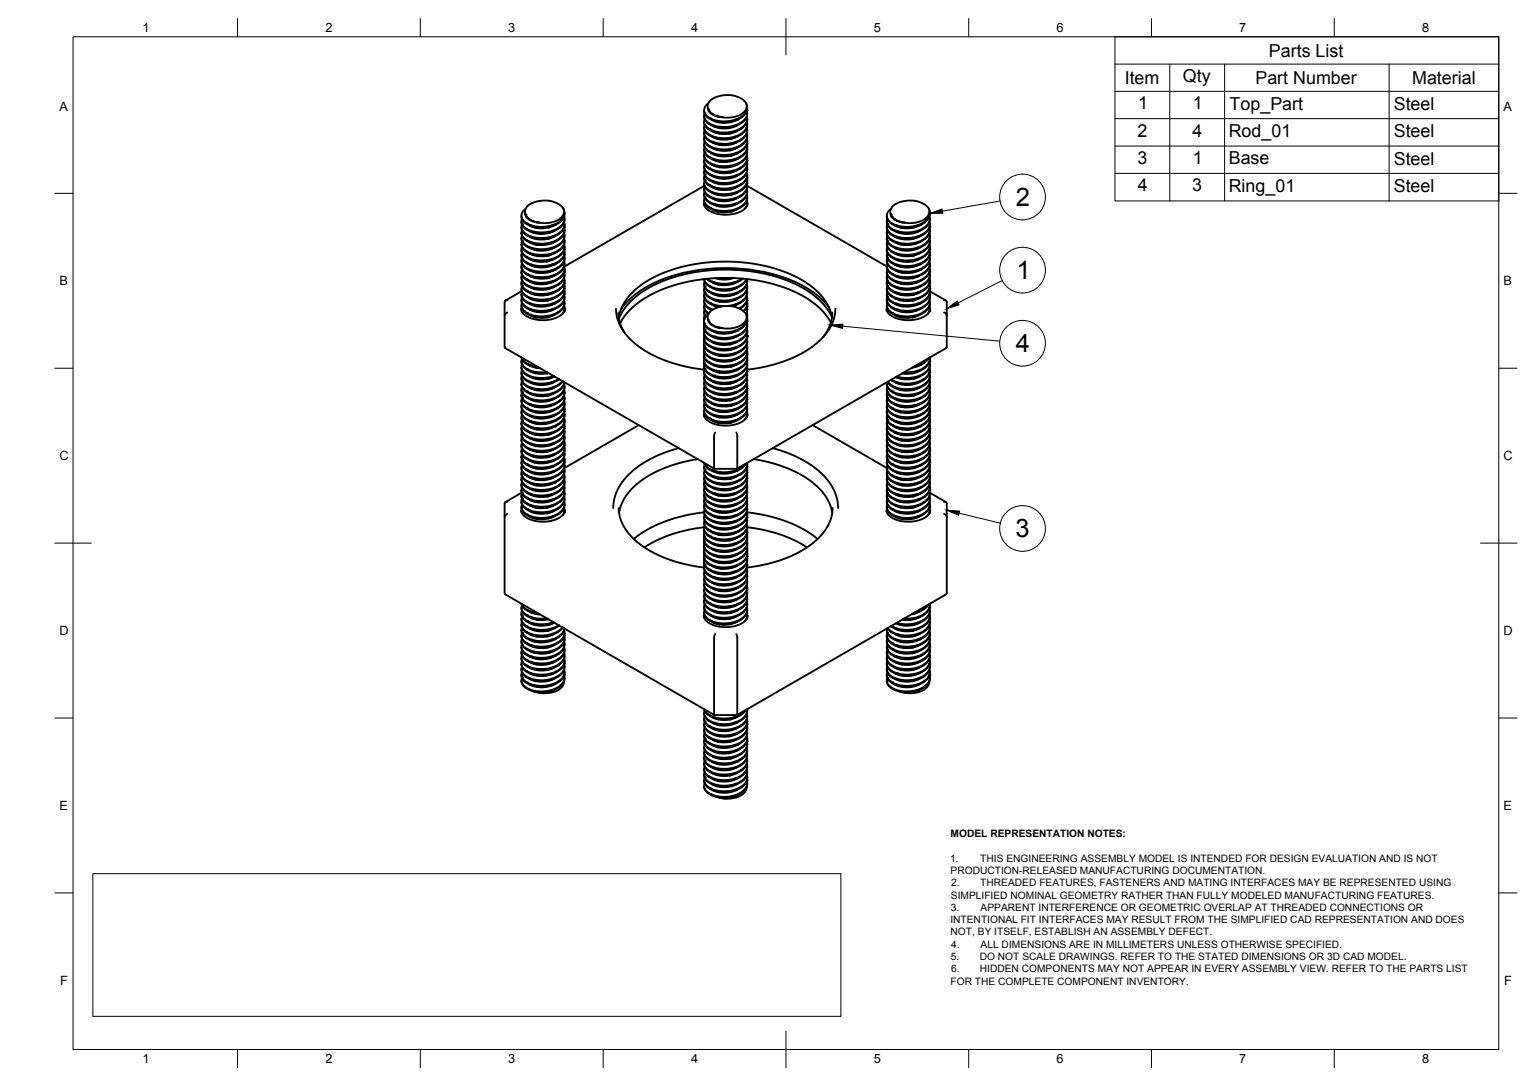
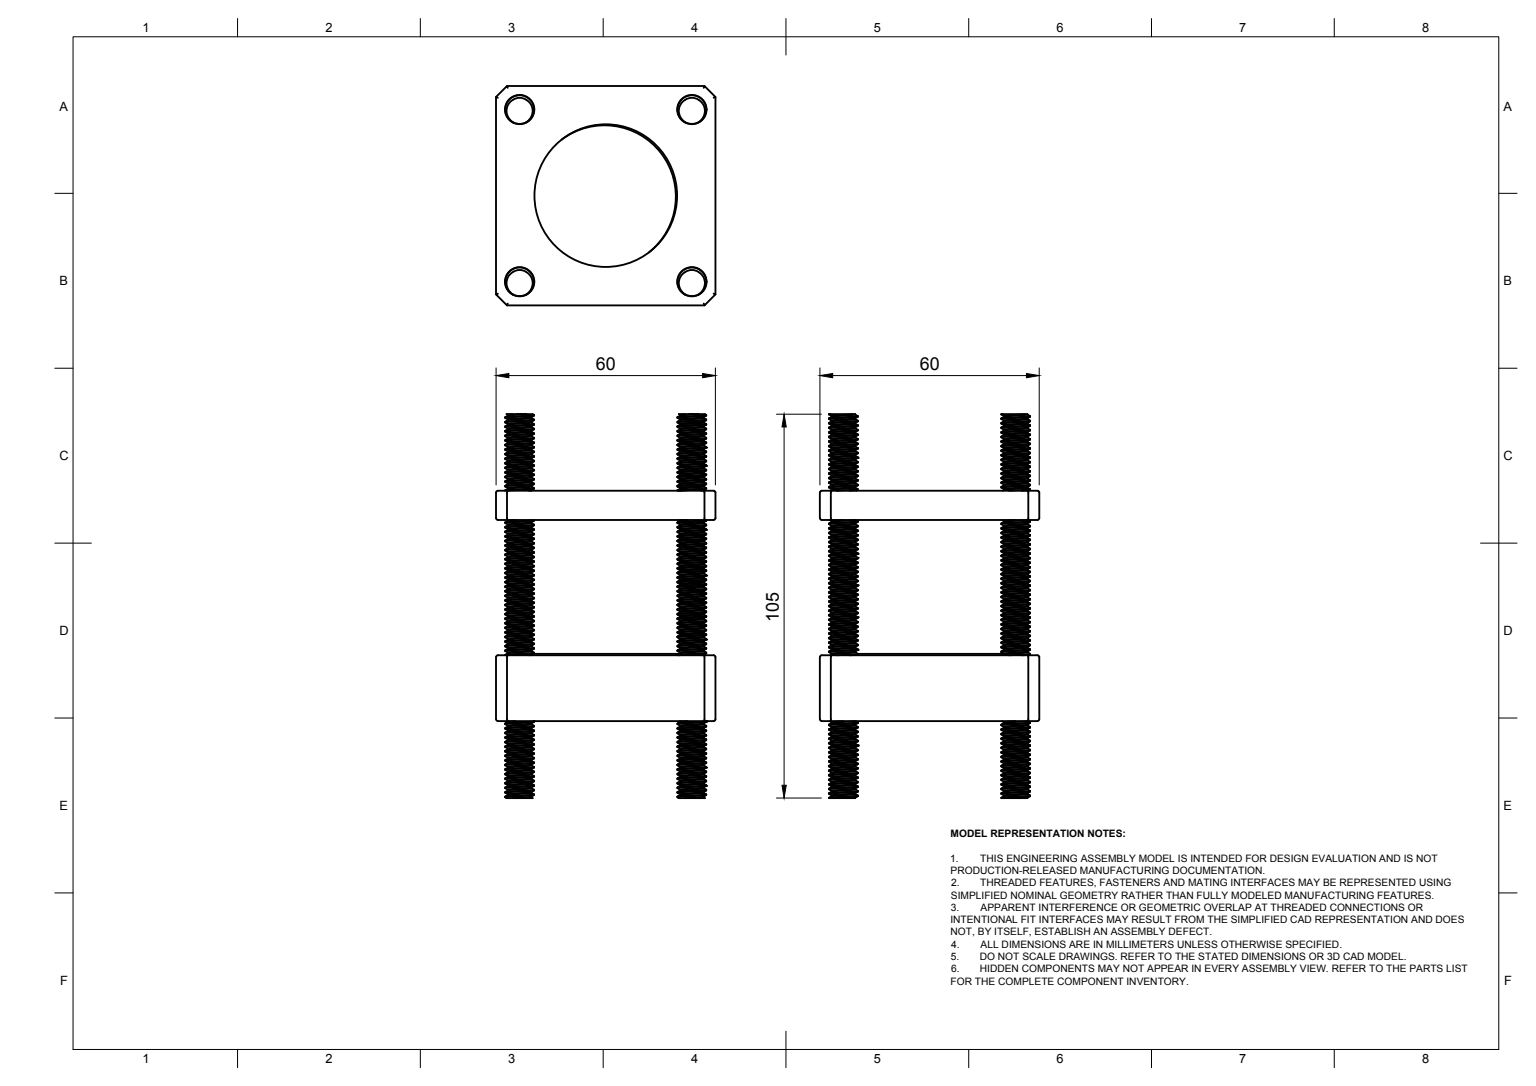
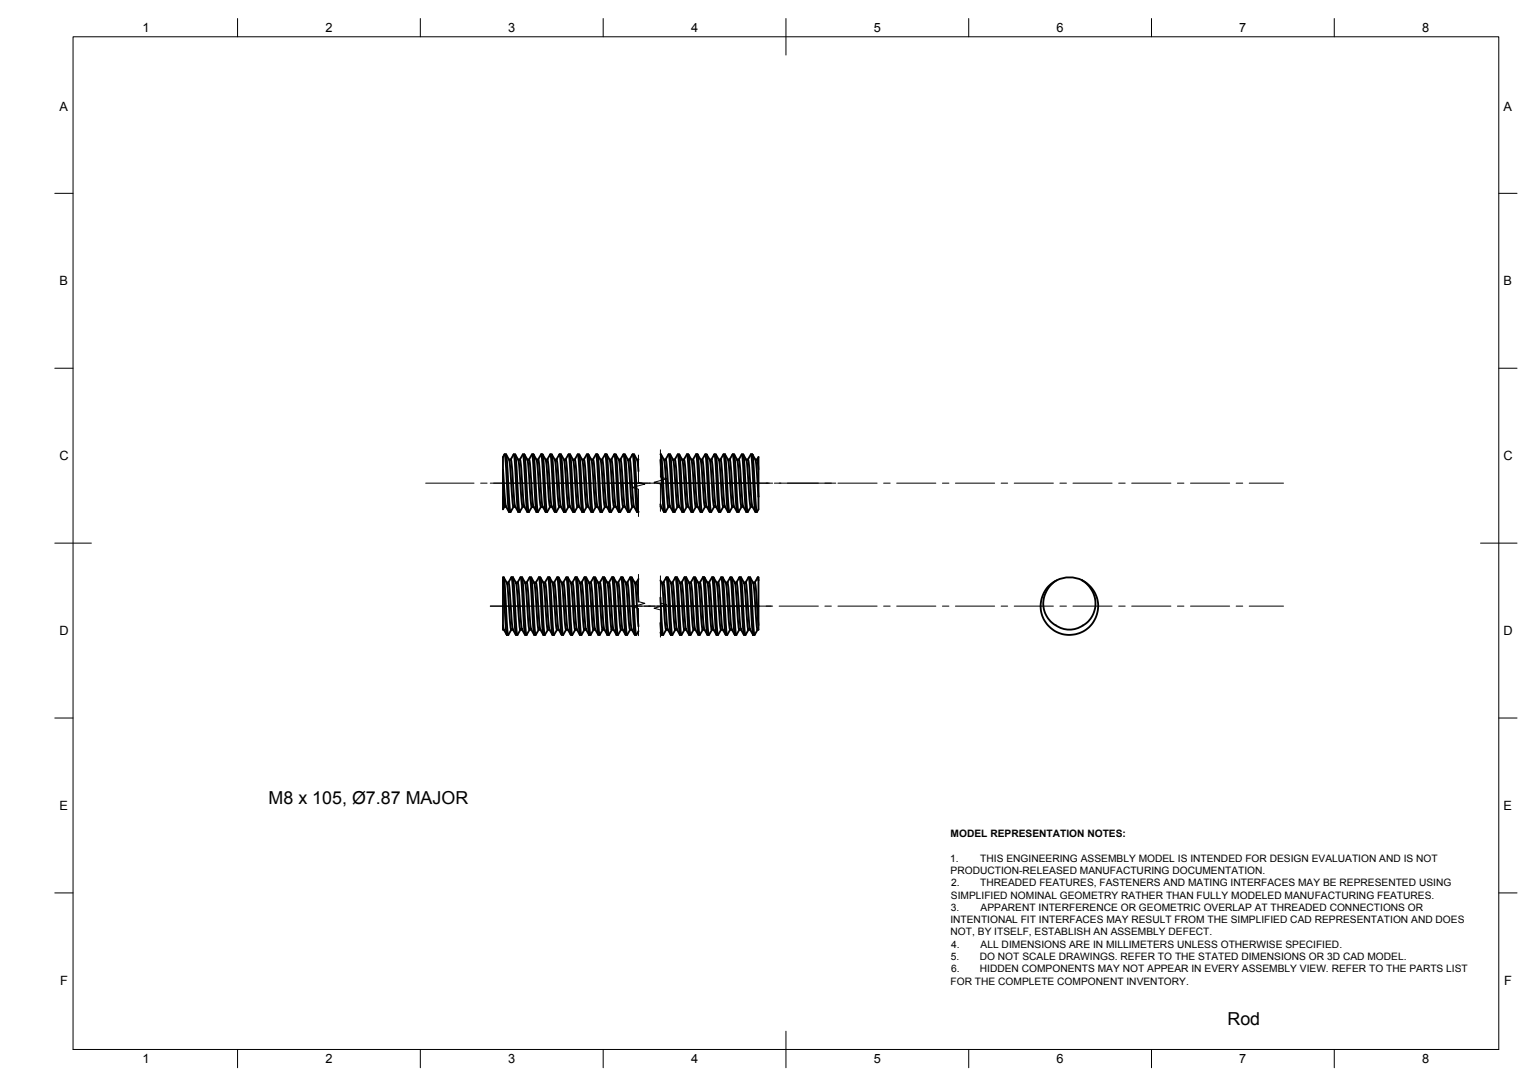
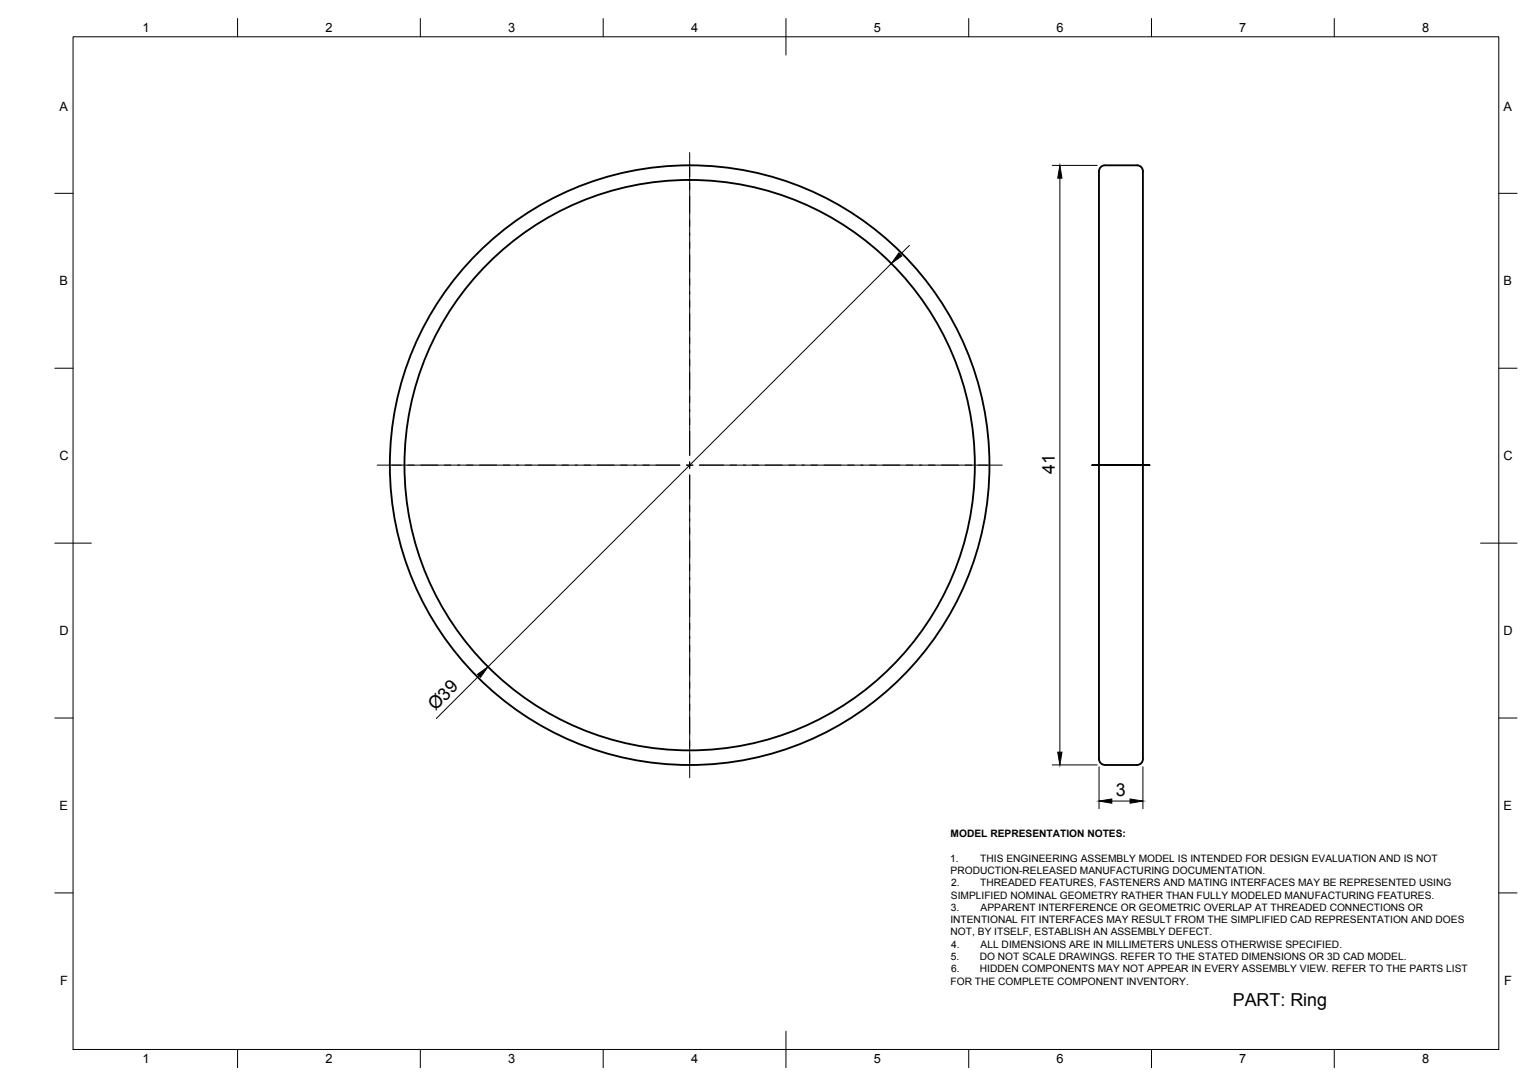
ISO-10303-21;
HEADER;
/* Generated by software containing ST-Developer
 * from STEP Tools, Inc. (www.steptools.com) 
 */

FILE_DESCRIPTION(
/* description */ (''),
/* implementation_level */ '2;1');

FILE_NAME(
/* name */ 'BR-170',
/* time_stamp */ '2026-10-05T14:32:37-07:00',
/* author */ (''),
/* organization */ (''),
/* preprocessor_version */ 'ST-DEVELOPER v20.2',
/* originating_system */ 'Autodesk Translation Framework v15.15.0.0',
/* authorisation */ '');

FILE_SCHEMA (('AUTOMOTIVE_DESIGN { 1 0 10303 214 3 1 1 }'));
ENDSEC;

DATA;
#10=MECHANICAL_DESIGN_GEOMETRIC_PRESENTATION_REPRESENTATION('',(#494,#495,
#496,#497),#74103);
#11=ITEM_DEFINED_TRANSFORMATION($,$,#4623,#4938);
#12=ITEM_DEFINED_TRANSFORMATION($,$,#4845,#4939);
#13=ITEM_DEFINED_TRANSFORMATION($,$,#4729,#4940);
#14=ITEM_DEFINED_TRANSFORMATION($,$,#4824,#4941);
#15=ITEM_DEFINED_TRANSFORMATION($,$,#4824,#4942);
#16=ITEM_DEFINED_TRANSFORMATION($,$,#4824,#4943);
#17=ITEM_DEFINED_TRANSFORMATION($,$,#4845,#4944);
#18=ITEM_DEFINED_TRANSFORMATION($,$,#4845,#4945);
#19=ITEM_DEFINED_TRANSFORMATION($,$,#4845,#4946);
#20=(
REPRESENTATION_RELATIONSHIP($,$,#74128,#74127)
REPRESENTATION_RELATIONSHIP_WITH_TRANSFORMATION(#11)
SHAPE_REPRESENTATION_RELATIONSHIP()
);
#21=(
REPRESENTATION_RELATIONSHIP($,$,#74131,#74127)
REPRESENTATION_RELATIONSHIP_WITH_TRANSFORMATION(#12)
SHAPE_REPRESENTATION_RELATIONSHIP()
);
#22=(
REPRESENTATION_RELATIONSHIP($,$,#74129,#74127)
REPRESENTATION_RELATIONSHIP_WITH_TRANSFORMATION(#13)
SHAPE_REPRESENTATION_RELATIONSHIP()
);
#23=(
REPRESENTATION_RELATIONSHIP($,$,#74130,#74127)
REPRESENTATION_RELATIONSHIP_WITH_TRANSFORMATION(#14)
SHAPE_REPRESENTATION_RELATIONSHIP()
);
#24=(
REPRESENTATION_RELATIONSHIP($,$,#74130,#74127)
REPRESENTATION_RELATIONSHIP_WITH_TRANSFORMATION(#15)
SHAPE_REPRESENTATION_RELATIONSHIP()
);
#25=(
REPRESENTATION_RELATIONSHIP($,$,#74130,#74127)
REPRESENTATION_RELATIONSHIP_WITH_TRANSFORMATION(#16)
SHAPE_REPRESENTATION_RELATIONSHIP()
);
#26=(
REPRESENTATION_RELATIONSHIP($,$,#74131,#74127)
REPRESENTATION_RELATIONSHIP_WITH_TRANSFORMATION(#17)
SHAPE_REPRESENTATION_RELATIONSHIP()
);
#27=(
REPRESENTATION_RELATIONSHIP($,$,#74131,#74127)
REPRESENTATION_RELATIONSHIP_WITH_TRANSFORMATION(#18)
SHAPE_REPRESENTATION_RELATIONSHIP()
);
#28=(
REPRESENTATION_RELATIONSHIP($,$,#74131,#74127)
REPRESENTATION_RELATIONSHIP_WITH_TRANSFORMATION(#19)
SHAPE_REPRESENTATION_RELATIONSHIP()
);
#29=CONTEXT_DEPENDENT_SHAPE_REPRESENTATION(#20,#74118);
#30=CONTEXT_DEPENDENT_SHAPE_REPRESENTATION(#21,#74119);
#31=CONTEXT_DEPENDENT_SHAPE_REPRESENTATION(#22,#74120);
#32=CONTEXT_DEPENDENT_SHAPE_REPRESENTATION(#23,#74121);
#33=CONTEXT_DEPENDENT_SHAPE_REPRESENTATION(#24,#74122);
#34=CONTEXT_DEPENDENT_SHAPE_REPRESENTATION(#25,#74123);
#35=CONTEXT_DEPENDENT_SHAPE_REPRESENTATION(#26,#74124);
#36=CONTEXT_DEPENDENT_SHAPE_REPRESENTATION(#27,#74125);
#37=CONTEXT_DEPENDENT_SHAPE_REPRESENTATION(#28,#74126);
#38=NEXT_ASSEMBLY_USAGE_OCCURRENCE('Top_Part:1','Top_Part:1',
'Top_Part:1',#74133,#74134,'Top_Part:1');
#39=NEXT_ASSEMBLY_USAGE_OCCURRENCE('Rod_01:1','Rod_01:1','Rod_01:1',#74133,
#74137,'Rod_01:1');
#40=NEXT_ASSEMBLY_USAGE_OCCURRENCE('Base:1','Base:1','Base:1',#74133,#74135,
'Base:1');
#41=NEXT_ASSEMBLY_USAGE_OCCURRENCE('Ring_01:1','Ring_01:1','Ring_01:1',
#74133,#74136,'Ring_01:1');
#42=NEXT_ASSEMBLY_USAGE_OCCURRENCE('Ring_01:2','Ring_01:2','Ring_01:2',
#74133,#74136,'Ring_01:2');
#43=NEXT_ASSEMBLY_USAGE_OCCURRENCE('Ring_01:3','Ring_01:3','Ring_01:3',
#74133,#74136,'Ring_01:3');
#44=NEXT_ASSEMBLY_USAGE_OCCURRENCE('Rod_01:2','Rod_01:2','Rod_01:2',#74133,
#74137,'Rod_01:2');
#45=NEXT_ASSEMBLY_USAGE_OCCURRENCE('Rod_01:3','Rod_01:3','Rod_01:3',#74133,
#74137,'Rod_01:3');
#46=NEXT_ASSEMBLY_USAGE_OCCURRENCE('Rod_01:4','Rod_01:4','Rod_01:4',#74133,
#74137,'Rod_01:4');
#47=B_SPLINE_SURFACE_WITH_KNOTS('',3,3,((#69430,#69431,#69432,#69433,#69434,
#69435,#69436,#69437,#69438,#69439,#69440,#69441,#69442,#69443,#69444,#69445,
#69446,#69447,#69448,#69449,#69450,#69451,#69452,#69453,#69454,#69455,#69456,
#69457,#69458,#69459,#69460,#69461,#69462,#69463,#69464,#69465,#69466,#69467,
#69468,#69469,#69470,#69471,#69472,#69473,#69474,#69475,#69476,#69477,#69478,
#69479,#69480,#69481,#69482,#69483,#69484,#69485,#69486,#69487,#69488,#69489,
#69490,#69491,#69492,#69493,#69494,#69495,#69496,#69497,#69498,#69499,#69500,
#69501,#69502,#69503,#69504,#69505,#69506,#69507,#69508,#69509,#69510,#69511,
#69512,#69513,#69514,#69515,#69516,#69517,#69518,#69519,#69520,#69521,#69522,
#69523,#69524,#69525,#69526,#69527,#69528,#69529,#69530,#69531,#69532,#69533,
#69534,#69535,#69536,#69537,#69538,#69539,#69540,#69541,#69542,#69543,#69544,
#69545,#69546,#69547,#69548,#69549,#69550,#69551,#69552,#69553,#69554,#69555,
#69556,#69557,#69558,#69559,#69560,#69561,#69562,#69563,#69564,#69565,#69566,
#69567,#69568,#69569,#69570,#69571,#69572,#69573,#69574,#69575,#69576,#69577,
#69578,#69579,#69580,#69581,#69582,#69583,#69584,#69585,#69586,#69587,#69588,
#69589,#69590,#69591,#69592,#69593,#69594,#69595,#69596,#69597,#69598,#69599,
#69600,#69601,#69602,#69603,#69604,#69605,#69606,#69607,#69608,#69609,#69610,
#69611,#69612,#69613,#69614,#69615,#69616,#69617,#69618,#69619,#69620,#69621,
#69622,#69623,#69624,#69625,#69626,#69627,#69628,#69629,#69630,#69631,#69632,
#69633,#69634,#69635,#69636,#69637,#69638,#69639,#69640,#69641,#69642,#69643,
#69644,#69645,#69646,#69647,#69648,#69649,#69650,#69651,#69652,#69653,#69654,
#69655,#69656,#69657,#69658,#69659,#69660,#69661,#69662,#69663,#69664,#69665,
#69666,#69667,#69668,#69669,#69670,#69671,#69672,#69673,#69674,#69675,#69676,
#69677,#69678,#69679,#69680,#69681,#69682,#69683,#69684,#69685,#69686,#69687,
#69688,#69689,#69690,#69691,#69692,#69693,#69694,#69695,#69696,#69697,#69698,
#69699,#69700,#69701,#69702,#69703,#69704,#69705,#69706,#69707,#69708,#69709,
#69710,#69711,#69712,#69713,#69714,#69715,#69716,#69717,#69718,#69719,#69720,
#69721,#69722,#69723,#69724,#69725,#69726,#69727,#69728,#69729,#69730,#69731,
#69732,#69733,#69734,#69735,#69736,#69737,#69738,#69739,#69740,#69741,#69742,
#69743,#69744,#69745,#69746,#69747,#69748,#69749,#69750,#69751,#69752,#69753,
#69754,#69755,#69756,#69757,#69758,#69759,#69760,#69761,#69762,#69763,#69764,
#69765,#69766,#69767,#69768,#69769,#69770,#69771,#69772,#69773,#69774,#69775,
#69776,#69777,#69778,#69779,#69780,#69781,#69782,#69783,#69784,#69785,#69786,
#69787,#69788,#69789,#69790,#69791,#69792,#69793,#69794,#69795,#69796,#69797,
#69798,#69799,#69800,#69801,#69802,#69803,#69804,#69805,#69806,#69807,#69808,
#69809,#69810,#69811,#69812,#69813,#69814,#69815,#69816,#69817,#69818,#69819,
#69820,#69821,#69822,#69823,#69824,#69825,#69826,#69827,#69828,#69829,#69830,
#69831,#69832,#69833,#69834,#69835,#69836,#69837,#69838,#69839,#69840,#69841,
#69842,#69843,#69844,#69845,#69846,#69847,#69848,#69849,#69850,#69851,#69852,
#69853,#69854,#69855,#69856,#69857,#69858,#69859,#69860,#69861,#69862,#69863,
#69864,#69865,#69866,#69867,#69868,#69869,#69870,#69871,#69872,#69873,#69874,
#69875,#69876,#69877,#69878,#69879,#69880,#69881,#69882,#69883,#69884,#69885,
#69886,#69887,#69888,#69889,#69890,#69891,#69892,#69893,#69894,#69895,#69896,
#69897,#69898,#69899,#69900,#69901,#69902,#69903,#69904,#69905,#69906,#69907,
#69908,#69909,#69910,#69911,#69912,#69913,#69914,#69915,#69916,#69917,#69918,
#69919,#69920,#69921,#69922,#69923,#69924,#69925,#69926,#69927,#69928,#69929,
#69930,#69931,#69932,#69933,#69934,#69935,#69936,#69937,#69938,#69939,#69940,
#69941,#69942,#69943,#69944,#69945,#69946,#69947,#69948,#69949,#69950,#69951,
#69952,#69953,#69954,#69955,#69956,#69957,#69958,#69959,#69960,#69961,#69962),
(#69963,#69964,#69965,#69966,#69967,#69968,#69969,#69970,#69971,#69972,
#69973,#69974,#69975,#69976,#69977,#69978,#69979,#69980,#69981,#69982,#69983,
#69984,#69985,#69986,#69987,#69988,#69989,#69990,#69991,#69992,#69993,#69994,
#69995,#69996,#69997,#69998,#69999,#70000,#70001,#70002,#70003,#70004,#70005,
#70006,#70007,#70008,#70009,#70010,#70011,#70012,#70013,#70014,#70015,#70016,
#70017,#70018,#70019,#70020,#70021,#70022,#70023,#70024,#70025,#70026,#70027,
#70028,#70029,#70030,#70031,#70032,#70033,#70034,#70035,#70036,#70037,#70038,
#70039,#70040,#70041,#70042,#70043,#70044,#70045,#70046,#70047,#70048,#70049,
#70050,#70051,#70052,#70053,#70054,#70055,#70056,#70057,#70058,#70059,#70060,
#70061,#70062,#70063,#70064,#70065,#70066,#70067,#70068,#70069,#70070,#70071,
#70072,#70073,#70074,#70075,#70076,#70077,#70078,#70079,#70080,#70081,#70082,
#70083,#70084,#70085,#70086,#70087,#70088,#70089,#70090,#70091,#70092,#70093,
#70094,#70095,#70096,#70097,#70098,#70099,#70100,#70101,#70102,#70103,#70104,
#70105,#70106,#70107,#70108,#70109,#70110,#70111,#70112,#70113,#70114,#70115,
#70116,#70117,#70118,#70119,#70120,#70121,#70122,#70123,#70124,#70125,#70126,
#70127,#70128,#70129,#70130,#70131,#70132,#70133,#70134,#70135,#70136,#70137,
#70138,#70139,#70140,#70141,#70142,#70143,#70144,#70145,#70146,#70147,#70148,
#70149,#70150,#70151,#70152,#70153,#70154,#70155,#70156,#70157,#70158,#70159,
#70160,#70161,#70162,#70163,#70164,#70165,#70166,#70167,#70168,#70169,#70170,
#70171,#70172,#70173,#70174,#70175,#70176,#70177,#70178,#70179,#70180,#70181,
#70182,#70183,#70184,#70185,#70186,#70187,#70188,#70189,#70190,#70191,#70192,
#70193,#70194,#70195,#70196,#70197,#70198,#70199,#70200,#70201,#70202,#70203,
#70204,#70205,#70206,#70207,#70208,#70209,#70210,#70211,#70212,#70213,#70214,
#70215,#70216,#70217,#70218,#70219,#70220,#70221,#70222,#70223,#70224,#70225,
#70226,#70227,#70228,#70229,#70230,#70231,#70232,#70233,#70234,#70235,#70236,
#70237,#70238,#70239,#70240,#70241,#70242,#70243,#70244,#70245,#70246,#70247,
#70248,#70249,#70250,#70251,#70252,#70253,#70254,#70255,#70256,#70257,#70258,
#70259,#70260,#70261,#70262,#70263,#70264,#70265,#70266,#70267,#70268,#70269,
#70270,#70271,#70272,#70273,#70274,#70275,#70276,#70277,#70278,#70279,#70280,
#70281,#70282,#70283,#70284,#70285,#70286,#70287,#70288,#70289,#70290,#70291,
#70292,#70293,#70294,#70295,#70296,#70297,#70298,#70299,#70300,#70301,#70302,
#70303,#70304,#70305,#70306,#70307,#70308,#70309,#70310,#70311,#70312,#70313,
#70314,#70315,#70316,#70317,#70318,#70319,#70320,#70321,#70322,#70323,#70324,
#70325,#70326,#70327,#70328,#70329,#70330,#70331,#70332,#70333,#70334,#70335,
#70336,#70337,#70338,#70339,#70340,#70341,#70342,#70343,#70344,#70345,#70346,
#70347,#70348,#70349,#70350,#70351,#70352,#70353,#70354,#70355,#70356,#70357,
#70358,#70359,#70360,#70361,#70362,#70363,#70364,#70365,#70366,#70367,#70368,
#70369,#70370,#70371,#70372,#70373,#70374,#70375,#70376,#70377,#70378,#70379,
#70380,#70381,#70382,#70383,#70384,#70385,#70386,#70387,#70388,#70389,#70390,
#70391,#70392,#70393,#70394,#70395,#70396,#70397,#70398,#70399,#70400,#70401,
#70402,#70403,#70404,#70405,#70406,#70407,#70408,#70409,#70410,#70411,#70412,
#70413,#70414,#70415,#70416,#70417,#70418,#70419,#70420,#70421,#70422,#70423,
#70424,#70425,#70426,#70427,#70428,#70429,#70430,#70431,#70432,#70433,#70434,
#70435,#70436,#70437,#70438,#70439,#70440,#70441,#70442,#70443,#70444,#70445,
#70446,#70447,#70448,#70449,#70450,#70451,#70452,#70453,#70454,#70455,#70456,
#70457,#70458,#70459,#70460,#70461,#70462,#70463,#70464,#70465,#70466,#70467,
#70468,#70469,#70470,#70471,#70472,#70473,#70474,#70475,#70476,#70477,#70478,
#70479,#70480,#70481,#70482,#70483,#70484,#70485,#70486,#70487,#70488,#70489,
#70490,#70491,#70492,#70493,#70494,#70495),(#70496,#70497,#70498,#70499,
#70500,#70501,#70502,#70503,#70504,#70505,#70506,#70507,#70508,#70509,#70510,
#70511,#70512,#70513,#70514,#70515,#70516,#70517,#70518,#70519,#70520,#70521,
#70522,#70523,#70524,#70525,#70526,#70527,#70528,#70529,#70530,#70531,#70532,
#70533,#70534,#70535,#70536,#70537,#70538,#70539,#70540,#70541,#70542,#70543,
#70544,#70545,#70546,#70547,#70548,#70549,#70550,#70551,#70552,#70553,#70554,
#70555,#70556,#70557,#70558,#70559,#70560,#70561,#70562,#70563,#70564,#70565,
#70566,#70567,#70568,#70569,#70570,#70571,#70572,#70573,#70574,#70575,#70576,
#70577,#70578,#70579,#70580,#70581,#70582,#70583,#70584,#70585,#70586,#70587,
#70588,#70589,#70590,#70591,#70592,#70593,#70594,#70595,#70596,#70597,#70598,
#70599,#70600,#70601,#70602,#70603,#70604,#70605,#70606,#70607,#70608,#70609,
#70610,#70611,#70612,#70613,#70614,#70615,#70616,#70617,#70618,#70619,#70620,
#70621,#70622,#70623,#70624,#70625,#70626,#70627,#70628,#70629,#70630,#70631,
#70632,#70633,#70634,#70635,#70636,#70637,#70638,#70639,#70640,#70641,#70642,
#70643,#70644,#70645,#70646,#70647,#70648,#70649,#70650,#70651,#70652,#70653,
#70654,#70655,#70656,#70657,#70658,#70659,#70660,#70661,#70662,#70663,#70664,
#70665,#70666,#70667,#70668,#70669,#70670,#70671,#70672,#70673,#70674,#70675,
#70676,#70677,#70678,#70679,#70680,#70681,#70682,#70683,#70684,#70685,#70686,
#70687,#70688,#70689,#70690,#70691,#70692,#70693,#70694,#70695,#70696,#70697,
#70698,#70699,#70700,#70701,#70702,#70703,#70704,#70705,#70706,#70707,#70708,
#70709,#70710,#70711,#70712,#70713,#70714,#70715,#70716,#70717,#70718,#70719,
#70720,#70721,#70722,#70723,#70724,#70725,#70726,#70727,#70728,#70729,#70730,
#70731,#70732,#70733,#70734,#70735,#70736,#70737,#70738,#70739,#70740,#70741,
#70742,#70743,#70744,#70745,#70746,#70747,#70748,#70749,#70750,#70751,#70752,
#70753,#70754,#70755,#70756,#70757,#70758,#70759,#70760,#70761,#70762,#70763,
#70764,#70765,#70766,#70767,#70768,#70769,#70770,#70771,#70772,#70773,#70774,
#70775,#70776,#70777,#70778,#70779,#70780,#70781,#70782,#70783,#70784,#70785,
#70786,#70787,#70788,#70789,#70790,#70791,#70792,#70793,#70794,#70795,#70796,
#70797,#70798,#70799,#70800,#70801,#70802,#70803,#70804,#70805,#70806,#70807,
#70808,#70809,#70810,#70811,#70812,#70813,#70814,#70815,#70816,#70817,#70818,
#70819,#70820,#70821,#70822,#70823,#70824,#70825,#70826,#70827,#70828,#70829,
#70830,#70831,#70832,#70833,#70834,#70835,#70836,#70837,#70838,#70839,#70840,
#70841,#70842,#70843,#70844,#70845,#70846,#70847,#70848,#70849,#70850,#70851,
#70852,#70853,#70854,#70855,#70856,#70857,#70858,#70859,#70860,#70861,#70862,
#70863,#70864,#70865,#70866,#70867,#70868,#70869,#70870,#70871,#70872,#70873,
#70874,#70875,#70876,#70877,#70878,#70879,#70880,#70881,#70882,#70883,#70884,
#70885,#70886,#70887,#70888,#70889,#70890,#70891,#70892,#70893,#70894,#70895,
#70896,#70897,#70898,#70899,#70900,#70901,#70902,#70903,#70904,#70905,#70906,
#70907,#70908,#70909,#70910,#70911,#70912,#70913,#70914,#70915,#70916,#70917,
#70918,#70919,#70920,#70921,#70922,#70923,#70924,#70925,#70926,#70927,#70928,
#70929,#70930,#70931,#70932,#70933,#70934,#70935,#70936,#70937,#70938,#70939,
#70940,#70941,#70942,#70943,#70944,#70945,#70946,#70947,#70948,#70949,#70950,
#70951,#70952,#70953,#70954,#70955,#70956,#70957,#70958,#70959,#70960,#70961,
#70962,#70963,#70964,#70965,#70966,#70967,#70968,#70969,#70970,#70971,#70972,
#70973,#70974,#70975,#70976,#70977,#70978,#70979,#70980,#70981,#70982,#70983,
#70984,#70985,#70986,#70987,#70988,#70989,#70990,#70991,#70992,#70993,#70994,
#70995,#70996,#70997,#70998,#70999,#71000,#71001,#71002,#71003,#71004,#71005,
#71006,#71007,#71008,#71009,#71010,#71011,#71012,#71013,#71014,#71015,#71016,
#71017,#71018,#71019,#71020,#71021,#71022,#71023,#71024,#71025,#71026,#71027,
#71028),(#71029,#71030,#71031,#71032,#71033,#71034,#71035,#71036,#71037,
#71038,#71039,#71040,#71041,#71042,#71043,#71044,#71045,#71046,#71047,#71048,
#71049,#71050,#71051,#71052,#71053,#71054,#71055,#71056,#71057,#71058,#71059,
#71060,#71061,#71062,#71063,#71064,#71065,#71066,#71067,#71068,#71069,#71070,
#71071,#71072,#71073,#71074,#71075,#71076,#71077,#71078,#71079,#71080,#71081,
#71082,#71083,#71084,#71085,#71086,#71087,#71088,#71089,#71090,#71091,#71092,
#71093,#71094,#71095,#71096,#71097,#71098,#71099,#71100,#71101,#71102,#71103,
#71104,#71105,#71106,#71107,#71108,#71109,#71110,#71111,#71112,#71113,#71114,
#71115,#71116,#71117,#71118,#71119,#71120,#71121,#71122,#71123,#71124,#71125,
#71126,#71127,#71128,#71129,#71130,#71131,#71132,#71133,#71134,#71135,#71136,
#71137,#71138,#71139,#71140,#71141,#71142,#71143,#71144,#71145,#71146,#71147,
#71148,#71149,#71150,#71151,#71152,#71153,#71154,#71155,#71156,#71157,#71158,
#71159,#71160,#71161,#71162,#71163,#71164,#71165,#71166,#71167,#71168,#71169,
#71170,#71171,#71172,#71173,#71174,#71175,#71176,#71177,#71178,#71179,#71180,
#71181,#71182,#71183,#71184,#71185,#71186,#71187,#71188,#71189,#71190,#71191,
#71192,#71193,#71194,#71195,#71196,#71197,#71198,#71199,#71200,#71201,#71202,
#71203,#71204,#71205,#71206,#71207,#71208,#71209,#71210,#71211,#71212,#71213,
#71214,#71215,#71216,#71217,#71218,#71219,#71220,#71221,#71222,#71223,#71224,
#71225,#71226,#71227,#71228,#71229,#71230,#71231,#71232,#71233,#71234,#71235,
#71236,#71237,#71238,#71239,#71240,#71241,#71242,#71243,#71244,#71245,#71246,
#71247,#71248,#71249,#71250,#71251,#71252,#71253,#71254,#71255,#71256,#71257,
#71258,#71259,#71260,#71261,#71262,#71263,#71264,#71265,#71266,#71267,#71268,
#71269,#71270,#71271,#71272,#71273,#71274,#71275,#71276,#71277,#71278,#71279,
#71280,#71281,#71282,#71283,#71284,#71285,#71286,#71287,#71288,#71289,#71290,
#71291,#71292,#71293,#71294,#71295,#71296,#71297,#71298,#71299,#71300,#71301,
#71302,#71303,#71304,#71305,#71306,#71307,#71308,#71309,#71310,#71311,#71312,
#71313,#71314,#71315,#71316,#71317,#71318,#71319,#71320,#71321,#71322,#71323,
#71324,#71325,#71326,#71327,#71328,#71329,#71330,#71331,#71332,#71333,#71334,
#71335,#71336,#71337,#71338,#71339,#71340,#71341,#71342,#71343,#71344,#71345,
#71346,#71347,#71348,#71349,#71350,#71351,#71352,#71353,#71354,#71355,#71356,
#71357,#71358,#71359,#71360,#71361,#71362,#71363,#71364,#71365,#71366,#71367,
#71368,#71369,#71370,#71371,#71372,#71373,#71374,#71375,#71376,#71377,#71378,
#71379,#71380,#71381,#71382,#71383,#71384,#71385,#71386,#71387,#71388,#71389,
#71390,#71391,#71392,#71393,#71394,#71395,#71396,#71397,#71398,#71399,#71400,
#71401,#71402,#71403,#71404,#71405,#71406,#71407,#71408,#71409,#71410,#71411,
#71412,#71413,#71414,#71415,#71416,#71417,#71418,#71419,#71420,#71421,#71422,
#71423,#71424,#71425,#71426,#71427,#71428,#71429,#71430,#71431,#71432,#71433,
#71434,#71435,#71436,#71437,#71438,#71439,#71440,#71441,#71442,#71443,#71444,
#71445,#71446,#71447,#71448,#71449,#71450,#71451,#71452,#71453,#71454,#71455,
#71456,#71457,#71458,#71459,#71460,#71461,#71462,#71463,#71464,#71465,#71466,
#71467,#71468,#71469,#71470,#71471,#71472,#71473,#71474,#71475,#71476,#71477,
#71478,#71479,#71480,#71481,#71482,#71483,#71484,#71485,#71486,#71487,#71488,
#71489,#71490,#71491,#71492,#71493,#71494,#71495,#71496,#71497,#71498,#71499,
#71500,#71501,#71502,#71503,#71504,#71505,#71506,#71507,#71508,#71509,#71510,
#71511,#71512,#71513,#71514,#71515,#71516,#71517,#71518,#71519,#71520,#71521,
#71522,#71523,#71524,#71525,#71526,#71527,#71528,#71529,#71530,#71531,#71532,
#71533,#71534,#71535,#71536,#71537,#71538,#71539,#71540,#71541,#71542,#71543,
#71544,#71545,#71546,#71547,#71548,#71549,#71550,#71551,#71552,#71553,#71554,
#71555,#71556,#71557,#71558,#71559,#71560,#71561)),.UNSPECIFIED.,.F.,.F.,
 .F.,(4,4),(4,1,1,1,1,1,1,1,1,1,1,1,1,1,1,1,1,1,1,1,1,1,1,1,1,1,1,1,1,1,
1,1,1,1,1,1,1,1,1,1,1,1,1,1,1,1,1,1,1,1,1,1,1,1,1,1,1,1,1,1,1,1,1,1,1,1,
1,1,1,1,1,1,1,1,1,1,1,1,1,1,1,1,1,1,1,1,1,1,1,1,1,1,1,1,1,1,1,1,1,1,1,1,
1,1,1,1,1,1,1,1,1,1,1,1,1,1,1,1,1,1,1,1,1,1,1,1,1,1,1,1,1,1,1,1,1,1,1,1,
1,1,1,1,1,1,1,1,1,1,1,1,1,1,1,1,1,1,1,1,1,1,1,1,1,1,1,1,1,1,1,1,1,1,1,1,
1,1,1,1,1,1,1,1,1,1,1,1,1,1,1,1,1,1,1,1,1,1,1,1,1,1,1,1,1,1,1,1,1,1,1,1,
1,1,1,1,1,1,1,1,1,1,1,1,1,1,1,1,1,1,1,1,1,1,1,1,1,1,1,1,1,1,1,1,1,1,1,1,
1,1,1,1,1,1,1,1,1,1,1,1,1,1,1,1,1,1,1,1,1,1,1,1,1,1,1,1,1,1,1,1,1,1,1,1,
1,1,1,1,1,1,1,1,1,1,1,1,1,1,1,1,1,1,1,1,1,1,1,1,1,1,1,1,1,1,1,1,1,1,1,1,
1,1,1,1,1,1,1,1,1,1,1,1,1,1,1,1,1,1,1,1,1,1,1,1,1,1,1,1,1,1,1,1,1,1,1,1,
1,1,1,1,1,1,1,1,1,1,1,1,1,1,1,1,1,1,1,1,1,1,1,1,1,1,1,1,1,1,1,1,1,1,1,1,
1,1,1,1,1,1,1,1,1,1,1,1,1,1,1,1,1,1,1,1,1,1,1,1,1,1,1,1,1,1,1,1,1,1,1,1,
1,1,1,1,1,1,1,1,1,1,1,1,1,1,1,1,1,1,1,1,1,1,1,1,1,1,1,1,1,1,1,1,1,1,1,1,
1,1,1,1,1,1,1,1,1,1,1,1,1,1,1,1,1,1,1,1,1,1,1,1,1,1,1,1,1,1,1,1,1,1,1,1,
1,1,1,1,1,1,1,1,1,1,1,1,1,1,1,1,1,1,1,1,1,1,1,1,1,1,1,1,1,1,1,1,4),(-0.000646701964609084,
0.0823585128613958),(8.31473274985906,9.3144474053319,10.3141620608047,
11.3138767162776,12.3135913717504,13.3133060272232,14.3130206826961,15.3127353381689,
16.3124499936417,17.3121646491146,18.3118793045874,19.3115939600602,20.3113086155331,
21.3110232710059,22.3107379264787,23.3104525819516,24.3101672374244,25.3098818928972,
26.30959654837,27.3093112038429,28.3090258593157,29.3087405147885,30.3084551702614,
31.3081698257342,32.307884481207,33.3075991366799,34.3073137921527,35.3070284476255,
36.3067431030984,37.3064577585712,38.306172414044,39.3058870695169,40.3056017249897,
41.3053163804625,42.3050310359354,43.3047456914082,44.304460346881,45.3041750023539,
46.3038896578267,47.3036043132995,48.3033189687724,49.3030336242452,50.302748279718,
51.3024629351909,52.3021775906637,53.3018922461365,54.3016069016094,55.3013215570822,
56.301036212555,57.3007508680278,58.3004655235007,59.3001801789735,60.2998948344463,
61.2996094899192,62.299324145392,63.2990388008648,64.2987534563377,65.2984681118105,
66.2981827672834,67.2978974227562,68.297612078229,69.2973267337018,70.2970413891747,
71.2967560446475,72.2964707001203,73.2961853555932,74.295900011066,75.2956146665388,
76.2953293220117,77.2950439774845,78.2947586329573,79.2944732884302,80.294187943903,
81.2939025993758,82.2936172548487,83.2933319103215,84.2930465657943,85.2927612212672,
86.29247587674,87.2921905322128,88.2919051876857,89.2916198431585,90.2913344986313,
91.2910491541042,92.290763809577,93.2904784650498,94.2901931205227,95.2899077759955,
96.2896224314683,97.2893370869411,98.289051742414,99.2887663978868,100.28848105336,
101.288195708832,102.287910364305,103.287625019778,104.287339675251,105.287054330724,
106.286768986197,107.286483641669,108.286198297142,109.285912952615,110.285627608088,
111.285342263561,112.285056919034,113.284771574506,114.284486229979,115.284200885452,
116.283915540925,117.283630196398,118.283344851871,119.283059507343,120.282774162816,
121.282488818289,122.282203473762,123.281918129235,124.281632784708,125.28134744018,
126.281062095653,127.280776751126,128.280491406599,129.280206062072,130.279920717545,
131.279635373017,132.27935002849,133.279064683963,134.278779339436,135.278493994909,
136.278208650382,137.277923305854,138.277637961327,139.2773526168,140.277067272273,
141.276781927746,142.276496583219,143.276211238691,144.275925894164,145.275640549637,
146.27535520511,147.275069860583,148.274784516056,149.274499171528,150.274213827001,
151.273928482474,152.273643137947,153.27335779342,154.273072448893,155.272787104365,
156.272501759838,157.272216415311,158.271931070784,159.271645726257,160.27136038173,
161.271075037202,162.270789692675,163.270504348148,164.270219003621,165.269933659094,
166.269648314567,167.269362970039,168.269077625512,169.268792280985,170.268506936458,
171.268221591931,172.267936247404,173.267650902876,174.267365558349,175.267080213822,
176.266794869295,177.266509524768,178.266224180241,179.265938835713,180.265653491186,
181.265368146659,182.265082802132,183.264797457605,184.264512113078,185.26422676855,
186.263941424023,187.263656079496,188.263370734969,189.263085390442,190.262800045915,
191.262514701387,192.26222935686,193.261944012333,194.261658667806,195.261373323279,
196.261087978752,197.260802634224,198.260517289697,199.26023194517,200.259946600643,
201.259661256116,202.259375911589,203.259090567061,204.258805222534,205.258519878007,
206.25823453348,207.257949188953,208.257663844426,209.257378499898,210.257093155371,
211.256807810844,212.256522466317,213.25623712179,214.255951777263,215.255666432735,
216.255381088208,217.255095743681,218.254810399154,219.254525054627,220.2542397101,
221.253954365572,222.253669021045,223.253383676518,224.253098331991,225.252812987464,
226.252527642937,227.252242298409,228.251956953882,229.251671609355,230.251386264828,
231.251100920301,232.250815575774,233.250530231246,234.250244886719,235.249959542192,
236.249674197665,237.249388853138,238.249103508611,239.248818164083,240.248532819556,
241.248247475029,242.247962130502,243.247676785975,244.247391441448,245.24710609692,
246.246820752393,247.246535407866,248.246250063339,249.245964718812,250.245679374285,
251.245394029757,252.24510868523,253.244823340703,254.244537996176,255.244252651649,
256.243967307122,257.243681962594,258.243396618067,259.24311127354,260.242825929013,
261.242540584486,262.242255239959,263.241969895431,264.241684550904,265.241399206377,
266.24111386185,267.240828517323,268.240543172795,269.240257828268,270.239972483741,
271.239687139214,272.239401794687,273.23911645016,274.238831105632,275.238545761105,
276.238260416578,277.237975072051,278.237689727524,279.237404382997,280.237119038469,
281.236833693942,282.236548349415,283.236263004888,284.235977660361,285.235692315834,
286.235406971306,287.235121626779,288.234836282252,289.234550937725,290.234265593198,
291.233980248671,292.233694904143,293.233409559616,294.233124215089,295.232838870562,
296.232553526035,297.232268181508,298.23198283698,299.231697492453,300.231412147926,
301.231126803399,302.230841458872,303.230556114345,304.230270769817,305.22998542529,
306.229700080763,307.229414736236,308.229129391709,309.228844047182,310.228558702654,
311.228273358127,312.2279880136,313.227702669073,314.227417324546,315.227131980019,
316.226846635491,317.226561290964,318.226275946437,319.22599060191,320.225705257383,
321.225419912856,322.225134568328,323.224849223801,324.224563879274,325.224278534747,
326.22399319022,327.223707845693,328.223422501165,329.223137156638,330.222851812111,
331.222566467584,332.222281123057,333.22199577853,334.221710434002,335.221425089475,
336.221139744948,337.220854400421,338.220569055894,339.220283711367,340.219998366839,
341.219713022312,342.219427677785,343.219142333258,344.218856988731,345.218571644204,
346.218286299676,347.218000955149,348.217715610622,349.217430266095,350.217144921568,
351.216859577041,352.216574232513,353.216288887986,354.216003543459,355.215718198932,
356.215432854405,357.215147509878,358.21486216535,359.214576820823,360.214291476296,
361.214006131769,362.213720787242,363.213435442715,364.213150098187,365.21286475366,
366.212579409133,367.212294064606,368.212008720079,369.211723375552,370.211438031024,
371.211152686497,372.21086734197,373.210581997443,374.210296652916,375.210011308389,
376.209725963861,377.209440619334,378.209155274807,379.20886993028,380.208584585753,
381.208299241226,382.208013896698,383.207728552171,384.207443207644,385.207157863117,
386.20687251859,387.206587174063,388.206301829535,389.206016485008,390.205731140481,
391.205445795954,392.205160451427,393.2048751069,394.204589762372,395.204304417845,
396.204019073318,397.203733728791,398.203448384264,399.203163039737,400.202877695209,
401.202592350682,402.202307006155,403.202021661628,404.201736317101,405.201450972574,
406.201165628046,407.200880283519,408.200594938992,409.200309594465,410.200024249938,
411.199738905411,412.199453560883,413.199168216356,414.198882871829,415.198597527302,
416.198312182775,417.198026838248,418.19774149372,419.197456149193,420.197170804666,
421.196885460139,422.196600115612,423.196314771085,424.196029426557,425.19574408203,
426.195458737503,427.195173392976,428.194888048449,429.194602703922,430.194317359394,
431.194032014867,432.19374667034,433.193461325813,434.193175981286,435.192890636758,
436.192605292231,437.192319947704,438.192034603177,439.19174925865,440.191463914123,
441.191178569595,442.190893225068,443.190607880541,444.190322536014,445.190037191487,
446.18975184696,447.189466502432,448.189181157905,449.188895813378,450.188610468851,
451.188325124324,452.188039779797,453.187754435269,454.187469090742,455.187183746215,
456.186898401688,457.186613057161,458.186327712634,459.186042368106,460.185757023579,
461.185471679052,462.185186334525,463.184900989998,464.184615645471,465.184330300943,
466.184044956416,467.183759611889,468.183474267362,469.183188922835,470.182903578308,
471.18261823378,472.182332889253,473.182047544726,474.181762200199,475.181476855672,
476.181191511145,477.180906166617,478.18062082209,479.180335477563,480.180050133036,
481.179764788509,482.179479443982,483.179194099454,484.178908754927,485.1786234104,
486.178338065873,487.178052721346,488.177767376819,489.177482032291,490.177196687764,
491.176911343237,492.17662599871,493.176340654183,494.176055309656,495.175769965128,
496.175484620601,497.175199276074,498.174913931547,499.17462858702,500.174343242493,
501.174057897965,502.173772553438,503.173487208911,504.173201864384,505.172916519857,
506.17263117533,507.172345830802,508.172060486275,509.171775141748,510.171489797221,
511.171204452694,512.170919108167,513.170633763639,514.170348419112,515.170063074585,
516.169777730058,517.169492385531,518.169207041004,519.168921696476,520.168636351949,
521.168351007422,522.168065662895,523.167780318368,524.167494973841,525.167209629313,
526.166924284786,527.166638940259,528.166353595732,529.166068251205,530.165782906678,
531.16549756215,532.165212217623,533.164926873096,534.164641528569,535.164356184042,
536.164070839515,537.163785494987,538.164146852425),.UNSPECIFIED.);
#48=B_SPLINE_SURFACE_WITH_KNOTS('',3,3,((#71753,#71754,#71755,#71756,#71757,
#71758,#71759,#71760,#71761,#71762,#71763,#71764,#71765,#71766,#71767,#71768,
#71769,#71770,#71771,#71772,#71773,#71774,#71775,#71776,#71777,#71778,#71779,
#71780,#71781,#71782,#71783,#71784,#71785,#71786,#71787,#71788,#71789,#71790,
#71791,#71792,#71793,#71794,#71795,#71796,#71797,#71798,#71799,#71800,#71801,
#71802,#71803,#71804,#71805,#71806,#71807,#71808,#71809,#71810,#71811,#71812,
#71813,#71814,#71815,#71816,#71817,#71818,#71819,#71820,#71821,#71822,#71823,
#71824,#71825,#71826,#71827,#71828,#71829,#71830,#71831,#71832,#71833,#71834,
#71835,#71836,#71837,#71838,#71839,#71840,#71841,#71842,#71843,#71844,#71845,
#71846,#71847,#71848,#71849,#71850,#71851,#71852,#71853,#71854,#71855,#71856,
#71857,#71858,#71859,#71860,#71861,#71862,#71863,#71864,#71865,#71866,#71867,
#71868,#71869,#71870,#71871,#71872,#71873,#71874,#71875,#71876,#71877,#71878,
#71879,#71880,#71881,#71882,#71883,#71884,#71885,#71886,#71887,#71888,#71889,
#71890,#71891,#71892,#71893,#71894,#71895,#71896,#71897,#71898,#71899,#71900,
#71901,#71902,#71903,#71904,#71905,#71906,#71907,#71908,#71909,#71910,#71911,
#71912,#71913,#71914,#71915,#71916,#71917,#71918,#71919,#71920,#71921,#71922,
#71923,#71924,#71925,#71926,#71927,#71928,#71929,#71930,#71931,#71932,#71933,
#71934,#71935,#71936,#71937,#71938,#71939,#71940,#71941,#71942,#71943,#71944,
#71945,#71946,#71947,#71948,#71949,#71950,#71951,#71952,#71953,#71954,#71955,
#71956,#71957,#71958,#71959,#71960,#71961,#71962,#71963,#71964,#71965,#71966,
#71967,#71968,#71969,#71970,#71971,#71972,#71973,#71974,#71975,#71976,#71977,
#71978,#71979,#71980,#71981,#71982,#71983,#71984,#71985,#71986,#71987,#71988,
#71989,#71990,#71991,#71992,#71993,#71994,#71995,#71996,#71997,#71998,#71999,
#72000,#72001,#72002,#72003,#72004,#72005,#72006,#72007,#72008,#72009,#72010,
#72011,#72012,#72013,#72014,#72015,#72016,#72017,#72018,#72019,#72020,#72021,
#72022,#72023,#72024,#72025,#72026,#72027,#72028,#72029,#72030,#72031,#72032,
#72033,#72034,#72035,#72036,#72037,#72038,#72039,#72040,#72041,#72042,#72043,
#72044,#72045,#72046,#72047,#72048,#72049,#72050,#72051,#72052,#72053,#72054,
#72055,#72056,#72057,#72058,#72059,#72060,#72061,#72062,#72063,#72064,#72065,
#72066,#72067,#72068,#72069,#72070,#72071,#72072,#72073,#72074,#72075,#72076,
#72077,#72078,#72079,#72080,#72081,#72082,#72083,#72084,#72085,#72086,#72087,
#72088,#72089,#72090,#72091,#72092,#72093,#72094,#72095,#72096,#72097,#72098,
#72099,#72100,#72101,#72102,#72103,#72104,#72105,#72106,#72107,#72108,#72109,
#72110,#72111,#72112,#72113,#72114,#72115,#72116,#72117,#72118,#72119,#72120,
#72121,#72122,#72123,#72124,#72125,#72126,#72127,#72128,#72129,#72130,#72131,
#72132,#72133,#72134,#72135,#72136,#72137,#72138,#72139,#72140,#72141,#72142,
#72143,#72144,#72145,#72146,#72147,#72148,#72149,#72150,#72151,#72152,#72153,
#72154,#72155,#72156,#72157,#72158,#72159,#72160,#72161,#72162,#72163,#72164,
#72165,#72166,#72167,#72168,#72169,#72170,#72171,#72172,#72173,#72174,#72175,
#72176,#72177,#72178,#72179,#72180,#72181,#72182,#72183,#72184,#72185,#72186,
#72187,#72188,#72189,#72190,#72191,#72192,#72193,#72194,#72195,#72196,#72197,
#72198,#72199,#72200,#72201,#72202,#72203,#72204,#72205,#72206,#72207,#72208,
#72209,#72210,#72211,#72212,#72213,#72214,#72215,#72216,#72217,#72218,#72219,
#72220,#72221,#72222,#72223,#72224,#72225,#72226,#72227,#72228,#72229,#72230,
#72231,#72232,#72233,#72234,#72235,#72236,#72237,#72238,#72239,#72240,#72241,
#72242,#72243,#72244,#72245,#72246,#72247,#72248,#72249,#72250,#72251,#72252,
#72253,#72254,#72255,#72256,#72257,#72258,#72259,#72260,#72261,#72262,#72263,
#72264,#72265,#72266,#72267,#72268,#72269,#72270,#72271,#72272,#72273,#72274,
#72275,#72276,#72277,#72278,#72279,#72280,#72281,#72282,#72283,#72284,#72285),
(#72286,#72287,#72288,#72289,#72290,#72291,#72292,#72293,#72294,#72295,
#72296,#72297,#72298,#72299,#72300,#72301,#72302,#72303,#72304,#72305,#72306,
#72307,#72308,#72309,#72310,#72311,#72312,#72313,#72314,#72315,#72316,#72317,
#72318,#72319,#72320,#72321,#72322,#72323,#72324,#72325,#72326,#72327,#72328,
#72329,#72330,#72331,#72332,#72333,#72334,#72335,#72336,#72337,#72338,#72339,
#72340,#72341,#72342,#72343,#72344,#72345,#72346,#72347,#72348,#72349,#72350,
#72351,#72352,#72353,#72354,#72355,#72356,#72357,#72358,#72359,#72360,#72361,
#72362,#72363,#72364,#72365,#72366,#72367,#72368,#72369,#72370,#72371,#72372,
#72373,#72374,#72375,#72376,#72377,#72378,#72379,#72380,#72381,#72382,#72383,
#72384,#72385,#72386,#72387,#72388,#72389,#72390,#72391,#72392,#72393,#72394,
#72395,#72396,#72397,#72398,#72399,#72400,#72401,#72402,#72403,#72404,#72405,
#72406,#72407,#72408,#72409,#72410,#72411,#72412,#72413,#72414,#72415,#72416,
#72417,#72418,#72419,#72420,#72421,#72422,#72423,#72424,#72425,#72426,#72427,
#72428,#72429,#72430,#72431,#72432,#72433,#72434,#72435,#72436,#72437,#72438,
#72439,#72440,#72441,#72442,#72443,#72444,#72445,#72446,#72447,#72448,#72449,
#72450,#72451,#72452,#72453,#72454,#72455,#72456,#72457,#72458,#72459,#72460,
#72461,#72462,#72463,#72464,#72465,#72466,#72467,#72468,#72469,#72470,#72471,
#72472,#72473,#72474,#72475,#72476,#72477,#72478,#72479,#72480,#72481,#72482,
#72483,#72484,#72485,#72486,#72487,#72488,#72489,#72490,#72491,#72492,#72493,
#72494,#72495,#72496,#72497,#72498,#72499,#72500,#72501,#72502,#72503,#72504,
#72505,#72506,#72507,#72508,#72509,#72510,#72511,#72512,#72513,#72514,#72515,
#72516,#72517,#72518,#72519,#72520,#72521,#72522,#72523,#72524,#72525,#72526,
#72527,#72528,#72529,#72530,#72531,#72532,#72533,#72534,#72535,#72536,#72537,
#72538,#72539,#72540,#72541,#72542,#72543,#72544,#72545,#72546,#72547,#72548,
#72549,#72550,#72551,#72552,#72553,#72554,#72555,#72556,#72557,#72558,#72559,
#72560,#72561,#72562,#72563,#72564,#72565,#72566,#72567,#72568,#72569,#72570,
#72571,#72572,#72573,#72574,#72575,#72576,#72577,#72578,#72579,#72580,#72581,
#72582,#72583,#72584,#72585,#72586,#72587,#72588,#72589,#72590,#72591,#72592,
#72593,#72594,#72595,#72596,#72597,#72598,#72599,#72600,#72601,#72602,#72603,
#72604,#72605,#72606,#72607,#72608,#72609,#72610,#72611,#72612,#72613,#72614,
#72615,#72616,#72617,#72618,#72619,#72620,#72621,#72622,#72623,#72624,#72625,
#72626,#72627,#72628,#72629,#72630,#72631,#72632,#72633,#72634,#72635,#72636,
#72637,#72638,#72639,#72640,#72641,#72642,#72643,#72644,#72645,#72646,#72647,
#72648,#72649,#72650,#72651,#72652,#72653,#72654,#72655,#72656,#72657,#72658,
#72659,#72660,#72661,#72662,#72663,#72664,#72665,#72666,#72667,#72668,#72669,
#72670,#72671,#72672,#72673,#72674,#72675,#72676,#72677,#72678,#72679,#72680,
#72681,#72682,#72683,#72684,#72685,#72686,#72687,#72688,#72689,#72690,#72691,
#72692,#72693,#72694,#72695,#72696,#72697,#72698,#72699,#72700,#72701,#72702,
#72703,#72704,#72705,#72706,#72707,#72708,#72709,#72710,#72711,#72712,#72713,
#72714,#72715,#72716,#72717,#72718,#72719,#72720,#72721,#72722,#72723,#72724,
#72725,#72726,#72727,#72728,#72729,#72730,#72731,#72732,#72733,#72734,#72735,
#72736,#72737,#72738,#72739,#72740,#72741,#72742,#72743,#72744,#72745,#72746,
#72747,#72748,#72749,#72750,#72751,#72752,#72753,#72754,#72755,#72756,#72757,
#72758,#72759,#72760,#72761,#72762,#72763,#72764,#72765,#72766,#72767,#72768,
#72769,#72770,#72771,#72772,#72773,#72774,#72775,#72776,#72777,#72778,#72779,
#72780,#72781,#72782,#72783,#72784,#72785,#72786,#72787,#72788,#72789,#72790,
#72791,#72792,#72793,#72794,#72795,#72796,#72797,#72798,#72799,#72800,#72801,
#72802,#72803,#72804,#72805,#72806,#72807,#72808,#72809,#72810,#72811,#72812,
#72813,#72814,#72815,#72816,#72817,#72818),(#72819,#72820,#72821,#72822,
#72823,#72824,#72825,#72826,#72827,#72828,#72829,#72830,#72831,#72832,#72833,
#72834,#72835,#72836,#72837,#72838,#72839,#72840,#72841,#72842,#72843,#72844,
#72845,#72846,#72847,#72848,#72849,#72850,#72851,#72852,#72853,#72854,#72855,
#72856,#72857,#72858,#72859,#72860,#72861,#72862,#72863,#72864,#72865,#72866,
#72867,#72868,#72869,#72870,#72871,#72872,#72873,#72874,#72875,#72876,#72877,
#72878,#72879,#72880,#72881,#72882,#72883,#72884,#72885,#72886,#72887,#72888,
#72889,#72890,#72891,#72892,#72893,#72894,#72895,#72896,#72897,#72898,#72899,
#72900,#72901,#72902,#72903,#72904,#72905,#72906,#72907,#72908,#72909,#72910,
#72911,#72912,#72913,#72914,#72915,#72916,#72917,#72918,#72919,#72920,#72921,
#72922,#72923,#72924,#72925,#72926,#72927,#72928,#72929,#72930,#72931,#72932,
#72933,#72934,#72935,#72936,#72937,#72938,#72939,#72940,#72941,#72942,#72943,
#72944,#72945,#72946,#72947,#72948,#72949,#72950,#72951,#72952,#72953,#72954,
#72955,#72956,#72957,#72958,#72959,#72960,#72961,#72962,#72963,#72964,#72965,
#72966,#72967,#72968,#72969,#72970,#72971,#72972,#72973,#72974,#72975,#72976,
#72977,#72978,#72979,#72980,#72981,#72982,#72983,#72984,#72985,#72986,#72987,
#72988,#72989,#72990,#72991,#72992,#72993,#72994,#72995,#72996,#72997,#72998,
#72999,#73000,#73001,#73002,#73003,#73004,#73005,#73006,#73007,#73008,#73009,
#73010,#73011,#73012,#73013,#73014,#73015,#73016,#73017,#73018,#73019,#73020,
#73021,#73022,#73023,#73024,#73025,#73026,#73027,#73028,#73029,#73030,#73031,
#73032,#73033,#73034,#73035,#73036,#73037,#73038,#73039,#73040,#73041,#73042,
#73043,#73044,#73045,#73046,#73047,#73048,#73049,#73050,#73051,#73052,#73053,
#73054,#73055,#73056,#73057,#73058,#73059,#73060,#73061,#73062,#73063,#73064,
#73065,#73066,#73067,#73068,#73069,#73070,#73071,#73072,#73073,#73074,#73075,
#73076,#73077,#73078,#73079,#73080,#73081,#73082,#73083,#73084,#73085,#73086,
#73087,#73088,#73089,#73090,#73091,#73092,#73093,#73094,#73095,#73096,#73097,
#73098,#73099,#73100,#73101,#73102,#73103,#73104,#73105,#73106,#73107,#73108,
#73109,#73110,#73111,#73112,#73113,#73114,#73115,#73116,#73117,#73118,#73119,
#73120,#73121,#73122,#73123,#73124,#73125,#73126,#73127,#73128,#73129,#73130,
#73131,#73132,#73133,#73134,#73135,#73136,#73137,#73138,#73139,#73140,#73141,
#73142,#73143,#73144,#73145,#73146,#73147,#73148,#73149,#73150,#73151,#73152,
#73153,#73154,#73155,#73156,#73157,#73158,#73159,#73160,#73161,#73162,#73163,
#73164,#73165,#73166,#73167,#73168,#73169,#73170,#73171,#73172,#73173,#73174,
#73175,#73176,#73177,#73178,#73179,#73180,#73181,#73182,#73183,#73184,#73185,
#73186,#73187,#73188,#73189,#73190,#73191,#73192,#73193,#73194,#73195,#73196,
#73197,#73198,#73199,#73200,#73201,#73202,#73203,#73204,#73205,#73206,#73207,
#73208,#73209,#73210,#73211,#73212,#73213,#73214,#73215,#73216,#73217,#73218,
#73219,#73220,#73221,#73222,#73223,#73224,#73225,#73226,#73227,#73228,#73229,
#73230,#73231,#73232,#73233,#73234,#73235,#73236,#73237,#73238,#73239,#73240,
#73241,#73242,#73243,#73244,#73245,#73246,#73247,#73248,#73249,#73250,#73251,
#73252,#73253,#73254,#73255,#73256,#73257,#73258,#73259,#73260,#73261,#73262,
#73263,#73264,#73265,#73266,#73267,#73268,#73269,#73270,#73271,#73272,#73273,
#73274,#73275,#73276,#73277,#73278,#73279,#73280,#73281,#73282,#73283,#73284,
#73285,#73286,#73287,#73288,#73289,#73290,#73291,#73292,#73293,#73294,#73295,
#73296,#73297,#73298,#73299,#73300,#73301,#73302,#73303,#73304,#73305,#73306,
#73307,#73308,#73309,#73310,#73311,#73312,#73313,#73314,#73315,#73316,#73317,
#73318,#73319,#73320,#73321,#73322,#73323,#73324,#73325,#73326,#73327,#73328,
#73329,#73330,#73331,#73332,#73333,#73334,#73335,#73336,#73337,#73338,#73339,
#73340,#73341,#73342,#73343,#73344,#73345,#73346,#73347,#73348,#73349,#73350,
#73351),(#73352,#73353,#73354,#73355,#73356,#73357,#73358,#73359,#73360,
#73361,#73362,#73363,#73364,#73365,#73366,#73367,#73368,#73369,#73370,#73371,
#73372,#73373,#73374,#73375,#73376,#73377,#73378,#73379,#73380,#73381,#73382,
#73383,#73384,#73385,#73386,#73387,#73388,#73389,#73390,#73391,#73392,#73393,
#73394,#73395,#73396,#73397,#73398,#73399,#73400,#73401,#73402,#73403,#73404,
#73405,#73406,#73407,#73408,#73409,#73410,#73411,#73412,#73413,#73414,#73415,
#73416,#73417,#73418,#73419,#73420,#73421,#73422,#73423,#73424,#73425,#73426,
#73427,#73428,#73429,#73430,#73431,#73432,#73433,#73434,#73435,#73436,#73437,
#73438,#73439,#73440,#73441,#73442,#73443,#73444,#73445,#73446,#73447,#73448,
#73449,#73450,#73451,#73452,#73453,#73454,#73455,#73456,#73457,#73458,#73459,
#73460,#73461,#73462,#73463,#73464,#73465,#73466,#73467,#73468,#73469,#73470,
#73471,#73472,#73473,#73474,#73475,#73476,#73477,#73478,#73479,#73480,#73481,
#73482,#73483,#73484,#73485,#73486,#73487,#73488,#73489,#73490,#73491,#73492,
#73493,#73494,#73495,#73496,#73497,#73498,#73499,#73500,#73501,#73502,#73503,
#73504,#73505,#73506,#73507,#73508,#73509,#73510,#73511,#73512,#73513,#73514,
#73515,#73516,#73517,#73518,#73519,#73520,#73521,#73522,#73523,#73524,#73525,
#73526,#73527,#73528,#73529,#73530,#73531,#73532,#73533,#73534,#73535,#73536,
#73537,#73538,#73539,#73540,#73541,#73542,#73543,#73544,#73545,#73546,#73547,
#73548,#73549,#73550,#73551,#73552,#73553,#73554,#73555,#73556,#73557,#73558,
#73559,#73560,#73561,#73562,#73563,#73564,#73565,#73566,#73567,#73568,#73569,
#73570,#73571,#73572,#73573,#73574,#73575,#73576,#73577,#73578,#73579,#73580,
#73581,#73582,#73583,#73584,#73585,#73586,#73587,#73588,#73589,#73590,#73591,
#73592,#73593,#73594,#73595,#73596,#73597,#73598,#73599,#73600,#73601,#73602,
#73603,#73604,#73605,#73606,#73607,#73608,#73609,#73610,#73611,#73612,#73613,
#73614,#73615,#73616,#73617,#73618,#73619,#73620,#73621,#73622,#73623,#73624,
#73625,#73626,#73627,#73628,#73629,#73630,#73631,#73632,#73633,#73634,#73635,
#73636,#73637,#73638,#73639,#73640,#73641,#73642,#73643,#73644,#73645,#73646,
#73647,#73648,#73649,#73650,#73651,#73652,#73653,#73654,#73655,#73656,#73657,
#73658,#73659,#73660,#73661,#73662,#73663,#73664,#73665,#73666,#73667,#73668,
#73669,#73670,#73671,#73672,#73673,#73674,#73675,#73676,#73677,#73678,#73679,
#73680,#73681,#73682,#73683,#73684,#73685,#73686,#73687,#73688,#73689,#73690,
#73691,#73692,#73693,#73694,#73695,#73696,#73697,#73698,#73699,#73700,#73701,
#73702,#73703,#73704,#73705,#73706,#73707,#73708,#73709,#73710,#73711,#73712,
#73713,#73714,#73715,#73716,#73717,#73718,#73719,#73720,#73721,#73722,#73723,
#73724,#73725,#73726,#73727,#73728,#73729,#73730,#73731,#73732,#73733,#73734,
#73735,#73736,#73737,#73738,#73739,#73740,#73741,#73742,#73743,#73744,#73745,
#73746,#73747,#73748,#73749,#73750,#73751,#73752,#73753,#73754,#73755,#73756,
#73757,#73758,#73759,#73760,#73761,#73762,#73763,#73764,#73765,#73766,#73767,
#73768,#73769,#73770,#73771,#73772,#73773,#73774,#73775,#73776,#73777,#73778,
#73779,#73780,#73781,#73782,#73783,#73784,#73785,#73786,#73787,#73788,#73789,
#73790,#73791,#73792,#73793,#73794,#73795,#73796,#73797,#73798,#73799,#73800,
#73801,#73802,#73803,#73804,#73805,#73806,#73807,#73808,#73809,#73810,#73811,
#73812,#73813,#73814,#73815,#73816,#73817,#73818,#73819,#73820,#73821,#73822,
#73823,#73824,#73825,#73826,#73827,#73828,#73829,#73830,#73831,#73832,#73833,
#73834,#73835,#73836,#73837,#73838,#73839,#73840,#73841,#73842,#73843,#73844,
#73845,#73846,#73847,#73848,#73849,#73850,#73851,#73852,#73853,#73854,#73855,
#73856,#73857,#73858,#73859,#73860,#73861,#73862,#73863,#73864,#73865,#73866,
#73867,#73868,#73869,#73870,#73871,#73872,#73873,#73874,#73875,#73876,#73877,
#73878,#73879,#73880,#73881,#73882,#73883,#73884)),.UNSPECIFIED.,.F.,.F.,
 .F.,(4,4),(4,1,1,1,1,1,1,1,1,1,1,1,1,1,1,1,1,1,1,1,1,1,1,1,1,1,1,1,1,1,
1,1,1,1,1,1,1,1,1,1,1,1,1,1,1,1,1,1,1,1,1,1,1,1,1,1,1,1,1,1,1,1,1,1,1,1,
1,1,1,1,1,1,1,1,1,1,1,1,1,1,1,1,1,1,1,1,1,1,1,1,1,1,1,1,1,1,1,1,1,1,1,1,
1,1,1,1,1,1,1,1,1,1,1,1,1,1,1,1,1,1,1,1,1,1,1,1,1,1,1,1,1,1,1,1,1,1,1,1,
1,1,1,1,1,1,1,1,1,1,1,1,1,1,1,1,1,1,1,1,1,1,1,1,1,1,1,1,1,1,1,1,1,1,1,1,
1,1,1,1,1,1,1,1,1,1,1,1,1,1,1,1,1,1,1,1,1,1,1,1,1,1,1,1,1,1,1,1,1,1,1,1,
1,1,1,1,1,1,1,1,1,1,1,1,1,1,1,1,1,1,1,1,1,1,1,1,1,1,1,1,1,1,1,1,1,1,1,1,
1,1,1,1,1,1,1,1,1,1,1,1,1,1,1,1,1,1,1,1,1,1,1,1,1,1,1,1,1,1,1,1,1,1,1,1,
1,1,1,1,1,1,1,1,1,1,1,1,1,1,1,1,1,1,1,1,1,1,1,1,1,1,1,1,1,1,1,1,1,1,1,1,
1,1,1,1,1,1,1,1,1,1,1,1,1,1,1,1,1,1,1,1,1,1,1,1,1,1,1,1,1,1,1,1,1,1,1,1,
1,1,1,1,1,1,1,1,1,1,1,1,1,1,1,1,1,1,1,1,1,1,1,1,1,1,1,1,1,1,1,1,1,1,1,1,
1,1,1,1,1,1,1,1,1,1,1,1,1,1,1,1,1,1,1,1,1,1,1,1,1,1,1,1,1,1,1,1,1,1,1,1,
1,1,1,1,1,1,1,1,1,1,1,1,1,1,1,1,1,1,1,1,1,1,1,1,1,1,1,1,1,1,1,1,1,1,1,1,
1,1,1,1,1,1,1,1,1,1,1,1,1,1,1,1,1,1,1,1,1,1,1,1,1,1,1,1,1,1,1,1,1,1,1,1,
1,1,1,1,1,1,1,1,1,1,1,1,1,1,1,1,1,1,1,1,1,1,1,1,1,1,1,1,1,1,1,1,4),(-0.000330931146184842,
0.0826790177557676),(11.6145478157386,12.6149288832288,13.6146435387017,
14.6143581941745,15.6140728496473,16.6137875051202,17.613502160593,18.6132168160658,
19.6129314715387,20.6126461270115,21.6123607824843,22.6120754379572,23.61179009343,
24.6115047489028,25.6112194043757,26.6109340598485,27.6106487153213,28.6103633707942,
29.610078026267,30.6097926817398,31.6095073372127,32.6092219926855,33.6089366481583,
34.6086513036311,35.608365959104,36.6080806145768,37.6077952700496,38.6075099255225,
39.6072245809953,40.6069392364681,41.606653891941,42.6063685474138,43.6060832028866,
44.6057978583595,45.6055125138323,46.6052271693051,47.604941824778,48.6046564802508,
49.6043711357236,50.6040857911965,51.6038004466693,52.6035151021421,53.603229757615,
54.6029444130878,55.6026590685606,56.6023737240335,57.6020883795063,58.6018030349791,
59.6015176904519,60.6012323459248,61.6009470013976,62.6006616568704,63.6003763123433,
64.6000909678161,65.5998056232889,66.5995202787618,67.5992349342346,68.5989495897074,
69.5986642451803,70.5983789006531,71.5980935561259,72.5978082115988,73.5975228670716,
74.5972375225444,75.5969521780173,76.5966668334901,77.5963814889629,78.5960961444358,
79.5958107999086,80.5955254553814,81.5952401108542,82.5949547663271,83.5946694217999,
84.5943840772727,85.5940987327456,86.5938133882184,87.5935280436913,88.5932426991641,
89.5929573546369,90.5926720101097,91.5923866655826,92.5921013210554,93.5918159765282,
94.5915306320011,95.5912452874739,96.5909599429467,97.5906745984196,98.5903892538924,
99.5901039093652,100.589818564838,101.589533220311,102.589247875784,103.588962531257,
104.588677186729,105.588391842202,106.588106497675,107.587821153148,108.587535808621,
109.587250464094,110.586965119566,111.586679775039,112.586394430512,113.586109085985,
114.585823741458,115.585538396931,116.585253052403,117.584967707876,118.584682363349,
119.584397018822,120.584111674295,121.583826329768,122.58354098524,123.583255640713,
124.582970296186,125.582684951659,126.582399607132,127.582114262605,128.581828918077,
129.58154357355,130.581258229023,131.580972884496,132.580687539969,133.580402195442,
134.580116850914,135.579831506387,136.57954616186,137.579260817333,138.578975472806,
139.578690128279,140.578404783751,141.578119439224,142.577834094697,143.57754875017,
144.577263405643,145.576978061116,146.576692716588,147.576407372061,148.576122027534,
149.575836683007,150.57555133848,151.575265993952,152.574980649425,153.574695304898,
154.574409960371,155.574124615844,156.573839271317,157.573553926789,158.573268582262,
159.572983237735,160.572697893208,161.572412548681,162.572127204154,163.571841859626,
164.571556515099,165.571271170572,166.570985826045,167.570700481518,168.570415136991,
169.570129792463,170.569844447936,171.569559103409,172.569273758882,173.568988414355,
174.568703069828,175.5684177253,176.568132380773,177.567847036246,178.567561691719,
179.567276347192,180.566991002665,181.566705658137,182.56642031361,183.566134969083,
184.565849624556,185.565564280029,186.565278935502,187.564993590974,188.564708246447,
189.56442290192,190.564137557393,191.563852212866,192.563566868339,193.563281523811,
194.562996179284,195.562710834757,196.56242549023,197.562140145703,198.561854801176,
199.561569456648,200.561284112121,201.560998767594,202.560713423067,203.56042807854,
204.560142734013,205.559857389485,206.559572044958,207.559286700431,208.559001355904,
209.558716011377,210.55843066685,211.558145322322,212.557859977795,213.557574633268,
214.557289288741,215.557003944214,216.556718599687,217.556433255159,218.556147910632,
219.555862566105,220.555577221578,221.555291877051,222.555006532524,223.554721187996,
224.554435843469,225.554150498942,226.553865154415,227.553579809888,228.553294465361,
229.553009120833,230.552723776306,231.552438431779,232.552153087252,233.551867742725,
234.551582398198,235.55129705367,236.551011709143,237.550726364616,238.550441020089,
239.550155675562,240.549870331035,241.549584986507,242.54929964198,243.549014297453,
244.548728952926,245.548443608399,246.548158263872,247.547872919344,248.547587574817,
249.54730223029,250.547016885763,251.546731541236,252.546446196709,253.546160852181,
254.545875507654,255.545590163127,256.5453048186,257.545019474073,258.544734129546,
259.544448785018,260.544163440491,261.543878095964,262.543592751437,263.54330740691,
264.543022062382,265.542736717855,266.542451373328,267.542166028801,268.541880684274,
269.541595339747,270.541309995219,271.541024650692,272.540739306165,273.540453961638,
274.540168617111,275.539883272584,276.539597928056,277.539312583529,278.539027239002,
279.538741894475,280.538456549948,281.538171205421,282.537885860893,283.537600516366,
284.537315171839,285.537029827312,286.536744482785,287.536459138258,288.53617379373,
289.535888449203,290.535603104676,291.535317760149,292.535032415622,293.534747071095,
294.534461726567,295.53417638204,296.533891037513,297.533605692986,298.533320348459,
299.533035003932,300.532749659404,301.532464314877,302.53217897035,303.531893625823,
304.531608281296,305.531322936769,306.531037592241,307.530752247714,308.530466903187,
309.53018155866,310.529896214133,311.529610869606,312.529325525078,313.529040180551,
314.528754836024,315.528469491497,316.52818414697,317.527898802443,318.527613457915,
319.527328113388,320.527042768861,321.526757424334,322.526472079807,323.52618673528,
324.525901390752,325.525616046225,326.525330701698,327.525045357171,328.524760012644,
329.524474668117,330.524189323589,331.523903979062,332.523618634535,333.523333290008,
334.523047945481,335.522762600954,336.522477256426,337.522191911899,338.521906567372,
339.521621222845,340.521335878318,341.521050533791,342.520765189263,343.520479844736,
344.520194500209,345.519909155682,346.519623811155,347.519338466628,348.5190531221,
349.518767777573,350.518482433046,351.518197088519,352.517911743992,353.517626399465,
354.517341054937,355.51705571041,356.516770365883,357.516485021356,358.516199676829,
359.515914332302,360.515628987774,361.515343643247,362.51505829872,363.514772954193,
364.514487609666,365.514202265139,366.513916920611,367.513631576084,368.513346231557,
369.51306088703,370.512775542503,371.512490197976,372.512204853448,373.511919508921,
374.511634164394,375.511348819867,376.51106347534,377.510778130813,378.510492786285,
379.510207441758,380.509922097231,381.509636752704,382.509351408177,383.509066063649,
384.508780719122,385.508495374595,386.508210030068,387.507924685541,388.507639341014,
389.507353996486,390.507068651959,391.506783307432,392.506497962905,393.506212618378,
394.505927273851,395.505641929323,396.505356584796,397.505071240269,398.504785895742,
399.504500551215,400.504215206688,401.50392986216,402.503644517633,403.503359173106,
404.503073828579,405.502788484052,406.502503139525,407.502217794997,408.50193245047,
409.501647105943,410.501361761416,411.501076416889,412.500791072362,413.500505727834,
414.500220383307,415.49993503878,416.499649694253,417.499364349726,418.499079005199,
419.498793660671,420.498508316144,421.498222971617,422.49793762709,423.497652282563,
424.497366938036,425.497081593508,426.496796248981,427.496510904454,428.496225559927,
429.4959402154,430.495654870873,431.495369526345,432.495084181818,433.494798837291,
434.494513492764,435.494228148237,436.49394280371,437.493657459182,438.493372114655,
439.493086770128,440.492801425601,441.492516081074,442.492230736547,443.491945392019,
444.491660047492,445.491374702965,446.491089358438,447.490804013911,448.490518669384,
449.490233324856,450.489947980329,451.489662635802,452.489377291275,453.489091946748,
454.488806602221,455.488521257693,456.488235913166,457.487950568639,458.487665224112,
459.487379879585,460.487094535058,461.48680919053,462.486523846003,463.486238501476,
464.485953156949,465.485667812422,466.485382467895,467.485097123367,468.48481177884,
469.484526434313,470.484241089786,471.483955745259,472.483670400732,473.483385056204,
474.483099711677,475.48281436715,476.482529022623,477.482243678096,478.481958333569,
479.481672989041,480.481387644514,481.481102299987,482.48081695546,483.480531610933,
484.480246266406,485.479960921878,486.479675577351,487.479390232824,488.479104888297,
489.47881954377,490.478534199243,491.478248854715,492.477963510188,493.477678165661,
494.477392821134,495.477107476607,496.47682213208,497.476536787552,498.476251443025,
499.475966098498,500.475680753971,501.475395409444,502.475110064917,503.474824720389,
504.474539375862,505.474254031335,506.473968686808,507.473683342281,508.473397997753,
509.473112653226,510.472827308699,511.472541964172,512.472256619645,513.471971275118,
514.471685930591,515.471400586063,516.471115241536,517.470829897009,518.470544552482,
519.470259207955,520.469973863428,521.4696885189,522.469403174373,523.469117829846,
524.468832485319,525.468547140792,526.468261796265,527.467976451737,528.46769110721,
529.467405762683,530.467120418156,531.466835073629,532.466549729102,533.466264384574,
534.465979040047,535.46569369552,536.465408350993,537.465123006466,538.464837661939,
539.464552317411,540.464266972884,541.463981628357),.UNSPECIFIED.);
#49=B_SPLINE_CURVE_WITH_KNOTS('',3,(#6229,#6230,#6231,#6232,#6233,#6234,
#6235,#6236,#6237,#6238,#6239,#6240,#6241,#6242,#6243,#6244,#6245,#6246,
#6247,#6248,#6249,#6250,#6251,#6252,#6253,#6254,#6255,#6256,#6257,#6258,
#6259,#6260,#6261,#6262,#6263,#6264,#6265,#6266,#6267,#6268,#6269,#6270,
#6271,#6272,#6273,#6274,#6275,#6276,#6277,#6278,#6279,#6280,#6281,#6282,
#6283,#6284,#6285,#6286,#6287,#6288,#6289,#6290,#6291,#6292,#6293,#6294,
#6295,#6296,#6297,#6298,#6299,#6300,#6301,#6302,#6303,#6304,#6305,#6306,
#6307,#6308,#6309,#6310,#6311,#6312,#6313,#6314,#6315,#6316,#6317,#6318,
#6319,#6320,#6321,#6322,#6323,#6324,#6325,#6326,#6327,#6328,#6329,#6330,
#6331,#6332,#6333,#6334,#6335,#6336,#6337,#6338,#6339,#6340),
 .UNSPECIFIED.,.F.,.F.,(4,3,3,3,3,3,3,3,3,3,3,3,3,3,3,3,3,3,3,3,3,3,3,3,
3,3,3,3,3,3,3,3,3,3,3,3,3,4),(10.3762600297592,10.4685665931634,10.5607519230172,
10.6548925221748,10.7469246166194,10.8389288274898,10.9309307648174,11.0266672526824,
11.1187945753552,11.21098417842,11.3033079207642,11.3138767162776,11.4071165017747,
11.5002333969254,11.5932547895379,11.6862120629539,11.7791363956122,11.8720524013631,
11.9649846805265,12.0580178810066,12.1511041087062,12.2443458788881,12.3135913717504,
12.4065309273335,12.4993426448501,12.5920543448581,12.6846963965842,12.7773022111874,
12.8698967723451,12.9625050478778,13.0552122586236,13.1479708846286,13.2408858091675,
13.3133060272232,13.4063880812434,13.4993598882143,13.5922296797452,13.6621187583616),
 .UNSPECIFIED.);
#50=B_SPLINE_CURVE_WITH_KNOTS('',3,(#6343,#6344,#6345,#6346,#6347,#6348,
#6349,#6350,#6351,#6352,#6353,#6354,#6355,#6356,#6357,#6358,#6359,#6360,
#6361,#6362,#6363,#6364,#6365,#6366,#6367,#6368,#6369,#6370,#6371,#6372,
#6373,#6374,#6375,#6376,#6377,#6378,#6379,#6380,#6381,#6382,#6383,#6384,
#6385,#6386,#6387,#6388,#6389,#6390,#6391,#6392,#6393,#6394,#6395,#6396,
#6397,#6398,#6399,#6400,#6401,#6402,#6403,#6404,#6405,#6406,#6407,#6408,
#6409,#6410,#6411,#6412),.UNSPECIFIED.,.F.,.F.,(4,3,3,3,3,3,3,3,3,3,3,3,
3,3,3,3,3,3,3,3,3,3,3,4),(11.615214227756,11.7104959116212,11.8057232883005,
11.9009184235368,11.9961303776916,12.0913569841311,12.1866182838285,12.2819343459706,
12.3773918355249,12.4729276001673,12.5686320048391,12.6149288832288,12.7070190024734,
12.7989699433795,12.8908105692998,12.9825692112577,13.074284158239,13.1659812591482,
13.2576863409985,13.3494866953367,13.4413348419307,13.5333428212227,13.6146435387017,
13.6618816120544),.UNSPECIFIED.);
#51=B_SPLINE_CURVE_WITH_KNOTS('',3,(#6418,#6419,#6420,#6421,#6422,#6423,
#6424,#6425,#6426,#6427,#6428,#6429,#6430,#6431,#6432,#6433,#6434,#6435,
#6436,#6437,#6438,#6439,#6440,#6441,#6442,#6443,#6444,#6445,#6446,#6447,
#6448,#6449,#6450,#6451,#6452,#6453,#6454,#6455,#6456,#6457,#6458,#6459,
#6460,#6461,#6462,#6463,#6464,#6465,#6466,#6467,#6468,#6469,#6470,#6471,
#6472,#6473,#6474,#6475,#6476,#6477,#6478,#6479,#6480,#6481,#6482,#6483,
#6484,#6485,#6486,#6487,#6488,#6489,#6490,#6491,#6492,#6493,#6494,#6495,
#6496,#6497,#6498,#6499,#6500,#6501,#6502,#6503,#6504,#6505,#6506,#6507,
#6508,#6509,#6510,#6511,#6512,#6513,#6514,#6515,#6516,#6517,#6518,#6519,
#6520,#6521,#6522,#6523,#6524,#6525,#6526,#6527,#6528,#6529,#6530,#6531,
#6532,#6533,#6534,#6535,#6536,#6537,#6538,#6539,#6540,#6541,#6542,#6543,
#6544,#6545,#6546,#6547,#6548,#6549,#6550,#6551,#6552,#6553,#6554,#6555,
#6556,#6557,#6558,#6559,#6560,#6561,#6562,#6563,#6564,#6565,#6566,#6567,
#6568,#6569,#6570,#6571,#6572,#6573,#6574,#6575,#6576,#6577,#6578,#6579,
#6580,#6581,#6582,#6583,#6584,#6585,#6586,#6587,#6588,#6589,#6590,#6591,
#6592,#6593,#6594,#6595,#6596,#6597,#6598,#6599,#6600,#6601,#6602,#6603,
#6604,#6605,#6606,#6607,#6608,#6609,#6610,#6611,#6612,#6613,#6614,#6615,
#6616,#6617,#6618,#6619,#6620,#6621,#6622,#6623,#6624,#6625,#6626,#6627,
#6628,#6629,#6630,#6631,#6632,#6633,#6634,#6635,#6636,#6637,#6638,#6639,
#6640,#6641),.UNSPECIFIED.,.F.,.F.,(4,2,2,2,2,2,2,2,2,2,2,2,2,2,2,2,2,2,
2,2,2,2,2,2,2,2,2,2,2,2,2,2,2,2,2,2,2,2,2,2,2,2,2,2,2,2,2,2,2,2,2,2,2,2,
2,2,2,2,2,2,2,2,2,2,2,2,2,2,2,2,2,2,2,2,2,2,2,2,2,2,2,2,2,2,2,2,2,2,2,2,
2,2,2,2,2,2,2,2,2,2,2,2,2,2,2,2,2,2,2,2,2,4),(-1.37050854120238,-1.33686904903339,
-1.33072403175994,-1.3288424066245,-1.32782554961424,-1.32684093532529,
-1.32565745787055,-1.32438895674942,-1.32241511154026,-1.31870205271146,
-1.28627791863757,-1.19926958768006,-1.16918622785395,-1.16721306646538,
-1.16646094713311,-1.16592393006015,-1.16541214936304,-1.16468441681,-1.16317092933403,
-1.14800714537606,-1.11834817571685,-1.0136951735994,-1.00754311183712,
-1.00566095854807,-1.00464417289918,-1.00373609491063,-1.00258295445742,
-1.00056264173604,-0.998101189694289,-0.993082440173186,-0.979991937626143,
-0.94892155709358,-0.854519963144241,-0.853262234263941,-0.851558616924278,
-0.850783309512972,-0.846170558774688,-0.844061146189821,-0.843287995728194,
-0.842745323028977,-0.842235931456424,-0.841523897978037,-0.840089157684197,
-0.82851852733971,-0.802213413640655,-0.791146689138107,-0.697761319418871,
-0.69575606688349,-0.691947664512984,-0.690830319699865,-0.684432465447507,
-0.682521001318348,-0.681384501819927,-0.680393748831362,-0.679164802063678,
-0.676799969115957,-0.673816631864688,-0.667310530459367,-0.648755647389044,
-0.612459523118121,-0.526346307995641,-0.526230332752949,-0.521572468867822,
-0.520511571556346,-0.519817869748106,-0.519312876766996,-0.518682589921299,
-0.517630001664061,-0.513738110463563,-0.486702008753863,-0.461910725925344,
-0.454196416613347,-0.447518154764842,-0.44163307395454,-0.421390758091795,
-0.378559862049454,-0.376244316775148,-0.372542987023873,-0.370309069712533,
-0.361945413504594,-0.360041423042474,-0.358795075578016,-0.357846978087917,
-0.356902683870432,-0.355246391938894,-0.350322464057847,-0.342892733340551,
-0.32080454515825,-0.277021714141936,-0.20291752202762,-0.198618262379819,
-0.197488127251727,-0.196834009920347,-0.196273762780795,-0.195586586322357,
-0.194270153380627,-0.186184436428434,-0.171723167580107,-0.0703203637749224,
-0.0647305693058463,-0.0591438239231535,-0.0571526928326631,-0.0527632841355329,
-0.039330003794461,-0.0370918086250107,-0.0357589772463339,-0.0347398117165327,
-0.0337993895037417,-0.0327331461366012,-0.0312440460767627,-0.0287420106566131,
-0.000966338742490973),.UNSPECIFIED.);
#52=B_SPLINE_CURVE_WITH_KNOTS('',3,(#6642,#6643,#6644,#6645,#6646,#6647,
#6648,#6649,#6650,#6651,#6652,#6653,#6654,#6655,#6656,#6657,#6658,#6659,
#6660,#6661,#6662,#6663,#6664,#6665,#6666,#6667,#6668,#6669,#6670,#6671,
#6672,#6673,#6674,#6675,#6676,#6677,#6678,#6679,#6680,#6681,#6682,#6683,
#6684,#6685,#6686,#6687,#6688,#6689,#6690,#6691,#6692,#6693,#6694,#6695,
#6696,#6697,#6698,#6699,#6700,#6701,#6702,#6703,#6704,#6705,#6706,#6707,
#6708),.UNSPECIFIED.,.F.,.F.,(4,3,3,3,3,3,3,3,3,3,3,3,3,3,3,3,3,3,3,3,3,
3,4),(13.6621187583616,13.7549005319316,13.8476657797449,13.9404392779984,
14.0335846291728,14.1264999104908,14.2197602965935,14.3130206826961,14.4061140507736,
14.49908173365,14.5919513377176,14.6847535760267,14.7775209326273,14.8702782077547,
14.963050186716,15.0559216401269,15.1488450689533,15.2419240039525,15.3127353381689,
15.4164785260033,15.5199069032915,15.6227703545641,15.7079632677646),
 .UNSPECIFIED.);
#53=B_SPLINE_CURVE_WITH_KNOTS('',3,(#6710,#6711,#6712,#6713,#6714,#6715,
#6716,#6717,#6718,#6719,#6720,#6721,#6722,#6723,#6724,#6725,#6726,#6727,
#6728,#6729,#6730,#6731,#6732,#6733,#6734,#6735,#6736,#6737,#6738,#6739,
#6740,#6741,#6742,#6743,#6744,#6745,#6746,#6747,#6748,#6749,#6750,#6751,
#6752,#6753,#6754,#6755,#6756,#6757,#6758,#6759,#6760,#6761,#6762,#6763,
#6764,#6765,#6766,#6767,#6768,#6769,#6770,#6771,#6772,#6773,#6774,#6775,
#6776,#6777,#6778,#6779),.UNSPECIFIED.,.F.,.F.,(4,3,3,3,3,3,3,3,3,3,3,3,
3,3,3,3,3,3,3,3,3,3,3,4),(13.6618816120544,13.755040813502,13.8480880614116,
13.943871828007,14.0367832476407,14.1296722777591,14.2225635417726,14.3154816579344,
14.4085037791136,14.5015885715,14.5948115027264,14.6143581941745,14.7075979796716,
14.8007148748224,14.8937362674349,14.9866935408508,15.0796178735092,15.1725338792599,
15.2654661584234,15.3584993589035,15.4515855866031,15.544827356785,15.6140728496473,
15.70796326795),.UNSPECIFIED.);
#54=B_SPLINE_CURVE_WITH_KNOTS('',3,(#6780,#6781,#6782,#6783,#6784,#6785,
#6786,#6787,#6788,#6789,#6790,#6791,#6792,#6793,#6794,#6795,#6796,#6797,
#6798,#6799,#6800,#6801,#6802,#6803,#6804,#6805,#6806,#6807,#6808,#6809,
#6810,#6811,#6812,#6813,#6814,#6815,#6816,#6817,#6818,#6819,#6820,#6821,
#6822,#6823,#6824,#6825,#6826,#6827,#6828,#6829,#6830,#6831,#6832,#6833,
#6834,#6835,#6836,#6837,#6838,#6839,#6840,#6841,#6842,#6843,#6844,#6845,
#6846,#6847,#6848,#6849,#6850,#6851,#6852,#6853,#6854,#6855,#6856,#6857,
#6858,#6859,#6860,#6861,#6862,#6863,#6864,#6865,#6866,#6867,#6868,#6869,
#6870,#6871,#6872,#6873,#6874,#6875,#6876,#6877,#6878,#6879,#6880,#6881,
#6882,#6883,#6884,#6885,#6886,#6887,#6888,#6889,#6890,#6891,#6892,#6893,
#6894,#6895,#6896,#6897,#6898,#6899,#6900,#6901,#6902,#6903,#6904,#6905,
#6906,#6907,#6908,#6909,#6910,#6911,#6912,#6913,#6914,#6915,#6916,#6917,
#6918,#6919,#6920,#6921,#6922,#6923,#6924,#6925,#6926,#6927,#6928,#6929,
#6930,#6931,#6932,#6933,#6934,#6935,#6936,#6937,#6938,#6939,#6940,#6941,
#6942,#6943,#6944,#6945,#6946,#6947,#6948,#6949,#6950,#6951,#6952,#6953,
#6954,#6955,#6956,#6957,#6958,#6959,#6960,#6961,#6962,#6963,#6964,#6965,
#6966,#6967,#6968,#6969,#6970,#6971,#6972,#6973,#6974,#6975,#6976,#6977,
#6978,#6979,#6980,#6981,#6982,#6983,#6984,#6985),.UNSPECIFIED.,.F.,.F.,
(4,2,2,2,2,2,2,2,2,2,2,2,2,2,2,2,2,2,2,2,2,2,2,2,2,2,2,2,2,2,2,2,2,2,2,
2,2,2,2,2,2,2,2,2,2,2,2,2,2,2,2,2,2,2,2,2,2,2,2,2,2,2,2,2,2,2,2,2,2,2,2,
2,2,2,2,2,2,2,2,2,2,2,2,2,2,2,2,2,2,2,2,2,2,2,2,2,2,2,2,2,2,2,4),(-4.06088750423127,
-3.98270680377003,-3.94902050874879,-3.93409679396766,-3.93173231106793,
-3.93050319997425,-3.92950573566426,-3.92851018028234,-3.92670761804885,
-3.92112233105714,-3.91621589067004,-3.91231513591603,-3.90979295400919,
-3.90855754571573,-3.90581624275564,-3.89863734561648,-3.80758676832066,
-3.79004338162275,-3.77660679586409,-3.77003879478894,-3.76880560729759,
-3.76825770336036,-3.76771751123279,-3.76717913951976,-3.7664216875051,
-3.76485491606738,-3.74853125028312,-3.74465622348553,-3.71561920182063,
-3.69457362358076,-3.64797354334687,-3.62313993854728,-3.6103993048201,
-3.60811419000323,-3.60689397465597,-3.60588689544302,-3.60486742733792,
-3.60298036921095,-3.59681251006346,-3.49391762777491,-3.46308145032798,
-3.45285932932485,-3.4493084620027,-3.447677660958,-3.44638470406621,-3.44570413703487,
-3.44514324778417,-3.44449194039282,-3.44337540036809,-3.43921909765203,
-3.37821818726799,-3.33515428180871,-3.29388134256588,-3.28737714752424,
-3.2855357866189,-3.28441486424675,-3.28340407126987,-3.28211496037622,
-3.27948937864557,-3.26356391662639,-3.26223176063392,-3.26027790675209,
-3.25718179573601,-3.25516490570098,-3.20437135341289,-3.1551247179711,
-3.13378540525712,-3.12788843578953,-3.12552012774694,-3.12431033772132,
-3.12329856556556,-3.12268249932224,-3.12211950360246,-3.12139626465456,
-3.1202377181613,-3.11424596499402,-3.11201577424126,-3.11011324882386,
-3.05696943428382,-3.00971316395337,-2.97065748142882,-2.96651050500656,
-2.96339939236119,-2.96201884361775,-2.96099595663445,-2.96004672655908,
-2.95875164760135,-2.9561977915361,-2.93537339284446,-2.93245578340497,
-2.8814031397907,-2.82524128965409,-2.80468746681851,-2.80249864285803,
-2.80135655517014,-2.80063314076899,-2.79996306429501,-2.79941399138725,
-2.79884711383219,-2.79779503118521,-2.79433434734377,-2.73746932256422,
-2.69251420336544),.UNSPECIFIED.);
#55=B_SPLINE_CURVE_WITH_KNOTS('',3,(#6990,#6991,#6992,#6993,#6994,#6995,
#6996,#6997,#6998,#6999,#7000,#7001,#7002,#7003,#7004,#7005,#7006,#7007,
#7008,#7009,#7010,#7011,#7012,#7013,#7014,#7015,#7016,#7017,#7018,#7019,
#7020,#7021,#7022,#7023,#7024,#7025,#7026,#7027,#7028,#7029,#7030,#7031,
#7032,#7033,#7034,#7035,#7036,#7037,#7038,#7039,#7040,#7041,#7042,#7043,
#7044,#7045,#7046,#7047,#7048,#7049,#7050,#7051,#7052,#7053,#7054,#7055,
#7056,#7057,#7058,#7059,#7060,#7061,#7062,#7063,#7064,#7065,#7066,#7067,
#7068,#7069,#7070,#7071,#7072,#7073,#7074,#7075,#7076,#7077,#7078,#7079,
#7080,#7081,#7082,#7083,#7084,#7085,#7086,#7087,#7088,#7089,#7090,#7091,
#7092,#7093,#7094,#7095,#7096,#7097,#7098,#7099,#7100,#7101,#7102,#7103,
#7104,#7105,#7106,#7107,#7108,#7109,#7110,#7111,#7112,#7113,#7114,#7115,
#7116,#7117,#7118,#7119,#7120,#7121,#7122,#7123,#7124,#7125,#7126,#7127,
#7128,#7129,#7130,#7131,#7132,#7133,#7134,#7135,#7136,#7137,#7138,#7139,
#7140,#7141,#7142,#7143,#7144,#7145,#7146,#7147,#7148,#7149,#7150,#7151,
#7152,#7153,#7154,#7155,#7156,#7157,#7158,#7159,#7160,#7161,#7162,#7163,
#7164,#7165,#7166,#7167,#7168,#7169,#7170,#7171,#7172,#7173,#7174,#7175,
#7176,#7177,#7178,#7179,#7180,#7181,#7182,#7183,#7184,#7185,#7186,#7187,
#7188,#7189,#7190,#7191,#7192,#7193,#7194,#7195,#7196,#7197,#7198,#7199,
#7200,#7201,#7202,#7203,#7204,#7205,#7206,#7207,#7208,#7209,#7210,#7211,
#7212,#7213,#7214,#7215,#7216,#7217,#7218,#7219,#7220,#7221,#7222,#7223,
#7224,#7225,#7226,#7227,#7228,#7229,#7230,#7231,#7232,#7233,#7234,#7235,
#7236,#7237,#7238,#7239,#7240,#7241,#7242,#7243,#7244,#7245,#7246,#7247,
#7248,#7249,#7250,#7251,#7252,#7253,#7254,#7255,#7256,#7257,#7258,#7259,
#7260,#7261,#7262,#7263,#7264,#7265,#7266,#7267,#7268,#7269,#7270,#7271,
#7272,#7273,#7274,#7275,#7276,#7277,#7278,#7279,#7280,#7281,#7282,#7283,
#7284,#7285,#7286,#7287,#7288,#7289,#7290,#7291,#7292,#7293,#7294,#7295),
 .UNSPECIFIED.,.F.,.F.,(4,2,2,2,2,2,2,2,2,2,2,2,2,2,2,2,2,2,2,2,2,2,2,2,
2,2,2,2,2,2,2,2,2,2,2,2,2,2,2,2,2,2,2,2,2,2,2,2,2,2,2,2,2,2,2,2,2,2,2,2,
2,2,2,2,2,2,2,2,2,2,2,2,2,2,2,2,2,2,2,2,2,2,2,2,2,2,2,2,2,2,2,2,2,2,2,2,
2,2,2,2,2,2,2,2,2,2,2,2,2,2,2,2,2,2,2,2,2,2,2,2,2,2,2,2,2,2,2,2,2,2,2,2,
2,2,2,2,2,2,2,2,2,2,2,2,2,2,2,2,2,2,2,2,4),(-3.4011377333033,-3.36823275924315,
-3.32533821537189,-3.27265437450256,-3.26865604607521,-3.26712639407524,
-3.2660739058206,-3.265043853067,-3.26380381678253,-3.26071400730694,-3.23220829558781,
-3.15095176434001,-3.12670411423292,-3.11475843323702,-3.1095136941263,
-3.10734121394413,-3.10620484611436,-3.10548345364643,-3.10481468339031,
-3.10429026756391,-3.10372889855353,-3.10270445685079,-3.09947053752061,
-3.04465964380899,-2.99454811141961,-2.96197290683038,-2.94728522867798,
-2.94491569875493,-2.94367932266106,-2.94267361224274,-2.94166786225046,
-2.93984131905043,-2.93414075334494,-2.93199195630718,-2.93160372108128,
-2.92851576866371,-2.92529794307563,-2.92322211794468,-2.9214532133722,
-2.91788094095474,-2.91376041243119,-2.83684897212456,-2.78518882672316,
-2.78368387208337,-2.7828098117944,-2.78203145617703,-2.78146702604608,
-2.78094044604795,-2.78022822524511,-2.77884177618253,-2.76833995864156,
-2.76641873406103,-2.76596119188914,-2.76472792758538,-2.76410563134707,
-2.69643998339443,-2.66153335048973,-2.63677116201241,-2.62412549906813,
-2.62184887722492,-2.62063216696009,-2.619724946571,-2.61858923324097,-2.61668153574633,
-2.61031680908487,-2.60636053074062,-2.60453904677733,-2.60198303071082,
-2.60152037623093,-2.59792402391556,-2.59672914490128,-2.59521926603126,
-2.58879152634298,-2.49809378839896,-2.47777153010542,-2.46279548833425,
-2.46097426568099,-2.45997357685033,-2.45930908792335,-2.45868089262802,
-2.45813218770527,-2.45743330613678,-2.45635570409385,-2.45148937546274,
-2.36098632184745,-2.33635010651568,-2.3128519701406,-2.30092112236153,
-2.29868134046041,-2.29747248323213,-2.29647745532457,-2.29545743433319,
-2.29356051817955,-2.28728834135306,-2.18099183893918,-2.16118010117057,
-2.14190503157979,-2.13721228745901,-2.1360907578785,-2.13544529991579,
-2.13488394985283,-2.13418459046293,-2.1331055409029,-2.12822180998189,
-2.032103268204,-1.9795721898221,-1.97611649381286,-1.97478101856965,-1.97382020337401,
-1.97280157186733,-1.97145534867438,-1.9685365723614,-1.92259296791803,
-1.87159625811684,-1.83509096392933,-1.83051685145161,-1.82919163820721,
-1.82886588656804,-1.82786851269959,-1.82748621335548,-1.82671557103509,
-1.81485654514485,-1.81342044189802,-1.8126954739005,-1.81216559767254,
-1.81159218325346,-1.81080431591203,-1.80896805578428,-1.80646730613653,
-1.71769871049646,-1.65712461093832,-1.65320117553788,-1.65179181790613,
-1.65081095645836,-1.6498204432176,-1.648568924652,-1.64720618779517,-1.64500858022436,
-1.64070728726306,-1.59914549485817,-1.54797600162877,-1.50528006205352,
-1.50276683936719,-1.49171924381045,-1.49017615949073,-1.48943945626034,
-1.48887237287596,-1.48825567194553,-1.48726262420503,-1.48394832870727,
-1.46329367104304,-1.44475410509111,-1.37050854120238),.UNSPECIFIED.);
#56=B_SPLINE_CURVE_WITH_KNOTS('',3,(#7296,#7297,#7298,#7299,#7300,#7301,
#7302,#7303,#7304,#7305,#7306,#7307,#7308,#7309,#7310,#7311,#7312,#7313,
#7314,#7315,#7316,#7317,#7318,#7319,#7320,#7321,#7322,#7323,#7324,#7325,
#7326,#7327,#7328,#7329,#7330,#7331,#7332,#7333,#7334,#7335,#7336,#7337,
#7338,#7339,#7340,#7341,#7342,#7343,#7344,#7345,#7346,#7347,#7348,#7349,
#7350,#7351,#7352,#7353,#7354,#7355,#7356,#7357,#7358,#7359,#7360,#7361,
#7362,#7363,#7364,#7365,#7366,#7367,#7368,#7369,#7370,#7371,#7372,#7373,
#7374,#7375,#7376,#7377,#7378,#7379,#7380,#7381,#7382,#7383,#7384,#7385,
#7386,#7387,#7388,#7389,#7390,#7391,#7392,#7393,#7394,#7395,#7396,#7397,
#7398,#7399,#7400,#7401,#7402,#7403,#7404,#7405,#7406,#7407,#7408,#7409,
#7410,#7411,#7412,#7413,#7414,#7415,#7416,#7417,#7418,#7419,#7420,#7421,
#7422,#7423,#7424,#7425,#7426,#7427,#7428,#7429,#7430,#7431,#7432,#7433,
#7434,#7435,#7436,#7437,#7438,#7439,#7440,#7441,#7442,#7443,#7444,#7445,
#7446,#7447,#7448,#7449,#7450,#7451,#7452,#7453,#7454,#7455,#7456,#7457,
#7458,#7459,#7460,#7461,#7462,#7463,#7464,#7465,#7466,#7467,#7468,#7469,
#7470,#7471,#7472,#7473,#7474,#7475,#7476,#7477,#7478,#7479,#7480,#7481,
#7482,#7483,#7484,#7485,#7486,#7487,#7488,#7489,#7490,#7491,#7492,#7493,
#7494,#7495,#7496,#7497,#7498,#7499,#7500,#7501,#7502,#7503,#7504,#7505,
#7506,#7507,#7508,#7509,#7510,#7511,#7512,#7513,#7514,#7515,#7516,#7517,
#7518,#7519,#7520,#7521,#7522,#7523,#7524,#7525,#7526,#7527,#7528,#7529,
#7530,#7531,#7532,#7533,#7534,#7535,#7536,#7537,#7538,#7539,#7540,#7541,
#7542,#7543,#7544,#7545,#7546,#7547,#7548,#7549,#7550,#7551,#7552,#7553,
#7554,#7555,#7556,#7557,#7558,#7559,#7560,#7561,#7562,#7563),
 .UNSPECIFIED.,.F.,.F.,(4,2,2,2,2,2,2,2,2,2,2,2,2,2,2,2,2,2,2,2,2,2,2,2,
2,2,2,2,2,2,2,2,2,2,2,2,2,2,2,2,2,2,2,2,2,2,2,2,2,2,2,2,2,2,2,2,2,2,2,2,
2,2,2,2,2,2,2,2,2,2,2,2,2,2,2,2,2,2,2,2,2,2,2,2,2,2,2,2,2,2,2,2,2,2,2,2,
2,2,2,2,2,2,2,2,2,2,2,2,2,2,2,2,2,2,2,2,2,2,2,2,2,2,2,2,2,2,2,2,2,2,2,2,
2,4),(-2.69251420336544,-2.68743982535714,-2.65670177515205,-2.64243281012259,
-2.64008073513957,-2.63884792231432,-2.63784229275467,-2.63683426427094,
-2.63499691828289,-2.62921290210747,-2.51143796312435,-2.48004853099937,
-2.47865904349976,-2.47783210181189,-2.47708786259477,-2.47652916151592,
-2.47599386585528,-2.47524827367568,-2.47331619898672,-2.44599466435854,
-2.35668072882398,-2.33189655382166,-2.31921224504848,-2.31693399151984,
-2.31571706237886,-2.3148099609339,-2.31381865280317,-2.3120635098971,-2.30689736605355,
-2.22623717162586,-2.18360411974992,-2.16439293879996,-2.15594739736146,
-2.1546152455268,-2.15392442368147,-2.15336391139615,-2.15271262869491,
-2.15159371303526,-2.14740359044218,-2.07653151215772,-2.0314321842155,
-2.01934157870124,-2.01594347965038,-2.01286236046132,-1.99679998770164,
-1.99416828925841,-1.99287827098515,-1.99186772900896,-1.99074807308968,
-1.98891104724204,-1.98244468198175,-1.94156700420968,-1.89078621850982,
-1.83588688648386,-1.83251607524864,-1.83147484998298,-1.83091017756209,
-1.83040554070078,-1.82973706651059,-1.8285100164995,-1.82224745656665,
-1.80971373122685,-1.78612899253336,-1.67856948429592,-1.67242843821675,
-1.67054751116332,-1.66953091806029,-1.66852640434665,-1.66733340638653,
-1.6651348378526,-1.66240542810702,-1.60674448273095,-1.52135221251814,
-1.51027509585722,-1.50873099538414,-1.50799415273625,-1.50742714350185,
-1.50681077345624,-1.50581859792568,-1.50251024972305,-1.48191202369889,
-1.46051674485748,-1.35552683343781,-1.34934410262455,-1.34745832000521,
-1.34644082583539,-1.34544611770702,-1.34425915877244,-1.3420869824649,
-1.33939755051221,-1.28717929727067,-1.191452680538,-1.18653362244472,-1.18545204534978,
-1.18475205439321,-1.18419087652432,-1.18354637425512,-1.18242834828442,
-1.1777755789512,-1.15443954878669,-1.10891751165469,-1.07967579614171,
-1.02894701027745,-1.02551165061383,-1.02417976765711,-1.02322008538327,
-1.02220131377168,-1.02087964575332,-1.01806464060844,-1.01436656814974,
-1.00568249936415,-0.985107469143868,-0.935354203012806,-0.875932703915884,
-0.864292370535118,-0.862864123902574,-0.862141248974212,-0.861612002916771,
-0.861038348984915,-0.860248572322031,-0.85840077336365,-0.810428042730951,
-0.740767073980838,-0.705665428428054,-0.70247901695341,-0.701189372013492,
-0.700240680139341,-0.699280419850705,-0.697957571269769,-0.695136013903449,
-0.691427643732457,-0.682711188630784,-0.664998255990807,-0.662324499038495),
 .UNSPECIFIED.);
#57=B_SPLINE_CURVE_WITH_KNOTS('',3,(#7569,#7570,#7571,#7572,#7573,#7574,
#7575,#7576,#7577,#7578,#7579,#7580,#7581,#7582,#7583,#7584,#7585,#7586,
#7587,#7588,#7589,#7590,#7591,#7592,#7593,#7594,#7595,#7596,#7597,#7598,
#7599,#7600,#7601,#7602,#7603,#7604,#7605,#7606,#7607,#7608,#7609,#7610,
#7611,#7612,#7613,#7614,#7615,#7616,#7617,#7618,#7619,#7620,#7621,#7622,
#7623,#7624,#7625,#7626,#7627,#7628,#7629,#7630,#7631,#7632,#7633,#7634,
#7635,#7636,#7637,#7638,#7639,#7640,#7641,#7642,#7643,#7644,#7645,#7646,
#7647,#7648,#7649,#7650,#7651,#7652,#7653,#7654,#7655,#7656,#7657,#7658,
#7659,#7660,#7661,#7662,#7663,#7664,#7665,#7666,#7667,#7668,#7669,#7670,
#7671,#7672,#7673,#7674,#7675,#7676,#7677,#7678,#7679,#7680,#7681,#7682,
#7683,#7684,#7685,#7686,#7687,#7688,#7689,#7690,#7691,#7692,#7693,#7694,
#7695,#7696,#7697,#7698,#7699,#7700,#7701,#7702,#7703,#7704,#7705,#7706,
#7707,#7708,#7709,#7710,#7711,#7712,#7713,#7714,#7715,#7716,#7717,#7718,
#7719,#7720,#7721,#7722,#7723,#7724,#7725,#7726,#7727,#7728,#7729,#7730,
#7731,#7732,#7733,#7734,#7735,#7736,#7737,#7738,#7739,#7740,#7741,#7742,
#7743,#7744,#7745,#7746,#7747,#7748,#7749,#7750,#7751,#7752,#7753,#7754,
#7755,#7756,#7757,#7758,#7759,#7760,#7761,#7762,#7763,#7764,#7765,#7766,
#7767,#7768,#7769,#7770,#7771,#7772,#7773,#7774,#7775,#7776,#7777,#7778,
#7779,#7780,#7781,#7782),.UNSPECIFIED.,.F.,.F.,(4,2,2,2,2,2,2,2,2,2,2,2,
2,2,2,2,2,2,2,2,2,2,2,2,2,2,2,2,2,2,2,2,2,2,2,2,2,2,2,2,2,2,2,2,2,2,2,2,
2,2,2,2,2,2,2,2,2,2,2,2,2,2,2,2,2,2,2,2,2,2,2,2,2,2,2,2,2,2,2,2,2,2,2,2,
2,2,2,2,2,2,2,2,2,2,2,2,2,2,2,2,2,2,2,2,2,2,4),(-1.3701619549454,-1.34115135310392,
-1.31831143699482,-1.30718929834551,-1.30564344268663,-1.30490626846844,
-1.30435218608931,-1.30375216196324,-1.3031277417398,-1.30222323139391,
-1.30064309239597,-1.24528350026959,-1.15177538253259,-1.14613845984611,
-1.1443203021435,-1.14331636224977,-1.14231064046418,-1.14107155873233,
-1.13868849943003,-1.12366248269812,-1.08974344022715,-0.987868290400893,
-0.986822996530763,-0.983186710591633,-0.982113951081348,-0.981542821111783,
-0.98099365147284,-0.980329445335926,-0.979614060402389,-0.978492035852106,
-0.976357342255281,-0.971236116919608,-0.955627814543821,-0.934846726973935,
-0.852954257674139,-0.825111183074129,-0.822039555561863,-0.820802474280758,
-0.819773155029944,-0.818719659790828,-0.81718534091166,-0.813156739775617,
-0.758839966014531,-0.747758346212163,-0.665010199820993,-0.660321635888516,
-0.659258604637777,-0.65856430707468,-0.658015962476613,-0.657384888306055,
-0.656716066726844,-0.65570497956919,-0.653857248037782,-0.649645546401276,
-0.636737810240214,-0.612905633827277,-0.506307326496183,-0.499990038807665,
-0.498088066322018,-0.496953741209485,-0.496046491865546,-0.494828274735134,
-0.492544085647648,-0.479740753278492,-0.454951691761461,-0.426336711451099,
-0.417587091025077,-0.410178173361807,-0.403755795062053,-0.382479796443228,
-0.350300316886761,-0.337965584207506,-0.336513557558312,-0.335784655597205,
-0.335253856673224,-0.334692898554503,-0.333933312413152,-0.333085051521418,
-0.331643159827392,-0.32863425489269,-0.320470219075656,-0.29463715519072,
-0.204446540705489,-0.198191257648153,-0.196622558825525,-0.195413048405089,
-0.194131911134594,-0.178294807567187,-0.175674360440021,-0.174386559422068,
-0.173376236049085,-0.172255261325581,-0.170412504796756,-0.163890267301671,
-0.12241414700715,-0.0246162518267315,-0.0211795458601249,-0.0194053746103256,
-0.0142397686502214,-0.0131389262299117,-0.0124329152529533,-0.011900026942397,
-0.0113735739312462,-0.0107535690494248,-0.00985983528173989,-0.00681011635358851,
-0.000961031473661812),.UNSPECIFIED.);
#58=B_SPLINE_CURVE_WITH_KNOTS('',3,(#7783,#7784,#7785,#7786,#7787,#7788,
#7789,#7790,#7791,#7792,#7793,#7794,#7795,#7796,#7797,#7798,#7799,#7800,
#7801,#7802,#7803,#7804,#7805,#7806,#7807,#7808,#7809,#7810,#7811,#7812,
#7813,#7814,#7815,#7816,#7817,#7818,#7819,#7820,#7821,#7822,#7823,#7824,
#7825,#7826,#7827,#7828,#7829,#7830,#7831,#7832,#7833,#7834,#7835,#7836,
#7837,#7838,#7839,#7840,#7841,#7842,#7843,#7844,#7845,#7846,#7847,#7848,
#7849,#7850,#7851,#7852,#7853,#7854,#7855,#7856,#7857,#7858,#7859,#7860,
#7861,#7862,#7863,#7864,#7865,#7866,#7867,#7868,#7869,#7870,#7871,#7872,
#7873,#7874,#7875,#7876,#7877,#7878),.UNSPECIFIED.,.F.,.F.,(4,2,2,2,2,2,
2,2,2,2,2,2,2,2,2,2,2,2,2,2,2,2,2,2,2,2,2,2,2,2,2,2,2,2,2,2,2,2,2,2,2,2,
2,2,2,2,2,4),(-4.06232412567137,-3.96648542039376,-3.91745202059908,-3.91421284775563,
-3.9128083751604,-3.91178041528948,-3.91083535965951,-3.90955947355159,
-3.9064506929146,-3.8747357219951,-3.78887590179063,-3.7756751336445,-3.76010141945642,
-3.75519218831468,-3.75312329102701,-3.75202650859378,-3.75109128955129,
-3.7504930279537,-3.74993642574647,-3.74919383136785,-3.74756103250365,
-3.73466055024734,-3.70723196379845,-3.68300067981111,-3.63224595767332,
-3.59793957823797,-3.5921300575717,-3.59036326721542,-3.58925927663615,
-3.58824463406113,-3.58694545772515,-3.58419647026443,-3.56559655365699,
-3.56409065731819,-3.55754880898839,-3.46820308152277,-3.44286360191163,
-3.43422314357478,-3.43108660190526,-3.42959997565459,-3.42873342317246,
-3.42796037449361,-3.42739701062215,-3.42686930655741,-3.42615245717212,
-3.42474780319502,-3.41376750612561,-3.4011377333033),.UNSPECIFIED.);
#59=B_SPLINE_CURVE_WITH_KNOTS('',3,(#7880,#7881,#7882,#7883,#7884,#7885,
#7886,#7887,#7888,#7889,#7890,#7891,#7892,#7893,#7894,#7895,#7896,#7897,
#7898,#7899,#7900,#7901,#7902,#7903,#7904,#7905,#7906,#7907,#7908,#7909,
#7910,#7911,#7912,#7913,#7914,#7915,#7916,#7917,#7918,#7919,#7920,#7921,
#7922,#7923,#7924,#7925,#7926,#7927,#7928,#7929,#7930,#7931,#7932,#7933,
#7934,#7935,#7936,#7937,#7938,#7939,#7940,#7941,#7942,#7943,#7944,#7945,
#7946,#7947,#7948,#7949,#7950,#7951,#7952,#7953,#7954,#7955,#7956,#7957,
#7958,#7959,#7960,#7961,#7962,#7963,#7964,#7965,#7966,#7967,#7968,#7969,
#7970,#7971,#7972,#7973,#7974,#7975,#7976,#7977),.UNSPECIFIED.,.F.,.F.,
(4,2,2,2,2,2,2,2,2,2,2,2,2,2,2,2,2,2,2,2,2,2,2,2,2,2,2,2,2,2,2,2,2,2,2,
2,2,2,2,2,2,2,2,2,2,2,2,2,4),(-0.662324499038495,-0.626175222042389,-0.552344439691317,
-0.54131308533216,-0.539906618530502,-0.539189281204045,-0.538661429449004,
-0.538086599985878,-0.537290470234446,-0.535406146089974,-0.500679915735166,
-0.491155572976965,-0.483490151623553,-0.477046575968648,-0.471502134149543,
-0.425114532282901,-0.411311074824101,-0.382554733539475,-0.379498385594101,
-0.378243028774384,-0.377302877209851,-0.376347958398889,-0.375341429865526,
-0.372969289010916,-0.358026215372137,-0.32436524713951,-0.308620889977391,
-0.222511483520392,-0.22214655906175,-0.22131142190472,-0.217568310114071,
-0.216483410522155,-0.215909810754102,-0.215405633767391,-0.214749497017367,
-0.213579298370337,-0.208222875361436,-0.126052566752693,-0.108774115850613,
-0.102898337167071,-0.0599323184146636,-0.0566002057968977,-0.0552854519641184,
-0.0543301611443897,-0.0533086148152846,-0.0523063404258367,-0.0509863049470586,
-0.0488902604045168,-0.000961571770198283),.UNSPECIFIED.);
#60=B_SPLINE_CURVE_WITH_KNOTS('',3,(#7978,#7979,#7980,#7981,#7982,#7983,
#7984,#7985,#7986,#7987,#7988,#7989,#7990,#7991,#7992,#7993,#7994,#7995,
#7996,#7997,#7998,#7999,#8000,#8001,#8002,#8003,#8004,#8005,#8006,#8007,
#8008,#8009,#8010,#8011,#8012,#8013,#8014,#8015,#8016,#8017,#8018,#8019,
#8020,#8021,#8022,#8023,#8024,#8025,#8026,#8027,#8028,#8029,#8030,#8031,
#8032,#8033,#8034,#8035,#8036,#8037,#8038,#8039,#8040,#8041,#8042,#8043,
#8044,#8045,#8046,#8047,#8048,#8049,#8050,#8051,#8052,#8053,#8054,#8055,
#8056,#8057,#8058,#8059,#8060,#8061,#8062,#8063,#8064,#8065,#8066,#8067,
#8068,#8069,#8070,#8071,#8072,#8073,#8074,#8075,#8076,#8077,#8078,#8079,
#8080,#8081,#8082,#8083,#8084,#8085,#8086,#8087,#8088,#8089,#8090,#8091,
#8092,#8093,#8094,#8095,#8096,#8097,#8098,#8099,#8100,#8101,#8102,#8103,
#8104,#8105,#8106,#8107,#8108,#8109,#8110,#8111,#8112,#8113,#8114,#8115,
#8116,#8117,#8118,#8119,#8120,#8121,#8122,#8123,#8124,#8125,#8126,#8127,
#8128,#8129,#8130,#8131,#8132,#8133,#8134,#8135,#8136,#8137,#8138,#8139,
#8140,#8141,#8142,#8143,#8144,#8145,#8146,#8147,#8148,#8149,#8150,#8151,
#8152,#8153,#8154,#8155),.UNSPECIFIED.,.F.,.F.,(4,2,2,2,2,2,2,2,2,2,2,2,
2,2,2,2,2,2,2,2,2,2,2,2,2,2,2,2,2,2,2,2,2,2,2,2,2,2,2,2,2,2,2,2,2,2,2,2,
2,2,2,2,2,2,2,2,2,2,2,2,2,2,2,2,2,2,2,2,2,2,2,2,2,2,2,2,2,2,2,2,2,2,2,2,
2,2,2,2,4),(-4.06054529852164,-3.98499342916419,-3.96351933523899,-3.95458984271673,
-3.95323878401419,-3.95254398434728,-3.95203688610906,-3.95148678706787,
-3.95051806646734,-3.94770210468645,-3.90001299330774,-3.84766270383631,
-3.82771146819536,-3.79595055807878,-3.79302160190387,-3.79195328463526,
-3.7910119860081,-3.78999227252994,-3.78866075176049,-3.78584856748139,
-3.76480733076895,-3.76223716102674,-3.74640747779537,-3.7210404799264,
-3.70226630622101,-3.66438359736754,-3.64155118912963,-3.63182187502163,
-3.63044238804677,-3.62974169932912,-3.62923388473046,-3.62868651327399,
-3.6277313640613,-3.62501262598604,-3.62256216102106,-3.53672861148087,
-3.50251456318248,-3.48236223092972,-3.47180603464155,-3.46965169258818,
-3.46866804518156,-3.46769606043423,-3.4667298715607,-3.4653734753377,-3.46257824363259,
-3.43347623187295,-3.38507497476963,-3.34963539046534,-3.32727707081713,
-3.31681389342674,-3.30882084993112,-3.30750761579816,-3.30682078487585,
-3.30626048572905,-3.30560598286827,-3.30447325828035,-3.30014349969786,
-3.22589303350608,-3.17725600621282,-3.15877126067808,-3.15228340077766,
-3.1493063812167,-3.14694759491979,-3.1457191457725,-3.14480787156796,-3.14383417408783,
-3.14245006371774,-3.13868966235461,-3.05957683303757,-3.01421957331284,
-2.99019544265606,-2.98554901355322,-2.98443154252778,-2.98378719074342,
-2.98322603903951,-2.98252594638656,-2.98144396557571,-2.97651924030072,
-2.88158371114211,-2.8286678032174,-2.82597007868055,-2.82379545857293,
-2.8226063431288,-2.82169971238678,-2.82056255518472,-2.8186472056681,-2.81221278259547,
-2.70676879774558,-2.6920647855843),.UNSPECIFIED.);
#61=B_SPLINE_CURVE_WITH_KNOTS('',3,(#8160,#8161,#8162,#8163,#8164,#8165,
#8166,#8167,#8168,#8169,#8170,#8171,#8172,#8173,#8174,#8175,#8176,#8177,
#8178,#8179,#8180,#8181,#8182,#8183,#8184,#8185,#8186,#8187,#8188,#8189,
#8190,#8191,#8192,#8193,#8194,#8195,#8196,#8197,#8198,#8199,#8200,#8201,
#8202,#8203,#8204,#8205,#8206,#8207,#8208,#8209,#8210,#8211,#8212,#8213,
#8214,#8215,#8216,#8217,#8218,#8219,#8220,#8221,#8222,#8223,#8224,#8225,
#8226,#8227,#8228,#8229,#8230,#8231,#8232,#8233,#8234,#8235,#8236,#8237,
#8238,#8239,#8240,#8241,#8242,#8243,#8244,#8245,#8246,#8247,#8248,#8249,
#8250,#8251,#8252,#8253,#8254,#8255,#8256,#8257,#8258,#8259,#8260,#8261,
#8262,#8263,#8264,#8265,#8266,#8267,#8268,#8269,#8270,#8271,#8272,#8273,
#8274,#8275,#8276,#8277,#8278,#8279,#8280,#8281,#8282,#8283,#8284,#8285,
#8286,#8287,#8288,#8289,#8290,#8291,#8292,#8293,#8294,#8295,#8296,#8297,
#8298,#8299,#8300,#8301,#8302,#8303,#8304,#8305,#8306,#8307,#8308,#8309,
#8310,#8311,#8312,#8313,#8314,#8315,#8316,#8317,#8318,#8319,#8320,#8321,
#8322,#8323,#8324,#8325,#8326,#8327,#8328,#8329,#8330,#8331,#8332,#8333,
#8334,#8335,#8336,#8337,#8338,#8339,#8340,#8341,#8342,#8343,#8344,#8345,
#8346,#8347,#8348,#8349,#8350,#8351,#8352,#8353,#8354,#8355,#8356,#8357,
#8358,#8359,#8360,#8361,#8362,#8363,#8364,#8365,#8366,#8367,#8368,#8369,
#8370,#8371,#8372,#8373,#8374,#8375,#8376,#8377,#8378,#8379,#8380,#8381,
#8382,#8383,#8384,#8385,#8386,#8387,#8388,#8389,#8390,#8391,#8392,#8393,
#8394,#8395,#8396,#8397,#8398,#8399,#8400,#8401,#8402,#8403,#8404,#8405,
#8406,#8407,#8408,#8409,#8410,#8411,#8412,#8413,#8414,#8415,#8416,#8417,
#8418,#8419,#8420,#8421,#8422,#8423,#8424,#8425,#8426,#8427,#8428,#8429,
#8430,#8431,#8432,#8433,#8434,#8435,#8436,#8437,#8438,#8439,#8440,#8441,
#8442,#8443,#8444,#8445,#8446,#8447),.UNSPECIFIED.,.F.,.F.,(4,2,2,2,2,2,
2,2,2,2,2,2,2,2,2,2,2,2,2,2,2,2,2,2,2,2,2,2,2,2,2,2,2,2,2,2,2,2,2,2,2,2,
2,2,2,2,2,2,2,2,2,2,2,2,2,2,2,2,2,2,2,2,2,2,2,2,2,2,2,2,2,2,2,2,2,2,2,2,
2,2,2,2,2,2,2,2,2,2,2,2,2,2,2,2,2,2,2,2,2,2,2,2,2,2,2,2,2,2,2,2,2,2,2,2,
2,2,2,2,2,2,2,2,2,2,2,2,2,2,2,2,2,2,2,2,2,2,2,2,2,2,2,2,2,4),(-3.4011014600555,
-3.39940690323357,-3.36821987190727,-3.30906870334161,-3.29935110609441,
-3.28807316327819,-3.27184011470122,-3.24994950733,-3.24528032609246,-3.24416062170285,
-3.2435155487649,-3.24295411679195,-3.24225412307298,-3.2411731245627,-3.23626566689753,
-3.14036220638563,-3.10216066430334,-3.09150590138587,-3.08719901143788,
-3.08499918454455,-3.08363544201015,-3.08238367081698,-3.08139290121133,
-3.08041224923559,-3.07900398090188,-3.07508859236555,-3.0112223607403,
-2.97240527940232,-2.96314717273488,-2.92404966028106,-2.92164154053198,
-2.92076268779955,-2.92017109449524,-2.91959758810996,-2.91890661572345,
-2.91718392001004,-2.90149083721128,-2.81497729793915,-2.76886105966987,
-2.7643054894577,-2.76201315710154,-2.76061070199914,-2.75932974800709,
-2.75833544147687,-2.7573656446848,-2.75599680856933,-2.75233520602908,
-2.69646612233531,-2.66685302246514,-2.60001381245473,-2.59826906781251,
-2.59749748183649,-2.59692686035156,-2.59639279454439,-2.59565192534417,
-2.59415280855494,-2.5803285603877,-2.57958608687794,-2.57754255472367,
-2.57639270456604,-2.4890183126688,-2.44548986278611,-2.44107462095199,
-2.43883439737757,-2.43745376762172,-2.43618981222795,-2.43519760947577,
-2.43422212780552,-2.43254708841092,-2.42793862720706,-2.35769359271476,
-2.33170256884607,-2.30388935359502,-2.29084594135386,-2.28117132325032,
-2.27598888088953,-2.2748308049314,-2.27417732336373,-2.27367319426155,
-2.27309750749487,-2.27200227891033,-2.26816606493582,-2.26746175827766,
-2.16447935097377,-2.13136885459105,-2.11654750944929,-2.11417242570336,
-2.11293486850434,-2.11202542158643,-2.11104418129392,-2.1093397513608,
-2.10453191919316,-2.03132658348778,-1.95700579608364,-1.95274821953981,
-1.95162232699873,-1.95096927304073,-1.95040867107091,-1.94971953446012,
-1.94839604318288,-1.94016937207797,-1.92269442738877,-1.8978763978881,
-1.821232657027,-1.81401550114089,-1.8123170311346,-1.81111419628571,-1.8094506028626,
-1.80738480834939,-1.80604608859597,-1.80401203016697,-1.80185476084991,
-1.79308955402763,-1.7911532017242,-1.78989709401582,-1.78888977685416,
-1.78774889838939,-1.78581815796213,-1.77837235200505,-1.68702556580016,
-1.64335131533585,-1.64298019569692,-1.64206622556867,-1.63038694086426,
-1.62881908297876,-1.62807735792684,-1.62752258343268,-1.62701725393456,
-1.62616202898285,-1.62517961730373,-1.62340473675258,-1.60908957788495,
-1.59123682585296,-1.47526132780508,-1.46924213718703,-1.46737582758715,
-1.46636209971794,-1.46535724172279,-1.46413474859306,-1.46183059637055,
-1.44861454618318,-1.42730382860027,-1.38255916814419,-1.3701619549454),
 .UNSPECIFIED.);
#62=B_SPLINE_CURVE_WITH_KNOTS('',3,(#8448,#8449,#8450,#8451,#8452,#8453,
#8454,#8455,#8456,#8457,#8458,#8459,#8460,#8461,#8462,#8463,#8464,#8465,
#8466,#8467,#8468,#8469,#8470,#8471,#8472,#8473,#8474,#8475,#8476,#8477,
#8478,#8479,#8480,#8481,#8482,#8483,#8484,#8485,#8486,#8487,#8488,#8489,
#8490,#8491,#8492,#8493,#8494,#8495,#8496,#8497,#8498,#8499,#8500,#8501,
#8502,#8503,#8504,#8505,#8506,#8507,#8508,#8509,#8510,#8511,#8512,#8513,
#8514,#8515,#8516,#8517,#8518,#8519,#8520,#8521,#8522,#8523,#8524,#8525,
#8526,#8527,#8528,#8529,#8530,#8531,#8532,#8533,#8534,#8535,#8536,#8537,
#8538,#8539,#8540,#8541,#8542,#8543,#8544,#8545,#8546,#8547,#8548,#8549,
#8550,#8551,#8552,#8553,#8554,#8555,#8556,#8557,#8558,#8559,#8560,#8561,
#8562,#8563,#8564,#8565,#8566,#8567,#8568,#8569,#8570,#8571,#8572,#8573,
#8574,#8575,#8576,#8577,#8578,#8579,#8580,#8581,#8582,#8583,#8584,#8585,
#8586,#8587,#8588,#8589,#8590,#8591,#8592,#8593,#8594,#8595,#8596,#8597,
#8598,#8599,#8600,#8601,#8602,#8603,#8604,#8605,#8606,#8607,#8608,#8609,
#8610,#8611,#8612,#8613,#8614,#8615,#8616,#8617,#8618,#8619,#8620,#8621,
#8622,#8623,#8624,#8625,#8626,#8627,#8628,#8629,#8630,#8631,#8632,#8633,
#8634,#8635,#8636,#8637,#8638,#8639,#8640,#8641,#8642,#8643,#8644,#8645,
#8646,#8647,#8648,#8649,#8650,#8651,#8652,#8653,#8654,#8655,#8656,#8657,
#8658,#8659,#8660,#8661,#8662,#8663,#8664,#8665,#8666,#8667,#8668,#8669,
#8670,#8671,#8672,#8673,#8674,#8675,#8676,#8677,#8678,#8679,#8680,#8681,
#8682,#8683,#8684,#8685,#8686,#8687,#8688,#8689,#8690,#8691,#8692,#8693,
#8694,#8695,#8696,#8697,#8698,#8699,#8700,#8701,#8702,#8703,#8704,#8705,
#8706,#8707),.UNSPECIFIED.,.F.,.F.,(4,2,2,2,2,2,2,2,2,2,2,2,2,2,2,2,2,2,
2,2,2,2,2,2,2,2,2,2,2,2,2,2,2,2,2,2,2,2,2,2,2,2,2,2,2,2,2,2,2,2,2,2,2,2,
2,2,2,2,2,2,2,2,2,2,2,2,2,2,2,2,2,2,2,2,2,2,2,2,2,2,2,2,2,2,2,2,2,2,2,2,
2,2,2,2,2,2,2,2,2,2,2,2,2,2,2,2,2,2,2,2,2,2,2,2,2,2,2,2,2,2,2,2,2,2,2,2,
2,2,2,4),(-2.6920647855843,-2.66439261547396,-2.66193825728155,-2.66105299386178,
-2.66046018819521,-2.6598879651661,-2.65920135247204,-2.65756862797743,
-2.64406122980707,-2.64053004716835,-2.56143407129139,-2.5056417960861,
-2.50291085483323,-2.50071109499098,-2.49951789594537,-2.49851337085416,
-2.49749689004228,-2.49561653548507,-2.48948027174901,-2.38667307843778,
-2.34027846590777,-2.33855360027067,-2.33778574179126,-2.33721584912747,
-2.33668093742887,-2.33593656977653,-2.33401120484566,-2.30710349538859,
-2.21743524360764,-2.19279905329067,-2.17989162835144,-2.17760238305398,
-2.17638310291426,-2.17537843865337,-2.17436282065688,-2.17248698357659,
-2.1663889042745,-2.05648998007698,-2.03056475998383,-2.01699332659318,
-2.01535823770699,-2.01467111254571,-2.0140986696264,-2.01350586053559,
-2.01262100101754,-2.01017032332889,-1.96809556660331,-1.86200096319919,
-1.85585457622815,-1.85397288165234,-1.85295606383677,-1.85195144726959,
-1.85073399928539,-1.84845343997416,-1.83572390997298,-1.81091914864285,
-1.7213192650137,-1.69425360604937,-1.69232564832215,-1.69158082104481,
-1.69104576288015,-1.69047589252731,-1.68970836279523,-1.68810122419827,
-1.68592167227656,-1.66553866046491,-1.65233079280088,-1.5648096915393,
-1.53482899583954,-1.53201243250427,-1.53065067214364,-1.52968292349312,
-1.52876931186694,-1.52749990888916,-1.5250215757515,-1.50875902994798,
-1.46976995418952,-1.39929752851573,-1.37126321419471,-1.3693200759058,
-1.36857276604585,-1.36803705525047,-1.36752459514755,-1.36679288908419,
-1.36529022067289,-1.35180677557876,-1.32683745905079,-1.25789085770878,
-1.21232048863365,-1.20895036993735,-1.20762926120843,-1.2066723500484,
-1.20565187119117,-1.20429300032847,-1.20139080977996,-1.17621503570113,
-1.15530484615385,-1.09474525280727,-1.04952295291457,-1.04668888547896,
-1.04571731400844,-1.04516658429636,-1.04465953398093,-1.04396574864625,
-1.04264688189498,-1.03444003665025,-1.01706883906462,-0.951643867993534,
-0.889959209039997,-0.886170537817232,-0.884781846522835,-0.883806746443549,
-0.882895608308876,-0.881644348070232,-0.879268059234405,-0.864062309113781,
-0.82939499609107,-0.78215980211301,-0.727249928427786,-0.723878179017082,
-0.722836679154761,-0.722271860405961,-0.721767149491578,-0.721098633495444,
-0.720390907539149,-0.717514463815689,-0.71305909372594,-0.69915158303225,
-0.680503822703977,-0.661689072177721),.UNSPECIFIED.);
#63=B_SPLINE_CURVE_WITH_KNOTS('',3,(#8713,#8714,#8715,#8716,#8717,#8718,
#8719,#8720,#8721,#8722,#8723,#8724,#8725,#8726,#8727,#8728,#8729,#8730,
#8731,#8732,#8733,#8734,#8735,#8736,#8737,#8738,#8739,#8740,#8741,#8742,
#8743,#8744,#8745,#8746,#8747,#8748,#8749,#8750,#8751,#8752,#8753,#8754,
#8755,#8756,#8757,#8758,#8759,#8760,#8761,#8762,#8763,#8764,#8765,#8766,
#8767,#8768,#8769,#8770,#8771,#8772,#8773,#8774,#8775,#8776,#8777,#8778,
#8779,#8780,#8781,#8782,#8783,#8784,#8785,#8786,#8787,#8788,#8789,#8790,
#8791,#8792,#8793,#8794,#8795,#8796,#8797,#8798,#8799,#8800,#8801,#8802,
#8803,#8804,#8805,#8806,#8807,#8808,#8809,#8810,#8811,#8812,#8813,#8814,
#8815,#8816,#8817,#8818,#8819,#8820,#8821,#8822,#8823,#8824,#8825,#8826,
#8827,#8828,#8829,#8830,#8831,#8832,#8833,#8834,#8835,#8836,#8837,#8838,
#8839,#8840,#8841,#8842,#8843,#8844,#8845,#8846,#8847,#8848,#8849,#8850,
#8851,#8852,#8853,#8854,#8855,#8856,#8857,#8858,#8859,#8860,#8861,#8862,
#8863,#8864,#8865,#8866,#8867,#8868,#8869,#8870,#8871,#8872,#8873,#8874,
#8875,#8876,#8877,#8878,#8879,#8880,#8881,#8882,#8883,#8884,#8885,#8886,
#8887,#8888,#8889,#8890,#8891,#8892,#8893,#8894,#8895,#8896),
 .UNSPECIFIED.,.F.,.F.,(4,2,2,2,2,2,2,2,2,2,2,2,2,2,2,2,2,2,2,2,2,2,2,2,
2,2,2,2,2,2,2,2,2,2,2,2,2,2,2,2,2,2,2,2,2,2,2,2,2,2,2,2,2,2,2,2,2,2,2,2,
2,2,2,2,2,2,2,2,2,2,2,2,2,2,2,2,2,2,2,2,2,2,2,2,2,2,2,2,2,2,2,4),(-1.37035830239853,
-1.31313469101143,-1.28727965526401,-1.28426708703911,-1.28291822818799,
-1.28191644837135,-1.28086040695646,-1.27977354847701,-1.2782345349457,
-1.2756126501719,-1.2288193851385,-1.14860878768378,-1.14293376372204,-1.14074797571466,
-1.14047560813828,-1.13957734603937,-1.13793978753991,-1.13721267716872,
-1.12337513007256,-1.12187579809469,-1.1211349326605,-1.12060091996006,
-1.12003040419328,-1.11925904343146,-1.11751515380254,-1.05374170161686,
-0.993413216191368,-0.964378189601015,-0.961584130435153,-0.9602278372092,
-0.95926151143448,-0.958266871905048,-0.956977065171376,-0.95556234090598,
-0.953240486527951,-0.948604637073653,-0.936840576964002,-0.911121856136205,
-0.861652194387613,-0.811880750102781,-0.800279953603009,-0.798852923724145,
-0.798130299688123,-0.797601061850922,-0.797027252856783,-0.796236957908265,
-0.79438656020786,-0.744558170991191,-0.703913481258456,-0.6424904784718,
-0.638706943199471,-0.637318984531292,-0.636344039736707,-0.635351752003725,
-0.634084742226636,-0.632701647372255,-0.63045544182614,-0.62602391725306,
-0.614951456988997,-0.574360562937398,-0.481440911052703,-0.476567587938416,
-0.475489403267113,-0.474790329948266,-0.474229030039711,-0.473583432638654,
-0.472461149625609,-0.467758159441654,-0.426623297611181,-0.385670316276792,
-0.361297649963714,-0.318768890711419,-0.315443933775958,-0.31413025679984,
-0.313175136936421,-0.31217363314459,-0.310846434625592,-0.309380139520474,
-0.306934604089779,-0.301960731676674,-0.210513498715984,-0.16914182131995,
-0.166176332788331,-0.154126780661544,-0.152524337792522,-0.151787175084658,
-0.151219934211912,-0.150603296624108,-0.149610752665144,-0.146301732861082,
-0.125702996532957,-0.000961965831634676),.UNSPECIFIED.);
#64=B_SPLINE_CURVE_WITH_KNOTS('',3,(#8897,#8898,#8899,#8900,#8901,#8902,
#8903,#8904,#8905,#8906,#8907,#8908,#8909,#8910,#8911,#8912,#8913,#8914,
#8915,#8916,#8917,#8918,#8919,#8920,#8921,#8922,#8923,#8924,#8925,#8926,
#8927,#8928,#8929,#8930,#8931,#8932,#8933,#8934,#8935,#8936,#8937,#8938,
#8939,#8940,#8941,#8942,#8943,#8944,#8945,#8946,#8947,#8948,#8949,#8950,
#8951,#8952,#8953,#8954,#8955,#8956,#8957,#8958,#8959,#8960,#8961,#8962,
#8963,#8964,#8965,#8966,#8967,#8968,#8969,#8970,#8971,#8972,#8973,#8974,
#8975,#8976,#8977,#8978,#8979,#8980,#8981,#8982,#8983,#8984,#8985,#8986,
#8987,#8988,#8989,#8990,#8991,#8992,#8993,#8994,#8995,#8996,#8997,#8998,
#8999,#9000,#9001,#9002,#9003,#9004,#9005,#9006,#9007,#9008,#9009,#9010,
#9011,#9012,#9013,#9014,#9015,#9016),.UNSPECIFIED.,.F.,.F.,(4,2,2,2,2,2,
2,2,2,2,2,2,2,2,2,2,2,2,2,2,2,2,2,2,2,2,2,2,2,2,2,2,2,2,2,2,2,2,2,2,2,2,
2,2,2,2,2,2,2,2,2,2,2,2,2,2,2,2,2,4),(-4.06269744394932,-4.05769728268495,
-4.05419629673872,-4.05294702562819,-4.05196861910404,-4.0509894985384,
-4.05001337596529,-4.04833553111765,-4.04370937424276,-4.03757889468122,
-3.92938250846978,-3.914999855999,-3.89455864540268,-3.89126521792167,-3.89027431643437,
-3.88965799366881,-3.88909054528441,-3.8883524303158,-3.88674523345941,
-3.87457357768122,-3.87138149839504,-3.87039493851564,-3.86953012344522,
-3.79046894215544,-3.74926025335208,-3.73808046044618,-3.7336163870156,
-3.73135782098288,-3.72996937850653,-3.72869875596071,-3.72770560947298,
-3.72673173606717,-3.72534850187567,-3.72159730980179,-3.66086285289679,
-3.63147909661404,-3.62248639548299,-3.59378428428253,-3.57693136772514,
-3.56874615748008,-3.56742409996392,-3.56673514001948,-3.56617438810977,
-3.5655208236653,-3.56439324801888,-3.56012080636243,-3.5573491571516,-3.55584622145444,
-3.55456601528934,-3.46797793993311,-3.43119932851864,-3.41668157031755,
-3.41126043071538,-3.4086541645731,-3.40712139099913,-3.4057464346528,-3.40473662551545,
-3.40379344411166,-3.40252675287791,-3.4011014600555),.UNSPECIFIED.);
#65=B_SPLINE_CURVE_WITH_KNOTS('',3,(#9018,#9019,#9020,#9021,#9022,#9023,
#9024,#9025,#9026,#9027,#9028,#9029,#9030,#9031,#9032,#9033,#9034,#9035,
#9036,#9037,#9038,#9039,#9040,#9041,#9042,#9043,#9044,#9045,#9046,#9047,
#9048,#9049,#9050,#9051,#9052,#9053,#9054,#9055,#9056,#9057,#9058,#9059,
#9060,#9061,#9062,#9063,#9064,#9065,#9066,#9067,#9068,#9069,#9070,#9071,
#9072,#9073,#9074,#9075,#9076,#9077,#9078,#9079,#9080,#9081,#9082,#9083,
#9084,#9085,#9086,#9087,#9088,#9089,#9090,#9091,#9092,#9093,#9094,#9095,
#9096,#9097,#9098,#9099,#9100,#9101,#9102,#9103,#9104,#9105,#9106,#9107,
#9108,#9109,#9110,#9111,#9112,#9113,#9114,#9115,#9116,#9117,#9118,#9119,
#9120,#9121,#9122,#9123,#9124,#9125,#9126,#9127,#9128,#9129),
 .UNSPECIFIED.,.F.,.F.,(4,2,2,2,2,2,2,2,2,2,2,2,2,2,2,2,2,2,2,2,2,2,2,2,
2,2,2,2,2,2,2,2,2,2,2,2,2,2,2,2,2,2,2,2,2,2,2,2,2,2,2,2,2,2,2,4),(-0.661689072177721,
-0.635438189052493,-0.590996444194058,-0.58493164743744,-0.583468913200705,
-0.58224814615159,-0.580453319943521,-0.578372682005945,-0.576005193915886,
-0.57003350679353,-0.563972131075917,-0.562100578561216,-0.561085735082499,
-0.560080862959325,-0.558859928007559,-0.557564122547763,-0.552016600234222,
-0.519309604037286,-0.469724083183996,-0.410843999933654,-0.40985829866635,
-0.408088015642741,-0.401494588357825,-0.400296671927898,-0.39956884099718,
-0.399003123434441,-0.398382236902337,-0.397741810305707,-0.396798698479298,
-0.388532639403567,-0.370531405029497,-0.343430014275277,-0.318524206658404,
-0.245129471291207,-0.240599080285158,-0.238935990916333,-0.237962947212669,
-0.23705110872491,-0.235794798424088,-0.234449996398847,-0.232295025769849,
-0.215562697395506,-0.177460993323038,-0.164103860879277,-0.150549097395737,
-0.0822736035438614,-0.0781767092023072,-0.0770669934721367,-0.0764177237101079,
-0.0759129736330026,-0.0752443049929717,-0.0745363801645729,-0.0734321417212298,
-0.0713440483731208,-0.0663737342799348,-0.000961608844988501),
 .UNSPECIFIED.);
#66=B_SPLINE_CURVE_WITH_KNOTS('',3,(#9130,#9131,#9132,#9133,#9134,#9135,
#9136,#9137,#9138,#9139,#9140,#9141,#9142,#9143,#9144,#9145,#9146,#9147,
#9148,#9149,#9150,#9151,#9152,#9153,#9154,#9155,#9156,#9157,#9158,#9159,
#9160,#9161,#9162,#9163,#9164,#9165,#9166,#9167,#9168,#9169,#9170,#9171,
#9172,#9173,#9174,#9175,#9176,#9177,#9178,#9179,#9180,#9181,#9182,#9183,
#9184,#9185,#9186,#9187,#9188,#9189,#9190,#9191,#9192,#9193,#9194,#9195,
#9196,#9197,#9198,#9199,#9200,#9201,#9202,#9203,#9204,#9205,#9206,#9207,
#9208,#9209,#9210,#9211,#9212,#9213,#9214,#9215,#9216,#9217,#9218,#9219,
#9220,#9221,#9222,#9223,#9224,#9225,#9226,#9227,#9228,#9229,#9230,#9231,
#9232,#9233,#9234,#9235,#9236,#9237,#9238,#9239,#9240,#9241,#9242,#9243,
#9244,#9245,#9246,#9247,#9248,#9249,#9250,#9251,#9252,#9253,#9254,#9255,
#9256,#9257,#9258,#9259,#9260,#9261,#9262,#9263,#9264,#9265,#9266,#9267,
#9268,#9269,#9270,#9271,#9272,#9273,#9274,#9275,#9276,#9277,#9278,#9279,
#9280,#9281,#9282,#9283,#9284,#9285,#9286,#9287,#9288,#9289,#9290,#9291,
#9292,#9293,#9294,#9295,#9296,#9297,#9298,#9299,#9300,#9301,#9302,#9303,
#9304,#9305,#9306,#9307,#9308,#9309,#9310,#9311,#9312,#9313,#9314,#9315),
 .UNSPECIFIED.,.F.,.F.,(4,2,2,2,2,2,2,2,2,2,2,2,2,2,2,2,2,2,2,2,2,2,2,2,
2,2,2,2,2,2,2,2,2,2,2,2,2,2,2,2,2,2,2,2,2,2,2,2,2,2,2,2,2,2,2,2,2,2,2,2,
2,2,2,2,2,2,2,2,2,2,2,2,2,2,2,2,2,2,2,2,2,2,2,2,2,2,2,2,2,2,2,2,4),(-4.06100209435087,
-3.99455560708784,-3.9799802658478,-3.97790988131639,-3.97660085526456,
-3.97537049774392,-3.97446220133678,-3.97347818791015,-3.97175853731164,
-3.96684176792589,-3.8898848744918,-3.87632607302362,-3.86335695204296,
-3.82964209247129,-3.81598622941117,-3.81491794097997,-3.81422522916569,
-3.81356751272227,-3.81306352537448,-3.81249163710651,-3.81141437192997,
-3.80773615102716,-3.74489621682546,-3.72512656377337,-3.70572059584182,
-3.67134460217803,-3.66137806910723,-3.65518898642008,-3.65384984143269,
-3.65259772176189,-3.6516867355372,-3.65071253387599,-3.64904230119304,
-3.64446232015115,-3.57072446860636,-3.52360757989629,-3.49393137331868,
-3.49187666891556,-3.49124009192201,-3.49062194848218,-3.49005570650699,
-3.48932309362008,-3.48774316428525,-3.47625840010405,-3.42646231826365,
-3.37883915944638,-3.34767087233704,-3.3382353631171,-3.33230296159233,
-3.33098072401437,-3.3297408039214,-3.3288313216303,-3.32785167709853,-3.3264458286726,
-3.32254334017667,-3.26199759757763,-3.22016726552227,-3.17084226879795,
-3.16898847479866,-3.16818886319945,-3.1676135052689,-3.16708660809439,
-3.16637263726346,-3.16497889110281,-3.15427841300663,-3.1117435476327,
-3.04871541558155,-3.035863543586,-3.01149295543485,-3.00852050467562,-3.0071495207056,
-3.00612731388847,-3.00517410550499,-3.00386643315513,-3.00057430202474,
-2.95990623994496,-2.90573108384631,-2.84868236481933,-2.84633542609704,
-2.84545874198934,-2.84486782798132,-2.84429435542709,-2.84360270342334,
-2.84187453489065,-2.82596590609577,-2.82516723917376,-2.82398244416466,
-2.82283234395509,-2.81810332315078,-2.80653581748999,-2.74224851330479,
-2.71809003659731,-2.6925136763791),.UNSPECIFIED.);
#67=B_SPLINE_CURVE_WITH_KNOTS('',3,(#9320,#9321,#9322,#9323,#9324,#9325,
#9326,#9327,#9328,#9329,#9330,#9331,#9332,#9333,#9334,#9335,#9336,#9337,
#9338,#9339,#9340,#9341,#9342,#9343,#9344,#9345,#9346,#9347,#9348,#9349,
#9350,#9351,#9352,#9353,#9354,#9355,#9356,#9357,#9358,#9359,#9360,#9361,
#9362,#9363,#9364,#9365,#9366,#9367,#9368,#9369,#9370,#9371,#9372,#9373,
#9374,#9375,#9376,#9377,#9378,#9379,#9380,#9381,#9382,#9383,#9384,#9385,
#9386,#9387,#9388,#9389,#9390,#9391,#9392,#9393,#9394,#9395,#9396,#9397,
#9398,#9399,#9400,#9401,#9402,#9403,#9404,#9405,#9406,#9407,#9408,#9409,
#9410,#9411,#9412,#9413,#9414,#9415,#9416,#9417,#9418,#9419,#9420,#9421,
#9422,#9423,#9424,#9425,#9426,#9427,#9428,#9429,#9430,#9431,#9432,#9433,
#9434,#9435,#9436,#9437,#9438,#9439,#9440,#9441,#9442,#9443,#9444,#9445,
#9446,#9447,#9448,#9449,#9450,#9451,#9452,#9453,#9454,#9455,#9456,#9457,
#9458,#9459,#9460,#9461,#9462,#9463,#9464,#9465,#9466,#9467,#9468,#9469,
#9470,#9471,#9472,#9473,#9474,#9475,#9476,#9477,#9478,#9479,#9480,#9481,
#9482,#9483,#9484,#9485,#9486,#9487,#9488,#9489,#9490,#9491,#9492,#9493,
#9494,#9495,#9496,#9497,#9498,#9499,#9500,#9501,#9502,#9503,#9504,#9505,
#9506,#9507,#9508,#9509,#9510,#9511,#9512,#9513,#9514,#9515,#9516,#9517,
#9518,#9519,#9520,#9521,#9522,#9523,#9524,#9525,#9526,#9527,#9528,#9529,
#9530,#9531,#9532,#9533,#9534,#9535,#9536,#9537,#9538,#9539,#9540,#9541,
#9542,#9543,#9544,#9545,#9546,#9547,#9548,#9549,#9550,#9551,#9552,#9553,
#9554,#9555,#9556,#9557,#9558,#9559,#9560,#9561,#9562,#9563,#9564,#9565,
#9566,#9567,#9568,#9569,#9570,#9571,#9572,#9573,#9574,#9575,#9576,#9577,
#9578,#9579,#9580,#9581,#9582,#9583,#9584,#9585,#9586,#9587,#9588,#9589,
#9590,#9591,#9592,#9593,#9594,#9595,#9596,#9597,#9598,#9599,#9600,#9601,
#9602,#9603,#9604,#9605,#9606,#9607,#9608,#9609,#9610,#9611,#9612,#9613,
#9614,#9615,#9616,#9617,#9618,#9619),.UNSPECIFIED.,.F.,.F.,(4,2,2,2,2,2,
2,2,2,2,2,2,2,2,2,2,2,2,2,2,2,2,2,2,2,2,2,2,2,2,2,2,2,2,2,2,2,2,2,2,2,2,
2,2,2,2,2,2,2,2,2,2,2,2,2,2,2,2,2,2,2,2,2,2,2,2,2,2,2,2,2,2,2,2,2,2,2,2,
2,2,2,2,2,2,2,2,2,2,2,2,2,2,2,2,2,2,2,2,2,2,2,2,2,2,2,2,2,2,2,2,2,2,2,2,
2,2,2,2,2,2,2,2,2,2,2,2,2,2,2,2,2,2,2,2,2,2,2,2,2,2,2,2,2,2,2,2,2,2,2,4),
(-3.39999468752269,-3.39888508074895,-3.38864706455002,-3.38509663653904,
-3.38268746164111,-3.38181149302039,-3.38128715723683,-3.38071938172533,
-3.37997472378146,-3.3783895199414,-3.36620885509757,-3.36431102179285,
-3.36350557505008,-3.36066389792965,-3.35826263009743,-3.28322487147196,
-3.27240876426585,-3.25782147723038,-3.23721101923308,-3.22399249708449,
-3.22168999736582,-3.22046862673111,-3.21946481876955,-3.21845225744448,
-3.21658840847785,-3.21057959252479,-3.09478492549836,-3.07038515236454,
-3.06397606651343,-3.06145808168865,-3.06019301332519,-3.05917426282592,
-3.05854171868414,-3.05798110276021,-3.05728378940053,-3.05620999191957,
-3.05138190052675,-3.04960353058936,-2.95023621548289,-2.92055330625379,
-2.91441984394696,-2.90100967030443,-2.89869793968004,-2.89747449778693,
-2.89647044774759,-2.89545887927529,-2.89360042141055,-2.88763692976508,
-2.77233105442108,-2.73876116446253,-2.73735042193173,-2.73651509781933,
-2.73578906201379,-2.73522736804566,-2.73469843432204,-2.73397595410638,
-2.73254839467543,-2.72090997493493,-2.68617234992351,-2.6422701669739,
-2.58203916238946,-2.57692658816435,-2.57524317301434,-2.57415807470247,
-2.57313731475397,-2.57179671244384,-2.56953289705597,-2.56112848814692,
-2.55874935774861,-2.55747416869619,-2.55643606692916,-2.55434453136443,
-2.5524633351361,-2.55123620156271,-2.54953914460951,-2.54330753556182,
-2.53550203470692,-2.51802674103955,-2.44612949765603,-2.4383487614759,
-2.41763880761357,-2.41543956523201,-2.41429325959219,-2.41356785869525,
-2.41293267031608,-2.41238213272442,-2.41182567081232,-2.41082439908466,
-2.40776673548098,-2.35821704159072,-2.33281474312137,-2.30729793574649,
-2.27115952245672,-2.2555488883302,-2.25314360446534,-2.25190019672765,
-2.25089456907919,-2.24989370347248,-2.24808939695326,-2.24255523589577,
-2.12307154915067,-2.10104919731347,-2.09198834659389,-2.09063259873344,
-2.08993690514599,-2.08937614274246,-2.08881277172444,-2.08777782748419,
-2.0844578196934,-2.03185402404902,-1.96193156576471,-1.93351498386433,
-1.93042826785742,-1.92918895701729,-1.92815930181385,-1.92710701207653,
-1.92557727089689,-1.92157658895362,-1.8687140264278,-1.77366811607669,
-1.76873953027171,-1.76765722655489,-1.76695702573442,-1.76639585391538,
-1.76575155236312,-1.76463435124635,-1.75999152737085,-1.73561832620679,
-1.68788408213307,-1.61284999384229,-1.60813010439633,-1.60643876948035,
-1.60546029039319,-1.60447009905361,-1.60321326545907,-1.60184409976123,
-1.59963082210951,-1.59528713057083,-1.55299102686655,-1.45000802481392,
-1.44929931922799,-1.44546650164039,-1.4443717360424,-1.44379618910936,
-1.44329212511127,-1.44263864881901,-1.44148035732081,-1.43629338899788,
-1.38259972603757,-1.37035830239853),.UNSPECIFIED.);
#68=B_SPLINE_CURVE_WITH_KNOTS('',3,(#9620,#9621,#9622,#9623,#9624,#9625,
#9626,#9627,#9628,#9629,#9630,#9631,#9632,#9633,#9634,#9635,#9636,#9637,
#9638,#9639,#9640,#9641,#9642,#9643,#9644,#9645,#9646,#9647,#9648,#9649,
#9650,#9651,#9652,#9653,#9654,#9655,#9656,#9657,#9658,#9659,#9660,#9661,
#9662,#9663,#9664,#9665,#9666,#9667,#9668,#9669,#9670,#9671,#9672,#9673,
#9674,#9675,#9676,#9677,#9678,#9679,#9680,#9681,#9682,#9683,#9684,#9685,
#9686,#9687,#9688,#9689,#9690,#9691,#9692,#9693,#9694,#9695,#9696,#9697,
#9698,#9699,#9700,#9701,#9702,#9703,#9704,#9705,#9706,#9707,#9708,#9709,
#9710,#9711,#9712,#9713,#9714,#9715,#9716,#9717,#9718,#9719,#9720,#9721,
#9722,#9723,#9724,#9725,#9726,#9727,#9728,#9729,#9730,#9731,#9732,#9733,
#9734,#9735,#9736,#9737,#9738,#9739,#9740,#9741,#9742,#9743,#9744,#9745,
#9746,#9747,#9748,#9749,#9750,#9751,#9752,#9753,#9754,#9755,#9756,#9757,
#9758,#9759,#9760,#9761,#9762,#9763,#9764,#9765,#9766,#9767,#9768,#9769,
#9770,#9771,#9772,#9773,#9774,#9775,#9776,#9777,#9778,#9779,#9780,#9781,
#9782,#9783,#9784,#9785,#9786,#9787,#9788,#9789,#9790,#9791,#9792,#9793,
#9794,#9795,#9796,#9797,#9798,#9799,#9800,#9801,#9802,#9803,#9804,#9805,
#9806,#9807,#9808,#9809,#9810,#9811,#9812,#9813,#9814,#9815,#9816,#9817,
#9818,#9819,#9820,#9821,#9822,#9823,#9824,#9825,#9826,#9827,#9828,#9829,
#9830,#9831,#9832,#9833,#9834,#9835,#9836,#9837,#9838,#9839,#9840,#9841,
#9842,#9843,#9844,#9845,#9846,#9847,#9848,#9849,#9850,#9851,#9852,#9853,
#9854,#9855,#9856,#9857,#9858,#9859,#9860,#9861,#9862,#9863,#9864,#9865,
#9866,#9867,#9868,#9869,#9870,#9871,#9872,#9873,#9874,#9875,#9876,#9877,
#9878,#9879,#9880,#9881,#9882,#9883,#9884,#9885,#9886,#9887,#9888,#9889,
#9890,#9891,#9892,#9893,#9894,#9895,#9896,#9897),.UNSPECIFIED.,.F.,.F.,
(4,2,2,2,2,2,2,2,2,2,2,2,2,2,2,2,2,2,2,2,2,2,2,2,2,2,2,2,2,2,2,2,2,2,2,
2,2,2,2,2,2,2,2,2,2,2,2,2,2,2,2,2,2,2,2,2,2,2,2,2,2,2,2,2,2,2,2,2,2,2,2,
2,2,2,2,2,2,2,2,2,2,2,2,2,2,2,2,2,2,2,2,2,2,2,2,2,2,2,2,2,2,2,2,2,2,2,2,
2,2,2,2,2,2,2,2,2,2,2,2,2,2,2,2,2,2,2,2,2,2,2,2,2,2,2,2,2,2,2,4),(-2.6925136763791,
-2.691349806873,-2.68640116471688,-2.6847420978949,-2.68365459336578,-2.68263420918073,
-2.68129791328207,-2.67835241356829,-2.65458726286017,-2.57907715134864,
-2.52685699631286,-2.52369001010775,-2.52271639452321,-2.5220997531916,
-2.52153294171388,-2.52079693011943,-2.51919931032582,-2.50726036352065,
-2.50504097216832,-2.5045954377761,-2.50143518369202,-2.49992602349204,
-2.49005744146085,-2.40221200913805,-2.36925639200468,-2.36361340174826,
-2.36186981615955,-2.36076313081419,-2.3597493959125,-2.35845602235567,
-2.35573665319751,-2.33780810447716,-2.23833461440736,-2.20212271255252,
-2.20022827525242,-2.19943044815193,-2.19885534515629,-2.19832793751886,
-2.19761220027943,-2.19621182765393,-2.18534109143103,-2.09464422253666,
-2.06218172455028,-2.04193918166971,-2.03938353835468,-2.03810881243561,
-2.03719455235325,-2.03622905099406,-2.03487522894154,-2.03130487181021,
-1.97577546092888,-1.88285738028345,-1.87796215404449,-1.87688239824507,
-1.87618293235685,-1.8756217371776,-1.8749767271081,-1.87385661720462,-1.86917864839645,
-1.84850855819866,-1.82401713854521,-1.72446273836435,-1.71775253061962,
-1.71580567719067,-1.71466137512114,-1.7136643584933,-1.71241861201454,
-1.71000381108026,-1.69446940103456,-1.65855407987267,-1.56117872848709,
-1.56005999373534,-1.55536844185267,-1.55398410911901,-1.55327244697552,
-1.5527460198217,-1.55216990393184,-1.55138317673594,-1.54954048025857,
-1.54700661574797,-1.45836767630944,-1.39757116530015,-1.39378758417087,
-1.39239971367785,-1.39142486356331,-1.3905136993963,-1.38926200027535,
-1.38681901008649,-1.37053883454821,-1.33180691023247,-1.25892054890241,
-1.2329218234999,-1.23101122226387,-1.23026929813183,-1.22973502606504,
-1.22916472525219,-1.22840998355347,-1.22673891589629,-1.22449778758587,
-1.20312610057062,-1.14465354267821,-1.07538637235953,-1.07102003655398,
-1.06938228554458,-1.06841426881729,-1.06750074604691,-1.06623200970819,
-1.06370643325601,-1.04487226252374,-1.01612719711402,-0.951140483009,-0.928195914060588,
-0.923765851911744,-0.92344539762017,-0.922559001780413,-0.92206110623185,
-0.921239750865158,-0.909445831829231,-0.908012143660318,-0.907287848318172,
-0.906758201819078,-0.906184771704657,-0.905616981718027,-0.904234372019432,
-0.894275702962061,-0.868548219656582,-0.824502336248255,-0.786177246901088,
-0.750861781069498,-0.747670596246262,-0.746380038215635,-0.7454310422672,
-0.744405458233358,-0.743016065842197,-0.739862866114819,-0.735647400735218,
-0.72529396470047,-0.688761199217399,-0.662310186026634),.UNSPECIFIED.);
#69=B_SPLINE_CURVE_WITH_KNOTS('',3,(#9903,#9904,#9905,#9906,#9907,#9908,
#9909,#9910,#9911,#9912,#9913,#9914,#9915,#9916,#9917,#9918,#9919,#9920,
#9921,#9922,#9923,#9924,#9925,#9926,#9927,#9928,#9929,#9930,#9931,#9932,
#9933,#9934,#9935,#9936,#9937,#9938,#9939,#9940,#9941,#9942,#9943,#9944,
#9945,#9946,#9947,#9948,#9949,#9950,#9951,#9952,#9953,#9954,#9955,#9956,
#9957,#9958,#9959,#9960,#9961,#9962,#9963,#9964,#9965,#9966,#9967,#9968,
#9969,#9970,#9971,#9972,#9973,#9974,#9975,#9976,#9977,#9978,#9979,#9980,
#9981,#9982,#9983,#9984,#9985,#9986,#9987,#9988,#9989,#9990,#9991,#9992,
#9993,#9994,#9995,#9996,#9997,#9998,#9999,#10000,#10001,#10002,#10003,#10004,
#10005,#10006,#10007,#10008,#10009,#10010,#10011,#10012,#10013,#10014,#10015,
#10016,#10017,#10018,#10019,#10020,#10021,#10022,#10023,#10024,#10025,#10026,
#10027,#10028,#10029,#10030,#10031,#10032,#10033,#10034,#10035,#10036,#10037,
#10038,#10039,#10040,#10041,#10042,#10043,#10044,#10045,#10046,#10047,#10048,
#10049,#10050,#10051,#10052,#10053,#10054,#10055,#10056,#10057,#10058,#10059,
#10060,#10061,#10062,#10063,#10064,#10065,#10066,#10067,#10068,#10069,#10070,
#10071,#10072,#10073,#10074,#10075,#10076,#10077,#10078,#10079,#10080,#10081,
#10082,#10083,#10084,#10085,#10086,#10087,#10088,#10089,#10090,#10091,#10092,
#10093,#10094,#10095,#10096,#10097,#10098,#10099,#10100,#10101,#10102,#10103,
#10104),.UNSPECIFIED.,.F.,.F.,(4,2,2,2,2,2,2,2,2,2,2,2,2,2,2,2,2,2,2,2,
2,2,2,2,2,2,2,2,2,2,2,2,2,2,2,2,2,2,2,2,2,2,2,2,2,2,2,2,2,2,2,2,2,2,2,2,
2,2,2,2,2,2,2,2,2,2,2,2,2,2,2,2,2,2,2,2,2,2,2,2,2,2,2,2,2,2,2,2,2,2,2,2,
2,2,2,2,2,2,2,2,4),(-1.3702925990382,-1.3646065123406,-1.27381134544931,
-1.26205774028186,-1.26048731237941,-1.25974516762392,-1.25917732763983,
-1.2585757189674,-1.25762589165693,-1.25650806933852,-1.25438432904009,
-1.20624500881719,-1.12921162168623,-1.12272149643121,-1.12122673262677,
-1.12003174308615,-1.11602423209939,-1.11530461207618,-1.11455244310793,
-1.11259160846636,-1.1105820478428,-1.10240224398722,-1.09984033023852,
-1.09854647352297,-1.09753532305077,-1.09641744438754,-1.09458889816991,
-1.08820716803191,-1.04822639192728,-0.94698832566313,-0.944720812359825,
-0.939614549818961,-0.937602984484482,-0.936844557767111,-0.93630582110514,
-0.935765248411139,-0.935040869744138,-0.933530231521145,-0.931550960094603,
-0.926928277091865,-0.912352090239843,-0.86819304746328,-0.783333380593811,
-0.777841309673415,-0.776041777992556,-0.775041428159509,-0.774044511468714,
-0.772802473239471,-0.770406213141967,-0.755060245452764,-0.719928202648477,
-0.680221302447579,-0.627071353120496,-0.615888049739316,-0.614339582183063,
-0.613601817153927,-0.613034613347241,-0.612430946893631,-0.611472420612584,
-0.608449013701643,-0.603696300615647,-0.588628875062841,-0.558037195675566,
-0.480775846255374,-0.477210432570438,-0.456630396520522,-0.453799586835005,
-0.452484579458253,-0.451467380005995,-0.450370380424853,-0.448635643767317,
-0.443107075048842,-0.411414326406116,-0.364605389980612,-0.343762929276641,
-0.315764345385161,-0.304771280431548,-0.292978694522289,-0.291545053713341,
-0.290820771269963,-0.290291128937723,-0.289756696103606,-0.289196703169409,
-0.287886894078347,-0.279897516335745,-0.269422982829613,-0.250014896693966,
-0.159080377076261,-0.152993827463823,-0.151575859332063,-0.150360477391903,
-0.149235963728482,-0.133323365037272,-0.130698876511579,-0.129410171985675,
-0.128399637948359,-0.12727894164361,-0.125437813426122,-0.118933080236084,
-0.0776491223565139,-0.000962580391007859),.UNSPECIFIED.);
#70=B_SPLINE_CURVE_WITH_KNOTS('',3,(#10105,#10106,#10107,#10108,#10109,
#10110,#10111,#10112,#10113,#10114,#10115,#10116,#10117,#10118,#10119,#10120,
#10121,#10122,#10123,#10124,#10125,#10126,#10127,#10128,#10129,#10130,#10131,
#10132,#10133,#10134,#10135,#10136,#10137,#10138,#10139,#10140,#10141,#10142,
#10143,#10144,#10145,#10146,#10147,#10148,#10149,#10150,#10151,#10152,#10153,
#10154,#10155,#10156,#10157,#10158,#10159,#10160,#10161,#10162,#10163,#10164,
#10165,#10166,#10167,#10168,#10169,#10170,#10171,#10172,#10173,#10174,#10175,
#10176,#10177,#10178,#10179,#10180,#10181,#10182,#10183,#10184,#10185,#10186,
#10187,#10188,#10189,#10190,#10191,#10192,#10193,#10194,#10195,#10196,#10197,
#10198,#10199,#10200,#10201,#10202,#10203,#10204,#10205,#10206,#10207,#10208),
 .UNSPECIFIED.,.F.,.F.,(4,2,2,2,2,2,2,2,2,2,2,2,2,2,2,2,2,2,2,2,2,2,2,2,
2,2,2,2,2,2,2,2,2,2,2,2,2,2,2,2,2,2,2,2,2,2,2,2,2,2,2,4),(-4.06022502783442,
-4.02941315715002,-4.02823287730869,-4.02749340286536,-4.02693407807125,
-4.02640041630651,-4.02587157338326,-4.02514859807187,-4.02371819358163,
-4.01197934923213,-4.00949075323713,-4.0064615868957,-4.00521260221354,
-3.99508509257341,-3.99114949833664,-3.90677322024206,-3.8821592639454,
-3.86927324002438,-3.86698720772121,-3.86576956874246,-3.86486342118252,
-3.86373134735246,-3.86183522300634,-3.85555453413604,-3.74871266922852,
-3.72825477858468,-3.71320185323394,-3.70601251083289,-3.70474081534874,
-3.70418537588386,-3.70364868783383,-3.70311530088758,-3.70237512240616,
-3.70047179238169,-3.67479848416132,-3.63234380886613,-3.62733850302291,
-3.6215698809821,-3.6148179562441,-3.60673143078635,-3.59666542673705,-3.56642698230218,
-3.54702559194131,-3.54449541904677,-3.54322663484052,-3.54231396997977,
-3.54134768856648,-3.53998875073913,-3.53718047533541,-3.50744583280931,
-3.41987959723944,-3.39999468752269),.UNSPECIFIED.);
#71=B_SPLINE_CURVE_WITH_KNOTS('',3,(#10210,#10211,#10212,#10213,#10214,
#10215,#10216,#10217,#10218,#10219,#10220,#10221,#10222,#10223,#10224,#10225,
#10226,#10227,#10228,#10229,#10230,#10231,#10232,#10233,#10234,#10235,#10236,
#10237,#10238,#10239,#10240,#10241,#10242,#10243,#10244,#10245,#10246,#10247,
#10248,#10249,#10250,#10251,#10252,#10253,#10254,#10255,#10256,#10257,#10258,
#10259,#10260,#10261,#10262,#10263,#10264,#10265,#10266,#10267,#10268,#10269,
#10270,#10271,#10272,#10273,#10274,#10275,#10276,#10277,#10278,#10279,#10280,
#10281,#10282,#10283,#10284,#10285,#10286,#10287,#10288,#10289,#10290,#10291,
#10292,#10293,#10294,#10295,#10296,#10297,#10298,#10299,#10300,#10301,#10302,
#10303,#10304,#10305),.UNSPECIFIED.,.F.,.F.,(4,2,2,2,2,2,2,2,2,2,2,2,2,
2,2,2,2,2,2,2,2,2,2,2,2,2,2,2,2,2,2,2,2,2,2,2,2,2,2,2,2,2,2,2,2,2,2,4),
(-0.662310186026634,-0.63675288603753,-0.588333427674046,-0.585495917556745,
-0.584523823481245,-0.583972982986467,-0.583465948922825,-0.582926218405347,
-0.582247573747971,-0.579734924363326,-0.554581793756154,-0.513735407137791,
-0.430827978459099,-0.42545535422149,-0.423671792629946,-0.422674708205422,
-0.421677361040954,-0.420429282494195,-0.418003824836794,-0.402185690190519,
-0.365209064224272,-0.341759075045079,-0.318182644017952,-0.272511262305969,
-0.271630528862389,-0.269488261566253,-0.268791595284995,-0.263087101133857,
-0.261947064187762,-0.261228984229397,-0.260666055906529,-0.260033283919376,
-0.259375842766903,-0.258391869657778,-0.248318115196362,-0.218297281671593,
-0.196686020435488,-0.164401118176624,-0.105937940264548,-0.102102229561359,
-0.100706312914663,-0.0997292351256157,-0.0988186995731407,-0.0975720540397754,
-0.0951534505095346,-0.0921177860775552,-0.0854576127161563,-0.000962002473629624),
 .UNSPECIFIED.);
#72=B_SPLINE_CURVE_WITH_KNOTS('',3,(#10306,#10307,#10308,#10309,#10310,
#10311,#10312,#10313,#10314,#10315,#10316,#10317,#10318,#10319,#10320,#10321,
#10322,#10323,#10324,#10325,#10326,#10327,#10328,#10329,#10330,#10331,#10332,
#10333,#10334,#10335,#10336,#10337,#10338,#10339,#10340,#10341,#10342,#10343,
#10344,#10345,#10346,#10347,#10348,#10349,#10350,#10351,#10352,#10353,#10354,
#10355,#10356,#10357,#10358,#10359,#10360,#10361,#10362,#10363,#10364,#10365,
#10366,#10367,#10368,#10369,#10370,#10371,#10372,#10373,#10374,#10375,#10376,
#10377,#10378,#10379,#10380,#10381,#10382,#10383,#10384,#10385,#10386,#10387,
#10388,#10389,#10390,#10391,#10392,#10393,#10394,#10395,#10396,#10397,#10398,
#10399,#10400,#10401,#10402,#10403,#10404,#10405,#10406,#10407,#10408,#10409,
#10410,#10411,#10412,#10413,#10414,#10415,#10416,#10417,#10418,#10419,#10420,
#10421,#10422,#10423,#10424,#10425,#10426,#10427,#10428,#10429,#10430,#10431,
#10432,#10433,#10434,#10435,#10436,#10437,#10438,#10439,#10440,#10441,#10442,
#10443,#10444,#10445,#10446,#10447,#10448,#10449,#10450,#10451,#10452,#10453,
#10454,#10455,#10456,#10457,#10458,#10459,#10460,#10461,#10462,#10463,#10464,
#10465,#10466,#10467,#10468,#10469,#10470,#10471,#10472,#10473,#10474,#10475,
#10476,#10477,#10478,#10479,#10480,#10481,#10482,#10483,#10484,#10485,#10486,
#10487,#10488,#10489,#10490,#10491,#10492,#10493,#10494,#10495,#10496,#10497,
#10498,#10499,#10500,#10501,#10502,#10503,#10504,#10505,#10506,#10507,#10508,
#10509,#10510,#10511,#10512,#10513),.UNSPECIFIED.,.F.,.F.,(4,2,2,2,2,2,
2,2,2,2,2,2,2,2,2,2,2,2,2,2,2,2,2,2,2,2,2,2,2,2,2,2,2,2,2,2,2,2,2,2,2,2,
2,2,2,2,2,2,2,2,2,2,2,2,2,2,2,2,2,2,2,2,2,2,2,2,2,2,2,2,2,2,2,2,2,2,2,2,
2,2,2,2,2,2,2,2,2,2,2,2,2,2,2,2,2,2,2,2,2,2,2,2,2,4),(-4.06056306224649,
-4.00985058969614,-4.00047566401566,-3.99927624979501,-3.99852851797568,
-3.99796591941104,-3.99739545221306,-3.99686196455536,-3.99612255299507,
-3.99462843663741,-3.98095180342464,-3.93541206834487,-3.92650036975616,
-3.91864565346336,-3.90263572260438,-3.85548687998933,-3.84042440568608,
-3.83801353337325,-3.83676872045931,-3.83577191818468,-3.83477364763648,
-3.83298324221768,-3.82755697749892,-3.74384889337152,-3.72134051564925,
-3.69445809408888,-3.68274511411716,-3.67882574084003,-3.67622341349027,
-3.67553726710497,-3.67499540862029,-3.67443926633666,-3.6738805548619,
-3.67286882114242,-3.66973286857439,-3.61554262387277,-3.56900443110658,
-3.5615389306865,-3.53162004954608,-3.51746577710315,-3.5151073368869,-3.51387348504589,
-3.51296468059732,-3.51198212267652,-3.5105658689147,-3.50659468729772,
-3.50525807506071,-3.42574751033429,-3.37579235840384,-3.36107607754459,
-3.35402005146516,-3.35275377957752,-3.35207139440789,-3.35156565972193,
-3.35100929345434,-3.35000930641327,-3.34696359670673,-3.29818937034096,
-3.22980483856678,-3.21024608269278,-3.19475618838003,-3.19226724864279,
-3.19100618385251,-3.19009389309821,-3.18912317551664,-3.18775003749894,
-3.18405936842057,-3.12813059961869,-3.08586260021177,-3.05379676072633,
-3.03848417538124,-3.03366158559336,-3.03060479226204,-3.02964209897921,
-3.02902795844688,-3.02846032211443,-3.02771892548804,-3.02615182056934,
-3.01448024757926,-2.99043663390157,-2.98859997049405,-2.92422629668604,
-2.90054553349135,-2.87289571018539,-2.86980768386537,-2.86841422289142,
-2.86738814031535,-2.86644045265128,-2.86515437796379,-2.86263875821785,
-2.8429386004191,-2.83537413996105,-2.81050277336572,-2.74989750382703,
-2.72666473447658,-2.71056167749424,-2.70866304294895,-2.70720333005324,
-2.70648887007284,-2.70597692831379,-2.70544057491816,-2.70469054667675,
-2.70272995443796,-2.69255696121762),.UNSPECIFIED.);
#73=B_SPLINE_CURVE_WITH_KNOTS('',3,(#10518,#10519,#10520,#10521,#10522,
#10523,#10524,#10525,#10526,#10527,#10528,#10529,#10530,#10531,#10532,#10533,
#10534,#10535,#10536,#10537,#10538,#10539,#10540,#10541,#10542,#10543,#10544,
#10545,#10546,#10547,#10548,#10549,#10550,#10551,#10552,#10553,#10554,#10555,
#10556,#10557,#10558,#10559,#10560,#10561,#10562,#10563,#10564,#10565,#10566,
#10567,#10568,#10569,#10570,#10571,#10572,#10573,#10574,#10575,#10576,#10577,
#10578,#10579,#10580,#10581,#10582,#10583,#10584,#10585,#10586,#10587,#10588,
#10589,#10590,#10591,#10592,#10593,#10594,#10595,#10596,#10597,#10598,#10599,
#10600,#10601,#10602,#10603,#10604,#10605,#10606,#10607,#10608,#10609,#10610,
#10611,#10612,#10613,#10614,#10615,#10616,#10617,#10618,#10619,#10620,#10621,
#10622,#10623,#10624,#10625,#10626,#10627,#10628,#10629,#10630,#10631,#10632,
#10633,#10634,#10635,#10636,#10637,#10638,#10639,#10640,#10641,#10642,#10643,
#10644,#10645,#10646,#10647,#10648,#10649,#10650,#10651,#10652,#10653,#10654,
#10655,#10656,#10657,#10658,#10659,#10660,#10661,#10662,#10663,#10664,#10665,
#10666,#10667,#10668,#10669,#10670,#10671,#10672,#10673,#10674,#10675,#10676,
#10677,#10678,#10679,#10680,#10681,#10682,#10683,#10684,#10685,#10686,#10687,
#10688,#10689,#10690,#10691,#10692,#10693,#10694,#10695,#10696,#10697,#10698,
#10699,#10700,#10701,#10702,#10703,#10704,#10705,#10706,#10707,#10708,#10709,
#10710,#10711,#10712,#10713,#10714,#10715,#10716,#10717,#10718,#10719,#10720,
#10721,#10722,#10723,#10724,#10725,#10726,#10727,#10728,#10729,#10730,#10731,
#10732,#10733,#10734,#10735,#10736,#10737,#10738,#10739,#10740,#10741,#10742,
#10743,#10744,#10745,#10746,#10747,#10748,#10749,#10750,#10751,#10752,#10753,
#10754,#10755,#10756,#10757,#10758,#10759,#10760,#10761,#10762,#10763,#10764,
#10765,#10766,#10767,#10768,#10769,#10770,#10771,#10772,#10773,#10774,#10775,
#10776,#10777,#10778,#10779,#10780,#10781,#10782,#10783,#10784,#10785),
 .UNSPECIFIED.,.F.,.F.,(4,2,2,2,2,2,2,2,2,2,2,2,2,2,2,2,2,2,2,2,2,2,2,2,
2,2,2,2,2,2,2,2,2,2,2,2,2,2,2,2,2,2,2,2,2,2,2,2,2,2,2,2,2,2,2,2,2,2,2,2,
2,2,2,2,2,2,2,2,2,2,2,2,2,2,2,2,2,2,2,2,2,2,2,2,2,2,2,2,2,2,2,2,2,2,2,2,
2,2,2,2,2,2,2,2,2,2,2,2,2,2,2,2,2,2,2,2,2,2,2,2,2,2,2,2,2,2,2,2,2,2,2,2,
2,4),(-3.40057646114791,-3.3780758375725,-3.36840278722896,-3.36439526785602,
-3.36139066010006,-3.36003268291409,-3.35900778506154,-3.35805801068777,
-3.35676422234127,-3.35355406154749,-3.31732904006563,-3.25931176082143,
-3.20442000492122,-3.19964546742521,-3.19851778925455,-3.19787109583537,
-3.19731006463557,-3.19661289279918,-3.19554052128646,-3.19073688093825,
-3.09832867860021,-3.05734155849525,-3.04620138352563,-3.04174970751654,
-3.0384784757685,-3.03707203272324,-3.03603828474931,-3.03509933095838,
-3.03384862317527,-3.03069334908051,-2.9997172075566,-2.9073834549355,-2.88585953030803,
-2.87691742550064,-2.87556570906745,-2.87487069761884,-2.87436349810518,
-2.87381334287839,-2.87284465653319,-2.87002961105812,-2.82258056836125,
-2.76553546368132,-2.74376287413353,-2.72046257855111,-2.71740968374126,
-2.71500027297125,-2.71376159515059,-2.71284869005617,-2.71187876017533,
-2.71023148262299,-2.70580415276338,-2.63426635093943,-2.59485501008328,
-2.55547466289783,-2.55306270362863,-2.5521834029862,-2.55159179444874,
-2.55101850171338,-2.55032804948362,-2.54860802356007,-2.53299904863972,
-2.53178136180014,-2.52719285099008,-2.51082670325984,-2.43744959529829,
-2.39948166775018,-2.39540070561707,-2.39234956544545,-2.39098399974005,
-2.38995768692751,-2.38900967660309,-2.38772299610491,-2.38520569491823,
-2.36547304665328,-2.35916863505314,-2.31965368483067,-2.29150191595262,
-2.23174377692246,-2.22989088471125,-2.22910016632392,-2.22852629161711,
-2.22799716987455,-2.22727496350389,-2.22584954038574,-2.2142939055225,
-2.12000667675021,-2.09061033387173,-2.07151651223088,-2.06899302358442,
-2.0677247414752,-2.06681130988596,-2.06584317093537,-2.06447990860073,
-2.06165713416645,-2.03140669551207,-1.99870026317578,-1.91238098137092,
-1.90773273885563,-1.90659111469871,-1.90587251143088,-1.9053094776008,
-1.90467691294312,-1.90361277126463,-1.89959162510923,-1.87091329328997,
-1.75279313579684,-1.74703576206788,-1.74520218219657,-1.74419513535759,
-1.74318978669074,-1.74195629503858,-1.73959979183382,-1.72521372622106,
-1.69391427539177,-1.64349039658081,-1.58747708851794,-1.58414250765324,
-1.58310566475482,-1.5825418493938,-1.58199208355738,-1.58138143495541,
-1.58019275912579,-1.57871983899557,-1.52439730404018,-1.50196938745237,
-1.4285183148996,-1.42382087528214,-1.42213282314433,-1.42115497894894,
-1.42024486927613,-1.41900056264828,-1.41659254089449,-1.40093136737134,
-1.3702925990382),.UNSPECIFIED.);
#74=B_SPLINE_CURVE_WITH_KNOTS('',3,(#10786,#10787,#10788,#10789,#10790,
#10791,#10792,#10793,#10794,#10795,#10796,#10797,#10798,#10799,#10800,#10801,
#10802,#10803,#10804,#10805,#10806,#10807,#10808,#10809,#10810,#10811,#10812,
#10813,#10814,#10815,#10816,#10817,#10818,#10819,#10820,#10821,#10822,#10823,
#10824,#10825,#10826,#10827,#10828,#10829,#10830,#10831,#10832,#10833,#10834,
#10835,#10836,#10837,#10838,#10839,#10840,#10841,#10842,#10843,#10844,#10845,
#10846,#10847,#10848,#10849,#10850,#10851,#10852,#10853,#10854,#10855,#10856,
#10857,#10858,#10859,#10860,#10861,#10862,#10863,#10864,#10865,#10866,#10867,
#10868,#10869,#10870,#10871,#10872,#10873,#10874,#10875,#10876,#10877,#10878,
#10879,#10880,#10881,#10882,#10883,#10884,#10885,#10886,#10887,#10888,#10889,
#10890,#10891,#10892,#10893,#10894,#10895,#10896,#10897,#10898,#10899,#10900,
#10901,#10902,#10903,#10904,#10905,#10906,#10907,#10908,#10909,#10910,#10911,
#10912,#10913,#10914,#10915,#10916,#10917,#10918,#10919,#10920,#10921,#10922,
#10923,#10924,#10925,#10926,#10927,#10928,#10929,#10930,#10931,#10932,#10933,
#10934,#10935,#10936,#10937,#10938,#10939,#10940,#10941,#10942,#10943,#10944,
#10945,#10946,#10947,#10948,#10949,#10950,#10951,#10952,#10953,#10954,#10955,
#10956,#10957,#10958,#10959,#10960,#10961,#10962,#10963,#10964,#10965,#10966,
#10967,#10968,#10969,#10970,#10971,#10972,#10973,#10974,#10975,#10976,#10977,
#10978,#10979,#10980,#10981,#10982,#10983,#10984,#10985,#10986,#10987,#10988,
#10989,#10990,#10991,#10992,#10993,#10994,#10995,#10996,#10997,#10998,#10999,
#11000,#11001,#11002,#11003,#11004,#11005,#11006,#11007,#11008,#11009,#11010,
#11011,#11012,#11013,#11014,#11015,#11016,#11017,#11018,#11019,#11020,#11021,
#11022,#11023,#11024,#11025,#11026,#11027,#11028,#11029,#11030,#11031,#11032,
#11033,#11034,#11035,#11036,#11037,#11038,#11039,#11040,#11041,#11042,#11043,
#11044,#11045,#11046,#11047,#11048,#11049,#11050,#11051,#11052,#11053,#11054,
#11055,#11056,#11057,#11058,#11059),.UNSPECIFIED.,.F.,.F.,(4,2,2,2,2,2,
2,2,2,2,2,2,2,2,2,2,2,2,2,2,2,2,2,2,2,2,2,2,2,2,2,2,2,2,2,2,2,2,2,2,2,2,
2,2,2,2,2,2,2,2,2,2,2,2,2,2,2,2,2,2,2,2,2,2,2,2,2,2,2,2,2,2,2,2,2,2,2,2,
2,2,2,2,2,2,2,2,2,2,2,2,2,2,2,2,2,2,2,2,2,2,2,2,2,2,2,2,2,2,2,2,2,2,2,2,
2,2,2,2,2,2,2,2,2,2,2,2,2,2,2,2,2,2,2,2,2,2,4),(-2.69255696121762,-2.67347825365679,
-2.58627168165284,-2.56149935779709,-2.54871425959265,-2.54641935350897,
-2.54519901389999,-2.54419449474869,-2.54317989025542,-2.54130844106319,
-2.53524468708342,-2.53382390960164,-2.53032962086112,-2.52891162285775,
-2.52695364768927,-2.52638753891779,-2.52430067698228,-2.52283416157334,
-2.52162851903848,-2.43863644977151,-2.38689160927336,-2.38459379329566,
-2.38373349105708,-2.38314223414127,-2.38256896794985,-2.38187818563985,
-2.38015544412112,-2.36443917379122,-2.36316922629901,-2.36036926766921,
-2.33089201040431,-2.30943930201984,-2.26127805319402,-2.23771083080318,
-2.22575006705512,-2.2235092113134,-2.22230036069438,-2.22130564404892,
-2.22028621102971,-2.21839117853824,-2.21213174163553,-2.10603927950583,
-2.06406759692736,-2.06161860087352,-2.06073403343725,-2.06014132686672,
-2.05956890896528,-2.05888173030109,-2.05724612486324,-2.04365574694947,
-2.04264276182633,-2.04175486668268,-2.03980651095245,-2.03163715773507,
-2.00666100196485,-1.9321063232717,-1.90397608063725,-1.90089649835486,
-1.89965811561594,-1.89862846601625,-1.89757540094881,-1.89604310966808,
-1.89202774447157,-1.83842965554268,-1.74401127242429,-1.73915707855529,
-1.7380804923654,-1.73738194892242,-1.73682073384261,-1.73617485361328,
-1.7350511371394,-1.73032903796948,-1.68862554964978,-1.58501101641814,
-1.57878582148155,-1.5768946391431,-1.57587586821121,-1.57489139084082,
-1.57378044474401,-1.57172400210714,-1.56920970632291,-1.50931814281801,
-1.42059534518491,-1.41590881346204,-1.41484591730983,-1.41415164371323,
-1.41364679943432,-1.41301741940066,-1.41196762672463,-1.40809999507898,
-1.31951541095213,-1.25872899378092,-1.25491189372383,-1.25351877264869,
-1.25254242039694,-1.2515506176788,-1.25028713834807,-1.24890899174348,
-1.24667458029896,-1.24227469835377,-1.19900755503168,-1.11838292016377,
-1.1147739056282,-1.10971912165377,-1.0936723088765,-1.09196223365962,-1.09126180524186,
-1.09073813577941,-1.0901592269365,-1.08934194338152,-1.08733263624776,
-1.07582970671104,-1.05011163146483,-0.94025281949781,-0.938009259376781,
-0.932295131056112,-0.930466905752835,-0.929460849025636,-0.928459893107989,
-0.927251225905809,-0.924981745348664,-0.922144062674089,-0.916062186601247,
-0.899111483269984,-0.850763426831215,-0.774075947140235,-0.77303897685378,
-0.76941738138719,-0.768346310796388,-0.767775522739613,-0.767220581802722,
-0.766539180666425,-0.765252084217158,-0.757842297137281,-0.742329307309087,
-0.692272519594694,-0.661978904396988),.UNSPECIFIED.);
#75=B_SPLINE_CURVE_WITH_KNOTS('',3,(#11065,#11066,#11067,#11068,#11069,
#11070,#11071,#11072,#11073,#11074,#11075,#11076,#11077,#11078,#11079,#11080,
#11081,#11082,#11083,#11084,#11085,#11086,#11087,#11088,#11089,#11090,#11091,
#11092,#11093,#11094,#11095,#11096,#11097,#11098,#11099,#11100,#11101,#11102,
#11103,#11104,#11105,#11106,#11107,#11108,#11109,#11110,#11111,#11112,#11113,
#11114,#11115,#11116,#11117,#11118,#11119,#11120,#11121,#11122,#11123,#11124,
#11125,#11126,#11127,#11128,#11129,#11130,#11131,#11132,#11133,#11134,#11135,
#11136,#11137,#11138,#11139,#11140,#11141,#11142,#11143,#11144,#11145,#11146,
#11147,#11148,#11149,#11150,#11151,#11152,#11153,#11154,#11155,#11156,#11157,
#11158,#11159,#11160,#11161,#11162,#11163,#11164,#11165,#11166,#11167,#11168,
#11169,#11170,#11171,#11172,#11173,#11174,#11175,#11176,#11177,#11178,#11179,
#11180,#11181,#11182,#11183,#11184,#11185,#11186,#11187,#11188,#11189,#11190,
#11191,#11192,#11193,#11194,#11195,#11196,#11197,#11198,#11199,#11200,#11201,
#11202,#11203,#11204,#11205,#11206,#11207,#11208,#11209,#11210,#11211,#11212,
#11213,#11214,#11215,#11216,#11217,#11218,#11219,#11220,#11221,#11222,#11223,
#11224,#11225,#11226,#11227,#11228,#11229,#11230,#11231,#11232,#11233,#11234,
#11235,#11236,#11237,#11238,#11239,#11240,#11241,#11242,#11243,#11244,#11245,
#11246,#11247,#11248,#11249,#11250,#11251,#11252,#11253,#11254,#11255,#11256,
#11257,#11258,#11259,#11260,#11261,#11262,#11263,#11264,#11265,#11266,#11267,
#11268,#11269,#11270,#11271,#11272,#11273,#11274,#11275,#11276,#11277,#11278),
 .UNSPECIFIED.,.F.,.F.,(4,2,2,2,2,2,2,2,2,2,2,2,2,2,2,2,2,2,2,2,2,2,2,2,
2,2,2,2,2,2,2,2,2,2,2,2,2,2,2,2,2,2,2,2,2,2,2,2,2,2,2,2,2,2,2,2,2,2,2,2,
2,2,2,2,2,2,2,2,2,2,2,2,2,2,2,2,2,2,2,2,2,2,2,2,2,2,2,2,2,2,2,2,2,2,2,2,
2,2,2,2,2,2,2,2,2,2,4),(-1.36955217660447,-1.35438198264554,-1.25171466928822,
-1.25033018241312,-1.24914578420268,-1.24301205659692,-1.23878392598788,
-1.23716839589181,-1.23620494527356,-1.23529005058641,-1.23403597046894,
-1.23155997848618,-1.22839810301241,-1.20364425443094,-1.16867765533724,
-1.08136737778924,-1.07656897407976,-1.07549716123163,-1.07480024117134,
-1.07423933653693,-1.07359270291284,-1.07246491629994,-1.06768689371836,
-1.01284384328921,-0.942114783682391,-0.938532701363764,-0.917968568710297,
-0.915138967765725,-0.913824413434402,-0.912807518047145,-0.911866303834704,
-0.910303617717483,-0.906056780776339,-0.899891974116983,-0.882628837322805,
-0.832110521666651,-0.757878793394048,-0.753557253638437,-0.752425300070153,
-0.751770959267558,-0.751210624089526,-0.750523531878927,-0.749209144944406,
-0.741190293935152,-0.738233644375573,-0.708836955097061,-0.637043657867222,
-0.619994283552344,-0.614485917866933,-0.61316077870147,-0.611957685387143,
-0.610340246165035,-0.608271667092593,-0.607313404898065,-0.606954649605142,
-0.604895585846466,-0.603068038590231,-0.595302423768686,-0.592609148376004,
-0.591278027862611,-0.590318600232067,-0.5892998263656,-0.588302580971732,
-0.58601675705447,-0.573027783792601,-0.548746586826365,-0.517863639930038,
-0.441029531642349,-0.438542062858685,-0.431056438844321,-0.429807528471815,
-0.429064682762545,-0.428496772427648,-0.427883186691457,-0.426903424071744,
-0.423705627302623,-0.375612653486214,-0.349181283099561,-0.317951095689469,
-0.299029579476036,-0.292124685105148,-0.290630298769369,-0.289435352112233,
-0.285481070328898,-0.284903076009555,-0.283105697494471,-0.281984092017214,
-0.279456172279823,-0.271022965258246,-0.269113986430642,-0.267866539798169,
-0.266860117346127,-0.265913977110473,-0.264790170791789,-0.261315824987277,
-0.227785563293494,-0.207412476083892,-0.112675597240101,-0.107768758366129,
-0.10668800903978,-0.105988198957318,-0.105426928374396,-0.104782055466478,
-0.103662735871478,-0.098995661539217,-0.077082042319963,-0.000962379967314271),
 .UNSPECIFIED.);
#76=B_SPLINE_CURVE_WITH_KNOTS('',3,(#11279,#11280,#11281,#11282,#11283,
#11284,#11285,#11286,#11287,#11288,#11289,#11290,#11291,#11292,#11293,#11294,
#11295,#11296,#11297,#11298,#11299,#11300,#11301,#11302,#11303,#11304,#11305,
#11306,#11307,#11308,#11309,#11310,#11311,#11312,#11313,#11314,#11315,#11316,
#11317,#11318,#11319,#11320,#11321,#11322,#11323,#11324,#11325,#11326,#11327,
#11328,#11329,#11330,#11331,#11332,#11333,#11334,#11335,#11336,#11337,#11338,
#11339,#11340,#11341,#11342,#11343,#11344,#11345,#11346,#11347,#11348,#11349,
#11350,#11351,#11352,#11353,#11354,#11355,#11356,#11357,#11358,#11359,#11360,
#11361,#11362,#11363,#11364,#11365,#11366,#11367,#11368,#11369,#11370),
 .UNSPECIFIED.,.F.,.F.,(4,2,2,2,2,2,2,2,2,2,2,2,2,2,2,2,2,2,2,2,2,2,2,2,
2,2,2,2,2,2,2,2,2,2,2,2,2,2,2,2,2,2,2,2,2,4),(-4.06187856554517,-4.01028312517064,
-4.00820489509965,-4.0068923922961,-4.0058928370161,-4.00487275991072,-4.00391515288097,
-4.00259138783777,-3.99920542054684,-3.9525570417565,-3.94657911598626,
-3.88751088390632,-3.84654652891285,-3.84480147835424,-3.84402993595295,
-3.84345941770221,-3.84292550177109,-3.84218492111564,-3.84068664078943,
-3.82688268891551,-3.74615381186573,-3.7159189363492,-3.69966566393637,
-3.68621704629759,-3.68390936706516,-3.68290969500177,-3.68188956907854,
-3.6809321172671,-3.6796088846704,-3.67622598294025,-3.62977230807033,-3.58097983958198,
-3.57477522245894,-3.56738464730999,-3.54128548606904,-3.52895553115468,
-3.5227682477937,-3.5215455595657,-3.52087802652391,-3.5203734036592,-3.51972328912141,
-3.5186097497611,-3.51447447247373,-3.44129701154587,-3.41074387972596,
-3.40057646114791),.UNSPECIFIED.);
#77=B_SPLINE_CURVE_WITH_KNOTS('',3,(#11372,#11373,#11374,#11375,#11376,
#11377,#11378,#11379,#11380,#11381,#11382,#11383,#11384,#11385,#11386,#11387,
#11388,#11389,#11390,#11391,#11392,#11393,#11394,#11395,#11396,#11397,#11398,
#11399,#11400,#11401,#11402,#11403,#11404,#11405,#11406,#11407,#11408,#11409,
#11410,#11411,#11412,#11413,#11414,#11415,#11416,#11417,#11418,#11419,#11420,
#11421,#11422,#11423,#11424,#11425,#11426,#11427,#11428,#11429,#11430,#11431,
#11432,#11433,#11434,#11435,#11436,#11437,#11438,#11439,#11440,#11441,#11442,
#11443,#11444,#11445,#11446,#11447,#11448,#11449,#11450,#11451,#11452,#11453,
#11454,#11455,#11456,#11457,#11458,#11459,#11460,#11461,#11462,#11463,#11464,
#11465,#11466,#11467,#11468,#11469,#11470,#11471,#11472,#11473,#11474,#11475,
#11476,#11477,#11478,#11479,#11480,#11481,#11482,#11483,#11484,#11485),
 .UNSPECIFIED.,.F.,.F.,(4,2,2,2,2,2,2,2,2,2,2,2,2,2,2,2,2,2,2,2,2,2,2,2,
2,2,2,2,2,2,2,2,2,2,2,2,2,2,2,2,2,2,2,2,2,2,2,2,2,2,2,2,2,2,2,2,4),(-0.661978904396988,
-0.627113612311915,-0.625151163231897,-0.62348303709909,-0.62290918167699,
-0.620856007709331,-0.618943009507162,-0.610528516700987,-0.608266312585233,
-0.606925688624173,-0.605904347407471,-0.604962839063766,-0.6034324881459,
-0.599407480486424,-0.593643195553803,-0.577872309154318,-0.542083767646264,
-0.451494885974086,-0.44661902210718,-0.44554068247425,-0.444841586676769,
-0.444280321015988,-0.443634820720731,-0.44251284879718,-0.437813133082642,
-0.396765190853775,-0.361946912313917,-0.34265857858922,-0.312600887769801,
-0.307916047922302,-0.306381113769936,-0.305185331643166,-0.301966963503426,
-0.300776472795027,-0.298770439246987,-0.2972617768537,-0.293642477561785,
-0.286617164155146,-0.284658728239131,-0.283500186979867,-0.282497224578451,
-0.281533106752897,-0.27958565297195,-0.271909090059396,-0.258705282415628,
-0.235142472812011,-0.185650843905423,-0.135759820580576,-0.124318912392373,
-0.12274003009909,-0.122007385789521,-0.121440896279995,-0.120822250592115,
-0.119820473506015,-0.116426053729279,-0.094944610367713,-0.000962465205791075),
 .UNSPECIFIED.);
#78=B_SPLINE_CURVE_WITH_KNOTS('',3,(#11486,#11487,#11488,#11489,#11490,
#11491,#11492,#11493,#11494,#11495,#11496,#11497,#11498,#11499,#11500,#11501,
#11502,#11503,#11504,#11505,#11506,#11507,#11508,#11509,#11510,#11511,#11512,
#11513,#11514,#11515,#11516,#11517,#11518,#11519,#11520,#11521,#11522,#11523,
#11524,#11525,#11526,#11527,#11528,#11529,#11530,#11531,#11532,#11533,#11534,
#11535,#11536,#11537,#11538,#11539,#11540,#11541,#11542,#11543,#11544,#11545,
#11546,#11547,#11548,#11549,#11550,#11551,#11552,#11553,#11554,#11555,#11556,
#11557,#11558,#11559,#11560,#11561,#11562,#11563,#11564,#11565,#11566,#11567,
#11568,#11569,#11570,#11571,#11572,#11573,#11574,#11575,#11576,#11577,#11578,
#11579,#11580,#11581,#11582,#11583,#11584,#11585,#11586,#11587,#11588,#11589,
#11590,#11591,#11592,#11593,#11594,#11595,#11596,#11597,#11598,#11599,#11600,
#11601,#11602,#11603,#11604,#11605,#11606,#11607,#11608,#11609,#11610,#11611,
#11612,#11613,#11614,#11615,#11616,#11617,#11618,#11619,#11620,#11621,#11622,
#11623,#11624,#11625,#11626,#11627,#11628,#11629,#11630,#11631,#11632,#11633,
#11634,#11635,#11636,#11637,#11638,#11639,#11640,#11641,#11642,#11643,#11644,
#11645,#11646,#11647,#11648,#11649,#11650,#11651,#11652,#11653,#11654,#11655,
#11656,#11657,#11658,#11659,#11660,#11661,#11662,#11663,#11664,#11665,#11666,
#11667,#11668,#11669,#11670,#11671,#11672,#11673,#11674,#11675,#11676,#11677,
#11678,#11679,#11680,#11681,#11682,#11683,#11684,#11685,#11686,#11687,#11688,
#11689,#11690,#11691,#11692,#11693),.UNSPECIFIED.,.F.,.F.,(4,2,2,2,2,2,
2,2,2,2,2,2,2,2,2,2,2,2,2,2,2,2,2,2,2,2,2,2,2,2,2,2,2,2,2,2,2,2,2,2,2,2,
2,2,2,2,2,2,2,2,2,2,2,2,2,2,2,2,2,2,2,2,2,2,2,2,2,2,2,2,2,2,2,2,2,2,2,2,
2,2,2,2,2,2,2,2,2,2,2,2,2,2,2,2,2,2,2,2,2,2,2,2,2,4),(-4.06320052515722,
-4.02854659369987,-4.02599157095642,-4.02447993867694,-4.02340400408273,
-4.02246226240333,-4.02144475844287,-4.02012926886495,-4.01729707730144,
-3.99669577433376,-3.99312836322317,-3.98530089655057,-3.97963874261392,
-3.88624641242043,-3.8704720939628,-3.86288476576896,-3.86158897077024,
-3.8609055477264,-3.86035029452704,-3.85969415400662,-3.85855553514836,
-3.8541705904117,-3.85152464773105,-3.84994677000181,-3.84859115908881,
-3.75448400553711,-3.73323402184924,-3.71332681142404,-3.70286602615713,
-3.70071681448195,-3.69973324466078,-3.69876000633362,-3.69779226512787,
-3.69643140569658,-3.6936195848049,-3.66387448893644,-3.61235814755693,
-3.60669416211047,-3.60022607679449,-3.59270528889197,-3.54058024380383,
-3.53874399284793,-3.53795603208496,-3.53738251282187,-3.53685251236143,
-3.53612733400141,-3.53469069499509,-3.52282235557942,-3.4500196497108,
-3.41731444533606,-3.39305972575065,-3.38451997204443,-3.38086718866179,
-3.37891645798891,-3.37724671847994,-3.37617286166545,-3.37515480795055,
-3.37383603810287,-3.37098673137131,-3.34995425528351,-3.34772134843608,
-3.26007371048579,-3.24805499743998,-3.22583736628036,-3.21672609650072,
-3.21536768741551,-3.21467111370844,-3.21410988571839,-3.21346220395574,
-3.2123599241163,-3.20833776362933,-3.14026803353591,-3.09383598516356,
-3.06930428855282,-3.06114459270299,-3.05761346013487,-3.05490057619976,
-3.05359939075846,-3.05263339336126,-3.05167625924942,-3.05035532632213,
-3.04698823597713,-3.00171040552554,-2.95208950291395,-2.89643105074264,
-2.89301061865856,-2.89200587526018,-2.89138646188723,-2.89082000728871,
-2.89008841060147,-2.88851563696069,-2.87723505703119,-2.87498944770347,
-2.87402207025079,-2.79055858921925,-2.73577857512061,-2.73331283961937,
-2.7318380947509,-2.7305058327933,-2.72950310380974,-2.72854969004676,-2.72724288730549,
-2.72395893684818,-2.69352985927485),.UNSPECIFIED.);
#79=B_SPLINE_CURVE_WITH_KNOTS('',3,(#11698,#11699,#11700,#11701,#11702,
#11703,#11704,#11705,#11706,#11707,#11708,#11709,#11710,#11711,#11712,#11713,
#11714,#11715,#11716,#11717,#11718,#11719,#11720,#11721,#11722,#11723,#11724,
#11725,#11726,#11727,#11728,#11729,#11730,#11731,#11732,#11733,#11734,#11735,
#11736,#11737,#11738,#11739,#11740,#11741,#11742,#11743,#11744,#11745,#11746,
#11747,#11748,#11749,#11750,#11751,#11752,#11753,#11754,#11755,#11756,#11757,
#11758,#11759,#11760,#11761,#11762,#11763,#11764,#11765,#11766,#11767,#11768,
#11769,#11770,#11771,#11772,#11773,#11774,#11775,#11776,#11777,#11778,#11779,
#11780,#11781,#11782,#11783,#11784,#11785,#11786,#11787,#11788,#11789,#11790,
#11791,#11792,#11793,#11794,#11795,#11796,#11797,#11798,#11799,#11800,#11801,
#11802,#11803,#11804,#11805,#11806,#11807,#11808,#11809,#11810,#11811,#11812,
#11813,#11814,#11815,#11816,#11817,#11818,#11819,#11820,#11821,#11822,#11823,
#11824,#11825,#11826,#11827,#11828,#11829,#11830,#11831,#11832,#11833,#11834,
#11835,#11836,#11837,#11838,#11839,#11840,#11841,#11842,#11843,#11844,#11845,
#11846,#11847,#11848,#11849,#11850,#11851,#11852,#11853,#11854,#11855,#11856,
#11857,#11858,#11859,#11860,#11861,#11862,#11863,#11864,#11865,#11866,#11867,
#11868,#11869,#11870,#11871,#11872,#11873,#11874,#11875,#11876,#11877,#11878,
#11879,#11880,#11881,#11882,#11883,#11884,#11885,#11886,#11887,#11888,#11889,
#11890,#11891,#11892,#11893,#11894,#11895,#11896,#11897,#11898,#11899,#11900,
#11901,#11902,#11903,#11904,#11905,#11906,#11907,#11908,#11909,#11910,#11911,
#11912,#11913,#11914,#11915,#11916,#11917,#11918,#11919,#11920,#11921,#11922,
#11923,#11924,#11925,#11926,#11927,#11928,#11929,#11930,#11931,#11932,#11933,
#11934,#11935,#11936,#11937,#11938,#11939,#11940,#11941,#11942,#11943,#11944,
#11945,#11946,#11947,#11948,#11949,#11950,#11951,#11952,#11953,#11954,#11955,
#11956,#11957,#11958,#11959,#11960,#11961,#11962,#11963,#11964,#11965,#11966,
#11967,#11968,#11969,#11970,#11971,#11972,#11973,#11974,#11975,#11976,#11977,
#11978,#11979,#11980,#11981,#11982,#11983,#11984,#11985,#11986,#11987,#11988,
#11989,#11990,#11991,#11992,#11993,#11994,#11995,#11996,#11997,#11998,#11999),
 .UNSPECIFIED.,.F.,.F.,(4,2,2,2,2,2,2,2,2,2,2,2,2,2,2,2,2,2,2,2,2,2,2,2,
2,2,2,2,2,2,2,2,2,2,2,2,2,2,2,2,2,2,2,2,2,2,2,2,2,2,2,2,2,2,2,2,2,2,2,2,
2,2,2,2,2,2,2,2,2,2,2,2,2,2,2,2,2,2,2,2,2,2,2,2,2,2,2,2,2,2,2,2,2,2,2,2,
2,2,2,2,2,2,2,2,2,2,2,2,2,2,2,2,2,2,2,2,2,2,2,2,2,2,2,2,2,2,2,2,2,2,2,2,
2,2,2,2,2,2,2,2,2,2,2,2,2,2,2,2,2,2,4),(-3.39969022993959,-3.3786984878877,
-3.35948849290766,-3.34588685838186,-3.34066440146017,-3.33741257346593,
-3.33667800306114,-3.33599027095376,-3.33542991438605,-3.33486178715339,
-3.33380349977984,-3.33029044840005,-3.27407115351213,-3.23037848365561,
-3.19417663529458,-3.1785634569545,-3.17617159355712,-3.17491717091749,
-3.17400575597167,-3.17303227208262,-3.1716490720901,-3.16789482769006,
-3.1111685143221,-3.04883083834845,-3.01879730840282,-3.01469228204835,
-3.01361069668949,-3.01297432080491,-3.01241208527157,-3.01170007109684,
-3.01057962584175,-3.00803289862645,-2.95743123880408,-2.89036843290398,
-2.88079374861989,-2.85644449364307,-2.85354392084936,-2.85218550142441,
-2.85116523679675,-2.85020843480577,-2.84888733181381,-2.84551645678593,
-2.79985844443754,-2.72383796005469,-2.70139477583681,-2.69224033718215,
-2.69088518689225,-2.69018377698549,-2.68967584873648,-2.68912875353269,
-2.68833957542714,-2.68612486896696,-2.65176470822932,-2.57959614065157,
-2.55146179005225,-2.53912698298267,-2.53183584758135,-2.5299242234798,
-2.5287790683472,-2.52777253658323,-2.52652335916783,-2.52460876611352,
-2.51610554048112,-2.42034506873497,-2.39568997735949,-2.37218284936963,
-2.36981326432523,-2.36809663853903,-2.36730595152729,-2.36673211313041,
-2.36620303475001,-2.36548090202363,-2.36405566770089,-2.35250576326666,
-2.34899396760495,-2.25827081396586,-2.22885301940535,-2.20975161615233,
-2.20722801904973,-2.20595975867361,-2.20504637292322,-2.20407831055815,
-2.2027152019381,-2.19989289495155,-2.19231065962865,-2.19049665751667,
-2.18843335879618,-2.1879774800841,-2.18595995267805,-2.1842444171534,-2.18005147146979,
-2.17600593781256,-2.13071837941265,-2.0491810894737,-2.04555416463119,
-2.04452818154351,-2.04390419560876,-2.04333935203872,-2.042617587916,-2.04109496590049,
-2.0309832034178,-2.0038184010449,-1.91302938216084,-1.90676618036601,-1.90509849742528,
-1.90388230575305,-1.90277294404895,-1.88685573810697,-1.88423103243504,
-1.88294229078672,-1.88193175961283,-1.8808110993466,-1.87897010541056,
-1.87246659847572,-1.83119558278224,-1.7468639512005,-1.74290785871373,
-1.74173322294893,-1.73871648379443,-1.72360881608827,-1.72207368100775,
-1.72132394702616,-1.72078759294804,-1.72027546718284,-1.71954576601438,
-1.71802253485886,-1.70231312007715,-1.68480950659857,-1.56814511771077,
-1.56227450805133,-1.56042673025002,-1.55941684969971,-1.55841184490607,
-1.55720811082083,-1.55496048900531,-1.55215631988702,-1.53205293842959,
-1.4953197925989,-1.42967105561337,-1.41926180505218,-1.41767793565167,
-1.4168456357559,-1.40051394412944,-1.39894702510061,-1.39818954967374,
-1.3976511820023,-1.39714015844877,-1.3964168464538,-1.39492552270816,-1.3809138042181,
-1.36955217660447),.UNSPECIFIED.);
#80=B_SPLINE_CURVE_WITH_KNOTS('',3,(#12000,#12001,#12002,#12003,#12004,
#12005,#12006,#12007,#12008,#12009,#12010,#12011,#12012,#12013,#12014,#12015,
#12016,#12017,#12018,#12019,#12020,#12021,#12022,#12023,#12024,#12025,#12026,
#12027,#12028,#12029,#12030,#12031,#12032,#12033,#12034,#12035,#12036,#12037,
#12038,#12039,#12040,#12041,#12042,#12043,#12044,#12045,#12046,#12047,#12048,
#12049,#12050,#12051,#12052,#12053,#12054,#12055,#12056,#12057,#12058,#12059,
#12060,#12061,#12062,#12063,#12064,#12065,#12066,#12067,#12068,#12069,#12070,
#12071,#12072,#12073,#12074,#12075,#12076,#12077,#12078,#12079,#12080,#12081,
#12082,#12083,#12084,#12085,#12086,#12087,#12088,#12089,#12090,#12091,#12092,
#12093,#12094,#12095,#12096,#12097,#12098,#12099,#12100,#12101,#12102,#12103,
#12104,#12105,#12106,#12107,#12108,#12109,#12110,#12111,#12112,#12113,#12114,
#12115,#12116,#12117,#12118,#12119,#12120,#12121,#12122,#12123,#12124,#12125,
#12126,#12127,#12128,#12129,#12130,#12131,#12132,#12133,#12134,#12135,#12136,
#12137,#12138,#12139,#12140,#12141,#12142,#12143,#12144,#12145,#12146,#12147,
#12148,#12149,#12150,#12151,#12152,#12153,#12154,#12155,#12156,#12157,#12158,
#12159,#12160,#12161,#12162,#12163,#12164,#12165,#12166,#12167,#12168,#12169,
#12170,#12171,#12172,#12173,#12174,#12175,#12176,#12177,#12178,#12179,#12180,
#12181,#12182,#12183,#12184,#12185,#12186,#12187,#12188,#12189,#12190,#12191,
#12192,#12193,#12194,#12195,#12196,#12197,#12198,#12199,#12200,#12201,#12202,
#12203,#12204,#12205,#12206,#12207,#12208,#12209,#12210,#12211,#12212,#12213,
#12214,#12215,#12216,#12217,#12218,#12219,#12220,#12221,#12222,#12223,#12224,
#12225,#12226,#12227,#12228,#12229,#12230,#12231,#12232,#12233,#12234,#12235,
#12236,#12237,#12238,#12239,#12240,#12241,#12242,#12243,#12244,#12245,#12246,
#12247,#12248,#12249,#12250,#12251,#12252,#12253,#12254,#12255,#12256,#12257),
 .UNSPECIFIED.,.F.,.F.,(4,2,2,2,2,2,2,2,2,2,2,2,2,2,2,2,2,2,2,2,2,2,2,2,
2,2,2,2,2,2,2,2,2,2,2,2,2,2,2,2,2,2,2,2,2,2,2,2,2,2,2,2,2,2,2,2,2,2,2,2,
2,2,2,2,2,2,2,2,2,2,2,2,2,2,2,2,2,2,2,2,2,2,2,2,2,2,2,2,2,2,2,2,2,2,2,2,
2,2,2,2,2,2,2,2,2,2,2,2,2,2,2,2,2,2,2,2,2,2,2,2,2,2,2,2,2,2,2,2,4),(-2.69352985927485,
-2.68389408092132,-2.60895562576247,-2.57442617333315,-2.57001717621488,
-2.56891863774995,-2.56827823318252,-2.56771617440436,-2.56700928507732,
-2.56590617795353,-2.56117999440359,-2.46394710576004,-2.41681557895182,
-2.41220764718302,-2.40989587106581,-2.40848521826122,-2.40719934367583,
-2.40620397129558,-2.40523627289003,-2.4038755451556,-2.40106422809616,
-2.37133936304647,-2.3603291951398,-2.3343502247734,-2.31454743131305,-2.27191343437527,
-2.25012374099055,-2.246699990916,-2.24569497922519,-2.24507555973505,-2.24450920989543,
-2.24377789824917,-2.24256862938517,-2.23804864061365,-2.14719133378575,
-2.08851797323181,-2.08553160793023,-2.08417263674111,-2.0831519485819,
-2.0821947427239,-2.08087307150257,-2.07750068975277,-2.03181498087369,
-1.98056479987243,-1.92702006997968,-1.92363794576221,-1.92259502376976,
-1.92202982800443,-1.92152501194605,-1.92085668661933,-1.91963091765707,
-1.91339528336818,-1.90093649743885,-1.87739211464657,-1.76965303694037,
-1.76349706667714,-1.7616140385948,-1.76059684980213,-1.7595920855993,-1.75837477271154,
-1.75609539301282,-1.74339496883304,-1.71859441017217,-1.62915304762118,
-1.60187371291614,-1.59994212688075,-1.59919663265854,-1.59866134308105,
-1.59810283215021,-1.59735829862927,-1.59653133042307,-1.59514148102259,
-1.56367441790498,-1.44590148758449,-1.44010022486342,-1.43826091523625,
-1.43725261591757,-1.43624723253123,-1.43501548018086,-1.43266774869513,
-1.41849163181968,-1.3882140135813,-1.33839842020177,-1.28083526847851,
-1.27723866545663,-1.27617050602013,-1.27560032105911,-1.27505170089691,
-1.27438590571161,-1.2736687765961,-1.2725425666678,-1.27039683871987,-1.25054747273822,
-1.23743471056791,-1.16003570544902,-1.14806361545362,-1.11924620331764,
-1.11618834952474,-1.11493276805087,-1.11399259596314,-1.11295992814161,
-1.11153072021232,-1.10815124861225,-1.10355545695711,-1.05663818122653,
-0.965110746092647,-0.954966681861803,-0.953442507424782,-0.952720396319068,
-0.952168323258122,-0.951560783861697,-0.950586321666152,-0.949432248676162,
-0.947213137913438,-0.941815696279655,-0.925302507687756,-0.901010654267849,
-0.835269718565094,-0.819460834165034,-0.81687248291935,-0.795845331885353,
-0.792996734735651,-0.79167830333446,-0.790660514890877,-0.789564917209215,
-0.787836700103267,-0.782363986452277,-0.690580316824922,-0.662566381801328),
 .UNSPECIFIED.);
#81=B_SPLINE_CURVE_WITH_KNOTS('',3,(#12263,#12264,#12265,#12266,#12267,
#12268,#12269,#12270,#12271,#12272,#12273,#12274,#12275,#12276,#12277,#12278,
#12279,#12280,#12281,#12282,#12283,#12284,#12285,#12286,#12287,#12288,#12289,
#12290,#12291,#12292,#12293,#12294,#12295,#12296,#12297,#12298,#12299,#12300,
#12301,#12302,#12303,#12304,#12305,#12306,#12307,#12308,#12309,#12310,#12311,
#12312,#12313,#12314,#12315,#12316,#12317,#12318,#12319,#12320,#12321,#12322,
#12323,#12324,#12325,#12326,#12327,#12328,#12329,#12330,#12331,#12332,#12333,
#12334,#12335,#12336,#12337,#12338,#12339,#12340,#12341,#12342,#12343,#12344,
#12345,#12346,#12347,#12348,#12349,#12350,#12351,#12352,#12353,#12354,#12355,
#12356,#12357,#12358,#12359,#12360,#12361,#12362,#12363,#12364,#12365,#12366,
#12367,#12368,#12369,#12370,#12371,#12372,#12373,#12374,#12375,#12376,#12377,
#12378,#12379,#12380,#12381,#12382,#12383,#12384,#12385,#12386,#12387,#12388,
#12389,#12390,#12391,#12392,#12393,#12394,#12395,#12396,#12397,#12398,#12399,
#12400,#12401,#12402,#12403,#12404,#12405,#12406,#12407,#12408,#12409,#12410,
#12411,#12412,#12413,#12414,#12415,#12416,#12417,#12418,#12419,#12420,#12421,
#12422,#12423,#12424,#12425,#12426,#12427,#12428,#12429,#12430,#12431,#12432,
#12433,#12434,#12435,#12436,#12437,#12438,#12439,#12440,#12441,#12442,#12443,
#12444,#12445,#12446,#12447,#12448,#12449,#12450,#12451,#12452,#12453,#12454,
#12455,#12456,#12457,#12458,#12459,#12460,#12461,#12462,#12463,#12464,#12465,
#12466,#12467,#12468,#12469,#12470,#12471,#12472),.UNSPECIFIED.,.F.,.F.,
(4,2,2,2,2,2,2,2,2,2,2,2,2,2,2,2,2,2,2,2,2,2,2,2,2,2,2,2,2,2,2,2,2,2,2,
2,2,2,2,2,2,2,2,2,2,2,2,2,2,2,2,2,2,2,2,2,2,2,2,2,2,2,2,2,2,2,2,2,2,2,2,
2,2,2,2,2,2,2,2,2,2,2,2,2,2,2,2,2,2,2,2,2,2,2,2,2,2,2,2,2,2,2,2,2,4),(-1.3700182626362,
-1.36592562693376,-1.32703128660657,-1.25909429378232,-1.21787961320516,
-1.21546755798024,-1.21464948497662,-1.21409426026938,-1.21358817863959,
-1.2129032860087,-1.21162585450702,-1.20478274722828,-1.19054162214828,
-1.16723812606352,-1.10697677551043,-1.08480759494741,-1.07677163629666,
-1.07532377515967,-1.07410481494186,-1.07233361323219,-1.07025749908928,
-1.06713614545577,-1.06401195172129,-1.05616817902585,-1.05412729849195,
-1.05294968001654,-1.05204570821936,-1.05087779711243,-1.04886631659573,
-1.04039844011434,-1.01159811942756,-0.949868610417787,-0.90669708736391,
-0.906325899185845,-0.905417407009432,-0.893732973258678,-0.892165068910575,
-0.891423391432866,-0.890855583658289,-0.890241302265071,-0.889258754608297,
-0.88611724013485,-0.843727933985025,-0.79642093626542,-0.735959297627083,
-0.732167039801404,-0.730777755800238,-0.729802464698541,-0.72889132704975,
-0.727640345236682,-0.725249884435287,-0.709843293116012,-0.69029644310253,
-0.636374030976765,-0.592576630663127,-0.585624928757988,-0.584158212509357,
-0.582852244954422,-0.570808925093855,-0.56920707694905,-0.568470162594901,
-0.567903102066476,-0.567286649447224,-0.566294379877547,-0.563058952118846,
-0.533504230194774,-0.484529409184136,-0.413772855735669,-0.409410560106277,
-0.407773411133712,-0.406805491487863,-0.405891890800374,-0.40462277712555,
-0.403260255069271,-0.396705220210389,-0.385968489064426,-0.347295834274742,
-0.318840352571299,-0.277563615076129,-0.269436645821019,-0.265370862260202,
-0.264340778134366,-0.262008173980406,-0.259906803819862,-0.24787069071717,
-0.246269174766381,-0.24553234569493,-0.244965321982282,-0.244348879722596,
-0.243356564352854,-0.24219154956837,-0.228381061006591,-0.193047608999555,
-0.179385784785977,-0.165160845705691,-0.0914217283366651,-0.0897382975120328,
-0.0861859627833301,-0.0848347804093064,-0.0838698861247194,-0.0829551577119613,
-0.0816781069745883,-0.0803045910796622,-0.0780811396084523,-0.000961462500411059),
 .UNSPECIFIED.);
#82=B_SPLINE_CURVE_WITH_KNOTS('',3,(#12473,#12474,#12475,#12476,#12477,
#12478,#12479,#12480,#12481,#12482,#12483,#12484,#12485,#12486,#12487,#12488,
#12489,#12490,#12491,#12492,#12493,#12494,#12495,#12496,#12497,#12498,#12499,
#12500,#12501,#12502,#12503,#12504,#12505,#12506,#12507,#12508,#12509,#12510,
#12511,#12512,#12513,#12514,#12515,#12516,#12517,#12518,#12519,#12520,#12521,
#12522,#12523,#12524,#12525,#12526,#12527,#12528,#12529,#12530,#12531,#12532,
#12533,#12534,#12535,#12536,#12537,#12538,#12539,#12540,#12541,#12542,#12543,
#12544,#12545,#12546,#12547,#12548,#12549,#12550,#12551,#12552,#12553,#12554,
#12555,#12556,#12557,#12558,#12559,#12560,#12561,#12562,#12563,#12564),
 .UNSPECIFIED.,.F.,.F.,(4,2,2,2,2,2,2,2,2,2,2,2,2,2,2,2,2,2,2,2,2,2,2,2,
2,2,2,2,2,2,2,2,2,2,2,2,2,2,2,2,2,2,2,2,2,4),(-4.06035618685406,-3.99361167849707,
-3.98439999022834,-3.98322214866527,-3.98248341448087,-3.98179268930348,
-3.98123216837419,-3.98058076863918,-3.97946144696294,-3.97526766961926,
-3.90378714042804,-3.89074774847312,-3.8781122663538,-3.84219985006292,
-3.82546256057995,-3.82330259771421,-3.82195579736669,-3.82069809982943,
-3.81978625098544,-3.81881413273403,-3.81715495200595,-3.81264863723276,
-3.74278858558718,-3.71703578795096,-3.68974695454361,-3.66956640223594,
-3.66384816204599,-3.66036248865856,-3.65961238107755,-3.65891347862774,
-3.65835241515155,-3.65770720013465,-3.6566143936515,-3.65267846424478,
-3.58488437228641,-3.53713831131176,-3.50614519376003,-3.50030166824999,
-3.49898555618717,-3.49775003070747,-3.49684099707044,-3.49585916066768,
-3.49444560403126,-3.49049260806214,-3.42563801691695,-3.39969022993959),
 .UNSPECIFIED.);
#83=B_SPLINE_CURVE_WITH_KNOTS('',3,(#12566,#12567,#12568,#12569,#12570,
#12571,#12572,#12573,#12574,#12575,#12576,#12577,#12578,#12579,#12580,#12581,
#12582,#12583,#12584,#12585,#12586,#12587,#12588,#12589,#12590,#12591,#12592,
#12593,#12594,#12595,#12596,#12597,#12598,#12599,#12600,#12601,#12602,#12603,
#12604,#12605,#12606,#12607,#12608,#12609,#12610,#12611,#12612,#12613,#12614,
#12615,#12616,#12617,#12618,#12619,#12620,#12621,#12622,#12623,#12624,#12625,
#12626,#12627,#12628,#12629,#12630,#12631,#12632,#12633,#12634,#12635,#12636,
#12637,#12638,#12639,#12640,#12641,#12642,#12643,#12644,#12645,#12646,#12647,
#12648,#12649,#12650,#12651,#12652,#12653,#12654,#12655),.UNSPECIFIED.,
 .F.,.F.,(4,2,2,2,2,2,2,2,2,2,2,2,2,2,2,2,2,2,2,2,2,2,2,2,2,2,2,2,2,2,2,
2,2,2,2,2,2,2,2,2,2,2,2,2,4),(-0.662566381801328,-0.642307042402579,-0.631927247965306,
-0.630545453535587,-0.629834389016777,-0.629308056282692,-0.628743230621758,
-0.627963160501452,-0.627086856245606,-0.625576482979552,-0.622372085393098,
-0.613477033548835,-0.593317933234046,-0.47687922138088,-0.470865665074005,
-0.469000027277596,-0.467986425240083,-0.466981540872009,-0.465758797128514,
-0.463453519228134,-0.450214186112101,-0.429788140307287,-0.376603389375201,
-0.352555446920475,-0.310102493005206,-0.307662135184486,-0.306840102703051,
-0.306283784139431,-0.305730622929776,-0.305039438187828,-0.303775956894423,
-0.302135288918424,-0.298549825141854,-0.288178350049604,-0.257620541822341,
-0.154107817669735,-0.147874941188741,-0.145983065491394,-0.144964276040553,
-0.143969534392672,-0.142759728502392,-0.140514393987957,-0.128469004090863,
-0.104709114538698,-0.000962379493694885),.UNSPECIFIED.);
#84=B_SPLINE_CURVE_WITH_KNOTS('',3,(#12656,#12657,#12658,#12659,#12660,
#12661,#12662,#12663,#12664,#12665,#12666,#12667,#12668,#12669,#12670,#12671,
#12672,#12673,#12674,#12675,#12676,#12677,#12678,#12679,#12680,#12681,#12682,
#12683,#12684,#12685,#12686,#12687,#12688,#12689,#12690,#12691,#12692,#12693,
#12694,#12695,#12696,#12697,#12698,#12699,#12700,#12701,#12702,#12703,#12704,
#12705,#12706,#12707,#12708,#12709,#12710,#12711,#12712,#12713,#12714,#12715,
#12716,#12717,#12718,#12719,#12720,#12721,#12722,#12723,#12724,#12725,#12726,
#12727,#12728,#12729,#12730,#12731,#12732,#12733,#12734,#12735,#12736,#12737,
#12738,#12739,#12740,#12741,#12742,#12743,#12744,#12745,#12746,#12747,#12748,
#12749,#12750,#12751,#12752,#12753,#12754,#12755,#12756,#12757,#12758,#12759,
#12760,#12761,#12762,#12763,#12764,#12765,#12766,#12767,#12768,#12769,#12770,
#12771,#12772,#12773,#12774,#12775,#12776,#12777,#12778,#12779,#12780,#12781,
#12782,#12783,#12784,#12785,#12786,#12787,#12788,#12789,#12790,#12791,#12792,
#12793,#12794,#12795,#12796,#12797,#12798,#12799,#12800,#12801,#12802,#12803,
#12804,#12805,#12806,#12807,#12808,#12809,#12810,#12811,#12812,#12813,#12814,
#12815,#12816,#12817,#12818,#12819,#12820,#12821,#12822,#12823,#12824,#12825,
#12826,#12827,#12828,#12829,#12830,#12831,#12832,#12833,#12834,#12835,#12836,
#12837,#12838,#12839,#12840,#12841,#12842,#12843,#12844,#12845,#12846,#12847,
#12848,#12849,#12850,#12851,#12852,#12853,#12854,#12855,#12856,#12857,#12858,
#12859,#12860,#12861,#12862,#12863,#12864,#12865,#12866,#12867,#12868,#12869,
#12870,#12871),.UNSPECIFIED.,.F.,.F.,(4,2,2,2,2,2,2,2,2,2,2,2,2,2,2,2,2,
2,2,2,2,2,2,2,2,2,2,2,2,2,2,2,2,2,2,2,2,2,2,2,2,2,2,2,2,2,2,2,2,2,2,2,2,
2,2,2,2,2,2,2,2,2,2,2,2,2,2,2,2,2,2,2,2,2,2,2,2,2,2,2,2,2,2,2,2,2,2,2,2,
2,2,2,2,2,2,2,2,2,2,2,2,2,2,2,2,2,2,4),(-4.06047319610046,-4.04534584298061,
-4.04416539400911,-4.04342571802198,-4.04286616394116,-4.04233217020568,
-4.04180297221772,-4.04107932890953,-4.03964705149221,-4.02786985803002,
-4.0262296518368,-4.02273295415447,-3.93530219498073,-3.90496108430936,
-3.88551862057472,-3.88298665323852,-3.88171726745532,-3.88080428751781,
-3.87983778136405,-3.87847870528836,-3.87567072018144,-3.84597591307066,
-3.75834525501736,-3.74511926195674,-3.72942328193803,-3.72446010513923,
-3.7223747566678,-3.72127184208784,-3.72033338154978,-3.71973421294788,
-3.71917838645758,-3.71843917992707,-3.71720182332762,-3.70991742469021,
-3.65693198605897,-3.65171157372666,-3.64580315825785,-3.63901498916356,
-3.63106046243552,-3.62145481653966,-3.56675865525092,-3.56134919016542,
-3.5596294281448,-3.55853631809543,-3.55751883756009,-3.55619796928395,
-3.55333293238161,-3.53181712534797,-3.51438522036448,-3.51335591294048,
-3.43487651601576,-3.42175414833139,-3.40648152019466,-3.40167102851742,
-3.39963319065503,-3.39854848198509,-3.39784895002736,-3.39722245491491,
-3.39667359783532,-3.39610292231898,-3.39503112368044,-3.3913990297126,
-3.39034561572905,-3.30815746727068,-3.29739957779183,-3.28438570763044,
-3.25393966719276,-3.23973628797277,-3.23738856875607,-3.23615732533456,
-3.23515261322027,-3.2341452008143,-3.23230811804009,-3.22651846056045,
-3.10872130567222,-3.08564326288441,-3.07945647921663,-3.07700285920929,
-3.07576136466618,-3.07499607997045,-3.07431450390968,-3.07376151595188,
-3.07321463287533,-3.07226141163202,-3.06955450193642,-3.02624149133466,
-3.00985954781861,-2.96046465672555,-2.91803799525615,-2.91486242600556,
-2.91346939124196,-2.91244353904541,-2.91149600520922,-2.91021004927341,
-2.90769439567261,-2.88798357653557,-2.88168747283358,-2.80433381257472,
-2.75603059941067,-2.75390269102062,-2.75278338950051,-2.7520692484402,
-2.75140592379423,-2.75085691570476,-2.75028550288771,-2.74921062600865,
-2.7455534977854,-2.6924050095202),.UNSPECIFIED.);
#85=B_SPLINE_CURVE_WITH_KNOTS('',3,(#12876,#12877,#12878,#12879,#12880,
#12881,#12882,#12883,#12884,#12885,#12886,#12887,#12888,#12889,#12890,#12891,
#12892,#12893,#12894,#12895,#12896,#12897,#12898,#12899,#12900,#12901,#12902,
#12903,#12904,#12905,#12906,#12907,#12908,#12909,#12910,#12911,#12912,#12913,
#12914,#12915,#12916,#12917,#12918,#12919,#12920,#12921,#12922,#12923,#12924,
#12925,#12926,#12927,#12928,#12929,#12930,#12931,#12932,#12933,#12934,#12935,
#12936,#12937,#12938,#12939,#12940,#12941,#12942,#12943,#12944,#12945,#12946,
#12947,#12948,#12949,#12950,#12951,#12952,#12953,#12954,#12955,#12956,#12957,
#12958,#12959,#12960,#12961,#12962,#12963,#12964,#12965,#12966,#12967,#12968,
#12969,#12970,#12971,#12972,#12973,#12974,#12975,#12976,#12977,#12978,#12979,
#12980,#12981,#12982,#12983,#12984,#12985,#12986,#12987,#12988,#12989,#12990,
#12991,#12992,#12993,#12994,#12995,#12996,#12997,#12998,#12999,#13000,#13001,
#13002,#13003,#13004,#13005,#13006,#13007,#13008,#13009,#13010,#13011,#13012,
#13013,#13014,#13015,#13016,#13017,#13018,#13019,#13020,#13021,#13022,#13023,
#13024,#13025,#13026,#13027,#13028,#13029,#13030,#13031,#13032,#13033,#13034,
#13035,#13036,#13037,#13038,#13039,#13040,#13041,#13042,#13043,#13044,#13045,
#13046,#13047,#13048,#13049,#13050,#13051,#13052,#13053,#13054,#13055,#13056,
#13057,#13058,#13059,#13060,#13061,#13062,#13063,#13064,#13065,#13066,#13067,
#13068,#13069,#13070,#13071,#13072,#13073,#13074,#13075,#13076,#13077,#13078,
#13079,#13080,#13081,#13082,#13083,#13084,#13085,#13086,#13087,#13088,#13089,
#13090,#13091,#13092,#13093,#13094,#13095,#13096,#13097,#13098,#13099,#13100,
#13101,#13102,#13103,#13104,#13105,#13106,#13107,#13108,#13109,#13110,#13111,
#13112,#13113,#13114,#13115,#13116,#13117,#13118,#13119,#13120,#13121,#13122,
#13123,#13124,#13125,#13126,#13127,#13128,#13129,#13130,#13131,#13132,#13133,
#13134,#13135,#13136,#13137,#13138,#13139,#13140,#13141,#13142,#13143,#13144,
#13145,#13146,#13147,#13148,#13149,#13150,#13151,#13152,#13153,#13154,#13155,
#13156,#13157,#13158,#13159,#13160,#13161,#13162,#13163,#13164,#13165,#13166,
#13167),.UNSPECIFIED.,.F.,.F.,(4,2,2,2,2,2,2,2,2,2,2,2,2,2,2,2,2,2,2,2,
2,2,2,2,2,2,2,2,2,2,2,2,2,2,2,2,2,2,2,2,2,2,2,2,2,2,2,2,2,2,2,2,2,2,2,2,
2,2,2,2,2,2,2,2,2,2,2,2,2,2,2,2,2,2,2,2,2,2,2,2,2,2,2,2,2,2,2,2,2,2,2,2,
2,2,2,2,2,2,2,2,2,2,2,2,2,2,2,2,2,2,2,2,2,2,2,2,2,2,2,2,2,2,2,2,2,2,2,2,
2,2,2,2,2,2,2,2,2,2,2,2,2,2,2,2,2,4),(-3.39963798704962,-3.3801463624031,
-3.33503323920271,-3.31747483966743,-3.31498860782002,-3.31372820042422,
-3.31281609888343,-3.31184531483645,-3.3101923769096,-3.30572577982014,
-3.23578479200766,-3.19718455641332,-3.16541403173404,-3.15412338052256,
-3.15270150731027,-3.15212963486832,-3.15155394251863,-3.15102749152131,
-3.15031520774104,-3.14892793874885,-3.13839446348343,-3.1365083456454,
-3.1355832342568,-3.13412120005603,-3.11027876147053,-3.04140611119487,
-3.00000319293854,-2.99348740885993,-2.99164549279878,-2.9905248184623,
-2.98951462919597,-2.98822681126885,-2.98560567867272,-2.9773442356549,
-2.97586363935894,-2.97448427771589,-2.97213428695755,-2.97007180630593,
-2.96835338791431,-2.96715148591709,-2.9654647030675,-2.95822543174843,
-2.93329148827552,-2.88200765458009,-2.83254193996605,-2.83027173378525,
-2.82941336621256,-2.82882263855469,-2.82824911811561,-2.82755714495274,
-2.82582678866122,-2.80983706645041,-2.8028903314239,-2.72639022844628,
-2.68792343573436,-2.67171269761921,-2.66927301641488,-2.66802226850856,
-2.66711149323465,-2.66613677203362,-2.66474860313483,-2.6609612565459,
-2.60026563696323,-2.51140709835283,-2.50893300242785,-2.50712520641222,
-2.50634488924346,-2.50577010993714,-2.5052424755221,-2.50452567253001,
-2.50312096632339,-2.49213091847282,-2.49109047059713,-2.40545604696581,
-2.35100639651447,-2.34697619345248,-2.34544191327064,-2.3443886510429,
-2.34335972021447,-2.34212329769835,-2.33905431486547,-2.31127975027033,
-2.2217148279477,-2.18601475110079,-2.18412392317036,-2.1833267571815,-2.18275181345288,
-2.18222432256387,-2.18150814089206,-2.18010591665074,-2.16918354718316,
-2.1658631395019,-2.16545353103077,-2.16263341147185,-2.1608514978219,-2.15902128399188,
-2.12316188851408,-2.07229719421697,-2.03118377265546,-2.02482385120089,
-2.02291701539089,-2.02178167954957,-2.02087468505537,-2.01965817915969,
-2.01738162394926,-2.00472874048174,-1.97995857104196,-1.89085274533575,
-1.86319994536807,-1.86126286456821,-1.86051658610009,-1.85998118146519,
-1.85941161750617,-1.85864563128774,-1.85693088564842,-1.81478627941541,
-1.7621476763672,-1.70487425613477,-1.70108226061158,-1.69969310680157,
-1.69871791772339,-1.69780688383685,-1.69655605759408,-1.69433108046041,
-1.69146228328892,-1.67054178538779,-1.64795565705583,-1.56603769255167,
-1.54017868939998,-1.53827039839572,-1.53752885577601,-1.53699468089012,
-1.53642431052022,-1.53565368344678,-1.53406491830582,-1.52042369118033,
-1.49436519595056,-1.4161911279273,-1.38099170084747,-1.37780306017645,
-1.37651298043796,-1.37556413751083,-1.37453852831644,-1.37314876494592,
-1.37006446976188,-1.3700182626362),.UNSPECIFIED.);
#86=B_SPLINE_CURVE_WITH_KNOTS('',3,(#13168,#13169,#13170,#13171,#13172,
#13173,#13174,#13175,#13176,#13177,#13178,#13179,#13180,#13181,#13182,#13183,
#13184,#13185,#13186,#13187,#13188,#13189,#13190,#13191,#13192,#13193,#13194,
#13195,#13196,#13197,#13198,#13199,#13200,#13201,#13202,#13203,#13204,#13205,
#13206,#13207,#13208,#13209,#13210,#13211,#13212,#13213,#13214,#13215,#13216,
#13217,#13218,#13219,#13220,#13221,#13222,#13223,#13224,#13225,#13226,#13227,
#13228,#13229,#13230,#13231,#13232,#13233,#13234,#13235,#13236,#13237,#13238,
#13239,#13240,#13241,#13242,#13243,#13244,#13245,#13246,#13247,#13248,#13249,
#13250,#13251,#13252,#13253,#13254,#13255,#13256,#13257,#13258,#13259,#13260,
#13261,#13262,#13263,#13264,#13265,#13266,#13267,#13268,#13269,#13270,#13271,
#13272,#13273,#13274,#13275,#13276,#13277,#13278,#13279,#13280,#13281,#13282,
#13283,#13284,#13285,#13286,#13287,#13288,#13289,#13290,#13291,#13292,#13293,
#13294,#13295,#13296,#13297,#13298,#13299,#13300,#13301,#13302,#13303,#13304,
#13305,#13306,#13307,#13308,#13309,#13310,#13311,#13312,#13313,#13314,#13315,
#13316,#13317,#13318,#13319,#13320,#13321,#13322,#13323,#13324,#13325,#13326,
#13327,#13328,#13329,#13330,#13331,#13332,#13333,#13334,#13335,#13336,#13337,
#13338,#13339,#13340,#13341,#13342,#13343,#13344,#13345,#13346,#13347,#13348,
#13349,#13350,#13351,#13352,#13353,#13354,#13355,#13356,#13357,#13358,#13359,
#13360,#13361,#13362,#13363,#13364,#13365,#13366,#13367,#13368,#13369,#13370,
#13371,#13372,#13373,#13374,#13375,#13376,#13377,#13378,#13379,#13380,#13381,
#13382,#13383,#13384,#13385,#13386,#13387,#13388,#13389,#13390,#13391,#13392,
#13393,#13394,#13395,#13396,#13397,#13398,#13399,#13400,#13401,#13402,#13403,
#13404,#13405,#13406,#13407,#13408,#13409,#13410,#13411,#13412,#13413,#13414,
#13415,#13416,#13417,#13418,#13419,#13420,#13421,#13422,#13423,#13424,#13425,
#13426,#13427,#13428,#13429,#13430,#13431,#13432,#13433,#13434,#13435),
 .UNSPECIFIED.,.F.,.F.,(4,2,2,2,2,2,2,2,2,2,2,2,2,2,2,2,2,2,2,2,2,2,2,2,
2,2,2,2,2,2,2,2,2,2,2,2,2,2,2,2,2,2,2,2,2,2,2,2,2,2,2,2,2,2,2,2,2,2,2,2,
2,2,2,2,2,2,2,2,2,2,2,2,2,2,2,2,2,2,2,2,2,2,2,2,2,2,2,2,2,2,2,2,2,2,2,2,
2,2,2,2,2,2,2,2,2,2,2,2,2,2,2,2,2,2,2,2,2,2,2,2,2,2,2,2,2,2,2,2,2,2,2,2,
2,4),(-2.6924050095202,-2.68642891308495,-2.64342279511557,-2.60911170960607,
-2.59398314520964,-2.5915962610922,-2.5903564984864,-2.5893508801732,-2.5883475873379,
-2.5865321228209,-2.58091462116684,-2.48819071299198,-2.43336099519159,
-2.43109790870853,-2.42992737528862,-2.42919171106608,-2.42851294842858,
-2.42796299827926,-2.42731748260204,-2.42622333824083,-2.42227452987842,
-2.35808439070906,-2.33325900814762,-2.30428544406198,-2.27504080974453,
-2.2697836267792,-2.26808174249944,-2.26699221143255,-2.2659725753604,-2.26464106510559,
-2.26182857348486,-2.24077454455778,-2.23828694620631,-2.22172473220441,
-2.13832501443953,-2.11664611819253,-2.10766753253107,-2.10631461940788,
-2.10561942724472,-2.10505858878972,-2.10441054397551,-2.10330574668048,
-2.09925544159485,-2.03172869249018,-1.95195643851913,-1.94685995131592,
-1.94511457370892,-1.94412527893165,-1.94321788528285,-1.94199738915162,
-1.9397021457465,-1.92666792358696,-1.90254407047974,-1.81458824953252,
-1.80700198628684,-1.79811745036071,-1.79762434913496,-1.79680812683313,
-1.78500867117236,-1.78357487636116,-1.7828505835689,-1.78232096597438,
-1.78174759439861,-1.78095937424306,-1.77912044841993,-1.73401008824978,
-1.63026584462984,-1.62402675192692,-1.62213417783524,-1.62111526929572,
-1.6201868888682,-1.61904718632739,-1.61782195897111,-1.61595046703596,
-1.61250012800757,-1.58381013371298,-1.54061546022415,-1.46562662399494,
-1.46511055584924,-1.46113603254543,-1.46003913909064,-1.45939295372624,
-1.45883196278505,-1.45813432692258,-1.45676958414006,-1.44746566983231,
-1.42445685182236,-1.30655372447723,-1.30077308952915,-1.29893680009627,
-1.29792935119908,-1.29694439517905,-1.29574603455664,-1.29445773953861,
-1.29243651969806,-1.28859980192737,-1.25434760256718,-1.15940771580721,
-1.1555336512672,-1.1545735800796,-1.13892822369334,-1.13720757342173,-1.13651714760256,
-1.1359439873102,-1.13535263347187,-1.13447392429836,-1.13206489299596,
-1.09284674087391,-0.983821308633121,-0.977721682838613,-0.975846038465802,
-0.974830673799416,-0.973846436504311,-0.972662332388304,-0.971392381494991,
-0.969414633580607,-0.965690836890829,-0.933100508755005,-0.844865441353235,
-0.834999250179034,-0.833101662099482,-0.831773057111843,-0.815851704052827,
-0.814123258818844,-0.813431583065616,-0.812858125965805,-0.812267264778896,
-0.81139072582339,-0.808996437677532,-0.770749363486924,-0.758866562162959,
-0.74889831689786,-0.687082703388265,-0.662225552500327),.UNSPECIFIED.);
#87=B_SPLINE_CURVE_WITH_KNOTS('',3,(#13441,#13442,#13443,#13444,#13445,
#13446,#13447,#13448,#13449,#13450,#13451,#13452,#13453,#13454,#13455,#13456,
#13457,#13458,#13459,#13460,#13461,#13462,#13463,#13464,#13465,#13466,#13467,
#13468,#13469,#13470,#13471,#13472,#13473,#13474,#13475,#13476,#13477,#13478,
#13479,#13480,#13481,#13482,#13483,#13484,#13485,#13486,#13487,#13488,#13489,
#13490,#13491,#13492,#13493,#13494,#13495,#13496,#13497,#13498,#13499,#13500,
#13501,#13502,#13503,#13504,#13505,#13506,#13507,#13508,#13509,#13510,#13511,
#13512,#13513,#13514,#13515,#13516,#13517,#13518,#13519,#13520,#13521,#13522,
#13523,#13524,#13525,#13526,#13527,#13528,#13529,#13530,#13531,#13532,#13533,
#13534,#13535,#13536,#13537,#13538,#13539,#13540,#13541,#13542,#13543,#13544,
#13545,#13546,#13547,#13548,#13549,#13550,#13551,#13552,#13553,#13554,#13555,
#13556,#13557,#13558,#13559,#13560,#13561,#13562,#13563,#13564,#13565,#13566,
#13567,#13568,#13569,#13570,#13571,#13572,#13573,#13574,#13575,#13576,#13577,
#13578,#13579,#13580,#13581,#13582,#13583,#13584,#13585,#13586,#13587,#13588,
#13589,#13590,#13591,#13592,#13593,#13594,#13595,#13596,#13597,#13598,#13599,
#13600,#13601,#13602,#13603,#13604,#13605,#13606,#13607,#13608,#13609,#13610,
#13611,#13612,#13613,#13614,#13615,#13616,#13617,#13618,#13619,#13620,#13621,
#13622,#13623,#13624,#13625,#13626,#13627,#13628,#13629,#13630,#13631,#13632,
#13633,#13634,#13635,#13636,#13637,#13638,#13639,#13640,#13641,#13642,#13643,
#13644,#13645,#13646,#13647,#13648,#13649,#13650,#13651,#13652,#13653,#13654,
#13655,#13656,#13657,#13658,#13659,#13660,#13661,#13662,#13663,#13664,#13665,
#13666,#13667,#13668,#13669,#13670),.UNSPECIFIED.,.F.,.F.,(4,2,2,2,2,2,
2,2,2,2,2,2,2,2,2,2,2,2,2,2,2,2,2,2,2,2,2,2,2,2,2,2,2,2,2,2,2,2,2,2,2,2,
2,2,2,2,2,2,2,2,2,2,2,2,2,2,2,2,2,2,2,2,2,2,2,2,2,2,2,2,2,2,2,2,2,2,2,2,
2,2,2,2,2,2,2,2,2,2,2,2,2,2,2,2,2,2,2,2,2,2,2,2,2,2,2,2,2,2,2,2,2,2,2,2,
4),(-1.36933580029482,-1.36685434590888,-1.36489436748477,-1.35480597029584,
-1.35328431549134,-1.3525627033398,-1.35199784247543,-1.35137369114127,
-1.35036769919804,-1.34691195881337,-1.32465236042517,-1.25872574888066,
-1.19709907076041,-1.19331180451753,-1.19192329337445,-1.19094821534783,
-1.19003701479565,-1.18878553999599,-1.18634394507964,-1.17007358821919,
-1.13138876938743,-1.06590527017317,-1.05302557088158,-1.0506948760313,
-1.04925113861638,-1.04715896223443,-1.04631814496416,-1.04591121633372,
-1.0451413396503,-1.04440053621934,-1.04311229353906,-1.03188745467814,
-1.03031738950424,-1.02958648241428,-1.02902031422942,-1.02840095652667,
-1.02741593142817,-1.02416366506071,-1.01893919292446,-1.00541698416013,
-0.974196927855472,-0.932524209166809,-0.874216467908195,-0.870382552085268,
-0.868986838394231,-0.868009763794535,-0.867099121419448,-0.865852160241502,
-0.863432359506044,-0.849122318907712,-0.830666780537513,-0.79029497564326,
-0.748728636782336,-0.71809664715751,-0.716809030995085,-0.715305151953588,
-0.712529953720571,-0.708262431568275,-0.707135605047334,-0.70648236059627,
-0.705921812086907,-0.705383324993881,-0.704287162729645,-0.699881061533425,
-0.692083071464235,-0.67272299237665,-0.633143989027252,-0.552940401187442,
-0.547830955348225,-0.546083555098341,-0.545093722574369,-0.544186206801683,
-0.542966098823524,-0.540673383588316,-0.527947292407187,-0.495752375365148,
-0.487868121601157,-0.481545700416331,-0.43852589759176,-0.402500153446669,
-0.386264157382296,-0.384699329270653,-0.383942292282003,-0.383403977149381,
-0.382892781691509,-0.382344655882414,-0.381638936574097,-0.378789560123842,
-0.37438776330426,-0.360698708546912,-0.337609289557772,-0.317116640240227,
-0.285708452326109,-0.228315541179422,-0.22451663837901,-0.223126351679466,
-0.222150802348841,-0.221239777422601,-0.21998949920154,-0.21755356641792,
-0.202477368397074,-0.153312818696664,-0.136544937420956,-0.128280902080467,
-0.119063008784389,-0.0749051582841398,-0.0631519213070257,-0.0615814607740693,
-0.0608392917967397,-0.0602714293384798,-0.0596574167597624,-0.059026908384464,
-0.0581076872292814,-0.056491098985421,-0.000961071678187754),
 .UNSPECIFIED.);
#88=B_SPLINE_CURVE_WITH_KNOTS('',3,(#13671,#13672,#13673,#13674,#13675,
#13676,#13677,#13678,#13679,#13680,#13681,#13682,#13683,#13684,#13685,#13686,
#13687,#13688,#13689,#13690,#13691,#13692,#13693,#13694,#13695,#13696,#13697,
#13698,#13699,#13700,#13701,#13702,#13703,#13704,#13705,#13706,#13707,#13708,
#13709,#13710,#13711,#13712,#13713,#13714,#13715,#13716,#13717,#13718,#13719,
#13720,#13721,#13722,#13723,#13724,#13725,#13726,#13727,#13728,#13729,#13730,
#13731,#13732,#13733,#13734,#13735,#13736,#13737,#13738,#13739,#13740,#13741,
#13742,#13743,#13744,#13745,#13746,#13747,#13748,#13749,#13750,#13751,#13752,
#13753,#13754,#13755,#13756,#13757,#13758,#13759,#13760),.UNSPECIFIED.,
 .F.,.F.,(4,2,2,2,2,2,2,2,2,2,2,2,2,2,2,2,2,2,2,2,2,2,2,2,2,2,2,2,2,2,2,
2,2,2,2,2,2,2,2,2,2,2,2,2,4),(-4.06081080818158,-3.97254646944807,-3.96598950378341,
-3.96298913079805,-3.96059351635776,-3.95935201078245,-3.9583463749307,
-3.95734422127451,-3.95553403847313,-3.94995623461136,-3.85805141253993,
-3.83816751636306,-3.81202015485741,-3.79979020396287,-3.79875902822199,
-3.79808190059324,-3.79754275723518,-3.79703610009293,-3.7964848361183,
-3.79550986711415,-3.79265100789042,-3.74366436221132,-3.71970253130055,
-3.69647514053989,-3.65675031186624,-3.64021162345936,-3.63776051829344,
-3.6365073688447,-3.63559624731789,-3.63462248064216,-3.63323788429951,
-3.62947380489197,-3.57261200094989,-3.54162896394138,-3.50239471556971,
-3.47853849129411,-3.47599500762396,-3.47531398579534,-3.47477369631238,
-3.4742665248669,-3.47371730766684,-3.47275256641134,-3.46996415707241,
-3.42646651277619,-3.39963798704962),.UNSPECIFIED.);
#89=B_SPLINE_CURVE_WITH_KNOTS('',3,(#13762,#13763,#13764,#13765,#13766,
#13767,#13768,#13769,#13770,#13771,#13772,#13773,#13774,#13775,#13776,#13777,
#13778,#13779,#13780,#13781,#13782,#13783,#13784,#13785,#13786,#13787,#13788,
#13789,#13790,#13791,#13792,#13793,#13794,#13795,#13796,#13797,#13798,#13799,
#13800,#13801,#13802,#13803,#13804,#13805,#13806,#13807,#13808,#13809,#13810,
#13811,#13812,#13813,#13814,#13815,#13816,#13817,#13818,#13819,#13820,#13821,
#13822,#13823,#13824,#13825,#13826,#13827,#13828,#13829,#13830,#13831,#13832,
#13833,#13834,#13835,#13836,#13837,#13838,#13839,#13840,#13841,#13842,#13843,
#13844,#13845,#13846,#13847,#13848,#13849,#13850,#13851,#13852,#13853,#13854,
#13855,#13856,#13857,#13858,#13859,#13860,#13861,#13862,#13863,#13864,#13865,
#13866,#13867,#13868,#13869,#13870,#13871),.UNSPECIFIED.,.F.,.F.,(4,2,2,
2,2,2,2,2,2,2,2,2,2,2,2,2,2,2,2,2,2,2,2,2,2,2,2,2,2,2,2,2,2,2,2,2,2,2,2,
2,2,2,2,2,2,2,2,2,2,2,2,2,2,2,4),(-0.662225552500327,-0.656915475901761,
-0.654094279685166,-0.652731584139461,-0.651763761058461,-0.650769380826292,
-0.649484912821886,-0.648077451830496,-0.645772576183879,-0.607416192165025,
-0.509195274519436,-0.508993483768699,-0.507062659781684,-0.506699670647006,
-0.505795926386445,-0.505322534985358,-0.504525025115455,-0.492702146991682,
-0.49126760132188,-0.490543137750809,-0.490013495181177,-0.489440197184266,
-0.488652252520684,-0.486814750144522,-0.442009704914305,-0.418914184542673,
-0.390121669982303,-0.334541928051994,-0.331059469460802,-0.329719800275287,
-0.328758040194021,-0.327760691969241,-0.32645741569573,-0.325023968814133,
-0.322657030438605,-0.276333688584542,-0.173374216379223,-0.172657714031728,
-0.168830077812296,-0.16773580740683,-0.167160321233803,-0.1666561992001,
-0.16600249409107,-0.164843360661631,-0.159645732572176,-0.105976682679097,
-0.0344455005358403,-0.0131096786969769,-0.0083810641565655,-0.00668827843886096,
-0.00570931015307833,-0.00472820051572089,-0.0037516187691957,-0.00214249435605951,
-0.000961424493519781),.UNSPECIFIED.);
#90=B_SPLINE_CURVE_WITH_KNOTS('',3,(#13872,#13873,#13874,#13875,#13876,
#13877,#13878,#13879,#13880,#13881,#13882,#13883,#13884,#13885,#13886,#13887,
#13888,#13889,#13890,#13891,#13892,#13893,#13894,#13895,#13896,#13897,#13898,
#13899,#13900,#13901,#13902,#13903,#13904,#13905,#13906,#13907,#13908,#13909,
#13910,#13911,#13912,#13913,#13914,#13915,#13916,#13917,#13918,#13919,#13920,
#13921,#13922,#13923,#13924,#13925,#13926,#13927,#13928,#13929,#13930,#13931,
#13932,#13933,#13934,#13935,#13936,#13937,#13938,#13939,#13940,#13941,#13942,
#13943,#13944,#13945,#13946,#13947,#13948,#13949,#13950,#13951,#13952,#13953,
#13954,#13955,#13956,#13957,#13958,#13959,#13960,#13961,#13962,#13963,#13964,
#13965,#13966,#13967,#13968,#13969,#13970,#13971,#13972,#13973,#13974,#13975,
#13976,#13977,#13978,#13979,#13980,#13981,#13982,#13983,#13984,#13985,#13986,
#13987,#13988,#13989,#13990,#13991,#13992,#13993,#13994,#13995,#13996,#13997,
#13998,#13999,#14000,#14001,#14002,#14003,#14004,#14005,#14006,#14007,#14008,
#14009,#14010,#14011,#14012,#14013,#14014,#14015,#14016,#14017,#14018,#14019,
#14020,#14021,#14022,#14023,#14024,#14025,#14026,#14027,#14028,#14029,#14030,
#14031,#14032,#14033,#14034,#14035,#14036,#14037,#14038,#14039,#14040,#14041,
#14042,#14043),.UNSPECIFIED.,.F.,.F.,(4,2,2,2,2,2,2,2,2,2,2,2,2,2,2,2,2,
2,2,2,2,2,2,2,2,2,2,2,2,2,2,2,2,2,2,2,2,2,2,2,2,2,2,2,2,2,2,2,2,2,2,2,2,
2,2,2,2,2,2,2,2,2,2,2,2,2,2,2,2,2,2,2,2,2,2,2,2,2,2,2,2,2,2,2,2,4),(-4.06144638480364,
-4.05919065566942,-4.05240797511435,-3.95307084923477,-3.91100322525023,
-3.90626966855807,-3.90514515424867,-3.9044991495446,-3.9039380295739,-3.90323986657943,
-3.90216435092963,-3.89732232099656,-3.80722477802761,-3.76990221440686,
-3.75486044676713,-3.74636537497466,-3.74490620736317,-3.74358422074853,
-3.74258382916825,-3.74162763243638,-3.74030911630387,-3.73695406553281,
-3.69242830353027,-3.64226878304747,-3.5884916767847,-3.58332682229674,
-3.58217014215797,-3.58151704059188,-3.58101300797117,-3.58043721918569,
-3.57934116056596,-3.57549624057306,-3.57480496710874,-3.47182663685071,
-3.4295773122845,-3.42298330110116,-3.42162708554947,-3.42037954516056,
-3.41939014538462,-3.4184075240817,-3.41699122507982,-3.41301988914435,
-3.34837077914238,-3.30192778344226,-3.26121341061206,-3.25946289062047,
-3.25869043566116,-3.25811983883966,-3.25758629563526,-3.25684690632901,
-3.25535314513071,-3.24169502201747,-3.24097321767489,-3.23642293525557,
-3.22647997778993,-3.14395608015912,-3.1061319003723,-3.09996078234044,
-3.0986312201838,-3.09740300637273,-3.0964158872732,-3.09528045882963,-3.09345145010086,
-3.08743065874654,-2.97142865816801,-2.94710271775015,-2.93747541316192,
-2.9360991743505,-2.93539907398724,-2.93483779561794,-2.93427646322084,
-2.93325228912262,-2.93002026140098,-2.87469654985874,-2.82404422793751,
-2.8022728656313,-2.78620986520908,-2.77728541406992,-2.77580607264692,
-2.7744695323233,-2.77346665202304,-2.77251440473491,-2.77121127070329,
-2.76794725507986,-2.76576455985351,-2.6922410793174),.UNSPECIFIED.);
#91=B_SPLINE_CURVE_WITH_KNOTS('',3,(#14048,#14049,#14050,#14051,#14052,
#14053,#14054,#14055,#14056,#14057,#14058,#14059,#14060,#14061,#14062,#14063,
#14064,#14065,#14066,#14067,#14068,#14069,#14070,#14071,#14072,#14073,#14074,
#14075,#14076,#14077,#14078,#14079,#14080,#14081,#14082,#14083,#14084,#14085,
#14086,#14087,#14088,#14089,#14090,#14091,#14092,#14093,#14094,#14095,#14096,
#14097,#14098,#14099,#14100,#14101,#14102,#14103,#14104,#14105,#14106,#14107,
#14108,#14109,#14110,#14111,#14112,#14113,#14114,#14115,#14116,#14117,#14118,
#14119,#14120,#14121,#14122,#14123,#14124,#14125,#14126,#14127,#14128,#14129,
#14130,#14131,#14132,#14133,#14134,#14135,#14136,#14137,#14138,#14139,#14140,
#14141,#14142,#14143,#14144,#14145,#14146,#14147,#14148,#14149,#14150,#14151,
#14152,#14153,#14154,#14155,#14156,#14157,#14158,#14159,#14160,#14161,#14162,
#14163,#14164,#14165,#14166,#14167,#14168,#14169,#14170,#14171,#14172,#14173,
#14174,#14175,#14176,#14177,#14178,#14179,#14180,#14181,#14182,#14183,#14184,
#14185,#14186,#14187,#14188,#14189,#14190,#14191,#14192,#14193,#14194,#14195,
#14196,#14197,#14198,#14199,#14200,#14201,#14202,#14203,#14204,#14205,#14206,
#14207,#14208,#14209,#14210,#14211,#14212,#14213,#14214,#14215,#14216,#14217,
#14218,#14219,#14220,#14221,#14222,#14223,#14224,#14225,#14226,#14227,#14228,
#14229,#14230,#14231,#14232,#14233,#14234,#14235,#14236,#14237,#14238,#14239,
#14240,#14241,#14242,#14243,#14244,#14245,#14246,#14247,#14248,#14249,#14250,
#14251,#14252,#14253,#14254,#14255,#14256,#14257,#14258,#14259,#14260,#14261,
#14262,#14263,#14264,#14265,#14266,#14267,#14268,#14269,#14270,#14271,#14272,
#14273,#14274,#14275,#14276,#14277,#14278,#14279,#14280,#14281,#14282,#14283,
#14284,#14285,#14286,#14287,#14288,#14289,#14290,#14291,#14292,#14293,#14294,
#14295,#14296,#14297,#14298,#14299,#14300,#14301,#14302,#14303,#14304,#14305,
#14306,#14307,#14308,#14309,#14310,#14311,#14312,#14313,#14314,#14315,#14316,
#14317,#14318,#14319),.UNSPECIFIED.,.F.,.F.,(4,2,2,2,2,2,2,2,2,2,2,2,2,
2,2,2,2,2,2,2,2,2,2,2,2,2,2,2,2,2,2,2,2,2,2,2,2,2,2,2,2,2,2,2,2,2,2,2,2,
2,2,2,2,2,2,2,2,2,2,2,2,2,2,2,2,2,2,2,2,2,2,2,2,2,2,2,2,2,2,2,2,2,2,2,2,
2,2,2,2,2,2,2,2,2,2,2,2,2,2,2,2,2,2,2,2,2,2,2,2,2,2,2,2,2,2,2,2,2,2,2,2,
2,2,2,2,2,2,2,2,2,2,2,2,2,2,4),(-3.3998905608284,-3.36728512983728,-3.3165216220863,
-3.29570632376686,-3.29237695365769,-3.29138239889647,-3.29076545694202,
-3.29019859875152,-3.28946284154685,-3.28786700497707,-3.27598056772875,
-3.23198105457235,-3.18076690676289,-3.15238114038521,-3.13998197611609,
-3.13516108703912,-3.13277135392944,-3.13132835682328,-3.13006799864135,
-3.12906467308018,-3.12811325689239,-3.12681322208736,-3.12356706488969,
-3.0855108628911,-3.02936706775133,-2.9744847644014,-2.96970572635586,-2.96857766105995,
-2.96793086156635,-2.96736980881946,-2.96667270043273,-2.96560059202097,
-2.96080073717221,-2.87355072079388,-2.81239917000519,-2.80987572896211,
-2.80781582597809,-2.80665261889776,-2.80571970314026,-2.80470291168966,
-2.80282144819128,-2.79667725886823,-2.68911732543282,-2.66174267098193,
-2.64710249109855,-2.64559839026613,-2.64487240022135,-2.64436081871292,
-2.64382311078167,-2.64306850486718,-2.6410803078615,-2.60987299144671,
-2.5665066275203,-2.52174437638913,-2.49143691183562,-2.48787073890102,
-2.48595376388476,-2.48430629344025,-2.48323828799571,-2.48221827430095,
-2.48088630108514,-2.47807294162079,-2.45701599986302,-2.45471210149877,
-2.445019818415,-2.36282815790668,-2.3413564855565,-2.33174645977177,-2.32378480571599,
-2.32247247876214,-2.321785647723,-2.32127927532706,-2.32072487587035,-2.3197354266716,
-2.31677039913419,-2.31462818929304,-2.22872147501193,-2.18192664339179,
-2.16430705711538,-2.16182893207435,-2.16056979431106,-2.15965746997792,
-2.15868537829655,-2.15730807998916,-2.15359343388215,-2.15215529351109,
-2.07939411929984,-2.03049674697944,-2.02021791334108,-2.01765418671469,
-2.00133669964159,-1.99976965660553,-1.9990119964218,-1.99847344097666,
-1.99796219088357,-1.99723848147826,-1.99574604504187,-1.98170403922362,
-1.95507862560463,-1.84740260657027,-1.84595560832858,-1.84000167342805,
-1.83814327200301,-1.83713108216853,-1.83612600059368,-1.8349007012432,
-1.8325836561893,-1.81909510120922,-1.80058279614118,-1.7592247357299,-1.70323561741335,
-1.69832449905212,-1.69408189729303,-1.67817944339364,-1.67645107467533,
-1.67575926478383,-1.67518563150524,-1.67459451913173,-1.67373535088149,
-1.67144523440998,-1.62052436010717,-1.53977960825839,-1.5186843633618,
-1.51611832414237,-1.51481920601549,-1.51386804504227,-1.51284405677621,
-1.51146373831998,-1.50836035977558,-1.49011983684336,-1.4606238808476,
-1.37642590569432,-1.37376626747478,-1.37226986844979,-1.3702919615779,
-1.36933580029482),.UNSPECIFIED.);
#92=B_SPLINE_CURVE_WITH_KNOTS('',3,(#14320,#14321,#14322,#14323,#14324,
#14325,#14326,#14327,#14328,#14329,#14330,#14331,#14332,#14333,#14334,#14335,
#14336,#14337,#14338,#14339,#14340,#14341,#14342,#14343,#14344,#14345,#14346,
#14347,#14348,#14349,#14350,#14351,#14352,#14353,#14354,#14355,#14356,#14357,
#14358,#14359,#14360,#14361,#14362,#14363,#14364,#14365,#14366,#14367,#14368,
#14369,#14370,#14371,#14372,#14373,#14374,#14375,#14376,#14377,#14378,#14379,
#14380,#14381,#14382,#14383,#14384,#14385,#14386,#14387,#14388,#14389,#14390,
#14391,#14392,#14393,#14394,#14395,#14396,#14397,#14398,#14399,#14400,#14401,
#14402,#14403,#14404,#14405,#14406,#14407,#14408,#14409,#14410,#14411,#14412,
#14413,#14414,#14415,#14416,#14417,#14418,#14419,#14420,#14421,#14422,#14423,
#14424,#14425,#14426,#14427,#14428,#14429,#14430,#14431,#14432,#14433,#14434,
#14435,#14436,#14437,#14438,#14439,#14440,#14441,#14442,#14443,#14444,#14445,
#14446,#14447,#14448,#14449,#14450,#14451,#14452,#14453,#14454,#14455,#14456,
#14457,#14458,#14459,#14460,#14461,#14462,#14463,#14464,#14465,#14466,#14467,
#14468,#14469,#14470,#14471,#14472,#14473,#14474,#14475,#14476,#14477,#14478,
#14479,#14480,#14481,#14482,#14483,#14484,#14485,#14486,#14487,#14488,#14489,
#14490,#14491,#14492,#14493,#14494,#14495,#14496,#14497,#14498,#14499,#14500,
#14501,#14502,#14503,#14504,#14505,#14506,#14507,#14508,#14509,#14510,#14511,
#14512,#14513,#14514,#14515,#14516,#14517,#14518,#14519,#14520,#14521,#14522,
#14523,#14524,#14525,#14526,#14527,#14528,#14529,#14530,#14531,#14532,#14533,
#14534,#14535,#14536,#14537,#14538,#14539,#14540,#14541,#14542,#14543,#14544,
#14545,#14546,#14547,#14548,#14549,#14550,#14551,#14552,#14553,#14554,#14555,
#14556,#14557,#14558,#14559,#14560,#14561,#14562,#14563,#14564,#14565,#14566,
#14567,#14568,#14569,#14570,#14571,#14572,#14573,#14574,#14575,#14576,#14577,
#14578,#14579,#14580,#14581,#14582,#14583,#14584,#14585,#14586,#14587,#14588,
#14589,#14590,#14591,#14592,#14593,#14594,#14595,#14596,#14597,#14598,#14599,
#14600,#14601,#14602,#14603,#14604,#14605,#14606,#14607,#14608,#14609,#14610,
#14611),.UNSPECIFIED.,.F.,.F.,(4,2,2,2,2,2,2,2,2,2,2,2,2,2,2,2,2,2,2,2,
2,2,2,2,2,2,2,2,2,2,2,2,2,2,2,2,2,2,2,2,2,2,2,2,2,2,2,2,2,2,2,2,2,2,2,2,
2,2,2,2,2,2,2,2,2,2,2,2,2,2,2,2,2,2,2,2,2,2,2,2,2,2,2,2,2,2,2,2,2,2,2,2,
2,2,2,2,2,2,2,2,2,2,2,2,2,2,2,2,2,2,2,2,2,2,2,2,2,2,2,2,2,2,2,2,2,2,2,2,
2,2,2,2,2,2,2,2,2,2,2,2,2,2,2,2,2,4),(-2.6922410793174,-2.68713462272044,
-2.64823997998648,-2.62408582515161,-2.61450042249326,-2.61312557337638,
-2.61242574270667,-2.61186446364603,-2.61121958928161,-2.61012871639063,
-2.60621286827792,-2.60561728037059,-2.50244536075739,-2.46034444360088,
-2.45376363155032,-2.45240811610361,-2.45116107621633,-2.45017190993429,
-2.44918897635062,-2.44777179075376,-2.44379548677097,-2.44214989183045,
-2.35711071102754,-2.331909315746,-2.29283407919076,-2.29042678077883,-2.28954818758804,
-2.28895675687757,-2.28838339815196,-2.28769259177839,-2.28597024774855,
-2.270277566579,-2.22975440958395,-2.17871775924245,-2.15058635241785,-2.13196261563494,
-2.12945305774455,-2.12818757464308,-2.12727448816167,-2.12630516097562,
-2.12493767291909,-2.12128365515612,-2.06285430825287,-2.03077692330812,
-1.98320272125178,-1.9827691275745,-1.98211228742657,-1.98099312574363,
-1.96881277315717,-1.96722633012536,-1.96648094994786,-1.96591256137913,
-1.96529993928841,-1.96432476689283,-1.96116788120736,-1.90901210828921,
-1.84748766450742,-1.83134000860834,-1.80960283654488,-1.80672794264587,
-1.80540461505629,-1.80438611967032,-1.80329278402458,-1.8015744786572,
-1.79618406098519,-1.76574598111205,-1.72086324532706,-1.68873903751014,
-1.64735824939117,-1.64475232609375,-1.64381391807694,-1.64326982933107,
-1.64271553751978,-1.64199820900581,-1.6412086522539,-1.63990912343395,
-1.6372977843104,-1.60941290023342,-1.49017200065016,-1.48462612211848,
-1.48281988023028,-1.48181838956609,-1.48081242586797,-1.47956903877008,
-1.47716516419016,-1.4616084856093,-1.42567471149632,-1.33270251610063,
-1.32253259850076,-1.3210074890702,-1.32028528398105,-1.31972042577709,
-1.31910934427433,-1.31811887402089,-1.31694145154479,-1.31466018507528,
-1.23135337311723,-1.19359734994182,-1.1637887241948,-1.16097645325252,
-1.15961582414204,-1.15864845161507,-1.15773484750122,-1.15646490249426,
-1.15393294366652,-1.13454213039803,-1.10434983166698,-1.00349420131543,
-1.00105446347532,-0.998426007332181,-0.997484208043545,-0.996939417015215,
-0.996385338786349,-0.995668860798337,-0.994881252118572,-0.993586459037281,
-0.990988183862428,-0.98430248978452,-0.958260620862715,-0.872080674700547,
-0.865052497408185,-0.85978181409044,-0.855181814541239,-0.853109715711091,
-0.849293231856371,-0.845532490556877,-0.838770700936585,-0.836817912953404,
-0.835672171381988,-0.834675141219425,-0.833430981514482,-0.831024353935636,
-0.815408676963877,-0.779259016791593,-0.768382155130384,-0.686574073417267,
-0.676406981929468,-0.674881783655769,-0.674159475809447,-0.673594510143407,
-0.672983285351853,-0.671993516232607,-0.670816451190077,-0.668536307392394,
-0.662936658298539,-0.661877334975925),.UNSPECIFIED.);
#93=B_SPLINE_CURVE_WITH_KNOTS('',3,(#14617,#14618,#14619,#14620,#14621,
#14622,#14623,#14624,#14625,#14626,#14627,#14628,#14629,#14630,#14631,#14632,
#14633,#14634,#14635,#14636,#14637,#14638,#14639,#14640,#14641,#14642,#14643,
#14644,#14645,#14646,#14647,#14648,#14649,#14650,#14651,#14652,#14653,#14654,
#14655,#14656,#14657,#14658,#14659,#14660,#14661,#14662,#14663,#14664,#14665,
#14666,#14667,#14668,#14669,#14670,#14671,#14672,#14673,#14674,#14675,#14676,
#14677,#14678,#14679,#14680,#14681,#14682,#14683,#14684,#14685,#14686,#14687,
#14688,#14689,#14690,#14691,#14692,#14693,#14694,#14695,#14696,#14697,#14698,
#14699,#14700,#14701,#14702,#14703,#14704,#14705,#14706,#14707,#14708,#14709,
#14710,#14711,#14712,#14713,#14714,#14715,#14716,#14717,#14718,#14719,#14720,
#14721,#14722,#14723,#14724,#14725,#14726,#14727,#14728,#14729,#14730,#14731,
#14732,#14733,#14734,#14735,#14736,#14737,#14738,#14739,#14740,#14741,#14742,
#14743,#14744,#14745,#14746,#14747,#14748,#14749,#14750,#14751,#14752,#14753,
#14754,#14755,#14756,#14757,#14758,#14759,#14760,#14761,#14762,#14763,#14764,
#14765,#14766,#14767,#14768,#14769,#14770,#14771,#14772,#14773,#14774,#14775,
#14776,#14777,#14778,#14779,#14780,#14781,#14782,#14783,#14784,#14785,#14786,
#14787,#14788,#14789,#14790,#14791,#14792,#14793,#14794,#14795,#14796,#14797,
#14798,#14799,#14800,#14801,#14802,#14803,#14804,#14805,#14806,#14807,#14808,
#14809,#14810,#14811,#14812,#14813,#14814,#14815,#14816,#14817,#14818,#14819,
#14820,#14821,#14822,#14823,#14824,#14825,#14826,#14827,#14828,#14829,#14830,
#14831,#14832,#14833,#14834,#14835,#14836,#14837,#14838,#14839,#14840,#14841,
#14842,#14843,#14844,#14845,#14846,#14847,#14848,#14849,#14850,#14851,#14852),
 .UNSPECIFIED.,.F.,.F.,(4,2,2,2,2,2,2,2,2,2,2,2,2,2,2,2,2,2,2,2,2,2,2,2,
2,2,2,2,2,2,2,2,2,2,2,2,2,2,2,2,2,2,2,2,2,2,2,2,2,2,2,2,2,2,2,2,2,2,2,2,
2,2,2,2,2,2,2,2,2,2,2,2,2,2,2,2,2,2,2,2,2,2,2,2,2,2,2,2,2,2,2,2,2,2,2,2,
2,2,2,2,2,2,2,2,2,2,2,2,2,2,2,2,2,2,2,2,2,4),(-1.3706021342809,-1.33968790873535,
-1.33401856145952,-1.33219611259199,-1.33119124182556,-1.33020562887945,
-1.32900320820066,-1.32770815951129,-1.32567126229208,-1.32179411806332,
-1.28694575622446,-1.18969573353665,-1.18724711149206,-1.17210366014068,
-1.17056744965157,-1.16981741516319,-1.16928094905498,-1.16876880551868,
-1.16803922229462,-1.16651679777185,-1.15086122351035,-1.13346846105473,
-1.01711551700477,-1.01084781452235,-1.00895174280275,-1.00793206835958,
-1.00702199189956,-1.00587166081457,-1.00386491049888,-1.00142321564038,
-0.996459223325355,-0.983561038025477,-0.953233618460723,-0.860087611558867,
-0.848637054403729,-0.847057996362212,-0.846325398928482,-0.845759001205586,
-0.84514051388519,-0.844139117633422,-0.84074713483859,-0.819288600678181,
-0.804879385123748,-0.79419062765631,-0.706327556382138,-0.704355576413767,
-0.702290172124463,-0.688799318849554,-0.68655653396867,-0.685221665917053,
-0.684201348806267,-0.683134805995026,-0.68149517466419,-0.679587812504406,
-0.676045958981582,-0.667851210282897,-0.643240497144552,-0.555880283953574,
-0.544980834416855,-0.543055155749907,-0.541784414057877,-0.525796932951882,
-0.524066125889073,-0.523373908728048,-0.522800161807121,-0.522209173753513,
-0.521332755836952,-0.518940682511649,-0.480883771885869,-0.470737638773909,
-0.462440339963734,-0.455371834935408,-0.449211566916693,-0.443764109072833,
-0.391834080392399,-0.385723458468287,-0.384350631729943,-0.383139853290937,
-0.381890920660856,-0.380734584892317,-0.378726169769955,-0.378274759633109,
-0.376211384241394,-0.374396806030457,-0.36681284380364,-0.363990923932303,
-0.362627781209224,-0.361659596428653,-0.360686126573825,-0.359412315683539,
-0.356838541751506,-0.353525769315386,-0.346035527004777,-0.323716324096793,
-0.304845271156971,-0.2244268547986,-0.217235472111384,-0.216807594226912,
-0.214523303241535,-0.20262634171097,-0.201029914946419,-0.200293970633825,
-0.199727004845841,-0.199109983184496,-0.198115379408065,-0.194786555305278,
-0.17398250401675,-0.0770206757634432,-0.0714024034177756,-0.0435884196513709,
-0.0405174833187884,-0.0392804771056761,-0.0382511397177548,-0.0373052319327293,
-0.0362747903774904,-0.0348785279011245,-0.0326008214399287,-0.000960744511183088),
 .UNSPECIFIED.);
#94=B_SPLINE_CURVE_WITH_KNOTS('',3,(#14853,#14854,#14855,#14856,#14857,
#14858,#14859,#14860,#14861,#14862,#14863,#14864,#14865,#14866,#14867,#14868,
#14869,#14870,#14871,#14872,#14873,#14874,#14875,#14876,#14877,#14878,#14879,
#14880,#14881,#14882,#14883,#14884,#14885,#14886,#14887,#14888,#14889,#14890,
#14891,#14892,#14893,#14894,#14895,#14896,#14897,#14898,#14899,#14900,#14901,
#14902,#14903,#14904,#14905,#14906,#14907,#14908,#14909,#14910,#14911,#14912,
#14913,#14914,#14915,#14916,#14917,#14918,#14919,#14920,#14921,#14922,#14923,
#14924,#14925,#14926,#14927,#14928,#14929,#14930,#14931,#14932,#14933,#14934,
#14935,#14936,#14937,#14938,#14939,#14940,#14941,#14942,#14943,#14944,#14945,
#14946,#14947,#14948,#14949,#14950,#14951,#14952,#14953,#14954),
 .UNSPECIFIED.,.F.,.F.,(4,2,2,2,2,2,2,2,2,2,2,2,2,2,2,2,2,2,2,2,2,2,2,2,
2,2,2,2,2,2,2,2,2,2,2,2,2,2,2,2,2,2,2,2,2,2,2,2,2,2,4),(-4.06089064309864,
-3.96335235672118,-3.94175675000815,-3.93835198066777,-3.93734921724052,
-3.93673043128563,-3.93616413894775,-3.93543219329238,-3.93385652356892,
-3.92249076690551,-3.91961350040436,-3.91861505179853,-3.91748448977263,
-3.91660111691796,-3.87731498072753,-3.82630983363265,-3.81059068443923,
-3.78986722396061,-3.78279530828148,-3.77806295378722,-3.77643045528318,
-3.77548755109764,-3.7744768041985,-3.77318713787788,-3.77055829171436,
-3.7545630006739,-3.74990497964328,-3.74591858543458,-3.70217391470195,
-3.67084846939447,-3.61859619825551,-3.61540924804387,-3.61443062183609,
-3.61381722569045,-3.61324911756206,-3.61250549498024,-3.61086773933177,
-3.60682639938017,-3.51400656001251,-3.47646817282647,-3.46331420601142,
-3.45827684851337,-3.45580848090533,-3.45378609440468,-3.45263089382435,
-3.45172366915353,-3.45070819523185,-3.44883324870267,-3.44274305947501,
-3.43878172892971,-3.3998905608284),.UNSPECIFIED.);
#95=B_SPLINE_CURVE_WITH_KNOTS('',3,(#14956,#14957,#14958,#14959,#14960,
#14961,#14962,#14963,#14964,#14965,#14966,#14967,#14968,#14969,#14970,#14971,
#14972,#14973,#14974,#14975,#14976,#14977,#14978,#14979,#14980,#14981,#14982,
#14983,#14984,#14985,#14986,#14987,#14988,#14989,#14990,#14991,#14992,#14993,
#14994,#14995,#14996,#14997,#14998,#14999,#15000,#15001,#15002,#15003,#15004,
#15005,#15006,#15007,#15008,#15009,#15010,#15011,#15012,#15013,#15014,#15015,
#15016,#15017,#15018,#15019,#15020,#15021,#15022,#15023,#15024,#15025,#15026,
#15027,#15028,#15029,#15030,#15031,#15032,#15033,#15034,#15035,#15036,#15037,
#15038,#15039,#15040,#15041,#15042,#15043,#15044,#15045,#15046,#15047,#15048,
#15049,#15050,#15051,#15052,#15053,#15054,#15055,#15056,#15057,#15058,#15059,
#15060,#15061),.UNSPECIFIED.,.F.,.F.,(4,2,2,2,2,2,2,2,2,2,2,2,2,2,2,2,2,
2,2,2,2,2,2,2,2,2,2,2,2,2,2,2,2,2,2,2,2,2,2,2,2,2,2,2,2,2,2,2,2,2,2,2,4),
(-0.661877334975925,-0.643648093147668,-0.598629952563144,-0.593209413012196,
-0.519753098729238,-0.515191858152316,-0.513524045209656,-0.512550046423522,
-0.511638474291198,-0.510384341549493,-0.507930040296465,-0.491011222933779,
-0.449850944372571,-0.440733349264975,-0.433186533921284,-0.426761311763646,
-0.421189247754163,-0.416290444791287,-0.371545985948876,-0.370380562012174,
-0.369457716532448,-0.353765601871672,-0.352043229174806,-0.351352398356726,
-0.350779015061414,-0.350252870931183,-0.34944154868183,-0.347455288281762,
-0.344672343238775,-0.33733227221629,-0.312022014438792,-0.224118836026523,
-0.194673419639501,-0.191869549367345,-0.190510912482517,-0.189544015592249,
-0.188630095191333,-0.187358491820614,-0.184818789933339,-0.165163829781162,
-0.134271791019828,-0.0559302248217822,-0.0522241009295653,-0.0465244163130091,
-0.0307401376884319,-0.0290151397822052,-0.0283238822308065,-0.0277503922061148,
-0.0272242268041416,-0.0266439166341936,-0.0258493377915546,-0.0245377297322901,
-0.00096062754245072),.UNSPECIFIED.);
#96=B_SPLINE_CURVE_WITH_KNOTS('',3,(#15062,#15063,#15064,#15065,#15066,
#15067,#15068,#15069,#15070,#15071,#15072,#15073,#15074,#15075,#15076,#15077,
#15078,#15079,#15080,#15081,#15082,#15083,#15084,#15085,#15086,#15087,#15088,
#15089,#15090,#15091,#15092,#15093,#15094,#15095,#15096,#15097,#15098,#15099,
#15100,#15101,#15102,#15103,#15104,#15105,#15106,#15107,#15108,#15109,#15110,
#15111,#15112,#15113,#15114,#15115,#15116,#15117,#15118,#15119,#15120,#15121,
#15122,#15123,#15124,#15125,#15126,#15127,#15128,#15129,#15130,#15131,#15132,
#15133,#15134,#15135,#15136,#15137,#15138,#15139,#15140,#15141,#15142,#15143,
#15144,#15145,#15146,#15147,#15148,#15149,#15150,#15151,#15152,#15153,#15154,
#15155,#15156,#15157,#15158,#15159,#15160,#15161,#15162,#15163,#15164,#15165,
#15166,#15167,#15168,#15169,#15170,#15171,#15172,#15173,#15174,#15175,#15176,
#15177,#15178,#15179,#15180,#15181,#15182,#15183,#15184,#15185,#15186,#15187,
#15188,#15189,#15190,#15191,#15192,#15193,#15194,#15195,#15196,#15197,#15198,
#15199,#15200,#15201,#15202,#15203),.UNSPECIFIED.,.F.,.F.,(4,3,3,3,3,3,
3,3,3,3,3,3,3,3,3,3,3,3,3,3,3,3,3,3,3,3,3,3,3,3,3,3,3,3,3,3,3,3,3,3,3,3,
3,3,3,3,3,4),(103.672557568728,103.764546167889,103.856418305638,103.948199630661,
104.039931731389,104.131640502381,104.223351810979,104.315152260498,104.406995790917,
104.49899760578,104.588677186729,104.681750131005,104.774696970642,104.867545341827,
104.960325846482,105.053071168639,105.14580613374,105.238555552081,105.331404192816,
105.424304633428,105.517360529512,105.588391842202,105.681464786478,105.774411626115,
105.867259997299,105.960040501955,106.052785824111,106.145520789212,106.238270207553,
106.331118848288,106.4240192889,106.517075184984,106.588106497675,106.681179441951,
106.774126281588,106.866974652772,106.959755157428,107.052500479584,107.145235444685,
107.237984863027,107.330833503762,107.423733944374,107.516789840458,107.587821153148,
107.680878189667,107.773824604379,107.866666658252,107.909967710001),
 .UNSPECIFIED.);
#97=B_SPLINE_CURVE_WITH_KNOTS('',3,(#15208,#15209,#15210,#15211,#15212,
#15213,#15214,#15215,#15216,#15217,#15218,#15219,#15220,#15221,#15222,#15223,
#15224,#15225,#15226,#15227,#15228,#15229,#15230,#15231,#15232,#15233,#15234,
#15235,#15236,#15237,#15238,#15239,#15240,#15241,#15242,#15243,#15244,#15245,
#15246,#15247,#15248,#15249,#15250,#15251,#15252,#15253,#15254,#15255,#15256,
#15257,#15258,#15259,#15260,#15261,#15262,#15263,#15264,#15265,#15266,#15267,
#15268,#15269,#15270,#15271,#15272,#15273,#15274,#15275,#15276,#15277,#15278,
#15279,#15280,#15281,#15282,#15283,#15284,#15285,#15286,#15287,#15288,#15289,
#15290,#15291,#15292,#15293,#15294,#15295,#15296,#15297,#15298,#15299,#15300,
#15301,#15302,#15303,#15304,#15305,#15306,#15307,#15308,#15309,#15310,#15311,
#15312,#15313,#15314,#15315,#15316,#15317,#15318,#15319,#15320,#15321,#15322,
#15323,#15324,#15325,#15326,#15327,#15328,#15329,#15330,#15331,#15332,#15333,
#15334,#15335,#15336,#15337,#15338,#15339,#15340,#15341,#15342,#15343,#15344,
#15345,#15346,#15347,#15348,#15349,#15350,#15351,#15352,#15353,#15354,#15355,
#15356,#15357,#15358,#15359,#15360,#15361,#15362,#15363,#15364,#15365,#15366,
#15367,#15368,#15369,#15370,#15371,#15372,#15373,#15374,#15375,#15376,#15377,
#15378,#15379,#15380,#15381,#15382,#15383,#15384,#15385,#15386,#15387,#15388,
#15389,#15390,#15391,#15392,#15393,#15394,#15395,#15396,#15397,#15398,#15399,
#15400,#15401,#15402,#15403,#15404,#15405,#15406,#15407,#15408,#15409,#15410,
#15411,#15412,#15413,#15414,#15415,#15416,#15417,#15418,#15419,#15420,#15421,
#15422,#15423,#15424,#15425,#15426,#15427,#15428,#15429,#15430,#15431,#15432,
#15433,#15434,#15435,#15436,#15437,#15438,#15439,#15440,#15441,#15442,#15443,
#15444,#15445,#15446,#15447,#15448,#15449,#15450,#15451,#15452,#15453,#15454,
#15455,#15456,#15457,#15458,#15459,#15460,#15461,#15462,#15463,#15464,#15465,
#15466,#15467,#15468,#15469,#15470,#15471,#15472,#15473,#15474,#15475,#15476,
#15477,#15478,#15479,#15480,#15481,#15482,#15483,#15484,#15485,#15486,#15487,
#15488,#15489,#15490,#15491,#15492,#15493),.UNSPECIFIED.,.F.,.F.,(4,2,2,
2,2,2,2,2,2,2,2,2,2,2,2,2,2,2,2,2,2,2,2,2,2,2,2,2,2,2,2,2,2,2,2,2,2,2,2,
2,2,2,2,2,2,2,2,2,2,2,2,2,2,2,2,2,2,2,2,2,2,2,2,2,2,2,2,2,2,2,2,2,2,2,2,
2,2,2,2,2,2,2,2,2,2,2,2,2,2,2,2,2,2,2,2,2,2,2,2,2,2,2,2,2,2,2,2,2,2,2,2,
2,2,2,2,2,2,2,2,2,2,2,2,2,2,2,2,2,2,2,2,2,2,2,2,2,2,2,2,2,2,2,4),(-3.40187331252921,
-3.36412124741289,-3.30968310554371,-3.28608354083431,-3.27410832604247,
-3.27186664126087,-3.27065758594873,-3.2696628274175,-3.26864346275063,
-3.26674888429633,-3.26049364152775,-3.15332102102897,-3.1257659449776,
-3.11580735230516,-3.11232706015273,-3.11072202079272,-3.10980744504818,
-3.10917884723728,-3.1085758553691,-3.10802293458334,-3.10729205971141,
-3.10572208952273,-3.09449893029603,-3.09219247862971,-3.08920596146183,
-3.08809569036755,-3.07839057879091,-2.98858825442644,-2.96381425827186,
-2.95100065462571,-2.94871591170645,-2.94749755404456,-2.94649287895053,
-2.94547659206097,-2.94359760397715,-2.93747391092113,-2.82773537074217,
-2.78880149043531,-2.78733927968874,-2.78648263518727,-2.78571664844179,
-2.78515451385923,-2.78462497140541,-2.78390128039199,-2.78209775218967,
-2.76173234952193,-2.75726073354586,-2.69909324078275,-2.66508296371755,
-2.64039610954141,-2.62783194945586,-2.62555925016183,-2.62434330631159,
-2.62343608172097,-2.62229961111581,-2.62038884459864,-2.61399876941403,
-2.610051734052,-2.60824352892161,-2.60733015666557,-2.60621263482647,-2.6041198166312,
-2.60224541782368,-2.60101789112454,-2.59932561643077,-2.59308879565364,
-2.50205677295237,-2.48155234346152,-2.46650122405959,-2.46467469179825,
-2.46367188647583,-2.46300648749872,-2.46237763301092,-2.46182905485978,
-2.46113103489759,-2.46005629618995,-2.45522619501713,-2.36265078853053,
-2.3402540630495,-2.31659704727469,-2.30459564179387,-2.30235197212246,
-2.30114222195348,-2.30014708758433,-2.29912750990517,-2.29723304092275,
-2.29098231587382,-2.18671154325818,-2.15674679769867,-2.14641390693721,
-2.14097511127026,-2.13979909461423,-2.13914157569107,-2.13863723003993,
-2.13806439216471,-2.1369837437247,-2.13328004243408,-2.13238636149393,
-2.12981840417762,-2.12824965721844,-2.12691426838688,-2.03243562210988,
-2.01027382174837,-1.98259601532943,-1.9795283221164,-1.97829166807945,
-1.97726224509052,-1.97620817401335,-1.97467215817602,-1.9706342356214,
-1.91585480950935,-1.85558843051331,-1.84039005226584,-1.83240927518667,
-1.81860824190332,-1.81710973959543,-1.816368997954,-1.81583494124016,-1.81526424800612,
-1.81449242717506,-1.81274657021488,-1.7717242492526,-1.66353824274835,
-1.6574001086916,-1.65551917891161,-1.65450238888879,-1.65353048984947,
-1.65235227216252,-1.65109083620079,-1.64913385871923,-1.64546457146241,
-1.61367682834028,-1.56791778459778,-1.4984820109138,-1.49448297144557,
-1.49338328522574,-1.49273631606901,-1.49217519101371,-1.49147808848675,
-1.49011658876561,-1.48091265233273,-1.45831578482449,-1.3706021342809),
 .UNSPECIFIED.);
#98=B_SPLINE_CURVE_WITH_KNOTS('',3,(#15495,#15496,#15497,#15498,#15499,
#15500,#15501,#15502,#15503,#15504,#15505,#15506,#15507,#15508,#15509,#15510,
#15511,#15512,#15513,#15514,#15515,#15516,#15517,#15518,#15519,#15520,#15521,
#15522,#15523,#15524,#15525,#15526,#15527,#15528,#15529,#15530,#15531,#15532,
#15533,#15534,#15535,#15536,#15537,#15538,#15539,#15540,#15541,#15542,#15543,
#15544,#15545,#15546,#15547,#15548,#15549,#15550,#15551,#15552,#15553,#15554,
#15555,#15556,#15557,#15558,#15559,#15560,#15561,#15562,#15563,#15564),
 .UNSPECIFIED.,.F.,.F.,(4,3,3,3,3,3,3,3,3,3,3,3,3,3,3,3,3,3,3,3,3,3,3,4),
(107.909967710001,108.002728714755,108.095466118645,108.188204737573,108.280969381588,
108.373839389017,108.466771599224,108.559846662765,108.587535808621,108.680608752897,
108.773555592534,108.866403963719,108.959184468374,109.051929790531,109.144664755632,
109.237414173973,109.330262814708,109.42316325532,109.516219151404,109.587250464094,
109.693194910979,109.798742509158,109.903582591639,109.955742875448),
 .UNSPECIFIED.);
#99=B_SPLINE_CURVE_WITH_KNOTS('',3,(#15565,#15566,#15567,#15568,#15569,
#15570,#15571,#15572,#15573,#15574,#15575,#15576,#15577,#15578,#15579,#15580,
#15581,#15582,#15583,#15584,#15585,#15586,#15587,#15588,#15589,#15590,#15591,
#15592,#15593,#15594,#15595,#15596,#15597,#15598,#15599,#15600,#15601,#15602,
#15603,#15604,#15605,#15606,#15607,#15608,#15609,#15610,#15611,#15612,#15613,
#15614,#15615,#15616,#15617,#15618,#15619,#15620,#15621,#15622,#15623,#15624,
#15625,#15626,#15627,#15628,#15629,#15630,#15631,#15632,#15633,#15634,#15635,
#15636,#15637,#15638,#15639,#15640,#15641,#15642,#15643,#15644,#15645,#15646,
#15647,#15648,#15649,#15650,#15651,#15652,#15653,#15654,#15655,#15656,#15657,
#15658,#15659,#15660,#15661,#15662,#15663,#15664,#15665,#15666,#15667,#15668,
#15669,#15670,#15671,#15672,#15673,#15674,#15675,#15676,#15677,#15678,#15679,
#15680,#15681,#15682,#15683,#15684,#15685,#15686,#15687,#15688,#15689,#15690,
#15691,#15692,#15693,#15694,#15695,#15696,#15697,#15698,#15699,#15700,#15701,
#15702,#15703,#15704,#15705,#15706,#15707,#15708,#15709,#15710,#15711,#15712,
#15713,#15714,#15715,#15716,#15717,#15718,#15719,#15720,#15721,#15722,#15723,
#15724,#15725,#15726,#15727,#15728,#15729,#15730,#15731,#15732,#15733,#15734,
#15735,#15736,#15737,#15738,#15739,#15740,#15741,#15742,#15743,#15744,#15745,
#15746,#15747,#15748,#15749,#15750,#15751,#15752,#15753,#15754,#15755,#15756,
#15757,#15758,#15759,#15760,#15761,#15762,#15763,#15764,#15765,#15766,#15767,
#15768,#15769,#15770,#15771,#15772,#15773,#15774,#15775,#15776,#15777,#15778,
#15779,#15780,#15781,#15782,#15783,#15784,#15785,#15786,#15787,#15788,#15789,
#15790,#15791,#15792,#15793,#15794),.UNSPECIFIED.,.F.,.F.,(4,2,2,2,2,2,
2,2,2,2,2,2,2,2,2,2,2,2,2,2,2,2,2,2,2,2,2,2,2,2,2,2,2,2,2,2,2,2,2,2,2,2,
2,2,2,2,2,2,2,2,2,2,2,2,2,2,2,2,2,2,2,2,2,2,2,2,2,2,2,2,2,2,2,2,2,2,2,2,
2,2,2,2,2,2,2,2,2,2,2,2,2,2,2,2,2,2,2,2,2,2,2,2,2,2,2,2,2,2,2,2,2,2,2,2,
4),(-4.06398272956981,-4.02654081354827,-4.02446721588437,-4.02315633577637,
-4.02215694944922,-4.0211965879973,-4.02024817632782,-4.01896165171567,
-4.01644672542685,-3.99681327641816,-3.99055248907445,-3.98295092746506,
-3.97726740099106,-3.89472643356396,-3.86560891437986,-3.86293525861883,
-3.86099843345383,-3.86019292754274,-3.85961598417565,-3.85908953963678,
-3.85837891222914,-3.85699968832063,-3.84670078631966,-3.75261826487865,
-3.7278174683751,-3.71096634124997,-3.70490944193815,-3.70072162314768,
-3.69916617934145,-3.69822406961208,-3.69720511181753,-3.69588259377633,
-3.69301503694688,-3.68507315740922,-3.68273549462731,-3.68149055527552,
-3.68044338737323,-3.67978478709712,-3.6757927034971,-3.67459643863632,
-3.67310037544265,-3.66849699075183,-3.6611111438708,-3.60923402252179,
-3.60341269043478,-3.57432184551967,-3.54879406223136,-3.53887235319483,
-3.53748554181394,-3.53678297630624,-3.53627455231809,-3.53572725505765,
-3.53477405051823,-3.53207146328394,-3.52971850461946,-3.44456140600255,
-3.40691101698071,-3.38849483783438,-3.38202346311345,-3.37905135526909,
-3.37669424445445,-3.37546602027281,-3.37447386328896,-3.37333523506362,
-3.37141643028461,-3.36496208804944,-3.36104167655824,-3.35926349675722,
-3.35711468686016,-3.35503022912267,-3.35015563032939,-3.34515601621909,
-3.26083015931368,-3.24957928187052,-3.21629008336503,-3.21445309556672,
-3.21366482647362,-3.21309108577417,-3.21256088286679,-3.21183543072234,
-3.21039825905946,-3.19852592481607,-3.13956530349988,-3.09330829475832,
-3.0685063857932,-3.06010413968315,-3.05649486624137,-3.05373321458639,
-3.05242208983903,-3.05145815311605,-3.05050426580544,-3.04919648771829,
-3.04590838953056,-3.00566473059495,-2.96728200593774,-2.92047610553774,
-2.90090444746831,-2.89238870437015,-2.89105279108915,-2.89036078957903,
-2.88979970071162,-2.88923318120779,-2.8881845453131,-2.88475769855497,
-2.82866084758995,-2.73688129554516,-2.7332534662231,-2.73131225924506,
-2.72964797470032,-2.72857582118082,-2.72755680439306,-2.72623343293228,
-2.72336095381366,-2.70172361874953,-2.69388977725967),.UNSPECIFIED.);
#100=B_SPLINE_CURVE_WITH_KNOTS('',3,(#15800,#15801,#15802,#15803,#15804,
#15805,#15806,#15807,#15808,#15809,#15810,#15811,#15812,#15813,#15814,#15815,
#15816,#15817,#15818,#15819,#15820,#15821,#15822,#15823,#15824,#15825,#15826,
#15827,#15828,#15829,#15830,#15831,#15832,#15833,#15834,#15835,#15836,#15837,
#15838,#15839,#15840,#15841,#15842,#15843,#15844,#15845,#15846,#15847,#15848,
#15849,#15850,#15851,#15852,#15853,#15854,#15855,#15856,#15857,#15858,#15859,
#15860,#15861,#15862,#15863,#15864,#15865,#15866,#15867,#15868,#15869,#15870,
#15871,#15872,#15873,#15874,#15875,#15876,#15877,#15878,#15879,#15880,#15881,
#15882,#15883,#15884,#15885,#15886,#15887,#15888,#15889,#15890,#15891,#15892,
#15893,#15894,#15895,#15896,#15897,#15898,#15899,#15900,#15901,#15902,#15903,
#15904,#15905,#15906,#15907,#15908,#15909,#15910,#15911,#15912,#15913,#15914,
#15915,#15916,#15917,#15918,#15919,#15920,#15921,#15922,#15923,#15924,#15925,
#15926,#15927,#15928,#15929,#15930,#15931,#15932,#15933,#15934,#15935,#15936,
#15937,#15938,#15939,#15940,#15941,#15942,#15943,#15944,#15945,#15946,#15947,
#15948,#15949,#15950,#15951,#15952,#15953,#15954,#15955,#15956,#15957,#15958,
#15959,#15960,#15961,#15962,#15963,#15964,#15965,#15966,#15967,#15968,#15969,
#15970,#15971,#15972,#15973,#15974,#15975,#15976,#15977,#15978,#15979,#15980,
#15981,#15982,#15983,#15984,#15985,#15986,#15987,#15988,#15989,#15990,#15991,
#15992,#15993,#15994,#15995,#15996,#15997,#15998,#15999,#16000,#16001,#16002,
#16003,#16004,#16005,#16006,#16007,#16008,#16009,#16010,#16011,#16012,#16013,
#16014,#16015,#16016,#16017,#16018,#16019,#16020,#16021,#16022,#16023,#16024,
#16025),.UNSPECIFIED.,.F.,.F.,(4,2,2,2,2,2,2,2,2,2,2,2,2,2,2,2,2,2,2,2,
2,2,2,2,2,2,2,2,2,2,2,2,2,2,2,2,2,2,2,2,2,2,2,2,2,2,2,2,2,2,2,2,2,2,2,2,
2,2,2,2,2,2,2,2,2,2,2,2,2,2,2,2,2,2,2,2,2,2,2,2,2,2,2,2,2,2,2,2,2,2,2,2,
2,2,2,2,2,2,2,2,2,2,2,2,2,2,2,2,2,2,2,2,4),(-1.37047652883368,-1.32015777460888,
-1.31866669325793,-1.31713841650632,-1.31469840959735,-1.31341532264545,
-1.30992192873267,-1.30886572146225,-1.30829787964147,-1.30774832096595,
-1.30707857700824,-1.30635572846671,-1.30521599870066,-1.30303483706847,
-1.28262796328326,-1.26941444163345,-1.18240240930743,-1.15193855433878,
-1.14911052091622,-1.14774587239272,-1.14677727201455,-1.1458638296299,
-1.14459620530877,-1.14207645991256,-1.12311889143595,-1.0940855982088,
-0.991401973109268,-0.990372138340198,-0.986748198684808,-0.98567666999011,
-0.98510568741204,-0.984556342112059,-0.983888687264163,-0.983171268684019,
-0.982044564542278,-0.979897811491443,-0.974737869163734,-0.959430256075991,
-0.946215905879761,-0.859252288528087,-0.828716109103562,-0.825886092919283,
-0.824520857644493,-0.8235520078953,-0.822638465682966,-0.821370917252886,
-0.818852097037579,-0.799935527825703,-0.771015318814669,-0.758535945108684,
-0.747263999051615,-0.668316289869753,-0.667256980918422,-0.663622509221959,
-0.662549773116947,-0.661978548022892,-0.661429132480898,-0.660764599594385,
-0.660048822273431,-0.658926026716913,-0.656789537254835,-0.651662985562846,
-0.636072203056154,-0.614635644907025,-0.50957791636679,-0.503424390670518,
-0.501541571629006,-0.50052437820154,-0.499519535850313,-0.498302022789894,
-0.496021957196585,-0.483310172221965,-0.458504351789894,-0.430070672743369,
-0.421427016637148,-0.414111829165556,-0.407776380358645,-0.390596515324826,
-0.361798197447345,-0.341726506647209,-0.339929551797598,-0.339207013956112,
-0.338677782721056,-0.338115520135312,-0.337349416180117,-0.336491757610056,
-0.335027054029267,-0.331953504174857,-0.32355009940443,-0.301903294756425,
-0.186219288193886,-0.180223076974626,-0.178359645701891,-0.177346535773835,
-0.176341692319634,-0.175118351602603,-0.172810012876453,-0.159503064781469,
-0.144312393986993,-0.113889603883803,-0.0311711628329554,-0.0277257105112761,
-0.0255750214978552,-0.0239273561288705,-0.0176862322117764,-0.0165103725667851,
-0.0157813568243212,-0.0152362952012227,-0.0147109123534575,-0.0141006338598269,
-0.0132307052039227,-0.011735848888498,-0.000960909134095826),
 .UNSPECIFIED.);
#101=B_SPLINE_CURVE_WITH_KNOTS('',3,(#16026,#16027,#16028,#16029,#16030,
#16031,#16032,#16033,#16034,#16035,#16036,#16037,#16038,#16039,#16040,#16041,
#16042,#16043,#16044,#16045,#16046,#16047,#16048,#16049,#16050,#16051,#16052,
#16053,#16054,#16055,#16056,#16057,#16058,#16059,#16060,#16061,#16062,#16063,
#16064,#16065,#16066,#16067,#16068,#16069,#16070,#16071,#16072,#16073,#16074,
#16075,#16076,#16077,#16078,#16079,#16080,#16081,#16082,#16083,#16084,#16085,
#16086,#16087,#16088,#16089,#16090,#16091,#16092,#16093,#16094,#16095,#16096,
#16097,#16098,#16099,#16100,#16101,#16102,#16103,#16104,#16105,#16106,#16107,
#16108,#16109,#16110,#16111,#16112,#16113,#16114,#16115,#16116,#16117,#16118,
#16119,#16120,#16121,#16122,#16123,#16124,#16125,#16126,#16127,#16128,#16129,
#16130,#16131,#16132,#16133,#16134,#16135),.UNSPECIFIED.,.F.,.F.,(4,2,2,
2,2,2,2,2,2,2,2,2,2,2,2,2,2,2,2,2,2,2,2,2,2,2,2,2,2,2,2,2,2,2,2,2,2,2,2,
2,2,2,2,2,2,2,2,2,2,2,2,2,2,2,4),(-4.06305007721485,-3.97924169820498,-3.9244464609644,
-3.9190345797772,-3.91731422313055,-3.9162207785557,-3.91520301699057,-3.91388182695187,
-3.91101626260136,-3.90308596809809,-3.90123825875958,-3.8991811117024,
-3.89863748447152,-3.8978367324572,-3.89576500712487,-3.89418233327144,
-3.89297875150491,-3.89166879807271,-3.88550812741958,-3.79491451298384,
-3.76868497009556,-3.76086909432057,-3.75795521282537,-3.75654704327038,
-3.7557126879182,-3.75496272130919,-3.75440362541422,-3.75387023445072,
-3.75313115750644,-3.75163834424098,-3.73800291105518,-3.70971297963672,
-3.68536572454858,-3.6325979423156,-3.60908025085917,-3.59714155810716,
-3.59490212374948,-3.59369368950823,-3.59269913265779,-3.59167970264798,
-3.58978420336728,-3.58351933365664,-3.4764260459048,-3.45722877594643,
-3.44155274378925,-3.43644594432405,-3.43431586889472,-3.43319567853982,
-3.43224424692824,-3.43164226031687,-3.43108906362718,-3.43035608281952,
-3.42877459387615,-3.41725489965834,-3.40187331252921),.UNSPECIFIED.);
#102=B_SPLINE_CURVE_WITH_KNOTS('',3,(#16136,#16137,#16138,#16139,#16140,
#16141,#16142,#16143,#16144,#16145,#16146,#16147,#16148,#16149,#16150,#16151,
#16152,#16153,#16154,#16155,#16156,#16157,#16158,#16159,#16160,#16161,#16162,
#16163,#16164,#16165,#16166,#16167,#16168,#16169,#16170,#16171,#16172,#16173,
#16174,#16175,#16176,#16177,#16178,#16179,#16180,#16181,#16182,#16183,#16184,
#16185,#16186,#16187,#16188,#16189,#16190,#16191,#16192,#16193,#16194,#16195,
#16196,#16197,#16198,#16199,#16200,#16201,#16202,#16203,#16204,#16205,#16206,
#16207,#16208,#16209,#16210,#16211,#16212,#16213,#16214,#16215,#16216,#16217,
#16218,#16219,#16220,#16221,#16222,#16223,#16224,#16225,#16226,#16227,#16228,
#16229,#16230,#16231,#16232,#16233,#16234,#16235,#16236,#16237,#16238,#16239,
#16240,#16241,#16242,#16243,#16244,#16245,#16246,#16247,#16248,#16249,#16250,
#16251,#16252,#16253,#16254,#16255,#16256,#16257,#16258,#16259,#16260,#16261,
#16262,#16263,#16264,#16265,#16266,#16267,#16268,#16269,#16270,#16271,#16272,
#16273,#16274,#16275,#16276,#16277,#16278,#16279,#16280,#16281,#16282,#16283,
#16284,#16285,#16286,#16287,#16288,#16289,#16290,#16291,#16292,#16293,#16294,
#16295,#16296,#16297,#16298,#16299,#16300,#16301,#16302,#16303,#16304,#16305,
#16306,#16307,#16308,#16309,#16310,#16311,#16312,#16313,#16314,#16315,#16316,
#16317,#16318,#16319,#16320,#16321,#16322,#16323,#16324,#16325,#16326,#16327,
#16328,#16329,#16330,#16331,#16332,#16333,#16334,#16335,#16336,#16337,#16338,
#16339,#16340,#16341,#16342,#16343,#16344,#16345,#16346,#16347,#16348,#16349,
#16350,#16351,#16352,#16353,#16354,#16355,#16356,#16357,#16358,#16359,#16360,
#16361,#16362,#16363,#16364,#16365,#16366,#16367,#16368,#16369,#16370,#16371,
#16372,#16373,#16374,#16375,#16376,#16377,#16378,#16379,#16380,#16381,#16382,
#16383,#16384,#16385,#16386,#16387,#16388,#16389,#16390,#16391,#16392,#16393,
#16394,#16395,#16396,#16397,#16398,#16399,#16400,#16401,#16402,#16403,#16404,
#16405,#16406,#16407,#16408,#16409,#16410,#16411,#16412,#16413,#16414,#16415,
#16416,#16417,#16418,#16419,#16420,#16421,#16422,#16423,#16424,#16425),
 .UNSPECIFIED.,.F.,.F.,(4,2,2,2,2,2,2,2,2,2,2,2,2,2,2,2,2,2,2,2,2,2,2,2,
2,2,2,2,2,2,2,2,2,2,2,2,2,2,2,2,2,2,2,2,2,2,2,2,2,2,2,2,2,2,2,2,2,2,2,2,
2,2,2,2,2,2,2,2,2,2,2,2,2,2,2,2,2,2,2,2,2,2,2,2,2,2,2,2,2,2,2,2,2,2,2,2,
2,2,2,2,2,2,2,2,2,2,2,2,2,2,2,2,2,2,2,2,2,2,2,2,2,2,2,2,2,2,2,2,2,2,2,2,
2,2,2,2,2,2,2,2,2,2,2,2,4),(-2.69388977725967,-2.6851136547513,-2.61508267689467,
-2.57346186320606,-2.56874085581754,-2.56761681423595,-2.56697064634882,
-2.5664091192115,-2.56571010875245,-2.56463265998276,-2.55977238602004,
-2.46532306061889,-2.41568959032365,-2.41096053871554,-2.40860405341503,
-2.40717463869383,-2.40587521721452,-2.4048776062012,-2.4039141931778,-2.40256993632514,
-2.39982602501282,-2.39212326781216,-2.3903017890458,-2.38823990838823,
-2.38787532026275,-2.38692370568897,-2.38485288537864,-2.38323576033008,
-2.3820313730094,-2.3807166856708,-2.3751448680323,-2.35820669967274,-2.32027375313843,
-2.28706216750734,-2.24654485926836,-2.24479322940269,-2.24402024177927,
-2.24344923450465,-2.24291529478182,-2.24217533675948,-2.24068036653065,
-2.22700823551189,-2.22590929780619,-2.22031929864552,-2.12518392886676,
-2.09085500383044,-2.08504169249523,-2.08327375147513,-2.0821690422674,
-2.08115373943468,-2.07985371792872,-2.07710294276368,-2.05849088157125,
-2.05698223736249,-2.05042651663368,-2.03207056949148,-1.98163952081821,
-1.92564681838314,-1.92221191363842,-1.92116248378489,-1.92059590049224,
-1.92003498584034,-1.91934354497545,-1.91800977156754,-1.90954056255925,
-1.89021498696306,-1.84481093873609,-1.81454832599172,-1.79436341789003,
-1.76429220620313,-1.76147239776307,-1.76010948432152,-1.75914110446856,
-1.75822704975483,-1.75695727380209,-1.75442853761386,-1.73519315324488,
-1.70542779608413,-1.61955303866336,-1.61750300535891,-1.61730236241659,
-1.61457685229036,-1.61418079831197,-1.61206074665341,-1.60003086215566,
-1.59842886360977,-1.59769167048632,-1.59713759557758,-1.59653690345812,
-1.59591182193447,-1.59500613068263,-1.59342352533907,-1.53777337459545,
-1.44446072373319,-1.43882355023647,-1.43700460201491,-1.43600005926753,
-1.43499362553581,-1.43375350669716,-1.43136795542398,-1.41631078014225,
-1.38228818157669,-1.30454420496675,-1.2773032585065,-1.2753717200684,-1.27462607521874,
-1.27409062056098,-1.27353195134802,-1.2727867131723,-1.27195915095113,
-1.27056808868535,-1.23902434373396,-1.12128239433162,-1.11547286980214,
-1.11363210807778,-1.11262327901102,-1.11171811271651,-1.11052958564131,
-1.10838423209916,-1.09808135107253,-1.07861922967001,-1.01936677984926,
-0.963502042356076,-0.953313039447118,-0.951786579945251,-0.95106391431444,
-0.950515700316939,-0.949909496111643,-0.948941007298574,-0.947795579378007,
-0.945599540308642,-0.940278503737567,-0.929807066247697,-0.906269457025552,
-0.798485071534662,-0.792332489804904,-0.790449756938305,-0.789432565622241,
-0.788427697491999,-0.787210113173972,-0.784929795867358,-0.772213717519427,
-0.747406024807181,-0.69539673935075,-0.662451535145792),.UNSPECIFIED.);
#103=B_SPLINE_CURVE_WITH_KNOTS('',3,(#16430,#16431,#16432,#16433,#16434,
#16435,#16436,#16437,#16438,#16439,#16440,#16441,#16442,#16443,#16444,#16445,
#16446,#16447,#16448,#16449,#16450,#16451,#16452,#16453,#16454,#16455,#16456,
#16457,#16458,#16459,#16460,#16461,#16462,#16463,#16464,#16465,#16466,#16467,
#16468,#16469,#16470,#16471,#16472,#16473,#16474,#16475,#16476,#16477,#16478,
#16479,#16480,#16481,#16482,#16483,#16484,#16485,#16486,#16487,#16488,#16489,
#16490,#16491,#16492,#16493,#16494,#16495,#16496,#16497,#16498,#16499,#16500,
#16501,#16502,#16503,#16504,#16505,#16506,#16507,#16508,#16509,#16510,#16511,
#16512,#16513,#16514,#16515,#16516,#16517,#16518,#16519,#16520,#16521,#16522,
#16523,#16524,#16525,#16526,#16527,#16528,#16529,#16530,#16531,#16532,#16533,
#16534,#16535,#16536,#16537,#16538,#16539,#16540,#16541,#16542,#16543,#16544,
#16545,#16546,#16547,#16548,#16549,#16550,#16551,#16552,#16553,#16554,#16555,
#16556,#16557,#16558,#16559,#16560,#16561,#16562,#16563,#16564,#16565,#16566,
#16567,#16568,#16569,#16570,#16571,#16572,#16573,#16574,#16575,#16576,#16577,
#16578,#16579,#16580,#16581,#16582,#16583,#16584,#16585,#16586,#16587,#16588,
#16589,#16590,#16591,#16592,#16593,#16594,#16595,#16596,#16597,#16598,#16599,
#16600,#16601,#16602,#16603,#16604,#16605,#16606,#16607,#16608,#16609,#16610,
#16611,#16612,#16613,#16614,#16615,#16616,#16617,#16618,#16619,#16620,#16621,
#16622,#16623,#16624,#16625,#16626,#16627,#16628,#16629,#16630,#16631,#16632,
#16633,#16634,#16635,#16636,#16637,#16638,#16639,#16640,#16641,#16642,#16643,
#16644,#16645,#16646,#16647,#16648,#16649,#16650,#16651,#16652,#16653,#16654,
#16655,#16656,#16657,#16658,#16659,#16660,#16661,#16662,#16663,#16664,#16665,
#16666,#16667,#16668,#16669,#16670,#16671,#16672,#16673,#16674,#16675,#16676,
#16677,#16678,#16679,#16680,#16681,#16682,#16683,#16684,#16685,#16686,#16687,
#16688,#16689,#16690,#16691,#16692,#16693,#16694,#16695,#16696,#16697,#16698,
#16699,#16700,#16701,#16702,#16703,#16704,#16705,#16706,#16707,#16708,#16709,
#16710,#16711,#16712,#16713,#16714,#16715,#16716,#16717,#16718,#16719,#16720,
#16721,#16722,#16723),.UNSPECIFIED.,.F.,.F.,(4,2,2,2,2,2,2,2,2,2,2,2,2,
2,2,2,2,2,2,2,2,2,2,2,2,2,2,2,2,2,2,2,2,2,2,2,2,2,2,2,2,2,2,2,2,2,2,2,2,
2,2,2,2,2,2,2,2,2,2,2,2,2,2,2,2,2,2,2,2,2,2,2,2,2,2,2,2,2,2,2,2,2,2,2,2,
2,2,2,2,2,2,2,2,2,2,2,2,2,2,2,2,2,2,2,2,2,2,2,2,2,2,2,2,2,2,2,2,2,2,2,2,
2,2,2,2,2,2,2,2,2,2,2,2,2,2,2,2,2,2,2,2,2,2,2,2,2,4),(-3.40092133460055,
-3.37208765681694,-3.31259585721469,-3.30287183130673,-3.29158746134574,
-3.27527702434948,-3.25717197177797,-3.24888597237038,-3.24756043838951,
-3.24687104916474,-3.24631065909886,-3.24574362833148,-3.24469060006688,
-3.24122141334538,-3.18492861723304,-3.13471292523924,-3.10367567637488,
-3.09425915413262,-3.09033129069727,-3.08827509555633,-3.0869720042922,
-3.08576406007583,-3.08477821218417,-3.08377702567792,-3.08197218007508,
-3.0764366481723,-2.95691450953366,-2.94778867218672,-2.93384219629616,
-2.92575638141298,-2.92443895184821,-2.92375114518264,-2.92319068109186,
-2.92262240457085,-2.92156372400094,-2.91804841430752,-2.86060572053334,
-2.8107650970263,-2.77153003703433,-2.76736954974624,-2.76522490347797,
-2.76388445465652,-2.76264834371954,-2.76165979248964,-2.76067170750641,
-2.75923613124485,-2.75513646594884,-2.69248720588548,-2.60767496413981,
-2.60244469714682,-2.6012832540454,-2.60062903860656,-2.60012490403089,
-2.59954981358211,-2.59845751905003,-2.59464788579388,-2.5939069826619,
-2.49102007879781,-2.44866434201676,-2.44431637222793,-2.44210133799806,
-2.44073133572249,-2.43947506033328,-2.4384839714167,-2.43750558492391,
-2.4358154068616,-2.43110474638592,-2.35765706617824,-2.3317830747326,-2.30270885500215,
-2.28703564616352,-2.27953421961183,-2.27824284099499,-2.2775605428162,
-2.27700558081775,-2.27643540003602,-2.27536728549531,-2.27177116387227,
-2.27064391621703,-2.26817708014668,-2.26662127526971,-2.2652965151977,
-2.23423738136989,-2.17262510943809,-2.1358806488201,-2.12010503638469,
-2.11769231035247,-2.11644687972784,-2.1155364849899,-2.11455884679202,
-2.11316092862699,-2.10931221871045,-2.10778326254082,-2.03148842072216,
-1.96051602255745,-1.95624819748195,-1.95512130961897,-1.95446803346771,
-1.95390746014414,-1.9532186341145,-1.95189657368913,-1.94370358202902,
-1.92667926578758,-1.90207254210137,-1.82788091212383,-1.79813946047098,
-1.79532832375655,-1.79396783153678,-1.79300036966583,-1.79208652947597,
-1.79081601510622,-1.78828204470306,-1.76883578310293,-1.73850093792796,
-1.64532967358157,-1.63388389161355,-1.63230479047895,-1.63157209534144,
-1.6310186656775,-1.63050976754623,-1.62963997049116,-1.62863680051688,
-1.62680932053924,-1.61174540830877,-1.59121009070122,-1.50019332639202,
-1.49399410575801,-1.49262009457137,-1.49141530177704,-1.48988426238721,
-1.48780582812421,-1.487143904756,-1.48612181119718,-1.48477891199037,-1.48394343719247,
-1.48288896541455,-1.47796765379112,-1.47271119125132,-1.47094319661123,
-1.46994915323991,-1.46904227540172,-1.46782966682866,-1.46557240374456,
-1.45330935913335,-1.42909842763686,-1.3874405607434,-1.37047652883368),
 .UNSPECIFIED.);
#104=B_SPLINE_CURVE_WITH_KNOTS('',3,(#16725,#16726,#16727,#16728,#16729,
#16730,#16731,#16732,#16733,#16734,#16735,#16736,#16737,#16738,#16739,#16740,
#16741,#16742,#16743,#16744,#16745,#16746,#16747,#16748,#16749,#16750,#16751,
#16752,#16753,#16754,#16755,#16756,#16757,#16758,#16759,#16760,#16761,#16762,
#16763,#16764,#16765,#16766,#16767,#16768,#16769,#16770,#16771,#16772,#16773,
#16774,#16775,#16776,#16777,#16778,#16779,#16780,#16781,#16782,#16783,#16784,
#16785,#16786,#16787,#16788,#16789,#16790,#16791,#16792,#16793,#16794,#16795,
#16796,#16797,#16798,#16799,#16800,#16801,#16802,#16803,#16804,#16805,#16806,
#16807,#16808,#16809,#16810,#16811,#16812,#16813,#16814,#16815,#16816,#16817,
#16818,#16819,#16820,#16821,#16822,#16823,#16824,#16825,#16826),
 .UNSPECIFIED.,.F.,.F.,(4,2,2,2,2,2,2,2,2,2,2,2,2,2,2,2,2,2,2,2,2,2,2,2,
2,2,2,2,2,2,2,2,2,2,2,2,2,2,2,2,2,2,2,2,2,2,2,2,2,2,4),(-0.662451535145792,
-0.645810712341655,-0.644992134691527,-0.643181364863394,-0.642810009039171,
-0.641843904234085,-0.630229765060319,-0.628802146326098,-0.628079329335985,
-0.627550000758681,-0.626987636164697,-0.626220616775371,-0.625362573165249,
-0.623896974244966,-0.620820950420398,-0.612408530545876,-0.591397558806022,
-0.475122203490112,-0.469095202339053,-0.467227927771129,-0.466213998841606,
-0.465209145512529,-0.46398695277449,-0.461684246652782,-0.448499038718396,
-0.426312219124871,-0.374675550308374,-0.351107634455943,-0.308106662573644,
-0.305833170026884,-0.305035194368541,-0.304485632399452,-0.303937410649659,
-0.303235080666701,-0.301924337612005,-0.30020772363746,-0.296395477252509,
-0.285118325946625,-0.265002978359321,-0.174999601100703,-0.167332949980977,
-0.165301147192011,-0.147579253528041,-0.144868849869099,-0.143563104117543,
-0.142550501601466,-0.14143893040224,-0.139638392106187,-0.133522190226728,
-0.0962401497852022,-0.000962418729335946),.UNSPECIFIED.);
#105=B_SPLINE_CURVE_WITH_KNOTS('',3,(#16827,#16828,#16829,#16830,#16831,
#16832,#16833,#16834,#16835,#16836,#16837,#16838,#16839,#16840,#16841,#16842,
#16843,#16844,#16845,#16846,#16847,#16848,#16849,#16850,#16851,#16852,#16853,
#16854,#16855,#16856,#16857,#16858,#16859,#16860,#16861,#16862,#16863,#16864,
#16865,#16866,#16867,#16868,#16869,#16870,#16871,#16872,#16873,#16874,#16875,
#16876,#16877,#16878,#16879,#16880,#16881,#16882,#16883,#16884,#16885,#16886,
#16887,#16888,#16889,#16890,#16891,#16892,#16893,#16894,#16895,#16896,#16897,
#16898,#16899,#16900,#16901,#16902,#16903,#16904,#16905,#16906,#16907,#16908,
#16909,#16910,#16911,#16912,#16913,#16914,#16915,#16916,#16917,#16918,#16919,
#16920,#16921,#16922,#16923,#16924,#16925,#16926,#16927,#16928,#16929,#16930,
#16931,#16932,#16933,#16934,#16935,#16936,#16937,#16938,#16939,#16940,#16941,
#16942,#16943,#16944,#16945,#16946,#16947,#16948,#16949,#16950,#16951,#16952,
#16953,#16954,#16955,#16956,#16957,#16958,#16959,#16960,#16961,#16962,#16963,
#16964,#16965,#16966,#16967,#16968,#16969,#16970,#16971,#16972,#16973,#16974,
#16975,#16976,#16977,#16978,#16979,#16980,#16981,#16982,#16983,#16984,#16985,
#16986,#16987,#16988,#16989,#16990,#16991,#16992,#16993,#16994,#16995,#16996,
#16997,#16998,#16999,#17000,#17001,#17002,#17003,#17004,#17005,#17006,#17007,
#17008,#17009,#17010,#17011,#17012,#17013,#17014,#17015,#17016,#17017,#17018,
#17019,#17020,#17021,#17022,#17023,#17024,#17025,#17026,#17027,#17028,#17029,
#17030,#17031,#17032,#17033,#17034,#17035,#17036,#17037,#17038,#17039,#17040,
#17041,#17042,#17043,#17044,#17045,#17046,#17047,#17048,#17049,#17050,#17051,
#17052,#17053,#17054,#17055,#17056,#17057,#17058,#17059,#17060,#17061,#17062,
#17063,#17064,#17065,#17066),.UNSPECIFIED.,.F.,.F.,(4,2,2,2,2,2,2,2,2,2,
2,2,2,2,2,2,2,2,2,2,2,2,2,2,2,2,2,2,2,2,2,2,2,2,2,2,2,2,2,2,2,2,2,2,2,2,
2,2,2,2,2,2,2,2,2,2,2,2,2,2,2,2,2,2,2,2,2,2,2,2,2,2,2,2,2,2,2,2,2,2,2,2,
2,2,2,2,2,2,2,2,2,2,2,2,2,2,2,2,2,2,2,2,2,2,2,2,2,2,2,2,2,2,2,2,2,2,2,2,
2,4),(-4.05916345069716,-4.04238701742415,-4.0412065698486,-4.04046692611738,
-4.03990742164276,-4.03937351232827,-4.03884440649689,-4.03812094878392,
-4.03668921855855,-4.02492401590026,-4.02166665959467,-4.01813823905508,
-3.9311910304044,-3.90169236769069,-3.88256796975933,-3.88004547504971,
-3.87877812076469,-3.87786552687871,-3.87689843295007,-3.87553689947498,
-3.87271854108454,-3.84257004358246,-3.75536061535205,-3.73490766426559,
-3.72432949815798,-3.72069292615289,-3.71903545146009,-3.71772750156719,
-3.71704540014503,-3.71648838763052,-3.71584320447735,-3.71474935093017,
-3.71079893284687,-3.70739428217192,-3.70626206387556,-3.7045076413685,
-3.65362265165293,-3.6484681959611,-3.64263023559689,-3.63591998347896,
-3.62805570770431,-3.61856255594855,-3.60648396660814,-3.56522070048555,
-3.55871926063678,-3.55687939890934,-3.55575954493738,-3.55474981667737,
-3.55346220331885,-3.55084015757565,-3.53494715461474,-3.53379878434067,
-3.5325852347665,-3.53117874568734,-3.52542289888392,-3.48073866948945,
-3.43153015691186,-3.41025156527975,-3.40111765815316,-3.39785158352882,
-3.39632032357312,-3.39509350441574,-3.39442924084434,-3.39388048678388,
-3.39330996719067,-3.39223860286589,-3.38860919490417,-3.38755019788473,
-3.30514201999507,-3.29444807927639,-3.28153437390937,-3.24232442513772,
-3.23816708976306,-3.23504939593596,-3.23366720607616,-3.23264360723344,
-3.23169407521747,-3.2303991361461,-3.22784720277224,-3.20710276626331,
-3.20384980220311,-3.12578467054706,-3.10057067855046,-3.08208610857851,
-3.07657532391301,-3.0743225768046,-3.07315613877911,-3.07242234778116,
-3.07174471321827,-3.07119520108778,-3.07063293801307,-3.06960254686128,
-3.06631667699852,-3.00983817987694,-2.96129739873415,-2.9199064471678,
-2.91339311804808,-2.91155203701303,-2.91043190081032,-2.90942221607034,
-2.90813506801497,-2.90551539111582,-2.88966969124545,-2.88842054088033,
-2.88721063871179,-2.88571490739149,-2.88030591338413,-2.86004764387467,
-2.7865337635708,-2.77343855903824,-2.75370065406698,-2.75156289485082,
-2.75043998084599,-2.74972443465644,-2.74906021157489,-2.74851140739545,
-2.74794109974639,-2.7468709075016,-2.74325209895275,-2.69174590048981),
 .UNSPECIFIED.);
#106=B_SPLINE_CURVE_WITH_KNOTS('',3,(#17072,#17073,#17074,#17075,#17076,
#17077,#17078,#17079,#17080,#17081,#17082,#17083,#17084,#17085,#17086,#17087,
#17088,#17089,#17090,#17091,#17092,#17093,#17094,#17095,#17096,#17097,#17098,
#17099,#17100,#17101,#17102,#17103,#17104,#17105,#17106,#17107,#17108,#17109,
#17110,#17111,#17112,#17113,#17114,#17115,#17116,#17117,#17118,#17119,#17120,
#17121,#17122,#17123,#17124,#17125,#17126,#17127,#17128,#17129,#17130,#17131,
#17132,#17133,#17134,#17135,#17136,#17137,#17138,#17139,#17140,#17141,#17142,
#17143,#17144,#17145,#17146,#17147,#17148,#17149,#17150,#17151,#17152,#17153,
#17154,#17155,#17156,#17157,#17158,#17159,#17160,#17161,#17162,#17163,#17164,
#17165,#17166,#17167,#17168,#17169,#17170,#17171,#17172,#17173,#17174,#17175,
#17176,#17177,#17178,#17179,#17180,#17181,#17182,#17183,#17184,#17185,#17186,
#17187,#17188,#17189,#17190,#17191,#17192,#17193,#17194,#17195,#17196,#17197,
#17198,#17199,#17200,#17201,#17202,#17203,#17204,#17205,#17206,#17207,#17208,
#17209,#17210,#17211,#17212,#17213,#17214,#17215,#17216,#17217,#17218,#17219,
#17220,#17221,#17222,#17223,#17224,#17225,#17226,#17227,#17228,#17229,#17230,
#17231,#17232,#17233,#17234,#17235,#17236,#17237,#17238,#17239),
 .UNSPECIFIED.,.F.,.F.,(4,2,2,2,2,2,2,2,2,2,2,2,2,2,2,2,2,2,2,2,2,2,2,2,
2,2,2,2,2,2,2,2,2,2,2,2,2,2,2,2,2,2,2,2,2,2,2,2,2,2,2,2,2,2,2,2,2,2,2,2,
2,2,2,2,2,2,2,2,2,2,2,2,2,2,2,2,2,2,2,2,2,2,2,4),(-1.37002790224387,-1.29458298591376,
-1.28832508550233,-1.2864304459289,-1.28541121093775,-1.28442747248207,
-1.28324781545256,-1.28198537890397,-1.28002551568158,-1.27634808511337,
-1.24443219341799,-1.17754373071881,-1.12805991616991,-1.12519837762381,
-1.12422299783737,-1.123671630036,-1.12316495861639,-1.12247314039283,-1.12113598052038,
-1.11256179051614,-1.09266919370706,-1.0374060098776,-0.969107684862878,
-0.964884191471012,-0.963269402451135,-0.962306094948808,-0.961310768302774,
-0.960013783520247,-0.95858897723759,-0.956242509914642,-0.95153904273292,
-0.902399762192698,-0.807554643742085,-0.802637298308287,-0.801555880602724,
-0.800855951415351,-0.800294795385586,-0.799650287599147,-0.798532176764302,
-0.793878024485553,-0.770703558316142,-0.717435588570115,-0.686797711688131,
-0.644875675102968,-0.641561826201076,-0.640250351806751,-0.639296066098815,
-0.638294730544241,-0.636966622950325,-0.635498860213016,-0.633049327612804,
-0.628063681706848,-0.615089653853534,-0.584469575245545,-0.490284224177784,
-0.48019066509845,-0.478668854023999,-0.477947241727922,-0.477382413841213,
-0.476758334024105,-0.475731953869423,-0.472101190199959,-0.39060262223377,
-0.36530153366235,-0.321837415997487,-0.318498418093149,-0.317182581462893,
-0.316227074300268,-0.315226251145087,-0.313901775479984,-0.312439146319131,
-0.310002126542875,-0.305051208421974,-0.249972416504298,-0.16121522939384,
-0.156532897892942,-0.155470365242569,-0.154776212944072,-0.154271385927652,
-0.153641949625458,-0.152591867695583,-0.148721055014533,-0.0601448328895587,
-0.000961830990748762),.UNSPECIFIED.);
#107=B_SPLINE_CURVE_WITH_KNOTS('',3,(#17240,#17241,#17242,#17243,#17244,
#17245,#17246,#17247,#17248,#17249,#17250,#17251,#17252,#17253,#17254,#17255,
#17256,#17257,#17258,#17259,#17260,#17261,#17262,#17263,#17264,#17265,#17266,
#17267,#17268,#17269,#17270,#17271,#17272,#17273,#17274,#17275,#17276,#17277,
#17278,#17279,#17280,#17281,#17282,#17283,#17284,#17285,#17286,#17287,#17288,
#17289,#17290,#17291,#17292,#17293,#17294,#17295,#17296,#17297,#17298,#17299,
#17300,#17301,#17302,#17303,#17304,#17305,#17306,#17307,#17308,#17309,#17310,
#17311,#17312,#17313,#17314,#17315,#17316,#17317,#17318,#17319,#17320,#17321,
#17322,#17323,#17324,#17325,#17326,#17327,#17328,#17329,#17330,#17331,#17332,
#17333,#17334,#17335,#17336,#17337,#17338,#17339,#17340,#17341,#17342,#17343,
#17344,#17345,#17346,#17347),.UNSPECIFIED.,.F.,.F.,(4,2,2,2,2,2,2,2,2,2,
2,2,2,2,2,2,2,2,2,2,2,2,2,2,2,2,2,2,2,2,2,2,2,2,2,2,2,2,2,2,2,2,2,2,2,2,
2,2,2,2,2,2,2,4),(-4.06190468854636,-4.05761219415629,-4.05608881464177,
-4.05500854406393,-4.05406745855219,-4.05308867736803,-4.05178374552866,
-4.04968755611875,-4.04315095466864,-3.92840391957809,-3.90419065775357,
-3.89459214996301,-3.89321725719404,-3.89251757875117,-3.892009953747,-3.89146225608665,
-3.89050521829901,-3.88777302654306,-3.8453969310288,-3.78760225529129,
-3.74109176150481,-3.73651688209514,-3.73421771582856,-3.73281262704672,
-3.73152999954154,-3.73053584087752,-3.72956741803743,-3.72820254100494,
-3.72456322827935,-3.66534941440886,-3.6349238978713,-3.61149141065625,
-3.57322864657244,-3.57083416967513,-3.56995760052672,-3.56936673100346,
-3.56879327548793,-3.5681016143232,-3.56637326683988,-3.5504562188279,-3.54491878933992,
-3.52870610568813,-3.50950837695847,-3.46487134489713,-3.41829829944362,
-3.4137201847873,-3.41141981631327,-3.41001422015431,-3.40873113336743,
-3.40773691935731,-3.40676859542921,-3.40540410820989,-3.40257565754072,
-3.40092133460055),.UNSPECIFIED.);
#108=B_SPLINE_CURVE_WITH_KNOTS('',3,(#17348,#17349,#17350,#17351,#17352,
#17353,#17354,#17355,#17356,#17357,#17358,#17359,#17360,#17361,#17362,#17363,
#17364,#17365,#17366,#17367,#17368,#17369,#17370,#17371,#17372,#17373,#17374,
#17375,#17376,#17377,#17378,#17379,#17380,#17381,#17382,#17383,#17384,#17385,
#17386,#17387,#17388,#17389,#17390,#17391,#17392,#17393,#17394,#17395,#17396,
#17397,#17398,#17399,#17400,#17401,#17402,#17403,#17404,#17405,#17406,#17407,
#17408,#17409,#17410,#17411,#17412,#17413,#17414,#17415,#17416,#17417,#17418,
#17419,#17420,#17421,#17422,#17423,#17424,#17425,#17426,#17427,#17428,#17429,
#17430,#17431,#17432,#17433,#17434,#17435,#17436,#17437,#17438,#17439,#17440,
#17441,#17442,#17443,#17444,#17445,#17446,#17447,#17448,#17449,#17450,#17451,
#17452,#17453,#17454,#17455,#17456,#17457,#17458,#17459,#17460,#17461,#17462,
#17463,#17464,#17465,#17466,#17467,#17468,#17469,#17470,#17471,#17472,#17473,
#17474,#17475,#17476,#17477,#17478,#17479,#17480,#17481,#17482,#17483,#17484,
#17485,#17486,#17487,#17488,#17489,#17490,#17491,#17492,#17493,#17494,#17495,
#17496,#17497,#17498,#17499,#17500,#17501,#17502,#17503,#17504,#17505,#17506,
#17507,#17508,#17509,#17510,#17511,#17512,#17513,#17514,#17515,#17516,#17517,
#17518,#17519,#17520,#17521,#17522,#17523,#17524,#17525,#17526,#17527,#17528,
#17529,#17530,#17531,#17532,#17533,#17534,#17535,#17536,#17537,#17538,#17539,
#17540,#17541,#17542,#17543,#17544,#17545,#17546,#17547,#17548,#17549,#17550,
#17551,#17552,#17553,#17554,#17555,#17556,#17557,#17558,#17559,#17560,#17561,
#17562,#17563,#17564,#17565,#17566,#17567,#17568,#17569,#17570,#17571,#17572,
#17573,#17574,#17575,#17576,#17577,#17578,#17579,#17580,#17581,#17582,#17583,
#17584,#17585,#17586,#17587,#17588,#17589,#17590,#17591,#17592,#17593,#17594,
#17595,#17596,#17597,#17598,#17599,#17600,#17601,#17602,#17603,#17604,#17605,
#17606,#17607,#17608,#17609),.UNSPECIFIED.,.F.,.F.,(4,2,2,2,2,2,2,2,2,2,
2,2,2,2,2,2,2,2,2,2,2,2,2,2,2,2,2,2,2,2,2,2,2,2,2,2,2,2,2,2,2,2,2,2,2,2,
2,2,2,2,2,2,2,2,2,2,2,2,2,2,2,2,2,2,2,2,2,2,2,2,2,2,2,2,2,2,2,2,2,2,2,2,
2,2,2,2,2,2,2,2,2,2,2,2,2,2,2,2,2,2,2,2,2,2,2,2,2,2,2,2,2,2,2,2,2,2,2,2,
2,2,2,2,2,2,2,2,2,2,2,2,4),(-2.69174590048981,-2.68518422100538,-2.64003823633685,
-2.60659309213456,-2.59169192256623,-2.58931503417848,-2.58807770775278,
-2.58707267938913,-2.58606882256754,-2.58424911351925,-2.57859487991175,
-2.57414315645939,-2.57259213429865,-2.57085753983321,-2.56936317190141,
-2.56729950316768,-2.56617916488438,-2.56300960283324,-2.55676670780608,
-2.46584600275137,-2.44568437236955,-2.43038560345629,-2.42854262904682,
-2.42753364084114,-2.42686589087765,-2.42625938040751,-2.42575546550729,
-2.42517968100698,-2.42408247907887,-2.42022300962866,-2.35746791911276,
-2.33192924551851,-2.30190752123575,-2.28205772270088,-2.26881662806319,
-2.26651231815674,-2.26529023771498,-2.26428597610859,-2.26327306724939,
-2.2614088962616,-2.25540154310491,-2.13960846954174,-2.11515924678835,
-2.10550346585773,-2.10412673045116,-2.10342671501855,-2.1028656719539,
-2.10222149556217,-2.10113278542222,-2.09723415042546,-2.03121125257412,
-1.94981376148369,-1.94470382150031,-1.94295686441705,-1.94196743686215,
-1.94106038615009,-1.93984104290258,-1.93755021816621,-1.9245975184417,
-1.90010143480742,-1.81074963803791,-1.78343885676484,-1.78150762229552,
-1.78076242818885,-1.78022740943251,-1.77965787522611,-1.7788912910346,
-1.77717256811746,-1.73327966500754,-1.62812175692323,-1.62192907899042,
-1.62004235066097,-1.61902480023222,-1.61811763844147,-1.61698630835668,
-1.61577111044837,-1.61392312457034,-1.58992061227593,-1.56817641336249,
-1.51750027515747,-1.46219421320072,-1.45897098851102,-1.45794828032615,
-1.45738743478175,-1.45682643179475,-1.45612636192972,-1.45474918525135,
-1.44507755445118,-1.42056623661874,-1.30489392770242,-1.29889587327511,
-1.29703291311642,-1.29602029151251,-1.29503615893875,-1.29384711139481,
-1.29257162773646,-1.29058045929385,-1.2499399174154,-1.14391045076237,
-1.13646078816555,-1.13521411609317,-1.13447205707712,-1.13390442655053,
-1.13329081492958,-1.1323103301683,-1.12910432393532,-1.0808283994584,-1.02077805548855,
-0.978429817451106,-0.975109792652688,-0.973797522204595,-0.97284322924698,
-0.971842478659921,-0.970518016291771,-0.96905340597356,-0.966611113498652,
-0.913842469785866,-0.818160693128627,-0.813241130670578,-0.812159624357048,
-0.811459713751008,-0.810898623380081,-0.810254246866453,-0.809136500887032,
-0.804485742183531,-0.781021794947152,-0.765140823279486,-0.753974165049035,
-0.744311195506223,-0.685210091495683,-0.66212538598945),.UNSPECIFIED.);
#109=B_SPLINE_CURVE_WITH_KNOTS('',3,(#17614,#17615,#17616,#17617,#17618,
#17619,#17620,#17621,#17622,#17623,#17624,#17625,#17626,#17627,#17628,#17629,
#17630,#17631,#17632,#17633,#17634,#17635,#17636,#17637,#17638,#17639,#17640,
#17641,#17642,#17643,#17644,#17645,#17646,#17647,#17648,#17649,#17650,#17651,
#17652,#17653,#17654,#17655,#17656,#17657,#17658,#17659,#17660,#17661,#17662,
#17663,#17664,#17665,#17666,#17667,#17668,#17669,#17670,#17671,#17672,#17673,
#17674,#17675,#17676,#17677,#17678,#17679,#17680,#17681,#17682,#17683,#17684,
#17685,#17686,#17687,#17688,#17689,#17690,#17691,#17692,#17693,#17694,#17695,
#17696,#17697,#17698,#17699,#17700,#17701,#17702,#17703,#17704,#17705,#17706,
#17707,#17708,#17709,#17710,#17711,#17712,#17713,#17714,#17715,#17716,#17717,
#17718,#17719,#17720,#17721,#17722,#17723,#17724,#17725,#17726,#17727,#17728,
#17729,#17730,#17731,#17732,#17733,#17734,#17735,#17736,#17737,#17738,#17739,
#17740,#17741,#17742,#17743,#17744,#17745,#17746,#17747,#17748,#17749,#17750,
#17751,#17752,#17753,#17754,#17755,#17756,#17757,#17758,#17759,#17760,#17761,
#17762,#17763,#17764,#17765,#17766,#17767,#17768,#17769,#17770,#17771,#17772,
#17773,#17774,#17775,#17776,#17777,#17778,#17779,#17780,#17781,#17782,#17783,
#17784,#17785,#17786,#17787,#17788,#17789,#17790,#17791,#17792,#17793,#17794,
#17795,#17796,#17797,#17798,#17799,#17800,#17801,#17802,#17803,#17804,#17805,
#17806,#17807,#17808,#17809,#17810,#17811,#17812,#17813,#17814,#17815,#17816,
#17817,#17818,#17819,#17820,#17821,#17822,#17823,#17824,#17825,#17826,#17827,
#17828,#17829,#17830,#17831,#17832,#17833,#17834,#17835,#17836,#17837,#17838,
#17839,#17840,#17841,#17842,#17843,#17844,#17845,#17846,#17847,#17848,#17849,
#17850,#17851,#17852,#17853,#17854,#17855,#17856,#17857,#17858,#17859,#17860,
#17861,#17862,#17863,#17864,#17865,#17866,#17867,#17868,#17869,#17870,#17871,
#17872,#17873,#17874,#17875,#17876,#17877,#17878,#17879,#17880,#17881,#17882,
#17883,#17884,#17885,#17886,#17887,#17888,#17889,#17890,#17891,#17892,#17893,
#17894,#17895,#17896,#17897,#17898,#17899,#17900,#17901,#17902,#17903,#17904,
#17905,#17906,#17907),.UNSPECIFIED.,.F.,.F.,(4,2,2,2,2,2,2,2,2,2,2,2,2,
2,2,2,2,2,2,2,2,2,2,2,2,2,2,2,2,2,2,2,2,2,2,2,2,2,2,2,2,2,2,2,2,2,2,2,2,
2,2,2,2,2,2,2,2,2,2,2,2,2,2,2,2,2,2,2,2,2,2,2,2,2,2,2,2,2,2,2,2,2,2,2,2,
2,2,2,2,2,2,2,2,2,2,2,2,2,2,2,2,2,2,2,2,2,2,2,2,2,2,2,2,2,2,2,2,2,2,2,2,
2,2,2,2,2,2,2,2,2,2,2,2,2,2,2,2,2,2,2,2,2,2,2,2,2,4),(-3.39964611755361,
-3.39764880888014,-3.39028359886401,-3.38749424433923,-3.38550393410291,
-3.38469269291067,-3.38416690616382,-3.38359400042095,-3.38290404404684,
-3.38118540884625,-3.36559581815718,-3.36436761100055,-3.28070406807476,
-3.24304656119502,-3.22703271126754,-3.22461221137527,-3.22336563749605,
-3.22236898473675,-3.22122623484675,-3.21928478740514,-3.21261766559457,
-3.20881186389429,-3.20714389248125,-3.20505499277876,-3.20449832602741,
-3.20241085374811,-3.20095249922505,-3.1997471079553,-3.1984230487437,-3.1922863270394,
-3.10163115893095,-3.07529061139275,-3.06757581273616,-3.06468977181308,
-3.06329156039486,-3.06246134374105,-3.0617143696158,-3.06115588937341,
-3.06062177726627,-3.05987976564568,-3.05796726431532,-3.03180746501154,
-3.01888433749514,-2.95560870912241,-2.92423949613558,-2.90440753338004,
-2.9018638478,-2.90059180591221,-2.89967818185691,-2.89871216321321,-2.89735567976228,
-2.89455921559808,-2.86537843065831,-2.82456358735152,-2.76628710912738,
-2.74377472923209,-2.74146478104603,-2.74027675049345,-2.73953382822886,
-2.73885060380401,-2.73830037251212,-2.7377417052022,-2.73672975184566,
-2.73359093184269,-2.68277282211097,-2.61870836531877,-2.59392326861083,
-2.5812015010272,-2.57892208010584,-2.57770520857356,-2.57670105134096,
-2.57568468361527,-2.57380378207173,-2.5676596352238,-2.45877194550658,
-2.4191061799309,-2.41763814338397,-2.41677924292446,-2.41601039439534,
-2.41544842557432,-2.41491941479278,-2.41419714142552,-2.41277092951605,
-2.40118202915324,-2.35737506413223,-2.32944818877692,-2.29845856239273,
-2.25953607015129,-2.25642151629098,-2.25503938725787,-2.25401530686515,
-2.25306495253363,-2.25176831283154,-2.24921129294349,-2.22835565554174,
-2.22529473950393,-2.14729337158211,-2.12201290518429,-2.10337701005734,
-2.09502276808912,-2.0936943728541,-2.09300435900876,-2.09244390443422,
-2.09187718836772,-2.09082582177403,-2.08737088277271,-2.03160578560812,
-1.93986722104493,-1.93435358872919,-1.93255166984769,-1.93155110640454,
-1.93055470128873,-1.9293143747895,-1.92692480416711,-1.91172902694223,
-1.87715650469911,-1.78508051585075,-1.78446470697245,-1.77239739388375,
-1.77079491512526,-1.77005798632339,-1.7694910321886,-1.76887481618364,
-1.76788318212385,-1.76457926095916,-1.74402529726688,-1.72000062346364,
-1.61745201802918,-1.6113913106676,-1.60952027060051,-1.60850577276141,
-1.60752139961626,-1.60633420674337,-1.60506146114842,-1.6030771863552,
-1.59933660911843,-1.56650360112663,-1.47701329868817,-1.44984351680212,
-1.4479143038609,-1.44716938464344,-1.44663439303519,-1.44606472260467,
-1.44529767900208,-1.44357678235006,-1.39885146808684,-1.37002790224387),
 .UNSPECIFIED.);
#110=B_SPLINE_CURVE_WITH_KNOTS('',3,(#17909,#17910,#17911,#17912,#17913,
#17914,#17915,#17916,#17917,#17918,#17919,#17920,#17921,#17922,#17923,#17924,
#17925,#17926,#17927,#17928,#17929,#17930,#17931,#17932,#17933,#17934,#17935,
#17936,#17937,#17938,#17939,#17940,#17941,#17942,#17943,#17944,#17945,#17946,
#17947,#17948,#17949,#17950,#17951,#17952,#17953,#17954,#17955,#17956,#17957,
#17958,#17959,#17960,#17961,#17962,#17963,#17964,#17965,#17966,#17967,#17968,
#17969,#17970,#17971,#17972,#17973,#17974,#17975,#17976,#17977,#17978,#17979,
#17980,#17981,#17982,#17983,#17984,#17985,#17986,#17987,#17988,#17989,#17990,
#17991,#17992,#17993,#17994,#17995,#17996,#17997,#17998,#17999,#18000,#18001,
#18002,#18003,#18004,#18005,#18006,#18007,#18008,#18009,#18010,#18011,#18012),
 .UNSPECIFIED.,.F.,.F.,(4,2,2,2,2,2,2,2,2,2,2,2,2,2,2,2,2,2,2,2,2,2,2,2,
2,2,2,2,2,2,2,2,2,2,2,2,2,2,2,2,2,2,2,2,2,2,2,2,2,2,2,4),(-0.66212538598945,
-0.655149255888499,-0.652080313642583,-0.650811460957387,-0.649868153424591,
-0.648859619637481,-0.647488713627128,-0.645961473694271,-0.635908521032501,
-0.617069796067174,-0.593499644285835,-0.505001047530479,-0.504025019200631,
-0.503623336120885,-0.502843125226789,-0.490998101015034,-0.489562816761166,
-0.488838174162473,-0.488308493585097,-0.487735247959456,-0.486947537252467,
-0.48511130522012,-0.440577912753107,-0.417866669091863,-0.388735385598929,
-0.332843740543996,-0.329358827539456,-0.328018773799749,-0.32705692603359,
-0.326059655065999,-0.324756717039751,-0.323323765517538,-0.32095798966878,
-0.274723435099736,-0.171670772576037,-0.170995440758908,-0.167137915343662,
-0.16604039123246,-0.165464260407457,-0.164960166302212,-0.164307311623509,
-0.163151992707949,-0.158007635387551,-0.104186532232884,-0.0435463687287092,
-0.0107744231480432,-0.00654643351052616,-0.00493057774174045,-0.00396677176403925,
-0.00299633523756008,-0.00201057957694441,-0.000961474156681484),
 .UNSPECIFIED.);
#111=B_SPLINE_CURVE_WITH_KNOTS('',3,(#18013,#18014,#18015,#18016,#18017,
#18018,#18019,#18020,#18021,#18022,#18023,#18024,#18025,#18026,#18027,#18028,
#18029,#18030,#18031,#18032,#18033,#18034,#18035,#18036,#18037,#18038,#18039,
#18040,#18041,#18042,#18043,#18044,#18045,#18046,#18047,#18048,#18049,#18050,
#18051,#18052,#18053,#18054,#18055,#18056,#18057,#18058,#18059,#18060,#18061,
#18062,#18063,#18064,#18065,#18066,#18067,#18068,#18069,#18070,#18071,#18072,
#18073,#18074,#18075,#18076,#18077,#18078,#18079,#18080,#18081,#18082,#18083,
#18084,#18085,#18086,#18087,#18088,#18089,#18090,#18091,#18092,#18093,#18094,
#18095,#18096,#18097,#18098,#18099,#18100,#18101,#18102,#18103,#18104,#18105,
#18106,#18107,#18108,#18109,#18110,#18111,#18112,#18113,#18114,#18115,#18116,
#18117,#18118,#18119,#18120,#18121,#18122,#18123,#18124,#18125,#18126,#18127,
#18128,#18129,#18130,#18131,#18132,#18133,#18134,#18135,#18136,#18137,#18138,
#18139,#18140,#18141,#18142,#18143,#18144,#18145,#18146,#18147,#18148,#18149,
#18150,#18151,#18152,#18153,#18154,#18155,#18156,#18157,#18158,#18159,#18160,
#18161,#18162,#18163,#18164,#18165,#18166,#18167,#18168,#18169,#18170,#18171,
#18172,#18173,#18174,#18175,#18176,#18177,#18178,#18179,#18180,#18181,#18182,
#18183,#18184,#18185,#18186,#18187,#18188,#18189,#18190,#18191,#18192,#18193,
#18194,#18195,#18196,#18197,#18198,#18199,#18200,#18201,#18202,#18203,#18204,
#18205,#18206,#18207,#18208,#18209,#18210,#18211,#18212,#18213,#18214,#18215,
#18216,#18217,#18218,#18219,#18220,#18221,#18222,#18223,#18224,#18225,#18226,
#18227,#18228,#18229,#18230,#18231,#18232,#18233,#18234,#18235,#18236,#18237,
#18238,#18239,#18240,#18241,#18242,#18243,#18244,#18245,#18246,#18247,#18248,
#18249,#18250,#18251,#18252,#18253,#18254,#18255,#18256,#18257,#18258,#18259,
#18260,#18261,#18262,#18263,#18264,#18265,#18266,#18267,#18268,#18269,#18270,
#18271,#18272,#18273,#18274,#18275,#18276,#18277,#18278,#18279,#18280,#18281,
#18282,#18283,#18284,#18285,#18286,#18287,#18288,#18289,#18290,#18291,#18292,
#18293,#18294,#18295,#18296,#18297,#18298,#18299,#18300,#18301,#18302,#18303,
#18304,#18305,#18306,#18307,#18308,#18309,#18310,#18311,#18312,#18313,#18314,
#18315,#18316,#18317,#18318,#18319,#18320),.UNSPECIFIED.,.F.,.F.,(4,2,2,
2,2,2,2,2,2,2,2,2,2,2,2,2,2,2,2,2,2,2,2,2,2,2,2,2,2,2,2,2,2,2,2,2,2,2,2,
2,2,2,2,2,2,2,2,2,2,2,2,2,2,2,2,2,2,2,2,2,2,2,2,2,2,2,2,2,2,2,2,2,2,2,2,
2,2,2,2,2,2,2,2,2,2,2,2,2,2,2,2,2,2,2,2,2,2,2,2,2,2,2,2,2,2,2,2,2,2,2,2,
2,2,2,2,2,2,2,2,2,2,2,2,2,2,2,2,2,2,2,2,2,2,2,2,2,2,2,2,2,2,2,2,2,2,2,2,
2,2,2,2,2,2,4),(-4.06013899922515,-4.0586875745572,-4.05295619445666,-3.99595432886195,
-3.90743304213108,-3.90366172672679,-3.9026234205714,-3.90199788786373,
-3.90143561105364,-3.90071047995764,-3.89920370627736,-3.88936904934743,
-3.88684592202701,-3.81217450881903,-3.74707911988152,-3.74334802637265,
-3.7422113591884,-3.74112176452309,-3.74111999729241,-3.74111822680033,
-3.7411164531622,-3.74111467572886,-3.7411128952234,-3.74111111147165,-3.74110932534831,
-3.74110753614702,-3.7411057433825,-3.74110394773589,-3.74110214858439,
-3.74110034609982,-3.7410985400745,-3.74109673033107,-3.74109491721153,
-3.74109310051361,-3.74109128002891,-3.74108945631834,-3.74108762903612,
-3.74108579803414,-3.74108396384155,-3.74108212583386,-3.74108028448055,
-3.74107843874733,-3.7410765893995,-3.74107473673564,-3.74107288051646,
-3.74107102081256,-3.74106915737625,-3.74106729018932,-3.74106541859219,
-3.74106354290762,-3.74106166315262,-3.74105977868544,-3.74105789078802,
-3.74105599908219,-3.74105410274061,-3.74105220305217,-3.74105029914567,
-3.74104751496156,-3.74104470505104,-3.7410418684829,-3.74103900455023,
-3.74103611326526,-3.74103319465499,-3.74103024734447,-3.74102727051948,
-3.74102426449811,-3.74102122826827,-3.74101816106587,-3.7410150623111,
-3.74101193147574,-3.74100876844032,-3.74100557245444,-3.74100234234137,
-3.74099907762704,-3.74099577750281,-3.74099244148926,-3.7409890683824,
-3.74098565787669,-3.74098220890591,-3.74097872100004,-3.74097519287914,
-3.74097162372978,-3.74096801278414,-3.74096435879223,-3.74096066129493,
-3.74095691891617,-3.74095313081701,-3.74094929622517,-3.74094332869619,
-3.74093704221519,-3.74093041375631,-3.7409234120281,-3.7399139229473,-3.73854382662273,
-3.73553411410434,-3.70768162913358,-3.62007844788081,-3.60552854608082,
-3.58442644552575,-3.58106949416065,-3.58007204741027,-3.57945453703141,
-3.57888801313887,-3.57815385954381,-3.57656605164298,-3.5648825007658,
-3.56232404342509,-3.56027754174261,-3.4619521364563,-3.42279275873346,
-3.4199305806262,-3.41861253167617,-3.41761323426829,-3.4166563244859,-3.41513103219056,
-3.41126264148037,-3.34847176150003,-3.26355811940794,-3.25831745488997,
-3.25715554793509,-3.25650136437895,-3.25599739509,-3.25542264390492,-3.25433144278923,
-3.25052967342322,-3.24977986530622,-3.14697028190909,-3.11377686894825,
-3.09893687628056,-3.09656165651435,-3.09534132874385,-3.09435504983365,
-3.09321443905326,-3.09136357056326,-3.08515666266749,-2.98167556854355,
-2.93982136656069,-2.9350954318702,-2.93397165273407,-2.93332588423217,
-2.9327648558476,-2.93206666100736,-2.93099082796192,-2.92614329445909,
-2.82980065311447,-2.79195551304572,-2.77588988085229,-2.77346676628664,
-2.77223640868239,-2.77124893766084,-2.77025857221109,-2.76857508300121,
-2.76367198214429,-2.69189203107631),.UNSPECIFIED.);
#112=B_SPLINE_CURVE_WITH_KNOTS('',3,(#18326,#18327,#18328,#18329,#18330,
#18331,#18332,#18333,#18334,#18335,#18336,#18337,#18338,#18339,#18340,#18341,
#18342,#18343,#18344,#18345,#18346,#18347,#18348,#18349,#18350,#18351,#18352,
#18353,#18354,#18355,#18356,#18357,#18358,#18359,#18360,#18361,#18362,#18363,
#18364,#18365,#18366,#18367,#18368,#18369,#18370,#18371,#18372,#18373,#18374,
#18375,#18376,#18377,#18378,#18379,#18380,#18381,#18382,#18383,#18384,#18385,
#18386,#18387,#18388,#18389,#18390,#18391,#18392,#18393,#18394,#18395,#18396,
#18397,#18398,#18399,#18400,#18401,#18402,#18403,#18404,#18405,#18406,#18407,
#18408,#18409,#18410,#18411,#18412,#18413,#18414,#18415,#18416,#18417,#18418,
#18419,#18420,#18421,#18422,#18423,#18424,#18425,#18426,#18427,#18428,#18429,
#18430,#18431,#18432,#18433,#18434,#18435,#18436,#18437,#18438,#18439,#18440,
#18441,#18442,#18443,#18444,#18445,#18446,#18447,#18448,#18449,#18450,#18451,
#18452,#18453,#18454,#18455,#18456,#18457,#18458,#18459,#18460,#18461,#18462,
#18463,#18464,#18465,#18466,#18467,#18468,#18469,#18470,#18471,#18472,#18473,
#18474,#18475,#18476,#18477,#18478,#18479,#18480,#18481,#18482,#18483,#18484,
#18485,#18486,#18487,#18488,#18489,#18490,#18491,#18492,#18493,#18494,#18495,
#18496,#18497,#18498,#18499,#18500,#18501,#18502,#18503,#18504,#18505,#18506,
#18507,#18508,#18509,#18510,#18511,#18512,#18513,#18514,#18515,#18516,#18517,
#18518,#18519,#18520,#18521,#18522,#18523,#18524,#18525,#18526,#18527),
 .UNSPECIFIED.,.F.,.F.,(4,2,2,2,2,2,2,2,2,2,2,2,2,2,2,2,2,2,2,2,2,2,2,2,
2,2,2,2,2,2,2,2,2,2,2,2,2,2,2,2,2,2,2,2,2,2,2,2,2,2,2,2,2,2,2,2,2,2,2,2,
2,2,2,2,2,2,2,2,2,2,2,2,2,2,2,2,2,2,2,2,2,2,2,2,2,2,2,2,2,2,2,2,2,2,2,2,
2,2,2,2,4),(-1.37062515302182,-1.36641565482268,-1.27609363253147,-1.26562488983865,
-1.26423972759399,-1.26352783689801,-1.26300133782122,-1.26247372834128,
-1.26171841145412,-1.26087668762849,-1.25945086169902,-1.22444716232454,
-1.13858179229422,-1.10688293184699,-1.10377375487603,-1.10249756865072,
-1.10155223976081,-1.10052393330455,-1.09911889985823,-1.09587804837423,
-1.04675590837091,-0.946551994728326,-0.941859909657036,-0.940796500239114,
-0.940102038450828,-0.939575187889014,-0.93895137279626,-0.937907271255098,
-0.936650218564192,-0.934155066534423,-0.927827521204583,-0.899425032528053,
-0.808650900285716,-0.802532597614302,-0.801173537062347,-0.799964094549804,
-0.798665305579509,-0.782832549823992,-0.780211716714131,-0.778923583851746,
-0.777912934643645,-0.776791531014876,-0.774947915245976,-0.768421086683194,
-0.726905038828855,-0.68406974733959,-0.624696442346727,-0.622925876576024,
-0.618703690967211,-0.617581295242227,-0.616929046836719,-0.616424022140671,
-0.615771846088075,-0.614600359435976,-0.613154372708063,-0.610134125503863,
-0.601928887601961,-0.580910874897554,-0.464140372440386,-0.458268274441317,
-0.456420165562351,-0.455410135141127,-0.454405001029571,-0.453176438344879,
-0.450843551000649,-0.43700154314809,-0.408941259757973,-0.364818871370853,
-0.344159311728564,-0.314840045020435,-0.31358851248783,-0.310477109160586,
-0.308256695420992,-0.296314855252144,-0.294717055376978,-0.29398097973713,
-0.293414127242867,-0.292889086160957,-0.29199968528913,-0.289517197510724,
-0.285822258016314,-0.275015586313579,-0.255279241027809,-0.171671402440776,
-0.159356029159895,-0.157289607043008,-0.15350026880912,-0.152476312074276,
-0.150374446373386,-0.14988330362345,-0.146282643557815,-0.142688989105406,
-0.135623691065618,-0.133661519840756,-0.132502387149721,-0.131597772448471,
-0.130411008793144,-0.128271970319934,-0.118055918508685,-0.0988087748871246,
-0.000962583817212411),.UNSPECIFIED.);
#113=B_SPLINE_CURVE_WITH_KNOTS('',3,(#18528,#18529,#18530,#18531,#18532,
#18533,#18534,#18535,#18536,#18537,#18538,#18539,#18540,#18541,#18542,#18543,
#18544,#18545,#18546,#18547,#18548,#18549,#18550,#18551,#18552,#18553,#18554,
#18555,#18556,#18557,#18558,#18559,#18560,#18561,#18562,#18563,#18564,#18565,
#18566,#18567,#18568,#18569,#18570,#18571,#18572,#18573,#18574,#18575,#18576,
#18577,#18578,#18579,#18580,#18581,#18582,#18583,#18584,#18585,#18586,#18587,
#18588,#18589,#18590,#18591,#18592,#18593,#18594,#18595,#18596,#18597,#18598,
#18599,#18600,#18601,#18602,#18603,#18604,#18605,#18606,#18607,#18608,#18609,
#18610,#18611,#18612,#18613,#18614,#18615,#18616,#18617,#18618,#18619,#18620,
#18621,#18622,#18623,#18624,#18625,#18626,#18627,#18628,#18629,#18630,#18631,
#18632,#18633),.UNSPECIFIED.,.F.,.F.,(4,2,2,2,2,2,2,2,2,2,2,2,2,2,2,2,2,
2,2,2,2,2,2,2,2,2,2,2,2,2,2,2,2,2,2,2,2,2,2,2,2,2,2,2,2,2,2,2,2,2,2,2,4),
(-4.06029665726298,-4.0330737903042,-4.03176370135331,-4.03096997183204,
-4.03039022437582,-4.02986449540016,-4.02929144962724,-4.02860060027115,
-4.02687594833907,-4.01106606720309,-4.00984336132231,-4.00852759203014,
-4.00163337731891,-3.99781065304034,-3.91009007232647,-3.88535200576533,
-3.87253178240235,-3.87024812020121,-3.86903061361906,-3.86802678392069,
-3.86701147475226,-3.86513465134125,-3.8590208814528,-3.74931545505425,
-3.72766723372853,-3.71721139895684,-3.71193257618668,-3.7097500843038,
-3.70811682592704,-3.70736822882574,-3.70683438297157,-3.7063054457511,
-3.70558295904313,-3.70415538162247,-3.69251660275401,-3.68146748042713,
-3.63725605826443,-3.63216025395095,-3.62630630478957,-3.61947666376359,
-3.61132656722799,-3.60122956298365,-3.56541335487771,-3.54988863808648,
-3.54748673218128,-3.54624405741294,-3.54523851754718,-3.54423732196841,
-3.54243126367529,-3.53688341933244,-3.44549490931712,-3.41522988039278,
-3.39964611755361),.UNSPECIFIED.);
#114=B_SPLINE_CURVE_WITH_KNOTS('',3,(#18634,#18635,#18636,#18637,#18638,
#18639,#18640,#18641,#18642,#18643,#18644,#18645,#18646,#18647,#18648,#18649,
#18650,#18651,#18652,#18653,#18654,#18655,#18656,#18657,#18658,#18659,#18660,
#18661,#18662,#18663,#18664,#18665,#18666,#18667,#18668,#18669,#18670,#18671,
#18672,#18673,#18674,#18675,#18676,#18677,#18678,#18679,#18680,#18681,#18682,
#18683,#18684,#18685,#18686,#18687,#18688,#18689,#18690,#18691,#18692,#18693,
#18694,#18695,#18696,#18697,#18698,#18699,#18700,#18701,#18702,#18703,#18704,
#18705,#18706,#18707,#18708,#18709,#18710,#18711,#18712,#18713,#18714,#18715,
#18716,#18717,#18718,#18719,#18720,#18721,#18722,#18723,#18724,#18725,#18726,
#18727,#18728,#18729,#18730,#18731,#18732,#18733,#18734,#18735,#18736,#18737,
#18738,#18739,#18740,#18741,#18742,#18743,#18744,#18745,#18746,#18747,#18748,
#18749,#18750,#18751,#18752,#18753,#18754,#18755,#18756,#18757,#18758,#18759,
#18760,#18761,#18762,#18763,#18764,#18765,#18766,#18767,#18768,#18769,#18770,
#18771,#18772,#18773,#18774,#18775,#18776,#18777,#18778,#18779,#18780,#18781,
#18782,#18783,#18784,#18785,#18786,#18787,#18788,#18789,#18790,#18791,#18792,
#18793,#18794,#18795,#18796,#18797,#18798,#18799,#18800,#18801,#18802,#18803,
#18804,#18805,#18806,#18807,#18808,#18809,#18810,#18811,#18812,#18813,#18814,
#18815,#18816,#18817,#18818,#18819,#18820,#18821,#18822,#18823,#18824,#18825,
#18826,#18827,#18828,#18829,#18830,#18831,#18832,#18833,#18834,#18835,#18836,
#18837,#18838,#18839,#18840,#18841,#18842,#18843,#18844,#18845,#18846,#18847,
#18848,#18849,#18850,#18851,#18852,#18853,#18854,#18855,#18856,#18857,#18858,
#18859,#18860,#18861,#18862,#18863,#18864,#18865,#18866,#18867,#18868,#18869,
#18870,#18871,#18872,#18873,#18874,#18875,#18876,#18877,#18878,#18879,#18880,
#18881,#18882,#18883,#18884,#18885,#18886,#18887,#18888,#18889,#18890,#18891,
#18892,#18893,#18894,#18895,#18896,#18897,#18898,#18899,#18900,#18901,#18902,
#18903,#18904,#18905,#18906,#18907,#18908,#18909,#18910,#18911,#18912,#18913,
#18914,#18915,#18916,#18917,#18918,#18919,#18920,#18921,#18922,#18923,#18924,
#18925),.UNSPECIFIED.,.F.,.F.,(4,2,2,2,2,2,2,2,2,2,2,2,2,2,2,2,2,2,2,2,
2,2,2,2,2,2,2,2,2,2,2,2,2,2,2,2,2,2,2,2,2,2,2,2,2,2,2,2,2,2,2,2,2,2,2,2,
2,2,2,2,2,2,2,2,2,2,2,2,2,2,2,2,2,2,2,2,2,2,2,2,2,2,2,2,2,2,2,2,2,2,2,2,
2,2,2,2,2,2,2,2,2,2,2,2,2,2,2,2,2,2,2,2,2,2,2,2,2,2,2,2,2,2,2,2,2,2,2,2,
2,2,2,2,2,2,2,2,2,2,2,2,2,2,2,2,2,4),(-2.69189203107631,-2.68428954741764,
-2.63577028753381,-2.62012960018365,-2.61238426504089,-2.61108192787796,
-2.61039739510307,-2.6098914560354,-2.60933626224789,-2.60851802068271,
-2.60610395742506,-2.564929278542,-2.55019284037311,-2.49941060665319,-2.4674509839559,
-2.45291320005841,-2.4505502910439,-2.44933256056893,-2.44834619326602,
-2.44734936719158,-2.44563610965843,-2.44051929215305,-2.35731338105497,
-2.33387149942606,-2.30254696645546,-2.29394201988924,-2.28918833002886,
-2.28806237545317,-2.28741611932471,-2.28685513184095,-2.28615758357564,
-2.28508384177392,-2.28026230880883,-2.18738861074219,-2.13083518514162,
-2.12785887366782,-2.12650217679043,-2.12548225021629,-2.12452506714646,
-2.12320233496673,-2.11982140322233,-2.07345579051452,-2.06198652144675,
-2.03063095140453,-1.97859342104963,-1.96698553589971,-1.96555859045138,
-1.96483610477134,-1.96430701420904,-1.96373341107364,-1.96294347934999,
-1.96109429151167,-1.91191506401489,-1.83699430017802,-1.80815237797425,
-1.80509441513226,-1.80383898566697,-1.80289900119436,-1.80186661256809,
-1.80043792556712,-1.79706030830855,-1.7924673930074,-1.74559642138161,
-1.64808388347933,-1.64797257560582,-1.64330978443652,-1.64224875224037,
-1.64155514277817,-1.64103102677971,-1.64048243994302,-1.63951645074417,
-1.6383746596351,-1.63618784648208,-1.61568724978367,-1.60246140939823,
-1.51467727485812,-1.48511456120563,-1.48230817638317,-1.48094901167397,
-1.47998205258638,-1.47906832841281,-1.47779740410006,-1.47526053726908,
-1.45569619747916,-1.42504224288354,-1.33340698606674,-1.3320666941687,
-1.32090461532728,-1.31935709805975,-1.31861956395952,-1.31805243699706,
-1.31744875566235,-1.31649056345389,-1.31536015107664,-1.31320336592572,
-1.29317967364103,-1.26115104658759,-1.20041699230803,-1.1831287740944,
-1.17777754742295,-1.17539535899219,-1.17483817482101,-1.16119885319424,
-1.15894813934127,-1.15761091405091,-1.15659017354175,-1.15550263120088,
-1.1538103739092,-1.14863280827768,-1.12009233516503,-1.07716178845513,
-1.0015082165501,-0.997263024023724,-0.996138404731537,-0.995485673245957,
-0.994936220794554,-0.994265637615803,-0.993541869054831,-0.992399879013481,
-0.990212659799501,-0.984919984839318,-0.974430455778944,-0.94830974808123,
-0.843058150211126,-0.836976675519868,-0.835102846831557,-0.834087635337282,
-0.833082943865943,-0.831863013735416,-0.829570716675205,-0.816600450796806,
-0.792142239192224,-0.777669894878879,-0.766654656886504,-0.682022446493819,
-0.67998888177348,-0.676202864791703,-0.673710969432534,-0.672789109668688,
-0.672248301687609,-0.671706309084773,-0.670986762361964,-0.669498760182229,
-0.667556852017813,-0.663051728732441,-0.661909204026248),.UNSPECIFIED.);
#115=B_SPLINE_CURVE_WITH_KNOTS('',3,(#18930,#18931,#18932,#18933,#18934,
#18935,#18936,#18937,#18938,#18939,#18940,#18941,#18942,#18943,#18944,#18945,
#18946,#18947,#18948,#18949,#18950,#18951,#18952,#18953,#18954,#18955,#18956,
#18957,#18958,#18959,#18960,#18961,#18962,#18963,#18964,#18965,#18966,#18967,
#18968,#18969,#18970,#18971,#18972,#18973,#18974,#18975,#18976,#18977,#18978,
#18979,#18980,#18981,#18982,#18983,#18984,#18985,#18986,#18987,#18988,#18989,
#18990,#18991,#18992,#18993,#18994,#18995,#18996,#18997,#18998,#18999,#19000,
#19001,#19002,#19003,#19004,#19005,#19006,#19007,#19008,#19009,#19010,#19011,
#19012,#19013,#19014,#19015,#19016,#19017,#19018,#19019,#19020,#19021,#19022,
#19023,#19024,#19025,#19026,#19027,#19028,#19029,#19030,#19031,#19032,#19033,
#19034,#19035,#19036,#19037,#19038,#19039,#19040,#19041,#19042,#19043,#19044,
#19045,#19046,#19047,#19048,#19049,#19050,#19051,#19052,#19053,#19054,#19055,
#19056,#19057,#19058,#19059,#19060,#19061,#19062,#19063,#19064,#19065,#19066,
#19067,#19068,#19069,#19070,#19071,#19072,#19073,#19074,#19075,#19076,#19077,
#19078,#19079,#19080,#19081,#19082,#19083,#19084,#19085,#19086,#19087,#19088,
#19089,#19090,#19091,#19092,#19093,#19094,#19095,#19096,#19097,#19098,#19099,
#19100,#19101,#19102,#19103,#19104,#19105,#19106,#19107,#19108,#19109,#19110,
#19111,#19112,#19113,#19114,#19115,#19116,#19117,#19118,#19119,#19120,#19121,
#19122,#19123,#19124,#19125,#19126,#19127,#19128,#19129,#19130,#19131,#19132,
#19133,#19134,#19135,#19136,#19137,#19138,#19139,#19140,#19141,#19142,#19143,
#19144,#19145,#19146,#19147,#19148,#19149,#19150,#19151,#19152,#19153,#19154,
#19155,#19156,#19157,#19158,#19159,#19160,#19161,#19162,#19163,#19164,#19165,
#19166,#19167,#19168,#19169,#19170,#19171,#19172,#19173,#19174,#19175,#19176,
#19177,#19178,#19179,#19180,#19181,#19182,#19183,#19184,#19185,#19186,#19187,
#19188,#19189,#19190,#19191,#19192,#19193,#19194,#19195,#19196,#19197,#19198,
#19199,#19200,#19201,#19202,#19203,#19204,#19205,#19206,#19207,#19208,#19209,
#19210,#19211,#19212,#19213,#19214,#19215,#19216,#19217,#19218,#19219,#19220,
#19221,#19222,#19223,#19224,#19225,#19226,#19227,#19228,#19229,#19230,#19231,
#19232,#19233,#19234,#19235,#19236,#19237,#19238,#19239,#19240,#19241,#19242,
#19243,#19244,#19245,#19246,#19247,#19248,#19249,#19250,#19251,#19252,#19253,
#19254,#19255,#19256,#19257,#19258,#19259,#19260,#19261,#19262,#19263,#19264,
#19265,#19266,#19267,#19268,#19269),.UNSPECIFIED.,.F.,.F.,(4,2,2,2,2,2,
2,2,2,2,2,2,2,2,2,2,2,2,2,2,2,2,2,2,2,2,2,2,2,2,2,2,2,2,2,2,2,2,2,2,2,2,
2,2,2,2,2,2,2,2,2,2,2,2,2,2,2,2,2,2,2,2,2,2,2,2,2,2,2,2,2,2,2,2,2,2,2,2,
2,2,2,2,2,2,2,2,2,2,2,2,2,2,2,2,2,2,2,2,2,2,2,2,2,2,2,2,2,2,2,2,2,2,2,2,
2,2,2,2,2,2,2,2,2,2,2,2,2,2,2,2,2,2,2,2,2,2,2,2,2,2,2,2,2,2,2,2,2,2,2,2,
2,2,2,2,2,2,2,2,2,2,2,2,2,2,2,2,2,2,2,4),(-3.4001166352834,-3.39564261836977,
-3.37616524052795,-3.36941798495544,-3.36485558168374,-3.3632482619308,
-3.36230636766994,-3.36129397703547,-3.35998890427821,-3.35728133684505,
-3.33961572743597,-3.33518013814448,-3.31906953623153,-3.24018730414167,
-3.22759461540252,-3.20720523332922,-3.20252512153085,-3.20140498778015,
-3.2007600499941,-3.20019896994023,-3.19949971659798,-3.19842041850966,
-3.19352924184026,-3.10060309886798,-3.06918752383647,-3.05210539664945,
-3.04598842633795,-3.04176762323625,-3.04020882849883,-3.03926768004243,
-3.0382503793547,-3.03693302321202,-3.03408848868579,-3.01314356240239,
-3.01028412262459,-2.92224963350563,-2.90323327544859,-2.88257465692825,
-2.87926081585319,-2.87826808666874,-2.87765162627742,-2.87708475354703,
-2.87634835100729,-2.87474866373784,-2.86275543003986,-2.78145337213415,
-2.74808258044113,-2.72361434716246,-2.72047353004736,-2.71800753224254,
-2.71675729891402,-2.71584290321642,-2.71487786799725,-2.71325460944369,
-2.70897871509158,-2.63976086734888,-2.60475770566463,-2.57659600239261,
-2.56484949276183,-2.55691103753076,-2.55560017821475,-2.55491385154032,
-2.55440773804194,-2.55385350876891,-2.55303866911201,-2.55064852714377,
-2.50952779864725,-2.47577205766266,-2.43138002370964,-2.40155082020723,
-2.39801897501125,-2.396115577788,-2.39447877729578,-2.39341301322893,-2.39239261644031,
-2.39105652283003,-2.388809206635,-2.3752284595319,-2.37482097768049,-2.37105931791733,
-2.36986421081892,-2.3683635813474,-2.36191857079865,-2.33260941447581,
-2.31329725759443,-2.27791843377717,-2.24938214713646,-2.23444088820955,
-2.23293162307917,-2.23220478034812,-2.23169321709032,-2.23115610611128,
-2.23040323354746,-2.22842467048224,-2.19790230589511,-2.16823799983893,
-2.11866638260439,-2.07991458848427,-2.07578462549641,-2.07268303192678,
-2.07130320632852,-2.07027946409882,-2.06932844546283,-2.06802938822681,
-2.06546306160851,-2.04434849015913,-2.04280191404333,-2.03145870303487,
-1.98649813292062,-1.91513391353612,-1.91095137650226,-1.90983316408563,
-1.90918201246127,-1.90862145705115,-1.90793037727574,-1.90659705049921,
-1.89812291193671,-1.87875205747178,-1.83287173781374,-1.7859622288385,
-1.77835402456422,-1.77209394423961,-1.77063563252481,-1.76943343616851,
-1.76774319362738,-1.76567945694773,-1.76394298951131,-1.76355309734664,
-1.7626563397301,-1.76035941487434,-1.75150420858391,-1.74951747451604,
-1.74824588494161,-1.7472372968675,-1.74610676149564,-1.74422150470573,
-1.73726668053863,-1.69079917427546,-1.60332742698091,-1.6029479463537,
-1.60067882859647,-1.59985317398128,-1.5887261823831,-1.58718007304828,
-1.58644282478939,-1.58587574275852,-1.5852719599226,-1.5843134936857,-1.58318249126872,
-1.58102415313264,-1.53260425992577,-1.45501474975192,-1.44886593969182,
-1.44755085003209,-1.44634616004722,-1.44482420145199,-1.44274506882589,
-1.44209996053122,-1.44096799817853,-1.44013234428156,-1.43846164559023,
-1.4346519845408,-1.42798591948393,-1.42604390303145,-1.42490061909869,
-1.4239033794519,-1.42265591411376,-1.42023318024337,-1.40418746964708,
-1.37062515302182),.UNSPECIFIED.);
#116=B_SPLINE_CURVE_WITH_KNOTS('',3,(#19271,#19272,#19273,#19274,#19275,
#19276,#19277,#19278,#19279,#19280,#19281,#19282,#19283,#19284,#19285,#19286,
#19287,#19288,#19289,#19290,#19291,#19292,#19293,#19294,#19295,#19296,#19297,
#19298,#19299,#19300,#19301,#19302,#19303,#19304,#19305,#19306,#19307,#19308,
#19309,#19310,#19311,#19312,#19313,#19314,#19315,#19316,#19317,#19318,#19319,
#19320,#19321,#19322,#19323,#19324,#19325,#19326,#19327,#19328,#19329,#19330,
#19331,#19332,#19333,#19334,#19335,#19336,#19337,#19338,#19339,#19340,#19341,
#19342,#19343,#19344,#19345,#19346,#19347,#19348,#19349,#19350,#19351,#19352,
#19353,#19354,#19355,#19356,#19357,#19358,#19359,#19360,#19361,#19362,#19363,
#19364,#19365,#19366,#19367,#19368,#19369,#19370,#19371,#19372,#19373,#19374,
#19375,#19376,#19377,#19378,#19379,#19380,#19381,#19382,#19383,#19384,#19385,
#19386,#19387,#19388,#19389,#19390,#19391,#19392,#19393,#19394,#19395,#19396,
#19397,#19398,#19399,#19400,#19401,#19402),.UNSPECIFIED.,.F.,.F.,(4,2,2,
2,2,2,2,2,2,2,2,2,2,2,2,2,2,2,2,2,2,2,2,2,2,2,2,2,2,2,2,2,2,2,2,2,2,2,2,
2,2,2,2,2,2,2,2,2,2,2,2,2,2,2,2,2,2,2,2,2,2,2,2,2,2,4),(-0.661909204026248,
-0.64894264803278,-0.615825256544206,-0.5443609960742,-0.516002197635334,
-0.512916278428946,-0.511676844897361,-0.510646912975357,-0.509594162221055,
-0.508063426432141,-0.504058319056844,-0.451014403122912,-0.441219446831309,
-0.433199637354459,-0.426413430898802,-0.420550549096795,-0.415409209026523,
-0.368269023539108,-0.366492418389508,-0.36602307444709,-0.364593807208228,
-0.363806897593697,-0.3519689895989,-0.350533823138102,-0.34980916580575,
-0.34927943892428,-0.348744958111922,-0.347997179095996,-0.346367121026489,
-0.344191805489356,-0.338937959916859,-0.328394755129598,-0.308502790868293,
-0.2190657860621,-0.212593682883621,-0.21109924407627,-0.209904353644704,
-0.205963735391409,-0.205409206202199,-0.203284985320601,-0.201550802131789,
-0.197675256604626,-0.191141340166538,-0.189214338808994,-0.18807444314546,
-0.187167957324008,-0.185957437854189,-0.183709052622849,-0.171608261792693,
-0.147728591862738,-0.052618070603708,-0.0489589398069684,-0.0444524664038431,
-0.0436386920629048,-0.0417526484775384,-0.0413534608729569,-0.0400173683724421,
-0.0288495962310037,-0.0273017853572611,-0.0265641664968555,-0.0259969993937612,
-0.025471908524072,-0.0248660680095603,-0.0240071157144323,-0.0225391935736945,
-0.000960648637719504),.UNSPECIFIED.);
#117=B_SPLINE_CURVE_WITH_KNOTS('',3,(#19403,#19404,#19405,#19406,#19407,
#19408,#19409,#19410,#19411,#19412,#19413,#19414,#19415,#19416,#19417,#19418,
#19419,#19420,#19421,#19422,#19423,#19424,#19425,#19426,#19427,#19428,#19429,
#19430,#19431,#19432,#19433,#19434,#19435,#19436,#19437,#19438,#19439,#19440,
#19441,#19442,#19443,#19444,#19445,#19446,#19447,#19448,#19449,#19450,#19451,
#19452,#19453,#19454,#19455,#19456,#19457,#19458,#19459,#19460,#19461,#19462,
#19463,#19464,#19465,#19466,#19467,#19468,#19469,#19470,#19471,#19472,#19473,
#19474,#19475,#19476,#19477,#19478,#19479,#19480,#19481,#19482,#19483,#19484,
#19485,#19486,#19487,#19488,#19489,#19490,#19491,#19492,#19493,#19494,#19495,
#19496,#19497,#19498,#19499,#19500,#19501,#19502,#19503,#19504,#19505,#19506,
#19507,#19508,#19509,#19510,#19511,#19512,#19513,#19514,#19515,#19516,#19517,
#19518,#19519,#19520,#19521,#19522,#19523,#19524,#19525,#19526,#19527,#19528,
#19529,#19530,#19531,#19532,#19533,#19534,#19535,#19536,#19537,#19538,#19539,
#19540,#19541,#19542,#19543,#19544,#19545,#19546,#19547,#19548,#19549,#19550,
#19551,#19552,#19553,#19554,#19555,#19556,#19557,#19558,#19559,#19560,#19561,
#19562,#19563,#19564,#19565,#19566,#19567,#19568,#19569,#19570,#19571,#19572,
#19573,#19574,#19575,#19576,#19577,#19578,#19579,#19580,#19581,#19582,#19583,
#19584,#19585,#19586,#19587,#19588,#19589,#19590,#19591,#19592,#19593,#19594,
#19595,#19596,#19597,#19598,#19599,#19600,#19601,#19602,#19603,#19604,#19605,
#19606,#19607,#19608,#19609,#19610,#19611,#19612,#19613,#19614,#19615,#19616,
#19617,#19618,#19619,#19620,#19621,#19622,#19623,#19624,#19625,#19626,#19627,
#19628,#19629,#19630,#19631,#19632,#19633,#19634,#19635,#19636,#19637,#19638,
#19639,#19640,#19641,#19642,#19643,#19644,#19645,#19646,#19647,#19648),
 .UNSPECIFIED.,.F.,.F.,(4,2,2,2,2,2,2,2,2,2,2,2,2,2,2,2,2,2,2,2,2,2,2,2,
2,2,2,2,2,2,2,2,2,2,2,2,2,2,2,2,2,2,2,2,2,2,2,2,2,2,2,2,2,2,2,2,2,2,2,2,
2,2,2,2,2,2,2,2,2,2,2,2,2,2,2,2,2,2,2,2,2,2,2,2,2,2,2,2,2,2,2,2,2,2,2,2,
2,2,2,2,2,2,2,2,2,2,2,2,2,2,2,2,2,2,2,2,2,2,2,2,2,2,4),(-4.06067477183731,
-3.97551640619293,-3.9342284616751,-3.92772495826773,-3.92588498946432,
-3.92476517266495,-3.92375554426393,-3.92246814951183,-3.91984686563877,
-3.90396583415625,-3.90295869860179,-3.90173117253988,-3.9002119804425,
-3.89432030234605,-3.81658839468245,-3.79159166232957,-3.77368860319943,
-3.7682250166568,-3.76598654563151,-3.76432118432354,-3.76356574784999,
-3.76303343468061,-3.76250682440761,-3.76179313429406,-3.76039961735992,
-3.74968903149156,-3.71625838004261,-3.69518018081669,-3.65201766648963,
-3.62047670404653,-3.60604092805952,-3.60368353731701,-3.60245037507324,
-3.60144569757689,-3.60029045863565,-3.59834286996244,-3.59140702241851,
-3.58774543555818,-3.58406071244966,-3.58305700211639,-3.57976601426175,
-3.57857133878931,-3.57704299950396,-3.57063533556551,-3.49353204733034,
-3.4686513064837,-3.45331140846403,-3.45076992011312,-3.44549699742683,
-3.44331638907036,-3.44217719964726,-3.44121278003219,-3.44060813199362,
-3.44004195136439,-3.43930817802696,-3.4377209417783,-3.42603375358544,
-3.42513867933139,-3.42458461240024,-3.4237335467686,-3.4233510596538,-3.42250904713076,
-3.42040822392064,-3.41894690111654,-3.37564523076464,-3.33228234050492,
-3.30279574465384,-3.28367426668513,-3.28115146415914,-3.27988389619273,
-3.27897112507605,-3.27800382166548,-3.2766419577825,-3.27382280010805,
-3.26624431667473,-3.26443066446623,-3.26236874195894,-3.26192149977942,
-3.26002087266932,-3.25718406517421,-3.25453080176283,-3.24819757365304,
-3.15838578792251,-3.13280354848664,-3.12441487666233,-3.12134610741856,
-3.11988342403432,-3.11870176475175,-3.1180820179147,-3.1175329884998,-3.11688018000654,
-3.11575395648471,-3.11148714487279,-3.10871771107924,-3.10720408449865,
-3.10598422312306,-3.08739565940028,-2.99793681821398,-2.97315817473116,
-2.96044088479583,-2.95816211305024,-2.956945569,-2.95594167196336,-2.95492555898799,
-2.95304510364951,-2.94690220825838,-2.83798881269394,-2.82054046335701,
-2.79987321065769,-2.79767658182068,-2.79653124418734,-2.79556254638864,
-2.79495682144533,-2.79439079408035,-2.79365880230651,-2.79208153670383,
-2.78065897366069,-2.77954596476192,-2.777999644062,-2.77492103113334,-2.75066375205298,
-2.7183576420267,-2.6926898927874),.UNSPECIFIED.);
#118=B_SPLINE_CURVE_WITH_KNOTS('',3,(#19654,#19655,#19656,#19657,#19658,
#19659,#19660,#19661,#19662,#19663,#19664,#19665,#19666,#19667,#19668,#19669,
#19670,#19671,#19672,#19673,#19674,#19675,#19676,#19677,#19678,#19679,#19680,
#19681,#19682,#19683,#19684,#19685,#19686,#19687,#19688,#19689,#19690,#19691,
#19692,#19693,#19694,#19695,#19696,#19697,#19698,#19699,#19700,#19701,#19702,
#19703,#19704,#19705,#19706,#19707,#19708,#19709,#19710,#19711,#19712,#19713,
#19714,#19715,#19716,#19717,#19718,#19719,#19720,#19721,#19722,#19723,#19724,
#19725,#19726,#19727,#19728,#19729,#19730,#19731,#19732,#19733,#19734,#19735,
#19736,#19737,#19738,#19739,#19740,#19741,#19742,#19743,#19744,#19745,#19746,
#19747,#19748,#19749,#19750,#19751,#19752,#19753,#19754,#19755,#19756,#19757,
#19758,#19759,#19760,#19761,#19762,#19763,#19764,#19765,#19766,#19767,#19768,
#19769,#19770,#19771,#19772,#19773,#19774,#19775,#19776,#19777,#19778,#19779,
#19780,#19781,#19782,#19783,#19784,#19785,#19786,#19787,#19788,#19789,#19790,
#19791,#19792,#19793,#19794,#19795,#19796,#19797,#19798,#19799,#19800,#19801,
#19802,#19803,#19804,#19805,#19806,#19807,#19808,#19809,#19810,#19811,#19812,
#19813,#19814,#19815,#19816,#19817,#19818,#19819,#19820,#19821,#19822,#19823,
#19824,#19825,#19826,#19827,#19828,#19829,#19830,#19831,#19832,#19833,#19834,
#19835,#19836,#19837,#19838,#19839,#19840,#19841,#19842,#19843,#19844,#19845,
#19846,#19847,#19848,#19849),.UNSPECIFIED.,.F.,.F.,(4,2,2,2,2,2,2,2,2,2,
2,2,2,2,2,2,2,2,2,2,2,2,2,2,2,2,2,2,2,2,2,2,2,2,2,2,2,2,2,2,2,2,2,2,2,2,
2,2,2,2,2,2,2,2,2,2,2,2,2,2,2,2,2,2,2,2,2,2,2,2,2,2,2,2,2,2,2,2,2,2,2,2,
2,2,2,2,2,2,2,2,2,2,2,2,2,2,2,4),(-1.36960102657385,-1.34982761332196,-1.24890809839695,
-1.24272075299376,-1.24083457604496,-1.23981708968323,-1.23882252599685,
-1.2376358992272,-1.23547225687161,-1.23279091301979,-1.18122375085026,
-1.08474811374041,-1.07991196085698,-1.0788371021054,-1.07813924133682,
-1.07757827990661,-1.07693236305532,-1.0758077688474,-1.07107060341839,
-1.02886732836974,-0.946595968867606,-0.940605099092659,-0.939049465645938,
-0.937816098240649,-0.936810060770758,-0.92096351145887,-0.918342767296007,
-0.91705498295753,-0.916044747584459,-0.914946559303704,-0.913164350388299,
-0.907173809342364,-0.89762015760281,-0.865676629489227,-0.826471418902932,
-0.760631984890354,-0.756821620927213,-0.75572952277531,-0.755154617222093,
-0.75465069049022,-0.753996807615432,-0.752836133365388,-0.747612150863471,
-0.689411339787425,-0.633110379915867,-0.620751973431156,-0.617906243109689,
-0.616480196360992,-0.615273714997185,-0.613866172069521,-0.61176986249144,
-0.611258779020742,-0.608228095142774,-0.605285835283282,-0.601712844553965,
-0.599768078656407,-0.596092818235156,-0.594722176292371,-0.593752172237995,
-0.592839706060771,-0.591867511500152,-0.589828663436281,-0.580990681173594,
-0.565079977637646,-0.526060554051278,-0.438872147529599,-0.434072173214614,
-0.433000184184496,-0.432303181670121,-0.431742232340601,-0.431095571433228,
-0.429967797566877,-0.425190683234534,-0.370339811654537,-0.346775348786968,
-0.317096885436763,-0.301345038953997,-0.295090898114237,-0.291384491907739,
-0.275222402886052,-0.272585379971146,-0.271294188797298,-0.270283386382439,
-0.269340702951088,-0.268243023454457,-0.265030388520121,-0.233332259594882,
-0.21335180609637,-0.115854043978622,-0.111506568750345,-0.110078756724497,
-0.109358220791414,-0.108794973226389,-0.108163552433763,-0.107104517788285,
-0.103138472583711,-0.0751682503225802,-0.000962417701089617),
 .UNSPECIFIED.);
#119=B_SPLINE_CURVE_WITH_KNOTS('',3,(#19850,#19851,#19852,#19853,#19854,
#19855,#19856,#19857,#19858,#19859,#19860,#19861,#19862,#19863,#19864,#19865,
#19866,#19867,#19868,#19869,#19870,#19871,#19872,#19873,#19874,#19875,#19876,
#19877,#19878,#19879,#19880,#19881,#19882,#19883,#19884,#19885,#19886,#19887,
#19888,#19889,#19890,#19891,#19892,#19893,#19894,#19895,#19896,#19897,#19898,
#19899,#19900,#19901,#19902,#19903,#19904,#19905,#19906,#19907,#19908,#19909,
#19910,#19911,#19912,#19913,#19914,#19915,#19916,#19917,#19918,#19919,#19920,
#19921,#19922,#19923,#19924,#19925,#19926,#19927,#19928,#19929,#19930,#19931,
#19932,#19933,#19934,#19935,#19936,#19937,#19938,#19939,#19940,#19941,#19942,
#19943),.UNSPECIFIED.,.F.,.F.,(4,2,2,2,2,2,2,2,2,2,2,2,2,2,2,2,2,2,2,2,
2,2,2,2,2,2,2,2,2,2,2,2,2,2,2,2,2,2,2,2,2,2,2,2,2,2,4),(-4.06128526371725,
-4.01403618995952,-4.01152595456631,-4.01003311647368,-4.00896502788193,
-4.00802392688564,-4.00700442585582,-4.00567317438803,-4.00286152966641,
-3.98182348253844,-3.97954915416361,-3.96368781931084,-3.95863231897075,
-3.95274423953934,-3.87253627244141,-3.85144434700357,-3.84808841602249,
-3.84709110228388,-3.84647363530591,-3.84590712421589,-3.84517295092564,
-3.84358495971133,-3.83189569354908,-3.83099593072355,-3.75034058225151,
-3.73224143377886,-3.70305082147155,-3.68908120855673,-3.68675054332559,
-3.68574863716805,-3.68472746022651,-3.68377252179041,-3.68245826359875,
-3.67912746588137,-3.63618255982295,-3.58765059069244,-3.58169623636757,
-3.52890990782499,-3.52526005340221,-3.52423192291307,-3.52360755959704,
-3.52304300081289,-3.52232243367425,-3.52080540484074,-3.51081153605494,
-3.43568210163337,-3.4001166352834),.UNSPECIFIED.);
#120=B_SPLINE_CURVE_WITH_KNOTS('',3,(#19944,#19945,#19946,#19947,#19948,
#19949,#19950,#19951,#19952,#19953,#19954,#19955,#19956,#19957,#19958,#19959,
#19960,#19961,#19962,#19963,#19964,#19965,#19966,#19967,#19968,#19969,#19970,
#19971,#19972,#19973,#19974,#19975,#19976,#19977,#19978,#19979,#19980,#19981,
#19982,#19983,#19984,#19985,#19986,#19987,#19988,#19989,#19990,#19991,#19992,
#19993,#19994,#19995,#19996,#19997,#19998,#19999,#20000,#20001,#20002,#20003,
#20004,#20005,#20006,#20007,#20008,#20009,#20010,#20011,#20012,#20013,#20014,
#20015,#20016,#20017,#20018,#20019,#20020,#20021,#20022,#20023,#20024,#20025,
#20026,#20027,#20028,#20029,#20030,#20031,#20032,#20033,#20034,#20035,#20036,
#20037,#20038,#20039,#20040,#20041,#20042,#20043,#20044,#20045,#20046,#20047,
#20048,#20049,#20050,#20051,#20052,#20053,#20054,#20055,#20056,#20057,#20058,
#20059,#20060,#20061,#20062,#20063,#20064,#20065,#20066,#20067,#20068,#20069,
#20070,#20071,#20072,#20073,#20074,#20075,#20076,#20077,#20078,#20079,#20080,
#20081,#20082,#20083,#20084,#20085,#20086,#20087,#20088,#20089,#20090,#20091,
#20092,#20093,#20094,#20095,#20096,#20097,#20098,#20099,#20100,#20101,#20102,
#20103,#20104,#20105,#20106,#20107,#20108,#20109,#20110,#20111,#20112,#20113,
#20114,#20115,#20116,#20117,#20118,#20119,#20120,#20121,#20122,#20123,#20124,
#20125,#20126,#20127,#20128,#20129,#20130,#20131,#20132,#20133,#20134,#20135,
#20136,#20137,#20138,#20139,#20140,#20141,#20142,#20143,#20144,#20145,#20146,
#20147,#20148,#20149,#20150,#20151,#20152,#20153,#20154,#20155,#20156,#20157,
#20158,#20159,#20160,#20161,#20162,#20163,#20164,#20165,#20166,#20167,#20168,
#20169,#20170,#20171,#20172,#20173,#20174,#20175,#20176,#20177,#20178,#20179,
#20180,#20181,#20182,#20183,#20184,#20185,#20186,#20187,#20188,#20189,#20190,
#20191,#20192,#20193,#20194,#20195,#20196,#20197,#20198,#20199,#20200,#20201,
#20202,#20203,#20204,#20205,#20206,#20207,#20208,#20209,#20210,#20211,#20212,
#20213,#20214,#20215),.UNSPECIFIED.,.F.,.F.,(4,2,2,2,2,2,2,2,2,2,2,2,2,
2,2,2,2,2,2,2,2,2,2,2,2,2,2,2,2,2,2,2,2,2,2,2,2,2,2,2,2,2,2,2,2,2,2,2,2,
2,2,2,2,2,2,2,2,2,2,2,2,2,2,2,2,2,2,2,2,2,2,2,2,2,2,2,2,2,2,2,2,2,2,2,2,
2,2,2,2,2,2,2,2,2,2,2,2,2,2,2,2,2,2,2,2,2,2,2,2,2,2,2,2,2,2,2,2,2,2,2,2,
2,2,2,2,2,2,2,2,2,2,2,2,2,2,4),(-2.6926898927874,-2.67309610584487,-2.65079332468313,
-2.6376223350769,-2.63532116467435,-2.63409967375698,-2.63309533864024,
-2.632081881767,-2.63021533282697,-2.6241895089379,-2.50797674714693,-2.4903136656093,
-2.47608552821513,-2.4743172710447,-2.47333762249951,-2.47268205537713,
-2.47207555368219,-2.4715271305527,-2.47082739347038,-2.46974645239456,
-2.46483403008942,-2.36982806351589,-2.3520224639032,-2.32724270077514,
-2.31445625380223,-2.31217338982096,-2.31095567275187,-2.30995133689594,
-2.30893523174088,-2.30705610907138,-2.30092818926197,-2.19266536184236,
-2.15174924909108,-2.15000257646364,-2.14923082951768,-2.14866036331882,
-2.14812664817978,-2.14738657584853,-2.14589004330382,-2.13213786646308,
-2.13030845937606,-2.03150354455633,-2.01578039377114,-2.01323778502252,
-1.99220920365282,-1.9893978529876,-1.98806664174814,-1.98704712776963,
-1.98595762336159,-1.98425556599443,-1.97899618841049,-1.94972598638336,
-1.90580790895638,-1.83203006109701,-1.82778063464633,-1.82665580497947,
-1.82600314062181,-1.82544273263893,-1.82475365742679,-1.82342974653971,
-1.81518440728078,-1.79747160871322,-1.77256181535091,-1.70505671542748,
-1.66994256903903,-1.66675631053237,-1.665466817991,-1.66451827091473,-1.66351352612049,
-1.66216680657377,-1.66067109200021,-1.65815396504563,-1.59784210417049,
-1.50966089918513,-1.50862858552766,-1.50475311233365,-1.50366667055202,
-1.50302290574208,-1.50246162346838,-1.5017605388016,-1.50037923993155,
-1.49059743568069,-1.46602356718208,-1.35040889565067,-1.34445907007786,
-1.34260159083249,-1.34158982239805,-1.34058510790954,-1.33938500790588,
-1.33715211052937,-1.33437093403008,-1.28554542521502,-1.19180671739098,
-1.19006458328631,-1.1888837108712,-1.1820399564423,-1.18079197504582,-1.18004941480431,
-1.1794815650415,-1.17886788367999,-1.17788763418365,-1.17468537838819,
-1.12650129169932,-1.03420952760566,-1.03353359906517,-1.03070056822006,
-1.02193126400388,-1.01999500356996,-1.01873916102006,-1.01773219189751,
-1.01661487386807,-1.01475541697356,-1.01252870448309,-1.00814894137876,
-0.997248604953662,-0.957641827754534,-0.863436897465518,-0.858642230018257,
-0.857570621662452,-0.856873719572898,-0.856312751700649,-0.855665957665397,
-0.854537673064802,-0.849754446542577,-0.794918901056801,-0.727925121726972,
-0.700390097395911,-0.697633517928579,-0.696286600793523,-0.695322911328846,
-0.694352622595137,-0.693069516366336,-0.690446835669292,-0.687057802964749,
-0.679334366621671,-0.662311037573458),.UNSPECIFIED.);
#121=B_SPLINE_CURVE_WITH_KNOTS('',3,(#20220,#20221,#20222,#20223,#20224,
#20225,#20226,#20227,#20228,#20229,#20230,#20231,#20232,#20233,#20234,#20235,
#20236,#20237,#20238,#20239,#20240,#20241,#20242,#20243,#20244,#20245,#20246,
#20247,#20248,#20249,#20250,#20251,#20252,#20253,#20254,#20255,#20256,#20257,
#20258,#20259,#20260,#20261,#20262,#20263,#20264,#20265,#20266,#20267,#20268,
#20269,#20270,#20271,#20272,#20273,#20274,#20275,#20276,#20277,#20278,#20279,
#20280,#20281,#20282,#20283,#20284,#20285,#20286,#20287,#20288,#20289,#20290,
#20291,#20292,#20293,#20294,#20295,#20296,#20297,#20298,#20299,#20300,#20301,
#20302,#20303,#20304,#20305,#20306,#20307,#20308,#20309,#20310,#20311,#20312,
#20313,#20314,#20315,#20316,#20317,#20318,#20319,#20320,#20321,#20322,#20323,
#20324,#20325,#20326,#20327,#20328,#20329,#20330,#20331,#20332,#20333,#20334,
#20335,#20336,#20337,#20338,#20339,#20340,#20341,#20342,#20343,#20344,#20345,
#20346,#20347,#20348,#20349,#20350,#20351,#20352,#20353,#20354,#20355,#20356,
#20357,#20358,#20359,#20360,#20361,#20362,#20363,#20364,#20365,#20366,#20367,
#20368,#20369,#20370,#20371,#20372,#20373,#20374,#20375,#20376,#20377,#20378,
#20379,#20380,#20381,#20382,#20383,#20384,#20385,#20386,#20387,#20388,#20389,
#20390,#20391,#20392,#20393,#20394,#20395,#20396,#20397,#20398,#20399,#20400,
#20401,#20402,#20403,#20404,#20405,#20406,#20407,#20408,#20409,#20410,#20411,
#20412,#20413,#20414,#20415,#20416,#20417,#20418,#20419,#20420,#20421,#20422,
#20423,#20424,#20425,#20426,#20427,#20428,#20429,#20430,#20431,#20432,#20433,
#20434,#20435,#20436,#20437,#20438,#20439,#20440,#20441,#20442,#20443,#20444,
#20445,#20446,#20447,#20448,#20449,#20450,#20451,#20452,#20453,#20454,#20455,
#20456,#20457,#20458,#20459,#20460,#20461,#20462,#20463,#20464,#20465,#20466,
#20467,#20468,#20469,#20470,#20471,#20472,#20473,#20474,#20475,#20476,#20477,
#20478,#20479,#20480,#20481,#20482,#20483,#20484,#20485,#20486,#20487,#20488,
#20489,#20490,#20491,#20492,#20493,#20494,#20495,#20496,#20497,#20498,#20499,
#20500,#20501,#20502,#20503),.UNSPECIFIED.,.F.,.F.,(4,2,2,2,2,2,2,2,2,2,
2,2,2,2,2,2,2,2,2,2,2,2,2,2,2,2,2,2,2,2,2,2,2,2,2,2,2,2,2,2,2,2,2,2,2,2,
2,2,2,2,2,2,2,2,2,2,2,2,2,2,2,2,2,2,2,2,2,2,2,2,2,2,2,2,2,2,2,2,2,2,2,2,
2,2,2,2,2,2,2,2,2,2,2,2,2,2,2,2,2,2,2,2,2,2,2,2,2,2,2,2,2,2,2,2,2,2,2,2,
2,2,2,2,2,2,2,2,2,2,2,2,2,2,2,2,2,2,2,2,2,2,2,4),(-3.39850283521087,-3.37886812956445,
-3.35863417788478,-3.34815667885647,-3.3428698297973,-3.3395876243599,-3.33885124461285,
-3.33816229195313,-3.33760213256738,-3.3370352286123,-3.33598213307277,
-3.33251025005807,-3.27716760410847,-3.22895465939362,-3.19561684758958,
-3.18075950080207,-3.17839837805032,-3.1771508565237,-3.17624071684908,
-3.17526504871281,-3.17387280024893,-3.17005745442605,-3.11028981764791,
-3.04921563593415,-3.02668723895948,-3.01751398340293,-3.01615870372652,
-3.01545749525619,-3.01494982493158,-3.01440311675706,-3.01345038785351,
-3.01074596600773,-2.96837921632043,-2.91277159198561,-2.8743181558504,
-2.8581111532748,-2.85572669639301,-2.85445870946526,-2.85354576295307,
-2.85257839079847,-2.85121662197714,-2.84839828479699,-2.84081673236981,
-2.83900228001641,-2.8369399274836,-2.83649857993593,-2.83454470737958,
-2.83176097806481,-2.82864398242382,-2.76037986710993,-2.72113089851205,
-2.69774691342335,-2.69538517933984,-2.69364243940109,-2.69286518531221,
-2.69229398386132,-2.69176206386797,-2.69102820915135,-2.68916360644994,
-2.66571984327507,-2.59663181379918,-2.54019963759614,-2.53622532688605,
-2.53324123818374,-2.53187052946614,-2.53084866246442,-2.52989586798446,
-2.52858891470685,-2.52599041901296,-2.50388608054255,-2.49189420206403,
-2.40209123729086,-2.38080309629431,-2.37192935284491,-2.37058498347194,
-2.36988602781303,-2.36932513602276,-2.36876374324739,-2.36773823531028,
-2.36449315455294,-2.32356634328817,-2.30068727261435,-2.25214754331056,
-2.21396008915135,-2.21058521867599,-2.20915720567671,-2.20812512394539,
-2.20718529483922,-2.20592988903343,-2.2028710916244,-2.17397654566229,
-2.10376167784597,-2.05161848634036,-2.04846670436279,-2.04749241938952,
-2.04688018907063,-2.04631204496277,-2.04556682040451,-2.04398010615256,
-2.03177749085631,-2.03070064005706,-2.00584359882914,-1.91841591852406,
-1.89063640474908,-1.88756777891063,-1.88633158265758,-1.88530287138216,
-1.88424986712639,-1.88271602355577,-1.87868731257916,-1.82427536413008,
-1.73814774423759,-1.72657719722811,-1.72515173125588,-1.72442968233519,
-1.72390076138609,-1.72332719049738,-1.72253704007209,-1.7206861526361,
-1.66815061273637,-1.59809180037001,-1.56782790453629,-1.56500562514299,
-1.56364274645502,-1.56267494712003,-1.56176189117269,-1.56051969634375,
-1.55809103037091,-1.55500826702422,-1.53130386529167,-1.50867529136043,
-1.41839328011026,-1.41712017264588,-1.41530234542897,-1.40366426115492,
-1.4022363065904,-1.40151358132533,-1.40098444574681,-1.40041092582284,
-1.39962133865539,-1.39777399412751,-1.36960102657385),.UNSPECIFIED.);
#122=B_SPLINE_CURVE_WITH_KNOTS('',3,(#20505,#20506,#20507,#20508,#20509,
#20510,#20511,#20512,#20513,#20514,#20515,#20516,#20517,#20518,#20519,#20520,
#20521,#20522,#20523,#20524,#20525,#20526,#20527,#20528,#20529,#20530,#20531,
#20532,#20533,#20534,#20535,#20536,#20537,#20538,#20539,#20540,#20541,#20542,
#20543,#20544,#20545,#20546,#20547,#20548,#20549,#20550,#20551,#20552,#20553,
#20554,#20555,#20556,#20557,#20558,#20559,#20560,#20561,#20562,#20563,#20564,
#20565,#20566,#20567,#20568,#20569,#20570,#20571,#20572,#20573,#20574,#20575,
#20576,#20577,#20578,#20579,#20580,#20581,#20582,#20583,#20584,#20585,#20586,
#20587,#20588,#20589,#20590,#20591,#20592,#20593,#20594,#20595,#20596,#20597,
#20598,#20599,#20600,#20601,#20602,#20603,#20604,#20605,#20606,#20607,#20608,
#20609,#20610,#20611,#20612,#20613,#20614,#20615,#20616,#20617,#20618,#20619,
#20620),.UNSPECIFIED.,.F.,.F.,(4,2,2,2,2,2,2,2,2,2,2,2,2,2,2,2,2,2,2,2,
2,2,2,2,2,2,2,2,2,2,2,2,2,2,2,2,2,2,2,2,2,2,2,2,2,2,2,2,2,2,2,2,2,2,2,2,
2,4),(-0.662311037573458,-0.65615864758013,-0.621327529538634,-0.546607691738824,
-0.536271025882487,-0.534891182292375,-0.53418071286439,-0.533654619493689,
-0.533078302530182,-0.532274100277144,-0.530342446873173,-0.527677247150757,
-0.498714599855855,-0.473433228537379,-0.467231993997839,-0.461833297893715,
-0.414695956770623,-0.403065358324979,-0.396789851754358,-0.377110831010752,
-0.374595601363168,-0.373309493263339,-0.372361668917608,-0.371401948437605,
-0.370403468112348,-0.36810717373799,-0.354906680588511,-0.333674848406216,
-0.312504400846729,-0.217671366150407,-0.21275570861585,-0.211674206174472,
-0.210974135129431,-0.210412807011706,-0.209768036166981,-0.208649307564375,
-0.203990371876987,-0.181168749103709,-0.0987139729391346,-0.0929458877557674,
-0.0867890769430741,-0.0761086949448165,-0.0716907483743516,-0.0704319797769508,
-0.069289570689577,-0.0672269001869602,-0.0645928228927022,-0.0622057754009242,
-0.0552355304567586,-0.0516840728705253,-0.0503329443696014,-0.0493679951394072,
-0.0483967711885841,-0.0474118047662053,-0.0461420102717969,-0.0441651812178458,
-0.0418034854322739,-0.000960728331950941),.UNSPECIFIED.);
#123=B_SPLINE_CURVE_WITH_KNOTS('',3,(#20621,#20622,#20623,#20624,#20625,
#20626,#20627,#20628,#20629,#20630,#20631,#20632,#20633,#20634,#20635,#20636,
#20637,#20638,#20639,#20640,#20641,#20642,#20643,#20644,#20645,#20646,#20647,
#20648,#20649,#20650,#20651,#20652,#20653,#20654,#20655,#20656,#20657,#20658,
#20659,#20660,#20661,#20662,#20663,#20664,#20665,#20666,#20667,#20668,#20669,
#20670,#20671,#20672,#20673,#20674,#20675,#20676,#20677,#20678,#20679,#20680,
#20681,#20682,#20683,#20684,#20685,#20686,#20687,#20688,#20689,#20690,#20691,
#20692,#20693,#20694,#20695,#20696,#20697,#20698,#20699,#20700,#20701,#20702,
#20703,#20704,#20705,#20706,#20707,#20708,#20709,#20710,#20711,#20712,#20713,
#20714,#20715,#20716,#20717,#20718,#20719,#20720,#20721,#20722,#20723,#20724,
#20725,#20726,#20727,#20728,#20729,#20730,#20731,#20732,#20733,#20734,#20735,
#20736,#20737,#20738,#20739,#20740,#20741,#20742,#20743,#20744,#20745,#20746,
#20747,#20748,#20749,#20750,#20751,#20752,#20753,#20754,#20755,#20756,#20757,
#20758,#20759,#20760,#20761,#20762,#20763,#20764,#20765,#20766,#20767,#20768,
#20769,#20770,#20771,#20772,#20773,#20774,#20775,#20776,#20777,#20778,#20779,
#20780,#20781,#20782,#20783,#20784,#20785,#20786,#20787,#20788,#20789,#20790,
#20791,#20792,#20793,#20794,#20795,#20796,#20797,#20798,#20799,#20800,#20801,
#20802,#20803,#20804,#20805,#20806,#20807,#20808,#20809,#20810,#20811,#20812,
#20813,#20814,#20815,#20816,#20817,#20818,#20819,#20820,#20821,#20822,#20823,
#20824,#20825,#20826,#20827,#20828,#20829,#20830,#20831,#20832),
 .UNSPECIFIED.,.F.,.F.,(4,2,2,2,2,2,2,2,2,2,2,2,2,2,2,2,2,2,2,2,2,2,2,2,
2,2,2,2,2,2,2,2,2,2,2,2,2,2,2,2,2,2,2,2,2,2,2,2,2,2,2,2,2,2,2,2,2,2,2,2,
2,2,2,2,2,2,2,2,2,2,2,2,2,2,2,2,2,2,2,2,2,2,2,2,2,2,2,2,2,2,2,2,2,2,2,2,
2,2,2,2,2,2,2,2,2,4),(-4.06063332408298,-3.98236991709419,-3.95320453615512,
-3.95052955335759,-3.94859227911098,-3.94778707522546,-3.94721052505372,
-3.94668456591702,-3.94597477485033,-3.94459770260344,-3.93433364574729,
-3.84157460790404,-3.82739425556801,-3.80261686092121,-3.78982620747972,
-3.78754935282277,-3.78655292974462,-3.78559181464287,-3.78464181428129,
-3.78334716467498,-3.7801320560732,-3.74366656763003,-3.70375877370762,
-3.67040461009186,-3.64521482460296,-3.63271241003713,-3.62646192791595,
-3.62523558672442,-3.62456727221709,-3.6240626119361,-3.62341321174684,
-3.62230269576563,-3.6181969932488,-3.61785402268241,-3.61743362918342,
-3.52933667216842,-3.49468886115026,-3.4764059325892,-3.46997087970417,
-3.467011779248,-3.4646678291807,-3.46344063939049,-3.46244924477717,-3.46131146910951,
-3.45939393506891,-3.45294245443382,-3.44902628257763,-3.44725068513935,
-3.44510421343851,-3.4430214198239,-3.44121546447319,-3.43999371677761,
-3.43576387757898,-3.38331862852359,-3.3478774847442,-3.31901016227127,
-3.30881699017053,-3.30343285852135,-3.30226097034257,-3.30160456531029,
-3.30110050550384,-3.30052738456975,-3.29944441106512,-3.2957169802745,
-3.29486140579635,-3.21946970695645,-3.17112487026757,-3.1533080760608,
-3.14699593738473,-3.14407893408819,-3.14175845196327,-3.14053847068118,
-3.13954367627796,-3.13854584456083,-3.13675808601833,-3.13135286050662,
-3.126606525182,-3.12502934150732,-3.12400333337963,-3.12353258683031,-3.12233498535378,
-3.1202435137834,-3.11634149039697,-3.11276022528805,-3.01163211448398,
-2.98972837020966,-2.98069498812585,-2.97933988969156,-2.9786441827773,
-2.97808323518364,-2.97751952974331,-2.97648355902078,-2.97315703750576,
-2.91749739474139,-2.86347692809833,-2.82467482328823,-2.82140468273544,
-2.81885849671408,-2.81759011837506,-2.81661497617751,-2.81564436746798,
-2.81399355244866,-2.80954311589934,-2.73750778148851,-2.73165942825708,
-2.69197257292336),.UNSPECIFIED.);
#124=B_SPLINE_CURVE_WITH_KNOTS('',3,(#20838,#20839,#20840,#20841,#20842,
#20843,#20844,#20845,#20846,#20847,#20848,#20849,#20850,#20851,#20852,#20853,
#20854,#20855,#20856,#20857,#20858,#20859,#20860,#20861,#20862,#20863,#20864,
#20865,#20866,#20867,#20868,#20869,#20870,#20871,#20872,#20873,#20874,#20875,
#20876,#20877,#20878,#20879,#20880,#20881,#20882,#20883,#20884,#20885,#20886,
#20887,#20888,#20889,#20890,#20891,#20892,#20893,#20894,#20895,#20896,#20897,
#20898,#20899,#20900,#20901,#20902,#20903,#20904,#20905,#20906,#20907,#20908,
#20909,#20910,#20911,#20912,#20913,#20914,#20915,#20916,#20917,#20918,#20919,
#20920,#20921,#20922,#20923,#20924,#20925,#20926,#20927,#20928,#20929,#20930,
#20931,#20932,#20933,#20934,#20935,#20936,#20937,#20938,#20939,#20940,#20941,
#20942,#20943,#20944,#20945,#20946,#20947,#20948,#20949,#20950,#20951,#20952,
#20953,#20954,#20955,#20956,#20957,#20958,#20959,#20960,#20961,#20962,#20963,
#20964,#20965,#20966,#20967,#20968,#20969,#20970,#20971,#20972,#20973,#20974,
#20975,#20976,#20977,#20978,#20979,#20980,#20981,#20982,#20983,#20984,#20985,
#20986,#20987,#20988,#20989,#20990,#20991,#20992,#20993,#20994,#20995,#20996,
#20997,#20998,#20999,#21000,#21001,#21002,#21003,#21004,#21005,#21006,#21007,
#21008,#21009,#21010,#21011,#21012,#21013,#21014,#21015,#21016,#21017,#21018,
#21019,#21020,#21021),.UNSPECIFIED.,.F.,.F.,(4,2,2,2,2,2,2,2,2,2,2,2,2,
2,2,2,2,2,2,2,2,2,2,2,2,2,2,2,2,2,2,2,2,2,2,2,2,2,2,2,2,2,2,2,2,2,2,2,2,
2,2,2,2,2,2,2,2,2,2,2,2,2,2,2,2,2,2,2,2,2,2,2,2,2,2,2,2,2,2,2,2,2,2,2,2,
2,2,2,2,2,2,4),(-1.3699358201607,-1.36179106215317,-1.33700599593838,-1.26250800794385,
-1.22119362735239,-1.21873461434529,-1.21781859495292,-1.21727897556568,
-1.2167684148196,-1.21604836910061,-1.21460325264151,-1.20387418969816,
-1.1745527156667,-1.11414316664539,-1.06168371488393,-1.05822984159744,
-1.05689488358093,-1.0559343769297,-1.05491601390065,-1.05357004652269,
-1.05072962867412,-1.02626798798076,-1.01711969656458,-0.951238458716924,
-0.905843311234644,-0.905155783260641,-0.896754164277783,-0.89533322147786,
-0.894614214596374,-0.894051207980658,-0.893419040152832,-0.89276244664608,
-0.890510383945906,-0.871438213757604,-0.852249316263751,-0.803495795394027,
-0.739442413547856,-0.735500614661386,-0.734088646566974,-0.733107179052976,
-0.732197914129689,-0.730961202072346,-0.729643479836477,-0.723781333455508,
-0.714489497572144,-0.6843874755459,-0.635848988356629,-0.576781444265308,
-0.573196265074093,-0.57212946056436,-0.571559566551961,-0.571004622957775,
-0.570321975310099,-0.569594523395977,-0.566443918806259,-0.537851381464733,
-0.490782728245281,-0.417331891131705,-0.412768252981907,-0.411100235969678,
-0.410126302354737,-0.409214909514243,-0.407961207719627,-0.406619963347496,
-0.400402331781344,-0.390376348937076,-0.35566722600915,-0.319610410938011,
-0.254029909536792,-0.250280406441938,-0.249194910144441,-0.248621253097742,
-0.24811717128004,-0.247461360125111,-0.24677140022959,-0.245709852847748,
-0.232056823450463,-0.19815637288566,-0.185123259500274,-0.171506873114694,
-0.119528406112877,-0.110777651274884,-0.107669823985291,-0.0916032390522574,
-0.0889709189572523,-0.0876806029094163,-0.0866698307376031,-0.0855499228265693,
-0.0843957491233048,-0.0826936213980666,-0.0796703625964687,-0.000961575125209731),
 .UNSPECIFIED.);
#125=B_SPLINE_CURVE_WITH_KNOTS('',3,(#21022,#21023,#21024,#21025,#21026,
#21027,#21028,#21029,#21030,#21031,#21032,#21033,#21034,#21035,#21036,#21037,
#21038,#21039,#21040,#21041,#21042,#21043,#21044,#21045,#21046,#21047,#21048,
#21049,#21050,#21051,#21052,#21053,#21054,#21055,#21056,#21057,#21058,#21059,
#21060,#21061,#21062,#21063,#21064,#21065,#21066,#21067,#21068,#21069,#21070,
#21071,#21072,#21073,#21074,#21075,#21076,#21077,#21078,#21079,#21080,#21081,
#21082,#21083,#21084,#21085,#21086,#21087,#21088,#21089,#21090,#21091,#21092,
#21093,#21094,#21095,#21096,#21097,#21098,#21099,#21100,#21101,#21102,#21103,
#21104,#21105,#21106,#21107,#21108,#21109,#21110,#21111,#21112,#21113,#21114,
#21115,#21116,#21117,#21118,#21119,#21120,#21121,#21122,#21123,#21124,#21125,
#21126,#21127,#21128,#21129,#21130,#21131),.UNSPECIFIED.,.F.,.F.,(4,2,2,
2,2,2,2,2,2,2,2,2,2,2,2,2,2,2,2,2,2,2,2,2,2,2,2,2,2,2,2,2,2,2,2,2,2,2,2,
2,2,2,2,2,2,2,2,2,2,2,2,2,2,2,4),(-4.05879903554358,-3.99554088987618,-3.98621912338381,
-3.98503812881777,-3.98429819559836,-3.98360668770163,-3.98304637835795,
-3.98239618382111,-3.98128120791761,-3.97712723929307,-3.90870012322013,
-3.89521413325899,-3.88194115673587,-3.84409423659441,-3.82737011219942,
-3.8252062298073,-3.82385799780418,-3.82259940454519,-3.82168779637406,
-3.82071676951049,-3.81906151916928,-3.81457777495714,-3.7416071005807,
-3.71739937374859,-3.6918251124252,-3.67155298878052,-3.66582267743168,
-3.66233178819508,-3.66158159881658,-3.66088271451388,-3.6603218979078,
-3.65967722540041,-3.65858593458801,-3.65466124682145,-3.58976116230847,
-3.5406275262575,-3.50903661801502,-3.50249712733391,-3.50113652069968,
-3.49986898133139,-3.49895612217392,-3.4979886247264,-3.49662632269505,
-3.49380572196624,-3.48622776825605,-3.48441706283362,-3.4823554363696,
-3.48188080183464,-3.48103750001944,-3.47700410389334,-3.47580949027072,
-3.4743142426484,-3.46972980628327,-3.42460957868219,-3.39850283521087),
 .UNSPECIFIED.);
#126=B_SPLINE_CURVE_WITH_KNOTS('',3,(#21132,#21133,#21134,#21135,#21136,
#21137,#21138,#21139,#21140,#21141,#21142,#21143,#21144,#21145,#21146,#21147,
#21148,#21149,#21150,#21151,#21152,#21153,#21154,#21155,#21156,#21157,#21158,
#21159,#21160,#21161,#21162,#21163,#21164,#21165,#21166,#21167,#21168,#21169,
#21170,#21171,#21172,#21173,#21174,#21175,#21176,#21177,#21178,#21179,#21180,
#21181,#21182,#21183,#21184,#21185,#21186,#21187,#21188,#21189,#21190,#21191,
#21192,#21193,#21194,#21195,#21196,#21197,#21198,#21199,#21200,#21201,#21202,
#21203,#21204,#21205,#21206,#21207,#21208,#21209,#21210,#21211,#21212,#21213,
#21214,#21215,#21216,#21217,#21218,#21219,#21220,#21221,#21222,#21223,#21224,
#21225,#21226,#21227,#21228,#21229,#21230,#21231,#21232,#21233,#21234,#21235,
#21236,#21237,#21238,#21239,#21240,#21241,#21242,#21243,#21244,#21245,#21246,
#21247,#21248,#21249,#21250,#21251,#21252,#21253,#21254,#21255,#21256,#21257,
#21258,#21259,#21260,#21261,#21262,#21263,#21264,#21265,#21266,#21267,#21268,
#21269,#21270,#21271,#21272,#21273,#21274,#21275,#21276,#21277,#21278,#21279,
#21280,#21281,#21282,#21283,#21284,#21285,#21286,#21287,#21288,#21289,#21290,
#21291,#21292,#21293,#21294,#21295,#21296,#21297,#21298,#21299,#21300,#21301,
#21302,#21303,#21304,#21305,#21306,#21307,#21308,#21309,#21310,#21311,#21312,
#21313,#21314,#21315,#21316,#21317,#21318,#21319,#21320,#21321,#21322,#21323,
#21324,#21325,#21326,#21327,#21328,#21329,#21330,#21331,#21332,#21333,#21334,
#21335,#21336,#21337,#21338,#21339,#21340,#21341,#21342,#21343,#21344,#21345,
#21346,#21347,#21348,#21349,#21350,#21351,#21352,#21353,#21354,#21355,#21356,
#21357,#21358,#21359,#21360,#21361,#21362,#21363,#21364,#21365,#21366,#21367,
#21368,#21369,#21370,#21371,#21372,#21373,#21374,#21375,#21376,#21377,#21378,
#21379,#21380,#21381,#21382,#21383,#21384,#21385,#21386,#21387,#21388,#21389,
#21390,#21391,#21392,#21393,#21394,#21395,#21396,#21397,#21398,#21399,#21400,
#21401,#21402,#21403,#21404,#21405,#21406,#21407,#21408,#21409,#21410,#21411,
#21412,#21413,#21414,#21415,#21416,#21417,#21418,#21419),.UNSPECIFIED.,
 .F.,.F.,(4,2,2,2,2,2,2,2,2,2,2,2,2,2,2,2,2,2,2,2,2,2,2,2,2,2,2,2,2,2,2,
2,2,2,2,2,2,2,2,2,2,2,2,2,2,2,2,2,2,2,2,2,2,2,2,2,2,2,2,2,2,2,2,2,2,2,2,
2,2,2,2,2,2,2,2,2,2,2,2,2,2,2,2,2,2,2,2,2,2,2,2,2,2,2,2,2,2,2,2,2,2,2,2,
2,2,2,2,2,2,2,2,2,2,2,2,2,2,2,2,2,2,2,2,2,2,2,2,2,2,2,2,2,2,2,2,2,2,2,2,
2,2,2,2,4),(-2.69197257292336,-2.68558870129701,-2.66197432596306,-2.65732281965966,
-2.65620475698648,-2.65556017445217,-2.65499888971945,-2.65429871859818,
-2.65321677820789,-2.6482947366379,-2.55263675802256,-2.49984122693837,
-2.49739779419988,-2.49593251052439,-2.49460753532955,-2.4936063254273,
-2.49265165286103,-2.49133892620616,-2.48801813592373,-2.44567859191875,
-2.39872534191373,-2.37499323447793,-2.3362198199124,-2.33381717772997,
-2.33293929681208,-2.33234804835674,-2.33177462881831,-2.33108347569428,
-2.32935883503651,-2.31358264844087,-2.31036822500928,-2.25628471440178,
-2.21082490355755,-2.18700079132994,-2.17492369987761,-2.1726764694906,
-2.1714661553163,-2.17047126273508,-2.16945255230329,-2.16756151098957,
-2.16133698384822,-2.05444444382153,-2.03064192808659,-2.02911065115783,
-2.02652218651379,-2.02593947813371,-2.01212372440356,-2.01062498993237,
-2.00988425790518,-2.0093502659947,-2.00877969844171,-2.00800814222508,
-2.00626328234132,-1.96524687361196,-1.85708769983655,-1.85095311777042,
-1.84907282605336,-1.84805628217632,-1.84705163282641,-1.8458337094549,
-1.84355097253,-1.83077785636157,-1.80597512459368,-1.71619481115066,-1.6893468850248,
-1.68742236962878,-1.68667810568068,-1.68614319260008,-1.68557322423781,
-1.6848051389134,-1.68312046652754,-1.68085309042961,-1.6590548811644,-1.63514327775534,
-1.55139690222005,-1.52956577859469,-1.52672439216678,-1.52538691167949,
-1.52436610645546,-1.52327862093308,-1.52158671018237,-1.51652232160609,
-1.45628053824052,-1.38467312540276,-1.38300216294716,-1.38212046344854,
-1.38100624156066,-1.38011864633581,-1.37977223855767,-1.37884347203643,
-1.37839978712563,-1.37762182981665,-1.36577082316945,-1.36433508942931,
-1.36361024735128,-1.36308043411033,-1.3625070581423,-1.36171919124365,
-1.35992603610337,-1.35747595786608,-1.26852972763752,-1.20788237429976,
-1.20409557524715,-1.20270717231946,-1.20173215053389,-1.20082098680541,
-1.19956953811251,-1.19718005917181,-1.18175771447576,-1.14627263588776,
-1.08547717658398,-1.04406229685018,-1.04155987831136,-1.04063639832981,
-1.04009526286447,-1.03958522583693,-1.03886899605185,-1.03753216136736,
-1.02793239847405,-1.00368360305475,-0.948181389592564,-0.885069889383899,
-0.881191899349148,-0.879789513393375,-0.87881063862359,-0.877900579757035,
-0.87665789336991,-0.874321858833368,-0.860604748253787,-0.83329142814411,
-0.775457946310528,-0.730581824977383,-0.719733106799663,-0.718333429689929,
-0.717617822010414,-0.717090399030972,-0.716515165503138,-0.715716956764076,
-0.713867675680136,-0.711320399142619,-0.70481222419764,-0.696070547323417,
-0.684622170995794,-0.66165633052871),.UNSPECIFIED.);
#127=B_SPLINE_CURVE_WITH_KNOTS('',3,(#21424,#21425,#21426,#21427,#21428,
#21429,#21430,#21431,#21432,#21433,#21434,#21435,#21436,#21437,#21438,#21439,
#21440,#21441,#21442,#21443,#21444,#21445,#21446,#21447,#21448,#21449,#21450,
#21451,#21452,#21453,#21454,#21455,#21456,#21457,#21458,#21459,#21460,#21461,
#21462,#21463,#21464,#21465,#21466,#21467,#21468,#21469,#21470,#21471,#21472,
#21473,#21474,#21475,#21476,#21477,#21478,#21479,#21480,#21481,#21482,#21483,
#21484,#21485,#21486,#21487,#21488,#21489,#21490,#21491,#21492,#21493,#21494,
#21495,#21496,#21497,#21498,#21499,#21500,#21501,#21502,#21503,#21504,#21505,
#21506,#21507,#21508,#21509,#21510,#21511,#21512,#21513,#21514,#21515,#21516,
#21517,#21518,#21519,#21520,#21521,#21522,#21523,#21524,#21525,#21526,#21527,
#21528,#21529,#21530,#21531,#21532,#21533,#21534,#21535,#21536,#21537,#21538,
#21539,#21540,#21541,#21542,#21543,#21544,#21545,#21546,#21547,#21548,#21549,
#21550,#21551,#21552,#21553,#21554,#21555,#21556,#21557,#21558,#21559,#21560,
#21561,#21562,#21563,#21564,#21565,#21566,#21567,#21568,#21569,#21570,#21571,
#21572,#21573,#21574,#21575,#21576,#21577,#21578,#21579,#21580,#21581,#21582,
#21583,#21584,#21585,#21586,#21587,#21588,#21589,#21590,#21591,#21592,#21593,
#21594,#21595,#21596,#21597,#21598,#21599,#21600,#21601,#21602,#21603,#21604,
#21605,#21606,#21607,#21608,#21609,#21610,#21611,#21612,#21613,#21614,#21615,
#21616,#21617,#21618,#21619,#21620,#21621,#21622,#21623,#21624,#21625,#21626,
#21627,#21628,#21629,#21630,#21631,#21632,#21633,#21634,#21635,#21636,#21637,
#21638,#21639,#21640,#21641,#21642,#21643,#21644,#21645,#21646,#21647,#21648,
#21649,#21650,#21651,#21652,#21653,#21654,#21655,#21656,#21657,#21658,#21659,
#21660,#21661,#21662,#21663,#21664,#21665,#21666,#21667,#21668,#21669,#21670,
#21671,#21672,#21673,#21674,#21675,#21676,#21677,#21678,#21679,#21680,#21681,
#21682,#21683,#21684,#21685,#21686,#21687,#21688,#21689,#21690,#21691,#21692,
#21693,#21694,#21695,#21696,#21697,#21698,#21699,#21700,#21701,#21702,#21703,
#21704,#21705,#21706,#21707,#21708,#21709,#21710,#21711,#21712,#21713,#21714,
#21715,#21716,#21717,#21718,#21719,#21720,#21721,#21722,#21723,#21724,#21725,
#21726,#21727,#21728,#21729,#21730,#21731,#21732,#21733,#21734,#21735),
 .UNSPECIFIED.,.F.,.F.,(4,2,2,2,2,2,2,2,2,2,2,2,2,2,2,2,2,2,2,2,2,2,2,2,
2,2,2,2,2,2,2,2,2,2,2,2,2,2,2,2,2,2,2,2,2,2,2,2,2,2,2,2,2,2,2,2,2,2,2,2,
2,2,2,2,2,2,2,2,2,2,2,2,2,2,2,2,2,2,2,2,2,2,2,2,2,2,2,2,2,2,2,2,2,2,2,2,
2,2,2,2,2,2,2,2,2,2,2,2,2,2,2,2,2,2,2,2,2,2,2,2,2,2,2,2,2,2,2,2,2,2,2,2,
2,2,2,2,2,2,2,2,2,2,2,2,2,2,2,2,2,2,2,2,2,2,2,4),(-3.39994190379461,-3.36686671547447,
-3.3353143830966,-3.32088860049697,-3.31851875602958,-3.31728242357063,
-3.31637324834893,-3.31539169536757,-3.31368516309039,-3.30886169714366,
-3.23465097473941,-3.18488367286284,-3.16591242973773,-3.16034992324727,
-3.15693752967021,-3.15593522920706,-3.1553119929754,-3.15474703411569,
-3.15402406301256,-3.15249496903317,-3.14223517336176,-3.11168002817093,
-3.04859834456225,-3.01783989468509,-2.99824871151382,-2.99570139463886,
-2.99442829638924,-2.99351421204596,-2.99254798202207,-2.99119165018948,
-2.98839694551298,-2.95932544966547,-2.94092748259092,-2.88926552585634,
-2.83712026523338,-2.83399167194498,-2.83301979899301,-2.83240351614683,
-2.8318365067624,-2.83109951512332,-2.8295545202872,-2.81845345414458,-2.81706355541898,
-2.81543496704861,-2.8123635238008,-2.80950952767162,-2.79962581751556,
-2.7208056509041,-2.68047808446914,-2.67625076409714,-2.6730904645732,-2.67169993695668,
-2.67067429421303,-2.66972579526836,-2.66843675721008,-2.6652535811524,
-2.63029675143227,-2.62598101683703,-2.55653590222699,-2.53454206936298,
-2.51432613623547,-2.51106838865576,-2.51008401004515,-2.50946487433436,
-2.50889877342128,-2.50816776951067,-2.50659679170939,-2.49534468176697,
-2.39767689545897,-2.35743677085424,-2.35105242774565,-2.34920988297564,
-2.34808896687107,-2.34707865085006,-2.34579079668514,-2.34317002487223,
-2.32732565526589,-2.32605362037779,-2.32484356954319,-2.32335734684001,
-2.31793892446429,-2.31107748677495,-2.2201415332063,-2.19777364778313,
-2.18862767193993,-2.187268558565,-2.1865720666893,-2.18601112699911,-2.18536402764059,
-2.18426332121985,-2.18025267640077,-2.17978475919677,-2.07644517793773,
-2.03106152580403,-2.027288211116,-2.02590209091859,-2.02492783924187,-2.02401673205298,
-2.02276433029175,-2.02031723875477,-2.00358819772434,-1.96317906022367,
-1.86996907063978,-1.86539299402114,-1.86421448054179,-1.86349249576684,
-1.86292765753868,-1.86230386418786,-1.86127861082753,-1.85765838314073,
-1.776143950284,-1.73096656151708,-1.72666906629073,-1.72462057014749,-1.72341556570895,
-1.72191617834342,-1.7198341138536,-1.71922605406235,-1.71777617153632,
-1.71717606508104,-1.71543648900971,-1.71155567855791,-1.70503258657368,
-1.70310681812096,-1.70196719615696,-1.7010606744472,-1.69984978381114,
-1.69764462865564,-1.68622134319837,-1.66388713706814,-1.6197904993009,
-1.56402705404717,-1.5613312353022,-1.55976279743349,-1.55900937887274,
-1.54310235539281,-1.54137404069008,-1.54068229855055,-1.54010873964246,
-1.5395177235168,-1.53864086524163,-1.53630061824498,-1.47992250780356,
-1.40229277090721,-1.39874793901543,-1.39668724913639,-1.3928877448191,
-1.38932053123187,-1.38787135919095,-1.38195088094742,-1.38009682707836,
-1.37908563541282,-1.37808067429462,-1.37685425645365,-1.37457771026683,
-1.3699358201607),.UNSPECIFIED.);
#128=B_SPLINE_CURVE_WITH_KNOTS('',3,(#21737,#21738,#21739,#21740,#21741,
#21742,#21743,#21744,#21745,#21746,#21747,#21748,#21749,#21750,#21751,#21752,
#21753,#21754,#21755,#21756,#21757,#21758,#21759,#21760,#21761,#21762,#21763,
#21764,#21765,#21766,#21767,#21768,#21769,#21770,#21771,#21772,#21773,#21774,
#21775,#21776,#21777,#21778,#21779,#21780,#21781,#21782,#21783,#21784,#21785,
#21786,#21787,#21788,#21789,#21790,#21791,#21792,#21793,#21794,#21795,#21796,
#21797,#21798,#21799,#21800,#21801,#21802,#21803,#21804,#21805,#21806,#21807,
#21808,#21809,#21810,#21811,#21812,#21813,#21814,#21815,#21816,#21817,#21818,
#21819,#21820,#21821,#21822,#21823,#21824,#21825,#21826,#21827,#21828,#21829,
#21830,#21831,#21832,#21833,#21834,#21835,#21836),.UNSPECIFIED.,.F.,.F.,
(4,2,2,2,2,2,2,2,2,2,2,2,2,2,2,2,2,2,2,2,2,2,2,2,2,2,2,2,2,2,2,2,2,2,2,
2,2,2,2,2,2,2,2,2,2,2,2,2,2,4),(-0.66165633052871,-0.635984384500012,-0.562974439167031,
-0.55846545761205,-0.556805679247827,-0.555833318267037,-0.554921310569708,
-0.553663501486698,-0.552316608348213,-0.54600727273951,-0.512179291842036,
-0.460240222757477,-0.399721702144545,-0.395981677764637,-0.394897181874368,
-0.394323694392617,-0.393819559522827,-0.393163399143196,-0.392472969700445,
-0.389819399905494,-0.385801683552211,-0.373690020797935,-0.343571448335568,
-0.31846175840726,-0.283613520019905,-0.267874805845795,-0.238065132715674,
-0.235252396569741,-0.233891513264224,-0.232923946812276,-0.232010148828416,
-0.230739917280611,-0.229375868741327,-0.227175090855721,-0.210421535739774,
-0.169549262745376,-0.155229153504232,-0.140886456995155,-0.0865925462122985,
-0.085810963723819,-0.0739648514776291,-0.0725293002386787,-0.0718045093759444,
-0.0712747139713807,-0.070701337578965,-0.0699134359344539,-0.0690395041762753,
-0.0675348758374232,-0.0643468711601317,-0.00096143554933532),
 .UNSPECIFIED.);
#129=B_SPLINE_CURVE_WITH_KNOTS('',3,(#21837,#21838,#21839,#21840,#21841,
#21842,#21843,#21844,#21845,#21846,#21847,#21848,#21849,#21850,#21851,#21852,
#21853,#21854,#21855,#21856,#21857,#21858,#21859,#21860,#21861,#21862,#21863,
#21864,#21865,#21866,#21867,#21868,#21869,#21870,#21871,#21872,#21873,#21874,
#21875,#21876,#21877,#21878,#21879,#21880,#21881,#21882,#21883,#21884,#21885,
#21886,#21887,#21888,#21889,#21890,#21891,#21892,#21893,#21894,#21895,#21896,
#21897,#21898,#21899,#21900,#21901,#21902,#21903,#21904,#21905,#21906,#21907,
#21908,#21909,#21910,#21911,#21912,#21913,#21914,#21915,#21916,#21917,#21918,
#21919,#21920,#21921,#21922,#21923,#21924,#21925,#21926,#21927,#21928,#21929,
#21930,#21931,#21932,#21933,#21934,#21935,#21936,#21937,#21938,#21939,#21940,
#21941,#21942,#21943,#21944,#21945,#21946,#21947,#21948,#21949,#21950,#21951,
#21952,#21953,#21954,#21955,#21956,#21957,#21958,#21959,#21960,#21961,#21962,
#21963,#21964,#21965,#21966,#21967,#21968,#21969,#21970,#21971,#21972,#21973,
#21974,#21975,#21976,#21977,#21978,#21979,#21980,#21981,#21982,#21983,#21984,
#21985,#21986,#21987,#21988,#21989,#21990,#21991,#21992,#21993,#21994,#21995,
#21996,#21997,#21998,#21999,#22000,#22001,#22002,#22003,#22004,#22005,#22006,
#22007,#22008,#22009,#22010,#22011,#22012,#22013,#22014,#22015,#22016,#22017,
#22018,#22019,#22020,#22021,#22022),.UNSPECIFIED.,.F.,.F.,(4,2,2,2,2,2,
2,2,2,2,2,2,2,2,2,2,2,2,2,2,2,2,2,2,2,2,2,2,2,2,2,2,2,2,2,2,2,2,2,2,2,2,
2,2,2,2,2,2,2,2,2,2,2,2,2,2,2,2,2,2,2,2,2,2,2,2,2,2,2,2,2,2,2,2,2,2,2,2,
2,2,2,2,2,2,2,2,2,2,2,2,2,2,4),(-4.06047580903049,-3.98883313326063,-3.97433174222971,
-3.97231615819279,-3.97103026322687,-3.96981660773599,-3.9689101138855,
-3.96791765123857,-3.96615558855538,-3.96093779637892,-3.87982606029779,
-3.86711580617506,-3.85513990465006,-3.82410279092963,-3.81045430326376,
-3.80939165982954,-3.80870133594423,-3.80804533399209,-3.80754143495988,
-3.80696833782391,-3.80588493988309,-3.80215190100195,-3.74191149701363,
-3.70677328960837,-3.66727014731604,-3.65078911791453,-3.64906328254663,
-3.64753294432398,-3.64648057880591,-3.64545111107353,-3.64421233997431,
-3.64112862306226,-3.61281424433995,-3.5955781109469,-3.56064874121213,
-3.5133444215052,-3.4879053506647,-3.48626766082138,-3.48567275931329,-3.48508275686296,
-3.48450875733961,-3.48381483723945,-3.48214040520487,-3.46729561720466,
-3.46590327425025,-3.46492562397453,-3.46331580987113,-3.425703124508,-3.37740946237235,
-3.34309732977652,-3.3331423515119,-3.32695868926105,-3.32562004072067,
-3.32436829888795,-3.32345741237483,-3.32248315168608,-3.32081240291859,
-3.31622857999019,-3.24619217601516,-3.19027105678354,-3.1728249390854,
-3.16461403063333,-3.16329556551346,-3.16260203825595,-3.16209519610309,
-3.16154471064184,-3.16057361738588,-3.15774124008521,-3.11245370346695,
-3.05411473487646,-3.03178403192391,-3.00612640876865,-3.00314283346351,
-3.00176982781755,-3.00074735164778,-2.99979478305143,-2.99848937510751,
-2.99521015756728,-2.95532292213387,-2.90218565081376,-2.86662338193906,
-2.84999521019353,-2.8418396676274,-2.84052324068034,-2.83996270506864,
-2.83939335217304,-2.83885807977053,-2.83811188456463,-2.83617445442692,
-2.80846934513124,-2.74391432612601,-2.69999660334342,-2.69216032599444),
 .UNSPECIFIED.);
#130=B_SPLINE_CURVE_WITH_KNOTS('',3,(#22028,#22029,#22030,#22031,#22032,
#22033,#22034,#22035,#22036,#22037,#22038,#22039,#22040,#22041,#22042,#22043,
#22044,#22045,#22046,#22047,#22048,#22049,#22050,#22051,#22052,#22053,#22054,
#22055,#22056,#22057,#22058,#22059,#22060,#22061,#22062,#22063,#22064,#22065,
#22066,#22067,#22068,#22069,#22070,#22071,#22072,#22073,#22074,#22075,#22076,
#22077,#22078,#22079,#22080,#22081,#22082,#22083,#22084,#22085,#22086,#22087,
#22088,#22089,#22090,#22091,#22092,#22093,#22094,#22095,#22096,#22097,#22098,
#22099,#22100,#22101,#22102,#22103,#22104,#22105,#22106,#22107,#22108,#22109,
#22110,#22111,#22112,#22113,#22114,#22115,#22116,#22117,#22118,#22119,#22120,
#22121,#22122,#22123,#22124,#22125,#22126,#22127,#22128,#22129,#22130,#22131,
#22132,#22133,#22134,#22135,#22136,#22137,#22138,#22139,#22140,#22141,#22142,
#22143,#22144,#22145,#22146,#22147,#22148,#22149,#22150,#22151,#22152,#22153,
#22154,#22155,#22156,#22157,#22158,#22159,#22160,#22161,#22162,#22163,#22164,
#22165,#22166,#22167,#22168,#22169,#22170,#22171,#22172,#22173,#22174,#22175,
#22176,#22177,#22178,#22179,#22180,#22181,#22182,#22183,#22184,#22185,#22186,
#22187,#22188,#22189,#22190,#22191,#22192,#22193,#22194,#22195,#22196,#22197,
#22198,#22199,#22200,#22201,#22202,#22203,#22204,#22205,#22206,#22207,#22208,
#22209,#22210,#22211,#22212,#22213,#22214,#22215,#22216,#22217,#22218,#22219,
#22220,#22221,#22222,#22223,#22224,#22225,#22226,#22227,#22228,#22229,#22230,
#22231,#22232,#22233,#22234,#22235,#22236,#22237,#22238,#22239,#22240,#22241,
#22242,#22243,#22244,#22245,#22246,#22247),.UNSPECIFIED.,.F.,.F.,(4,2,2,
2,2,2,2,2,2,2,2,2,2,2,2,2,2,2,2,2,2,2,2,2,2,2,2,2,2,2,2,2,2,2,2,2,2,2,2,
2,2,2,2,2,2,2,2,2,2,2,2,2,2,2,2,2,2,2,2,2,2,2,2,2,2,2,2,2,2,2,2,2,2,2,2,
2,2,2,2,2,2,2,2,2,2,2,2,2,2,2,2,2,2,2,2,2,2,2,2,2,2,2,2,2,2,2,2,2,2,4),
(-1.36933136652665,-1.35859732837197,-1.35679844377335,-1.3560756299863,
-1.35554637601637,-1.35497267364315,-1.35419864345503,-1.35242748297969,
-1.35001542973958,-1.29723606513501,-1.23799221414758,-1.2202622694919,
-1.19902079686839,-1.1961645522769,-1.19484476680884,-1.19382686061541,
-1.19273205156696,-1.19100700614308,-1.18567401504065,-1.15554947806589,
-1.08392996334039,-1.03702220569548,-1.03420218753497,-1.0332327701601,
-1.03268247099359,-1.0321753118985,-1.03163529287504,-1.03052243514212,
-1.02591438107519,-0.986920138840623,-0.941386962772281,-0.877672530167167,
-0.873749491490016,-0.872340260322915,-0.871359481999703,-0.870449906166499,
-0.869211323069769,-0.86683139099472,-0.852481402160477,-0.834722860015409,
-0.79528494363612,-0.754802711299645,-0.713568240721987,-0.711147339135666,
-0.710328017645314,-0.709772443060438,-0.709266430859045,-0.708729123885893,
-0.708058962826953,-0.705648388506033,-0.702093570402397,-0.691843265438953,
-0.651595348269289,-0.623878390672399,-0.59084091278337,-0.578798136419498,
-0.572594587476458,-0.571198852570911,-0.569993318363737,-0.568512451345134,
-0.566427324196033,-0.565844930417326,-0.5641022026392,-0.563076093071555,
-0.561496730412553,-0.556726341606073,-0.551340673535203,-0.54955529351537,
-0.548557801069253,-0.547560445768462,-0.546312955568382,-0.543890556503511,
-0.528720613115969,-0.49936180784944,-0.491941695176374,-0.445450396081606,
-0.401591305535271,-0.389481453388935,-0.387877094519413,-0.387139706156022,
-0.386572570986094,-0.385956335709198,-0.385322617974015,-0.384395670430321,
-0.376732035161832,-0.360961361345349,-0.338245353325395,-0.317451678039698,
-0.233796636418477,-0.228371867418463,-0.22658133227778,-0.22558284130101,
-0.224585720923131,-0.22334036572751,-0.220927982166584,-0.205857449705273,
-0.158454538121891,-0.142348808427161,-0.134443639150519,-0.125493795394888,
-0.0690603051038075,-0.0655771059460002,-0.0645222179554844,-0.0639547035293388,
-0.0633941699555315,-0.0628556305844188,-0.0621810628609401,-0.0611562183700187,
-0.0592733000428786,-0.000961179395231121),.UNSPECIFIED.);
#131=B_SPLINE_CURVE_WITH_KNOTS('',3,(#22248,#22249,#22250,#22251,#22252,
#22253,#22254,#22255,#22256,#22257,#22258,#22259,#22260,#22261,#22262,#22263,
#22264,#22265,#22266,#22267,#22268,#22269,#22270,#22271,#22272,#22273,#22274,
#22275,#22276,#22277,#22278,#22279,#22280,#22281,#22282,#22283,#22284,#22285,
#22286,#22287,#22288,#22289,#22290,#22291,#22292,#22293,#22294,#22295,#22296,
#22297,#22298,#22299,#22300,#22301,#22302,#22303,#22304,#22305,#22306,#22307,
#22308,#22309,#22310,#22311,#22312,#22313,#22314,#22315,#22316,#22317,#22318,
#22319,#22320,#22321,#22322,#22323,#22324,#22325,#22326,#22327,#22328,#22329,
#22330,#22331,#22332,#22333,#22334,#22335,#22336,#22337,#22338,#22339),
 .UNSPECIFIED.,.F.,.F.,(4,2,2,2,2,2,2,2,2,2,2,2,2,2,2,2,2,2,2,2,2,2,2,2,
2,2,2,2,2,2,2,2,2,2,2,2,2,2,2,2,2,2,2,2,2,4),(-4.06120382105492,-3.97640958314511,
-3.96975879707925,-3.96672639584915,-3.96430994746887,-3.96306390334572,
-3.9621535973804,-3.96117656644359,-3.9597803792858,-3.95594182519937,-3.89726557700427,
-3.86480146420021,-3.84329555144617,-3.81339687041797,-3.80343721157549,
-3.80245568316642,-3.80179931577592,-3.80116733848241,-3.80060440339047,
-3.79988535767731,-3.79846392784794,-3.79005022970795,-3.78938383091348,
-3.74400169621109,-3.72002255434853,-3.69601452988427,-3.65958898768583,
-3.64391669635236,-3.64149710214395,-3.64025038758376,-3.63925332739859,
-3.63825585745862,-3.63646977753036,-3.63107681825785,-3.54785806701969,
-3.5071706777738,-3.48213777894182,-3.47963593964031,-3.47895828503783,
-3.47841890659564,-3.4779120817863,-3.47736088245231,-3.47638665970961,
-3.47353389442328,-3.42479367187728,-3.39994190379461),.UNSPECIFIED.);
#132=B_SPLINE_CURVE_WITH_KNOTS('',3,(#22340,#22341,#22342,#22343,#22344,
#22345,#22346,#22347,#22348,#22349,#22350,#22351,#22352,#22353,#22354,#22355,
#22356,#22357,#22358,#22359,#22360,#22361,#22362,#22363,#22364,#22365,#22366,
#22367,#22368,#22369,#22370,#22371,#22372,#22373,#22374,#22375,#22376,#22377,
#22378,#22379,#22380,#22381,#22382,#22383,#22384,#22385,#22386,#22387,#22388,
#22389,#22390,#22391,#22392,#22393,#22394,#22395,#22396,#22397,#22398,#22399,
#22400,#22401,#22402,#22403,#22404,#22405,#22406,#22407,#22408,#22409,#22410,
#22411,#22412,#22413,#22414,#22415,#22416,#22417,#22418,#22419,#22420,#22421,
#22422,#22423,#22424,#22425,#22426,#22427,#22428,#22429,#22430,#22431,#22432,
#22433,#22434,#22435,#22436,#22437,#22438,#22439,#22440,#22441,#22442,#22443,
#22444,#22445,#22446,#22447,#22448,#22449,#22450,#22451,#22452,#22453,#22454,
#22455,#22456,#22457,#22458,#22459,#22460,#22461,#22462,#22463,#22464,#22465,
#22466,#22467,#22468,#22469,#22470,#22471,#22472,#22473,#22474,#22475,#22476,
#22477,#22478,#22479,#22480,#22481,#22482,#22483,#22484,#22485,#22486,#22487,
#22488,#22489,#22490,#22491,#22492,#22493,#22494,#22495,#22496,#22497,#22498,
#22499,#22500,#22501,#22502,#22503,#22504,#22505,#22506,#22507,#22508,#22509,
#22510,#22511,#22512,#22513,#22514,#22515,#22516,#22517,#22518,#22519,#22520,
#22521,#22522,#22523,#22524,#22525,#22526,#22527,#22528,#22529,#22530,#22531,
#22532,#22533,#22534,#22535,#22536,#22537,#22538,#22539,#22540,#22541,#22542,
#22543,#22544,#22545,#22546,#22547,#22548,#22549,#22550,#22551,#22552,#22553,
#22554,#22555,#22556,#22557,#22558,#22559,#22560,#22561,#22562,#22563,#22564,
#22565,#22566,#22567,#22568,#22569,#22570,#22571,#22572,#22573,#22574,#22575,
#22576,#22577,#22578,#22579,#22580,#22581,#22582,#22583,#22584,#22585,#22586,
#22587,#22588,#22589,#22590,#22591,#22592,#22593,#22594,#22595,#22596,#22597,
#22598,#22599,#22600,#22601,#22602,#22603,#22604,#22605,#22606,#22607,#22608,
#22609,#22610,#22611,#22612,#22613,#22614,#22615),.UNSPECIFIED.,.F.,.F.,
(4,2,2,2,2,2,2,2,2,2,2,2,2,2,2,2,2,2,2,2,2,2,2,2,2,2,2,2,2,2,2,2,2,2,2,
2,2,2,2,2,2,2,2,2,2,2,2,2,2,2,2,2,2,2,2,2,2,2,2,2,2,2,2,2,2,2,2,2,2,2,2,
2,2,2,2,2,2,2,2,2,2,2,2,2,2,2,2,2,2,2,2,2,2,2,2,2,2,2,2,2,2,2,2,2,2,2,2,
2,2,2,2,2,2,2,2,2,2,2,2,2,2,2,2,2,2,2,2,2,2,2,2,2,2,2,2,2,2,4),(-2.69216032599444,
-2.68256417590344,-2.68007713642079,-2.6788062022544,-2.67789264630646,
-2.67692602743868,-2.67556760439536,-2.67276359534767,-2.64327892100576,
-2.57086876165611,-2.52042625896441,-2.5181422908361,-2.51728383272484,
-2.51669308696804,-2.51611956159346,-2.51542759662574,-2.51369733528641,
-2.49771168508564,-2.41046215113946,-2.37493365698338,-2.35950229976759,
-2.35711082110835,-2.35585997463697,-2.35494919890404,-2.35397454470261,
-2.35258658412885,-2.34880049841245,-2.2880662356285,-2.19930509586882,
-2.19680480713766,-2.19496902789737,-2.19418144646227,-2.19360827039963,
-2.19307863629407,-2.1923540315637,-2.1909187478434,-2.17907073651276,-2.12977394733911,
-2.08031455149015,-2.04176552373685,-2.03764833910232,-2.03455448358542,
-2.03317608994889,-2.03215261015968,-2.03120126284038,-2.02964907861517,
-2.02550019593995,-1.97134839628577,-1.87763228495316,-1.87283790101063,
-1.87176629945954,-1.87106939154301,-1.87050841205929,-1.86986159689154,
-1.86873325614486,-1.86394951813639,-1.80911394186765,-1.74311979734322,
-1.71462403543459,-1.71153454203009,-1.71029458016937,-1.70926456707442,
-1.70821209800044,-1.70668243512435,-1.70277420196482,-1.65350355853836,
-1.56391901330394,-1.56218150430741,-1.55047099935864,-1.54904016339376,
-1.54831657964489,-1.54778710342285,-1.547213504572,-1.5464402249623,-1.54467402977646,
-1.5422700451172,-1.46078336800303,-1.41563364008452,-1.41121782448186,
-1.4096041767702,-1.40840915117971,-1.4045518372305,-1.40409700130604,-1.39063331823151,
-1.38839187943923,-1.38705736102138,-1.38603704690316,-1.38494836940782,
-1.38325107425292,-1.37814516105983,-1.31782573627011,-1.2524940840427,
-1.24879604868922,-1.24368515122984,-1.22766826844726,-1.22593662829394,
-1.22524427368686,-1.22467048991183,-1.22407954653552,-1.22322096294083,
-1.22095467146577,-1.17183282655734,-1.11892842194507,-1.09893475995475,
-1.06867398955178,-1.06585070310348,-1.06448723373829,-1.06351896770124,
-1.06260543310214,-1.06133703451081,-1.05888273429333,-1.04148420725421,
-0.998092735258393,-0.9462339516449,-0.922939634532858,-0.92100927969179,
-0.904769821228077,-0.903204833015748,-0.902447730867808,-0.901909374934994,
-0.901398145291054,-0.900674195685458,-0.899210215999472,-0.886232376356095,
-0.861009631202176,-0.816054798288133,-0.781907803041267,-0.745979175078631,
-0.742774989588326,-0.741482132788039,-0.740532510972375,-0.739507269624768,
-0.738120140040361,-0.735078190385059,-0.730994764849574,-0.721074799918885,
-0.68696880144044,-0.662395452864075),.UNSPECIFIED.);
#133=B_SPLINE_CURVE_WITH_KNOTS('',3,(#22620,#22621,#22622,#22623,#22624,
#22625,#22626,#22627,#22628,#22629,#22630,#22631,#22632,#22633,#22634,#22635,
#22636,#22637,#22638,#22639,#22640,#22641,#22642,#22643,#22644,#22645,#22646,
#22647,#22648,#22649,#22650,#22651,#22652,#22653,#22654,#22655,#22656,#22657,
#22658,#22659,#22660,#22661,#22662,#22663,#22664,#22665,#22666,#22667,#22668,
#22669,#22670,#22671,#22672,#22673,#22674,#22675,#22676,#22677,#22678,#22679,
#22680,#22681,#22682,#22683,#22684,#22685,#22686,#22687,#22688,#22689,#22690,
#22691,#22692,#22693,#22694,#22695,#22696,#22697,#22698,#22699,#22700,#22701,
#22702,#22703,#22704,#22705,#22706,#22707,#22708,#22709,#22710,#22711,#22712,
#22713,#22714,#22715,#22716,#22717,#22718,#22719,#22720,#22721,#22722,#22723,
#22724,#22725,#22726,#22727,#22728,#22729,#22730,#22731,#22732,#22733,#22734,
#22735,#22736,#22737,#22738,#22739,#22740,#22741,#22742,#22743,#22744,#22745,
#22746,#22747,#22748,#22749,#22750,#22751,#22752,#22753,#22754,#22755,#22756,
#22757,#22758,#22759,#22760,#22761,#22762,#22763,#22764,#22765,#22766,#22767,
#22768,#22769,#22770,#22771,#22772,#22773,#22774,#22775,#22776,#22777,#22778,
#22779,#22780,#22781,#22782,#22783,#22784,#22785,#22786,#22787,#22788,#22789,
#22790,#22791,#22792,#22793,#22794,#22795,#22796,#22797,#22798,#22799,#22800,
#22801,#22802,#22803,#22804,#22805,#22806,#22807,#22808,#22809,#22810,#22811,
#22812,#22813,#22814,#22815,#22816,#22817,#22818,#22819,#22820,#22821,#22822,
#22823,#22824,#22825,#22826,#22827,#22828,#22829,#22830,#22831,#22832,#22833,
#22834,#22835,#22836,#22837,#22838,#22839,#22840,#22841,#22842,#22843,#22844,
#22845,#22846,#22847,#22848,#22849,#22850,#22851,#22852,#22853,#22854,#22855,
#22856,#22857,#22858,#22859,#22860,#22861,#22862,#22863,#22864,#22865,#22866,
#22867,#22868,#22869,#22870,#22871,#22872,#22873,#22874,#22875,#22876,#22877,
#22878,#22879,#22880,#22881,#22882,#22883,#22884,#22885,#22886,#22887,#22888,
#22889,#22890,#22891,#22892,#22893,#22894,#22895,#22896,#22897,#22898,#22899,
#22900,#22901,#22902,#22903,#22904,#22905,#22906,#22907,#22908,#22909),
 .UNSPECIFIED.,.F.,.F.,(4,2,2,2,2,2,2,2,2,2,2,2,2,2,2,2,2,2,2,2,2,2,2,2,
2,2,2,2,2,2,2,2,2,2,2,2,2,2,2,2,2,2,2,2,2,2,2,2,2,2,2,2,2,2,2,2,2,2,2,2,
2,2,2,2,2,2,2,2,2,2,2,2,2,2,2,2,2,2,2,2,2,2,2,2,2,2,2,2,2,2,2,2,2,2,2,2,
2,2,2,2,2,2,2,2,2,2,2,2,2,2,2,2,2,2,2,2,2,2,2,2,2,2,2,2,2,2,2,2,2,2,2,2,
2,2,2,2,2,2,2,2,2,2,2,2,4),(-3.39977149278874,-3.38090444245079,-3.34558587810495,
-3.29698398445742,-3.29513477038172,-3.2943446600453,-3.29377086426373,
-3.29324155046521,-3.29251869404242,-3.29109082141869,-3.27946752807907,
-3.27851113591785,-3.27791993458937,-3.27535674479116,-3.21737635612005,
-3.17205070245837,-3.14839549078539,-3.14053273971339,-3.13709799326763,
-3.13444542537949,-3.13315666524144,-3.13218771724792,-3.1312260803416,
-3.12988740567935,-3.12641208834923,-3.07178887484913,-3.03252891959327,
-2.97764820410214,-2.97286607845193,-2.9717376936666,-2.97109078116529,
-2.97052967304816,-2.96983255046175,-2.96876052033718,-2.96396260594337,
-2.87655431671365,-2.8155400939395,-2.81301730177609,-2.81151909283647,
-2.81016892174822,-2.80916371719404,-2.80821499292269,-2.80692557156988,
-2.80374106149397,-2.76871256812483,-2.6861348869615,-2.67294394698349,
-2.6574246147251,-2.65001321130818,-2.64872593199498,-2.64804444686028,
-2.64748944441994,-2.6469185996763,-2.64584744123566,-2.64222572299929,
-2.64118773642224,-2.64087829827459,-2.54317278266234,-2.49647707131484,
-2.49189195377732,-2.48958879730833,-2.48818188948226,-2.48689864547418,
-2.48590469157775,-2.48493658992919,-2.48357365316847,-2.48075244045645,
-2.4505770359127,-2.43163922203203,-2.36658929029306,-2.32852548778813,
-2.32613335409478,-2.32525692182561,-2.3246659266834,-2.32409217472185,
-2.32339995470954,-2.32166915212564,-2.30568284989736,-2.30441447683426,
-2.30212845782966,-2.2921277586897,-2.24595588792538,-2.20148288131914,
-2.18055017202233,-2.16732336259214,-2.1650184638292,-2.16379570749562,
-2.16288786280276,-2.16189928442285,-2.16015836863715,-2.1550963624773,
-2.14994731037251,-2.14887023577338,-2.14748281520703,-2.14697493512781,
-2.14561049694145,-2.14352001371974,-2.14166729228366,-2.14044159183517,
-2.1386827353804,-2.1310226569701,-2.05564338000376,-2.03051649775536,-2.00495779899638,
-2.00305443343479,-2.00231367367199,-2.00177967169533,-2.0012091033308,
-2.00043756338333,-1.99869281358552,-1.95768226619634,-1.84993839895519,
-1.8434532454316,-1.8415317447069,-1.84039302913161,-1.83948632541065,-1.83827403833674,
-1.83601765734853,-1.82376595128609,-1.79957709990969,-1.75378016684408,
-1.69540852828863,-1.69364875373075,-1.69169087896402,-1.68122655765804,
-1.67984167366494,-1.67912989312402,-1.67860345939771,-1.6780274200856,
-1.67724096301429,-1.67539993296399,-1.67286869204425,-1.58422623865686,
-1.52342992023747,-1.51964633387812,-1.51825851644815,-1.51728372084873,
-1.51637262137671,-1.51512103251473,-1.51267833237566,-1.49731365652859,
-1.46183850426419,-1.38162107220087,-1.37876532622551,-1.36933136652665),
 .UNSPECIFIED.);
#134=B_SPLINE_CURVE_WITH_KNOTS('',3,(#22911,#22912,#22913,#22914,#22915,
#22916,#22917,#22918,#22919,#22920,#22921,#22922,#22923,#22924,#22925,#22926,
#22927,#22928,#22929,#22930,#22931,#22932,#22933,#22934,#22935,#22936,#22937,
#22938,#22939,#22940,#22941,#22942,#22943,#22944,#22945,#22946,#22947,#22948,
#22949,#22950,#22951,#22952,#22953,#22954,#22955,#22956,#22957,#22958,#22959,
#22960,#22961,#22962,#22963,#22964,#22965,#22966,#22967,#22968,#22969,#22970,
#22971,#22972,#22973,#22974,#22975,#22976,#22977,#22978,#22979,#22980,#22981,
#22982,#22983,#22984,#22985,#22986,#22987,#22988,#22989,#22990,#22991,#22992,
#22993,#22994,#22995,#22996,#22997,#22998,#22999,#23000,#23001,#23002,#23003,
#23004,#23005,#23006,#23007,#23008,#23009,#23010,#23011,#23012),
 .UNSPECIFIED.,.F.,.F.,(4,2,2,2,2,2,2,2,2,2,2,2,2,2,2,2,2,2,2,2,2,2,2,2,
2,2,2,2,2,2,2,2,2,2,2,2,2,2,2,2,2,2,2,2,2,2,2,2,2,2,4),(-0.662395452864075,
-0.636565501350124,-0.590829186366297,-0.589512179980496,-0.587975443379499,
-0.585595470404861,-0.583104391398326,-0.580517051134528,-0.579581367318058,
-0.579037786371118,-0.578528599275995,-0.577818467473817,-0.57705282609667,
-0.573316651020191,-0.547688846920168,-0.504753401896079,-0.425388452164051,
-0.42070173659393,-0.418843089666003,-0.417830834810713,-0.416825732222374,
-0.41560047040439,-0.414298672346237,-0.40867105374896,-0.39985425249306,
-0.390990068151443,-0.350308828085196,-0.319371310780197,-0.261149804359824,
-0.257753554155548,-0.256709046194757,-0.256143601808686,-0.25563892205914,
-0.254971287059037,-0.254264803884776,-0.25316399171694,-0.239472971966821,
-0.209699904381192,-0.19815665668234,-0.1857773545203,-0.102943180665461,
-0.0975759915845706,-0.0957931285325462,-0.0947961661521012,-0.0937987644111212,
-0.0925503530051014,-0.0912164737157821,-0.0890874625231243,-0.0849683350027143,
-0.0749314486993903,-0.000961829325271721),.UNSPECIFIED.);
#135=B_SPLINE_CURVE_WITH_KNOTS('',3,(#23013,#23014,#23015,#23016,#23017,
#23018,#23019,#23020,#23021,#23022,#23023,#23024,#23025,#23026,#23027,#23028,
#23029,#23030,#23031,#23032,#23033,#23034,#23035,#23036,#23037,#23038,#23039,
#23040,#23041,#23042,#23043,#23044,#23045,#23046,#23047,#23048,#23049,#23050,
#23051,#23052,#23053,#23054,#23055,#23056,#23057,#23058,#23059,#23060,#23061,
#23062,#23063,#23064,#23065,#23066,#23067,#23068,#23069,#23070,#23071,#23072,
#23073,#23074,#23075,#23076,#23077,#23078,#23079,#23080,#23081,#23082,#23083,
#23084,#23085,#23086,#23087,#23088,#23089,#23090,#23091,#23092,#23093,#23094,
#23095,#23096,#23097,#23098,#23099,#23100,#23101,#23102,#23103,#23104,#23105,
#23106,#23107,#23108,#23109,#23110,#23111,#23112,#23113,#23114,#23115,#23116,
#23117,#23118,#23119,#23120,#23121,#23122,#23123,#23124,#23125,#23126,#23127,
#23128,#23129,#23130,#23131,#23132,#23133,#23134,#23135,#23136,#23137,#23138,
#23139,#23140,#23141,#23142,#23143,#23144,#23145,#23146,#23147,#23148,#23149,
#23150,#23151,#23152,#23153,#23154,#23155,#23156,#23157,#23158,#23159,#23160,
#23161,#23162,#23163,#23164,#23165,#23166,#23167,#23168,#23169,#23170,#23171,
#23172,#23173,#23174,#23175,#23176,#23177,#23178,#23179,#23180,#23181,#23182,
#23183,#23184,#23185,#23186,#23187,#23188,#23189,#23190,#23191,#23192,#23193,
#23194,#23195,#23196,#23197,#23198,#23199,#23200,#23201,#23202,#23203,#23204,
#23205,#23206,#23207,#23208,#23209,#23210,#23211,#23212,#23213,#23214,#23215,
#23216,#23217,#23218),.UNSPECIFIED.,.F.,.F.,(4,2,2,2,2,2,2,2,2,2,2,2,2,
2,2,2,2,2,2,2,2,2,2,2,2,2,2,2,2,2,2,2,2,2,2,2,2,2,2,2,2,2,2,2,2,2,2,2,2,
2,2,2,2,2,2,2,2,2,2,2,2,2,2,2,2,2,2,2,2,2,2,2,2,2,2,2,2,2,2,2,2,2,2,2,2,
2,2,2,2,2,2,2,2,2,2,2,2,2,2,2,2,2,4),(-4.06006530123386,-3.99593991466936,
-3.99430387186957,-3.9933769546758,-3.99274336851389,-3.99212731294241,
-3.9915604833862,-3.99082368469873,-3.98922136288891,-3.9771514282463,-3.97510372004162,
-3.97461684272393,-3.97374861055896,-3.96784184438647,-3.95507851342347,
-3.92543386522881,-3.91690570768221,-3.90966437886953,-3.89489898230916,
-3.85256905838493,-3.83588564108468,-3.83381613980117,-3.83250748149031,
-3.83127738652211,-3.83036911203196,-3.82938495512678,-3.82796266426522,
-3.82395043408515,-3.82266924319363,-3.74316329855756,-3.72031522011211,
-3.69481234516365,-3.67906531570999,-3.67407311879412,-3.67093248230224,
-3.67020563918313,-3.66952348234982,-3.66896871779134,-3.66839881246668,
-3.66733142307643,-3.6637395159226,-3.60549518398974,-3.55950594500283,
-3.55189279906574,-3.51687800481418,-3.51100915382049,-3.50969145809721,
-3.50845483010772,-3.50754577578874,-3.50656467935198,-3.50485977975429,
-3.50004614720885,-3.42544685303681,-3.37701913855712,-3.35727362876052,
-3.34873949569421,-3.34740795648504,-3.34671162303826,-3.34615080630097,
-3.34558777111391,-3.34455452491803,-3.34124837980412,-3.28905379980431,
-3.22614436275744,-3.20153367704954,-3.18913095355246,-3.18682598251588,
-3.18559021312565,-3.18468124314283,-3.18369971007095,-3.18228699071446,
-3.178338898215,-3.11411446234708,-3.06060876373378,-3.03538624870023,-3.0259492755416,
-3.02458443852319,-3.02388107681627,-3.02337298006682,-3.02282691301624,
-3.02187801821909,-3.01920017826794,-2.97745115374412,-2.91086901244872,
-2.87166941637895,-2.86539241627176,-2.86355689715973,-2.86243762648458,
-2.86142708543733,-2.86013658978368,-2.85750224874746,-2.84138979380937,
-2.83808653633522,-2.81844691435209,-2.75778430521744,-2.70557692191206,
-2.70241421602068,-2.70144053860748,-2.7008239226418,-2.70025717708969,
-2.69952130947825,-2.6979242304867,-2.69214944809879),.UNSPECIFIED.);
#136=B_SPLINE_CURVE_WITH_KNOTS('',3,(#23224,#23225,#23226,#23227,#23228,
#23229,#23230,#23231,#23232,#23233,#23234,#23235,#23236,#23237,#23238,#23239,
#23240,#23241,#23242,#23243,#23244,#23245,#23246,#23247,#23248,#23249,#23250,
#23251,#23252,#23253,#23254,#23255,#23256,#23257,#23258,#23259,#23260,#23261,
#23262,#23263,#23264,#23265,#23266,#23267,#23268,#23269,#23270,#23271,#23272,
#23273,#23274,#23275,#23276,#23277,#23278,#23279,#23280,#23281,#23282,#23283,
#23284,#23285,#23286,#23287,#23288,#23289,#23290,#23291,#23292,#23293,#23294,
#23295,#23296,#23297,#23298,#23299,#23300,#23301,#23302,#23303,#23304,#23305,
#23306,#23307,#23308,#23309,#23310,#23311,#23312,#23313,#23314,#23315,#23316,
#23317,#23318,#23319,#23320,#23321,#23322,#23323,#23324,#23325,#23326,#23327,
#23328,#23329,#23330,#23331,#23332,#23333,#23334,#23335,#23336,#23337,#23338,
#23339,#23340,#23341,#23342,#23343,#23344,#23345,#23346,#23347,#23348,#23349,
#23350,#23351,#23352,#23353,#23354,#23355,#23356,#23357,#23358,#23359,#23360,
#23361,#23362,#23363,#23364,#23365,#23366,#23367,#23368,#23369,#23370,#23371,
#23372,#23373,#23374,#23375,#23376,#23377,#23378,#23379,#23380,#23381,#23382,
#23383,#23384,#23385,#23386,#23387,#23388,#23389,#23390,#23391,#23392,#23393,
#23394,#23395,#23396,#23397,#23398,#23399,#23400,#23401,#23402,#23403,#23404,
#23405,#23406,#23407,#23408,#23409,#23410,#23411,#23412,#23413,#23414,#23415,
#23416,#23417,#23418,#23419,#23420,#23421,#23422,#23423,#23424,#23425,#23426,
#23427,#23428,#23429,#23430,#23431,#23432,#23433,#23434,#23435,#23436,#23437),
 .UNSPECIFIED.,.F.,.F.,(4,2,2,2,2,2,2,2,2,2,2,2,2,2,2,2,2,2,2,2,2,2,2,2,
2,2,2,2,2,2,2,2,2,2,2,2,2,2,2,2,2,2,2,2,2,2,2,2,2,2,2,2,2,2,2,2,2,2,2,2,
2,2,2,2,2,2,2,2,2,2,2,2,2,2,2,2,2,2,2,2,2,2,2,2,2,2,2,2,2,2,2,2,2,2,2,2,
2,2,2,2,2,2,2,2,2,2,4),(-1.37024023670309,-1.36885167238846,-1.33918962176659,
-1.33638108529293,-1.33502146057737,-1.3340544383004,-1.33305966031228,
-1.33177427202646,-1.3303641635137,-1.3280530028917,-1.32344559768138,-1.27628892863603,
-1.17911015497803,-1.17434917215125,-1.17326514267846,-1.1725643668986,
-1.17200309625918,-1.17135908291938,-1.17024336810341,-1.16562014005557,
-1.12657943799402,-1.02060934691787,-1.0140511329824,-1.01212151688076,
-1.01098112950292,-1.00998834902539,-1.00876456961566,-1.00642464706627,
-1.00347844038503,-0.997080642333151,-0.977435942618436,-0.927270753068591,
-0.886221429308439,-0.873693875777526,-0.867040205987696,-0.852105177954858,
-0.850427825445548,-0.849733316503579,-0.849159091260957,-0.84856913663225,
-0.847696981178548,-0.84533302716629,-0.787568498767643,-0.711474735972392,
-0.708321437405196,-0.692358461587232,-0.689731838698381,-0.688442875037336,
-0.687432500458816,-0.686334866794259,-0.684559153910981,-0.682455766303399,
-0.678403807561126,-0.668585031234653,-0.635050126915235,-0.532622904138751,
-0.531763392050551,-0.528038059754367,-0.526955284617288,-0.526382182847298,
-0.525878091846954,-0.525221580052896,-0.524049310450672,-0.518660244991595,
-0.508455649384645,-0.479514883812686,-0.470545709694636,-0.463050638639729,
-0.456597765866444,-0.450942365951417,-0.399256529645745,-0.370093641699301,
-0.367296592158299,-0.365939646120318,-0.364973218567505,-0.36400101406144,
-0.363017270793776,-0.360863175342903,-0.350312791231922,-0.330173896685716,
-0.309272020054442,-0.215129716287474,-0.213784119410423,-0.212208998046509,
-0.209582714806551,-0.209190457159851,-0.205121174966834,-0.204014264593347,
-0.203365635890036,-0.20280470427498,-0.202109923132213,-0.200759446328427,
-0.191852023116426,-0.170477733469139,-0.0836889393789725,-0.0780371380388596,
-0.0704778394857391,-0.0674444858369929,-0.046585140615017,-0.0440273660684284,
-0.0427303186481333,-0.0417796549327277,-0.0408180730834325,-0.0398220982889161,
-0.0385198626423396,-0.0364660321025074,-0.000960727209027502),
 .UNSPECIFIED.);
#137=B_SPLINE_CURVE_WITH_KNOTS('',3,(#23438,#23439,#23440,#23441,#23442,
#23443,#23444,#23445,#23446,#23447,#23448,#23449,#23450,#23451,#23452,#23453,
#23454,#23455,#23456,#23457,#23458,#23459,#23460,#23461,#23462,#23463,#23464,
#23465,#23466,#23467,#23468,#23469,#23470,#23471,#23472,#23473,#23474,#23475,
#23476,#23477,#23478,#23479,#23480,#23481,#23482,#23483,#23484,#23485,#23486,
#23487,#23488,#23489,#23490,#23491,#23492,#23493,#23494,#23495,#23496,#23497,
#23498,#23499,#23500,#23501,#23502,#23503,#23504,#23505,#23506,#23507,#23508,
#23509,#23510,#23511,#23512,#23513,#23514,#23515,#23516,#23517,#23518,#23519,
#23520,#23521,#23522,#23523,#23524,#23525,#23526,#23527,#23528,#23529),
 .UNSPECIFIED.,.F.,.F.,(4,2,2,2,2,2,2,2,2,2,2,2,2,2,2,2,2,2,2,2,2,2,2,2,
2,2,2,2,2,2,2,2,2,2,2,2,2,2,2,2,2,2,2,2,2,4),(-4.06085215427619,-3.96661118569572,
-3.94505040122191,-3.94164875373561,-3.94064622429485,-3.94002742739455,
-3.93946101715168,-3.93872877242596,-3.93715189450824,-3.92576039072985,
-3.92461321105174,-3.881110884479,-3.82992662093111,-3.81419971635615,-3.79323860015488,
-3.7823613668101,-3.78018703772864,-3.779201058095,-3.77823068752792,-3.77726700444125,
-3.77592080727929,-3.77316795992076,-3.74580419666669,-3.70680899915316,
-3.67860169565895,-3.6237167615223,-3.61893501839857,-3.61780662874518,
-3.61715969714152,-3.6165985625392,-3.61590139435704,-3.61482927084666,
-3.61003056804398,-3.51717975406838,-3.47935504024415,-3.46641744885073,
-3.46144162184887,-3.45899543550808,-3.45698860284708,-3.45583645997346,
-3.45492707099901,-3.45390846893587,-3.45201849694706,-3.44580458898125,
-3.4444266686727,-3.39977149278874),.UNSPECIFIED.);
#138=B_SPLINE_CURVE_WITH_KNOTS('',3,(#23530,#23531,#23532,#23533,#23534,
#23535,#23536,#23537,#23538,#23539,#23540,#23541,#23542,#23543,#23544,#23545,
#23546,#23547,#23548,#23549,#23550,#23551,#23552,#23553,#23554,#23555,#23556,
#23557,#23558,#23559,#23560,#23561,#23562,#23563,#23564,#23565,#23566,#23567,
#23568,#23569,#23570,#23571,#23572,#23573,#23574,#23575,#23576,#23577,#23578,
#23579,#23580,#23581,#23582,#23583,#23584,#23585,#23586,#23587,#23588,#23589,
#23590,#23591,#23592,#23593,#23594,#23595,#23596,#23597,#23598,#23599,#23600,
#23601,#23602,#23603,#23604,#23605,#23606,#23607,#23608,#23609,#23610,#23611,
#23612,#23613,#23614,#23615,#23616,#23617,#23618,#23619,#23620,#23621,#23622,
#23623,#23624,#23625,#23626,#23627,#23628,#23629,#23630,#23631,#23632,#23633,
#23634,#23635,#23636,#23637,#23638,#23639,#23640,#23641,#23642,#23643,#23644,
#23645,#23646,#23647,#23648,#23649,#23650,#23651,#23652,#23653,#23654,#23655,
#23656,#23657,#23658,#23659,#23660,#23661,#23662,#23663,#23664,#23665,#23666,
#23667,#23668,#23669,#23670,#23671,#23672,#23673,#23674,#23675,#23676,#23677,
#23678,#23679,#23680,#23681,#23682,#23683,#23684,#23685,#23686,#23687,#23688,
#23689,#23690,#23691,#23692,#23693,#23694,#23695,#23696,#23697,#23698,#23699,
#23700,#23701,#23702,#23703,#23704,#23705,#23706,#23707,#23708,#23709,#23710,
#23711,#23712,#23713,#23714,#23715,#23716,#23717,#23718,#23719,#23720,#23721,
#23722,#23723,#23724,#23725,#23726,#23727,#23728,#23729,#23730,#23731,#23732,
#23733,#23734,#23735,#23736,#23737,#23738,#23739,#23740,#23741,#23742,#23743,
#23744,#23745,#23746,#23747,#23748,#23749,#23750,#23751,#23752,#23753,#23754,
#23755,#23756,#23757,#23758,#23759,#23760,#23761,#23762,#23763,#23764,#23765,
#23766,#23767,#23768,#23769,#23770,#23771,#23772,#23773,#23774,#23775,#23776,
#23777,#23778,#23779,#23780,#23781,#23782,#23783,#23784,#23785,#23786,#23787,
#23788,#23789,#23790,#23791,#23792,#23793,#23794,#23795,#23796,#23797,#23798,
#23799,#23800,#23801,#23802,#23803,#23804,#23805,#23806,#23807,#23808,#23809,
#23810,#23811,#23812,#23813,#23814,#23815,#23816,#23817,#23818,#23819,#23820,
#23821,#23822,#23823),.UNSPECIFIED.,.F.,.F.,(4,2,2,2,2,2,2,2,2,2,2,2,2,
2,2,2,2,2,2,2,2,2,2,2,2,2,2,2,2,2,2,2,2,2,2,2,2,2,2,2,2,2,2,2,2,2,2,2,2,
2,2,2,2,2,2,2,2,2,2,2,2,2,2,2,2,2,2,2,2,2,2,2,2,2,2,2,2,2,2,2,2,2,2,2,2,
2,2,2,2,2,2,2,2,2,2,2,2,2,2,2,2,2,2,2,2,2,2,2,2,2,2,2,2,2,2,2,2,2,2,2,2,
2,2,2,2,2,2,2,2,2,2,2,2,2,2,2,2,2,2,2,2,2,2,2,2,2,4),(-2.69214944809879,
-2.68599658157334,-2.67164723329084,-2.65509714678797,-2.62302784577316,
-2.57819043594351,-2.55508852161463,-2.54343864667162,-2.54116300941676,
-2.53993686756713,-2.5389320190232,-2.5379208437841,-2.536066545589,-2.53014312996771,
-2.52835564554769,-2.52586301442259,-2.52446243206274,-2.52344138183711,
-2.52302472034248,-2.43489025317887,-2.38268558995137,-2.37952643746347,
-2.37855319968038,-2.37793656392635,-2.37736971714667,-2.37663360430841,
-2.37503554803698,-2.36308644350046,-2.36087945763509,-2.36049387330735,
-2.32702594666857,-2.30391962788928,-2.25052638850229,-2.23391651921538,
-2.22054467523627,-2.21823333148908,-2.21700936486661,-2.21600450708303,
-2.21499180532168,-2.21313034550096,-2.20715001965889,-2.10547356610973,
-2.08147726364995,-2.05996426419309,-2.05656741720115,-2.05556550413876,
-2.05494690653567,-2.0543805526434,-2.05364820869943,-2.0520704543158,-2.04065253546098,
-2.03952931049749,-2.03914938575955,-2.03631552362315,-2.0352630986408,
-2.03410163508923,-2.03130204021125,-2.00261033368606,-1.93396926714356,
-1.89894135520261,-1.89575631506156,-1.89446685351192,-1.89351816229621,
-1.89249242633389,-1.89110197661171,-1.88794272980815,-1.84713509200039,
-1.78939754286815,-1.74366517471266,-1.74246691729439,-1.74094611924842,
-1.73823781239039,-1.73391081223565,-1.7327781881313,-1.73212361544069,
-1.73156317725347,-1.73087607758004,-1.72956203351273,-1.72155551617218,
-1.71106989723019,-1.68755219755491,-1.57975761495329,-1.57361537612516,
-1.57173429009616,-1.57071765644577,-1.5697131311958,-1.56852014575054,
-1.56632053594682,-1.5635903138388,-1.50786062815447,-1.43010552010928,
-1.42871949470108,-1.42786781760932,-1.42684354708768,-1.41167903906937,
-1.41014209882668,-1.4093919523983,-1.40885551810102,-1.40834350163467,
-1.40761425417709,-1.40609313506553,-1.39049976505409,-1.3732305669527,
-1.25634517856986,-1.25038514061555,-1.24852638739162,-1.24751435322766,
-1.24650964645382,-1.24530990826964,-1.24308525745988,-1.24031256631594,
-1.17480270146845,-1.09798392690746,-1.09545748565058,-1.08800232770736,
-1.08675514599148,-1.08601284293542,-1.08544506075773,-1.08483132089616,
-1.08385070524348,-1.08064490803196,-1.03238043366701,-0.940483867016562,
-0.939790740022388,-0.938376955615533,-0.934889008839562,-0.93347217413441,
-0.927396635145153,-0.92552378011985,-0.924508907565407,-0.923504432870422,
-0.922309172581548,-0.92010157690178,-0.917357183811406,-0.911542850101569,
-0.895585524246291,-0.878811346126955,-0.775268882508638,-0.765126928909412,
-0.763603068084822,-0.762873291272256,-0.762309023457881,-0.761682957156301,
-0.76064752433179,-0.756925759970814,-0.668028289659514,-0.661829640843947),
 .UNSPECIFIED.);
#139=B_SPLINE_CURVE_WITH_KNOTS('',3,(#23828,#23829,#23830,#23831,#23832,
#23833,#23834,#23835,#23836,#23837,#23838,#23839,#23840,#23841,#23842,#23843,
#23844,#23845,#23846,#23847,#23848,#23849,#23850,#23851,#23852,#23853,#23854,
#23855,#23856,#23857,#23858,#23859,#23860,#23861,#23862,#23863,#23864,#23865,
#23866,#23867,#23868,#23869,#23870,#23871,#23872,#23873,#23874,#23875,#23876,
#23877,#23878,#23879,#23880,#23881,#23882,#23883,#23884,#23885,#23886,#23887,
#23888,#23889,#23890,#23891,#23892,#23893,#23894,#23895,#23896,#23897,#23898,
#23899,#23900,#23901,#23902,#23903,#23904,#23905,#23906,#23907,#23908,#23909,
#23910,#23911,#23912,#23913,#23914,#23915,#23916,#23917,#23918,#23919,#23920,
#23921,#23922,#23923,#23924,#23925,#23926,#23927,#23928,#23929,#23930,#23931,
#23932,#23933,#23934,#23935,#23936,#23937,#23938,#23939,#23940,#23941,#23942,
#23943,#23944,#23945,#23946,#23947,#23948,#23949,#23950,#23951,#23952,#23953,
#23954,#23955,#23956,#23957,#23958,#23959,#23960,#23961,#23962,#23963,#23964,
#23965,#23966,#23967,#23968,#23969,#23970,#23971,#23972,#23973,#23974,#23975,
#23976,#23977,#23978,#23979,#23980,#23981,#23982,#23983,#23984,#23985,#23986,
#23987,#23988,#23989,#23990,#23991,#23992,#23993,#23994,#23995,#23996,#23997,
#23998,#23999,#24000,#24001,#24002,#24003,#24004,#24005,#24006,#24007,#24008,
#24009,#24010,#24011,#24012,#24013,#24014,#24015,#24016,#24017,#24018,#24019,
#24020,#24021,#24022,#24023,#24024,#24025,#24026,#24027,#24028,#24029,#24030,
#24031,#24032,#24033,#24034,#24035,#24036,#24037,#24038,#24039,#24040,#24041,
#24042,#24043,#24044,#24045,#24046,#24047,#24048,#24049,#24050,#24051,#24052,
#24053,#24054,#24055,#24056,#24057,#24058,#24059,#24060,#24061,#24062,#24063,
#24064,#24065,#24066,#24067,#24068,#24069,#24070,#24071,#24072,#24073,#24074,
#24075,#24076,#24077,#24078,#24079,#24080,#24081,#24082,#24083,#24084,#24085,
#24086,#24087,#24088,#24089,#24090,#24091,#24092,#24093,#24094,#24095,#24096,
#24097,#24098,#24099,#24100,#24101,#24102,#24103),.UNSPECIFIED.,.F.,.F.,
(4,2,2,2,2,2,2,2,2,2,2,2,2,2,2,2,2,2,2,2,2,2,2,2,2,2,2,2,2,2,2,2,2,2,2,
2,2,2,2,2,2,2,2,2,2,2,2,2,2,2,2,2,2,2,2,2,2,2,2,2,2,2,2,2,2,2,2,2,2,2,2,
2,2,2,2,2,2,2,2,2,2,2,2,2,2,2,2,2,2,2,2,2,2,2,2,2,2,2,2,2,2,2,2,2,2,2,2,
2,2,2,2,2,2,2,2,2,2,2,2,2,2,2,2,2,2,2,2,2,2,2,2,2,2,2,2,2,2,4),(-3.40024812751307,
-3.37021916983221,-3.32505019996527,-3.29549526830059,-3.27634593457388,
-3.27382180366001,-3.27255376852381,-3.27164074029554,-3.27067323796775,
-3.26931121453177,-3.26649211847317,-3.25891046188894,-3.25709606806721,
-3.25503353230855,-3.25458896974936,-3.25267312412952,-3.24984890603887,
-3.24865288393459,-3.24708911667439,-3.23994482018547,-3.15121175955301,
-3.12608702916532,-3.1172488270471,-3.1140601592006,-3.11255553194174,-3.11168174036197,
-3.11090401195614,-3.11033974796076,-3.10981351113754,-3.10910193962852,
-3.10771729758783,-3.09724890235979,-3.03503339651356,-2.98935503809951,
-2.95761659599998,-2.9520834524647,-2.9503486946786,-2.94925202831025,-2.9482353774998,
-2.94692141582952,-2.9440941679695,-2.92357931905998,-2.91988743292052,
-2.84174555527698,-2.79252922098714,-2.79036968852979,-2.78923835395744,
-2.78851916476895,-2.7878519530383,-2.7873038773602,-2.78673510546515,-2.78567331828929,
-2.78212950731031,-2.78092411161475,-2.7784739014207,-2.77692093140824,
-2.77549266362795,-2.68198167080393,-2.64592939769034,-2.63034070536811,
-2.62793597241531,-2.62669255959398,-2.62568678346382,-2.62468565083225,
-2.62288053256954,-2.61734151151723,-2.52610469716422,-2.46866414594993,
-2.4669309876275,-2.46596527014986,-2.46531553269414,-2.46469783232534,
-2.46417692554638,-2.46347710868523,-2.46239584831783,-2.45747895060558,
-2.36318259380599,-2.34220468439246,-2.32268794950534,-2.30730096877307,
-2.30490399878233,-2.30366218180784,-2.30265648912325,-2.30165444058315,
-2.29984489728978,-2.29427231313607,-2.17518737874915,-2.15286470772111,
-2.14372993825883,-2.14237127619577,-2.1416748952449,-2.14111398449238,
-2.14046685084458,-2.13936592841587,-2.13535293397075,-2.13488836811322,
-2.03154911500209,-1.98560467267569,-1.98222998666102,-1.98090832922995,
-1.97995145026512,-1.97893140643873,-1.97757380041888,-1.97459247319502,
-1.9168325927431,-1.83074030828404,-1.82084482997164,-1.81933216524787,
-1.81860461207888,-1.81804064490914,-1.81741342729343,-1.81637276606867,
-1.81259753465822,-1.72383023213061,-1.66332207640873,-1.65938351405851,
-1.65797215662046,-1.6569909468046,-1.65600096995921,-1.65475202895635,
-1.65339223458445,-1.65120127405137,-1.64691717922249,-1.6056349906904,
-1.55463124828268,-1.51653942581854,-1.51528751052423,-1.51211488756194,
-1.51021841535422,-1.49802245798605,-1.49643573940522,-1.4956904168319,
-1.49512215526703,-1.49450975473211,-1.49353510962024,-1.49038140500459,
-1.4382436320602,-1.37024023670309),.UNSPECIFIED.);
#140=B_SPLINE_CURVE_WITH_KNOTS('',3,(#24105,#24106,#24107,#24108,#24109,
#24110,#24111,#24112,#24113,#24114,#24115,#24116,#24117,#24118,#24119,#24120,
#24121,#24122,#24123,#24124,#24125,#24126,#24127,#24128,#24129,#24130,#24131,
#24132,#24133,#24134,#24135,#24136,#24137,#24138,#24139,#24140,#24141,#24142,
#24143,#24144,#24145,#24146,#24147,#24148,#24149,#24150,#24151,#24152,#24153,
#24154,#24155,#24156,#24157,#24158,#24159,#24160,#24161,#24162,#24163,#24164,
#24165,#24166,#24167,#24168,#24169,#24170,#24171,#24172,#24173,#24174,#24175,
#24176,#24177,#24178,#24179,#24180,#24181,#24182,#24183,#24184,#24185,#24186,
#24187,#24188,#24189,#24190,#24191,#24192,#24193,#24194,#24195,#24196),
 .UNSPECIFIED.,.F.,.F.,(4,2,2,2,2,2,2,2,2,2,2,2,2,2,2,2,2,2,2,2,2,2,2,2,
2,2,2,2,2,2,2,2,2,2,2,2,2,2,2,2,2,2,2,2,2,4),(-0.661829640843947,-0.612715495677179,
-0.609522028636577,-0.604119517181893,-0.602332136058833,-0.601334391212832,
-0.600339656054466,-0.599119487924847,-0.596806779067315,-0.593896446576099,
-0.587603514970783,-0.569857605629294,-0.535118957266086,-0.468698656885868,
-0.442776896139604,-0.44086781458186,-0.440126211952284,-0.439592078982841,
-0.439021836344277,-0.438251521035448,-0.43651283520404,-0.380557851560157,
-0.352976448378946,-0.317068882730308,-0.305814394758379,-0.303764843847665,
-0.283059322801507,-0.280223842026451,-0.278908057692136,-0.277890852002289,
-0.276949508423118,-0.275874397196253,-0.272880906583698,-0.245790281652857,
-0.226149685341142,-0.122939428242058,-0.122348526875143,-0.118428655112071,
-0.117337330991179,-0.116692336686235,-0.116131046265131,-0.115431322461575,
-0.114057065785592,-0.104489937707715,-0.0741047509759709,-0.000962458815746768),
 .UNSPECIFIED.);
#141=B_SPLINE_CURVE_WITH_KNOTS('',3,(#24197,#24198,#24199,#24200,#24201,
#24202,#24203,#24204,#24205,#24206,#24207,#24208,#24209,#24210,#24211,#24212,
#24213,#24214,#24215,#24216,#24217,#24218,#24219,#24220,#24221,#24222,#24223,
#24224,#24225,#24226,#24227,#24228,#24229,#24230,#24231,#24232,#24233,#24234,
#24235,#24236,#24237,#24238,#24239,#24240,#24241,#24242,#24243,#24244,#24245,
#24246,#24247,#24248,#24249,#24250,#24251,#24252,#24253,#24254,#24255,#24256,
#24257,#24258,#24259,#24260,#24261,#24262,#24263,#24264,#24265,#24266,#24267,
#24268,#24269,#24270,#24271,#24272,#24273,#24274,#24275,#24276,#24277,#24278,
#24279,#24280,#24281,#24282,#24283,#24284,#24285,#24286,#24287,#24288,#24289,
#24290,#24291,#24292,#24293,#24294,#24295,#24296,#24297,#24298,#24299,#24300,
#24301,#24302,#24303,#24304,#24305,#24306,#24307,#24308,#24309,#24310,#24311,
#24312,#24313,#24314,#24315,#24316,#24317,#24318,#24319,#24320,#24321,#24322,
#24323,#24324,#24325,#24326,#24327,#24328,#24329,#24330,#24331,#24332,#24333,
#24334,#24335,#24336,#24337,#24338,#24339,#24340,#24341,#24342,#24343,#24344,
#24345,#24346,#24347,#24348,#24349,#24350,#24351,#24352,#24353,#24354,#24355,
#24356,#24357,#24358,#24359,#24360,#24361,#24362,#24363,#24364,#24365,#24366,
#24367,#24368,#24369,#24370,#24371,#24372,#24373,#24374,#24375,#24376,#24377,
#24378,#24379,#24380,#24381,#24382,#24383,#24384,#24385,#24386,#24387,#24388),
 .UNSPECIFIED.,.F.,.F.,(4,2,2,2,2,2,2,2,2,2,2,2,2,2,2,2,2,2,2,2,2,2,2,2,
2,2,2,2,2,2,2,2,2,2,2,2,2,2,2,2,2,2,2,2,2,2,2,2,2,2,2,2,2,2,2,2,2,2,2,2,
2,2,2,2,2,2,2,2,2,2,2,2,2,2,2,2,2,2,2,2,2,2,2,2,2,2,2,2,2,2,2,2,2,2,2,4),
(-4.06434128415624,-4.0235371652522,-4.02147772617206,-4.0201729447231,
-4.01917586288143,-4.0182144098793,-4.01726414507108,-4.01596962822361,
-4.01275735295853,-3.97648937458706,-3.97075261283844,-3.88496254663774,
-3.86338044728011,-3.85870753133827,-3.8575873851824,-3.85694213702144,
-3.85638060100868,-3.85568053937851,-3.85459955003203,-3.84982856687511,
-3.75265760584019,-3.72967907984624,-3.70953059977957,-3.69897396417434,
-3.69681873467038,-3.69583448739759,-3.6948617922275,-3.69389487008252,
-3.692537242744,-3.68973882301341,-3.66056268890683,-3.62783061094541,-3.53916688352163,
-3.53530040134573,-3.53425040860409,-3.53362080452173,-3.53311572485325,
-3.53242104173421,-3.53135736474281,-3.52666512443278,-3.52470534154804,
-3.52268180933885,-3.52177204832499,-3.44482679401666,-3.40988559860286,
-3.38736966622947,-3.3798251942801,-3.37649407866723,-3.37390737872275,
-3.37263117305147,-3.37165782117644,-3.37069000434681,-3.36932931693261,
-3.36651875320827,-3.33684487209056,-3.24939477818891,-3.23528733525964,
-3.21987123318882,-3.2125110214233,-3.21122568242145,-3.21054439387533,
-3.20998911961032,-3.2094176112918,-3.2083440938561,-3.20470484662442,-3.20370616047174,
-3.12780535613794,-3.06003893212251,-3.05485716287473,-3.05233629789206,
-3.05027706748941,-3.04911388927411,-3.04820856951106,-3.04719831149225,
-3.04535136529604,-3.03949502681541,-2.94860271366907,-2.89370248792994,
-2.88891342821127,-2.88778405825408,-2.88713669242884,-2.88657525872605,
-2.88587781754436,-2.88480545482924,-2.88000857223905,-2.79325492436669,
-2.75746353606728,-2.73286597244475,-2.72971425450522,-2.72724047666725,
-2.72598815011584,-2.72500628237635,-2.72402647278784,-2.7226221422139,
-2.71873495995085,-2.69413699669498),.UNSPECIFIED.);
#142=B_SPLINE_CURVE_WITH_KNOTS('',3,(#24394,#24395,#24396,#24397,#24398,
#24399,#24400,#24401,#24402,#24403,#24404,#24405,#24406,#24407,#24408,#24409,
#24410,#24411,#24412,#24413,#24414,#24415,#24416,#24417,#24418,#24419,#24420,
#24421,#24422,#24423,#24424,#24425,#24426,#24427,#24428,#24429,#24430,#24431,
#24432,#24433,#24434,#24435,#24436,#24437,#24438,#24439,#24440,#24441,#24442,
#24443,#24444,#24445,#24446,#24447,#24448,#24449,#24450,#24451,#24452,#24453,
#24454,#24455,#24456,#24457,#24458,#24459,#24460,#24461,#24462,#24463,#24464,
#24465,#24466,#24467,#24468,#24469,#24470,#24471,#24472,#24473,#24474,#24475,
#24476,#24477,#24478,#24479,#24480,#24481,#24482,#24483,#24484,#24485,#24486,
#24487,#24488,#24489,#24490,#24491,#24492,#24493,#24494,#24495,#24496,#24497,
#24498,#24499,#24500,#24501,#24502,#24503,#24504,#24505,#24506,#24507,#24508,
#24509,#24510,#24511,#24512,#24513,#24514,#24515,#24516,#24517,#24518,#24519,
#24520,#24521,#24522,#24523,#24524,#24525,#24526,#24527,#24528,#24529,#24530,
#24531,#24532,#24533,#24534,#24535,#24536,#24537,#24538,#24539,#24540,#24541,
#24542,#24543,#24544,#24545,#24546,#24547,#24548,#24549,#24550,#24551,#24552,
#24553,#24554,#24555,#24556,#24557,#24558,#24559,#24560,#24561,#24562,#24563,
#24564,#24565,#24566,#24567,#24568,#24569,#24570,#24571,#24572,#24573,#24574,
#24575,#24576,#24577,#24578,#24579,#24580,#24581,#24582,#24583,#24584,#24585,
#24586,#24587,#24588,#24589,#24590,#24591,#24592,#24593,#24594,#24595,#24596,
#24597,#24598,#24599,#24600,#24601,#24602,#24603,#24604,#24605,#24606,#24607,
#24608,#24609,#24610,#24611,#24612,#24613),.UNSPECIFIED.,.F.,.F.,(4,2,2,
2,2,2,2,2,2,2,2,2,2,2,2,2,2,2,2,2,2,2,2,2,2,2,2,2,2,2,2,2,2,2,2,2,2,2,2,
2,2,2,2,2,2,2,2,2,2,2,2,2,2,2,2,2,2,2,2,2,2,2,2,2,2,2,2,2,2,2,2,2,2,2,2,
2,2,2,2,2,2,2,2,2,2,2,2,2,2,2,2,2,2,2,2,2,2,2,2,2,2,2,2,2,2,2,2,2,2,4),
(-1.37029241472368,-1.34852183284429,-1.32293951683633,-1.32190342284898,
-1.32024765934368,-1.31568780184551,-1.31290518130904,-1.31194094441941,
-1.31139159029801,-1.31083876931964,-1.31013340499299,-1.30936095701649,
-1.30810273240195,-1.30560447221522,-1.21681269106214,-1.15605542670002,
-1.15226951861025,-1.15088107844413,-1.14990591692488,-1.1489945323053,
-1.14774264003818,-1.14529965598708,-1.12871102886337,-1.08886453232611,
-1.02576386691761,-0.991713875009911,-0.989560785485333,-0.988780806232009,
-0.988236141085219,-0.987681891714349,-0.987015362115503,-0.986251110731604,
-0.985012511128443,-0.982567395750004,-0.976411545159215,-0.953528875623381,
-0.835360269432715,-0.829606039922391,-0.827772662119502,-0.826765541908211,
-0.825760001368634,-0.824526100042465,-0.822168279555364,-0.807758621240536,
-0.776358983332107,-0.763557029442697,-0.752734994118637,-0.671336471262862,
-0.670352264020728,-0.666707046606074,-0.665633237725656,-0.665061881665321,
-0.664512611575234,-0.663901279564926,-0.663207842460111,-0.662138098892671,
-0.660139713329433,-0.655456388248882,-0.640646275202323,-0.627648913650835,
-0.512387104486719,-0.50642894179736,-0.504570223350185,-0.503558085194288,
-0.502553197247076,-0.50132834042526,-0.499012752832494,-0.4855490784644,
-0.469710938186427,-0.437836036271502,-0.4285707453202,-0.420841685803779,
-0.414214832438632,-0.408426633596053,-0.390147630057129,-0.373870415288781,
-0.345056568661516,-0.343102105789311,-0.342353047923185,-0.341816943064706,
-0.341278234841024,-0.340548126230012,-0.339006781639323,-0.336978302727952,
-0.332198752012145,-0.317035413522846,-0.303946243446485,-0.231170726504234,
-0.214521106857462,-0.185638263948231,-0.182579033906513,-0.181323329014338,
-0.180383230149897,-0.179350806895634,-0.177922239428873,-0.1745456798893,
-0.136176385911942,-0.037752960116968,-0.0342634325543829,-0.0338225101078654,
-0.0321021075804736,-0.0213809779737077,-0.0199861799137145,-0.019271842407949,
-0.0187447579747701,-0.0182119709174758,-0.0176494579022497,-0.0169022101124036,
-0.0157041435510641,-0.00096080709203007),.UNSPECIFIED.);
#143=B_SPLINE_CURVE_WITH_KNOTS('',3,(#24614,#24615,#24616,#24617,#24618,
#24619,#24620,#24621,#24622,#24623,#24624,#24625,#24626,#24627,#24628,#24629,
#24630,#24631,#24632,#24633,#24634,#24635,#24636,#24637,#24638,#24639,#24640,
#24641,#24642,#24643,#24644,#24645,#24646,#24647,#24648,#24649,#24650,#24651,
#24652,#24653,#24654,#24655,#24656,#24657,#24658,#24659,#24660,#24661,#24662,
#24663,#24664,#24665,#24666,#24667,#24668,#24669,#24670,#24671,#24672,#24673,
#24674,#24675,#24676,#24677,#24678,#24679,#24680,#24681,#24682,#24683,#24684,
#24685,#24686,#24687,#24688,#24689,#24690,#24691,#24692,#24693,#24694,#24695,
#24696,#24697,#24698,#24699,#24700,#24701,#24702,#24703,#24704,#24705),
 .UNSPECIFIED.,.F.,.F.,(4,2,2,2,2,2,2,2,2,2,2,2,2,2,2,2,2,2,2,2,2,2,2,2,
2,2,2,2,2,2,2,2,2,2,2,2,2,2,2,2,2,2,2,2,2,4),(-4.06134520834936,-3.96837948446271,
-3.9364107850448,-3.92187733576561,-3.91951624335496,-3.91828247988687,
-3.91727798879559,-3.91627270178459,-3.91444486983007,-3.90872447596486,
-3.79049585550717,-3.76979665848526,-3.76230356525439,-3.7594789094282,
-3.75810271474695,-3.75728164958469,-3.75654128918839,-3.75598402753498,
-3.75544818963429,-3.75469930248761,-3.75274412429328,-3.72382050698897,
-3.71026053601232,-3.68639899843738,-3.63442545529601,-3.61208571490417,
-3.59892025391591,-3.59661980038905,-3.59539866077819,-3.59439459939926,
-3.59338140594459,-3.59151530522612,-3.58549063863911,-3.4693180023132,
-3.44878262753612,-3.44002310160713,-3.43685535994991,-3.43535805703827,
-3.43448728028723,-3.43371128428702,-3.43314755786976,-3.43262086474612,
-3.43190732131699,-3.43051485449375,-3.4198407493259,-3.40024812751307),
 .UNSPECIFIED.);
#144=B_SPLINE_CURVE_WITH_KNOTS('',3,(#24706,#24707,#24708,#24709,#24710,
#24711,#24712,#24713,#24714,#24715,#24716,#24717,#24718,#24719,#24720,#24721,
#24722,#24723,#24724,#24725,#24726,#24727,#24728,#24729,#24730,#24731,#24732,
#24733,#24734,#24735,#24736,#24737,#24738,#24739,#24740,#24741,#24742,#24743,
#24744,#24745,#24746,#24747,#24748,#24749,#24750,#24751,#24752,#24753,#24754,
#24755,#24756,#24757,#24758,#24759,#24760,#24761,#24762,#24763,#24764,#24765,
#24766,#24767,#24768,#24769,#24770,#24771,#24772,#24773,#24774,#24775,#24776,
#24777,#24778,#24779,#24780,#24781,#24782,#24783,#24784,#24785,#24786,#24787,
#24788,#24789,#24790,#24791,#24792,#24793,#24794,#24795,#24796,#24797,#24798,
#24799,#24800,#24801,#24802,#24803,#24804,#24805,#24806,#24807,#24808,#24809,
#24810,#24811,#24812,#24813,#24814,#24815,#24816,#24817,#24818,#24819,#24820,
#24821,#24822,#24823,#24824,#24825,#24826,#24827,#24828,#24829,#24830,#24831,
#24832,#24833,#24834,#24835,#24836,#24837,#24838,#24839,#24840,#24841,#24842,
#24843,#24844,#24845,#24846,#24847,#24848,#24849,#24850,#24851,#24852,#24853,
#24854,#24855,#24856,#24857,#24858,#24859,#24860,#24861,#24862,#24863,#24864,
#24865,#24866,#24867,#24868,#24869,#24870,#24871,#24872,#24873,#24874,#24875,
#24876,#24877,#24878,#24879,#24880,#24881,#24882,#24883,#24884,#24885,#24886,
#24887,#24888,#24889,#24890,#24891,#24892,#24893,#24894,#24895,#24896,#24897,
#24898,#24899,#24900,#24901,#24902,#24903,#24904,#24905,#24906,#24907,#24908,
#24909,#24910,#24911,#24912,#24913,#24914,#24915,#24916,#24917,#24918,#24919,
#24920,#24921,#24922,#24923,#24924,#24925,#24926,#24927,#24928,#24929,#24930,
#24931,#24932,#24933,#24934,#24935,#24936,#24937,#24938,#24939,#24940,#24941,
#24942,#24943,#24944,#24945,#24946,#24947,#24948,#24949,#24950,#24951,#24952,
#24953,#24954,#24955,#24956,#24957,#24958,#24959,#24960,#24961,#24962,#24963),
 .UNSPECIFIED.,.F.,.F.,(4,2,2,2,2,2,2,2,2,2,2,2,2,2,2,2,2,2,2,2,2,2,2,2,
2,2,2,2,2,2,2,2,2,2,2,2,2,2,2,2,2,2,2,2,2,2,2,2,2,2,2,2,2,2,2,2,2,2,2,2,
2,2,2,2,2,2,2,2,2,2,2,2,2,2,2,2,2,2,2,2,2,2,2,2,2,2,2,2,2,2,2,2,2,2,2,2,
2,2,2,2,2,2,2,2,2,2,2,2,2,2,2,2,2,2,2,2,2,2,2,2,2,2,2,2,2,2,2,2,4),(-2.69413699669498,
-2.65797776204501,-2.56931048756278,-2.56543521196518,-2.5643842166337,
-2.56375429385175,-2.56324910870668,-2.56255451391301,-2.56149139705641,
-2.55680783167898,-2.46801353521712,-2.40813218440491,-2.40561640634868,
-2.4041207825857,-2.40277371487563,-2.40176817375987,-2.40081836411621,
-2.39952637163187,-2.39632998847909,-2.36084875337876,-2.33231101723818,
-2.31117440016871,-2.26557826022934,-2.25003376666667,-2.24260966383499,
-2.24132123523769,-2.24063926694692,-2.24008393596067,-2.23951281047455,
-2.23844129049829,-2.2348197614001,-2.17592014514316,-2.12654974716623,
-2.08424067310959,-2.08106316752288,-2.07966882575442,-2.07864183293595,
-2.07769311971313,-2.07640537097843,-2.07388564174684,-2.05412065468879,
-2.04780444377394,-2.03225337437467,-1.9834337411955,-1.93172019386119,
-1.91994713227829,-1.91851341140619,-1.91778884323659,-1.91725887431838,
-1.91668497125008,-1.91589575837881,-1.91405334140259,-1.86842143808323,
-1.76504935290494,-1.75883181450551,-1.75694085555721,-1.75592174891191,
-1.75492619560002,-1.75371468991757,-1.75146410969886,-1.73934326474796,
-1.71542218993718,-1.66983139631379,-1.59983232496637,-1.59583271754432,
-1.59473265491292,-1.59408541648728,-1.59353514947438,-1.59285742383072,
-1.59212330276364,-1.59095696848503,-1.58870581325269,-1.56718073530101,
-1.54317890354222,-1.50380677742589,-1.438992685355,-1.43503797408942,-1.43362346308503,
-1.43264085978811,-1.4317310357451,-1.4304943134161,-1.42812538488915,-1.41347923261291,
-1.38108711810398,-1.32996150914465,-1.2759824527835,-1.27258227925585,
-1.2715369193024,-1.27097109186211,-1.27042111694214,-1.26974708236269,
-1.26901862253513,-1.2678658018507,-1.26565047210073,-1.24470459842785,
-1.22298393026765,-1.11866745130031,-1.11241699140463,-1.11052222025656,
-1.10950239922201,-1.10850697640287,-1.10729680437512,-1.10505214411997,
-1.09304078830953,-1.06935809579366,-1.02396750534711,-0.964205306191557,
-0.950353234860537,-0.948852988011463,-0.948111730139071,-0.947577462289241,
-0.947018098770191,-0.946289924464967,-0.945467787321109,-0.944089852382067,
-0.941261804712596,-0.93376064929237,-0.902449198161415,-0.795457231966841,
-0.789166929538688,-0.787267626220621,-0.786133589670826,-0.785225835029717,
-0.784005988649509,-0.781715658909512,-0.7688016245874,-0.744143923004743,
-0.69298902551095,-0.66256616552324),.UNSPECIFIED.);
#145=B_SPLINE_CURVE_WITH_KNOTS('',3,(#24968,#24969,#24970,#24971,#24972,
#24973,#24974,#24975,#24976,#24977,#24978,#24979,#24980,#24981,#24982,#24983,
#24984,#24985,#24986,#24987,#24988,#24989,#24990,#24991,#24992,#24993,#24994,
#24995,#24996,#24997,#24998,#24999,#25000,#25001,#25002,#25003,#25004,#25005,
#25006,#25007,#25008,#25009,#25010,#25011,#25012,#25013,#25014,#25015,#25016,
#25017,#25018,#25019,#25020,#25021,#25022,#25023,#25024,#25025,#25026,#25027,
#25028,#25029,#25030,#25031,#25032,#25033,#25034,#25035,#25036,#25037,#25038,
#25039,#25040,#25041,#25042,#25043,#25044,#25045,#25046,#25047,#25048,#25049,
#25050,#25051,#25052,#25053,#25054,#25055,#25056,#25057,#25058,#25059,#25060,
#25061,#25062,#25063,#25064,#25065,#25066,#25067,#25068,#25069,#25070,#25071,
#25072,#25073,#25074,#25075,#25076,#25077,#25078,#25079,#25080,#25081,#25082,
#25083,#25084,#25085,#25086,#25087,#25088,#25089,#25090,#25091,#25092,#25093,
#25094,#25095,#25096,#25097,#25098,#25099,#25100,#25101,#25102,#25103,#25104,
#25105,#25106,#25107,#25108,#25109,#25110,#25111,#25112,#25113,#25114,#25115,
#25116,#25117,#25118,#25119,#25120,#25121,#25122,#25123,#25124,#25125,#25126,
#25127,#25128,#25129,#25130,#25131,#25132,#25133,#25134,#25135,#25136,#25137,
#25138,#25139,#25140,#25141,#25142,#25143,#25144,#25145,#25146,#25147,#25148,
#25149,#25150,#25151,#25152,#25153,#25154,#25155,#25156,#25157,#25158,#25159,
#25160,#25161,#25162,#25163,#25164,#25165,#25166,#25167,#25168,#25169,#25170,
#25171,#25172,#25173,#25174,#25175,#25176,#25177,#25178,#25179,#25180,#25181,
#25182,#25183,#25184,#25185,#25186,#25187,#25188,#25189,#25190,#25191,#25192,
#25193,#25194,#25195,#25196,#25197,#25198,#25199,#25200,#25201,#25202,#25203,
#25204,#25205,#25206,#25207,#25208,#25209,#25210,#25211,#25212,#25213,#25214,
#25215,#25216,#25217,#25218,#25219,#25220,#25221,#25222,#25223,#25224,#25225,
#25226,#25227,#25228,#25229,#25230,#25231,#25232,#25233,#25234,#25235),
 .UNSPECIFIED.,.F.,.F.,(4,2,2,2,2,2,2,2,2,2,2,2,2,2,2,2,2,2,2,2,2,2,2,2,
2,2,2,2,2,2,2,2,2,2,2,2,2,2,2,2,2,2,2,2,2,2,2,2,2,2,2,2,2,2,2,2,2,2,2,2,
2,2,2,2,2,2,2,2,2,2,2,2,2,2,2,2,2,2,2,2,2,2,2,2,2,2,2,2,2,2,2,2,2,2,2,2,
2,2,2,2,2,2,2,2,2,2,2,2,2,2,2,2,2,2,2,2,2,2,2,2,2,2,2,2,2,2,2,2,2,2,2,2,
2,4),(-3.40165445961574,-3.37651397343408,-3.31546800009253,-3.3055998640551,
-3.29396037018036,-3.26719634061028,-3.25311387375933,-3.25162047993218,
-3.25089653352018,-3.25038520291807,-3.24984664392857,-3.24908910657498,
-3.24752273708241,-3.23123774401991,-3.23022642079531,-3.22777500349404,
-3.13227826096747,-3.09785532997197,-3.09400584524469,-3.09197936447331,
-3.09068857816998,-3.08948930936203,-3.08850363838942,-3.08749657854455,
-3.08566417248586,-3.07991939968857,-2.96163122907052,-2.95278662553835,
-2.93700132916986,-2.92939720600353,-2.92810061813168,-2.92741701828514,
-2.92686174596242,-2.92620572969147,-2.92506768209998,-2.92068870539787,
-2.91803591657381,-2.91645773231244,-2.91509026791511,-2.82059313048553,
-2.77564341861965,-2.77114935357919,-2.7688796939199,-2.76748663922636,
-2.76621237580926,-2.7652188597922,-2.76424628694146,-2.76258668675173,
-2.7580812877869,-2.68495853290408,-2.63437171567505,-2.61050859690884,
-2.60585756064919,-2.60473925821006,-2.60409447560672,-2.60353297882944,
-2.60283249502999,-2.60174998251649,-2.5968239649577,-2.5011547536028,-2.45274112610681,
-2.44807013939555,-2.44573516061797,-2.44431484185283,-2.44302214861118,
-2.44202576751674,-2.44106056102874,-2.43970897634766,-2.43615578235766,
-2.43448157044393,-2.3576469212505,-2.33098899209477,-2.29861840213104,
-2.28331145355877,-2.28179484072996,-2.28106630172311,-2.28055423752006,
-2.28001724589956,-2.27926553826187,-2.27729565075319,-2.24748171454464,
-2.16024537730253,-2.13625534223526,-2.12319767711703,-2.1209005669633,
-2.11967934854468,-2.11877153337843,-2.11778189287501,-2.11603620855763,
-2.11094079922776,-2.03141703483579,-1.96353232804275,-1.95945518807607,
-1.95834730569696,-1.95769835664803,-1.95713730476804,-1.95644257414832,
-1.95509281509891,-1.94621081317906,-1.92494782026015,-1.87578506546496,
-1.82511041445525,-1.82150465774966,-1.80093991482197,-1.79810903878438,
-1.7967937601229,-1.7957762479802,-1.7946788091398,-1.79294316156894,-1.78740991264778,
-1.75568061070349,-1.70995083999306,-1.64042837910348,-1.6363908266861,
-1.63528697858705,-1.63463894565946,-1.63408883271241,-1.63341233050254,
-1.63267997428938,-1.63151771686193,-1.62927718663556,-1.60792121829486,
-1.58417470245642,-1.48202673335687,-1.47606685813653,-1.47420745542301,
-1.47319491108913,-1.47218959857971,-1.47096419336311,-1.46864747618132,
-1.45517478309306,-1.43885884009542,-1.41487041060513,-1.37029241472368),
 .UNSPECIFIED.);
#146=B_SPLINE_CURVE_WITH_KNOTS('',3,(#25237,#25238,#25239,#25240,#25241,
#25242,#25243,#25244,#25245,#25246,#25247,#25248,#25249,#25250,#25251,#25252,
#25253,#25254,#25255,#25256,#25257,#25258,#25259,#25260,#25261,#25262,#25263,
#25264,#25265,#25266,#25267,#25268,#25269,#25270,#25271,#25272,#25273,#25274,
#25275,#25276,#25277,#25278,#25279,#25280,#25281,#25282,#25283,#25284,#25285,
#25286,#25287,#25288,#25289,#25290,#25291,#25292,#25293,#25294,#25295,#25296,
#25297,#25298,#25299,#25300,#25301,#25302,#25303,#25304,#25305,#25306,#25307,
#25308,#25309,#25310,#25311,#25312,#25313,#25314,#25315,#25316,#25317,#25318,
#25319,#25320,#25321,#25322,#25323,#25324,#25325,#25326,#25327,#25328,#25329,
#25330),.UNSPECIFIED.,.F.,.F.,(4,2,2,2,2,2,2,2,2,2,2,2,2,2,2,2,2,2,2,2,
2,2,2,2,2,2,2,2,2,2,2,2,2,2,2,2,2,2,2,2,2,2,2,2,2,2,4),(-0.66256616552324,
-0.650642016057342,-0.627475925094102,-0.62561516282241,-0.624881560281531,
-0.624349371729995,-0.623788924323196,-0.623032695985302,-0.622189761079398,
-0.620761154543921,-0.61779040074806,-0.609768495821252,-0.589501938977944,
-0.471571106734159,-0.465783642166481,-0.463945924216361,-0.462937861064067,
-0.461932304695768,-0.460699741725335,-0.458348635350572,-0.444099907637023,
-0.413458500453692,-0.36897150926728,-0.347330245893649,-0.311466084634063,
-0.310602870351287,-0.303457661623643,-0.302227387371033,-0.301489951931337,
-0.300934018935329,-0.300333286097983,-0.299387675320691,-0.29646845572393,
-0.29192714869184,-0.277672888677262,-0.250982452063922,-0.148756806892039,
-0.142772884609283,-0.140910911626179,-0.139898067918963,-0.138893155076745,
-0.137669246928664,-0.135358390084581,-0.121999232846878,-0.119887552893688,
-0.0848123304289776,-0.000962485193680865),.UNSPECIFIED.);
#147=B_SPLINE_CURVE_WITH_KNOTS('',3,(#25331,#25332,#25333,#25334,#25335,
#25336,#25337,#25338,#25339,#25340,#25341,#25342,#25343,#25344,#25345,#25346,
#25347,#25348,#25349,#25350,#25351,#25352,#25353,#25354,#25355,#25356,#25357,
#25358,#25359,#25360,#25361,#25362,#25363,#25364,#25365,#25366,#25367,#25368,
#25369,#25370,#25371,#25372,#25373,#25374,#25375,#25376,#25377,#25378,#25379,
#25380,#25381,#25382,#25383,#25384,#25385,#25386,#25387,#25388,#25389,#25390,
#25391,#25392,#25393,#25394,#25395,#25396,#25397,#25398,#25399,#25400,#25401,
#25402,#25403,#25404,#25405,#25406,#25407,#25408,#25409,#25410,#25411,#25412,
#25413,#25414,#25415,#25416,#25417,#25418,#25419,#25420,#25421,#25422,#25423,
#25424,#25425,#25426,#25427,#25428,#25429,#25430,#25431,#25432,#25433,#25434,
#25435,#25436,#25437,#25438,#25439,#25440,#25441,#25442,#25443,#25444,#25445,
#25446,#25447,#25448,#25449,#25450,#25451,#25452,#25453,#25454,#25455,#25456,
#25457,#25458,#25459,#25460,#25461,#25462,#25463,#25464,#25465,#25466,#25467,
#25468,#25469,#25470,#25471,#25472,#25473,#25474,#25475,#25476,#25477,#25478,
#25479,#25480,#25481,#25482,#25483,#25484,#25485,#25486,#25487,#25488,#25489,
#25490,#25491,#25492,#25493,#25494,#25495,#25496,#25497,#25498,#25499,#25500,
#25501,#25502,#25503,#25504,#25505,#25506,#25507,#25508,#25509,#25510,#25511,
#25512,#25513,#25514,#25515,#25516,#25517,#25518,#25519,#25520,#25521,#25522,
#25523,#25524,#25525,#25526,#25527,#25528,#25529,#25530,#25531,#25532,#25533,
#25534,#25535,#25536,#25537,#25538,#25539,#25540,#25541,#25542,#25543,#25544,
#25545,#25546,#25547,#25548,#25549,#25550,#25551,#25552,#25553,#25554,#25555,
#25556),.UNSPECIFIED.,.F.,.F.,(4,2,2,2,2,2,2,2,2,2,2,2,2,2,2,2,2,2,2,2,
2,2,2,2,2,2,2,2,2,2,2,2,2,2,2,2,2,2,2,2,2,2,2,2,2,2,2,2,2,2,2,2,2,2,2,2,
2,2,2,2,2,2,2,2,2,2,2,2,2,2,2,2,2,2,2,2,2,2,2,2,2,2,2,2,2,2,2,2,2,2,2,2,
2,2,2,2,2,2,2,2,2,2,2,2,2,2,2,2,2,2,2,2,4),(-4.06163240503467,-4.04157573871171,
-4.04038201218937,-4.03963672300573,-4.0390750840685,-4.03854225091604,
-4.03801492403181,-4.03729886330514,-4.03589657414182,-4.02496218233544,
-4.02165983126325,-4.02093279376469,-4.01760821936916,-4.0140022612106,
-3.91647499154767,-3.89304517433229,-3.88114562152254,-3.87890888848764,
-3.87770131040074,-3.87679556589489,-3.87565467318111,-3.87372130724079,
-3.86712512399437,-3.8632839039215,-3.85934748122755,-3.85727724938406,
-3.85553286928691,-3.85431652569437,-3.85243683125332,-3.84515648624425,
-3.75504915554739,-3.73426065508786,-3.72343230095042,-3.71973263653401,
-3.71724397111261,-3.71635637203914,-3.71583160126477,-3.71526486181131,
-3.71452813641032,-3.71298339915092,-3.70187492498724,-3.69944465522738,
-3.65297477414986,-3.64811917839652,-3.64263042313296,-3.63634166400954,
-3.62901188123814,-3.59918788681215,-3.57227927282716,-3.5585504412355,
-3.55622343135512,-3.55499645190537,-3.5539918368805,-3.55298167272471,
-3.55113144962901,-3.5452382130096,-3.42856493187509,-3.40752233891435,
-3.39931294818784,-3.39629208498634,-3.39484607536417,-3.39367524510972,
-3.39302310729654,-3.39251844971999,-3.39195191389418,-3.39090135838375,
-3.38745295466888,-3.29862834838403,-3.28752756707905,-3.27293780923546,
-3.24825155902145,-3.23537512073953,-3.23308778798072,-3.23186909255781,
-3.23096200222637,-3.22982854702158,-3.22792962567114,-3.22163566559073,
-3.11531009309017,-3.09538121386358,-3.07959756646609,-3.07456765324311,
-3.07246130587609,-3.07135017461772,-3.07063941780253,-3.06997820865267,
-3.06942925963572,-3.06885594749971,-3.0677719646759,-3.06403533195082,
-3.06319326508204,-2.95986961545267,-2.91796811334442,-2.91140622988108,
-2.90955959352537,-2.90843781969178,-2.90742778519324,-2.90614173724338,
-2.90352964544845,-2.88103381242773,-2.86886802818526,-2.78493286844683,
-2.771758488508,-2.7516230394206,-2.74945952361181,-2.74832662820939,-2.74760674657255,
-2.74693941431449,-2.7463901610028,-2.74582137478078,-2.74475978602781,
-2.74121851702462,-2.69291085651066),.UNSPECIFIED.);
#148=B_SPLINE_CURVE_WITH_KNOTS('',3,(#25562,#25563,#25564,#25565,#25566,
#25567,#25568,#25569,#25570,#25571,#25572,#25573,#25574,#25575,#25576,#25577,
#25578,#25579,#25580,#25581,#25582,#25583,#25584,#25585,#25586,#25587,#25588,
#25589,#25590,#25591,#25592,#25593,#25594,#25595,#25596,#25597,#25598,#25599,
#25600,#25601,#25602,#25603,#25604,#25605,#25606,#25607,#25608,#25609,#25610,
#25611,#25612,#25613,#25614,#25615,#25616,#25617,#25618,#25619,#25620,#25621,
#25622,#25623,#25624,#25625,#25626,#25627,#25628,#25629,#25630,#25631,#25632,
#25633,#25634,#25635,#25636,#25637,#25638,#25639,#25640,#25641,#25642,#25643,
#25644,#25645,#25646,#25647,#25648,#25649,#25650,#25651,#25652,#25653,#25654,
#25655,#25656,#25657,#25658,#25659,#25660,#25661,#25662,#25663,#25664,#25665,
#25666,#25667,#25668,#25669,#25670,#25671,#25672,#25673,#25674,#25675,#25676,
#25677,#25678,#25679,#25680,#25681,#25682,#25683,#25684,#25685,#25686,#25687,
#25688,#25689,#25690,#25691,#25692,#25693,#25694,#25695,#25696,#25697,#25698,
#25699,#25700,#25701,#25702,#25703,#25704,#25705,#25706,#25707,#25708,#25709,
#25710,#25711,#25712,#25713,#25714,#25715,#25716,#25717,#25718,#25719,#25720,
#25721,#25722,#25723,#25724,#25725,#25726,#25727,#25728,#25729,#25730,#25731,
#25732,#25733,#25734,#25735,#25736,#25737,#25738,#25739,#25740,#25741,#25742,
#25743,#25744,#25745),.UNSPECIFIED.,.F.,.F.,(4,2,2,2,2,2,2,2,2,2,2,2,2,
2,2,2,2,2,2,2,2,2,2,2,2,2,2,2,2,2,2,2,2,2,2,2,2,2,2,2,2,2,2,2,2,2,2,2,2,
2,2,2,2,2,2,2,2,2,2,2,2,2,2,2,2,2,2,2,2,2,2,2,2,2,2,2,2,2,2,2,2,2,2,2,2,
2,2,2,2,2,2,4),(-1.36994082487413,-1.29603031198163,-1.29492405155685,-1.29097890040597,
-1.28956651607252,-1.28858499749473,-1.28759533239186,-1.2863455444552,
-1.28498602773553,-1.28279577186211,-1.23873322779561,-1.18847552089364,
-1.13212801695096,-1.12865639430014,-1.1276029913557,-1.12703583714301,
-1.12647537588788,-1.12578597295757,-1.12446063616401,-1.11618252681527,
-1.09815219310377,-1.06594107454888,-0.997095234521415,-0.984161026241984,
-0.983254624225425,-0.969794336805012,-0.967354308988684,-0.966076315947826,
-0.965087812338502,-0.963990292039223,-0.962843346257242,-0.961158379590627,
-0.946133958449461,-0.912221055408388,-0.834128051109883,-0.807182576143023,
-0.805256765335285,-0.804512362897235,-0.803977473044589,-0.80340764905284,
-0.802639959516383,-0.800915790566093,-0.754767053782881,-0.721703380028494,
-0.719073473633127,-0.688566799212006,-0.648197139496502,-0.644909582623209,
-0.643602521349625,-0.642649333299487,-0.64164720603178,-0.640314730180309,
-0.638840954602102,-0.636377016551929,-0.585924081096949,-0.504414296391204,
-0.501348766352125,-0.500210244449823,-0.483903780959305,-0.482337225289159,
-0.481579752799313,-0.48104130908245,-0.480530146495798,-0.479806531466997,
-0.478314176922611,-0.464265304664495,-0.437612850160603,-0.374178376701174,
-0.325373235946942,-0.321959878370101,-0.320631548344275,-0.319672724424056,
-0.318673671339005,-0.317360235912869,-0.315912921617537,-0.313512805330025,
-0.264500142443476,-0.17001048278854,-0.168371874730889,-0.16694049061098,
-0.164941408620806,-0.159977242239485,-0.158891862606302,-0.158190569316189,
-0.157629121469594,-0.156985167881734,-0.155870201828929,-0.151258814046137,
-0.112526851773713,-0.00998850380131196,-0.00354524911410741,-0.00096169998764838),
 .UNSPECIFIED.);
#149=B_SPLINE_CURVE_WITH_KNOTS('',3,(#25746,#25747,#25748,#25749,#25750,
#25751,#25752,#25753,#25754,#25755,#25756,#25757,#25758,#25759,#25760,#25761,
#25762,#25763,#25764,#25765,#25766,#25767,#25768,#25769,#25770,#25771,#25772,
#25773,#25774,#25775,#25776,#25777,#25778,#25779,#25780,#25781,#25782,#25783,
#25784,#25785,#25786,#25787,#25788,#25789,#25790,#25791,#25792,#25793,#25794,
#25795,#25796,#25797,#25798,#25799,#25800,#25801,#25802,#25803,#25804,#25805,
#25806,#25807,#25808,#25809,#25810,#25811,#25812,#25813,#25814,#25815,#25816,
#25817,#25818,#25819,#25820,#25821,#25822,#25823,#25824,#25825,#25826,#25827,
#25828,#25829,#25830,#25831,#25832,#25833,#25834,#25835,#25836,#25837,#25838,
#25839,#25840,#25841,#25842,#25843,#25844,#25845,#25846,#25847),
 .UNSPECIFIED.,.F.,.F.,(4,2,2,2,2,2,2,2,2,2,2,2,2,2,2,2,2,2,2,2,2,2,2,2,
2,2,2,2,2,2,2,2,2,2,2,2,2,2,2,2,2,2,2,2,2,2,2,2,2,2,4),(-4.06334679065876,
-4.0614676879816,-4.06023683188313,-4.0592641980323,-4.05827705711106,-4.05728978078462,
-4.05555580478751,-4.05054278406359,-4.02655588148113,-3.93101169180052,
-3.9028098550946,-3.89882546095418,-3.89776450235261,-3.89713252793102,
-3.89656917207661,-3.89584901909655,-3.89470271198501,-3.88891192429347,
-3.88757741407342,-3.88650615930939,-3.88473245356577,-3.79028214035835,
-3.74549045229745,-3.74100514892433,-3.73873880066728,-3.73734717590536,
-3.73607402101243,-3.73508072801975,-3.73410790828129,-3.73272815964916,
-3.72899836538777,-3.66801956698602,-3.57943188427975,-3.5755380354782,
-3.57448554566139,-3.5738554466752,-3.57329168545548,-3.57256820155787,
-3.57107737979007,-3.56680112404204,-3.46927446488557,-3.42239407658512,
-3.417798908159,-3.41549186252672,-3.41408320032954,-3.41279768493003,-3.41180262857148,
-3.41083425782256,-3.40947097156366,-3.40664913081027,-3.40165445961574),
 .UNSPECIFIED.);
#150=B_SPLINE_CURVE_WITH_KNOTS('',3,(#25848,#25849,#25850,#25851,#25852,
#25853,#25854,#25855,#25856,#25857,#25858,#25859,#25860,#25861,#25862,#25863,
#25864,#25865,#25866,#25867,#25868,#25869,#25870,#25871,#25872,#25873,#25874,
#25875,#25876,#25877,#25878,#25879,#25880,#25881,#25882,#25883,#25884,#25885,
#25886,#25887,#25888,#25889,#25890,#25891,#25892,#25893,#25894,#25895,#25896,
#25897,#25898,#25899,#25900,#25901,#25902,#25903,#25904,#25905,#25906,#25907,
#25908,#25909,#25910,#25911,#25912,#25913,#25914,#25915,#25916,#25917,#25918,
#25919,#25920,#25921,#25922,#25923,#25924,#25925,#25926,#25927,#25928,#25929,
#25930,#25931,#25932,#25933,#25934,#25935,#25936,#25937,#25938,#25939,#25940,
#25941,#25942,#25943,#25944,#25945,#25946,#25947,#25948,#25949,#25950,#25951,
#25952,#25953,#25954,#25955,#25956,#25957,#25958,#25959,#25960,#25961,#25962,
#25963,#25964,#25965,#25966,#25967,#25968,#25969,#25970,#25971,#25972,#25973,
#25974,#25975,#25976,#25977,#25978,#25979,#25980,#25981,#25982,#25983,#25984,
#25985,#25986,#25987,#25988,#25989,#25990,#25991,#25992,#25993,#25994,#25995,
#25996,#25997,#25998,#25999,#26000,#26001,#26002,#26003,#26004,#26005,#26006,
#26007,#26008,#26009,#26010,#26011,#26012,#26013,#26014,#26015,#26016,#26017,
#26018,#26019,#26020,#26021,#26022,#26023,#26024,#26025,#26026,#26027,#26028,
#26029,#26030,#26031,#26032,#26033,#26034,#26035,#26036,#26037,#26038,#26039,
#26040,#26041,#26042,#26043,#26044,#26045,#26046,#26047,#26048,#26049,#26050,
#26051,#26052,#26053,#26054,#26055,#26056,#26057,#26058,#26059,#26060,#26061,
#26062,#26063,#26064,#26065,#26066,#26067,#26068,#26069,#26070,#26071,#26072,
#26073,#26074,#26075,#26076,#26077,#26078,#26079,#26080,#26081,#26082,#26083,
#26084,#26085,#26086,#26087,#26088,#26089,#26090,#26091,#26092,#26093,#26094,
#26095,#26096,#26097,#26098,#26099,#26100,#26101,#26102,#26103,#26104,#26105,
#26106,#26107),.UNSPECIFIED.,.F.,.F.,(4,2,2,2,2,2,2,2,2,2,2,2,2,2,2,2,2,
2,2,2,2,2,2,2,2,2,2,2,2,2,2,2,2,2,2,2,2,2,2,2,2,2,2,2,2,2,2,2,2,2,2,2,2,
2,2,2,2,2,2,2,2,2,2,2,2,2,2,2,2,2,2,2,2,2,2,2,2,2,2,2,2,2,2,2,2,2,2,2,2,
2,2,2,2,2,2,2,2,2,2,2,2,2,2,2,2,2,2,2,2,2,2,2,2,2,2,2,2,2,2,2,2,2,2,2,2,
2,2,2,2,4),(-2.69291085651066,-2.68483550196456,-2.63175781315807,-2.59453214581927,
-2.58842111889877,-2.58662122692198,-2.58550985634893,-2.58449730481997,
-2.58319143929397,-2.58048011880597,-2.5627341192017,-2.56070138624403,
-2.5554977272015,-2.47750698729298,-2.42871120830902,-2.4265515182855,-2.42542005379274,
-2.42470075482836,-2.42403387557628,-2.42347995758067,-2.42290948848786,
-2.42183967505021,-2.41822796826577,-2.3584291822467,-2.33287252748695,
-2.30398635587902,-2.27929043290245,-2.26641354891322,-2.26412582489114,
-2.26290688320973,-2.26190225157808,-2.26088645654468,-2.25900968153982,
-2.25290365961186,-2.14298108650705,-2.1045499646331,-2.10215219233093,
-2.10127492902509,-2.10068374611877,-2.10011010983474,-2.09941837242733,
-2.09769057906015,-2.08181125684333,-2.08043691419415,-2.07839069856121,
-2.03210973013485,-1.94744299533067,-1.94224607278765,-1.9404864877677,
-1.93949420115805,-1.93858713024149,-1.93737161160444,-1.93510041509311,
-1.92256147488824,-1.89789957648225,-1.80996532116847,-1.8062218569041,
-1.79586973230887,-1.79507323407456,-1.79354893993996,-1.79281544358036,
-1.79154642977009,-1.78029833685377,-1.77872725313645,-1.77799612124083,
-1.77742988718088,-1.77681056963108,-1.77580567093845,-1.77238181189004,
-1.75059182328577,-1.72632260840022,-1.67037088712027,-1.62202120263258,
-1.61861268862138,-1.61716706029754,-1.61614241426979,-1.61519354646335,
-1.61417263921128,-1.61161591158002,-1.59135857889265,-1.5588587626773,
-1.46137199625791,-1.45696788098358,-1.45557285966385,-1.45485925454564,
-1.45429662086237,-1.45366071900825,-1.45258211618047,-1.44840291232943,
-1.41756323602812,-1.30205182218662,-1.29607304721407,-1.2942487356737,
-1.29313690631429,-1.29214303502324,-1.29117456508021,-1.28913758390785,
-1.28039658225398,-1.26477103761199,-1.24223401994546,-1.19147447850136,
-1.1362534129299,-1.1330601389816,-1.13204086129924,-1.1314804921133,-1.13092437392153,
-1.13022495392216,-1.12885214501725,-1.11932666108276,-1.09083100733912,
-1.00240288889988,-0.975035052016722,-0.972038341799565,-0.970670524523666,
-0.969661761801333,-0.96871831060029,-0.967675708467565,-0.964911838216675,
-0.93420291292175,-0.922831668509246,-0.838592420836438,-0.81150048814873,
-0.809572003159847,-0.808827057408071,-0.808291942922505,-0.807722040540725,
-0.806954514568413,-0.805231830163798,-0.759955563739871,-0.662267969628587),
 .UNSPECIFIED.);
#151=B_SPLINE_CURVE_WITH_KNOTS('',3,(#26112,#26113,#26114,#26115,#26116,
#26117,#26118,#26119,#26120,#26121,#26122,#26123,#26124,#26125,#26126,#26127,
#26128,#26129,#26130,#26131,#26132,#26133,#26134,#26135,#26136,#26137,#26138,
#26139,#26140,#26141,#26142,#26143,#26144,#26145,#26146,#26147,#26148,#26149,
#26150,#26151,#26152,#26153,#26154,#26155,#26156,#26157,#26158,#26159,#26160,
#26161,#26162,#26163,#26164,#26165,#26166,#26167,#26168,#26169,#26170,#26171,
#26172,#26173,#26174,#26175,#26176,#26177,#26178,#26179,#26180,#26181,#26182,
#26183,#26184,#26185,#26186,#26187,#26188,#26189,#26190,#26191,#26192,#26193,
#26194,#26195,#26196,#26197,#26198,#26199,#26200,#26201,#26202,#26203,#26204,
#26205,#26206,#26207,#26208,#26209,#26210,#26211,#26212,#26213,#26214,#26215,
#26216,#26217,#26218,#26219,#26220,#26221,#26222,#26223,#26224,#26225,#26226,
#26227,#26228,#26229,#26230,#26231,#26232,#26233,#26234,#26235,#26236,#26237,
#26238,#26239,#26240,#26241,#26242,#26243,#26244,#26245,#26246,#26247,#26248,
#26249,#26250,#26251,#26252,#26253,#26254,#26255,#26256,#26257,#26258,#26259,
#26260,#26261,#26262,#26263,#26264,#26265,#26266,#26267,#26268,#26269,#26270,
#26271,#26272,#26273,#26274,#26275,#26276,#26277,#26278,#26279,#26280,#26281,
#26282,#26283,#26284,#26285,#26286,#26287,#26288,#26289,#26290,#26291,#26292,
#26293,#26294,#26295,#26296,#26297,#26298,#26299,#26300,#26301,#26302,#26303,
#26304,#26305,#26306,#26307,#26308,#26309,#26310,#26311,#26312,#26313,#26314,
#26315,#26316,#26317,#26318,#26319,#26320,#26321,#26322,#26323,#26324,#26325,
#26326,#26327,#26328,#26329,#26330,#26331,#26332,#26333,#26334,#26335,#26336,
#26337,#26338,#26339,#26340,#26341,#26342,#26343,#26344,#26345,#26346,#26347,
#26348,#26349,#26350,#26351,#26352,#26353,#26354,#26355,#26356,#26357,#26358,
#26359,#26360,#26361,#26362,#26363,#26364,#26365,#26366,#26367,#26368,#26369,
#26370,#26371,#26372,#26373,#26374,#26375,#26376,#26377,#26378,#26379,#26380,
#26381,#26382,#26383,#26384,#26385,#26386,#26387,#26388,#26389,#26390,#26391,
#26392,#26393,#26394,#26395,#26396,#26397,#26398,#26399,#26400,#26401,#26402,
#26403,#26404,#26405,#26406,#26407,#26408,#26409,#26410,#26411),
 .UNSPECIFIED.,.F.,.F.,(4,2,2,2,2,2,2,2,2,2,2,2,2,2,2,2,2,2,2,2,2,2,2,2,
2,2,2,2,2,2,2,2,2,2,2,2,2,2,2,2,2,2,2,2,2,2,2,2,2,2,2,2,2,2,2,2,2,2,2,2,
2,2,2,2,2,2,2,2,2,2,2,2,2,2,2,2,2,2,2,2,2,2,2,2,2,2,2,2,2,2,2,2,2,2,2,2,
2,2,2,2,2,2,2,2,2,2,2,2,2,2,2,2,2,2,2,2,2,2,2,2,2,2,2,2,2,2,2,2,2,2,2,2,
2,2,2,2,2,2,2,2,2,2,2,2,2,2,2,2,2,4),(-3.39905562805101,-3.3986699384756,
-3.39720180526091,-3.39190640431446,-3.38971888762928,-3.38808097034261,
-3.38733247960283,-3.3867986607061,-3.38626974911432,-3.38554728983858,
-3.38411974379569,-3.37248028154884,-3.28933011170741,-3.27783349011705,
-3.24888080575984,-3.22995922470087,-3.22744230425333,-3.2261759310716,
-3.22526332232139,-3.22429554298103,-3.22293194666987,-3.22010574508331,
-3.18963746712672,-3.10268644497334,-3.07632509123859,-3.06978633775776,
-3.06723084153549,-3.06595196616715,-3.06517117168965,-3.06445971556827,
-3.06390666882451,-3.06336054141764,-3.06241065271926,-3.05972482703521,
-3.01720005158188,-2.98411126843357,-2.94025091241868,-2.91100757322446,
-2.90575142860157,-2.90405015562316,-2.90296108636246,-2.90194193229755,
-2.90061112298654,-2.8978003724413,-2.87676775237228,-2.87420551087048,
-2.8583565003042,-2.79843755596687,-2.74624998893677,-2.74414329951607,
-2.74303218260706,-2.74232154754129,-2.74169176920089,-2.74114234503394,
-2.74057827571828,-2.73953932909358,-2.73618511443869,-2.68283241446274,
-2.62323973103681,-2.5889514290326,-2.58314482637424,-2.58137887768191,
-2.58027540224033,-2.57926122580341,-2.57796263625027,-2.5752148524396,
-2.55662202539812,-2.55510995371541,-2.54833664258733,-2.4715202614367,
-2.46071833832439,-2.42215998939823,-2.42070194060178,-2.41984719434025,
-2.41908319135597,-2.41852160291228,-2.4179923249728,-2.41726865202679,
-2.4158365566108,-2.40407091510391,-2.37530191281133,-2.35692500368991,
-2.32727054756971,-2.29077996059181,-2.27139508429334,-2.26112417283738,
-2.25898218897382,-2.25779504572126,-2.25689071284536,-2.25588258531324,
-2.25404245997039,-2.24823003307144,-2.13068933116611,-2.10156316604489,
-2.09889049714317,-2.09695468628881,-2.09614988910252,-2.09557355722074,
-2.09504774530097,-2.0943380789986,-2.09296103325885,-2.08268953884468,
-2.08086863707242,-2.07784366970475,-2.07654119765468,-2.03125364127204,
-1.99906316433315,-1.97884394746461,-1.97161463890321,-1.93973307258011,
-1.93662013100313,-1.93534346946044,-1.93439818211379,-1.9333703030968,
-1.93196653990711,-1.92873164333418,-1.88020924667334,-1.7879215533845,
-1.78657229472881,-1.77542135151552,-1.77387436359239,-1.77313696918752,
-1.77256989857996,-1.77195380463532,-1.77096289000188,-1.76766602530795,
-1.74718532434993,-1.73396230204563,-1.64632871888124,-1.61659057824934,
-1.61353052414316,-1.61226317438258,-1.61132017450241,-1.61032300956624,
-1.60895754589759,-1.60743792718969,-1.60486296867588,-1.56146999677902,
-1.51111495076938,-1.45500715430153,-1.45157858195507,-1.45053031726415,
-1.44996419452574,-1.44940362642723,-1.44871245411735,-1.44737871334427,
-1.43889460717303,-1.41946963007192,-1.37324998273249,-1.36994082487413),
 .UNSPECIFIED.);
#152=B_SPLINE_CURVE_WITH_KNOTS('',3,(#26413,#26414,#26415,#26416,#26417,
#26418,#26419,#26420,#26421,#26422,#26423,#26424,#26425,#26426,#26427,#26428,
#26429,#26430,#26431,#26432,#26433,#26434,#26435,#26436,#26437,#26438,#26439,
#26440,#26441,#26442,#26443,#26444,#26445,#26446,#26447,#26448,#26449,#26450,
#26451,#26452,#26453,#26454,#26455,#26456,#26457,#26458,#26459,#26460,#26461,
#26462,#26463,#26464,#26465,#26466,#26467,#26468,#26469,#26470,#26471,#26472,
#26473,#26474,#26475,#26476,#26477,#26478,#26479,#26480,#26481,#26482,#26483,
#26484,#26485,#26486,#26487,#26488,#26489,#26490,#26491,#26492,#26493,#26494,
#26495,#26496,#26497,#26498,#26499,#26500,#26501,#26502,#26503,#26504,#26505,
#26506,#26507,#26508,#26509,#26510,#26511,#26512),.UNSPECIFIED.,.F.,.F.,
(4,2,2,2,2,2,2,2,2,2,2,2,2,2,2,2,2,2,2,2,2,2,2,2,2,2,2,2,2,2,2,2,2,2,2,
2,2,2,2,2,2,2,2,2,2,2,2,2,2,4),(-0.662267969628587,-0.656023241631284,-0.649906582883767,
-0.64806596154954,-0.646950363692581,-0.645954340698451,-0.644987197316384,
-0.642963829703752,-0.634398844025601,-0.542932602219484,-0.497333269948792,
-0.495144278173578,-0.494245840517306,-0.490575941454874,-0.486880676462917,
-0.485801182679687,-0.485228684430029,-0.484724483902254,-0.484066939921601,
-0.482890258037996,-0.477437933404764,-0.467069832420578,-0.436585264058004,
-0.414257558544152,-0.389882563565053,-0.329821797885483,-0.326147117059869,
-0.324654368488396,-0.323619287580412,-0.322666199478999,-0.321655778378131,
-0.319198646559563,-0.302198934422417,-0.260708699561111,-0.175336862317592,
-0.16466336406662,-0.163270153193844,-0.162556139838001,-0.16202905573395,
-0.161453333567352,-0.160652932858231,-0.158744386743169,-0.156119409559968,
-0.127971580737986,-0.0317350575781189,-0.0223250194030482,-0.00512195002278438,
-0.00248768498826383,-0.00122476864328915,-0.000961573598619955),
 .UNSPECIFIED.);
#153=B_SPLINE_CURVE_WITH_KNOTS('',3,(#26513,#26514,#26515,#26516,#26517,
#26518,#26519,#26520,#26521,#26522,#26523,#26524,#26525,#26526,#26527,#26528,
#26529,#26530,#26531,#26532,#26533,#26534,#26535,#26536,#26537,#26538,#26539,
#26540,#26541,#26542,#26543,#26544,#26545,#26546,#26547,#26548,#26549,#26550,
#26551,#26552,#26553,#26554,#26555,#26556,#26557,#26558,#26559,#26560,#26561,
#26562,#26563,#26564,#26565,#26566,#26567,#26568,#26569,#26570,#26571,#26572,
#26573,#26574,#26575,#26576,#26577,#26578,#26579,#26580,#26581,#26582,#26583,
#26584,#26585,#26586,#26587,#26588,#26589,#26590,#26591,#26592,#26593,#26594,
#26595,#26596,#26597,#26598,#26599,#26600,#26601,#26602,#26603,#26604,#26605,
#26606,#26607,#26608,#26609,#26610,#26611,#26612,#26613,#26614,#26615,#26616,
#26617,#26618,#26619,#26620,#26621,#26622,#26623,#26624,#26625,#26626,#26627,
#26628,#26629,#26630,#26631,#26632,#26633,#26634,#26635,#26636,#26637,#26638,
#26639,#26640,#26641,#26642,#26643,#26644,#26645,#26646,#26647,#26648,#26649,
#26650,#26651,#26652,#26653,#26654,#26655,#26656,#26657,#26658,#26659,#26660,
#26661,#26662,#26663,#26664,#26665,#26666,#26667,#26668,#26669,#26670,#26671,
#26672,#26673,#26674,#26675,#26676,#26677,#26678,#26679,#26680,#26681,#26682,
#26683,#26684,#26685,#26686,#26687,#26688,#26689,#26690,#26691,#26692,#26693,
#26694,#26695,#26696),.UNSPECIFIED.,.F.,.F.,(4,2,2,2,2,2,2,2,2,2,2,2,2,
2,2,2,2,2,2,2,2,2,2,2,2,2,2,2,2,2,2,2,2,2,2,2,2,2,2,2,2,2,2,2,2,2,2,2,2,
2,2,2,2,2,2,2,2,2,2,2,2,2,2,2,2,2,2,2,2,2,2,2,2,2,2,2,2,2,2,2,2,2,2,2,2,
2,2,2,2,2,2,4),(-4.06231940115315,-4.06180759515383,-4.06079267865506,-4.05939540104,
-4.05624487799662,-4.0532022843239,-3.9424777929911,-3.90396032272885,-3.90156122198485,
-3.90068376038417,-3.90009253062331,-3.89951891829682,-3.89882728977886,
-3.89710018829005,-3.88124564745109,-3.83630906365861,-3.78677498115249,
-3.76088784226537,-3.74304340076237,-3.74055807558855,-3.73954468988837,
-3.73853530026321,-3.73759188141429,-3.73613538678742,-3.73266658508861,
-3.67873597587883,-3.64085397514781,-3.63143354367246,-3.60038961646899,
-3.58754743551197,-3.57947671512071,-3.5781598278382,-3.57747209254732,
-3.57691157692918,-3.57634315327523,-3.57528392699597,-3.57176455340614,
-3.51497871156925,-3.46492125578514,-3.4207589708795,-3.4178533296904,-3.41679587937533,
-3.41575921816129,-3.41474546475796,-3.41335356104129,-3.41023291768028,
-3.37806717194243,-3.32556928343734,-3.31603859829061,-3.30572739075148,
-3.29307842166342,-3.27327501218121,-3.26458607681714,-3.25654649446471,
-3.255230961657,-3.25454352106071,-3.25398303182519,-3.25332865876994,-3.25219700649735,
-3.24788046080548,-3.17371029214313,-3.13003583735646,-3.10097359772646,
-3.09573641244768,-3.09447138566884,-3.09329064532566,-3.09233920123119,
-3.09132991006396,-3.08955980118985,-3.0840167303125,-2.9646942651452,-2.95556621861452,
-2.94045892842583,-2.93323472331399,-2.93195626433792,-2.93127657644906,
-2.9307215382597,-2.93014932162394,-2.9290717029883,-2.92539458002595,-2.92412346345475,
-2.82631763989466,-2.80257022693576,-2.77707481939084,-2.77224766956423,
-2.77101389900872,-2.77004036023397,-2.76905108190309,-2.76806482889069,
-2.7664019721073,-2.76164844464432,-2.69296972658525),.UNSPECIFIED.);
#154=B_SPLINE_CURVE_WITH_KNOTS('',3,(#26702,#26703,#26704,#26705,#26706,
#26707,#26708,#26709,#26710,#26711,#26712,#26713,#26714,#26715,#26716,#26717,
#26718,#26719,#26720,#26721,#26722,#26723,#26724,#26725,#26726,#26727,#26728,
#26729,#26730,#26731,#26732,#26733,#26734,#26735,#26736,#26737,#26738,#26739,
#26740,#26741,#26742,#26743,#26744,#26745,#26746,#26747,#26748,#26749,#26750,
#26751,#26752,#26753,#26754,#26755,#26756,#26757,#26758,#26759,#26760,#26761,
#26762,#26763,#26764,#26765,#26766,#26767,#26768,#26769,#26770,#26771,#26772,
#26773,#26774,#26775,#26776,#26777,#26778,#26779,#26780,#26781,#26782,#26783,
#26784,#26785,#26786,#26787,#26788,#26789,#26790,#26791,#26792,#26793,#26794,
#26795,#26796,#26797,#26798,#26799,#26800,#26801,#26802,#26803,#26804,#26805,
#26806,#26807,#26808,#26809,#26810,#26811,#26812,#26813,#26814,#26815,#26816,
#26817,#26818,#26819,#26820,#26821,#26822,#26823,#26824,#26825,#26826,#26827,
#26828,#26829,#26830,#26831,#26832,#26833,#26834,#26835,#26836,#26837,#26838,
#26839,#26840,#26841,#26842,#26843,#26844,#26845,#26846,#26847,#26848,#26849,
#26850,#26851,#26852,#26853,#26854,#26855,#26856,#26857,#26858,#26859,#26860,
#26861,#26862,#26863,#26864,#26865,#26866,#26867,#26868,#26869,#26870,#26871,
#26872,#26873,#26874,#26875,#26876,#26877,#26878,#26879,#26880,#26881,#26882,
#26883,#26884,#26885,#26886,#26887,#26888,#26889,#26890,#26891,#26892,#26893,
#26894,#26895,#26896,#26897,#26898,#26899,#26900,#26901,#26902,#26903,#26904,
#26905,#26906,#26907),.UNSPECIFIED.,.F.,.F.,(4,2,2,2,2,2,2,2,2,2,2,2,2,
2,2,2,2,2,2,2,2,2,2,2,2,2,2,2,2,2,2,2,2,2,2,2,2,2,2,2,2,2,2,2,2,2,2,2,2,
2,2,2,2,2,2,2,2,2,2,2,2,2,2,2,2,2,2,2,2,2,2,2,2,2,2,2,2,2,2,2,2,2,2,2,2,
2,2,2,2,2,2,2,2,2,2,2,2,2,2,2,2,2,4),(-1.37023206616483,-1.36812966361624,
-1.31495988064365,-1.28033116872487,-1.26872960285219,-1.26730259113486,
-1.26657998762061,-1.26605077026252,-1.26548848956129,-1.26472150735698,
-1.26386347679314,-1.26239780624463,-1.21544819021846,-1.1932339046631,
-1.11272357861048,-1.10757180926247,-1.10581847031458,-1.10482746207289,
-1.10392019817567,-1.10270240312946,-1.10042043505791,-1.0876645510105,
-1.06285764487118,-0.973142332264336,-0.954735945592908,-0.953459607769599,
-0.951956994763824,-0.949186331896358,-0.944914352439075,-0.943787044256786,
-0.943133664459087,-0.942584157805125,-0.941914368128,-0.940664557757263,
-0.939097805969844,-0.93572985566497,-0.92620885310859,-0.899459465785207,
-0.790737433724329,-0.784595174758264,-0.782713971899396,-0.781697251055323,
-0.780692624614882,-0.779475013023821,-0.777193699614575,-0.76444906438141,
-0.739643230788104,-0.689662903122298,-0.625647408021433,-0.621708484638798,
-0.620615248209474,-0.61996986684673,-0.619412573859502,-0.618729544632254,
-0.617416517373076,-0.615752896765813,-0.612099286665519,-0.601457722911825,
-0.568140987320813,-0.498018646632726,-0.485493248689937,-0.482050548550778,
-0.47887318870941,-0.462939220777084,-0.460313579950492,-0.459024613167074,
-0.458014013093852,-0.456893387024039,-0.455052701898673,-0.44855281448265,
-0.407322099037772,-0.365246197278059,-0.344693621299669,-0.313483607794391,
-0.29972154074754,-0.29822460434893,-0.297484392501702,-0.296950603967475,
-0.296413443383186,-0.295677169972216,-0.294102935764683,-0.292021725646933,
-0.287073339626908,-0.271407256029271,-0.256206865639362,-0.166479195264413,
-0.16011771861926,-0.158437408867385,-0.157235944336469,-0.155485998957491,
-0.153424555031228,-0.149574665412683,-0.145998697765913,-0.144549876647307,
-0.138643839787367,-0.136791574428554,-0.135780742574086,-0.134775747228059,
-0.13354871754341,-0.13122286451297,-0.117534835788489,-0.0912986355765214,
-0.00096255119342937),.UNSPECIFIED.);
#155=B_SPLINE_CURVE_WITH_KNOTS('',3,(#26908,#26909,#26910,#26911,#26912,
#26913,#26914,#26915,#26916,#26917,#26918,#26919,#26920,#26921,#26922,#26923,
#26924,#26925,#26926,#26927,#26928,#26929,#26930,#26931,#26932,#26933,#26934,
#26935,#26936,#26937,#26938,#26939,#26940,#26941,#26942,#26943,#26944,#26945,
#26946,#26947,#26948,#26949,#26950,#26951,#26952,#26953,#26954,#26955,#26956,
#26957,#26958,#26959,#26960,#26961,#26962,#26963,#26964,#26965,#26966,#26967,
#26968,#26969,#26970,#26971,#26972,#26973,#26974,#26975,#26976,#26977,#26978,
#26979,#26980,#26981,#26982,#26983,#26984,#26985,#26986,#26987,#26988,#26989,
#26990,#26991,#26992,#26993,#26994,#26995,#26996,#26997,#26998,#26999,#27000,
#27001,#27002,#27003,#27004,#27005,#27006,#27007,#27008,#27009,#27010,#27011,
#27012,#27013,#27014,#27015,#27016,#27017,#27018,#27019,#27020,#27021,#27022,
#27023,#27024,#27025,#27026,#27027,#27028,#27029),.UNSPECIFIED.,.F.,.F.,
(4,2,2,2,2,2,2,2,2,2,2,2,2,2,2,2,2,2,2,2,2,2,2,2,2,2,2,2,2,2,2,2,2,2,2,
2,2,2,2,2,2,2,2,2,2,2,2,2,2,2,2,2,2,2,2,2,2,2,2,2,4),(-4.0595736983573,
-4.0360030272802,-4.03453647378078,-4.03367831943194,-4.03307303464023,
-4.03254841386927,-4.03198175256297,-4.03124476428623,-4.02964042551851,
-4.01750352546539,-4.01634326598266,-4.01342588961253,-4.01274888999768,
-4.01050484083728,-4.00742193864187,-4.00370322584028,-3.91043602532289,
-3.8869449413952,-3.8750189499694,-3.87278119696411,-3.87157357934867,-3.87057964726954,
-3.86956081603211,-3.86766630772408,-3.8614037040846,-3.75438676477088,
-3.73730444856761,-3.72003811725165,-3.71461238701461,-3.71238529077751,
-3.71072461678017,-3.70997120270708,-3.70943840622781,-3.70891107597547,
-3.70819473527818,-3.70679108071026,-3.69581484089607,-3.69255725567441,
-3.69215376896637,-3.68993429776076,-3.68876801112298,-3.68762958165876,
-3.64096361949087,-3.63570444608284,-3.62967232937953,-3.62264150764535,
-3.61425214983486,-3.58571416026584,-3.55647372490919,-3.55121806510108,
-3.54951693657518,-3.54842795659784,-3.54740888383224,-3.54607817745163,
-3.54326763255019,-3.52223617698608,-3.51967663428222,-3.50304470260634,
-3.4439490838304,-3.41116981593671,-3.39905562805101),.UNSPECIFIED.);
#156=B_SPLINE_CURVE_WITH_KNOTS('',3,(#27030,#27031,#27032,#27033,#27034,
#27035,#27036,#27037,#27038,#27039,#27040,#27041,#27042,#27043,#27044,#27045,
#27046,#27047,#27048,#27049,#27050,#27051,#27052,#27053,#27054,#27055,#27056,
#27057,#27058,#27059,#27060,#27061,#27062,#27063,#27064,#27065,#27066,#27067,
#27068,#27069,#27070,#27071,#27072,#27073,#27074,#27075,#27076,#27077,#27078,
#27079,#27080,#27081,#27082,#27083,#27084,#27085,#27086,#27087,#27088,#27089,
#27090,#27091,#27092,#27093,#27094,#27095,#27096,#27097,#27098,#27099,#27100,
#27101,#27102,#27103,#27104,#27105,#27106,#27107,#27108,#27109,#27110,#27111,
#27112,#27113,#27114,#27115,#27116,#27117,#27118,#27119,#27120,#27121,#27122,
#27123,#27124,#27125,#27126,#27127,#27128,#27129,#27130,#27131,#27132,#27133,
#27134,#27135,#27136,#27137,#27138,#27139,#27140,#27141,#27142,#27143,#27144,
#27145,#27146,#27147,#27148,#27149,#27150,#27151,#27152,#27153,#27154,#27155,
#27156,#27157,#27158,#27159,#27160,#27161,#27162,#27163,#27164,#27165,#27166,
#27167,#27168,#27169,#27170,#27171,#27172,#27173,#27174,#27175,#27176,#27177,
#27178,#27179,#27180,#27181,#27182,#27183,#27184,#27185,#27186,#27187,#27188,
#27189,#27190,#27191,#27192,#27193,#27194,#27195,#27196,#27197,#27198,#27199,
#27200,#27201,#27202,#27203,#27204,#27205,#27206,#27207,#27208,#27209,#27210,
#27211,#27212,#27213,#27214,#27215,#27216,#27217,#27218,#27219,#27220,#27221,
#27222,#27223,#27224,#27225,#27226,#27227,#27228,#27229,#27230,#27231,#27232,
#27233,#27234,#27235,#27236,#27237,#27238,#27239,#27240,#27241,#27242,#27243,
#27244,#27245,#27246,#27247,#27248,#27249,#27250,#27251,#27252,#27253,#27254,
#27255,#27256,#27257,#27258,#27259,#27260,#27261,#27262,#27263,#27264,#27265,
#27266,#27267,#27268,#27269,#27270,#27271,#27272,#27273,#27274,#27275,#27276,
#27277,#27278,#27279,#27280,#27281,#27282,#27283,#27284,#27285,#27286,#27287,
#27288,#27289,#27290,#27291,#27292,#27293,#27294,#27295,#27296,#27297,#27298,
#27299,#27300,#27301,#27302,#27303,#27304,#27305,#27306,#27307),
 .UNSPECIFIED.,.F.,.F.,(4,2,2,2,2,2,2,2,2,2,2,2,2,2,2,2,2,2,2,2,2,2,2,2,
2,2,2,2,2,2,2,2,2,2,2,2,2,2,2,2,2,2,2,2,2,2,2,2,2,2,2,2,2,2,2,2,2,2,2,2,
2,2,2,2,2,2,2,2,2,2,2,2,2,2,2,2,2,2,2,2,2,2,2,2,2,2,2,2,2,2,2,2,2,2,2,2,
2,2,2,2,2,2,2,2,2,2,2,2,2,2,2,2,2,2,2,2,2,2,2,2,2,2,2,2,2,2,2,2,2,2,2,2,
2,2,2,2,2,2,4),(-2.69296972658525,-2.68468620652592,-2.63352519680715,-2.6182365888233,
-2.61011838253823,-2.60879928708178,-2.60811100746982,-2.60755036311805,
-2.60689641371004,-2.60576694829455,-2.60147429737921,-2.59872629691198,
-2.59720788919815,-2.59566566349393,-2.50120186431907,-2.4780487026467,
-2.45373803643959,-2.44905109680547,-2.4478285730644,-2.44685846506811,
-2.44587051189853,-2.44487845943118,-2.4431884798215,-2.43824264444029,
-2.35786091843149,-2.33341673362223,-2.28759442114962,-2.2858703351091,
-2.28510250368146,-2.28453250266342,-2.2839973924358,-2.28325260083479,
-2.28132532815549,-2.25432165401615,-2.16470364356597,-2.13990040469293,
-2.12715509849113,-2.12487339187887,-2.12365553594263,-2.12274813961794,
-2.12175690076819,-2.1200029257124,-2.11484773872556,-2.03124541945865,
-2.01978652501483,-1.96653518848808,-1.96329838690281,-1.96227344424423,
-1.96171189357669,-1.96115053236802,-1.96045052999302,-1.95907512181122,
-1.94947742453603,-1.92527915279096,-1.80913421109112,-1.80310822712246,
-1.80124104596287,-1.80022711855255,-1.79922223566509,-1.79799996208462,
-1.7956969696173,-1.78250668904225,-1.76043456294154,-1.71524525396862,
-1.64429818254088,-1.64025784649695,-1.63915396906366,-1.63850607627418,
-1.63795617911194,-1.63728022051704,-1.63654839176301,-1.63538717231963,
-1.63314907708181,-1.61182682690689,-1.58813702575893,-1.48597514754955,
-1.48000520119616,-1.47814498336495,-1.4771325149925,-1.47612760739122,
-1.47490317346367,-1.47258972709476,-1.45917379146959,-1.45617966016763,
-1.417751180141,-1.32200936824588,-1.31721589594803,-1.31614425704099,-1.31544728125959,
-1.31489881552251,-1.31426988132161,-1.3136038726633,-1.31259948926256,
-1.3107688116457,-1.29565720447254,-1.27595610282393,-1.18645218391262,
-1.15888713637253,-1.15612957322812,-1.15478234103768,-1.15381850215633,
-1.1529033248201,-1.15162331684002,-1.14904229011477,-1.12784712069007,
-1.09276110614157,-1.01015758496455,-0.994982195665562,-0.993444778731139,
-0.992694452782116,-0.992157914440362,-0.991600267651387,-0.990859872937615,
-0.990038966680772,-0.988663745114621,-0.985842831217513,-0.978366231558549,
-0.947222800880595,-0.840039543798158,-0.833793577999617,-0.831900024574466,
-0.830880827702061,-0.829885994805833,-0.828676512595485,-0.826433051695557,
-0.814426316917824,-0.790752097293392,-0.775497557761709,-0.76404449059069,
-0.675783404928685,-0.670986130144879,-0.669914221039829,-0.669217174634,
-0.668688996514639,-0.668066653879922,-0.667027732648787,-0.665779053523944,
-0.663306456513448,-0.661993518361974),.UNSPECIFIED.);
#157=B_SPLINE_CURVE_WITH_KNOTS('',3,(#27312,#27313,#27314,#27315,#27316,
#27317,#27318,#27319,#27320,#27321,#27322,#27323,#27324,#27325,#27326,#27327,
#27328,#27329,#27330,#27331,#27332,#27333,#27334,#27335,#27336,#27337,#27338,
#27339,#27340,#27341,#27342,#27343,#27344,#27345,#27346,#27347,#27348,#27349,
#27350,#27351,#27352,#27353,#27354,#27355,#27356,#27357,#27358,#27359,#27360,
#27361,#27362,#27363,#27364,#27365,#27366,#27367,#27368,#27369,#27370,#27371,
#27372,#27373,#27374,#27375,#27376,#27377,#27378,#27379,#27380,#27381,#27382,
#27383,#27384,#27385,#27386,#27387,#27388,#27389,#27390,#27391,#27392,#27393,
#27394,#27395,#27396,#27397,#27398,#27399,#27400,#27401,#27402,#27403,#27404,
#27405,#27406,#27407,#27408,#27409,#27410,#27411,#27412,#27413,#27414,#27415,
#27416,#27417,#27418,#27419,#27420,#27421,#27422,#27423,#27424,#27425,#27426,
#27427,#27428,#27429,#27430,#27431,#27432,#27433,#27434,#27435,#27436,#27437,
#27438,#27439,#27440,#27441,#27442,#27443,#27444,#27445,#27446,#27447,#27448,
#27449,#27450,#27451,#27452,#27453,#27454,#27455,#27456,#27457,#27458,#27459,
#27460,#27461,#27462,#27463,#27464,#27465,#27466,#27467,#27468,#27469,#27470,
#27471,#27472,#27473,#27474,#27475,#27476,#27477,#27478,#27479,#27480,#27481,
#27482,#27483,#27484,#27485,#27486,#27487,#27488,#27489,#27490,#27491,#27492,
#27493,#27494,#27495,#27496,#27497,#27498,#27499,#27500,#27501,#27502,#27503,
#27504,#27505,#27506,#27507,#27508,#27509,#27510,#27511,#27512,#27513,#27514,
#27515,#27516,#27517,#27518,#27519,#27520,#27521,#27522,#27523,#27524,#27525,
#27526,#27527,#27528,#27529,#27530,#27531,#27532,#27533,#27534,#27535,#27536,
#27537,#27538,#27539,#27540,#27541,#27542,#27543,#27544,#27545,#27546,#27547,
#27548,#27549,#27550,#27551,#27552,#27553,#27554,#27555,#27556,#27557,#27558,
#27559,#27560,#27561,#27562,#27563,#27564,#27565,#27566,#27567,#27568,#27569,
#27570,#27571,#27572,#27573,#27574,#27575,#27576,#27577,#27578,#27579,#27580,
#27581,#27582,#27583,#27584,#27585,#27586,#27587,#27588,#27589,#27590,#27591,
#27592,#27593,#27594,#27595,#27596,#27597,#27598,#27599,#27600,#27601,#27602,
#27603,#27604,#27605,#27606,#27607,#27608,#27609,#27610,#27611,#27612,#27613,
#27614,#27615,#27616,#27617,#27618,#27619,#27620,#27621,#27622,#27623,#27624,
#27625,#27626,#27627,#27628,#27629,#27630,#27631,#27632,#27633,#27634,#27635,
#27636,#27637,#27638,#27639),.UNSPECIFIED.,.F.,.F.,(4,2,2,2,2,2,2,2,2,2,
2,2,2,2,2,2,2,2,2,2,2,2,2,2,2,2,2,2,2,2,2,2,2,2,2,2,2,2,2,2,2,2,2,2,2,2,
2,2,2,2,2,2,2,2,2,2,2,2,2,2,2,2,2,2,2,2,2,2,2,2,2,2,2,2,2,2,2,2,2,2,2,2,
2,2,2,2,2,2,2,2,2,2,2,2,2,2,2,2,2,2,2,2,2,2,2,2,2,2,2,2,2,2,2,2,2,2,2,2,
2,2,2,2,2,2,2,2,2,2,2,2,2,2,2,2,2,2,2,2,2,2,2,2,2,2,2,2,2,2,2,2,2,2,2,2,
2,2,2,2,2,2,2,2,2,4),(-3.4002569369755,-3.38093995940539,-3.37341079928351,
-3.37008548941887,-3.36750340359851,-3.3662285434227,-3.36525601960506,
-3.36428900049934,-3.36292924331676,-3.36011998148307,-3.35252177029656,
-3.35071066604326,-3.34864899011589,-3.34815750990674,-3.34732539752986,
-3.34525421173314,-3.34416589161872,-3.34291406015038,-3.3385200749501,
-3.32571359872987,-3.24124747164086,-3.21009659761013,-3.20589763438741,
-3.20481768677689,-3.20418170915364,-3.20361946518758,-3.20290696255715,
-3.20151596137098,-3.19366591882803,-3.19171327653128,-3.18898195229666,
-3.1272665039378,-3.07498842346378,-3.05634890687441,-3.04982044030199,
-3.04682958654872,-3.04446180850954,-3.04323147190637,-3.0423199323534,
-3.04134703805543,-3.03996587873886,-3.03622444786655,-2.97548396196246,
-2.88655186498026,-2.88283016006228,-2.88179472278712,-2.88116864984802,
-2.88060437268379,-2.87987458188804,-2.8783506817698,-2.86820839051684,
-2.86594505042802,-2.86546547661213,-2.86349671000043,-2.86268981598813,
-2.8595505643578,-2.81731343944554,-2.75442024638738,-2.72749737034993,
-2.7241745247365,-2.72159231182345,-2.72031810304185,-2.71934503212131,
-2.71837733333718,-2.71701560673443,-2.71419898711682,-2.68420888765903,
-2.6068255610027,-2.58369538013232,-2.56793273690783,-2.56035389617473,
-2.55905896442276,-2.55837592846615,-2.55782095464187,-2.55716510355392,
-2.55602688873731,-2.55164248460288,-2.54899972179354,-2.5474772056455,
-2.54629161904587,-2.51528661276665,-2.44232825266544,-2.42642243784693,
-2.40386603522981,-2.40087015809707,-2.39849729139373,-2.39726664838713,
-2.39635494364062,-2.39538189007008,-2.39371840535778,-2.38918472862111,
-2.38341325011321,-2.38227032591378,-2.38088439264233,-2.37894305518372,
-2.37837562470634,-2.37628840720606,-2.37481979235509,-2.37361387204093,
-2.37210375379169,-2.36686026009919,-2.36001768813458,-2.32940600358046,
-2.30747938817261,-2.2608147556054,-2.24021800829072,-2.23691007142292,
-2.23591792270941,-2.2353015473718,-2.23473455926844,-2.23399774126582,
-2.23245362832372,-2.22137477363897,-2.12964916937907,-2.09807296602918,
-2.07816049228507,-2.0756138393405,-2.07434091796376,-2.07342689973637,
-2.07246068343944,-2.07110427940657,-2.0683091308718,-2.03921450140264,
-2.03134310858651,-1.93917165727649,-1.91531810570055,-1.91344486421595,
-1.91270927362096,-1.91217668778318,-1.91160535625868,-1.91082892035555,
-1.9090566328447,-1.87295494700478,-1.78354673816582,-1.75586814299778,
-1.7528013317979,-1.75156511164259,-1.75053608091139,-1.74948244328074,
-1.74794711719066,-1.74391133762156,-1.68918390093871,-1.59594390177468,
-1.59107756364401,-1.59000005870167,-1.58930125992211,-1.58875278979557,
-1.58819081722363,-1.58719764503819,-1.5860163442883,-1.58372488918079,
-1.50003354017457,-1.47220520921794,-1.4667337350966,-1.45456638542023,
-1.4326801241291,-1.42966674982342,-1.42831771091131,-1.42729492657737,
-1.42621188405194,-1.42454018554547,-1.41952611685813,-1.39241695924802,
-1.37023206616483),.UNSPECIFIED.);
#158=B_SPLINE_CURVE_WITH_KNOTS('',3,(#27641,#27642,#27643,#27644,#27645,
#27646,#27647,#27648,#27649,#27650,#27651,#27652,#27653,#27654,#27655,#27656,
#27657,#27658,#27659,#27660,#27661,#27662,#27663,#27664,#27665,#27666,#27667,
#27668,#27669,#27670,#27671,#27672,#27673,#27674,#27675,#27676,#27677,#27678,
#27679,#27680,#27681,#27682,#27683,#27684,#27685,#27686,#27687,#27688,#27689,
#27690,#27691,#27692,#27693,#27694,#27695,#27696,#27697,#27698,#27699,#27700,
#27701,#27702,#27703,#27704,#27705,#27706,#27707,#27708,#27709,#27710,#27711,
#27712,#27713,#27714,#27715,#27716,#27717,#27718,#27719,#27720,#27721,#27722,
#27723,#27724,#27725,#27726,#27727,#27728,#27729,#27730,#27731,#27732,#27733,
#27734,#27735,#27736,#27737,#27738,#27739,#27740,#27741,#27742,#27743,#27744,
#27745,#27746,#27747,#27748,#27749,#27750,#27751,#27752,#27753,#27754,#27755,
#27756),.UNSPECIFIED.,.F.,.F.,(4,2,2,2,2,2,2,2,2,2,2,2,2,2,2,2,2,2,2,2,
2,2,2,2,2,2,2,2,2,2,2,2,2,2,2,2,2,2,2,2,2,2,2,2,2,2,2,2,2,2,2,2,2,2,2,2,
2,4),(-0.661993518361974,-0.657056024906029,-0.64455550155935,-0.631528307324102,
-0.591945605773106,-0.539939346178486,-0.531487654507164,-0.528148183098432,
-0.512107096918439,-0.509475892209214,-0.508185732301801,-0.507174903091217,
-0.506054747920254,-0.504216490000417,-0.497741670140338,-0.456782010869626,
-0.444732500093355,-0.435274402998439,-0.427447812110566,-0.420777149300173,
-0.414980685938955,-0.409870138691596,-0.360774216062856,-0.348778831212832,
-0.347178811475139,-0.346442246396423,-0.345875244647594,-0.34527101670619,
-0.344326148893519,-0.343203655121641,-0.3410677203874,-0.33594243601775,
-0.320357196401774,-0.298962932460557,-0.19388969406574,-0.187752934782705,
-0.185872464077233,-0.184855930337792,-0.183851358010691,-0.182633624223373,
-0.180351526931455,-0.167588943195702,-0.14278596003204,-0.0460035589539252,
-0.0424290591130526,-0.0419995758919044,-0.0401952507269741,-0.0397605070169934,
-0.0375005820256303,-0.0255868872461024,-0.0239899666073891,-0.0232539826081721,
-0.0226870666209287,-0.0221619295362122,-0.0215553304639403,-0.0206945042194828,
-0.0192219951723436,-0.000960706335596301),.UNSPECIFIED.);
#159=B_SPLINE_CURVE_WITH_KNOTS('',3,(#27757,#27758,#27759,#27760,#27761,
#27762,#27763,#27764,#27765,#27766,#27767,#27768,#27769,#27770,#27771,#27772,
#27773,#27774,#27775,#27776,#27777,#27778,#27779,#27780,#27781,#27782,#27783,
#27784,#27785,#27786,#27787,#27788,#27789,#27790,#27791,#27792,#27793,#27794,
#27795,#27796,#27797,#27798,#27799,#27800,#27801,#27802,#27803,#27804,#27805,
#27806,#27807,#27808,#27809,#27810,#27811,#27812,#27813,#27814,#27815,#27816,
#27817,#27818,#27819,#27820,#27821,#27822,#27823,#27824,#27825,#27826,#27827,
#27828,#27829,#27830,#27831,#27832,#27833,#27834,#27835,#27836,#27837,#27838,
#27839,#27840,#27841,#27842,#27843,#27844,#27845,#27846,#27847,#27848,#27849,
#27850,#27851,#27852,#27853,#27854,#27855,#27856,#27857,#27858,#27859,#27860,
#27861,#27862,#27863,#27864,#27865,#27866,#27867,#27868,#27869,#27870,#27871,
#27872,#27873,#27874,#27875,#27876,#27877,#27878,#27879,#27880,#27881,#27882,
#27883,#27884,#27885,#27886,#27887,#27888,#27889,#27890,#27891,#27892,#27893,
#27894,#27895,#27896,#27897,#27898),.UNSPECIFIED.,.F.,.F.,(4,3,3,3,3,3,
3,3,3,3,3,3,3,3,3,3,3,3,3,3,3,3,3,3,3,3,3,3,3,3,3,3,3,3,3,3,3,3,3,3,3,3,
3,3,3,3,3,4),(235.619449019477,235.711588498819,235.803608643581,235.897034026776,
235.988906495499,236.080753124543,236.172599664933,236.267202675985,236.359179201164,
236.455095455154,236.551011709143,236.644084653419,236.737031493056,236.829879864241,
236.922660368896,237.015405691053,237.108140656154,237.200890074495,237.29373871523,
237.386639155842,237.479695051926,237.550726364616,237.643799308892,237.736746148529,
237.829594519714,237.922375024369,238.015120346525,238.107855311627,238.200604729968,
238.293453370703,238.386353811314,238.479409707399,238.550441020089,238.643513964365,
238.736460804002,238.829309175187,238.922089679842,239.014835001998,239.1075699671,
239.200319385441,239.293168026176,239.386068466788,239.479124362872,239.550155675562,
239.643215759794,239.736165073806,239.829009492343,239.856887423777),
 .UNSPECIFIED.);
#160=B_SPLINE_CURVE_WITH_KNOTS('',3,(#27904,#27905,#27906,#27907,#27908,
#27909,#27910,#27911,#27912,#27913,#27914,#27915,#27916,#27917,#27918,#27919,
#27920,#27921,#27922,#27923,#27924,#27925,#27926,#27927,#27928,#27929,#27930,
#27931,#27932,#27933,#27934,#27935,#27936,#27937,#27938,#27939,#27940,#27941,
#27942,#27943,#27944,#27945,#27946,#27947,#27948,#27949,#27950,#27951,#27952,
#27953,#27954,#27955,#27956,#27957,#27958,#27959,#27960,#27961,#27962,#27963,
#27964,#27965,#27966,#27967,#27968,#27969,#27970,#27971,#27972,#27973,#27974,
#27975,#27976,#27977,#27978,#27979,#27980,#27981,#27982,#27983,#27984,#27985,
#27986,#27987,#27988,#27989,#27990,#27991,#27992,#27993,#27994,#27995,#27996,
#27997,#27998,#27999,#28000,#28001,#28002,#28003,#28004,#28005,#28006,#28007,
#28008,#28009,#28010,#28011,#28012,#28013,#28014,#28015,#28016,#28017,#28018,
#28019,#28020,#28021,#28022,#28023,#28024,#28025,#28026,#28027,#28028,#28029,
#28030,#28031,#28032,#28033,#28034,#28035,#28036,#28037,#28038,#28039,#28040,
#28041,#28042,#28043,#28044,#28045,#28046,#28047,#28048,#28049,#28050,#28051,
#28052,#28053,#28054,#28055,#28056,#28057,#28058,#28059,#28060,#28061,#28062,
#28063,#28064,#28065,#28066,#28067,#28068,#28069,#28070,#28071,#28072,#28073,
#28074,#28075,#28076,#28077,#28078,#28079,#28080,#28081,#28082,#28083,#28084,
#28085,#28086,#28087),.UNSPECIFIED.,.F.,.F.,(4,2,2,2,2,2,2,2,2,2,2,2,2,
2,2,2,2,2,2,2,2,2,2,2,2,2,2,2,2,2,2,2,2,2,2,2,2,2,2,2,2,2,2,2,2,2,2,2,2,
2,2,2,2,2,2,2,2,2,2,2,2,2,2,2,2,2,2,2,2,2,2,2,2,2,2,2,2,2,2,2,2,2,2,2,2,
2,2,2,2,2,2,4),(-1.36964518659505,-1.35975521995957,-1.25221247044986,-1.24603872561589,
-1.24415411894559,-1.24313691849069,-1.24214228601081,-1.24095509171357,
-1.23878819228145,-1.23610249248161,-1.18418133570106,-1.0881222005116,
-1.08323509407694,-1.08215611015818,-1.08145694932376,-1.08089586817511,
-1.08025084420382,-1.07913035277394,-1.07444586256288,-1.0545836011284,
-1.03077005348896,-0.944693752867164,-0.942787746443107,-0.941588893058248,
-0.939578726665857,-0.937511240345363,-0.924055961152037,-0.921815410778207,
-0.920481349241073,-0.919461342314697,-0.918394920738009,-0.916858606550287,
-0.912394283568249,-0.905830187262344,-0.887052510767496,-0.839181454072609,
-0.764565146174441,-0.760194084514816,-0.759057295142652,-0.758401839851488,
-0.757846942006245,-0.757163679609985,-0.755867361496471,-0.748254899327575,
-0.732478997414089,-0.685667855198492,-0.630631190666143,-0.602098458404161,
-0.599008170200547,-0.597768149156477,-0.596738189390438,-0.595792210724733,
-0.594370217201789,-0.591018276918166,-0.586425405027232,-0.57480665890243,
-0.549957270598971,-0.522968189632089,-0.448420917945021,-0.437954453149053,
-0.436569588387037,-0.435857850159551,-0.435331463641723,-0.434755492389919,
-0.433952955921809,-0.432030899990704,-0.429382296803235,-0.400754802601841,
-0.361553413704037,-0.342067093199293,-0.315265346544721,-0.279490054839314,
-0.276289555008935,-0.274997477411947,-0.27404817323545,-0.273087522243546,
-0.272090563374284,-0.270785302315558,-0.265101133131289,-0.23845151304283,
-0.219045845906396,-0.124622635263907,-0.122570917098694,-0.114777439237883,
-0.11338936113078,-0.112677364559283,-0.112115021162796,-0.111478389864372,
-0.110396057690462,-0.10617244933288,-0.0746703960157407,-0.000962444157103762),
 .UNSPECIFIED.);
#161=B_SPLINE_CURVE_WITH_KNOTS('',3,(#28088,#28089,#28090,#28091,#28092,
#28093,#28094,#28095,#28096,#28097,#28098,#28099,#28100,#28101,#28102,#28103,
#28104,#28105,#28106,#28107,#28108,#28109,#28110,#28111,#28112,#28113,#28114,
#28115,#28116,#28117,#28118,#28119,#28120,#28121,#28122,#28123,#28124,#28125,
#28126,#28127,#28128,#28129,#28130,#28131,#28132,#28133,#28134,#28135,#28136,
#28137,#28138,#28139,#28140,#28141,#28142,#28143,#28144,#28145,#28146,#28147,
#28148,#28149,#28150,#28151,#28152,#28153,#28154,#28155,#28156,#28157,#28158,
#28159,#28160,#28161,#28162,#28163,#28164,#28165,#28166,#28167,#28168,#28169,
#28170,#28171,#28172,#28173,#28174,#28175,#28176,#28177,#28178,#28179,#28180,
#28181,#28182,#28183,#28184,#28185,#28186,#28187,#28188,#28189),
 .UNSPECIFIED.,.F.,.F.,(4,2,2,2,2,2,2,2,2,2,2,2,2,2,2,2,2,2,2,2,2,2,2,2,
2,2,2,2,2,2,2,2,2,2,2,2,2,2,2,2,2,2,2,2,2,2,2,2,2,2,4),(-4.0614126760776,
-4.01647200025967,-4.0144111607206,-4.0131061350028,-4.01210939553672,-4.01114902005165,
-4.0101999949457,-4.00890840447316,-4.00570965605267,-3.96998663233961,
-3.96536191495626,-3.9595499448839,-3.87547234980412,-3.85483521113081,
-3.85152352851727,-3.85053106586202,-3.84991468297022,-3.84934781966848,
-3.84861134456723,-3.84701116741295,-3.84291310887089,-3.75497311112632,
-3.738950535384,-3.70704022945973,-3.69749140593914,-3.69352252020025,-3.69052237851775,
-3.68945430605423,-3.68851316880395,-3.68749360677421,-3.68616216852436,
-3.68334973942876,-3.66229340280372,-3.65983042983541,-3.6432968181915,
-3.59526136873034,-3.58958945602919,-3.58301287211838,-3.57520788600347,
-3.5655369517722,-3.53009789336455,-3.52820904759051,-3.5274122765838,-3.52683745477759,
-3.52630995777336,-3.52559359698803,-3.5241905155016,-3.51324216205479,
-3.43936917897931,-3.40340392295659,-3.4002569369755),.UNSPECIFIED.);
#162=B_SPLINE_CURVE_WITH_KNOTS('',3,(#28191,#28192,#28193,#28194,#28195,
#28196,#28197,#28198,#28199,#28200,#28201,#28202,#28203,#28204,#28205,#28206,
#28207,#28208,#28209,#28210,#28211,#28212,#28213,#28214,#28215,#28216,#28217,
#28218,#28219,#28220,#28221,#28222,#28223,#28224,#28225,#28226,#28227,#28228,
#28229,#28230,#28231,#28232,#28233,#28234,#28235,#28236,#28237,#28238,#28239,
#28240,#28241,#28242,#28243,#28244,#28245,#28246,#28247,#28248,#28249,#28250,
#28251,#28252,#28253,#28254,#28255,#28256,#28257,#28258,#28259,#28260),
 .UNSPECIFIED.,.F.,.F.,(4,3,3,3,3,3,3,3,3,3,3,3,3,3,3,3,3,3,3,3,3,3,3,4),
(239.856887423777,239.949654754809,240.042394360245,240.135131058889,240.227889660377,
240.320751501073,240.413671838076,240.50673938925,240.549870331035,240.642943275311,
240.735890114948,240.828738486133,240.921518990788,241.014264312944,241.106999278045,
241.199748696387,241.292597337122,241.385497777733,241.478553673818,241.549584986507,
241.656946697205,241.763846790162,241.869934978222,241.902634326219),
 .UNSPECIFIED.);
#163=B_SPLINE_CURVE_WITH_KNOTS('',3,(#28261,#28262,#28263,#28264,#28265,
#28266,#28267,#28268,#28269,#28270,#28271,#28272,#28273,#28274,#28275,#28276,
#28277,#28278,#28279,#28280,#28281,#28282,#28283,#28284,#28285,#28286,#28287,
#28288,#28289,#28290,#28291,#28292,#28293,#28294,#28295,#28296,#28297,#28298,
#28299,#28300,#28301,#28302,#28303,#28304,#28305,#28306,#28307,#28308,#28309,
#28310,#28311,#28312,#28313,#28314,#28315,#28316,#28317,#28318,#28319,#28320,
#28321,#28322,#28323,#28324,#28325,#28326,#28327,#28328,#28329,#28330,#28331,
#28332,#28333,#28334,#28335,#28336,#28337,#28338,#28339,#28340,#28341,#28342,
#28343,#28344,#28345,#28346,#28347,#28348,#28349,#28350,#28351,#28352,#28353,
#28354,#28355,#28356,#28357,#28358,#28359,#28360,#28361,#28362,#28363,#28364,
#28365,#28366,#28367,#28368,#28369,#28370,#28371,#28372,#28373,#28374,#28375,
#28376,#28377,#28378,#28379,#28380,#28381,#28382,#28383,#28384,#28385,#28386,
#28387,#28388,#28389,#28390,#28391,#28392,#28393,#28394,#28395,#28396,#28397,
#28398,#28399,#28400,#28401,#28402,#28403,#28404,#28405,#28406,#28407,#28408,
#28409,#28410,#28411,#28412,#28413,#28414,#28415,#28416,#28417,#28418,#28419,
#28420,#28421,#28422,#28423,#28424,#28425,#28426,#28427,#28428,#28429,#28430,
#28431,#28432,#28433,#28434,#28435,#28436,#28437,#28438,#28439,#28440,#28441,
#28442,#28443,#28444,#28445,#28446,#28447,#28448,#28449,#28450,#28451,#28452,
#28453,#28454,#28455,#28456,#28457,#28458,#28459,#28460,#28461,#28462,#28463,
#28464,#28465,#28466,#28467,#28468,#28469,#28470,#28471,#28472,#28473,#28474,
#28475,#28476,#28477,#28478,#28479,#28480,#28481,#28482,#28483,#28484),
 .UNSPECIFIED.,.F.,.F.,(4,2,2,2,2,2,2,2,2,2,2,2,2,2,2,2,2,2,2,2,2,2,2,2,
2,2,2,2,2,2,2,2,2,2,2,2,2,2,2,2,2,2,2,2,2,2,2,2,2,2,2,2,2,2,2,2,2,2,2,2,
2,2,2,2,2,2,2,2,2,2,2,2,2,2,2,2,2,2,2,2,2,2,2,2,2,2,2,2,2,2,2,2,2,2,2,2,
2,2,2,2,2,2,2,2,2,2,2,2,2,2,2,4),(-4.06280686652475,-4.02033455512575,-4.01828026331028,
-4.01697778898361,-4.01598168379191,-4.01502005815009,-4.01406936210687,
-4.01277240793497,-4.01021522245632,-3.98937646105168,-3.97187848069651,
-3.9661173537507,-3.89668375234783,-3.85664369166857,-3.85489375311297,
-3.85412125783269,-3.85355051365799,-3.85301674460424,-3.85227690920787,
-3.85078183068219,-3.83709118141168,-3.83619183631263,-3.83528921572824,
-3.83383899752311,-3.8322731292852,-3.7529103983421,-3.73382734546682,-3.70906060048441,
-3.69624899056542,-3.69397108344244,-3.69297442645236,-3.69201320003456,
-3.69106311636581,-3.68976854274453,-3.6865545855394,-3.65016425872698,
-3.60234397955488,-3.59686443417707,-3.59056616260913,-3.58318894624673,
-3.55843308008148,-3.53594786162888,-3.53245862649552,-3.53144680872277,
-3.53082595530709,-3.53026019415803,-3.52953221008705,-3.52833383921899,
-3.52173355676252,-3.51997444106321,-3.51898482182036,-3.44233812414972,
-3.40697939713944,-3.38461269742447,-3.37710900162285,-3.37379170851011,
-3.37121417009501,-3.36994010590472,-3.36896674987163,-3.36799871662067,
-3.36663613852138,-3.36381652041266,-3.33371356198764,-3.25484073651609,
-3.24406671242419,-3.22858395719762,-3.21608630485069,-3.20983721983953,
-3.20861077935588,-3.20794235949533,-3.20743759628141,-3.20687258857956,
-3.20583037495989,-3.20245342949653,-3.1465978316981,-3.05847040457446,
-3.05275659812867,-3.05004711352875,-3.04786285490288,-3.04667219649783,
-3.04576513783412,-3.04462833392618,-3.04271571183145,-3.03630850011037,
-3.03237018918773,-3.03064550855694,-3.02802764036341,-3.02756282889643,
-2.93218027663408,-2.88761261626813,-2.88577564572208,-2.88498764372232,
-2.88441419591528,-2.88388433587575,-2.88315945905523,-2.88172374830638,
-2.86987688788731,-2.86909644032182,-2.86869496537234,-2.86771856919629,
-2.86491098912547,-2.82074618689506,-2.7580569001728,-2.73096769952892,
-2.727632340423,-2.72504194653146,-2.72376593754306,-2.72279306223058,-2.72182576120225,
-2.72046611205756,-2.71765870658509,-2.69355746220323),.UNSPECIFIED.);
#164=B_SPLINE_CURVE_WITH_KNOTS('',3,(#28489,#28490,#28491,#28492,#28493,
#28494,#28495,#28496,#28497,#28498,#28499,#28500,#28501,#28502,#28503,#28504,
#28505,#28506,#28507,#28508,#28509,#28510,#28511,#28512,#28513,#28514,#28515,
#28516,#28517,#28518,#28519,#28520,#28521,#28522,#28523,#28524,#28525,#28526,
#28527,#28528,#28529,#28530,#28531,#28532,#28533,#28534,#28535,#28536,#28537,
#28538,#28539,#28540,#28541,#28542,#28543,#28544,#28545,#28546,#28547,#28548,
#28549,#28550,#28551,#28552,#28553,#28554,#28555,#28556,#28557,#28558,#28559,
#28560,#28561,#28562,#28563,#28564,#28565,#28566,#28567,#28568,#28569,#28570,
#28571,#28572,#28573,#28574,#28575,#28576,#28577,#28578,#28579,#28580,#28581,
#28582,#28583,#28584,#28585,#28586,#28587,#28588,#28589,#28590,#28591,#28592,
#28593,#28594,#28595,#28596,#28597,#28598,#28599,#28600,#28601,#28602,#28603,
#28604,#28605,#28606,#28607,#28608,#28609,#28610,#28611,#28612,#28613,#28614,
#28615,#28616,#28617,#28618,#28619,#28620,#28621,#28622,#28623,#28624,#28625,
#28626,#28627,#28628,#28629,#28630,#28631,#28632,#28633,#28634,#28635,#28636,
#28637,#28638,#28639,#28640,#28641,#28642,#28643,#28644,#28645,#28646,#28647,
#28648,#28649,#28650,#28651,#28652,#28653,#28654,#28655,#28656,#28657,#28658,
#28659,#28660,#28661,#28662,#28663,#28664,#28665,#28666,#28667,#28668,#28669,
#28670,#28671,#28672,#28673,#28674,#28675,#28676,#28677,#28678,#28679,#28680,
#28681,#28682,#28683,#28684,#28685,#28686,#28687,#28688,#28689,#28690,#28691,
#28692,#28693,#28694,#28695,#28696,#28697,#28698,#28699,#28700,#28701,#28702,
#28703,#28704,#28705,#28706,#28707,#28708,#28709,#28710,#28711,#28712,#28713,
#28714,#28715,#28716,#28717,#28718,#28719,#28720,#28721,#28722,#28723,#28724,
#28725,#28726,#28727,#28728,#28729,#28730,#28731,#28732,#28733,#28734,#28735,
#28736,#28737,#28738,#28739,#28740,#28741,#28742,#28743,#28744,#28745,#28746,
#28747,#28748,#28749,#28750,#28751,#28752,#28753,#28754,#28755,#28756,#28757,
#28758,#28759,#28760,#28761,#28762,#28763,#28764,#28765,#28766,#28767,#28768,
#28769,#28770,#28771,#28772,#28773,#28774,#28775,#28776,#28777,#28778,#28779,
#28780,#28781,#28782,#28783,#28784,#28785,#28786,#28787,#28788,#28789,#28790,
#28791,#28792,#28793,#28794,#28795,#28796,#28797,#28798,#28799,#28800,#28801,
#28802,#28803,#28804,#28805,#28806,#28807,#28808,#28809,#28810,#28811,#28812,
#28813,#28814,#28815,#28816,#28817,#28818,#28819,#28820,#28821,#28822,#28823,
#28824,#28825,#28826,#28827,#28828,#28829,#28830),.UNSPECIFIED.,.F.,.F.,
(4,2,2,2,2,2,2,2,2,2,2,2,2,2,2,2,2,2,2,2,2,2,2,2,2,2,2,2,2,2,2,2,2,2,2,
2,2,2,2,2,2,2,2,2,2,2,2,2,2,2,2,2,2,2,2,2,2,2,2,2,2,2,2,2,2,2,2,2,2,2,2,
2,2,2,2,2,2,2,2,2,2,2,2,2,2,2,2,2,2,2,2,2,2,2,2,2,2,2,2,2,2,2,2,2,2,2,2,
2,2,2,2,2,2,2,2,2,2,2,2,2,2,2,2,2,2,2,2,2,2,2,2,2,2,2,2,2,2,2,2,2,2,2,2,
2,2,2,2,2,2,2,2,2,2,2,2,2,2,2,2,2,2,2,2,2,2,2,2,2,2,2,4),(-3.39967567881543,
-3.3830953443525,-3.36505840107934,-3.35124254130715,-3.34681003894987,
-3.34394518201433,-3.34323831832382,-3.34257042209722,-3.34206574325176,
-3.34150050644599,-3.34045696262515,-3.3370684895889,-3.28345086884869,
-3.23196100923378,-3.21074239750237,-3.18738545504777,-3.18347741124127,
-3.18194673803801,-3.18089395532038,-3.17986393347204,-3.17862431948622,
-3.17553758177969,-3.14715331885114,-3.13298651681843,-3.12434090791465,
-3.07956953116939,-3.04489480200288,-3.0294959522054,-3.0217081232995,-3.02040717666493,
-3.01971722478535,-3.01921061360912,-3.01865800942075,-3.01767709244384,
-3.01477412252933,-2.96708900932264,-2.8955753256884,-2.87329328342076,
-2.86188973755712,-2.85968533238123,-2.85847452284638,-2.85756792346845,
-2.85642802281662,-2.85450134444521,-2.84797136152875,-2.84409236979748,
-2.84009737720496,-2.83962227563945,-2.83751398695264,-2.83649547778602,
-2.83525627693123,-2.83282249996698,-2.82189256993927,-2.80218570973055,
-2.73266058932669,-2.70844494495866,-2.69885456085533,-2.69748390660192,
-2.69677918901473,-2.69627077366496,-2.69572500543677,-2.69494076929004,
-2.692759130891,-2.65773612233269,-2.57657039176738,-2.55177576204388,-2.53902122466936,
-2.53674608155657,-2.53551987748489,-2.53451480886989,-2.53350326935687,
-2.53164789378162,-2.52571786318746,-2.52426859443777,-2.52070525944668,
-2.51923848221267,-2.51684774587235,-2.51478463134214,-2.51306405552507,
-2.51186176783343,-2.51041499536734,-2.50414798392216,-2.49651832444404,
-2.41126865027625,-2.39815012828021,-2.38292339364967,-2.37565956109738,
-2.37441672858754,-2.37372128087645,-2.3731603308833,-2.37259644404695,
-2.37155964300261,-2.36822656639715,-2.3656046874333,-2.3639455116607,-2.32914627964105,
-2.30881886748014,-2.26924090307963,-2.22231723008055,-2.21772040054798,
-2.21434012995641,-2.21291066925041,-2.21187785023757,-2.21093756139645,
-2.20968185477298,-2.20662384807957,-2.17781148637259,-2.15938127774399,
-2.10393396551719,-2.07893568341549,-2.05581323323315,-2.05346626471223,
-2.05172077953906,-2.05094913177385,-2.05037857006137,-2.04984463929117,
-2.04910407716114,-2.04760595681434,-2.03380957435978,-2.03321213411386,
-2.0327519061593,-2.03138941978545,-2.0310974982289,-2.01059889328218,-1.91962341717732,
-1.91339744935615,-1.91176746808171,-1.91054662736731,-1.90875043988151,
-1.90666967589999,-1.90432937867575,-1.89885659743068,-1.89236855048891,
-1.8904466835123,-1.88930786558113,-1.88840114434487,-1.88718891561229,
-1.88493290446546,-1.87268923043861,-1.84851606945835,-1.80273139451716,
-1.73342268557157,-1.72940430090167,-1.72830270177766,-1.72765534317654,
-1.72709434603407,-1.72639799770446,-1.72503983562958,-1.71592347012686,
-1.69368208996812,-1.57447947769436,-1.56892555173749,-1.56711822683182,
-1.56611649987859,-1.56511053675389,-1.56389249389707,-1.56157776777885,
-1.55867147420948,-1.53726858295719,-1.51515903607891,-1.46439043804796,
-1.40947707420535,-1.40610418846373,-1.40506269379156,-1.40449795680927,
-1.40399336550636,-1.40332507474768,-1.402098570233,-1.39584303416573,-1.38332780208467,
-1.36964518659505),.UNSPECIFIED.);
#165=B_SPLINE_CURVE_WITH_KNOTS('',3,(#28831,#28832,#28833,#28834,#28835,
#28836,#28837,#28838,#28839,#28840,#28841,#28842,#28843,#28844,#28845,#28846,
#28847,#28848,#28849,#28850,#28851,#28852,#28853,#28854,#28855,#28856,#28857,
#28858,#28859,#28860,#28861,#28862,#28863,#28864,#28865,#28866,#28867,#28868,
#28869,#28870,#28871,#28872,#28873,#28874,#28875,#28876,#28877,#28878,#28879,
#28880,#28881,#28882,#28883,#28884,#28885,#28886,#28887,#28888,#28889,#28890,
#28891,#28892,#28893,#28894,#28895,#28896,#28897,#28898,#28899,#28900,#28901,
#28902,#28903,#28904,#28905,#28906,#28907,#28908,#28909,#28910,#28911,#28912,
#28913,#28914,#28915,#28916,#28917,#28918,#28919,#28920,#28921,#28922,#28923,
#28924,#28925,#28926,#28927,#28928,#28929,#28930,#28931,#28932,#28933,#28934,
#28935,#28936,#28937,#28938,#28939,#28940,#28941,#28942,#28943,#28944,#28945,
#28946,#28947,#28948,#28949,#28950,#28951,#28952,#28953,#28954,#28955,#28956,
#28957,#28958,#28959,#28960,#28961,#28962,#28963,#28964,#28965,#28966,#28967,
#28968,#28969,#28970,#28971,#28972,#28973,#28974,#28975,#28976,#28977,#28978,
#28979,#28980,#28981,#28982,#28983,#28984,#28985,#28986,#28987,#28988,#28989,
#28990,#28991,#28992,#28993,#28994,#28995,#28996,#28997,#28998,#28999,#29000,
#29001,#29002,#29003,#29004,#29005,#29006,#29007,#29008,#29009,#29010,#29011,
#29012,#29013,#29014,#29015,#29016,#29017,#29018,#29019,#29020,#29021,#29022,
#29023,#29024,#29025,#29026,#29027,#29028,#29029,#29030,#29031,#29032,#29033,
#29034,#29035,#29036,#29037,#29038,#29039,#29040,#29041,#29042,#29043,#29044,
#29045,#29046,#29047,#29048,#29049,#29050,#29051,#29052,#29053,#29054,#29055,
#29056,#29057,#29058,#29059,#29060,#29061,#29062,#29063,#29064,#29065,#29066,
#29067,#29068,#29069,#29070,#29071,#29072,#29073,#29074,#29075,#29076,#29077,
#29078,#29079,#29080,#29081,#29082,#29083,#29084,#29085,#29086,#29087,#29088,
#29089,#29090,#29091,#29092,#29093,#29094,#29095,#29096,#29097,#29098,#29099,
#29100,#29101,#29102,#29103,#29104,#29105,#29106,#29107,#29108,#29109,#29110,
#29111,#29112,#29113,#29114,#29115,#29116,#29117,#29118,#29119,#29120,#29121,
#29122,#29123,#29124,#29125,#29126,#29127,#29128,#29129,#29130,#29131,#29132),
 .UNSPECIFIED.,.F.,.F.,(4,2,2,2,2,2,2,2,2,2,2,2,2,2,2,2,2,2,2,2,2,2,2,2,
2,2,2,2,2,2,2,2,2,2,2,2,2,2,2,2,2,2,2,2,2,2,2,2,2,2,2,2,2,2,2,2,2,2,2,2,
2,2,2,2,2,2,2,2,2,2,2,2,2,2,2,2,2,2,2,2,2,2,2,2,2,2,2,2,2,2,2,2,2,2,2,2,
2,2,2,2,2,2,2,2,2,2,2,2,2,2,2,2,2,2,2,2,2,2,2,2,2,2,2,2,2,2,2,2,2,2,2,2,
2,2,2,2,2,2,2,2,2,2,2,2,2,2,2,2,2,2,4),(-2.69355746220323,-2.68808306254334,
-2.62719530091855,-2.58710670620264,-2.56655536599016,-2.56325152708279,
-2.56225965768096,-2.56164323541506,-2.56107604888027,-2.5603387592859,
-2.55910913355782,-2.55197717350271,-2.55109710005247,-2.54927839451393,
-2.51932178551233,-2.44684404078419,-2.40936417828723,-2.40531415628346,
-2.40321120527166,-2.40143490616236,-2.40033717294215,-2.39932623264292,
-2.39803595481395,-2.39540459282004,-2.37936419524275,-2.3737100390951,
-2.36230558443699,-2.33611098358868,-2.3179497229805,-2.28412447272664,
-2.25603349973043,-2.24597180476589,-2.24063821455095,-2.23946957510403,
-2.23881377634759,-2.23830960283575,-2.23773573275443,-2.23664951053699,
-2.23289464585289,-2.17257939771721,-2.12376406221615,-2.08255218915795,
-2.07938813241006,-2.07799670224624,-2.07697068689038,-2.07602205082008,
-2.07473314384821,-2.07155188620082,-2.03671642646023,-2.03227512053579,
-1.93099216521922,-1.93050906976677,-1.92819468347773,-1.91809829629106,
-1.91657600068083,-1.91585415134862,-1.91528913463021,-1.9146648421775,
-1.91363810309304,-1.91000597677765,-1.8284814678248,-1.78330370166505,
-1.77894325300126,-1.7772053427426,-1.77600942279755,-1.77280217221968,
-1.77158341580513,-1.76974774863945,-1.76855822077632,-1.76170540018213,
-1.75690003471109,-1.75519567542311,-1.75421426707334,-1.75330453315126,
-1.75206638509156,-1.74968949168405,-1.7348363538769,-1.70160248806689,
-1.5986930804288,-1.59794265375855,-1.59413772848069,-1.59304568146722,
-1.59247049595745,-1.59192115075449,-1.59126215306876,-1.59055402440825,
-1.58944956892835,-1.58736127619187,-1.5352086449426,-1.472686211226,-1.43628958236054,
-1.43307446237775,-1.43177939194847,-1.43082893312545,-1.42980354215728,
-1.42841753832034,-1.42528533507357,-1.37899662759809,-1.32804289250425,
-1.2743199967189,-1.27093233841915,-1.26988856673512,-1.26932309980844,
-1.26877313132404,-1.2680986671437,-1.26736958659043,-1.26621521988017,
-1.26399570538079,-1.24298090419219,-1.22050986619115,-1.11701857741683,
-1.11078839972635,-1.10889615890344,-1.10787691636606,-1.10688157368256,
-1.10567081170219,-1.10342304277453,-1.09134970370977,-1.06753034135642,
-1.02202868496824,-0.963425007183822,-0.96022518209887,-0.948626872810102,
-0.947199581960736,-0.946476768450457,-0.94594736424881,-0.945384821164841,
-0.944620035148599,-0.943762948896898,-0.942299833024079,-0.939231137478979,
-0.930846720530321,-0.905234721674861,-0.815350773001681,-0.809017938289967,
-0.806384931076438,-0.803358502883731,-0.801735783618388,-0.80111608468074,
-0.799073471602111,-0.797001856796111,-0.78845719154436,-0.786356191131843,
-0.785049202922835,-0.784036044018823,-0.782924271235241,-0.781124315072967,
-0.775018514762417,-0.737850470757028,-0.690261267276854,-0.66274989517157),
 .UNSPECIFIED.);
#166=B_SPLINE_CURVE_WITH_KNOTS('',3,(#29138,#29139,#29140,#29141,#29142,
#29143,#29144,#29145,#29146,#29147,#29148,#29149,#29150,#29151,#29152,#29153,
#29154,#29155,#29156,#29157,#29158,#29159,#29160,#29161,#29162,#29163,#29164,
#29165,#29166,#29167,#29168,#29169,#29170,#29171,#29172,#29173,#29174,#29175,
#29176,#29177,#29178,#29179,#29180,#29181,#29182,#29183,#29184,#29185,#29186,
#29187,#29188,#29189,#29190,#29191,#29192,#29193,#29194,#29195,#29196,#29197,
#29198,#29199,#29200,#29201,#29202,#29203,#29204,#29205,#29206,#29207,#29208,
#29209,#29210,#29211,#29212,#29213,#29214,#29215,#29216,#29217,#29218,#29219,
#29220,#29221,#29222,#29223,#29224,#29225,#29226,#29227,#29228,#29229,#29230,
#29231,#29232,#29233,#29234,#29235,#29236,#29237,#29238,#29239,#29240,#29241,
#29242,#29243,#29244,#29245,#29246,#29247,#29248,#29249,#29250,#29251,#29252,
#29253,#29254,#29255,#29256,#29257,#29258,#29259,#29260,#29261,#29262,#29263,
#29264,#29265,#29266,#29267,#29268,#29269,#29270,#29271,#29272,#29273,#29274,
#29275,#29276,#29277,#29278,#29279,#29280,#29281,#29282,#29283,#29284,#29285,
#29286,#29287,#29288,#29289,#29290,#29291,#29292,#29293,#29294,#29295,#29296,
#29297,#29298,#29299,#29300,#29301,#29302,#29303,#29304,#29305,#29306,#29307,
#29308,#29309,#29310,#29311,#29312,#29313,#29314,#29315),.UNSPECIFIED.,
 .F.,.F.,(4,2,2,2,2,2,2,2,2,2,2,2,2,2,2,2,2,2,2,2,2,2,2,2,2,2,2,2,2,2,2,
2,2,2,2,2,2,2,2,2,2,2,2,2,2,2,2,2,2,2,2,2,2,2,2,2,2,2,2,2,2,2,2,2,2,2,2,
2,2,2,2,2,2,2,2,2,2,2,2,2,2,2,2,2,2,2,2,2,4),(-1.36999387029904,-1.36038551158595,
-1.31762389844499,-1.25380100434518,-1.22391567831664,-1.22194538346997,
-1.22119375969203,-1.22065690797706,-1.22014504569075,-1.21941690416308,
-1.21793194522755,-1.20457680034161,-1.1796388353013,-1.12019064637841,
-1.06527158973772,-1.06167038334164,-1.06031142000509,-1.05934442968768,
-1.05843053403945,-1.05715914521277,-1.05469019191152,-1.03684037426563,
-1.01088149984525,-0.95016165050593,-0.902122011800938,-0.899298503146542,
-0.898328561177153,-0.897778168686198,-0.897271054294852,-0.896576618448713,
-0.895254638190057,-0.887698305568242,-0.871918434385414,-0.813991369035933,
-0.743680678251719,-0.739063303907374,-0.737387096331901,-0.736411503145224,
-0.735500551964762,-0.734250553054612,-0.732914455732495,-0.72677599850109,
-0.716915438851108,-0.683146275052802,-0.635827942009692,-0.579873465717165,
-0.576480404111557,-0.575436334007658,-0.574871006961547,-0.574366361840461,
-0.573698673410449,-0.572992097181906,-0.570128194105219,-0.542310602154769,
-0.497010928625636,-0.447298036523179,-0.418567796280074,-0.415512149567664,
-0.414256919163544,-0.413316801673658,-0.412283987369497,-0.41085419677846,
-0.409269047897842,-0.397881355157689,-0.375636457701275,-0.344808510529104,
-0.318708951535554,-0.257246151634893,-0.253628453478827,-0.252557847130535,
-0.251987161400847,-0.251432228617072,-0.25075070803629,-0.250024842406989,
-0.248877826889085,-0.235115973156202,-0.203226660131071,-0.190895198563999,
-0.177895355223375,-0.0983105449797796,-0.0933098889715865,-0.0915778119650202,
-0.0905910739618273,-0.0896829651126328,-0.0884569241156662,-0.0871540150667666,
-0.0850985267796175,-0.0705133346622887,-0.000961684070864306),
 .UNSPECIFIED.);
#167=B_SPLINE_CURVE_WITH_KNOTS('',3,(#29316,#29317,#29318,#29319,#29320,
#29321,#29322,#29323,#29324,#29325,#29326,#29327,#29328,#29329,#29330,#29331,
#29332,#29333,#29334,#29335,#29336,#29337,#29338,#29339,#29340,#29341,#29342,
#29343,#29344,#29345,#29346,#29347,#29348,#29349,#29350,#29351,#29352,#29353,
#29354,#29355,#29356,#29357,#29358,#29359,#29360,#29361,#29362,#29363,#29364,
#29365,#29366,#29367,#29368,#29369,#29370,#29371,#29372,#29373,#29374,#29375,
#29376,#29377,#29378,#29379,#29380,#29381,#29382,#29383,#29384,#29385,#29386,
#29387,#29388,#29389,#29390,#29391,#29392,#29393,#29394,#29395,#29396,#29397,
#29398,#29399,#29400,#29401,#29402,#29403,#29404,#29405,#29406,#29407),
 .UNSPECIFIED.,.F.,.F.,(4,2,2,2,2,2,2,2,2,2,2,2,2,2,2,2,2,2,2,2,2,2,2,2,
2,2,2,2,2,2,2,2,2,2,2,2,2,2,2,2,2,2,2,2,2,4),(-4.06042054730363,-4.0005922877394,
-3.99116121478614,-3.98996052414148,-3.98921216445221,-3.98851447950181,
-3.98795337919572,-3.98730698927864,-3.98620956858338,-3.98223137651607,
-3.91660742706423,-3.9025091505805,-3.88845987089132,-3.84780723330483,
-3.83107095889533,-3.82934432305439,-3.8278132670144,-3.82676039226049,
-3.82573041420785,-3.82449101440008,-3.8214056561052,-3.79307297794185,
-3.74181051804254,-3.7073756672315,-3.67843355687513,-3.66787240049278,
-3.66682003530468,-3.66613390771164,-3.66548081486157,-3.6649767453648,
-3.66440086791002,-3.66330450125364,-3.65945723082002,-3.59730971379012,
-3.54645244330157,-3.51345236418847,-3.50705908331055,-3.50570685660638,
-3.50444516776489,-3.50353259334251,-3.50256173085758,-3.50118864717936,
-3.49749964592874,-3.44158656742523,-3.42639287204158,-3.39967567881543),
 .UNSPECIFIED.);
#168=B_SPLINE_CURVE_WITH_KNOTS('',3,(#29409,#29410,#29411,#29412,#29413,
#29414,#29415,#29416,#29417,#29418,#29419,#29420,#29421,#29422,#29423,#29424,
#29425,#29426,#29427,#29428,#29429,#29430,#29431,#29432,#29433,#29434,#29435,
#29436,#29437,#29438,#29439,#29440,#29441,#29442,#29443,#29444,#29445,#29446,
#29447,#29448,#29449,#29450,#29451,#29452,#29453,#29454,#29455,#29456,#29457,
#29458,#29459,#29460,#29461,#29462,#29463,#29464,#29465,#29466,#29467,#29468,
#29469,#29470,#29471,#29472,#29473,#29474,#29475,#29476,#29477,#29478,#29479,
#29480,#29481,#29482,#29483,#29484,#29485,#29486,#29487,#29488,#29489,#29490,
#29491,#29492,#29493,#29494,#29495,#29496,#29497,#29498),.UNSPECIFIED.,
 .F.,.F.,(4,2,2,2,2,2,2,2,2,2,2,2,2,2,2,2,2,2,2,2,2,2,2,2,2,2,2,2,2,2,2,
2,2,2,2,2,2,2,2,2,2,2,2,2,4),(-0.66274989517157,-0.650332479888293,-0.626028375200515,
-0.624146309993,-0.623409073511506,-0.622875939399027,-0.62231613242395,
-0.621563469297492,-0.620725503751429,-0.619308982368471,-0.616372339296391,
-0.608475599872263,-0.588717528200964,-0.469897195849882,-0.464264192079036,
-0.462446273011553,-0.461442224522316,-0.4604362378638,-0.459196598665069,
-0.45681174857044,-0.441752122397939,-0.407709364426341,-0.36632142642992,
-0.345660776798058,-0.312286497900439,-0.302230681626929,-0.300710540127436,
-0.299989240076922,-0.299441827947265,-0.298916550261646,-0.298020513245856,
-0.295483348160206,-0.291688190419691,-0.280480244061581,-0.262474943293934,
-0.147176473275608,-0.14121527052928,-0.139356235956649,-0.138344066927424,
-0.137339237884532,-0.136114582720796,-0.13379976636545,-0.120350841565661,
-0.106877449195167,-0.0009625259518426),.UNSPECIFIED.);
#169=B_SPLINE_CURVE_WITH_KNOTS('',3,(#29499,#29500,#29501,#29502,#29503,
#29504,#29505,#29506,#29507,#29508,#29509,#29510,#29511,#29512,#29513,#29514,
#29515,#29516,#29517,#29518,#29519,#29520,#29521,#29522,#29523,#29524,#29525,
#29526,#29527,#29528,#29529,#29530,#29531,#29532,#29533,#29534,#29535,#29536,
#29537,#29538,#29539,#29540,#29541,#29542,#29543,#29544,#29545,#29546,#29547,
#29548,#29549,#29550,#29551,#29552,#29553,#29554,#29555,#29556,#29557,#29558,
#29559,#29560,#29561,#29562,#29563,#29564,#29565,#29566,#29567,#29568,#29569,
#29570,#29571,#29572,#29573,#29574,#29575,#29576,#29577,#29578,#29579,#29580,
#29581,#29582,#29583,#29584,#29585,#29586,#29587,#29588,#29589,#29590,#29591,
#29592,#29593,#29594,#29595,#29596,#29597,#29598,#29599,#29600,#29601,#29602,
#29603,#29604,#29605,#29606,#29607,#29608,#29609,#29610,#29611,#29612,#29613,
#29614,#29615,#29616,#29617,#29618,#29619,#29620,#29621,#29622,#29623,#29624,
#29625,#29626,#29627,#29628,#29629,#29630,#29631,#29632,#29633,#29634,#29635,
#29636,#29637,#29638,#29639,#29640),.UNSPECIFIED.,.F.,.F.,(4,3,3,3,3,3,
3,3,3,3,3,3,3,3,3,3,3,3,3,3,3,3,3,3,3,3,3,3,3,3,3,3,3,3,3,3,3,3,3,3,3,3,
3,3,3,3,3,4),(254.469004940774,254.545875507654,254.63894845193,254.731895291567,
254.824743662751,254.917524167407,255.010269489563,255.103004454664,255.195753873006,
255.288602513741,255.381502954352,255.474558850437,255.545590163127,255.638663107403,
255.73160994704,255.824458318225,255.91723882288,256.009984145037,256.102719110138,
256.195468528479,256.288317169214,256.381217609826,256.47427350591,256.5453048186,
256.638377762876,256.731324602513,256.824172973698,256.916953478353,257.00969880051,
257.102433765611,257.195183183952,257.288031824687,257.380932265299,257.473988161383,
257.545019474073,257.638092418349,257.731039257986,257.823887629171,257.916668133826,
258.009413455982,258.102148421083,258.194897839424,258.28774648016,258.380646920771,
258.473702816855,258.544734129546,258.637790900267,258.706503083453),
 .UNSPECIFIED.);
#170=B_SPLINE_CURVE_WITH_KNOTS('',3,(#29645,#29646,#29647,#29648,#29649,
#29650,#29651,#29652,#29653,#29654,#29655,#29656,#29657,#29658,#29659,#29660,
#29661,#29662,#29663,#29664,#29665,#29666,#29667,#29668,#29669,#29670,#29671,
#29672,#29673,#29674,#29675,#29676,#29677,#29678,#29679,#29680,#29681,#29682,
#29683,#29684,#29685,#29686,#29687,#29688,#29689,#29690,#29691,#29692,#29693,
#29694,#29695,#29696,#29697,#29698,#29699,#29700,#29701,#29702,#29703,#29704,
#29705,#29706,#29707,#29708,#29709,#29710,#29711,#29712,#29713,#29714,#29715,
#29716,#29717,#29718,#29719,#29720,#29721,#29722,#29723,#29724,#29725,#29726,
#29727,#29728,#29729,#29730,#29731,#29732,#29733,#29734,#29735,#29736,#29737,
#29738,#29739,#29740,#29741,#29742,#29743,#29744,#29745,#29746,#29747,#29748,
#29749,#29750,#29751,#29752,#29753,#29754,#29755,#29756,#29757,#29758,#29759,
#29760,#29761,#29762,#29763,#29764,#29765,#29766,#29767,#29768,#29769,#29770,
#29771,#29772,#29773,#29774,#29775,#29776,#29777,#29778,#29779,#29780,#29781,
#29782,#29783,#29784,#29785,#29786,#29787,#29788,#29789,#29790,#29791,#29792,
#29793,#29794,#29795,#29796,#29797,#29798,#29799,#29800,#29801,#29802,#29803,
#29804,#29805,#29806,#29807,#29808,#29809,#29810,#29811,#29812,#29813,#29814,
#29815,#29816,#29817,#29818,#29819,#29820,#29821,#29822,#29823,#29824,#29825,
#29826,#29827,#29828,#29829,#29830,#29831,#29832,#29833,#29834,#29835,#29836,
#29837,#29838,#29839,#29840,#29841,#29842,#29843,#29844,#29845,#29846,#29847,
#29848,#29849,#29850,#29851,#29852,#29853,#29854,#29855,#29856,#29857,#29858,
#29859,#29860,#29861,#29862,#29863,#29864,#29865,#29866,#29867,#29868,#29869,
#29870,#29871,#29872,#29873,#29874,#29875,#29876,#29877,#29878,#29879,#29880,
#29881,#29882,#29883,#29884,#29885,#29886,#29887,#29888,#29889,#29890,#29891,
#29892,#29893,#29894,#29895,#29896,#29897,#29898,#29899,#29900,#29901,#29902,
#29903,#29904,#29905,#29906,#29907,#29908,#29909,#29910,#29911,#29912,#29913,
#29914,#29915,#29916,#29917,#29918,#29919,#29920,#29921,#29922,#29923,#29924,
#29925,#29926,#29927,#29928,#29929,#29930,#29931,#29932,#29933,#29934,#29935,
#29936),.UNSPECIFIED.,.F.,.F.,(4,2,2,2,2,2,2,2,2,2,2,2,2,2,2,2,2,2,2,2,
2,2,2,2,2,2,2,2,2,2,2,2,2,2,2,2,2,2,2,2,2,2,2,2,2,2,2,2,2,2,2,2,2,2,2,2,
2,2,2,2,2,2,2,2,2,2,2,2,2,2,2,2,2,2,2,2,2,2,2,2,2,2,2,2,2,2,2,2,2,2,2,2,
2,2,2,2,2,2,2,2,2,2,2,2,2,2,2,2,2,2,2,2,2,2,2,2,2,2,2,2,2,2,2,2,2,2,2,2,
2,2,2,2,2,2,2,2,2,2,2,2,2,2,2,2,2,4),(-3.40020035460252,-3.37286992496302,
-3.33938983808234,-3.32957834964395,-3.32552806993047,-3.32250593341849,
-3.32112261612971,-3.3200980357239,-3.31914748865394,-3.31785100422736,
-3.31529554340392,-3.29450308006559,-3.2841432276615,-3.24474903084824,
-3.20284843490037,-3.17560404763391,-3.16598130893913,-3.16083249817106,
-3.15967897127555,-3.15913505007261,-3.15862603599585,-3.15808203204834,
-3.15714415144621,-3.15454198037331,-3.11289451322465,-3.05353867732869,
-3.01725699256773,-3.0016206479176,-2.99920245977703,-2.9979558462115,-2.99704525874983,
-2.99606805380082,-2.99467183376306,-2.99083453559922,-2.93240477410701,
-2.87519691964922,-2.85503013039824,-2.84373552930794,-2.83794528969366,
-2.83674856143262,-2.83620032910944,-2.83568906211055,-2.83515077738968,
-2.83439394905162,-2.83239224441933,-2.80009786213856,-2.72383646978531,
-2.69693301090561,-2.6787955560365,-2.67627113280134,-2.67500259601845,
-2.67408906614203,-2.67312090198149,-2.6717577334953,-2.6689355739256,-2.6387194190394,
-2.56737060364562,-2.51655752140246,-2.51426870371452,-2.51340942430432,
-2.51281832449685,-2.5122446247344,-2.51155264505258,-2.50982337591692,
-2.4938923087519,-2.40048234513647,-2.36082536469448,-2.35449622612228,
-2.35265922771945,-2.35153940071005,-2.3505285821419,-2.34923804218408,
-2.34660469172915,-2.33051799772303,-2.32736706143738,-2.23331025915569,
-2.20667746912396,-2.19225218253274,-2.19075225018191,-2.19002709632715,
-2.18951565801942,-2.18897768324674,-2.18822205392241,-2.18622746944434,
-2.15451950293483,-2.06903949927627,-2.03677469318652,-2.03118324905011,
-2.0294411490242,-2.02845236386875,-2.027544613661,-2.02632240888829,-2.02401993966408,
-2.01084274740894,-1.98844610656616,-1.94307710785031,-1.87253908005348,
-1.86855205930114,-1.86745368447779,-1.86680705391547,-1.86624594790404,
-1.86554851732254,-1.8641852720124,-1.85493054193059,-1.83212564149997,
-1.73549867441092,-1.7293578678983,-1.72803477100936,-1.72682910529024,
-1.72536177532305,-1.72327480512574,-1.72270859141192,-1.72075203419565,
-1.71933692420312,-1.71584673195347,-1.71442861548772,-1.70835394451707,
-1.70648085120586,-1.70546573810381,-1.70446095523809,-1.70324064220095,
-1.70099263967282,-1.68877521011319,-1.66461607915038,-1.61884322998537,
-1.55572416253681,-1.55400791951182,-1.55274686202051,-1.54788902012261,
-1.5451860328601,-1.54423316117979,-1.54368618724262,-1.54317814961806,
-1.54247625174226,-1.54111899723276,-1.53265096850607,-1.51303160234241,
-1.43383805647339,-1.38788865099564,-1.38451325687428,-1.3831913029516,
-1.38223420269518,-1.38121391678574,-1.37985597799712,-1.37696414030964,
-1.36999387029904),.UNSPECIFIED.);
#171=B_SPLINE_CURVE_WITH_KNOTS('',3,(#29938,#29939,#29940,#29941,#29942,
#29943,#29944,#29945,#29946,#29947,#29948,#29949,#29950,#29951,#29952,#29953,
#29954,#29955,#29956,#29957,#29958,#29959,#29960,#29961,#29962,#29963,#29964,
#29965,#29966,#29967,#29968,#29969,#29970,#29971,#29972,#29973,#29974,#29975,
#29976,#29977,#29978,#29979,#29980,#29981,#29982,#29983,#29984,#29985,#29986,
#29987,#29988,#29989,#29990,#29991,#29992,#29993,#29994,#29995,#29996,#29997,
#29998,#29999,#30000,#30001,#30002,#30003,#30004),.UNSPECIFIED.,.F.,.F.,
(4,3,3,3,3,3,3,3,3,3,3,3,3,3,3,3,3,3,3,3,3,3,4),(258.706503083453,258.799374498467,
258.892508784286,258.985260787678,259.077996047084,259.170739374796,259.264166727352,
259.357052077616,259.450750431317,259.544448785018,259.637521729293,259.730468568931,
259.823316940115,259.916097444771,260.008842766927,260.101577732028,260.194327150369,
260.287175791104,260.380076231715,260.4731321278,260.544163440491,260.67516406308,
260.752190247954),.UNSPECIFIED.);
#172=B_SPLINE_CURVE_WITH_KNOTS('',3,(#30005,#30006,#30007,#30008,#30009,
#30010,#30011,#30012,#30013,#30014,#30015,#30016,#30017,#30018,#30019,#30020,
#30021,#30022,#30023,#30024,#30025,#30026,#30027,#30028,#30029,#30030,#30031,
#30032,#30033,#30034,#30035,#30036,#30037,#30038,#30039,#30040,#30041,#30042,
#30043,#30044,#30045,#30046,#30047,#30048,#30049,#30050,#30051,#30052,#30053,
#30054,#30055,#30056,#30057,#30058,#30059,#30060,#30061,#30062,#30063,#30064,
#30065,#30066,#30067,#30068,#30069,#30070,#30071,#30072,#30073,#30074,#30075,
#30076,#30077,#30078,#30079,#30080,#30081,#30082,#30083,#30084,#30085,#30086,
#30087,#30088,#30089,#30090,#30091,#30092,#30093,#30094,#30095,#30096,#30097,
#30098,#30099,#30100,#30101,#30102,#30103,#30104,#30105,#30106,#30107,#30108,
#30109,#30110,#30111,#30112,#30113,#30114,#30115,#30116,#30117,#30118,#30119,
#30120,#30121,#30122,#30123,#30124,#30125,#30126,#30127,#30128,#30129,#30130,
#30131,#30132,#30133,#30134,#30135,#30136,#30137,#30138,#30139,#30140,#30141,
#30142,#30143,#30144,#30145,#30146,#30147,#30148,#30149,#30150,#30151,#30152,
#30153,#30154,#30155,#30156,#30157,#30158,#30159,#30160,#30161,#30162,#30163,
#30164,#30165,#30166,#30167,#30168,#30169,#30170,#30171,#30172,#30173,#30174,
#30175,#30176,#30177,#30178,#30179,#30180,#30181,#30182,#30183,#30184,#30185,
#30186,#30187,#30188,#30189,#30190,#30191,#30192,#30193,#30194,#30195,#30196,
#30197,#30198),.UNSPECIFIED.,.F.,.F.,(4,2,2,2,2,2,2,2,2,2,2,2,2,2,2,2,2,
2,2,2,2,2,2,2,2,2,2,2,2,2,2,2,2,2,2,2,2,2,2,2,2,2,2,2,2,2,2,2,2,2,2,2,2,
2,2,2,2,2,2,2,2,2,2,2,2,2,2,2,2,2,2,2,2,2,2,2,2,2,2,2,2,2,2,2,2,2,2,2,2,
2,2,2,2,2,2,2,4),(-4.06112921706716,-3.99952851532468,-3.98053447412182,
-3.97391345062148,-3.97089124990811,-3.96848146199215,-3.96723691515219,
-3.96624018267477,-3.96524186186338,-3.9634510376057,-3.9580211956521,-3.87425784785127,
-3.86206194772413,-3.85077444982639,-3.82185557989671,-3.80804043109872,
-3.80686960787162,-3.80613384473297,-3.80544527476301,-3.80488493760528,
-3.80431743320141,-3.80326202539012,-3.79977270101839,-3.74333468066042,
-3.7162653577986,-3.6853947360215,-3.66060802632784,-3.64785124553421,-3.64555785575898,
-3.64433783035865,-3.64343056503086,-3.6424411919896,-3.64069509869915,
-3.63559270803827,-3.55540863638263,-3.51261763606852,-3.48547780529754,
-3.48363903037883,-3.48300731859009,-3.48239252526604,-3.48182513114613,
-3.48108521897648,-3.47984613987233,-3.4725385975809,-3.47188518929711,
-3.47002180672503,-3.42594428605793,-3.37659622176019,-3.34071141219027,
-3.33047470238178,-3.32415600101936,-3.32280853346351,-3.32155036292091,
-3.32063847397662,-3.31966659723736,-3.31800853348013,-3.31350931295932,
-3.24048713832828,-3.1851290131769,-3.16941407347762,-3.16170814242443,
-3.16041120950007,-3.15972220444836,-3.15921578592962,-3.15866289018175,
-3.15785284878809,-3.15549635783017,-3.11445846781135,-3.05953304842109,
-3.01909050397777,-3.00236679610937,-2.99992982363778,-2.99866854606279,
-2.99775619567953,-2.99678550284927,-2.99541254557325,-2.99172321742471,
-2.93580968400112,-2.88036834265004,-2.86029346088551,-2.84138581136272,
-2.83826297786502,-2.83729155482927,-2.83667540460607,-2.83610840962103,
-2.83537128833854,-2.83376784259632,-2.82167583971944,-2.81965157443225,
-2.81924525341923,-2.81748741743982,-2.81640948552166,-2.81480242289232,
-2.8039779214992,-2.73415234090667,-2.69567812464718,-2.69249402637897),
 .UNSPECIFIED.);
#173=B_SPLINE_CURVE_WITH_KNOTS('',3,(#30204,#30205,#30206,#30207,#30208,
#30209,#30210,#30211,#30212,#30213,#30214,#30215,#30216,#30217,#30218,#30219,
#30220,#30221,#30222,#30223,#30224,#30225,#30226,#30227,#30228,#30229,#30230,
#30231,#30232,#30233,#30234,#30235,#30236,#30237,#30238,#30239,#30240,#30241,
#30242,#30243,#30244,#30245,#30246,#30247,#30248,#30249,#30250,#30251,#30252,
#30253,#30254,#30255,#30256,#30257,#30258,#30259,#30260,#30261,#30262,#30263,
#30264,#30265,#30266,#30267,#30268,#30269,#30270,#30271,#30272,#30273,#30274,
#30275,#30276,#30277,#30278,#30279,#30280,#30281,#30282,#30283,#30284,#30285,
#30286,#30287,#30288,#30289,#30290,#30291,#30292,#30293,#30294,#30295,#30296,
#30297,#30298,#30299,#30300,#30301,#30302,#30303,#30304,#30305,#30306,#30307,
#30308,#30309,#30310,#30311,#30312,#30313,#30314,#30315,#30316,#30317,#30318,
#30319,#30320,#30321,#30322,#30323,#30324,#30325,#30326,#30327,#30328,#30329,
#30330,#30331,#30332,#30333,#30334,#30335,#30336,#30337,#30338,#30339,#30340,
#30341,#30342,#30343,#30344,#30345,#30346,#30347,#30348,#30349,#30350,#30351,
#30352,#30353,#30354,#30355,#30356,#30357,#30358,#30359,#30360,#30361,#30362,
#30363,#30364,#30365,#30366,#30367,#30368,#30369,#30370,#30371,#30372,#30373,
#30374,#30375,#30376,#30377,#30378,#30379,#30380,#30381,#30382,#30383,#30384,
#30385,#30386,#30387,#30388,#30389,#30390,#30391,#30392,#30393,#30394,#30395,
#30396,#30397,#30398,#30399,#30400,#30401,#30402,#30403),.UNSPECIFIED.,
 .F.,.F.,(4,2,2,2,2,2,2,2,2,2,2,2,2,2,2,2,2,2,2,2,2,2,2,2,2,2,2,2,2,2,2,
2,2,2,2,2,2,2,2,2,2,2,2,2,2,2,2,2,2,2,2,2,2,2,2,2,2,2,2,2,2,2,2,2,2,2,2,
2,2,2,2,2,2,2,2,2,2,2,2,2,2,2,2,2,2,2,2,2,2,2,2,2,2,2,2,2,2,2,2,4),(-1.3693964092334,
-1.36183439143161,-1.36010319153898,-1.35941094504259,-1.35883722412521,
-1.35824631706058,-1.35738774872029,-1.35510335019303,-1.30469303630108,
-1.2448958121231,-1.2284289213657,-1.22211036730221,-1.21833670807719,-1.20208421397686,
-1.19944273305659,-1.19815058222417,-1.19713958817945,-1.19602067894988,
-1.19418771517626,-1.18789162911997,-1.14857759964781,-1.0805957109202,
-1.06483799454862,-1.03920499263226,-1.03730055369081,-1.03655966834246,
-1.0360256769157,-1.03545521873882,-1.03489280902372,-1.03356034031026,
-1.02501038137103,-1.00519442111407,-0.94854448356068,-0.902992456867276,
-0.900523872630309,-0.87947565454661,-0.876662910235612,-0.875331177247815,
-0.874311325157472,-0.873221519279924,-0.871519114858775,-0.866378945849957,
-0.842713618877838,-0.819747677814011,-0.76675100800911,-0.717581830234194,
-0.714718787904132,-0.713742997986063,-0.713191423705019,-0.712684578634125,
-0.711992547399501,-0.710681876017459,-0.702665426873464,-0.697023549330324,
-0.672461574805865,-0.633638711634387,-0.559398272293452,-0.558836508289221,
-0.554416477653384,-0.552770375573333,-0.551800710323614,-0.550887775478914,
-0.549623245088429,-0.548267054066933,-0.541809770541231,-0.506611221790919,
-0.498859904550877,-0.451990904665234,-0.395415657720684,-0.39191541499804,
-0.390858499559347,-0.390290571184745,-0.389730064843355,-0.389041648668859,
-0.388306182843127,-0.3850435462767,-0.379798867627013,-0.367932205113843,
-0.341137085985596,-0.318131079871123,-0.236913392853596,-0.23168252000432,
-0.229918188753276,-0.228924982149571,-0.228018130382196,-0.226804469889529,
-0.224541768058863,-0.212405067709946,-0.143914481944666,-0.132434716809599,
-0.0815972688082654,-0.0698091558616626,-0.0683756690717537,-0.0676514255875008,
-0.0671217931249414,-0.066548354386866,-0.0659805484161044,-0.0652189038625169,
-0.0639864071546979,-0.000961292996707948),.UNSPECIFIED.);
#174=B_SPLINE_CURVE_WITH_KNOTS('',3,(#30404,#30405,#30406,#30407,#30408,
#30409,#30410,#30411,#30412,#30413,#30414,#30415,#30416,#30417,#30418,#30419,
#30420,#30421,#30422,#30423,#30424,#30425,#30426,#30427,#30428,#30429,#30430,
#30431,#30432,#30433,#30434,#30435,#30436,#30437,#30438,#30439,#30440,#30441,
#30442,#30443,#30444,#30445,#30446,#30447,#30448,#30449,#30450,#30451,#30452,
#30453,#30454,#30455,#30456,#30457,#30458,#30459,#30460,#30461,#30462,#30463,
#30464,#30465,#30466,#30467,#30468,#30469,#30470,#30471,#30472,#30473,#30474,
#30475,#30476,#30477,#30478,#30479,#30480,#30481,#30482,#30483,#30484,#30485,
#30486,#30487,#30488,#30489,#30490,#30491,#30492,#30493,#30494,#30495,#30496,
#30497),.UNSPECIFIED.,.F.,.F.,(4,2,2,2,2,2,2,2,2,2,2,2,2,2,2,2,2,2,2,2,
2,2,2,2,2,2,2,2,2,2,2,2,2,2,2,2,2,2,2,2,2,2,2,2,2,2,4),(-4.06159336205859,
-3.99887010139295,-3.98005278788117,-3.973477430799,-3.97047047861041,-3.96807041057785,
-3.96682765673153,-3.96583078164577,-3.96483099104849,-3.96303389041738,
-3.95755932108663,-3.87303910799899,-3.86092619524348,-3.84976664354091,
-3.8211125343086,-3.80741249455709,-3.80630786437716,-3.80559979486472,
-3.80493103976298,-3.80442631822024,-3.80386166428903,-3.80282096307824,
-3.79945572828611,-3.74364984006477,-3.71603882454403,-3.68438630978772,
-3.65978046623324,-3.64729849982294,-3.64501824938511,-3.64380079053548,
-3.64289352602596,-3.64190226898059,-3.64014782893529,-3.63498832635877,
-3.55437381501121,-3.51385549988604,-3.49547979083049,-3.48419226853867,
-3.4827699658635,-3.48219787328426,-3.48162195136153,-3.48109526778725,
-3.48038263679504,-3.47899459597122,-3.46845176566513,-3.42568150182095,
-3.40020035460252),.UNSPECIFIED.);
#175=B_SPLINE_CURVE_WITH_KNOTS('',3,(#30498,#30499,#30500,#30501,#30502,
#30503,#30504,#30505,#30506,#30507,#30508,#30509,#30510,#30511,#30512,#30513,
#30514,#30515,#30516,#30517,#30518,#30519,#30520,#30521,#30522,#30523,#30524,
#30525,#30526,#30527,#30528,#30529,#30530,#30531,#30532,#30533,#30534,#30535,
#30536,#30537,#30538,#30539,#30540,#30541,#30542,#30543,#30544,#30545,#30546,
#30547,#30548,#30549,#30550,#30551,#30552,#30553,#30554,#30555,#30556,#30557,
#30558,#30559,#30560,#30561,#30562,#30563,#30564,#30565,#30566,#30567,#30568,
#30569,#30570,#30571,#30572,#30573,#30574,#30575,#30576,#30577,#30578,#30579,
#30580,#30581,#30582,#30583,#30584,#30585,#30586,#30587,#30588,#30589,#30590,
#30591,#30592,#30593,#30594,#30595,#30596,#30597,#30598,#30599,#30600,#30601,
#30602,#30603,#30604,#30605,#30606,#30607,#30608,#30609,#30610,#30611,#30612,
#30613,#30614,#30615,#30616,#30617,#30618,#30619,#30620,#30621,#30622,#30623,
#30624,#30625,#30626,#30627,#30628,#30629,#30630,#30631,#30632,#30633,#30634,
#30635,#30636,#30637,#30638,#30639,#30640,#30641,#30642,#30643,#30644,#30645,
#30646,#30647,#30648,#30649,#30650,#30651,#30652,#30653,#30654,#30655,#30656,
#30657,#30658,#30659,#30660,#30661,#30662,#30663,#30664,#30665,#30666,#30667,
#30668,#30669,#30670,#30671,#30672,#30673,#30674,#30675,#30676,#30677,#30678,
#30679,#30680,#30681,#30682,#30683,#30684,#30685,#30686,#30687,#30688,#30689,
#30690,#30691,#30692,#30693,#30694,#30695,#30696,#30697,#30698,#30699,#30700,
#30701,#30702,#30703,#30704,#30705,#30706,#30707,#30708,#30709,#30710,#30711,
#30712,#30713,#30714,#30715,#30716,#30717,#30718,#30719,#30720,#30721,#30722,
#30723,#30724,#30725,#30726,#30727,#30728,#30729,#30730,#30731,#30732,#30733,
#30734,#30735,#30736,#30737,#30738,#30739,#30740,#30741,#30742,#30743,#30744,
#30745,#30746,#30747,#30748,#30749,#30750,#30751,#30752,#30753,#30754,#30755,
#30756,#30757,#30758,#30759,#30760,#30761,#30762,#30763,#30764,#30765,#30766,
#30767,#30768,#30769,#30770,#30771,#30772,#30773,#30774,#30775,#30776,#30777,
#30778,#30779,#30780,#30781,#30782,#30783,#30784,#30785,#30786,#30787,#30788,
#30789,#30790,#30791,#30792,#30793,#30794,#30795,#30796,#30797,#30798,#30799,
#30800,#30801,#30802,#30803,#30804,#30805,#30806,#30807,#30808,#30809),
 .UNSPECIFIED.,.F.,.F.,(4,2,2,2,2,2,2,2,2,2,2,2,2,2,2,2,2,2,2,2,2,2,2,2,
2,2,2,2,2,2,2,2,2,2,2,2,2,2,2,2,2,2,2,2,2,2,2,2,2,2,2,2,2,2,2,2,2,2,2,2,
2,2,2,2,2,2,2,2,2,2,2,2,2,2,2,2,2,2,2,2,2,2,2,2,2,2,2,2,2,2,2,2,2,2,2,2,
2,2,2,2,2,2,2,2,2,2,2,2,2,2,2,2,2,2,2,2,2,2,2,2,2,2,2,2,2,2,2,2,2,2,2,2,
2,2,2,2,2,2,2,2,2,2,2,2,2,2,2,2,2,2,2,2,2,2,2,4),(-2.69249402637897,-2.67946463668276,
-2.67702422137398,-2.67577316515414,-2.67486219303942,-2.67388728734497,
-2.67249889944679,-2.66871122340817,-2.60799749771988,-2.5191478792325,
-2.51666595625057,-2.5148539143885,-2.514072506601,-2.51349743250879,-2.51296989519231,
-2.51225375602772,-2.51085192768008,-2.49994450458902,-2.45516160274233,
-2.36281457493466,-2.35547737922528,-2.35354318286739,-2.35240169304034,
-2.35139471732816,-2.3501401917013,-2.34820843898228,-2.33949521373088,
-2.33728128680638,-2.3352569798727,-2.3345927468463,-2.33300804766535,-2.32853492723566,
-2.3119192632956,-2.24880265539618,-2.1960242694092,-2.19236410575416,-2.19133482478078,
-2.19071013711643,-2.19014553700179,-2.18942525122613,-2.18791004194552,
-2.17796017589408,-2.08659169317583,-2.03433773191786,-2.03126820599149,
-2.03003159948487,-2.02900252786405,-2.02794913534297,-2.02641469068709,
-2.0223841989686,-1.96793370091752,-1.8743455635147,-1.86955292834131,-1.86848141873188,
-1.86778451662508,-1.8672235053693,-1.86657661277041,-1.86544803535368,
-1.86066185269588,-1.80582898886298,-1.7396880423071,-1.71132372305559,
-1.70823769455867,-1.70699825658492,-1.70596833654851,-1.70491561382164,
-1.70338494768895,-1.69946965522598,-1.64986819289321,-1.56382885985272,
-1.56291518796767,-1.56029950838556,-1.5598038218094,-1.55898482240542,
-1.54718683955472,-1.54575292810751,-1.54502854694235,-1.54449885061102,
-1.54392537957018,-1.54315289457259,-1.54139183153711,-1.53899621999878,
-1.45747679823816,-1.41229425846852,-1.40799722915126,-1.40595104425385,
-1.40474598873148,-1.40323814151953,-1.40115695618339,-1.40053504869551,
-1.39921573186698,-1.39874974815342,-1.39752938877203,-1.39435920412947,
-1.38659930565743,-1.38456655308647,-1.38339080697997,-1.38239594189719,
-1.38118943855668,-1.37900484029176,-1.36794577688663,-1.3465228297865,
-1.30415819221214,-1.24047784010733,-1.23835859953043,-1.23617267173459,
-1.23415843269291,-1.22408171676777,-1.22256058618864,-1.22183907500437,
-1.22127422706386,-1.2206500194128,-1.21964378153587,-1.21621048399678,
-1.13281131416596,-1.09660634635944,-1.08978248178416,-1.08434638888271,
-1.08295171041495,-1.08174625091998,-1.08026302207705,-1.07817838664266,
-1.0775920382433,-1.07589779111494,-1.07495263438374,-1.07222771756648,
-1.06373154765066,-1.06181731377792,-1.06056813295458,-1.05956144238387,
-1.05841593713943,-1.05650332789887,-1.04922580395954,-1.01622776644239,
-0.951273214040969,-0.902952901245586,-0.900119869414113,-0.899148424568292,
-0.898597701395266,-0.898090615477028,-0.897396718877762,-0.896077428880517,
-0.887858070659571,-0.87034158846105,-0.813649386766575,-0.744323227927764,
-0.739839795904135,-0.738183876341585,-0.737212241251194,-0.736299922102091,
-0.735040127441836,-0.733690509118304,-0.727342204009417,-0.717043392512378,
-0.680814601167412,-0.662293107873676),.UNSPECIFIED.);
#176=B_SPLINE_CURVE_WITH_KNOTS('',3,(#30814,#30815,#30816,#30817,#30818,
#30819,#30820,#30821,#30822,#30823,#30824,#30825,#30826,#30827,#30828,#30829,
#30830,#30831,#30832,#30833,#30834,#30835,#30836,#30837,#30838,#30839,#30840,
#30841,#30842,#30843,#30844,#30845,#30846,#30847,#30848,#30849,#30850,#30851,
#30852,#30853,#30854,#30855,#30856,#30857,#30858,#30859,#30860,#30861,#30862,
#30863,#30864,#30865,#30866,#30867,#30868,#30869,#30870,#30871,#30872,#30873,
#30874,#30875,#30876,#30877,#30878,#30879,#30880,#30881,#30882,#30883,#30884,
#30885,#30886,#30887,#30888,#30889,#30890,#30891,#30892,#30893,#30894,#30895,
#30896,#30897,#30898,#30899,#30900,#30901,#30902,#30903,#30904,#30905,#30906,
#30907,#30908,#30909,#30910,#30911,#30912,#30913,#30914,#30915,#30916,#30917,
#30918,#30919,#30920,#30921,#30922,#30923,#30924,#30925,#30926,#30927,#30928,
#30929,#30930,#30931,#30932,#30933,#30934,#30935,#30936,#30937,#30938,#30939,
#30940,#30941,#30942,#30943,#30944,#30945,#30946,#30947,#30948,#30949,#30950,
#30951,#30952,#30953,#30954,#30955,#30956,#30957,#30958,#30959,#30960,#30961,
#30962,#30963,#30964,#30965,#30966,#30967,#30968,#30969,#30970,#30971,#30972,
#30973,#30974,#30975,#30976,#30977,#30978,#30979,#30980,#30981,#30982,#30983,
#30984,#30985,#30986,#30987,#30988,#30989,#30990,#30991,#30992,#30993,#30994,
#30995,#30996,#30997,#30998,#30999,#31000,#31001,#31002,#31003,#31004,#31005,
#31006,#31007,#31008,#31009,#31010,#31011,#31012,#31013,#31014,#31015,#31016,
#31017,#31018,#31019,#31020,#31021,#31022,#31023,#31024,#31025,#31026,#31027,
#31028,#31029,#31030,#31031,#31032,#31033,#31034,#31035,#31036,#31037,#31038,
#31039,#31040,#31041,#31042,#31043,#31044,#31045,#31046,#31047,#31048,#31049,
#31050,#31051,#31052,#31053,#31054,#31055,#31056,#31057,#31058,#31059,#31060,
#31061,#31062,#31063,#31064,#31065,#31066,#31067,#31068,#31069,#31070,#31071,
#31072,#31073,#31074,#31075,#31076,#31077),.UNSPECIFIED.,.F.,.F.,(4,2,2,
2,2,2,2,2,2,2,2,2,2,2,2,2,2,2,2,2,2,2,2,2,2,2,2,2,2,2,2,2,2,2,2,2,2,2,2,
2,2,2,2,2,2,2,2,2,2,2,2,2,2,2,2,2,2,2,2,2,2,2,2,2,2,2,2,2,2,2,2,2,2,2,2,
2,2,2,2,2,2,2,2,2,2,2,2,2,2,2,2,2,2,2,2,2,2,2,2,2,2,2,2,2,2,2,2,2,2,2,2,
2,2,2,2,2,2,2,2,2,2,2,2,2,2,2,2,2,2,2,2,4),(-3.39927600084928,-3.37983339994959,
-3.34294734504984,-3.31433754663311,-3.30418735458775,-3.29882030444007,
-3.29764984383165,-3.29699388183311,-3.29648999236438,-3.2959168839376,
-3.29483339945536,-3.29109948697606,-3.29025532320103,-3.21490936905459,
-3.16755329055488,-3.14905012806519,-3.14255781321543,-3.13957945591476,
-3.13721882384085,-3.13599073195639,-3.13500037271095,-3.1338642541134,
-3.13195298730607,-3.12555202678434,-3.12161458651954,-3.12020473076913,
-3.11935000604415,-3.01984423732388,-2.98039665705453,-2.97575814675145,
-2.97464139795801,-2.97399725493184,-2.973436157739,-2.97273596942656,-2.97165353768983,
-2.96672206909679,-2.87137035732331,-2.82010506282366,-2.81682148915416,
-2.81426671493517,-2.81299700275787,-2.8120047868187,-2.81103160777165,
-2.80936629754912,-2.80481828421088,-2.73111340778257,-2.68256256963272,
-2.66190940206984,-2.65317197193653,-2.65182849917876,-2.65113539101577,
-2.65062860361498,-2.65007792907969,-2.64910586928944,-2.64626693994028,
-2.59782986577639,-2.52715242147492,-2.49979581152239,-2.49517749171423,
-2.49286236629535,-2.49145066566343,-2.4901642771863,-2.48916945831023,
-2.48820307448141,-2.48684546159887,-2.48404467661298,-2.45469282491939,
-2.36670907214967,-2.35346793164522,-2.33293593130824,-2.32963464118569,
-2.3286433758527,-2.32802729163341,-2.32746039005114,-2.32672343564521,
-2.32517815358206,-2.31406380224303,-2.22071699463133,-2.19035163301207,
-2.17089613266334,-2.16836285217489,-2.16709284088173,-2.16617942405667,
-2.16521246745381,-2.16385277770752,-2.16104358893022,-2.13134048927929,
-2.04365628199531,-2.03042309445068,-2.01940389077499,-2.00766771637792,
-2.0060982465228,-2.00535640695997,-2.00478873437102,-2.0041748636839,-2.0031935221447,
-1.99998089796753,-1.95154853065194,-1.90179336369731,-1.84947307008481,
-1.8460211363495,-1.84468665128501,-1.84372639110705,-1.84270820287488,
-1.84136232043809,-1.83844332240344,-1.79228637482434,-1.68759240910398,
-1.68380751800067,-1.68271808456167,-1.6821436354163,-1.68163957939732,
-1.68098479851308,-1.67987833338735,-1.67514345594757,-1.63265139736368,
-1.55223836542906,-1.54527219738183,-1.54377274317074,-1.54257783707578,
-1.53879692162831,-1.53838448508005,-1.52482418715018,-1.52257779404412,
-1.52124190185589,-1.52022145830609,-1.51913353482445,-1.51743925095977,
-1.51234770027879,-1.45206474110987,-1.37783960546454,-1.3693964092334),
 .UNSPECIFIED.);
#177=B_SPLINE_CURVE_WITH_KNOTS('',3,(#31079,#31080,#31081,#31082,#31083,
#31084,#31085,#31086,#31087,#31088,#31089,#31090,#31091,#31092,#31093,#31094,
#31095,#31096,#31097,#31098,#31099,#31100,#31101,#31102,#31103,#31104,#31105,
#31106,#31107,#31108,#31109,#31110,#31111,#31112,#31113,#31114,#31115,#31116,
#31117,#31118,#31119,#31120,#31121,#31122,#31123,#31124,#31125,#31126,#31127,
#31128,#31129,#31130,#31131,#31132,#31133,#31134,#31135,#31136,#31137,#31138,
#31139,#31140,#31141,#31142,#31143,#31144,#31145,#31146,#31147,#31148,#31149,
#31150,#31151,#31152,#31153,#31154,#31155,#31156,#31157,#31158,#31159,#31160,
#31161,#31162,#31163,#31164,#31165,#31166,#31167,#31168,#31169,#31170,#31171,
#31172,#31173,#31174,#31175,#31176),.UNSPECIFIED.,.F.,.F.,(4,2,2,2,2,2,
2,2,2,2,2,2,2,2,2,2,2,2,2,2,2,2,2,2,2,2,2,2,2,2,2,2,2,2,2,2,2,2,2,2,2,2,
2,2,2,2,2,2,4),(-0.662293107873676,-0.63546222695704,-0.624451999974867,
-0.57998846595183,-0.577166231313401,-0.576196463240149,-0.575646089194518,
-0.575138940377343,-0.57444437948297,-0.573700372012397,-0.570306893612535,
-0.54328226613345,-0.498543488887952,-0.446538136168641,-0.438044811829723,
-0.434725077017795,-0.418691546503556,-0.416060707706702,-0.414770615999668,
-0.413759789163189,-0.412639584224645,-0.410801125156248,-0.404460584912384,
-0.394177663305687,-0.35803734504289,-0.337988470814761,-0.317499512253371,
-0.257902129752157,-0.254430867780443,-0.253377355129703,-0.252810094191357,
-0.252249496564011,-0.251559880463779,-0.250822756417118,-0.24964891974005,
-0.235827407491852,-0.204478681377695,-0.192326481256771,-0.179475010979865,
-0.0992817518153433,-0.0941736302836654,-0.0924263964261471,-0.0914365858229751,
-0.0905290460283361,-0.0893088400560055,-0.0880140445847176,-0.0859778652052487,
-0.07142706603922,-0.000961713208880687),.UNSPECIFIED.);
#178=B_SPLINE_CURVE_WITH_KNOTS('',3,(#31177,#31178,#31179,#31180,#31181,
#31182,#31183,#31184,#31185,#31186,#31187,#31188,#31189,#31190,#31191,#31192,
#31193,#31194,#31195,#31196,#31197,#31198,#31199,#31200,#31201,#31202,#31203,
#31204,#31205,#31206,#31207,#31208,#31209,#31210,#31211,#31212,#31213,#31214,
#31215,#31216,#31217,#31218,#31219,#31220,#31221,#31222,#31223,#31224,#31225,
#31226,#31227,#31228,#31229,#31230,#31231,#31232,#31233,#31234,#31235,#31236,
#31237,#31238,#31239,#31240,#31241,#31242,#31243,#31244,#31245,#31246,#31247,
#31248,#31249,#31250,#31251,#31252,#31253,#31254,#31255,#31256,#31257,#31258,
#31259,#31260,#31261,#31262,#31263,#31264,#31265,#31266,#31267,#31268,#31269,
#31270,#31271,#31272,#31273,#31274,#31275,#31276,#31277,#31278,#31279,#31280,
#31281,#31282,#31283,#31284,#31285,#31286,#31287,#31288,#31289,#31290,#31291,
#31292,#31293,#31294,#31295,#31296,#31297,#31298,#31299,#31300,#31301,#31302,
#31303,#31304,#31305,#31306,#31307,#31308,#31309,#31310,#31311,#31312,#31313,
#31314,#31315,#31316,#31317,#31318,#31319,#31320,#31321,#31322,#31323,#31324,
#31325,#31326,#31327,#31328,#31329,#31330,#31331,#31332,#31333,#31334,#31335,
#31336,#31337,#31338,#31339,#31340,#31341,#31342,#31343,#31344,#31345,#31346,
#31347,#31348,#31349,#31350,#31351,#31352,#31353,#31354,#31355,#31356,#31357,
#31358,#31359,#31360,#31361,#31362,#31363,#31364,#31365,#31366,#31367,#31368,
#31369,#31370,#31371,#31372,#31373,#31374,#31375,#31376,#31377,#31378,#31379,
#31380,#31381,#31382,#31383,#31384,#31385,#31386,#31387,#31388),
 .UNSPECIFIED.,.F.,.F.,(4,2,2,2,2,2,2,2,2,2,2,2,2,2,2,2,2,2,2,2,2,2,2,2,
2,2,2,2,2,2,2,2,2,2,2,2,2,2,2,2,2,2,2,2,2,2,2,2,2,2,2,2,2,2,2,2,2,2,2,2,
2,2,2,2,2,2,2,2,2,2,2,2,2,2,2,2,2,2,2,2,2,2,2,2,2,2,2,2,2,2,2,2,2,2,2,2,
2,2,2,2,2,2,2,2,2,4),(-4.05923983194716,-3.99321314324124,-3.99085281993977,
-3.98964595230853,-3.98889513521332,-3.98819576457848,-3.98763479961503,
-3.98699022511209,-3.98589971888069,-3.98198383015804,-3.91710302758606,
-3.90292332503484,-3.8887812530649,-3.84812030474508,-3.83145431077663,
-3.82948587418539,-3.82778430468028,-3.82669501191882,-3.8256756248618,
-3.82434447707302,-3.82153288675943,-3.80048992725936,-3.79796289195734,
-3.78223587827113,-3.74089080667007,-3.70727527801193,-3.67831340478061,
-3.66775859531027,-3.6667032203646,-3.66601595659678,-3.66536214060095,
-3.66485831290565,-3.66428357111583,-3.66319193431783,-3.65938455327526,
-3.59801733697653,-3.54762186422377,-3.51719127705408,-3.50753684356768,
-3.50601831407394,-3.50463660064491,-3.50361273206204,-3.50266250567028,
-3.50136593462497,-3.4988087324421,-3.47793873738283,-3.47491991104323,
-3.42411055110869,-3.37266898708488,-3.35320366501896,-3.34472415821614,
-3.34339487790831,-3.34269908680512,-3.34213838585762,-3.34157519488595,
-3.34054090911407,-3.33722556866146,-3.28481362755085,-3.23536624646431,
-3.20053167210251,-3.18528301493135,-3.18290588191762,-3.18165478509397,
-3.18074401005344,-3.17976952977881,-3.17838210664701,-3.17459926413326,
-3.11368800684472,-3.06057675435992,-3.03568403802857,-3.02218647654392,
-3.02071189329907,-3.01998602306998,-3.01947469495743,-3.01893741088122,
-3.01818364398593,-3.01619904280879,-2.98518561667614,-2.93394584779512,
-2.89348437829834,-2.87171769633277,-2.86203547376924,-2.85993677071331,
-2.85874963993316,-2.8578452007547,-2.8566869183132,-2.8547276713905,-2.84768731741567,
-2.84408045408066,-2.84046395043769,-2.83997337032818,-2.83607936221074,
-2.83488454535907,-2.83338928057516,-2.82876982538296,-2.76338751758028,
-2.7252217569821,-2.70216418592773,-2.69982155907997,-2.69809220985762,
-2.69731608751809,-2.69674498616846,-2.69621261434858,-2.69547731868621,
-2.6936048244233,-2.69161531677502),.UNSPECIFIED.);
#179=B_SPLINE_CURVE_WITH_KNOTS('',3,(#31394,#31395,#31396,#31397,#31398,
#31399,#31400,#31401,#31402,#31403,#31404,#31405,#31406,#31407,#31408,#31409,
#31410,#31411,#31412,#31413,#31414,#31415,#31416,#31417,#31418,#31419,#31420,
#31421,#31422,#31423,#31424,#31425,#31426,#31427,#31428,#31429,#31430,#31431,
#31432,#31433,#31434,#31435,#31436,#31437,#31438,#31439,#31440,#31441,#31442,
#31443,#31444,#31445,#31446,#31447,#31448,#31449,#31450,#31451,#31452,#31453,
#31454,#31455,#31456,#31457,#31458,#31459,#31460,#31461,#31462,#31463,#31464,
#31465,#31466,#31467,#31468,#31469,#31470,#31471,#31472,#31473,#31474,#31475,
#31476,#31477,#31478,#31479,#31480,#31481,#31482,#31483,#31484,#31485,#31486,
#31487,#31488,#31489,#31490,#31491,#31492,#31493,#31494,#31495,#31496,#31497,
#31498,#31499,#31500,#31501,#31502,#31503,#31504,#31505,#31506,#31507,#31508,
#31509,#31510,#31511,#31512,#31513,#31514,#31515,#31516,#31517,#31518,#31519,
#31520,#31521,#31522,#31523,#31524,#31525,#31526,#31527,#31528,#31529,#31530,
#31531,#31532,#31533,#31534,#31535),.UNSPECIFIED.,.F.,.F.,(4,3,3,3,3,3,
3,3,3,3,3,3,3,3,3,3,3,3,3,3,3,3,3,3,3,3,3,3,3,3,3,3,3,3,3,3,3,3,3,3,3,3,
3,3,3,3,3,4),(279.601746169492,279.694968836592,279.788194706647,279.881447740152,
279.974818258919,280.068250010175,280.161852771942,280.237119038469,280.330191982745,
280.423138822382,280.515987193567,280.608767698222,280.701513020379,280.79424798548,
280.886997403821,280.979846044556,281.072746485167,281.165802381252,281.236833693942,
281.329906638218,281.422853477855,281.51570184904,281.608482353695,281.701227675851,
281.793962640953,281.886712059294,281.979560700029,282.07246114064,282.165517036725,
282.236548349415,282.329621293691,282.422568133328,282.515416504513,282.608197009168,
282.700942331324,282.793677296426,282.886426714767,282.979275355502,283.072175796113,
283.165231692198,283.236263004888,283.329324259851,283.422266293444,283.515114136645,
283.60789190088,283.700628731049,283.793365131737,283.838365347136),
 .UNSPECIFIED.);
#180=B_SPLINE_CURVE_WITH_KNOTS('',3,(#31536,#31537,#31538,#31539,#31540,
#31541,#31542,#31543,#31544,#31545,#31546,#31547,#31548,#31549,#31550,#31551,
#31552,#31553,#31554,#31555,#31556,#31557,#31558,#31559,#31560,#31561,#31562,
#31563,#31564,#31565,#31566,#31567,#31568,#31569,#31570,#31571,#31572,#31573,
#31574,#31575,#31576,#31577,#31578,#31579,#31580,#31581,#31582,#31583,#31584,
#31585,#31586,#31587,#31588,#31589,#31590,#31591,#31592,#31593,#31594,#31595,
#31596,#31597,#31598,#31599,#31600,#31601,#31602,#31603,#31604,#31605,#31606,
#31607,#31608,#31609,#31610,#31611,#31612,#31613,#31614,#31615,#31616,#31617,
#31618,#31619,#31620,#31621,#31622,#31623,#31624,#31625,#31626,#31627,#31628,
#31629,#31630,#31631,#31632,#31633,#31634,#31635,#31636,#31637,#31638,#31639,
#31640,#31641),.UNSPECIFIED.,.F.,.F.,(4,2,2,2,2,2,2,2,2,2,2,2,2,2,2,2,2,
2,2,2,2,2,2,2,2,2,2,2,2,2,2,2,2,2,2,2,2,2,2,2,2,2,2,2,2,2,2,2,2,2,2,2,4),
(-4.06014804983483,-3.97627233438681,-3.9540983489275,-3.94499999060754,
-3.94364269485105,-3.94294661142199,-3.94238573801438,-3.94173842067592,
-3.94063665693829,-3.93661534681092,-3.93616197487211,-3.83281327894976,
-3.81563438869693,-3.7954845909032,-3.78493039389705,-3.7827758412725,-3.78179224787277,
-3.78082040480629,-3.77985437709963,-3.77849835854609,-3.77570439382236,
-3.74664651748312,-3.71659417216206,-3.6958895607374,-3.6551563427794,-3.63790786143977,
-3.62229831450554,-3.62077722836758,-3.62004809810623,-3.61953620227033,
-3.61899993004642,-3.61825006656294,-3.61671389026045,-3.60156765415293,
-3.59955044851104,-3.59804814868023,-3.50174633992608,-3.4802367045534,
-3.46854252317124,-3.46392757857399,-3.46056123883827,-3.45913781847436,
-3.45819224174273,-3.45716299063785,-3.45592498330869,-3.45284580079668,
-3.44519475740641,-3.44337966653802,-3.44131925848713,-3.44081022737214,
-3.43874865156816,-3.43711525853886,-3.39927600084928),.UNSPECIFIED.);
#181=B_SPLINE_CURVE_WITH_KNOTS('',3,(#31642,#31643,#31644,#31645,#31646,
#31647,#31648,#31649,#31650,#31651,#31652,#31653,#31654,#31655,#31656,#31657,
#31658,#31659,#31660,#31661,#31662,#31663,#31664,#31665,#31666,#31667,#31668,
#31669,#31670,#31671,#31672,#31673,#31674,#31675,#31676,#31677,#31678,#31679,
#31680,#31681,#31682,#31683,#31684,#31685,#31686,#31687,#31688,#31689,#31690,
#31691,#31692,#31693,#31694,#31695,#31696,#31697,#31698,#31699,#31700,#31701,
#31702,#31703,#31704,#31705,#31706,#31707,#31708,#31709,#31710,#31711,#31712,
#31713,#31714,#31715,#31716,#31717,#31718,#31719,#31720,#31721,#31722,#31723,
#31724,#31725,#31726,#31727,#31728,#31729,#31730,#31731,#31732,#31733,#31734,
#31735,#31736,#31737,#31738,#31739,#31740,#31741,#31742,#31743,#31744,#31745,
#31746,#31747,#31748,#31749,#31750,#31751,#31752,#31753,#31754,#31755,#31756,
#31757,#31758,#31759,#31760,#31761,#31762,#31763,#31764,#31765,#31766,#31767,
#31768,#31769,#31770,#31771,#31772,#31773,#31774,#31775,#31776,#31777,#31778,
#31779,#31780,#31781,#31782,#31783,#31784,#31785,#31786,#31787,#31788,#31789,
#31790,#31791,#31792,#31793,#31794,#31795,#31796,#31797,#31798,#31799,#31800,
#31801,#31802,#31803,#31804,#31805,#31806,#31807,#31808,#31809,#31810,#31811,
#31812,#31813,#31814,#31815,#31816,#31817,#31818,#31819,#31820,#31821,#31822,
#31823,#31824,#31825,#31826,#31827,#31828,#31829,#31830,#31831,#31832,#31833,
#31834,#31835,#31836,#31837,#31838,#31839,#31840,#31841,#31842,#31843,#31844,
#31845,#31846,#31847,#31848,#31849,#31850,#31851,#31852,#31853,#31854,#31855,
#31856,#31857,#31858,#31859,#31860,#31861,#31862,#31863,#31864,#31865,#31866,
#31867,#31868,#31869,#31870,#31871,#31872,#31873,#31874,#31875,#31876,#31877,
#31878,#31879,#31880,#31881,#31882,#31883,#31884,#31885,#31886,#31887,#31888,
#31889,#31890,#31891,#31892,#31893,#31894,#31895,#31896,#31897,#31898,#31899,
#31900,#31901,#31902,#31903,#31904,#31905,#31906,#31907,#31908,#31909,#31910,
#31911,#31912,#31913,#31914,#31915,#31916,#31917,#31918,#31919,#31920,#31921,
#31922,#31923,#31924,#31925,#31926,#31927,#31928,#31929,#31930,#31931,#31932,
#31933,#31934,#31935,#31936,#31937,#31938,#31939,#31940,#31941),
 .UNSPECIFIED.,.F.,.F.,(4,2,2,2,2,2,2,2,2,2,2,2,2,2,2,2,2,2,2,2,2,2,2,2,
2,2,2,2,2,2,2,2,2,2,2,2,2,2,2,2,2,2,2,2,2,2,2,2,2,2,2,2,2,2,2,2,2,2,2,2,
2,2,2,2,2,2,2,2,2,2,2,2,2,2,2,2,2,2,2,2,2,2,2,2,2,2,2,2,2,2,2,2,2,2,2,2,
2,2,2,2,2,2,2,2,2,2,2,2,2,2,2,2,2,2,2,2,2,2,2,2,2,2,2,2,2,2,2,2,2,2,2,2,
2,2,2,2,2,2,2,2,2,2,2,2,2,2,2,2,2,4),(-2.69161531677502,-2.66975863127559,
-2.59833333423941,-2.55681491066562,-2.53986877882376,-2.53739578120855,
-2.53612781025229,-2.53521471375916,-2.53424703289885,-2.53288458415628,
-2.53006404203878,-2.52248328754017,-2.52066917147998,-2.51860651883555,
-2.51815716531915,-2.51615439304126,-2.51343434507484,-2.51223794799365,
-2.5106657409351,-2.42562089209351,-2.40168041140071,-2.3792362626676,-2.37576459583974,
-2.37475705312234,-2.37413265711828,-2.37356817809527,-2.37284785744027,
-2.37133187915587,-2.36135881229659,-2.32584503346877,-2.30313882825556,
-2.25347891510951,-2.22981349995511,-2.21672833737523,-2.21443089930766,
-2.21321004493171,-2.21220553444244,-2.21119130648906,-2.20932161757998,
-2.20327203202333,-2.09964589395868,-2.05415320249531,-2.05231283231797,
-2.05152440393053,-2.05095103653307,-2.0504215369608,-2.04969757376217,
-2.04826494243929,-2.03649646694038,-2.03565884251949,-2.03528199951603,
-2.03187157186493,-2.03104695559205,-2.03082652130756,-2.00952304334794,
-1.93284316004468,-1.91586941545568,-1.91373382956355,-1.91082838371842,
-1.90958705994939,-1.90752321891598,-1.89401576177496,-1.89177232537155,
-1.89043736821384,-1.8894171575682,-1.88832901595168,-1.88663343240954,
-1.88142743795694,-1.85263253770397,-1.80927929752101,-1.7345363823492,
-1.73015126935101,-1.72901305613939,-1.72835724470118,-1.7278023272166,
-1.72711938891572,-1.72582472574377,-1.71824960573342,-1.70249511442728,
-1.67993871492696,-1.57615085386427,-1.56991613140896,-1.56802414454193,
-1.56700539239621,-1.56601074725647,-1.56482546976944,-1.56266088286365,
-1.55998337424128,-1.50875793597317,-1.4118720608639,-1.40707378289095,
-1.40600188921924,-1.40530489663068,-1.40474392006454,-1.40409718779382,
-1.4029691896418,-1.39818971006601,-1.34334308553238,-1.27932994616557,
-1.24894002507576,-1.24611414281008,-1.24475016038786,-1.24378186467486,
-1.2428083750859,-1.24153552447691,-1.23896730548812,-1.2356621084541,-1.20897675642653,
-1.14963715235865,-1.08766149683926,-1.08394766587589,-1.08286617372197,
-1.08229332471083,-1.08178921549943,-1.08113234591145,-1.07995847408672,
-1.07454601559485,-1.06428086581231,-1.03490157010068,-0.94550780530881,
-0.943948685276739,-0.942753773877978,-0.938709018586882,-0.937799471313907,
-0.937400876123338,-0.935338371134719,-0.933526261676283,-0.925947272321559,
-0.923123833474818,-0.921760477235901,-0.920792375958718,-0.91981903454206,
-0.918545998776772,-0.915972521573023,-0.912661283391196,-0.90517509229076,
-0.882869647019001,-0.838102651494489,-0.765143595793327,-0.761039580315633,
-0.759929254039053,-0.759279907608441,-0.758775256131499,-0.758106913623438,
-0.756880398879024,-0.750626525274491,-0.738116346911481,-0.722281313452548,
-0.682051515293471,-0.661851498152186),.UNSPECIFIED.);
#182=B_SPLINE_CURVE_WITH_KNOTS('',3,(#31947,#31948,#31949,#31950,#31951,
#31952,#31953,#31954,#31955,#31956,#31957,#31958,#31959,#31960,#31961,#31962,
#31963,#31964,#31965,#31966,#31967,#31968,#31969,#31970,#31971,#31972,#31973,
#31974,#31975,#31976,#31977,#31978,#31979,#31980,#31981,#31982,#31983,#31984,
#31985,#31986,#31987,#31988,#31989,#31990,#31991,#31992,#31993,#31994,#31995,
#31996,#31997,#31998,#31999,#32000,#32001,#32002,#32003,#32004,#32005,#32006,
#32007,#32008,#32009,#32010,#32011,#32012,#32013,#32014,#32015,#32016,#32017,
#32018,#32019,#32020,#32021,#32022,#32023,#32024,#32025,#32026,#32027,#32028,
#32029,#32030,#32031,#32032,#32033,#32034,#32035,#32036,#32037,#32038,#32039,
#32040,#32041,#32042,#32043,#32044,#32045,#32046,#32047,#32048,#32049,#32050,
#32051,#32052,#32053,#32054,#32055,#32056,#32057,#32058,#32059,#32060,#32061,
#32062,#32063,#32064,#32065,#32066,#32067,#32068,#32069,#32070,#32071,#32072,
#32073,#32074,#32075,#32076,#32077,#32078,#32079,#32080,#32081,#32082,#32083,
#32084,#32085,#32086,#32087,#32088,#32089,#32090,#32091,#32092,#32093,#32094,
#32095,#32096,#32097,#32098,#32099,#32100,#32101,#32102,#32103,#32104,#32105,
#32106,#32107,#32108,#32109,#32110,#32111,#32112,#32113,#32114,#32115,#32116,
#32117,#32118,#32119,#32120,#32121,#32122,#32123,#32124,#32125,#32126,#32127,
#32128,#32129,#32130,#32131,#32132,#32133,#32134,#32135,#32136,#32137,#32138,
#32139,#32140),.UNSPECIFIED.,.F.,.F.,(4,2,2,2,2,2,2,2,2,2,2,2,2,2,2,2,2,
2,2,2,2,2,2,2,2,2,2,2,2,2,2,2,2,2,2,2,2,2,2,2,2,2,2,2,2,2,2,2,2,2,2,2,2,
2,2,2,2,2,2,2,2,2,2,2,2,2,2,2,2,2,2,2,2,2,2,2,2,2,2,2,2,2,2,2,2,2,2,2,2,
2,2,2,2,2,2,2,4),(-1.36962946327728,-1.35522113359464,-1.25363486513697,
-1.24766842856606,-1.24580887865057,-1.24479667881036,-1.24379197755589,
-1.2425924874766,-1.24036948955681,-1.2375990067608,-1.1751740267707,-1.08960099478755,
-1.08490274856675,-1.08383909731689,-1.08314470479165,-1.0826400027721,
-1.08201105269236,-1.08096261244758,-1.07710682614834,-0.988526140506354,
-0.927669658193646,-0.923920123482608,-0.922537717341603,-0.921564494883401,
-0.920587582155144,-0.919325582573995,-0.916805239219223,-0.913577662701302,
-0.906344368579121,-0.884997542159967,-0.839546137460765,-0.766013276509471,
-0.761811049190314,-0.760690882538198,-0.760039285770672,-0.759478777792869,
-0.758788299546242,-0.757457792863099,-0.749052896954004,-0.730084821141988,
-0.68530174884738,-0.629620176574333,-0.623226227537091,-0.621673734057325,
-0.620477933864338,-0.617505887229563,-0.615788161049915,-0.615255073311271,
-0.613196538249033,-0.611362902684152,-0.603546201782025,-0.60059270160666,
-0.59925485857177,-0.598234150893916,-0.597292864485368,-0.595759805561137,
-0.591721518604337,-0.585930415487845,-0.570059610228783,-0.532771897432884,
-0.455568890971052,-0.453357010350174,-0.439769595928774,-0.438134232423592,
-0.43744714152551,-0.436874791326697,-0.436282148395612,-0.435397665123465,
-0.43294883232243,-0.390978849105762,-0.357727230013845,-0.318118385968153,
-0.305786357423783,-0.299791552671234,-0.298237601030414,-0.29700426618635,
-0.295998350722984,-0.280145278367768,-0.277523783189676,-0.276235671924949,
-0.275225199478065,-0.274282311194023,-0.273182904894614,-0.269953670638996,
-0.241541816256804,-0.221902483840598,-0.133180384072646,-0.116938634166373,
-0.115373604620995,-0.114616497005434,-0.11407814379619,-0.113566922577861,
-0.112842994707471,-0.111349115819227,-0.0972260317227201,-0.0703211750184439,
-0.000962450277454619),.UNSPECIFIED.);
#183=B_SPLINE_CURVE_WITH_KNOTS('',3,(#32141,#32142,#32143,#32144,#32145,
#32146,#32147,#32148,#32149,#32150,#32151,#32152,#32153,#32154,#32155,#32156,
#32157,#32158,#32159,#32160,#32161,#32162,#32163,#32164,#32165,#32166,#32167,
#32168,#32169,#32170,#32171,#32172,#32173,#32174,#32175,#32176,#32177,#32178,
#32179,#32180,#32181,#32182,#32183,#32184,#32185,#32186,#32187,#32188,#32189,
#32190,#32191,#32192,#32193,#32194,#32195,#32196,#32197,#32198,#32199,#32200,
#32201,#32202,#32203,#32204,#32205,#32206,#32207,#32208,#32209,#32210),
 .UNSPECIFIED.,.F.,.F.,(4,3,3,3,3,3,3,3,3,3,3,3,3,3,3,3,3,3,3,3,3,3,3,4),
(283.838365347136,283.931130707637,284.024001664162,284.116935236969,284.210011185465,
284.235977660361,284.329050604637,284.421997444274,284.514845815459,284.607626320114,
284.700371642271,284.793106607372,284.885856025713,284.978704666448,285.071605107059,
285.164661003144,285.235692315834,285.329019191919,285.422219967727,285.515319268183,
285.608340093871,285.701312563782,285.794286693993,285.884931476672),
 .UNSPECIFIED.);
#184=B_SPLINE_CURVE_WITH_KNOTS('',3,(#32212,#32213,#32214,#32215,#32216,
#32217,#32218,#32219,#32220,#32221,#32222,#32223,#32224,#32225,#32226,#32227,
#32228,#32229,#32230,#32231,#32232,#32233,#32234,#32235,#32236,#32237,#32238,
#32239,#32240,#32241,#32242,#32243,#32244,#32245,#32246,#32247,#32248,#32249,
#32250,#32251,#32252,#32253,#32254,#32255,#32256,#32257,#32258,#32259,#32260,
#32261,#32262,#32263,#32264,#32265,#32266,#32267,#32268,#32269,#32270,#32271,
#32272,#32273,#32274,#32275,#32276,#32277,#32278,#32279,#32280,#32281,#32282,
#32283,#32284,#32285,#32286,#32287,#32288,#32289,#32290,#32291,#32292,#32293,
#32294,#32295,#32296,#32297,#32298,#32299,#32300,#32301,#32302,#32303,#32304,
#32305,#32306,#32307,#32308,#32309,#32310,#32311,#32312,#32313,#32314,#32315,
#32316,#32317),.UNSPECIFIED.,.F.,.F.,(4,2,2,2,2,2,2,2,2,2,2,2,2,2,2,2,2,
2,2,2,2,2,2,2,2,2,2,2,2,2,2,2,2,2,2,2,2,2,2,2,2,2,2,2,2,2,2,2,2,2,2,2,4),
(-0.661851498152186,-0.62878770815041,-0.622426769083829,-0.620741194311147,
-0.619539344973217,-0.617814864606714,-0.615752489403866,-0.613183040637154,
-0.611331106699762,-0.607346415168121,-0.601044491102584,-0.599144316014681,
-0.598010388134803,-0.597103075690806,-0.596142074964848,-0.594227719906788,
-0.586915283219504,-0.574529656690142,-0.550759053929635,-0.523801621510284,
-0.449614013788087,-0.438864102791653,-0.437468203658721,-0.436753580704446,
-0.436226421530714,-0.435651002090432,-0.43485170074881,-0.432948943699684,
-0.430333817472526,-0.402374404755727,-0.362420115047496,-0.342627331205157,
-0.315287888133803,-0.280345138323659,-0.277161829476354,-0.275872647423816,
-0.274924009529335,-0.273963748096499,-0.272965945018782,-0.270676460027525,
-0.257626943913925,-0.233730766054508,-0.218776160636162,-0.127020883125178,
-0.115914215812652,-0.114368713049002,-0.113631505979336,-0.113064342891623,
-0.11244790457966,-0.111455922433078,-0.108150927225548,-0.0875907243741109,
-0.000962456779688808),.UNSPECIFIED.);
#185=B_SPLINE_CURVE_WITH_KNOTS('',3,(#32318,#32319,#32320,#32321,#32322,
#32323,#32324,#32325,#32326,#32327,#32328,#32329,#32330,#32331,#32332,#32333,
#32334,#32335,#32336,#32337,#32338,#32339,#32340,#32341,#32342,#32343,#32344,
#32345,#32346,#32347,#32348,#32349,#32350,#32351,#32352,#32353,#32354,#32355,
#32356,#32357,#32358,#32359,#32360,#32361,#32362,#32363,#32364,#32365,#32366,
#32367,#32368,#32369,#32370,#32371,#32372,#32373,#32374,#32375,#32376,#32377,
#32378,#32379,#32380,#32381,#32382,#32383,#32384,#32385,#32386,#32387,#32388,
#32389,#32390,#32391,#32392,#32393,#32394,#32395,#32396,#32397,#32398,#32399,
#32400,#32401,#32402,#32403,#32404,#32405,#32406,#32407,#32408,#32409,#32410,
#32411,#32412,#32413,#32414,#32415,#32416,#32417,#32418,#32419,#32420,#32421,
#32422,#32423,#32424,#32425,#32426,#32427,#32428,#32429,#32430,#32431,#32432,
#32433,#32434,#32435,#32436,#32437,#32438,#32439,#32440,#32441,#32442,#32443,
#32444,#32445,#32446,#32447,#32448,#32449,#32450,#32451,#32452,#32453,#32454,
#32455,#32456,#32457,#32458,#32459),.UNSPECIFIED.,.F.,.F.,(4,3,3,3,3,3,
3,3,3,3,3,3,3,3,3,3,3,3,3,3,3,3,3,3,3,3,3,3,3,3,3,3,3,3,3,3,3,3,3,3,3,3,
3,3,3,3,3,4),(285.884931476672,285.977853410009,286.070768379482,286.163700831097,
286.256961744019,286.350056827274,286.44340065503,286.536744482785,286.629817427061,
286.722764266698,286.815612637883,286.908393142538,287.001138464694,287.093873429795,
287.186622848136,287.279471488871,287.372371929483,287.465427825567,287.536459138258,
287.629532082534,287.722478922171,287.815327293356,287.908107798011,288.000853120167,
288.093588085268,288.186337503609,288.279186144344,288.372086584956,288.46514248104,
288.53617379373,288.629246738006,288.722193577643,288.815041948827,288.907822453483,
289.000567775639,289.09330274074,289.186052159081,289.278900799816,289.371801240428,
289.464857136512,289.535888449203,289.628951438742,289.721894824678,289.814743639923,
289.907520539162,290.000256353257,290.092987040943,290.12159641265),
 .UNSPECIFIED.);
#186=B_SPLINE_CURVE_WITH_KNOTS('',3,(#32464,#32465,#32466,#32467,#32468,
#32469,#32470,#32471,#32472,#32473,#32474,#32475,#32476,#32477,#32478,#32479,
#32480,#32481,#32482,#32483,#32484,#32485,#32486,#32487,#32488,#32489,#32490,
#32491,#32492,#32493,#32494,#32495,#32496,#32497,#32498,#32499,#32500,#32501,
#32502,#32503,#32504,#32505,#32506,#32507,#32508,#32509,#32510,#32511,#32512,
#32513,#32514,#32515,#32516,#32517,#32518,#32519,#32520,#32521,#32522,#32523,
#32524,#32525,#32526,#32527,#32528,#32529,#32530,#32531,#32532,#32533,#32534,
#32535,#32536,#32537,#32538,#32539,#32540,#32541,#32542,#32543,#32544,#32545,
#32546,#32547,#32548,#32549,#32550,#32551,#32552,#32553,#32554,#32555,#32556,
#32557,#32558,#32559,#32560,#32561,#32562,#32563,#32564,#32565,#32566,#32567,
#32568,#32569,#32570,#32571,#32572,#32573,#32574,#32575,#32576,#32577,#32578,
#32579,#32580,#32581,#32582,#32583,#32584,#32585,#32586,#32587,#32588,#32589,
#32590,#32591,#32592,#32593,#32594,#32595,#32596,#32597,#32598,#32599,#32600,
#32601,#32602,#32603,#32604,#32605,#32606,#32607,#32608,#32609,#32610,#32611,
#32612,#32613,#32614,#32615,#32616,#32617,#32618,#32619,#32620,#32621,#32622,
#32623,#32624,#32625,#32626,#32627,#32628,#32629,#32630,#32631,#32632,#32633,
#32634,#32635,#32636,#32637,#32638,#32639,#32640,#32641,#32642,#32643,#32644,
#32645,#32646,#32647,#32648,#32649,#32650,#32651,#32652,#32653,#32654,#32655,
#32656,#32657,#32658,#32659,#32660,#32661,#32662,#32663,#32664,#32665,#32666,
#32667,#32668,#32669,#32670,#32671,#32672,#32673,#32674,#32675,#32676,#32677,
#32678,#32679,#32680,#32681,#32682,#32683,#32684,#32685,#32686,#32687,#32688,
#32689,#32690,#32691,#32692,#32693,#32694,#32695,#32696,#32697,#32698,#32699,
#32700,#32701,#32702,#32703,#32704,#32705,#32706,#32707,#32708,#32709,#32710,
#32711,#32712,#32713,#32714,#32715,#32716,#32717,#32718,#32719,#32720,#32721,
#32722,#32723,#32724,#32725,#32726,#32727,#32728,#32729,#32730,#32731,#32732,
#32733),.UNSPECIFIED.,.F.,.F.,(4,2,2,2,2,2,2,2,2,2,2,2,2,2,2,2,2,2,2,2,
2,2,2,2,2,2,2,2,2,2,2,2,2,2,2,2,2,2,2,2,2,2,2,2,2,2,2,2,2,2,2,2,2,2,2,2,
2,2,2,2,2,2,2,2,2,2,2,2,2,2,2,2,2,2,2,2,2,2,2,2,2,2,2,2,2,2,2,2,2,2,2,2,
2,2,2,2,2,2,2,2,2,2,2,2,2,2,2,2,2,2,2,2,2,2,2,2,2,2,2,2,2,2,2,2,2,2,2,2,
2,2,2,2,2,2,4),(-3.39946882069219,-3.3747953566667,-3.35473878549777,-3.34614186934065,
-3.34480797227182,-3.34411119358856,-3.34355041302804,-3.34298774859426,
-3.34195610759352,-3.3386622723819,-3.28658709080641,-3.23587803266845,
-3.20173510423029,-3.18666802497955,-3.1842980535206,-3.18304846389771,
-3.18213787058331,-3.18116271711466,-3.17977288199556,-3.17597452378808,
-3.11402274281264,-3.06052394859133,-3.03288711168279,-3.02339449477033,
-3.02202784596771,-3.02132415256512,-3.0208160599466,-3.02027023431432,
-3.01932234286432,-3.01665078764087,-2.97488612171436,-2.91362283861595,
-2.89087215272044,-2.86460575711339,-2.86176760679706,-2.86042138330595,
-2.85940323974472,-2.85844324436091,-2.85710948258718,-2.85366137163933,
-2.80172560284016,-2.73192628271962,-2.70965694141235,-2.7005461519022,
-2.69919278536021,-2.69849186464927,-2.69793073560402,-2.6972871703058,
-2.69620112212845,-2.69232760340448,-2.62716973622437,-2.54480280835667,
-2.53965842725503,-2.53795695707984,-2.53686768670171,-2.53584829151332,
-2.53451709145403,-2.53170523942729,-2.51065557881264,-2.50816376113553,
-2.50031386415463,-2.41731035761435,-2.3915618927331,-2.38225779637452,
-2.37723467008438,-2.37609122407451,-2.37543601902907,-2.37493210520939,
-2.37435832042518,-2.3732716367524,-2.36950963015601,-2.36756259803964,
-2.36515406638197,-2.36280639565041,-2.32965639713687,-2.30919463607096,
-2.26855783266484,-2.2379033668598,-2.22492058896002,-2.21731889542604,
-2.21537496298488,-2.21423143997401,-2.21322494685541,-2.21197399707917,
-2.21005329921546,-2.20147214024632,-2.08839052542491,-2.07065961317895,
-2.05484016997293,-2.05331518800577,-2.05258518838787,-2.05207305556517,
-2.05153688171486,-2.05078768942265,-2.04925459292882,-2.03421796510482,
-2.03115426980831,-2.00754170660638,-1.90005731595792,-1.89392338325728,
-1.89204341514703,-1.89102707365398,-1.89002264154938,-1.88880500632726,
-1.88652288289963,-1.87375501198413,-1.84895713237321,-1.75920904399099,
-1.73234319425767,-1.73041870666273,-1.72967453892031,-1.72913972393592,
-1.72856988848492,-1.72780203048415,-1.72607684713483,-1.67940192224438,
-1.57688986440158,-1.57079222038806,-1.56891664632421,-1.56790120131222,
-1.56689672630908,-1.56570221603655,-1.56349553890872,-1.56075433596593,
-1.50400877058759,-1.42005597629361,-1.40865561322051,-1.40707877110983,
-1.40634667932272,-1.40578044653949,-1.40516190464683,-1.40415991931988,
-1.40076132207881,-1.37923116980918,-1.36962946327728),.UNSPECIFIED.);
#187=B_SPLINE_CURVE_WITH_KNOTS('',3,(#32735,#32736,#32737,#32738,#32739,
#32740,#32741,#32742,#32743,#32744,#32745,#32746,#32747,#32748,#32749,#32750,
#32751,#32752,#32753,#32754,#32755,#32756,#32757,#32758,#32759,#32760,#32761,
#32762,#32763,#32764,#32765,#32766,#32767,#32768,#32769,#32770,#32771,#32772,
#32773,#32774,#32775,#32776,#32777,#32778,#32779,#32780,#32781,#32782,#32783,
#32784,#32785,#32786,#32787,#32788,#32789,#32790,#32791,#32792,#32793,#32794,
#32795,#32796,#32797,#32798,#32799,#32800,#32801,#32802,#32803,#32804),
 .UNSPECIFIED.,.F.,.F.,(4,3,3,3,3,3,3,3,3,3,3,3,3,3,3,3,3,3,3,3,3,3,3,4),
(290.12159641265,290.214355285923,290.307217500986,290.40013838856,290.493206279757,
290.535603104676,290.628676048952,290.721622888589,290.814471259773,290.907251764429,
290.999997086585,291.092732051686,291.185481470027,291.278330110762,291.371230551374,
291.464286447458,291.535317760149,291.628979765018,291.722512329929,291.815939595004,
291.909279522268,292.002567165507,292.095842588612,292.168116783851),
 .UNSPECIFIED.);
#188=B_SPLINE_CURVE_WITH_KNOTS('',3,(#32805,#32806,#32807,#32808,#32809,
#32810,#32811,#32812,#32813,#32814,#32815,#32816,#32817,#32818,#32819,#32820,
#32821,#32822,#32823,#32824,#32825,#32826,#32827,#32828,#32829,#32830,#32831,
#32832,#32833,#32834,#32835,#32836,#32837,#32838,#32839,#32840,#32841,#32842,
#32843,#32844,#32845,#32846,#32847,#32848,#32849,#32850,#32851,#32852,#32853,
#32854,#32855,#32856,#32857,#32858,#32859,#32860,#32861,#32862,#32863,#32864,
#32865,#32866,#32867,#32868,#32869,#32870,#32871,#32872,#32873,#32874,#32875,
#32876,#32877,#32878,#32879,#32880,#32881,#32882,#32883,#32884,#32885,#32886,
#32887,#32888,#32889,#32890,#32891,#32892,#32893,#32894,#32895,#32896,#32897,
#32898,#32899,#32900,#32901,#32902,#32903,#32904,#32905,#32906,#32907,#32908,
#32909,#32910,#32911,#32912,#32913,#32914,#32915,#32916,#32917,#32918,#32919,
#32920,#32921,#32922,#32923,#32924,#32925,#32926,#32927,#32928,#32929,#32930,
#32931,#32932,#32933,#32934,#32935,#32936,#32937,#32938,#32939,#32940,#32941,
#32942,#32943,#32944,#32945,#32946,#32947,#32948,#32949,#32950,#32951,#32952,
#32953,#32954,#32955,#32956,#32957,#32958,#32959,#32960,#32961,#32962,#32963,
#32964,#32965,#32966,#32967,#32968,#32969,#32970,#32971,#32972,#32973,#32974,
#32975,#32976,#32977,#32978,#32979,#32980,#32981,#32982,#32983,#32984,#32985,
#32986),.UNSPECIFIED.,.F.,.F.,(4,2,2,2,2,2,2,2,2,2,2,2,2,2,2,2,2,2,2,2,
2,2,2,2,2,2,2,2,2,2,2,2,2,2,2,2,2,2,2,2,2,2,2,2,2,2,2,2,2,2,2,2,2,2,2,2,
2,2,2,2,2,2,2,2,2,2,2,2,2,2,2,2,2,2,2,2,2,2,2,2,2,2,2,2,2,2,2,2,2,2,4),
(-4.06049364980017,-3.96866139070536,-3.95255903839914,-3.9444154364705,
-3.94309564450125,-3.94240737724522,-3.94184693705834,-3.94127902782022,
-3.94022201045625,-3.93672030874366,-3.8801640131647,-3.8300373435895,-3.80706276264304,
-3.78527254650186,-3.78268961523789,-3.7816596482364,-3.78071377924466,
-3.77968431546979,-3.77844649048488,-3.77537005049096,-3.74734732799323,
-3.71697821305132,-3.6962998178066,-3.65608093857318,-3.64017852313725,
-3.62766967682958,-3.62141692146495,-3.62019049188046,-3.61952217824578,
-3.61901754096701,-3.61845272181062,-3.61741098928874,-3.61403666025984,
-3.55820241672813,-3.50778814243148,-3.47643070140119,-3.46696621401963,
-3.46101947008403,-3.45924120706139,-3.45814370834501,-3.45713304752249,
-3.4558431340794,-3.45321254196592,-3.43717746574158,-3.43384312679982,
-3.37212957750837,-3.32470932208807,-3.30695277305295,-3.29870183039683,
-3.29737754200379,-3.29668832811293,-3.29612783737283,-3.29547511009567,
-3.29435025374507,-3.29010159809445,-3.21635846200697,-3.17126001971995,
-3.14988942362271,-3.14264901224802,-3.13941886065546,-3.1368961829819,
-3.13563390021424,-3.13465687985068,-3.13368355509557,-3.13230110724487,
-3.12855208993668,-3.06775336834345,-2.9789500764597,-2.97516854144059,
-2.97412713137047,-2.97349966836303,-2.9729356163634,-2.97220814106656,
-2.9706963011772,-2.96082353092394,-2.95829942735653,-2.95727566983203,
-2.95517028747666,-2.95347412150494,-2.87433020000749,-2.81798145144374,
-2.81550027424065,-2.81401931847202,-2.812681603728,-2.81167863470589,-2.81072678607212,
-2.80942503547035,-2.80616880559577,-2.76756834632102,-2.70523002298853,
-2.69196489035576),.UNSPECIFIED.);
#189=B_SPLINE_CURVE_WITH_KNOTS('',3,(#32992,#32993,#32994,#32995,#32996,
#32997,#32998,#32999,#33000,#33001,#33002,#33003,#33004,#33005,#33006,#33007,
#33008,#33009,#33010,#33011,#33012,#33013,#33014,#33015,#33016,#33017,#33018,
#33019,#33020,#33021,#33022,#33023,#33024,#33025,#33026,#33027,#33028,#33029,
#33030,#33031,#33032,#33033,#33034,#33035,#33036,#33037,#33038,#33039,#33040,
#33041,#33042,#33043,#33044,#33045,#33046,#33047,#33048,#33049,#33050,#33051,
#33052,#33053,#33054,#33055,#33056,#33057,#33058,#33059,#33060,#33061,#33062,
#33063,#33064,#33065,#33066,#33067,#33068,#33069,#33070,#33071,#33072,#33073,
#33074,#33075,#33076,#33077,#33078,#33079,#33080,#33081,#33082,#33083,#33084,
#33085,#33086,#33087,#33088,#33089,#33090,#33091,#33092,#33093,#33094,#33095,
#33096,#33097,#33098,#33099,#33100,#33101,#33102,#33103,#33104,#33105,#33106,
#33107,#33108,#33109,#33110,#33111,#33112,#33113,#33114,#33115,#33116,#33117,
#33118,#33119,#33120,#33121,#33122,#33123,#33124,#33125,#33126,#33127,#33128,
#33129,#33130,#33131,#33132,#33133,#33134,#33135,#33136,#33137,#33138,#33139,
#33140,#33141,#33142,#33143,#33144,#33145,#33146,#33147,#33148,#33149,#33150,
#33151,#33152,#33153,#33154,#33155,#33156,#33157,#33158,#33159,#33160,#33161,
#33162,#33163,#33164,#33165,#33166,#33167,#33168,#33169,#33170,#33171,#33172,
#33173,#33174,#33175,#33176,#33177,#33178,#33179,#33180,#33181,#33182,#33183),
 .UNSPECIFIED.,.F.,.F.,(4,2,2,2,2,2,2,2,2,2,2,2,2,2,2,2,2,2,2,2,2,2,2,2,
2,2,2,2,2,2,2,2,2,2,2,2,2,2,2,2,2,2,2,2,2,2,2,2,2,2,2,2,2,2,2,2,2,2,2,2,
2,2,2,2,2,2,2,2,2,2,2,2,2,2,2,2,2,2,2,2,2,2,2,2,2,2,2,2,2,2,2,2,2,2,2,4),
(-1.37001951989838,-1.33384195289187,-1.26133785759749,-1.24760580787192,
-1.23654230157084,-1.22495630350067,-1.22352980407576,-1.22280731905288,
-1.22227812068599,-1.22170429146137,-1.22113582362372,-1.21974712171214,
-1.2095995986987,-1.18308104469748,-1.12352466489329,-1.06710228130897,
-1.0633697212079,-1.06198971529999,-1.06101696096122,-1.06010501517379,
-1.05884796509702,-1.05640955239577,-1.03990757588112,-1.00033093638571,
-0.947195837943482,-0.903720431137309,-0.900932954136615,-0.899968085314147,
-0.899418688458909,-0.898911281841867,-0.898214619850739,-0.896882283209202,
-0.888337738108694,-0.868550043038094,-0.814546528250962,-0.745185651351431,
-0.740673568241149,-0.739013276713724,-0.738040788504815,-0.737128773352301,
-0.735871129118376,-0.734524479869948,-0.728222842193891,-0.718021986793223,
-0.682337936791953,-0.635731134367314,-0.598076770995967,-0.596458298713943,
-0.594800544145728,-0.591809615152871,-0.591283188419006,-0.579081164603803,
-0.577493919732226,-0.576748377870124,-0.576179961505855,-0.575567406708466,
-0.574939023825919,-0.573105369800482,-0.544728635128748,-0.500107086275291,
-0.451910338511425,-0.441517513350794,-0.419885336804425,-0.417014281960592,
-0.41569165656435,-0.414673252016707,-0.413579571932325,-0.411859799344166,
-0.409865506868128,-0.396389610103376,-0.365446471370298,-0.341222376621425,
-0.318160566437614,-0.274517963715436,-0.272105182548319,-0.256372834912897,
-0.254649353402521,-0.253958355429252,-0.253384943163644,-0.252793570499035,
-0.25219671151592,-0.25136007156341,-0.246251348546714,-0.207546439446267,
-0.194651593239625,-0.181213869054641,-0.100239945664783,-0.0950341502386947,
-0.0932732621206296,-0.0922807486901239,-0.0913737775822311,-0.0901588465965395,
-0.0888713470097294,-0.0868524128794112,-0.0723359041243272,-0.000961742289995632),
 .UNSPECIFIED.);
#190=B_SPLINE_CURVE_WITH_KNOTS('',3,(#33184,#33185,#33186,#33187,#33188,
#33189,#33190,#33191,#33192,#33193,#33194,#33195,#33196,#33197,#33198,#33199,
#33200,#33201,#33202,#33203,#33204,#33205,#33206,#33207,#33208,#33209,#33210,
#33211,#33212,#33213,#33214,#33215,#33216,#33217,#33218,#33219,#33220,#33221,
#33222,#33223,#33224,#33225,#33226,#33227,#33228,#33229,#33230,#33231,#33232,
#33233,#33234,#33235,#33236,#33237,#33238,#33239,#33240,#33241,#33242,#33243,
#33244,#33245,#33246,#33247,#33248,#33249,#33250,#33251,#33252,#33253,#33254,
#33255,#33256,#33257,#33258,#33259,#33260,#33261,#33262,#33263,#33264,#33265,
#33266,#33267,#33268,#33269,#33270,#33271,#33272,#33273,#33274,#33275),
 .UNSPECIFIED.,.F.,.F.,(4,2,2,2,2,2,2,2,2,2,2,2,2,2,2,2,2,2,2,2,2,2,2,2,
2,2,2,2,2,2,2,2,2,2,2,2,2,2,2,2,2,2,2,2,2,4),(-4.05995217237598,-3.99475064873395,
-3.99239309084335,-3.99118726501826,-3.99043689203184,-3.98973784624697,
-3.98918206399342,-3.9885391678781,-3.9874557803825,-3.98360629885765,-3.91942180184273,
-3.9051376068729,-3.8908785334912,-3.85007080180934,-3.83336891425697,-3.83124479407454,
-3.82991318853611,-3.82866655327123,-3.82775637303666,-3.82678000793462,
-3.82509844524642,-3.82044281481705,-3.74962028963249,-3.74162419627269,
-3.70879809816409,-3.6798014111963,-3.66924699556814,-3.66818817714662,
-3.6674994680967,-3.66684462282559,-3.66634077235861,-3.66576683106831,
-3.66467917256168,-3.66090773211612,-3.60017045671843,-3.54848408029227,
-3.5148781270311,-3.50849986378626,-3.50714908002633,-3.50588858365521,
-3.50497656199414,-3.50400599795984,-3.50235376785339,-3.49789099074952,
-3.42492520502034,-3.39946882069219),.UNSPECIFIED.);
#191=B_SPLINE_CURVE_WITH_KNOTS('',3,(#33276,#33277,#33278,#33279,#33280,
#33281,#33282,#33283,#33284,#33285,#33286,#33287,#33288,#33289,#33290,#33291,
#33292,#33293,#33294,#33295,#33296,#33297,#33298,#33299,#33300,#33301,#33302,
#33303,#33304,#33305,#33306,#33307,#33308,#33309,#33310,#33311,#33312,#33313,
#33314,#33315,#33316,#33317,#33318,#33319,#33320,#33321,#33322,#33323,#33324,
#33325,#33326,#33327,#33328,#33329,#33330,#33331,#33332,#33333,#33334,#33335,
#33336,#33337,#33338,#33339,#33340,#33341,#33342,#33343,#33344,#33345,#33346,
#33347,#33348,#33349,#33350,#33351,#33352,#33353,#33354,#33355,#33356,#33357,
#33358,#33359,#33360,#33361,#33362,#33363,#33364,#33365,#33366,#33367,#33368,
#33369,#33370,#33371,#33372,#33373,#33374,#33375,#33376,#33377,#33378,#33379,
#33380,#33381,#33382,#33383,#33384,#33385,#33386,#33387,#33388,#33389,#33390,
#33391,#33392,#33393,#33394,#33395,#33396,#33397,#33398,#33399,#33400,#33401,
#33402,#33403,#33404,#33405,#33406,#33407,#33408,#33409,#33410,#33411,#33412,
#33413,#33414,#33415,#33416,#33417,#33418,#33419,#33420,#33421,#33422,#33423,
#33424,#33425,#33426,#33427,#33428,#33429,#33430,#33431,#33432,#33433,#33434,
#33435,#33436,#33437,#33438,#33439,#33440,#33441,#33442,#33443,#33444,#33445,
#33446,#33447,#33448,#33449,#33450,#33451,#33452,#33453,#33454,#33455,#33456,
#33457,#33458,#33459,#33460,#33461,#33462,#33463,#33464,#33465,#33466,#33467,
#33468,#33469,#33470,#33471,#33472,#33473,#33474,#33475,#33476,#33477,#33478,
#33479,#33480,#33481,#33482,#33483,#33484,#33485,#33486,#33487,#33488,#33489,
#33490,#33491,#33492,#33493,#33494,#33495,#33496,#33497,#33498,#33499,#33500,
#33501,#33502,#33503,#33504,#33505,#33506,#33507,#33508,#33509,#33510,#33511,
#33512,#33513,#33514,#33515,#33516,#33517,#33518,#33519,#33520,#33521,#33522,
#33523,#33524,#33525,#33526,#33527,#33528,#33529,#33530,#33531,#33532,#33533,
#33534,#33535,#33536,#33537,#33538,#33539,#33540,#33541,#33542,#33543,#33544,
#33545,#33546,#33547,#33548,#33549,#33550,#33551,#33552,#33553,#33554,#33555,
#33556,#33557,#33558,#33559,#33560,#33561,#33562,#33563,#33564,#33565,#33566,
#33567,#33568,#33569,#33570,#33571,#33572,#33573,#33574,#33575,#33576,#33577,
#33578,#33579,#33580,#33581,#33582,#33583,#33584,#33585,#33586,#33587,#33588,
#33589,#33590,#33591,#33592,#33593,#33594,#33595,#33596,#33597,#33598,#33599,
#33600,#33601,#33602,#33603,#33604,#33605,#33606,#33607,#33608,#33609,#33610,
#33611),.UNSPECIFIED.,.F.,.F.,(4,2,2,2,2,2,2,2,2,2,2,2,2,2,2,2,2,2,2,2,
2,2,2,2,2,2,2,2,2,2,2,2,2,2,2,2,2,2,2,2,2,2,2,2,2,2,2,2,2,2,2,2,2,2,2,2,
2,2,2,2,2,2,2,2,2,2,2,2,2,2,2,2,2,2,2,2,2,2,2,2,2,2,2,2,2,2,2,2,2,2,2,2,
2,2,2,2,2,2,2,2,2,2,2,2,2,2,2,2,2,2,2,2,2,2,2,2,2,2,2,2,2,2,2,2,2,2,2,2,
2,2,2,2,2,2,2,2,2,2,2,2,2,2,2,2,2,2,2,2,2,2,2,2,2,2,2,2,2,2,2,2,2,2,2,2,
2,2,2,4),(-2.69196489035576,-2.67988559045034,-2.66107800437888,-2.65269711684396,
-2.65136739332156,-2.65067700027773,-2.65011639701367,-2.64946450122639,
-2.64834337365824,-2.64413288301269,-2.64349567442083,-2.54578389547178,
-2.49911939113242,-2.49453620938231,-2.49223385904833,-2.49082735431544,
-2.48954459194083,-2.4885507938991,-2.48758281537956,-2.48622000385684,
-2.48339889374229,-2.47581508456675,-2.47400015382847,-2.47193678833891,
-2.47148933910139,-2.47062461443719,-2.46855371434399,-2.46695506995453,
-2.46575129478937,-2.46444065989919,-2.45827356631885,-2.38571838321001,
-2.330258739869,-2.32852033246666,-2.32775002631261,-2.32717974506188,-2.32664554202916,
-2.32590379118526,-2.32399405212404,-2.29804251249304,-2.25171156679459,
-2.2060888523969,-2.18312433676677,-2.16998034497103,-2.16767958228923,
-2.16645779504977,-2.16545295007134,-2.16443875248404,-2.16257018495806,
-2.15653266842959,-2.05405147146666,-2.03059288953971,-2.02795099538641,
-2.02626273152047,-2.02445389510806,-2.02425389814089,-2.02314305604937,
-2.00721064544119,-2.00548133670361,-2.00478934362467,-2.00421563456035,
-2.00362452575462,-2.00274764102565,-2.00035253988194,-1.96210329101591,
-1.85430008258221,-1.85168624365058,-1.84587572233047,-1.84403529750454,
-1.84302680189967,-1.84212202067322,-1.84093412102918,-1.83879026784531,
-1.82850126216438,-1.8090713693667,-1.78519956919261,-1.70098479676786,
-1.69895577251532,-1.68399892624409,-1.68232056654595,-1.68162576425897,
-1.68105134834994,-1.68046125311061,-1.67960676025654,-1.67734877790507,
-1.62938870886335,-1.54844085202926,-1.54539611703954,-1.52454507442936,
-1.52198772160104,-1.52069082578682,-1.51974024311909,-1.51871587810522,
-1.51733329848258,-1.5142925425652,-1.45011390999799,-1.37512112675312,
-1.37479316486045,-1.37387542093885,-1.37341923927877,-1.37263447660971,
-1.36079264237841,-1.35935724985527,-1.3586325032763,-1.35810272307618,
-1.35752934585705,-1.3567572753458,-1.35499762202247,-1.35260484985482,
-1.2710783283939,-1.22588723761503,-1.22162903142905,-1.21934424734738,
-1.21812198170695,-1.21630783992385,-1.21422370822404,-1.21224081883573,
-1.21077579873681,-1.20721482531136,-1.20576588225377,-1.19983229342685,
-1.19797641401661,-1.1969647384673,-1.19595962164296,-1.19473348633175,
-1.19241247272377,-1.18091295522845,-1.15804148871034,-1.08276423329172,
-1.03946705626177,-1.03668747423758,-1.03572378946233,-1.03517462172065,
-1.03466713992901,-1.03396994051874,-1.03263511779166,-1.02402679529242,
-1.0039291879329,-0.948086213892002,-0.902803771305496,-0.898893146005888,
-0.893881055616372,-0.891801761847728,-0.891154082310333,-0.890039029968144,
-0.889115540919865,-0.887289902427046,-0.883327565552538,-0.876973433301037,
-0.875066941199996,-0.873931479739374,-0.873024199062098,-0.871807070094902,
-0.869528576053658,-0.857095394282192,-0.838747158648885,-0.799647291606531,
-0.759559952187023,-0.716546212439798,-0.713780390124337,-0.712818425487851,
-0.712269602632748,-0.711762029549724,-0.71106408384531,-0.709725724526045,
-0.701025637766398,-0.680505225341358,-0.661714306709516),.UNSPECIFIED.);
#192=B_SPLINE_CURVE_WITH_KNOTS('',3,(#33616,#33617,#33618,#33619,#33620,
#33621,#33622,#33623,#33624,#33625,#33626,#33627,#33628,#33629,#33630,#33631,
#33632,#33633,#33634,#33635,#33636,#33637,#33638,#33639,#33640,#33641,#33642,
#33643,#33644,#33645,#33646,#33647,#33648,#33649,#33650,#33651,#33652,#33653,
#33654,#33655,#33656,#33657,#33658,#33659,#33660,#33661,#33662,#33663,#33664,
#33665,#33666,#33667,#33668,#33669,#33670,#33671,#33672,#33673,#33674,#33675,
#33676,#33677,#33678,#33679,#33680,#33681,#33682,#33683,#33684,#33685,#33686,
#33687,#33688,#33689,#33690,#33691,#33692,#33693,#33694,#33695,#33696,#33697,
#33698,#33699,#33700,#33701,#33702,#33703,#33704,#33705,#33706,#33707,#33708,
#33709,#33710,#33711,#33712,#33713,#33714,#33715,#33716,#33717,#33718,#33719,
#33720,#33721,#33722,#33723,#33724,#33725,#33726,#33727,#33728,#33729,#33730,
#33731,#33732,#33733,#33734,#33735,#33736,#33737,#33738,#33739,#33740,#33741,
#33742,#33743,#33744,#33745,#33746,#33747,#33748,#33749,#33750,#33751,#33752,
#33753,#33754,#33755,#33756,#33757,#33758,#33759,#33760,#33761,#33762,#33763,
#33764,#33765,#33766,#33767,#33768,#33769,#33770,#33771,#33772,#33773,#33774,
#33775,#33776,#33777,#33778,#33779,#33780,#33781,#33782,#33783,#33784,#33785,
#33786,#33787,#33788,#33789,#33790,#33791,#33792,#33793,#33794,#33795,#33796,
#33797,#33798,#33799,#33800,#33801,#33802,#33803,#33804,#33805,#33806,#33807,
#33808,#33809,#33810,#33811,#33812,#33813,#33814,#33815,#33816,#33817,#33818,
#33819,#33820,#33821,#33822,#33823,#33824,#33825,#33826,#33827,#33828,#33829,
#33830,#33831,#33832,#33833,#33834,#33835,#33836,#33837,#33838,#33839,#33840,
#33841,#33842,#33843,#33844,#33845,#33846,#33847,#33848,#33849,#33850,#33851,
#33852,#33853,#33854,#33855,#33856,#33857,#33858,#33859,#33860,#33861,#33862,
#33863,#33864,#33865,#33866,#33867,#33868,#33869,#33870,#33871,#33872,#33873,
#33874,#33875,#33876,#33877,#33878,#33879,#33880,#33881,#33882,#33883,#33884,
#33885,#33886,#33887,#33888,#33889,#33890,#33891,#33892,#33893,#33894,#33895,
#33896,#33897,#33898,#33899),.UNSPECIFIED.,.F.,.F.,(4,2,2,2,2,2,2,2,2,2,
2,2,2,2,2,2,2,2,2,2,2,2,2,2,2,2,2,2,2,2,2,2,2,2,2,2,2,2,2,2,2,2,2,2,2,2,
2,2,2,2,2,2,2,2,2,2,2,2,2,2,2,2,2,2,2,2,2,2,2,2,2,2,2,2,2,2,2,2,2,2,2,2,
2,2,2,2,2,2,2,2,2,2,2,2,2,2,2,2,2,2,2,2,2,2,2,2,2,2,2,2,2,2,2,2,2,2,2,2,
2,2,2,2,2,2,2,2,2,2,2,2,2,2,2,2,2,2,2,2,2,2,2,4),(-3.40031960104545,-3.37858596566821,
-3.34204290278943,-3.33168699115945,-3.32531132939754,-3.32346950753675,
-3.32234862735041,-3.32133808197795,-3.32004957550031,-3.31742622783241,
-3.30153740563715,-3.30053095438386,-3.29930128700355,-3.29777364376238,
-3.29180859814735,-3.27479264786146,-3.24283400124832,-3.18866203903901,
-3.17114467939654,-3.16292553074839,-3.16160643778006,-3.16091263948229,
-3.16040562404612,-3.1598549752801,-3.1588836576919,-3.15605099527295,-3.1103052125235,
-3.0407147163238,-3.01591881111591,-3.00321260793306,-3.00101774548281,
-2.99976746258046,-2.99885650826735,-2.99788110490574,-2.99649114271921,
-2.99269384864625,-2.93531761642701,-2.87770281134715,-2.8570719781358,
-2.84562529006256,-2.83977837291701,-2.83857819205993,-2.83802966815972,
-2.8375182721867,-2.83698050159037,-2.83622540727387,-2.83423364764439,
-2.80272497666804,-2.7314140934218,-2.69590094049992,-2.6804715464637,-2.67807963767929,
-2.67682844972011,-2.67591738673668,-2.67494238861362,-2.67355387719879,
-2.66976591455326,-2.60902648728431,-2.52019032074541,-2.51770180162407,
-2.51588590489689,-2.51510374180658,-2.51452848317502,-2.5140010453154,
-2.51328543002819,-2.51188577842982,-2.50103889461304,-2.49942857461786,
-2.40946539578203,-2.35958570957843,-2.35566503077078,-2.35413334851507,
-2.35308040908138,-2.3520506535724,-2.35081186621672,-2.34772983687318,
-2.31951045513813,-2.2259320754401,-2.19733700502889,-2.19468992760766,
-2.19276870695664,-2.19196619409804,-2.19139012144277,-2.19086355734503,
-2.19015145757485,-2.18876553612407,-2.17827833288975,-2.17670156006277,
-2.17451949914548,-2.08502621756368,-2.06546906493039,-2.03936091916682,
-2.03312913572029,-2.03131609339564,-2.03031304396214,-2.02930695571249,
-2.02806555586855,-2.02567222034358,-2.01039884511247,-1.97554064878654,
-1.89815227362373,-1.87167018362919,-1.86975148487277,-1.86900816986545,
-1.86847349605867,-1.86790335156602,-1.86713430534119,-1.86540323608492,
-1.81571242479545,-1.71614175700479,-1.71008966041106,-1.70821930026172,
-1.70720473354506,-1.7061999024436,-1.70497868121193,-1.70272652743159,
-1.69042830226335,-1.6661152553706,-1.58690869782724,-1.55983328964038,
-1.54799534292228,-1.54656009026855,-1.54583538169979,-1.54530561369377,
-1.54473223422214,-1.54396016034049,-1.54220111552757,-1.53980898108709,
-1.45827977638008,-1.41309223717623,-1.40881050178752,-1.40666508229784,
-1.40545411777425,-1.40421398400976,-1.38835107555408,-1.38572890887072,
-1.38444059029022,-1.38343001168435,-1.38230890890245,-1.38046629664485,
-1.37408171694971,-1.37001951989838),.UNSPECIFIED.);
#193=B_SPLINE_CURVE_WITH_KNOTS('',3,(#33901,#33902,#33903,#33904,#33905,
#33906,#33907,#33908,#33909,#33910,#33911,#33912,#33913,#33914,#33915,#33916,
#33917,#33918,#33919,#33920,#33921,#33922,#33923,#33924,#33925,#33926,#33927,
#33928,#33929,#33930,#33931,#33932,#33933,#33934,#33935,#33936,#33937,#33938,
#33939,#33940,#33941,#33942,#33943,#33944,#33945,#33946,#33947,#33948,#33949,
#33950,#33951,#33952,#33953,#33954,#33955,#33956,#33957,#33958,#33959,#33960,
#33961,#33962,#33963,#33964,#33965,#33966,#33967,#33968,#33969,#33970,#33971,
#33972,#33973,#33974,#33975,#33976,#33977,#33978,#33979,#33980,#33981,#33982,
#33983,#33984,#33985,#33986,#33987,#33988,#33989,#33990,#33991,#33992,#33993,
#33994,#33995,#33996,#33997,#33998,#33999,#34000),.UNSPECIFIED.,.F.,.F.,
(4,2,2,2,2,2,2,2,2,2,2,2,2,2,2,2,2,2,2,2,2,2,2,2,2,2,2,2,2,2,2,2,2,2,2,
2,2,2,2,2,2,2,2,2,2,2,2,2,2,4),(-0.661714306709516,-0.635155861013257,-0.583147181177871,
-0.574707142993514,-0.571366622201943,-0.555318144873497,-0.552686488171391,
-0.551396203393642,-0.550385320760791,-0.549265151959854,-0.547426975559338,
-0.541085059986963,-0.505475926761696,-0.497652337254771,-0.450371680231509,
-0.394414259378906,-0.391021287407128,-0.389977145694693,-0.389411757926836,
-0.388907045632092,-0.388239249353062,-0.387532551854712,-0.384671068759998,
-0.380245335982904,-0.366458966434406,-0.340495778906067,-0.317962982724283,
-0.236109005414714,-0.230819846597213,-0.229047464661966,-0.22805257767202,
-0.227145905011295,-0.225935003271963,-0.223685485098539,-0.220909226800922,
-0.202745987705646,-0.161187663257189,-0.146183727652005,-0.138788425803437,
-0.130217995586827,-0.0806258233802182,-0.0689693567103825,-0.0675403915251483,
-0.0668172791246116,-0.0662879198343354,-0.0657142175003553,-0.0651459714985782,
-0.0643831854514484,-0.0631479869242733,-0.000961264455892619),
 .UNSPECIFIED.);
#194=B_SPLINE_CURVE_WITH_KNOTS('',3,(#34001,#34002,#34003,#34004,#34005,
#34006,#34007,#34008,#34009,#34010,#34011,#34012,#34013,#34014,#34015,#34016,
#34017,#34018,#34019,#34020,#34021,#34022,#34023,#34024,#34025,#34026,#34027,
#34028,#34029,#34030,#34031,#34032,#34033,#34034,#34035,#34036,#34037,#34038,
#34039,#34040,#34041,#34042,#34043,#34044,#34045,#34046,#34047,#34048,#34049,
#34050,#34051,#34052,#34053,#34054,#34055,#34056,#34057,#34058,#34059,#34060,
#34061,#34062,#34063,#34064,#34065,#34066,#34067,#34068,#34069,#34070,#34071,
#34072,#34073,#34074,#34075,#34076,#34077,#34078,#34079,#34080,#34081,#34082,
#34083,#34084,#34085,#34086,#34087,#34088,#34089,#34090,#34091,#34092,#34093,
#34094,#34095,#34096,#34097,#34098,#34099,#34100,#34101,#34102,#34103,#34104,
#34105,#34106,#34107,#34108,#34109,#34110,#34111,#34112,#34113,#34114,#34115,
#34116,#34117,#34118,#34119,#34120,#34121,#34122,#34123,#34124,#34125,#34126,
#34127,#34128,#34129,#34130,#34131,#34132,#34133,#34134,#34135,#34136,#34137,
#34138,#34139,#34140,#34141,#34142,#34143,#34144,#34145,#34146,#34147,#34148,
#34149,#34150,#34151,#34152,#34153,#34154,#34155,#34156,#34157,#34158,#34159,
#34160,#34161,#34162,#34163,#34164,#34165,#34166,#34167,#34168,#34169,#34170,
#34171,#34172,#34173,#34174,#34175,#34176,#34177,#34178,#34179,#34180,#34181,
#34182,#34183,#34184,#34185,#34186,#34187,#34188,#34189,#34190,#34191,#34192),
 .UNSPECIFIED.,.F.,.F.,(4,2,2,2,2,2,2,2,2,2,2,2,2,2,2,2,2,2,2,2,2,2,2,2,
2,2,2,2,2,2,2,2,2,2,2,2,2,2,2,2,2,2,2,2,2,2,2,2,2,2,2,2,2,2,2,2,2,2,2,2,
2,2,2,2,2,2,2,2,2,2,2,2,2,2,2,2,2,2,2,2,2,2,2,2,2,2,2,2,2,2,2,2,2,2,2,4),
(-4.06120250444192,-3.99918442014338,-3.97930631026375,-3.97245430131076,
-3.96935382217528,-3.96689338419594,-3.96563804961657,-3.96472638594267,
-3.96375302634548,-3.96237065236763,-3.95862258174264,-3.90197817663135,
-3.87117623880489,-3.85915084194773,-3.84812713630132,-3.81980140646837,
-3.80615166927202,-3.80510122143711,-3.80441592066061,-3.80387424306457,
-3.80331294082442,-3.80275215296733,-3.80173052296751,-3.79851873396886,
-3.74327229041295,-3.71494410090933,-3.6820950081722,-3.65823012307622,
-3.64615291672165,-3.64389356966248,-3.64268062290855,-3.6417738315662,
-3.64078022087196,-3.63901390721368,-3.63376858894774,-3.55236588816066,
-3.51059901844262,-3.48507450573197,-3.48222466351395,-3.48151912684793,
-3.48097104919064,-3.48045987573046,-3.47992145824065,-3.47916408216207,
-3.47715895957184,-3.44457366375936,-3.43584770632301,-3.42618038379795,
-3.37804415611762,-3.33968680552567,-3.32350191370376,-3.32106250917843,
-3.31981148624461,-3.31890034081292,-3.31792506269318,-3.31625071151002,
-3.31164612546338,-3.24124622179403,-3.19662978553869,-3.17022921840333,
-3.16011078401114,-3.15872301741472,-3.15815464487417,-3.15758087265336,
-3.15705160030086,-3.15632882902214,-3.15490121035853,-3.14328347454265,
-3.1406562807068,-3.13821322748276,-3.1346856309721,-3.12962043349618,-3.11148376149684,
-3.04837543566185,-3.01526736944768,-3.00046351012277,-2.99807808490597,
-2.99683832600884,-2.99592858525164,-2.99494830051684,-2.99354091861809,
-2.98963027343245,-2.92607188418165,-2.86227859042434,-2.8399373648659,
-2.83763714710976,-2.83593073722175,-2.83516938076277,-2.83459790074512,
-2.83406537021941,-2.83333014668725,-2.83145934582591,-2.80775271161947,
-2.79712977109084,-2.714856685761,-2.69222113602705),.UNSPECIFIED.);
#195=B_SPLINE_CURVE_WITH_KNOTS('',3,(#34198,#34199,#34200,#34201,#34202,
#34203,#34204,#34205,#34206,#34207,#34208,#34209,#34210,#34211,#34212,#34213,
#34214,#34215,#34216,#34217,#34218,#34219,#34220,#34221,#34222,#34223,#34224,
#34225,#34226,#34227,#34228,#34229,#34230,#34231,#34232,#34233,#34234,#34235,
#34236,#34237,#34238,#34239,#34240,#34241,#34242,#34243,#34244,#34245,#34246,
#34247,#34248,#34249,#34250,#34251,#34252,#34253,#34254,#34255,#34256,#34257,
#34258,#34259,#34260,#34261,#34262,#34263,#34264,#34265,#34266,#34267,#34268,
#34269,#34270,#34271,#34272,#34273,#34274,#34275,#34276,#34277,#34278,#34279,
#34280,#34281,#34282,#34283,#34284,#34285,#34286,#34287,#34288,#34289,#34290,
#34291,#34292,#34293,#34294,#34295,#34296,#34297,#34298,#34299,#34300,#34301,
#34302,#34303,#34304,#34305,#34306,#34307,#34308,#34309,#34310,#34311,#34312,
#34313,#34314,#34315,#34316,#34317,#34318,#34319,#34320,#34321,#34322,#34323,
#34324,#34325,#34326,#34327,#34328,#34329,#34330,#34331,#34332,#34333,#34334,
#34335,#34336,#34337,#34338,#34339,#34340,#34341,#34342,#34343,#34344,#34345,
#34346,#34347,#34348,#34349,#34350,#34351,#34352,#34353,#34354,#34355,#34356,
#34357,#34358,#34359,#34360,#34361,#34362,#34363,#34364,#34365,#34366,#34367,
#34368,#34369,#34370,#34371,#34372,#34373,#34374,#34375,#34376,#34377,#34378,
#34379,#34380,#34381,#34382,#34383,#34384,#34385,#34386,#34387,#34388,#34389,
#34390,#34391,#34392,#34393,#34394,#34395,#34396,#34397,#34398,#34399,#34400,
#34401,#34402,#34403,#34404,#34405,#34406,#34407),.UNSPECIFIED.,.F.,.F.,
(4,2,2,2,2,2,2,2,2,2,2,2,2,2,2,2,2,2,2,2,2,2,2,2,2,2,2,2,2,2,2,2,2,2,2,
2,2,2,2,2,2,2,2,2,2,2,2,2,2,2,2,2,2,2,2,2,2,2,2,2,2,2,2,2,2,2,2,2,2,2,2,
2,2,2,2,2,2,2,2,2,2,2,2,2,2,2,2,2,2,2,2,2,2,2,2,2,2,2,2,2,2,2,2,2,4),(-1.36937854035984,
-1.3634723172623,-1.36174551579247,-1.36105398332151,-1.36048044199618,
-1.3598892754706,-1.35902954674267,-1.35673782810181,-1.30561628549484,
-1.24518139507054,-1.23373512806729,-1.20443443429959,-1.20163398311029,
-1.20027617363742,-1.19930948876856,-1.19839546191318,-1.197123221391,-1.19473789085815,
-1.17963189870071,-1.14506164471568,-1.0819184269639,-1.05671224188495,
-1.0557654430992,-1.05430451933929,-1.05380442215256,-1.05184664337504,
-1.04032362847726,-1.03874188451195,-1.03800878870454,-1.03744232841611,
-1.03682410748946,-1.03584393506711,-1.03264004028301,-1.0275140900212,
-1.01193481096117,-0.978707848292629,-0.93541628780569,-0.882128556336615,
-0.878666290770821,-0.877329857912462,-0.876368888755633,-0.875350586908099,
-0.8740056306571,-0.871167353657731,-0.835381480546332,-0.771769022766303,
-0.726250094588251,-0.725595403448691,-0.717169854782103,-0.715747541190581,
-0.715028194408765,-0.714465095903045,-0.713833010668201,-0.713176561917826,
-0.710921843950462,-0.707655461199289,-0.698524134151089,-0.673564283352825,
-0.633946561607865,-0.560604246141025,-0.556081471880356,-0.554419573164736,
-0.55344678419226,-0.552534899794554,-0.551278081413968,-0.549932564568261,
-0.543645083808342,-0.508881080530274,-0.501253350917058,-0.455119433085655,
-0.396923393145763,-0.393520610808073,-0.392475334735496,-0.391909747875618,
-0.391349007866288,-0.390656599058156,-0.389915581689917,-0.386570632367781,
-0.381152934825141,-0.364119840930446,-0.340063053735909,-0.317930664649403,
-0.238269110764213,-0.233253075657426,-0.231518773744755,-0.230531577436619,
-0.229623544168816,-0.228398350895961,-0.227096625067705,-0.225043965494342,
-0.208355550753423,-0.165744796485386,-0.150885342385304,-0.143597289840791,
-0.135040167623944,-0.0743255391874357,-0.0706175783568126,-0.0695366968133647,
-0.0689639436512813,-0.0684597903981726,-0.067802685786858,-0.0671109274784547,
-0.0660451376037627,-0.0640569238606386,-0.000961349633723722),
 .UNSPECIFIED.);
#196=B_SPLINE_CURVE_WITH_KNOTS('',3,(#34408,#34409,#34410,#34411,#34412,
#34413,#34414,#34415,#34416,#34417,#34418,#34419,#34420,#34421,#34422,#34423,
#34424,#34425,#34426,#34427,#34428,#34429,#34430,#34431,#34432,#34433,#34434,
#34435,#34436,#34437,#34438,#34439,#34440,#34441,#34442,#34443,#34444,#34445,
#34446,#34447,#34448,#34449,#34450,#34451,#34452,#34453,#34454,#34455,#34456,
#34457,#34458,#34459,#34460,#34461,#34462,#34463,#34464,#34465,#34466,#34467,
#34468,#34469,#34470,#34471,#34472,#34473,#34474,#34475,#34476,#34477,#34478,
#34479,#34480,#34481,#34482,#34483,#34484,#34485,#34486,#34487,#34488,#34489,
#34490,#34491,#34492,#34493,#34494,#34495,#34496,#34497,#34498,#34499,#34500,
#34501,#34502,#34503,#34504,#34505,#34506,#34507,#34508,#34509),
 .UNSPECIFIED.,.F.,.F.,(4,2,2,2,2,2,2,2,2,2,2,2,2,2,2,2,2,2,2,2,2,2,2,2,
2,2,2,2,2,2,2,2,2,2,2,2,2,2,2,2,2,2,2,2,2,2,2,2,2,2,4),(-4.06158595367141,
-4.02191754355619,-3.98734963289,-3.97734833853149,-3.97324013374581,-3.97111533590888,
-3.96978330937464,-3.96853628165005,-3.96753917307828,-3.96654182376634,
-3.96475642043572,-3.95936871268148,-3.87622350691803,-3.86391678081209,
-3.85247414675814,-3.82310764940002,-3.80929454365039,-3.80812519526036,
-3.80739000471178,-3.80670181649038,-3.80614140211298,-3.8055734862844,
-3.80451636353468,-3.80101354542866,-3.74444596338195,-3.72113619440367,
-3.69709789171262,-3.66401823454813,-3.65427615660725,-3.64819485858441,
-3.64686248993489,-3.64561519624684,-3.64461800613461,-3.64347468226601,
-3.64153236229673,-3.63693442007136,-3.5572789157746,-3.51424151727211,
-3.48764104228835,-3.48502935485469,-3.48434259350246,-3.48368906778184,
-3.48318504496849,-3.4826096305786,-3.48151537191065,-3.47768666159424,
-3.47525602581653,-3.47259664401322,-3.47181539190525,-3.42656940651116,
-3.40031960104545),.UNSPECIFIED.);
#197=B_SPLINE_CURVE_WITH_KNOTS('',3,(#34510,#34511,#34512,#34513,#34514,
#34515,#34516,#34517,#34518,#34519,#34520,#34521,#34522,#34523,#34524,#34525,
#34526,#34527,#34528,#34529,#34530,#34531,#34532,#34533,#34534,#34535,#34536,
#34537,#34538,#34539,#34540,#34541,#34542,#34543,#34544,#34545,#34546,#34547,
#34548,#34549,#34550,#34551,#34552,#34553,#34554,#34555,#34556,#34557,#34558,
#34559,#34560,#34561,#34562,#34563,#34564,#34565,#34566,#34567,#34568,#34569,
#34570,#34571,#34572,#34573,#34574,#34575,#34576,#34577,#34578,#34579,#34580,
#34581,#34582,#34583,#34584,#34585,#34586,#34587,#34588,#34589,#34590,#34591,
#34592,#34593,#34594,#34595,#34596,#34597,#34598,#34599,#34600,#34601,#34602,
#34603,#34604,#34605,#34606,#34607,#34608,#34609,#34610,#34611,#34612,#34613,
#34614,#34615,#34616,#34617,#34618,#34619,#34620,#34621,#34622,#34623,#34624,
#34625,#34626,#34627,#34628,#34629,#34630,#34631,#34632,#34633,#34634,#34635,
#34636,#34637,#34638,#34639,#34640,#34641,#34642,#34643,#34644,#34645,#34646,
#34647,#34648,#34649,#34650,#34651,#34652,#34653,#34654,#34655,#34656,#34657,
#34658,#34659,#34660,#34661,#34662,#34663,#34664,#34665,#34666,#34667,#34668,
#34669,#34670,#34671,#34672,#34673,#34674,#34675,#34676,#34677,#34678,#34679,
#34680,#34681,#34682,#34683,#34684,#34685,#34686,#34687,#34688,#34689,#34690,
#34691,#34692,#34693,#34694,#34695,#34696,#34697,#34698,#34699,#34700,#34701,
#34702,#34703,#34704,#34705,#34706,#34707,#34708,#34709,#34710,#34711,#34712,
#34713,#34714,#34715,#34716,#34717,#34718,#34719,#34720,#34721,#34722,#34723,
#34724,#34725,#34726,#34727,#34728,#34729,#34730,#34731,#34732,#34733,#34734,
#34735,#34736,#34737,#34738,#34739,#34740,#34741,#34742,#34743,#34744,#34745,
#34746,#34747,#34748,#34749,#34750,#34751,#34752,#34753,#34754,#34755,#34756,
#34757,#34758,#34759,#34760,#34761,#34762,#34763,#34764,#34765,#34766,#34767,
#34768,#34769,#34770,#34771,#34772,#34773,#34774,#34775,#34776,#34777,#34778,
#34779,#34780,#34781,#34782,#34783,#34784,#34785,#34786,#34787,#34788,#34789,
#34790,#34791,#34792,#34793,#34794,#34795,#34796,#34797,#34798,#34799,#34800,
#34801,#34802,#34803,#34804,#34805,#34806,#34807,#34808,#34809,#34810,#34811,
#34812,#34813,#34814,#34815,#34816,#34817,#34818,#34819,#34820,#34821,#34822,
#34823,#34824,#34825,#34826,#34827,#34828,#34829,#34830,#34831,#34832,#34833,
#34834,#34835,#34836,#34837,#34838,#34839,#34840,#34841,#34842,#34843,#34844,
#34845,#34846,#34847,#34848,#34849,#34850,#34851,#34852,#34853,#34854,#34855,
#34856,#34857,#34858,#34859),.UNSPECIFIED.,.F.,.F.,(4,2,2,2,2,2,2,2,2,2,
2,2,2,2,2,2,2,2,2,2,2,2,2,2,2,2,2,2,2,2,2,2,2,2,2,2,2,2,2,2,2,2,2,2,2,2,
2,2,2,2,2,2,2,2,2,2,2,2,2,2,2,2,2,2,2,2,2,2,2,2,2,2,2,2,2,2,2,2,2,2,2,2,
2,2,2,2,2,2,2,2,2,2,2,2,2,2,2,2,2,2,2,2,2,2,2,2,2,2,2,2,2,2,2,2,2,2,2,2,
2,2,2,2,2,2,2,2,2,2,2,2,2,2,2,2,2,2,2,2,2,2,2,2,2,2,2,2,2,2,2,2,2,2,2,2,
2,2,2,2,2,2,2,2,2,2,2,2,2,2,2,2,2,2,2,2,4),(-2.69222113602705,-2.69007669244753,
-2.67728559886547,-2.67498980848289,-2.67376902408037,-2.67276415203694,
-2.67174920237658,-2.66987714919404,-2.66381169811061,-2.66239029506412,
-2.65889458212385,-2.65771365598455,-2.65549007621675,-2.650889079938,-2.64873016428556,
-2.64248768955844,-2.63052833642712,-2.56038567940658,-2.53834384451203,
-2.51684845917666,-2.51459984263146,-2.5129260113745,-2.51216977746626,
-2.51159919277191,-2.51106530616863,-2.51032490437566,-2.50882741850581,
-2.49505223644312,-2.40113804136929,-2.3731638340581,-2.35533559392732,
-2.35244056477934,-2.35104898228777,-2.35002306809675,-2.34907467663945,
-2.34778633313151,-2.34460762651765,-2.30987302819446,-2.24691799208005,
-2.19411403221177,-2.19046574208848,-2.18943758639017,-2.18881310802637,
-2.18824837779029,-2.18752750157517,-2.18600948988397,-2.17600042327404,
-2.10549370050932,-2.06349067728953,-2.04216042947883,-2.03111750406284,
-2.02914656545614,-2.02787976873134,-2.02687153132289,-2.02573774188552,
-2.0238384252863,-2.01673629678524,-1.96837956833978,-1.8791335806374,-1.86832437764547,
-1.8669260711565,-1.86621077209071,-1.86568338541584,-1.86510799565668,
-1.86430922530314,-1.86241001255689,-1.85980111600087,-1.8319672512943,
-1.73464967918419,-1.72845447312895,-1.72709239599361,-1.72588815288837,
-1.72433173773147,-1.72225667399598,-1.7215350553389,-1.72078934587171,
-1.71882216875239,-1.71677840310659,-1.70839492383262,-1.70619283039254,
-1.70486991665283,-1.70385148127936,-1.70275795599506,-1.7010388204461,
-1.69575546139575,-1.66607484520001,-1.62177233162103,-1.56215191164498,
-1.5597680068299,-1.55860096947444,-1.55768257961346,-1.55583963904399,
-1.54525402936251,-1.54386436858947,-1.54315133126318,-1.5426245548735,
-1.54204874431662,-1.54124747040194,-1.53937190952313,-1.53678396528969,
-1.50935321250065,-1.43086455788118,-1.41287338972399,-1.40600106481876,
-1.40450612811347,-1.40331105485673,-1.39929948212293,-1.39856349846819,
-1.39786461242248,-1.39586020692061,-1.39363462371044,-1.38493149462545,
-1.38300040248388,-1.38174599027947,-1.38073889935247,-1.3795970567498,
-1.37770039473882,-1.37057596613914,-1.32162842904402,-1.25626955417356,
-1.2433875971673,-1.2416231741618,-1.2375937216333,-1.23683685254952,-1.2360231631778,
-1.22245729530725,-1.22082246530989,-1.22013541172246,-1.21956301247527,
-1.21897023129467,-1.2181031751475,-1.21575644509737,-1.1588175552152,-1.10529876343665,
-1.08818156626407,-1.08246838123858,-1.08106716718255,-1.07985348307207,
-1.07868891529225,-1.06278993416567,-1.06016589474539,-1.05887717959003,
-1.05786653079516,-1.05674559778234,-1.05494064439751,-1.04876535413208,
-1.02273995520031,-0.983768457662749,-0.939087701672631,-0.908653661530226,
-0.907330552650375,-0.905778085018777,-0.903340941370666,-0.902040061870972,
-0.898559695140791,-0.89750512534783,-0.896937665081658,-0.896377109344793,
-0.895687891046809,-0.894390377903307,-0.887647876153156,-0.873572102083395,
-0.854749327332244,-0.807608709245875,-0.793046201470491,-0.741237434638338,
-0.737789388646109,-0.736455278726315,-0.735494905655486,-0.734476244411601,
-0.733129139751278,-0.730236829094953,-0.705472169583721,-0.684076569345851,
-0.662296405813887),.UNSPECIFIED.);
#198=B_SPLINE_CURVE_WITH_KNOTS('',3,(#34864,#34865,#34866,#34867,#34868,
#34869,#34870,#34871,#34872,#34873,#34874,#34875,#34876,#34877,#34878,#34879,
#34880,#34881,#34882,#34883,#34884,#34885,#34886,#34887,#34888,#34889,#34890,
#34891,#34892,#34893,#34894,#34895,#34896,#34897,#34898,#34899,#34900,#34901,
#34902,#34903,#34904,#34905,#34906,#34907,#34908,#34909,#34910,#34911,#34912,
#34913,#34914,#34915,#34916,#34917,#34918,#34919,#34920,#34921,#34922,#34923,
#34924,#34925,#34926,#34927,#34928,#34929,#34930,#34931,#34932,#34933,#34934,
#34935,#34936,#34937,#34938,#34939,#34940,#34941,#34942,#34943,#34944,#34945,
#34946,#34947,#34948,#34949,#34950,#34951,#34952,#34953,#34954,#34955,#34956,
#34957,#34958,#34959,#34960,#34961,#34962,#34963,#34964,#34965,#34966,#34967,
#34968,#34969,#34970,#34971,#34972,#34973,#34974,#34975,#34976,#34977,#34978,
#34979,#34980,#34981,#34982,#34983,#34984,#34985,#34986,#34987,#34988,#34989,
#34990,#34991,#34992,#34993,#34994,#34995,#34996,#34997,#34998,#34999,#35000,
#35001,#35002,#35003,#35004,#35005,#35006,#35007,#35008,#35009,#35010,#35011,
#35012,#35013,#35014,#35015,#35016,#35017,#35018,#35019,#35020,#35021,#35022,
#35023,#35024,#35025,#35026,#35027,#35028,#35029,#35030,#35031,#35032,#35033,
#35034,#35035,#35036,#35037,#35038,#35039,#35040,#35041,#35042,#35043,#35044,
#35045,#35046,#35047,#35048,#35049,#35050,#35051,#35052,#35053,#35054,#35055,
#35056,#35057,#35058,#35059,#35060,#35061,#35062,#35063,#35064,#35065,#35066,
#35067,#35068,#35069,#35070,#35071,#35072,#35073,#35074,#35075,#35076,#35077,
#35078,#35079,#35080,#35081,#35082,#35083,#35084,#35085,#35086,#35087,#35088,
#35089,#35090,#35091,#35092,#35093,#35094,#35095,#35096,#35097,#35098,#35099,
#35100,#35101,#35102,#35103,#35104,#35105,#35106,#35107,#35108,#35109,#35110,
#35111,#35112,#35113,#35114,#35115,#35116,#35117,#35118,#35119,#35120,#35121,
#35122,#35123,#35124,#35125,#35126,#35127,#35128,#35129,#35130,#35131,#35132,
#35133,#35134,#35135,#35136,#35137,#35138,#35139,#35140,#35141,#35142,#35143,
#35144,#35145,#35146,#35147),.UNSPECIFIED.,.F.,.F.,(4,2,2,2,2,2,2,2,2,2,
2,2,2,2,2,2,2,2,2,2,2,2,2,2,2,2,2,2,2,2,2,2,2,2,2,2,2,2,2,2,2,2,2,2,2,2,
2,2,2,2,2,2,2,2,2,2,2,2,2,2,2,2,2,2,2,2,2,2,2,2,2,2,2,2,2,2,2,2,2,2,2,2,
2,2,2,2,2,2,2,2,2,2,2,2,2,2,2,2,2,2,2,2,2,2,2,2,2,2,2,2,2,2,2,2,2,2,2,2,
2,2,2,2,2,2,2,2,2,2,2,2,2,2,2,2,2,2,2,2,2,2,2,4),(-3.3997268905259,-3.3771628241713,
-3.33580946997168,-3.31958623260249,-3.30721025344548,-3.30100650200268,
-3.29978307411547,-3.29911548440289,-3.29861097737682,-3.29796123109853,
-3.29684884046162,-3.29272312729606,-3.21960477459023,-3.17514639748534,
-3.15281336210418,-3.14531925430101,-3.14200545004725,-3.13942995834573,
-3.13815685352547,-3.13718376212722,-3.13621593929206,-3.13485326258567,
-3.13203215755142,-3.12445058329786,-3.1226365225275,-3.12057358681922,
-3.12016219008537,-3.02643096784493,-3.00147711862295,-2.98091306671218,
-2.97760848151872,-2.97661677638162,-2.97600054632386,-2.97543360023269,
-2.97469671107584,-2.97309443211346,-2.96103256157469,-2.96041460730051,
-2.90278757345259,-2.84734695571871,-2.82211988874398,-2.8189222905335,
-2.81642226208569,-2.81516366249859,-2.81418542200147,-2.81321034088773,
-2.81182128215009,-2.80802918953171,-2.74673967723941,-2.70500090975098,
-2.68043397428133,-2.6596548145686,-2.65497819761206,-2.65385833165813,
-2.65321344878749,-2.65265235570614,-2.65195300785722,-2.65087341933944,
-2.64597870660815,-2.55003072503517,-2.52592121695208,-2.50193101117893,
-2.49728351518924,-2.49495755909327,-2.49354127869805,-2.49225164299211,
-2.49125621706937,-2.49029082036903,-2.48866550531583,-2.48437628302639,
-2.41860089249946,-2.3351499001201,-2.331698558582,-2.33069092234302,-2.33007111207734,
-2.3295052518304,-2.32877572167103,-2.32757182070025,-2.32304513326697,
-2.23259528749899,-2.19503804272193,-2.18588006768357,-2.17254437291696,
-2.17023488450645,-2.16901138462147,-2.16800664329261,-2.16699383285271,
-2.16513152212243,-2.15914335936802,-2.04353702228946,-2.03059217753551,
-2.02822635649256,-2.02430165344751,-2.02270650350391,-2.02196214656499,
-2.02066448263749,-2.00945136146132,-2.00788182360996,-2.00715103746717,
-2.00658490884384,-2.00596553805334,-2.00496019221423,-2.00153144610128,
-1.9796886182026,-1.9553774471919,-1.85436570928257,-1.8484384417654,-1.84658350234068,
-1.84557210638145,-1.84456711939132,-1.84334092750096,-1.84101915907977,
-1.82742228024506,-1.80313863628736,-1.71200382155643,-1.70391750093161,
-1.70151150895958,-1.69950436041351,-1.69889340012299,-1.69790082271575,
-1.68632120065326,-1.68489497096213,-1.68417257078319,-1.68364340965114,
-1.68306959561662,-1.68229509191869,-1.68052238064887,-1.67810713535117,
-1.62533341962038,-1.53500396945807,-1.52739156885379,-1.5245908151617,
-1.52323296988438,-1.52226630990573,-1.52135234762095,-1.52008026238806,
-1.51758886072771,-1.50045628761802,-1.45807328684913,-1.38463743457022,
-1.37932198100892,-1.36937854035984),.UNSPECIFIED.);
#199=B_SPLINE_CURVE_WITH_KNOTS('',3,(#35149,#35150,#35151,#35152,#35153,
#35154,#35155,#35156,#35157,#35158,#35159,#35160,#35161,#35162,#35163,#35164,
#35165,#35166,#35167,#35168,#35169,#35170,#35171,#35172,#35173,#35174,#35175,
#35176,#35177,#35178,#35179,#35180,#35181,#35182,#35183,#35184,#35185,#35186,
#35187,#35188,#35189,#35190,#35191,#35192,#35193,#35194,#35195,#35196,#35197,
#35198,#35199,#35200,#35201,#35202,#35203,#35204,#35205,#35206,#35207,#35208,
#35209,#35210,#35211,#35212,#35213,#35214,#35215,#35216,#35217,#35218,#35219,
#35220,#35221,#35222,#35223,#35224,#35225,#35226,#35227,#35228,#35229,#35230,
#35231,#35232,#35233,#35234,#35235,#35236,#35237,#35238,#35239,#35240,#35241,
#35242,#35243,#35244,#35245,#35246,#35247,#35248,#35249,#35250),
 .UNSPECIFIED.,.F.,.F.,(4,2,2,2,2,2,2,2,2,2,2,2,2,2,2,2,2,2,2,2,2,2,2,2,
2,2,2,2,2,2,2,2,2,2,2,2,2,2,2,2,2,2,2,2,2,2,2,2,2,2,4),(-0.662296405813887,
-0.635922143580946,-0.579178057163701,-0.575662803806911,-0.574604087012972,
-0.574035778638131,-0.573475275280843,-0.57278740858407,-0.572052717946922,
-0.568798381618287,-0.541102743316805,-0.495436529670279,-0.46387662861801,
-0.418219735819375,-0.414848173644762,-0.41352676323732,-0.412569725041022,
-0.411549196059965,-0.410190404548335,-0.408703849802014,-0.399799199677671,
-0.383732072701302,-0.347123216534896,-0.318961393345521,-0.272701284958046,
-0.271074414713863,-0.268857910349997,-0.267732393027013,-0.266277394276951,
-0.265427885007478,-0.253669165452721,-0.252236632201744,-0.251512608435462,
-0.250983010956051,-0.250409483142604,-0.249620739522225,-0.248745631022214,
-0.24268866252878,-0.203539279748206,-0.190232426429279,-0.17643499218325,
-0.0973312252954645,-0.092457088152077,-0.0907347286850655,-0.0897498971626706,
-0.0888412984790158,-0.0876112148140803,-0.0863027256173666,-0.084234053599299,
-0.0696288491241501,-0.00096165502097932),.UNSPECIFIED.);
#200=B_SPLINE_CURVE_WITH_KNOTS('',3,(#35251,#35252,#35253,#35254,#35255,
#35256,#35257,#35258,#35259,#35260,#35261,#35262,#35263,#35264,#35265,#35266,
#35267,#35268,#35269,#35270,#35271,#35272,#35273,#35274,#35275,#35276,#35277,
#35278,#35279,#35280,#35281,#35282,#35283,#35284,#35285,#35286,#35287,#35288,
#35289,#35290,#35291,#35292,#35293,#35294,#35295,#35296,#35297,#35298,#35299,
#35300,#35301,#35302,#35303,#35304,#35305,#35306,#35307,#35308,#35309,#35310,
#35311,#35312,#35313,#35314,#35315,#35316,#35317,#35318,#35319,#35320,#35321,
#35322,#35323,#35324,#35325,#35326,#35327,#35328,#35329,#35330,#35331,#35332,
#35333,#35334,#35335,#35336,#35337,#35338,#35339,#35340,#35341,#35342,#35343,
#35344,#35345,#35346,#35347,#35348,#35349,#35350,#35351,#35352,#35353,#35354,
#35355,#35356,#35357,#35358,#35359,#35360,#35361,#35362,#35363,#35364,#35365,
#35366,#35367,#35368,#35369,#35370,#35371,#35372,#35373,#35374,#35375,#35376,
#35377,#35378,#35379,#35380,#35381,#35382,#35383,#35384,#35385,#35386,#35387,
#35388,#35389,#35390,#35391,#35392),.UNSPECIFIED.,.F.,.F.,(4,3,3,3,3,3,
3,3,3,3,3,3,3,3,3,3,3,3,3,3,3,3,3,3,3,3,3,3,3,3,3,3,3,3,3,3,3,3,3,3,3,3,
3,3,3,3,3,4),(317.30085801257,317.426612624734,317.527898802443,317.620971746719,
317.713918586356,317.806766957541,317.899547462196,317.992292784352,318.085027749454,
318.177777167795,318.27062580853,318.363526249141,318.456582145226,318.527613457915,
318.620686402191,318.713633241828,318.806481613012,318.899262117668,318.992007439824,
319.084742404925,319.177491823266,319.270340464001,319.363240904613,319.456296800697,
319.527328113388,319.620401057664,319.713347897301,319.806196268486,319.898976773141,
319.991722095298,320.084457060399,320.17720647874,320.270055119475,320.362955560087,
320.456011456171,320.527042768861,320.620115713137,320.713062552774,320.805910923959,
320.898691428614,320.99143675077,321.084171715871,321.176921134213,321.269769774948,
321.362670215559,321.455726111644,321.526757424334,321.537850218284),
 .UNSPECIFIED.);
#201=B_SPLINE_CURVE_WITH_KNOTS('',3,(#35398,#35399,#35400,#35401,#35402,
#35403,#35404,#35405,#35406,#35407,#35408,#35409,#35410,#35411,#35412,#35413,
#35414,#35415,#35416,#35417,#35418,#35419,#35420,#35421,#35422,#35423,#35424,
#35425,#35426,#35427,#35428,#35429,#35430,#35431,#35432,#35433,#35434,#35435,
#35436,#35437,#35438,#35439,#35440,#35441,#35442,#35443,#35444,#35445,#35446,
#35447,#35448,#35449,#35450,#35451,#35452,#35453,#35454,#35455,#35456,#35457,
#35458,#35459,#35460,#35461,#35462,#35463,#35464,#35465,#35466,#35467,#35468,
#35469,#35470,#35471,#35472,#35473,#35474,#35475,#35476,#35477,#35478,#35479,
#35480,#35481,#35482,#35483,#35484,#35485,#35486,#35487,#35488,#35489,#35490,
#35491,#35492,#35493,#35494,#35495,#35496,#35497,#35498,#35499,#35500,#35501,
#35502,#35503,#35504,#35505,#35506,#35507,#35508,#35509,#35510,#35511,#35512,
#35513,#35514,#35515,#35516,#35517,#35518,#35519,#35520,#35521,#35522,#35523,
#35524,#35525,#35526,#35527,#35528,#35529,#35530,#35531,#35532,#35533,#35534,
#35535,#35536,#35537,#35538,#35539),.UNSPECIFIED.,.F.,.F.,(4,3,3,3,3,3,
3,3,3,3,3,3,3,3,3,3,3,3,3,3,3,3,3,3,3,3,3,3,3,3,3,3,3,3,3,3,3,3,3,3,3,3,
3,3,3,3,3,4),(323.584043319749,323.677168290332,323.770293186491,323.863442132054,
323.956705811341,324.050028268095,324.143522381568,324.224563879274,324.31763682355,
324.410583663187,324.503432034372,324.596212539027,324.688957861183,324.781692826285,
324.874442244626,324.967290885361,325.060191325973,325.153247222057,325.224278534747,
325.317351479023,325.41029831866,325.503146689845,325.5959271945,325.688672516656,
325.781407481758,325.874156900099,325.967005540834,326.059905981446,326.15296187753,
326.22399319022,326.317066134496,326.410012974133,326.502861345318,326.595641849973,
326.688387172129,326.781122137231,326.873871555572,326.966720196307,327.059620636918,
327.152676533003,327.223707845693,327.316769638063,327.409712089381,327.502560231227,
327.595337701616,327.688074190646,327.780808710477,327.820676619569),
 .UNSPECIFIED.);
#202=B_SPLINE_CURVE_WITH_KNOTS('',3,(#35540,#35541,#35542,#35543,#35544,
#35545,#35546,#35547,#35548,#35549,#35550,#35551,#35552,#35553,#35554,#35555,
#35556,#35557,#35558,#35559,#35560,#35561,#35562,#35563,#35564,#35565,#35566,
#35567,#35568,#35569,#35570,#35571,#35572,#35573,#35574,#35575,#35576,#35577,
#35578,#35579,#35580,#35581,#35582,#35583,#35584,#35585,#35586,#35587,#35588,
#35589,#35590,#35591,#35592,#35593,#35594,#35595,#35596,#35597,#35598,#35599,
#35600,#35601,#35602,#35603,#35604,#35605,#35606,#35607,#35608,#35609,#35610,
#35611,#35612,#35613,#35614,#35615,#35616,#35617,#35618,#35619,#35620,#35621,
#35622,#35623,#35624,#35625,#35626,#35627,#35628,#35629,#35630,#35631,#35632,
#35633),.UNSPECIFIED.,.F.,.F.,(4,2,2,2,2,2,2,2,2,2,2,2,2,2,2,2,2,2,2,2,
2,2,2,2,2,2,2,2,2,2,2,2,2,2,2,2,2,2,2,2,2,2,2,2,2,2,4),(-4.06047020503067,
-3.97913746508193,-3.95675138905933,-3.94703589900244,-3.94565686751046,
-3.94495626897608,-3.9444001811875,-3.94375797944412,-3.94267814510715,
-3.93886372511926,-3.93813114133112,-3.83525091816359,-3.81695395295451,
-3.79727610185871,-3.7869093526443,-3.78476606409044,-3.78378358585031,
-3.78281048023268,-3.78184265310799,-3.78048004407804,-3.77765931877126,
-3.747476617408,-3.71973348977647,-3.70078227916256,-3.6653111829581,-3.63837956341343,
-3.62425204445573,-3.62275850928821,-3.62203480495442,-3.621523763611,-3.62098562019866,
-3.62022884041364,-3.61822646690423,-3.58582521688203,-3.53072754904893,
-3.50179936755701,-3.47731315129606,-3.4688157931356,-3.46517712633776,
-3.4624011630548,-3.46108603969737,-3.46012434331055,-3.45917331974369,
-3.45787408608017,-3.45530690057294,-3.43416462328477,-3.3997268905259),
 .UNSPECIFIED.);
#203=B_SPLINE_CURVE_WITH_KNOTS('',3,(#35635,#35636,#35637,#35638,#35639,
#35640,#35641,#35642,#35643,#35644,#35645,#35646,#35647,#35648,#35649,#35650,
#35651,#35652,#35653,#35654,#35655,#35656,#35657,#35658,#35659,#35660,#35661,
#35662,#35663,#35664,#35665,#35666,#35667,#35668,#35669,#35670,#35671,#35672,
#35673,#35674,#35675,#35676,#35677,#35678,#35679,#35680,#35681,#35682,#35683,
#35684,#35685,#35686,#35687,#35688,#35689,#35690,#35691,#35692,#35693,#35694,
#35695,#35696,#35697,#35698,#35699,#35700,#35701,#35702,#35703,#35704),
 .UNSPECIFIED.,.F.,.F.,(4,3,3,3,3,3,3,3,3,3,3,3,3,3,3,3,3,3,3,3,3,3,3,4),
(321.537850218284,321.630906689133,321.723840353486,321.816678833244,321.909453844202,
322.002196630937,322.094932016044,322.187684809342,322.280538445769,322.373446537988,
322.466506761149,322.526472079807,322.619545024083,322.71249186372,322.805340234905,
322.89812073956,322.990866061716,323.083601026818,323.176350445159,323.269199085894,
323.362099526505,323.45515542259,323.52618673528,323.584043319749),
 .UNSPECIFIED.);
#204=B_SPLINE_CURVE_WITH_KNOTS('',3,(#35705,#35706,#35707,#35708,#35709,
#35710,#35711,#35712,#35713,#35714,#35715,#35716,#35717,#35718,#35719,#35720,
#35721,#35722,#35723,#35724,#35725,#35726,#35727,#35728,#35729,#35730,#35731,
#35732,#35733,#35734,#35735,#35736,#35737,#35738,#35739,#35740,#35741,#35742,
#35743,#35744,#35745,#35746,#35747,#35748,#35749,#35750,#35751,#35752,#35753,
#35754,#35755,#35756,#35757,#35758,#35759,#35760,#35761,#35762,#35763,#35764,
#35765,#35766,#35767,#35768,#35769,#35770,#35771,#35772,#35773,#35774,#35775,
#35776,#35777,#35778,#35779,#35780,#35781,#35782,#35783,#35784,#35785,#35786,
#35787,#35788,#35789,#35790,#35791,#35792,#35793,#35794,#35795,#35796,#35797,
#35798,#35799,#35800,#35801,#35802,#35803,#35804,#35805,#35806,#35807,#35808,
#35809,#35810,#35811,#35812,#35813,#35814,#35815,#35816,#35817,#35818,#35819,
#35820,#35821,#35822,#35823,#35824,#35825,#35826,#35827,#35828,#35829,#35830,
#35831,#35832,#35833,#35834,#35835,#35836,#35837,#35838,#35839,#35840,#35841,
#35842,#35843,#35844,#35845,#35846,#35847,#35848,#35849,#35850,#35851,#35852,
#35853,#35854,#35855,#35856,#35857,#35858,#35859,#35860,#35861,#35862,#35863,
#35864,#35865,#35866,#35867,#35868,#35869,#35870,#35871,#35872,#35873,#35874,
#35875,#35876,#35877,#35878,#35879,#35880,#35881,#35882),.UNSPECIFIED.,
 .F.,.F.,(4,2,2,2,2,2,2,2,2,2,2,2,2,2,2,2,2,2,2,2,2,2,2,2,2,2,2,2,2,2,2,
2,2,2,2,2,2,2,2,2,2,2,2,2,2,2,2,2,2,2,2,2,2,2,2,2,2,2,2,2,2,2,2,2,2,2,2,
2,2,2,2,2,2,2,2,2,2,2,2,2,2,2,2,2,2,2,2,2,4),(-4.06158467854896,-3.94923519837409,
-3.93599991200773,-3.92269161835556,-3.9203844843538,-3.91916195013851,
-3.91815785603613,-3.9171455743914,-3.91528387952344,-3.90929489692491,
-3.80707759085534,-3.780429788445,-3.76619296282042,-3.7616572197697,-3.75970599817688,
-3.75821443572828,-3.75749334496842,-3.75695237577373,-3.75641286978667,
-3.75549628555695,-3.75303613713578,-3.71082729871476,-3.68711829481489,
-3.63534543560341,-3.61305531884369,-3.59988583634365,-3.59758498231347,
-3.59636366562971,-3.59535947704117,-3.59434617080706,-3.59247990733709,
-3.58645506848342,-3.47028488122393,-3.44954831734609,-3.44091754313171,
-3.4377838867191,-3.43629841022243,-3.43543242139521,-3.43465982706144,
-3.43409669173043,-3.43356913708102,-3.43285237877034,-3.43144757090977,
-3.42044944837904,-3.37112334511462,-3.32644618364195,-3.29656769246454,
-3.27729574258921,-3.27476779063671,-3.27349887996492,-3.27258563400271,
-3.27161828333527,-3.27025709911317,-3.26744177157477,-3.23747617525587,
-3.15003519508914,-3.13680805481928,-3.12112328809136,-3.11616714365453,
-3.11408372764611,-3.11298141375338,-3.1122743967749,-3.1116395375029,-3.11109029036474,
-3.11052212319802,-3.10946342741072,-3.10594625200448,-3.10470127127753,
-3.00344560168929,-2.96917199121828,-2.95405383427677,-2.95166753945285,
-2.95042797212063,-2.94943171380618,-2.94843090627298,-2.94662747018178,
-2.94110146240276,-2.82165350108662,-2.79149660831535,-2.79012149833543,
-2.78930070309898,-2.78856044039257,-2.78800292280664,-2.78746653242957,
-2.78671645940916,-2.78475579041022,-2.75550863959052,-2.70226679468588,
-2.69256774355998),.UNSPECIFIED.);
#205=B_SPLINE_CURVE_WITH_KNOTS('',3,(#35888,#35889,#35890,#35891,#35892,
#35893,#35894,#35895,#35896,#35897,#35898,#35899,#35900,#35901,#35902,#35903,
#35904,#35905,#35906,#35907,#35908,#35909,#35910,#35911,#35912,#35913,#35914,
#35915,#35916,#35917,#35918,#35919,#35920,#35921,#35922,#35923,#35924,#35925,
#35926,#35927,#35928,#35929,#35930,#35931,#35932,#35933,#35934,#35935,#35936,
#35937,#35938,#35939,#35940,#35941,#35942,#35943,#35944,#35945,#35946,#35947,
#35948,#35949,#35950,#35951,#35952,#35953,#35954,#35955,#35956,#35957,#35958,
#35959,#35960,#35961,#35962,#35963,#35964,#35965,#35966,#35967,#35968,#35969,
#35970,#35971,#35972,#35973,#35974,#35975,#35976,#35977,#35978,#35979,#35980,
#35981,#35982,#35983,#35984,#35985,#35986,#35987,#35988,#35989,#35990,#35991,
#35992,#35993,#35994,#35995,#35996,#35997,#35998,#35999,#36000,#36001,#36002,
#36003,#36004,#36005,#36006,#36007,#36008,#36009,#36010,#36011,#36012,#36013,
#36014,#36015,#36016,#36017,#36018,#36019,#36020,#36021,#36022,#36023,#36024,
#36025,#36026,#36027,#36028,#36029,#36030,#36031,#36032,#36033,#36034,#36035,
#36036,#36037,#36038,#36039,#36040,#36041,#36042,#36043,#36044,#36045,#36046,
#36047,#36048,#36049,#36050,#36051,#36052,#36053,#36054,#36055,#36056,#36057,
#36058,#36059,#36060,#36061,#36062,#36063,#36064,#36065,#36066,#36067,#36068,
#36069,#36070,#36071,#36072,#36073,#36074,#36075,#36076,#36077,#36078,#36079,
#36080,#36081),.UNSPECIFIED.,.F.,.F.,(4,2,2,2,2,2,2,2,2,2,2,2,2,2,2,2,2,
2,2,2,2,2,2,2,2,2,2,2,2,2,2,2,2,2,2,2,2,2,2,2,2,2,2,2,2,2,2,2,2,2,2,2,2,
2,2,2,2,2,2,2,2,2,2,2,2,2,2,2,2,2,2,2,2,2,2,2,2,2,2,2,2,2,2,2,2,2,2,2,2,
2,2,2,2,2,2,2,4),(-1.36957890813418,-1.3469927902356,-1.28129777944894,
-1.25152420992124,-1.24871336565391,-1.24735327956401,-1.24638622643344,
-1.24541369757661,-1.24413920407232,-1.24156125744993,-1.23824079055204,
-1.21134103105977,-1.15226908486643,-1.09030224297907,-1.08659651797799,
-1.08551614712285,-1.08494363534349,-1.08443967805872,-1.08378280596457,
-1.08260835130867,-1.07718354387671,-1.0668852082195,-1.03720321283977,
-0.943982160690254,-0.927856248475247,-0.925221575850886,-0.92393113477301,
-0.922920735944101,-0.921824301649556,-0.920053931144378,-0.917957516927996,
-0.913923671016369,-0.904163212104042,-0.87096333445564,-0.768116345375349,
-0.767367264221802,-0.763564816951233,-0.762473575499792,-0.761898833557201,
-0.761394889744935,-0.760740763530272,-0.759579027392969,-0.754340217766761,
-0.669474815188671,-0.616912699767065,-0.614914589340625,-0.612703176358642,
-0.60399072960941,-0.602059251454564,-0.60080492525863,-0.599798125766958,
-0.598852927181849,-0.597159122101697,-0.591940639173503,-0.583933983672087,
-0.559813334771092,-0.530292740624415,-0.445331537452082,-0.444911824135395,
-0.440666295298508,-0.439541824557408,-0.438889228752894,-0.438328793300461,
-0.437639576422923,-0.436315066059272,-0.428056195575184,-0.410206857894458,
-0.365974713473903,-0.344819509431372,-0.31536455986921,-0.306912122631169,
-0.301949872315315,-0.297381658035824,-0.295320976351468,-0.291530083989753,
-0.287971479295353,-0.286522977077033,-0.280587581634551,-0.278731688241775,
-0.277720128875009,-0.27671520616753,-0.275752545798624,-0.274555248671002,
-0.270282797365475,-0.24423820822771,-0.22475262261072,-0.122157651599925,
-0.121329721449417,-0.117581853727496,-0.116496458495716,-0.115922778284382,
-0.115418633076506,-0.114762679901396,-0.11359321612561,-0.108246849665958,
-0.0271323909616345,-0.000962428845924314),.UNSPECIFIED.);
#206=B_SPLINE_CURVE_WITH_KNOTS('',3,(#36082,#36083,#36084,#36085,#36086,
#36087,#36088,#36089,#36090,#36091,#36092,#36093,#36094,#36095,#36096,#36097,
#36098,#36099,#36100,#36101,#36102,#36103,#36104,#36105,#36106,#36107,#36108,
#36109,#36110,#36111,#36112,#36113,#36114,#36115,#36116,#36117,#36118,#36119,
#36120,#36121,#36122,#36123,#36124,#36125,#36126,#36127,#36128,#36129,#36130,
#36131,#36132,#36133,#36134,#36135,#36136,#36137,#36138,#36139,#36140,#36141,
#36142,#36143,#36144,#36145,#36146,#36147,#36148,#36149,#36150,#36151),
 .UNSPECIFIED.,.F.,.F.,(4,3,3,3,3,3,3,3,3,3,3,3,3,3,3,3,3,3,3,3,3,3,3,4),
(327.820676619569,327.913439865354,328.006308009825,328.09923753556,328.192310868849,
328.223422501165,328.316495445441,328.409442285078,328.502290656262,328.595071160918,
328.687816483074,328.780551448175,328.873300866516,328.966149507252,329.059049947863,
329.152105843947,329.223137156638,329.316565251507,329.409866253897,329.50306464796,
329.596181863996,329.689249570431,329.782314572085,329.867228626929),
 .UNSPECIFIED.);
#207=B_SPLINE_CURVE_WITH_KNOTS('',3,(#36152,#36153,#36154,#36155,#36156,
#36157,#36158,#36159,#36160,#36161,#36162,#36163,#36164,#36165,#36166,#36167,
#36168,#36169,#36170,#36171,#36172,#36173,#36174,#36175,#36176,#36177,#36178,
#36179,#36180,#36181,#36182,#36183,#36184,#36185,#36186,#36187,#36188,#36189,
#36190,#36191,#36192,#36193,#36194,#36195,#36196,#36197,#36198,#36199,#36200,
#36201,#36202,#36203,#36204,#36205,#36206,#36207,#36208,#36209,#36210,#36211,
#36212,#36213,#36214,#36215,#36216,#36217,#36218,#36219,#36220,#36221,#36222,
#36223,#36224,#36225,#36226,#36227,#36228,#36229,#36230,#36231,#36232,#36233,
#36234,#36235,#36236,#36237,#36238,#36239,#36240,#36241,#36242,#36243,#36244,
#36245,#36246,#36247,#36248,#36249,#36250,#36251,#36252,#36253,#36254,#36255,
#36256,#36257,#36258,#36259,#36260,#36261,#36262,#36263,#36264,#36265,#36266,
#36267,#36268,#36269,#36270,#36271,#36272,#36273,#36274,#36275,#36276,#36277,
#36278,#36279,#36280,#36281,#36282,#36283,#36284,#36285,#36286,#36287,#36288,
#36289,#36290,#36291,#36292,#36293,#36294,#36295,#36296,#36297,#36298,#36299,
#36300,#36301,#36302,#36303,#36304,#36305,#36306,#36307,#36308,#36309,#36310,
#36311,#36312,#36313,#36314,#36315,#36316,#36317,#36318,#36319,#36320,#36321,
#36322,#36323,#36324,#36325,#36326,#36327,#36328,#36329,#36330,#36331,#36332,
#36333,#36334,#36335,#36336,#36337,#36338,#36339,#36340,#36341,#36342,#36343,
#36344,#36345,#36346,#36347,#36348,#36349,#36350,#36351,#36352,#36353,#36354,
#36355,#36356,#36357,#36358,#36359,#36360,#36361,#36362,#36363,#36364,#36365,
#36366,#36367,#36368,#36369,#36370,#36371,#36372,#36373,#36374,#36375,#36376,
#36377,#36378,#36379,#36380,#36381,#36382,#36383,#36384,#36385,#36386,#36387,
#36388,#36389,#36390,#36391,#36392,#36393,#36394,#36395,#36396,#36397,#36398,
#36399,#36400,#36401,#36402,#36403,#36404,#36405,#36406,#36407,#36408,#36409,
#36410,#36411,#36412,#36413,#36414,#36415,#36416,#36417,#36418,#36419,#36420,
#36421,#36422,#36423,#36424,#36425,#36426,#36427,#36428,#36429,#36430,#36431,
#36432,#36433,#36434,#36435,#36436,#36437,#36438,#36439,#36440,#36441),
 .UNSPECIFIED.,.F.,.F.,(4,2,2,2,2,2,2,2,2,2,2,2,2,2,2,2,2,2,2,2,2,2,2,2,
2,2,2,2,2,2,2,2,2,2,2,2,2,2,2,2,2,2,2,2,2,2,2,2,2,2,2,2,2,2,2,2,2,2,2,2,
2,2,2,2,2,2,2,2,2,2,2,2,2,2,2,2,2,2,2,2,2,2,2,2,2,2,2,2,2,2,2,2,2,2,2,2,
2,2,2,2,2,2,2,2,2,2,2,2,2,2,2,2,2,2,2,2,2,2,2,2,2,2,2,2,2,2,2,2,2,2,2,2,
2,2,2,2,2,2,2,2,2,2,2,2,4),(-2.69256774355998,-2.66996765412598,-2.63566077198389,
-2.62985109387609,-2.62808422619325,-2.62698018022388,-2.62596548190667,
-2.62466622748265,-2.62191704922497,-2.60331506507887,-2.60180195197674,
-2.5950314105217,-2.51817677740363,-2.48875635776303,-2.4700458035126,-2.46797349701839,
-2.46687536850086,-2.46617005212669,-2.46551300966961,-2.46498574490999,
-2.46432999646831,-2.46319213958975,-2.45881098272055,-2.45616494461932,
-2.45458776849015,-2.45322158818035,-2.35918880613108,-2.32412368799177,
-2.30801889969593,-2.30559418901551,-2.30434639556168,-2.3034358402617,
-2.30245952004982,-2.30106599394745,-2.29724499201814,-2.23938077463207,
-2.1797730545047,-2.15452365558019,-2.14467244427862,-2.14328889439957,
-2.1425873696778,-2.14202608198113,-2.1414656908577,-2.14044582356323,-2.13724668211284,
-2.08269059745371,-2.03178463617859,-2.01656255758589,-1.98624609127669,
-1.98342198169563,-1.98205845786337,-1.98109030822926,-1.98017700918456,
-1.97890913705524,-1.97638728378742,-1.95734236984911,-1.92807017578352,
-1.82572224798771,-1.82484877163046,-1.82113231211625,-1.82005042859805,
-1.81947744967867,-1.81897326980261,-1.8183163686792,-1.81714261509344,
-1.81173361166486,-1.80147795849957,-1.77218010118601,-1.66725100336038,
-1.66098835660767,-1.65909282521715,-1.65807322788367,-1.65709679229598,
-1.65600730015614,-1.65399156345612,-1.65153770550644,-1.59777846191563,
-1.50303865025389,-1.49813143157998,-1.49705063545071,-1.49635080202061,
-1.49578951729472,-1.49514463268809,-1.49402530364107,-1.4893583376198,
-1.46742676340644,-1.44241118702442,-1.38306936471926,-1.36372296834895,
-1.36003386894653,-1.33952399098644,-1.33669580755574,-1.33538124022475,
-1.33436404735965,-1.33328900351507,-1.3316102585462,-1.32964818383798,
-1.32596569920956,-1.29398676750816,-1.23402728794868,-1.17824008721575,
-1.17489067279343,-1.17385181917339,-1.1732874893112,-1.17272654098831,
-1.17203174405363,-1.17068125150515,-1.16177421683413,-1.14040191786627,
-1.03567646149139,-1.0338019612888,-1.0162034622433,-1.01349842175526,-1.0121936471515,
-1.01118107587685,-1.01009127412707,-1.00835068755469,-1.00629778474052,
-1.00237886405211,-0.992991521579222,-0.962168373499545,-0.912028914188886,
-0.855346795792154,-0.851836322314162,-0.850778213478055,-0.850210052297113,
-0.849649578891885,-0.848961582410445,-0.847643249812488,-0.839536101564362,
-0.824534978864349,-0.81011222550536,-0.799527976827988,-0.716224735434592,
-0.71417203858667,-0.693448939384863,-0.690612673562159,-0.689296705321461,
-0.688279434456218,-0.687205064749528,-0.685531850772112,-0.683575883153036,
-0.679908937780579,-0.671323053205383,-0.662358193112005),.UNSPECIFIED.);
#208=B_SPLINE_CURVE_WITH_KNOTS('',3,(#36446,#36447,#36448,#36449,#36450,
#36451,#36452,#36453,#36454,#36455,#36456,#36457,#36458,#36459,#36460,#36461,
#36462,#36463,#36464,#36465,#36466,#36467,#36468,#36469,#36470,#36471,#36472,
#36473,#36474,#36475,#36476,#36477,#36478,#36479,#36480,#36481,#36482,#36483,
#36484,#36485,#36486,#36487,#36488,#36489,#36490,#36491,#36492,#36493,#36494,
#36495,#36496,#36497,#36498,#36499,#36500,#36501,#36502,#36503,#36504,#36505,
#36506,#36507,#36508,#36509,#36510,#36511,#36512,#36513,#36514,#36515,#36516,
#36517,#36518,#36519,#36520,#36521,#36522,#36523,#36524,#36525,#36526,#36527,
#36528,#36529,#36530,#36531,#36532,#36533,#36534,#36535,#36536,#36537,#36538,
#36539,#36540,#36541,#36542,#36543,#36544,#36545,#36546,#36547,#36548,#36549,
#36550,#36551,#36552,#36553,#36554,#36555,#36556,#36557,#36558,#36559,#36560,
#36561,#36562,#36563,#36564,#36565,#36566,#36567,#36568,#36569,#36570,#36571,
#36572,#36573,#36574,#36575,#36576,#36577,#36578,#36579,#36580,#36581,#36582,
#36583,#36584,#36585,#36586,#36587,#36588,#36589,#36590,#36591,#36592,#36593,
#36594,#36595,#36596,#36597,#36598,#36599,#36600,#36601,#36602,#36603,#36604,
#36605,#36606,#36607,#36608,#36609,#36610,#36611,#36612,#36613,#36614,#36615,
#36616,#36617,#36618,#36619,#36620,#36621,#36622,#36623,#36624,#36625,#36626,
#36627,#36628,#36629,#36630,#36631,#36632,#36633,#36634,#36635,#36636,#36637,
#36638,#36639,#36640,#36641,#36642,#36643,#36644,#36645,#36646,#36647,#36648,
#36649,#36650,#36651,#36652,#36653,#36654,#36655,#36656,#36657,#36658,#36659,
#36660,#36661,#36662,#36663,#36664,#36665,#36666,#36667,#36668,#36669,#36670,
#36671,#36672,#36673,#36674,#36675,#36676,#36677,#36678,#36679,#36680,#36681,
#36682,#36683,#36684,#36685,#36686,#36687,#36688,#36689,#36690,#36691,#36692,
#36693,#36694,#36695,#36696,#36697,#36698,#36699,#36700,#36701,#36702,#36703,
#36704,#36705,#36706,#36707,#36708,#36709,#36710,#36711,#36712,#36713,#36714,
#36715,#36716,#36717,#36718,#36719,#36720,#36721,#36722,#36723,#36724,#36725,
#36726,#36727,#36728,#36729,#36730,#36731,#36732,#36733,#36734,#36735,#36736,
#36737,#36738,#36739,#36740,#36741,#36742,#36743,#36744,#36745,#36746,#36747,
#36748,#36749,#36750,#36751,#36752,#36753,#36754,#36755,#36756,#36757,#36758,
#36759,#36760,#36761,#36762,#36763,#36764,#36765),.UNSPECIFIED.,.F.,.F.,
(4,2,2,2,2,2,2,2,2,2,2,2,2,2,2,2,2,2,2,2,2,2,2,2,2,2,2,2,2,2,2,2,2,2,2,
2,2,2,2,2,2,2,2,2,2,2,2,2,2,2,2,2,2,2,2,2,2,2,2,2,2,2,2,2,2,2,2,2,2,2,2,
2,2,2,2,2,2,2,2,2,2,2,2,2,2,2,2,2,2,2,2,2,2,2,2,2,2,2,2,2,2,2,2,2,2,2,2,
2,2,2,2,2,2,2,2,2,2,2,2,2,2,2,2,2,2,2,2,2,2,2,2,2,2,2,2,2,2,2,2,2,2,2,2,
2,2,2,2,2,2,2,2,2,2,2,2,2,2,2,2,4),(-3.39861689288311,-3.39851652348514,
-3.36827023771839,-3.35602535036205,-3.34699561483257,-3.34564558857145,
-3.34494547623871,-3.34438453841218,-3.34382384136669,-3.34280163175715,
-3.33958389379969,-3.2885842080578,-3.23670937194651,-3.20258455361857,
-3.18753662018917,-3.18515915700513,-3.18390811145121,-3.18299746437958,
-3.1820232068261,-3.18063624436453,-3.17685553829957,-3.11569335840996,
-3.06628858321014,-3.03907612330084,-3.02449483328556,-3.02299860126879,
-3.02226845669901,-3.02175650609641,-3.02122078638098,-3.02047263358144,
-3.01852261416287,-2.98995595576426,-2.93814345150884,-2.89703691602468,
-2.87815288948963,-2.86470596169683,-2.86238812056126,-2.8611531181694,
-2.86014805802795,-2.8589936161466,-2.85705028863361,-2.85015738469181,
-2.84647027843376,-2.84490633688624,-2.84435319666325,-2.84294540478745,
-2.84233333239501,-2.84025219642572,-2.83875038684782,-2.83608980205276,
-2.83076484982645,-2.82380437727142,-2.80475873341698,-2.73981387447017,
-2.71432336364206,-2.70176394582584,-2.70028281793576,-2.6995556907845,
-2.69904421576642,-2.69850746631044,-2.6977555166482,-2.69578172595456,
-2.66555996394071,-2.58659208973241,-2.55615433323163,-2.54198489980303,
-2.53963623830013,-2.53839466110096,-2.53739841357727,-2.53625214003506,
-2.53429492945686,-2.52748614501906,-2.52375410452981,-2.52215215832779,
-2.52158904223564,-2.51968439490351,-2.51762162339136,-2.51649100574272,
-2.51365149540189,-2.42950603783512,-2.38122502499018,-2.3780325506904,
-2.37705572005625,-2.37643841495727,-2.37587207640918,-2.37513815952527,
-2.37355085025024,-2.36187058597992,-2.36096664951586,-2.3604068968493,
-2.32706861158301,-2.30473018161107,-2.25553440274245,-2.23129181515244,
-2.21900932405748,-2.21675210191722,-2.21553997139539,-2.21454543396193,
-2.21352870515074,-2.21164606736588,-2.20548761337272,-2.09640550436834,
-2.05726920926437,-2.05486155531322,-2.05398307363482,-2.05339179054112,
-2.05281863313086,-2.05212813671583,-2.05040691802231,-2.03473995067324,
-2.03342124108708,-2.03202265150054,-2.03068566771156,-2.00606142906807,
-1.90143488683449,-1.89518141067546,-1.89328739868671,-1.89226834765861,
-1.89127389965552,-1.89006522911721,-1.88782427961519,-1.87585350874735,
-1.85225864725069,-1.80696507188385,-1.77461275714598,-1.74769149736479,
-1.74715713969206,-1.74649456270382,-1.74540047671497,-1.73320818365469,
-1.7316218788423,-1.73087674393756,-1.73030862248911,-1.72969636994605,
-1.72872195418011,-1.72556893946214,-1.67344376111877,-1.60102359883175,
-1.59375478862298,-1.59176771332035,-1.59053921419318,-1.58953311838897,
-1.57365221254335,-1.57103011027865,-1.56974221440621,-1.56873214737932,
-1.56763435162468,-1.56585539872241,-1.56374849501562,-1.55968694774402,
-1.52200310950131,-1.43663997263336,-1.41082318375401,-1.40891624757298,
-1.40817511679209,-1.40764119906639,-1.40707106465453,-1.40630069128764,
-1.40456101703622,-1.36957890813418),.UNSPECIFIED.);
#209=B_SPLINE_CURVE_WITH_KNOTS('',3,(#36767,#36768,#36769,#36770,#36771,
#36772,#36773,#36774,#36775,#36776,#36777,#36778,#36779,#36780,#36781,#36782,
#36783,#36784,#36785,#36786,#36787,#36788,#36789,#36790,#36791,#36792,#36793,
#36794,#36795,#36796,#36797,#36798,#36799,#36800,#36801,#36802,#36803,#36804,
#36805,#36806,#36807,#36808,#36809,#36810,#36811,#36812,#36813,#36814,#36815,
#36816,#36817,#36818,#36819,#36820,#36821,#36822,#36823,#36824,#36825,#36826,
#36827,#36828,#36829,#36830,#36831,#36832,#36833,#36834,#36835,#36836,#36837,
#36838,#36839,#36840,#36841,#36842,#36843,#36844,#36845,#36846,#36847,#36848,
#36849,#36850,#36851,#36852,#36853,#36854,#36855,#36856,#36857,#36858,#36859,
#36860,#36861,#36862,#36863,#36864,#36865,#36866,#36867,#36868,#36869,#36870,
#36871,#36872,#36873,#36874,#36875,#36876,#36877,#36878,#36879,#36880,#36881,
#36882,#36883,#36884,#36885,#36886),.UNSPECIFIED.,.F.,.F.,(4,2,2,2,2,2,
2,2,2,2,2,2,2,2,2,2,2,2,2,2,2,2,2,2,2,2,2,2,2,2,2,2,2,2,2,2,2,2,2,2,2,2,
2,2,2,2,2,2,2,2,2,2,2,2,2,2,2,2,2,4),(-0.662358193112005,-0.647616252338287,
-0.614702519106575,-0.540092015397422,-0.52966865382535,-0.528285345126216,
-0.527573961132616,-0.527047617784055,-0.526471467835394,-0.525668281104276,
-0.523742771735117,-0.52108827083249,-0.492344765543757,-0.468341913570963,
-0.461357183285391,-0.455296062617719,-0.44995790422994,-0.40067392380545,
-0.370979369907446,-0.368169441813313,-0.366809275375872,-0.365841927592917,
-0.364869057430378,-0.363885777157978,-0.361736895955184,-0.351273079925747,
-0.331353298275014,-0.310014131092464,-0.216151449189928,-0.214553634804704,
-0.213070616363894,-0.210428850030765,-0.206041240766316,-0.204902546380952,
-0.204246494058574,-0.203691394797478,-0.203008260063377,-0.201713305942042,
-0.194138639463462,-0.17838142368069,-0.0853496718335142,-0.0796873961327089,
-0.072181127900674,-0.0669904556690061,-0.065437238334963,-0.0642295530878925,
-0.0628585826932495,-0.0607548061908026,-0.0602677090999533,-0.0565551932659298,
-0.052871225135495,-0.0459644942742916,-0.0440188418605291,-0.0428633689690836,
-0.041862153596501,-0.0408973949306642,-0.0396931275257946,-0.0378717285006105,
-0.0362097358738138,-0.000958175347923689),.UNSPECIFIED.);
#210=B_SPLINE_CURVE_WITH_KNOTS('',3,(#36887,#36888,#36889,#36890,#36891,
#36892,#36893,#36894,#36895,#36896,#36897,#36898,#36899,#36900,#36901,#36902,
#36903,#36904,#36905,#36906,#36907,#36908,#36909,#36910,#36911,#36912,#36913,
#36914,#36915,#36916,#36917,#36918,#36919,#36920,#36921,#36922,#36923,#36924,
#36925,#36926,#36927,#36928,#36929,#36930,#36931,#36932,#36933,#36934,#36935,
#36936,#36937,#36938,#36939,#36940,#36941,#36942,#36943,#36944,#36945,#36946,
#36947,#36948,#36949,#36950,#36951,#36952,#36953,#36954,#36955,#36956,#36957,
#36958,#36959,#36960,#36961,#36962,#36963,#36964,#36965,#36966,#36967,#36968,
#36969,#36970,#36971,#36972,#36973,#36974,#36975,#36976,#36977,#36978,#36979,
#36980,#36981,#36982,#36983,#36984,#36985,#36986,#36987,#36988,#36989,#36990,
#36991,#36992,#36993,#36994,#36995,#36996,#36997,#36998,#36999,#37000,#37001,
#37002,#37003,#37004,#37005,#37006,#37007,#37008,#37009,#37010,#37011,#37012,
#37013,#37014,#37015,#37016,#37017,#37018,#37019,#37020,#37021,#37022,#37023,
#37024,#37025,#37026,#37027,#37028),.UNSPECIFIED.,.F.,.F.,(4,3,3,3,3,3,
3,3,3,3,3,3,3,3,3,3,3,3,3,3,3,3,3,3,3,3,3,3,3,3,3,3,3,3,3,3,3,3,3,3,3,3,
3,3,3,3,3,4),(336.150413934108,336.255056496077,336.360156171105,336.465843880867,
336.522477256426,336.615550200702,336.708497040339,336.801345411524,336.894125916179,
336.986871238336,337.079606203437,337.172355621778,337.265204262513,337.358104703124,
337.451160599209,337.522191911899,337.615264856175,337.708211695812,337.801060066997,
337.893840571652,337.986585893809,338.07932085891,338.172070277251,338.264918917986,
338.357819358598,338.450875254682,338.521906567372,338.614979511648,338.707926351285,
338.80077472247,338.893555227125,338.986300549282,339.079035514383,339.171784932724,
339.264633573459,339.35753401407,339.450589910155,339.521621222845,339.614702988846,
339.711216056939,339.804052660664,339.896827067529,339.989564139875,340.082288702274,
340.175061494022,340.267863395383,340.360759758879,340.386807533587),
 .UNSPECIFIED.);
#211=B_SPLINE_CURVE_WITH_KNOTS('',3,(#37034,#37035,#37036,#37037,#37038,
#37039,#37040,#37041,#37042,#37043,#37044,#37045,#37046,#37047,#37048,#37049,
#37050,#37051,#37052,#37053,#37054,#37055,#37056,#37057,#37058,#37059,#37060,
#37061,#37062,#37063,#37064,#37065,#37066,#37067,#37068,#37069,#37070,#37071,
#37072,#37073,#37074,#37075,#37076,#37077,#37078,#37079,#37080,#37081,#37082,
#37083,#37084,#37085,#37086,#37087,#37088,#37089,#37090,#37091,#37092,#37093,
#37094,#37095,#37096,#37097,#37098,#37099,#37100,#37101,#37102,#37103,#37104,
#37105,#37106,#37107,#37108,#37109,#37110,#37111,#37112,#37113,#37114,#37115,
#37116,#37117,#37118,#37119,#37120,#37121,#37122,#37123,#37124,#37125,#37126,
#37127,#37128,#37129,#37130,#37131,#37132,#37133,#37134,#37135,#37136,#37137,
#37138,#37139,#37140,#37141,#37142,#37143,#37144,#37145,#37146,#37147,#37148,
#37149,#37150,#37151,#37152,#37153,#37154,#37155,#37156,#37157,#37158,#37159,
#37160,#37161,#37162,#37163,#37164,#37165,#37166,#37167,#37168,#37169,#37170,
#37171,#37172,#37173,#37174,#37175,#37176,#37177,#37178,#37179,#37180,#37181,
#37182,#37183,#37184,#37185,#37186,#37187,#37188,#37189,#37190,#37191,#37192,
#37193,#37194,#37195,#37196,#37197,#37198,#37199,#37200,#37201,#37202,#37203,
#37204,#37205,#37206,#37207,#37208,#37209,#37210,#37211,#37212,#37213,#37214,
#37215,#37216,#37217,#37218,#37219,#37220,#37221,#37222,#37223,#37224,#37225,
#37226,#37227,#37228,#37229),.UNSPECIFIED.,.F.,.F.,(4,2,2,2,2,2,2,2,2,2,
2,2,2,2,2,2,2,2,2,2,2,2,2,2,2,2,2,2,2,2,2,2,2,2,2,2,2,2,2,2,2,2,2,2,2,2,
2,2,2,2,2,2,2,2,2,2,2,2,2,2,2,2,2,2,2,2,2,2,2,2,2,2,2,2,2,2,2,2,2,2,2,2,
2,2,2,2,2,2,2,2,2,2,2,2,2,2,2,4),(-1.37005580231967,-1.33024580360612,-1.25976747071589,
-1.22732699997943,-1.22532367085035,-1.22456660024079,-1.22402827427647,
-1.22351707972821,-1.22279319089613,-1.2213293624247,-1.20834336199594,
-1.18312776894192,-1.1253464204192,-1.06882846069402,-1.06508845476252,
-1.06370733102199,-1.06273430621114,-1.06182252075083,-1.06056633840554,
-1.05812799461718,-1.04166633456679,-1.00224452419147,-0.947826806599637,
-0.905378626359692,-0.902642732017071,-0.901684988031656,-0.901137038948888,
-0.900629279587804,-0.899929567802679,-0.898582703622869,-0.889655800780411,
-0.868156124887796,-0.816947657365438,-0.771814035612302,-0.763968727815306,
-0.762576748009983,-0.761371407025166,-0.759881939527268,-0.757798152922224,
-0.757204406455709,-0.755598519374418,-0.754791288837574,-0.752392896527088,
-0.743795977717935,-0.741649397968903,-0.740342983766373,-0.739327099296034,
-0.738226187204517,-0.736473865355746,-0.730915072813556,-0.722236774576898,
-0.701245436118729,-0.63806871333048,-0.630014350343646,-0.582559398634975,
-0.579743080670572,-0.578774208415882,-0.57822401416436,-0.577716820865844,
-0.577021883151893,-0.576277351738385,-0.572875904693997,-0.546667491364594,
-0.503228306124239,-0.4243747544629,-0.419555190550068,-0.417849069572376,
-0.416867501604267,-0.415958154690557,-0.414721348299145,-0.413403532096508,
-0.407542562919724,-0.398252896075913,-0.368172590679002,-0.342495402157512,
-0.318402484770243,-0.260366926927176,-0.256928450608511,-0.255878891130257,
-0.255312448188767,-0.254751809138686,-0.254060907394055,-0.25332198162909,
-0.252143810125866,-0.23831051341243,-0.208329861789743,-0.196667345952084,
-0.184201381104297,-0.102044139889294,-0.0967295119488519,-0.094953789143961,
-0.0939582976298354,-0.09305183561242,-0.091842332165937,-0.090562366361816,
-0.088561293159636,-0.0740916733101073,-0.000961800400030715),
 .UNSPECIFIED.);
#212=B_SPLINE_CURVE_WITH_KNOTS('',3,(#37230,#37231,#37232,#37233,#37234,
#37235,#37236,#37237,#37238,#37239,#37240,#37241,#37242,#37243,#37244,#37245,
#37246,#37247,#37248,#37249,#37250,#37251,#37252,#37253,#37254,#37255,#37256,
#37257,#37258,#37259,#37260,#37261,#37262,#37263,#37264,#37265,#37266,#37267,
#37268,#37269,#37270,#37271,#37272,#37273,#37274,#37275,#37276,#37277,#37278,
#37279,#37280,#37281,#37282,#37283,#37284,#37285,#37286,#37287,#37288,#37289,
#37290,#37291,#37292,#37293,#37294,#37295,#37296,#37297,#37298,#37299,#37300,
#37301,#37302,#37303,#37304,#37305,#37306,#37307,#37308,#37309,#37310,#37311,
#37312,#37313,#37314,#37315,#37316,#37317,#37318,#37319,#37320,#37321,#37322,
#37323,#37324,#37325,#37326,#37327),.UNSPECIFIED.,.F.,.F.,(4,2,2,2,2,2,
2,2,2,2,2,2,2,2,2,2,2,2,2,2,2,2,2,2,2,2,2,2,2,2,2,2,2,2,2,2,2,2,2,2,2,2,
2,2,2,2,2,2,4),(-4.05896261844771,-3.99473034410128,-3.99274023828834,-3.9916739195815,
-3.99098209857863,-3.9903250601198,-3.98982122113935,-3.98924910602602,
-3.98817025384431,-3.98447649525557,-3.92166642543571,-3.90708517006878,
-3.89249015588519,-3.85066449864255,-3.83398016732095,-3.83189608600863,
-3.83058139021261,-3.82934700504211,-3.82843842056241,-3.82745669288872,
-3.82574776117373,-3.82090443335108,-3.7419525078443,-3.71863494111611,
-3.69238019397598,-3.67694520600631,-3.6720841731021,-3.66900756856252,
-3.6682853828613,-3.66760660682633,-3.66705210352949,-3.66648025187076,
-3.66540277632302,-3.66172140619556,-3.60235321536811,-3.54964971064022,
-3.51476279327677,-3.50907555017911,-3.50730945932002,-3.50620591410419,
-3.50519168646006,-3.50389304914685,-3.50114523135055,-3.48255403787029,
-3.48105085563132,-3.47649535737486,-3.46790799070911,-3.43040793471149,
-3.39861689288311),.UNSPECIFIED.);
#213=B_SPLINE_CURVE_WITH_KNOTS('',3,(#37329,#37330,#37331,#37332,#37333,
#37334,#37335,#37336,#37337,#37338,#37339,#37340,#37341,#37342,#37343,#37344,
#37345,#37346,#37347,#37348,#37349,#37350,#37351,#37352,#37353,#37354,#37355,
#37356,#37357,#37358,#37359,#37360,#37361,#37362,#37363,#37364,#37365,#37366,
#37367,#37368,#37369,#37370,#37371,#37372,#37373,#37374,#37375,#37376,#37377,
#37378,#37379,#37380,#37381,#37382,#37383,#37384,#37385,#37386,#37387,#37388,
#37389,#37390,#37391,#37392,#37393,#37394,#37395,#37396,#37397,#37398),
 .UNSPECIFIED.,.F.,.F.,(4,3,3,3,3,3,3,3,3,3,3,3,3,3,3,3,3,3,3,3,3,3,3,4),
(340.386807533587,340.479875861169,340.521335878318,340.614408822594,340.707355662231,
340.800204033416,340.892984538071,340.985729860227,341.078464825328,341.17121424367,
341.264062884405,341.356963325016,341.450019221101,341.521050533791,341.613050500166,
341.704925368368,341.796696229285,341.888409907799,341.980092335245,342.071769407751,
342.163522457848,342.255311878419,342.347246185093,342.43359924102),
 .UNSPECIFIED.);
#214=B_SPLINE_CURVE_WITH_KNOTS('',3,(#37399,#37400,#37401,#37402,#37403,
#37404,#37405,#37406,#37407,#37408,#37409,#37410,#37411,#37412,#37413,#37414,
#37415,#37416,#37417,#37418,#37419,#37420,#37421,#37422,#37423,#37424,#37425,
#37426,#37427,#37428,#37429,#37430,#37431,#37432,#37433,#37434,#37435,#37436,
#37437,#37438,#37439,#37440,#37441,#37442,#37443,#37444,#37445,#37446,#37447,
#37448,#37449,#37450,#37451,#37452,#37453,#37454,#37455,#37456,#37457,#37458,
#37459,#37460,#37461,#37462,#37463,#37464,#37465,#37466,#37467,#37468,#37469,
#37470,#37471,#37472,#37473,#37474,#37475,#37476,#37477,#37478,#37479,#37480,
#37481,#37482,#37483,#37484,#37485,#37486,#37487,#37488,#37489,#37490,#37491,
#37492,#37493,#37494,#37495,#37496,#37497,#37498,#37499,#37500,#37501,#37502,
#37503,#37504,#37505,#37506,#37507,#37508,#37509,#37510,#37511,#37512,#37513,
#37514,#37515,#37516,#37517,#37518,#37519,#37520,#37521,#37522,#37523,#37524,
#37525,#37526,#37527,#37528,#37529,#37530,#37531,#37532,#37533,#37534,#37535,
#37536,#37537,#37538,#37539,#37540,#37541,#37542,#37543,#37544,#37545,#37546,
#37547,#37548,#37549,#37550,#37551,#37552,#37553,#37554,#37555,#37556,#37557,
#37558,#37559,#37560,#37561,#37562,#37563,#37564,#37565,#37566,#37567,#37568,
#37569,#37570,#37571,#37572,#37573,#37574,#37575,#37576,#37577,#37578,#37579,
#37580,#37581,#37582,#37583,#37584,#37585,#37586,#37587,#37588,#37589,#37590,
#37591,#37592,#37593,#37594,#37595,#37596,#37597,#37598,#37599,#37600,#37601,
#37602,#37603,#37604,#37605,#37606,#37607,#37608,#37609,#37610,#37611,#37612,
#37613,#37614,#37615,#37616,#37617,#37618),.UNSPECIFIED.,.F.,.F.,(4,2,2,
2,2,2,2,2,2,2,2,2,2,2,2,2,2,2,2,2,2,2,2,2,2,2,2,2,2,2,2,2,2,2,2,2,2,2,2,
2,2,2,2,2,2,2,2,2,2,2,2,2,2,2,2,2,2,2,2,2,2,2,2,2,2,2,2,2,2,2,2,2,2,2,2,
2,2,2,2,2,2,2,2,2,2,2,2,2,2,2,2,2,2,2,2,2,2,2,2,2,2,2,2,2,2,2,2,2,2,4),
(-4.06090365677149,-4.03650691383421,-4.03503794306264,-4.03417874399937,
-4.03357297950052,-4.03304822228417,-4.0324815511079,-4.03174514766761,
-4.03014442835366,-4.01811042840495,-4.01602089160981,-4.01317938470109,
-4.00735164543766,-4.00361458512073,-3.91314864148911,-3.88841015083901,
-3.8755838029156,-3.8732995599677,-3.87208180539308,-3.87117511154732,-3.87004175666826,
-3.8681420646635,-3.86183775966219,-3.75546183898016,-3.73860015199207,
-3.72057574137164,-3.71510186543436,-3.7128600735121,-3.71119058723615,
-3.71043536912496,-3.70990277054107,-3.70937582265932,-3.70866129313091,
-3.70726500939176,-3.69649098928528,-3.69366958866057,-3.69249720088601,
-3.69169052936345,-3.68738954359101,-3.64083540286392,-3.63554893079418,
-3.62947718831727,-3.62238832983456,-3.61390976232042,-3.60334877943812,
-3.55406584824233,-3.55091995883006,-3.549532349416,-3.54850751750475,-3.54755881663269,
-3.54626804475409,-3.54307322948441,-3.50751592790596,-3.4253515613131,
-3.40466517629829,-3.39754077476591,-3.39223414559812,-3.3900430345461,
-3.38889974189793,-3.38793338559232,-3.3873277112151,-3.38676156172299,
-3.3860291877721,-3.38445023397392,-3.37298672281303,-3.37190600162919,
-3.28938725026323,-3.27789040266305,-3.24481470104432,-3.23000549721557,
-3.2276318155652,-3.22639493026571,-3.22548595260562,-3.22450519482492,
-3.22309492765316,-3.21916221855917,-3.21803989835553,-3.14422898426876,
-3.0958796153158,-3.07540150077243,-3.06963983773512,-3.06731164684711,
-3.06611677232777,-3.06511515865268,-3.06450136455486,-3.06393744727858,
-3.06320913044828,-3.06203503557193,-3.05581610874664,-2.94861772083537,
-2.90822775225174,-2.90507484152201,-2.90368603882563,-2.90266107104741,
-2.90171277293443,-2.9004233591971,-2.8972359902037,-2.86202406536336,-2.79827402491883,
-2.76610844390008,-2.74635411024007,-2.74421512002001,-2.74309167247973,
-2.74237585112871,-2.74173659961163,-2.74118706931024,-2.74062373911164,
-2.73958852076695,-2.73626490577119,-2.69269850522027),.UNSPECIFIED.);
#215=B_SPLINE_CURVE_WITH_KNOTS('',3,(#37623,#37624,#37625,#37626,#37627,
#37628,#37629,#37630,#37631,#37632,#37633,#37634,#37635,#37636,#37637,#37638,
#37639,#37640,#37641,#37642,#37643,#37644,#37645,#37646,#37647,#37648,#37649,
#37650,#37651,#37652,#37653,#37654,#37655,#37656,#37657,#37658,#37659,#37660,
#37661,#37662,#37663,#37664,#37665,#37666,#37667,#37668,#37669,#37670,#37671,
#37672,#37673,#37674,#37675,#37676,#37677,#37678,#37679,#37680,#37681,#37682,
#37683,#37684,#37685,#37686,#37687,#37688,#37689,#37690,#37691,#37692,#37693,
#37694,#37695,#37696,#37697,#37698,#37699,#37700,#37701,#37702,#37703,#37704,
#37705,#37706,#37707,#37708,#37709,#37710,#37711,#37712,#37713,#37714,#37715,
#37716,#37717,#37718,#37719,#37720,#37721,#37722,#37723,#37724,#37725,#37726,
#37727,#37728,#37729,#37730,#37731,#37732,#37733,#37734,#37735,#37736,#37737,
#37738,#37739,#37740,#37741,#37742,#37743,#37744,#37745,#37746,#37747,#37748,
#37749,#37750,#37751,#37752,#37753,#37754,#37755,#37756,#37757,#37758,#37759,
#37760,#37761,#37762,#37763,#37764,#37765,#37766,#37767,#37768,#37769,#37770,
#37771,#37772,#37773,#37774,#37775,#37776,#37777,#37778,#37779,#37780,#37781,
#37782,#37783,#37784,#37785,#37786,#37787,#37788,#37789,#37790,#37791,#37792,
#37793,#37794,#37795,#37796,#37797,#37798,#37799,#37800,#37801,#37802,#37803,
#37804,#37805,#37806,#37807,#37808,#37809,#37810,#37811,#37812,#37813,#37814,
#37815,#37816,#37817,#37818,#37819,#37820,#37821,#37822,#37823,#37824,#37825,
#37826,#37827,#37828,#37829,#37830,#37831,#37832,#37833,#37834,#37835,#37836,
#37837,#37838,#37839,#37840,#37841,#37842,#37843,#37844,#37845,#37846,#37847,
#37848,#37849,#37850,#37851,#37852,#37853,#37854,#37855,#37856,#37857,#37858,
#37859,#37860,#37861,#37862,#37863,#37864,#37865,#37866,#37867,#37868,#37869,
#37870,#37871,#37872,#37873,#37874,#37875,#37876,#37877,#37878,#37879,#37880,
#37881,#37882,#37883,#37884,#37885,#37886,#37887,#37888,#37889,#37890,#37891,
#37892,#37893,#37894,#37895,#37896,#37897,#37898,#37899,#37900),
 .UNSPECIFIED.,.F.,.F.,(4,2,2,2,2,2,2,2,2,2,2,2,2,2,2,2,2,2,2,2,2,2,2,2,
2,2,2,2,2,2,2,2,2,2,2,2,2,2,2,2,2,2,2,2,2,2,2,2,2,2,2,2,2,2,2,2,2,2,2,2,
2,2,2,2,2,2,2,2,2,2,2,2,2,2,2,2,2,2,2,2,2,2,2,2,2,2,2,2,2,2,2,2,2,2,2,2,
2,2,2,2,2,2,2,2,2,2,2,2,2,2,2,2,2,2,2,2,2,2,2,2,2,2,2,2,2,2,2,2,2,2,2,2,
2,2,2,2,2,2,4),(-3.40025096654499,-3.38155611820142,-3.34393882372037,-3.33338972967109,
-3.32692255626889,-3.32556558839844,-3.32430049310195,-3.32338749826037,
-3.32241809333174,-3.32077322908984,-3.31636102715128,-3.24562691126371,
-3.19082983785927,-3.17272910773228,-3.16445210494803,-3.16313055408729,
-3.16243620764226,-3.16192910254588,-3.16137866363258,-3.16040849738475,
-3.15758358424338,-3.11299468621227,-3.05431965029234,-3.0317508094232,
-3.00576699987662,-3.00286353359999,-3.00150536581751,-3.00048499657265,
-2.99952788218792,-2.99820600957199,-2.99483136415524,-2.94894244250121,
-2.89622382141443,-2.84403171867342,-2.8408854818025,-2.83991107487678,
-2.8392941635221,-2.83872726243023,-2.83799135228704,-2.83639480412127,
-2.82449631257564,-2.82222013743134,-2.82184149812791,-2.81969096127196,
-2.81854163675169,-2.81644671374313,-2.81281856171323,-2.80060771051165,
-2.72662369446285,-2.68725352174405,-2.68095192020027,-2.67911788794578,
-2.6779987177767,-2.67698774275303,-2.67569596828261,-2.67305648717332,
-2.6568455363385,-2.65244139698332,-2.64842184033646,-2.60312270076675,
-2.52156968367137,-2.51917408748517,-2.51741295251979,-2.51664051842196,
-2.51606705145154,-2.51553733472715,-2.51481289099728,-2.5133787543379,
-2.50157483587094,-2.49995370585496,-2.49854492846162,-2.41047518669012,
-2.36112641174212,-2.35721605464612,-2.35568601513499,-2.35463338275629,
-2.35360328475375,-2.3523633096534,-2.34927425952295,-2.3208035861809,-2.25472255978626,
-2.19985466633593,-2.19506996259308,-2.19394143822851,-2.19329452603415,
-2.19273346699345,-2.19203646784877,-2.19096474209843,-2.18617002164156,
-2.09293742067761,-2.0525817079453,-2.03586283693807,-2.03341569198889,
-2.03216311326978,-2.03125181606283,-2.03013943624266,-2.02833566801064,
-2.02219060757186,-1.98462458108777,-1.90098551366252,-1.8732857636046,
-1.87134772420953,-1.8706012255069,-1.87006571270415,-1.86949608198602,
-1.86873008676845,-1.86701565432522,-1.82507400083735,-1.72837526106657,
-1.72631118180589,-1.71279971177686,-1.71055580244768,-1.7092205919148,
-1.70820020408421,-1.70711188946695,-1.70541606933145,-1.70032140206661,
-1.64002545778456,-1.59451200929741,-1.55133546227645,-1.54856177637091,
-1.54759881508932,-1.54704983219648,-1.5465423747457,-1.54584498764939,
-1.544593531872,-1.54297319025427,-1.50379242476819,-1.43156030977308,-1.41971013121211,
-1.39077942276331,-1.38771854392708,-1.38646243209228,-1.38552212969164,
-1.38448958308601,-1.38306102914433,-1.37976380560742,-1.37526717837525,
-1.37005580231967),.UNSPECIFIED.);
#216=B_SPLINE_CURVE_WITH_KNOTS('',3,(#37901,#37902,#37903,#37904,#37905,
#37906,#37907,#37908,#37909,#37910,#37911,#37912,#37913,#37914,#37915,#37916,
#37917,#37918,#37919,#37920,#37921,#37922,#37923,#37924,#37925,#37926,#37927,
#37928,#37929,#37930,#37931,#37932,#37933,#37934,#37935,#37936,#37937,#37938,
#37939,#37940,#37941,#37942,#37943,#37944,#37945,#37946,#37947,#37948,#37949,
#37950,#37951,#37952,#37953,#37954,#37955,#37956,#37957,#37958,#37959,#37960,
#37961,#37962,#37963,#37964,#37965,#37966,#37967,#37968,#37969,#37970,#37971,
#37972,#37973,#37974,#37975,#37976,#37977,#37978,#37979,#37980,#37981,#37982,
#37983,#37984,#37985,#37986,#37987,#37988,#37989,#37990,#37991,#37992,#37993,
#37994,#37995,#37996,#37997,#37998,#37999,#38000,#38001,#38002,#38003,#38004,
#38005,#38006,#38007,#38008,#38009,#38010,#38011,#38012,#38013,#38014,#38015,
#38016,#38017,#38018,#38019,#38020,#38021,#38022,#38023,#38024,#38025,#38026,
#38027,#38028,#38029,#38030,#38031,#38032,#38033,#38034,#38035,#38036,#38037,
#38038,#38039,#38040,#38041,#38042,#38043,#38044,#38045,#38046,#38047,#38048,
#38049,#38050,#38051,#38052,#38053,#38054,#38055,#38056,#38057,#38058,#38059,
#38060,#38061,#38062,#38063,#38064,#38065,#38066,#38067,#38068,#38069,#38070,
#38071,#38072,#38073,#38074,#38075,#38076,#38077,#38078,#38079,#38080,#38081,
#38082,#38083,#38084,#38085,#38086,#38087,#38088,#38089,#38090,#38091,#38092,
#38093,#38094,#38095,#38096,#38097,#38098,#38099,#38100,#38101,#38102,#38103,
#38104,#38105,#38106,#38107,#38108,#38109,#38110,#38111,#38112,#38113,#38114,
#38115,#38116,#38117,#38118,#38119,#38120,#38121,#38122,#38123,#38124,#38125,
#38126,#38127,#38128,#38129,#38130,#38131,#38132,#38133,#38134,#38135,#38136,
#38137,#38138,#38139,#38140,#38141,#38142,#38143,#38144,#38145,#38146,#38147,
#38148,#38149,#38150,#38151,#38152,#38153,#38154,#38155,#38156,#38157,#38158,
#38159,#38160,#38161,#38162,#38163,#38164,#38165,#38166,#38167,#38168),
 .UNSPECIFIED.,.F.,.F.,(4,2,2,2,2,2,2,2,2,2,2,2,2,2,2,2,2,2,2,2,2,2,2,2,
2,2,2,2,2,2,2,2,2,2,2,2,2,2,2,2,2,2,2,2,2,2,2,2,2,2,2,2,2,2,2,2,2,2,2,2,
2,2,2,2,2,2,2,2,2,2,2,2,2,2,2,2,2,2,2,2,2,2,2,2,2,2,2,2,2,2,2,2,2,2,2,2,
2,2,2,2,2,2,2,2,2,2,2,2,2,2,2,2,2,2,2,2,2,2,2,2,2,2,2,2,2,2,2,2,2,2,2,2,
2,4),(-2.69269850522027,-2.68332553922718,-2.62048867816285,-2.59632731631076,
-2.58408716150558,-2.58183230508675,-2.58062075988093,-2.5796263475247,
-2.57860943570164,-2.57672555205305,-2.57055566976022,-2.46436782869153,
-2.42211956853202,-2.42063008724243,-2.41976246224811,-2.4189892401686,
-2.41842592393518,-2.41789872937814,-2.41718339976749,-2.41578417533183,
-2.40493560905856,-2.4033324964891,-2.40248250410415,-2.40175049514704,
-2.4013347787392,-2.40050076174969,-2.39841032175249,-2.39694335998903,
-2.35780648129755,-2.32953269623204,-2.2967733773997,-2.27315221088142,
-2.26116775899695,-2.25892597961488,-2.25771708355076,-2.2567225656347,
-2.25570354382474,-2.2538098852611,-2.24756000256042,-2.14040209746362,
-2.11671385998837,-2.10582211329231,-2.09787424955118,-2.09656296193655,
-2.09587653677614,-2.09537040445473,-2.09481620813607,-2.09400150830972,
-2.09161241384246,-2.05328129214903,-2.03202133373016,-1.9994680771561,
-1.94036227393768,-1.9367476625031,-1.93538667394232,-1.93441924155934,
-1.93350573989631,-1.93223618999126,-1.92970593647032,-1.91036996899143,
-1.88032205027464,-1.78928044733773,-1.77549282496975,-1.77399511399825,
-1.77325470213926,-1.77272085456881,-1.77215035657759,-1.77137875153678,
-1.76963317913417,-1.72844597672819,-1.62047994688679,-1.61435166694624,
-1.61247233333348,-1.61145609413407,-1.61047171524352,-1.60928715236349,
-1.60801785257924,-1.60604186074277,-1.56812619943236,-1.47413220014332,
-1.46575333273969,-1.46286235505579,-1.45213912180586,-1.4507442975097,
-1.45002997238769,-1.44950290967792,-1.44892746907769,-1.44812791533062,
-1.44622351683734,-1.44360551374404,-1.41558822615915,-1.29654548678039,
-1.29096791044087,-1.28915761351063,-1.28815535415416,-1.28716999357543,
-1.28596268773031,-1.28466191600338,-1.28261117468599,-1.22743010036261,
-1.13313105828487,-1.12830314847934,-1.12722889181132,-1.12653118451408,
-1.12597018646404,-1.12532404820821,-1.12419862339508,-1.11945171417449,
-1.07695250517436,-0.974114835876923,-0.96797050404025,-0.966089325860205,
-0.965072762440275,-0.964088967484302,-0.962905089844943,-0.9616369257758,
-0.959663549564539,-0.922140185093852,-0.829430174877555,-0.824070437235926,
-0.820254203183707,-0.818885882692225,-0.818470077000964,-0.817696775710925,
-0.805842762805436,-0.804407170265072,-0.803682449885206,-0.803152749727536,
-0.802579520431882,-0.801791897144688,-0.799956159517104,-0.797456091475399,
-0.708716229361596,-0.662248326428725),.UNSPECIFIED.);
#217=B_SPLINE_CURVE_WITH_KNOTS('',3,(#38174,#38175,#38176,#38177,#38178,
#38179,#38180,#38181,#38182,#38183,#38184,#38185,#38186,#38187,#38188,#38189,
#38190,#38191,#38192,#38193,#38194,#38195,#38196,#38197,#38198,#38199,#38200,
#38201,#38202,#38203,#38204,#38205,#38206,#38207,#38208,#38209,#38210,#38211,
#38212,#38213,#38214,#38215,#38216,#38217,#38218,#38219,#38220,#38221,#38222,
#38223,#38224,#38225,#38226,#38227,#38228,#38229,#38230,#38231,#38232,#38233,
#38234,#38235,#38236,#38237,#38238,#38239,#38240,#38241,#38242,#38243,#38244,
#38245,#38246,#38247,#38248,#38249,#38250,#38251,#38252,#38253,#38254,#38255,
#38256,#38257,#38258,#38259,#38260,#38261,#38262,#38263,#38264,#38265,#38266,
#38267,#38268,#38269,#38270,#38271,#38272,#38273,#38274,#38275,#38276,#38277,
#38278,#38279,#38280,#38281,#38282,#38283,#38284,#38285,#38286,#38287,#38288,
#38289,#38290,#38291,#38292,#38293,#38294,#38295,#38296,#38297,#38298,#38299,
#38300,#38301,#38302,#38303,#38304,#38305,#38306,#38307,#38308,#38309,#38310,
#38311,#38312,#38313,#38314,#38315,#38316,#38317,#38318,#38319,#38320,#38321,
#38322,#38323,#38324,#38325,#38326,#38327,#38328,#38329,#38330,#38331,#38332,
#38333,#38334,#38335,#38336,#38337,#38338,#38339,#38340,#38341,#38342,#38343,
#38344,#38345,#38346,#38347,#38348,#38349,#38350,#38351,#38352,#38353,#38354,
#38355,#38356,#38357,#38358,#38359,#38360,#38361,#38362,#38363,#38364,#38365,
#38366,#38367,#38368,#38369,#38370,#38371),.UNSPECIFIED.,.F.,.F.,(4,2,2,
2,2,2,2,2,2,2,2,2,2,2,2,2,2,2,2,2,2,2,2,2,2,2,2,2,2,2,2,2,2,2,2,2,2,2,2,
2,2,2,2,2,2,2,2,2,2,2,2,2,2,2,2,2,2,2,2,2,2,2,2,2,2,2,2,2,2,2,2,2,2,2,2,
2,2,2,2,2,2,2,2,2,2,2,2,2,2,2,2,2,2,2,2,2,2,2,4),(-1.36942377060857,-1.36559877502083,
-1.36362053690649,-1.36286760451683,-1.36233039018199,-1.36181867556833,
-1.36109153358451,-1.35961161092896,-1.34697148556379,-1.32152889274019,
-1.25630302805756,-1.23550284582958,-1.20615021107675,-1.20334845643425,
-1.20199030829124,-1.20102351557963,-1.20010949529152,-1.19883743689666,
-1.19645200889229,-1.18007908179885,-1.14099979542526,-1.08255363300622,
-1.05156743024829,-1.04963064631632,-1.041767365488,-1.04037537799865,-1.03966255684123,
-1.03910015562647,-1.03846410042036,-1.03740593381582,-1.03344020507378,
-1.00528182224472,-0.948729506704858,-0.884482542479156,-0.880533412635055,
-0.879120270479407,-0.878138427624577,-0.87722915907992,-0.875992965776401,
-0.873687147348508,-0.86070872706831,-0.836588400741853,-0.774685107884237,
-0.729638658213808,-0.719017702671611,-0.717626699217039,-0.716913323361167,
-0.716386468347071,-0.715810748423445,-0.715238985858369,-0.71381951318371,
-0.702624361397662,-0.684518239076959,-0.636044977739776,-0.562586983107782,
-0.557831569357439,-0.556134771667546,-0.55515507034229,-0.55424525423192,
-0.553004448865848,-0.551681088994354,-0.545732871049633,-0.511244622740464,
-0.458784160366601,-0.398706302005173,-0.39520880920484,-0.394152211316115,
-0.393584342815754,-0.393023824211013,-0.392335289717044,-0.391599661830646,
-0.388334734703975,-0.383085280962421,-0.37181597524073,-0.342917468096281,
-0.318447543880378,-0.239659998788011,-0.238856093904025,-0.234661294348008,
-0.233050789557542,-0.232088089921339,-0.231070665969788,-0.229731420928208,
-0.22827189523805,-0.225842373078562,-0.208854241193399,-0.168107931902686,
-0.1537095578637,-0.139288922174846,-0.0761971701861116,-0.0723180763900793,
-0.071218267628141,-0.0706417107919776,-0.0701376726271744,-0.0694854789227201,
-0.068800613824145,-0.0677512400895286,-0.0658053860028119,-0.000961407761673223),
 .UNSPECIFIED.);
#218=B_SPLINE_CURVE_WITH_KNOTS('',3,(#38372,#38373,#38374,#38375,#38376,
#38377,#38378,#38379,#38380,#38381,#38382,#38383,#38384,#38385,#38386,#38387,
#38388,#38389,#38390,#38391,#38392,#38393,#38394,#38395,#38396,#38397,#38398,
#38399,#38400,#38401,#38402,#38403,#38404,#38405,#38406,#38407,#38408,#38409,
#38410,#38411,#38412,#38413,#38414,#38415,#38416,#38417,#38418,#38419,#38420,
#38421,#38422,#38423,#38424,#38425,#38426,#38427,#38428,#38429,#38430,#38431,
#38432,#38433,#38434,#38435,#38436,#38437,#38438,#38439,#38440,#38441,#38442,
#38443,#38444,#38445,#38446,#38447,#38448,#38449,#38450,#38451,#38452,#38453,
#38454,#38455,#38456,#38457,#38458,#38459,#38460,#38461,#38462,#38463,#38464,
#38465,#38466,#38467),.UNSPECIFIED.,.F.,.F.,(4,2,2,2,2,2,2,2,2,2,2,2,2,
2,2,2,2,2,2,2,2,2,2,2,2,2,2,2,2,2,2,2,2,2,2,2,2,2,2,2,2,2,2,2,2,2,2,4),
(-4.06158259407951,-3.98902691859257,-3.97454587785814,-3.9725398664761,
-3.97125785962089,-3.97004690679561,-3.9691403957768,-3.96814588573345,
-3.96637471630796,-3.96109284372864,-3.87929163028354,-3.86674666089183,
-3.85498350879111,-3.82472061324442,-3.81089576516494,-3.80972124900028,
-3.80898388511476,-3.80829412993813,-3.80773361512119,-3.80716660628314,
-3.80611403914643,-3.80264980125633,-3.74480708704601,-3.72336325636554,
-3.70208068315013,-3.66634034905488,-3.65612899566236,-3.64982237700015,
-3.6484754502877,-3.64721762777941,-3.64630567426265,-3.64533343104751,
-3.64395501111696,-3.64023191138441,-3.63871254260851,-3.56437279448885,
-3.56026095102796,-3.51627888696708,-3.48859664585569,-3.4864713954419,
-3.48582545250585,-3.48520074651943,-3.48463611537343,-3.48391577138633,
-3.48240037145606,-3.47244749653559,-3.42701327748576,-3.40025096654499),
 .UNSPECIFIED.);
#219=B_SPLINE_CURVE_WITH_KNOTS('',3,(#38469,#38470,#38471,#38472,#38473,
#38474,#38475,#38476,#38477,#38478,#38479,#38480,#38481,#38482,#38483,#38484,
#38485,#38486,#38487,#38488,#38489,#38490,#38491,#38492,#38493,#38494,#38495,
#38496,#38497,#38498,#38499,#38500,#38501,#38502,#38503,#38504,#38505,#38506,
#38507,#38508,#38509,#38510,#38511,#38512,#38513,#38514,#38515,#38516,#38517,
#38518,#38519,#38520,#38521,#38522,#38523,#38524,#38525,#38526,#38527,#38528,
#38529,#38530,#38531,#38532,#38533,#38534,#38535,#38536,#38537,#38538,#38539,
#38540,#38541,#38542,#38543,#38544,#38545,#38546,#38547,#38548,#38549,#38550,
#38551,#38552,#38553,#38554),.UNSPECIFIED.,.F.,.F.,(4,2,2,2,2,2,2,2,2,2,
2,2,2,2,2,2,2,2,2,2,2,2,2,2,2,2,2,2,2,2,2,2,2,2,2,2,2,2,2,2,2,2,4),(-0.662248326428725,
-0.647939429323128,-0.644191399751803,-0.642809200227694,-0.641836019189344,
-0.64084355046288,-0.639573179308982,-0.638185328386442,-0.635927432817154,
-0.631463961838477,-0.587045294089171,-0.493121853742009,-0.482671181599808,
-0.481286865928025,-0.480575244506379,-0.480048863167519,-0.47947281359014,
-0.47867001851113,-0.476746637390012,-0.474095783395336,-0.445424450922808,
-0.379073631685477,-0.324539434749613,-0.321065826510201,-0.319727597728636,
-0.318766209030686,-0.317768618264209,-0.316463897247218,-0.315028611600712,
-0.312657281494422,-0.265986767841822,-0.163398479016872,-0.162571639898673,
-0.158822646186717,-0.157737070370335,-0.157163324557509,-0.156659138392786,
-0.156003154520508,-0.154833700610107,-0.149488436632919,-0.06850952425481,
-0.0127049774281039,-0.000961729954404432),.UNSPECIFIED.);
#220=B_SPLINE_CURVE_WITH_KNOTS('',3,(#38555,#38556,#38557,#38558,#38559,
#38560,#38561,#38562,#38563,#38564,#38565,#38566,#38567,#38568,#38569,#38570,
#38571,#38572,#38573,#38574,#38575,#38576,#38577,#38578,#38579,#38580,#38581,
#38582,#38583,#38584,#38585,#38586,#38587,#38588,#38589,#38590,#38591,#38592,
#38593,#38594,#38595,#38596,#38597,#38598,#38599,#38600,#38601,#38602,#38603,
#38604,#38605,#38606,#38607,#38608,#38609,#38610,#38611,#38612,#38613,#38614,
#38615,#38616,#38617,#38618,#38619,#38620,#38621,#38622,#38623,#38624,#38625,
#38626,#38627,#38628,#38629,#38630,#38631,#38632,#38633,#38634,#38635,#38636,
#38637,#38638,#38639,#38640,#38641,#38642,#38643,#38644,#38645,#38646,#38647,
#38648,#38649,#38650,#38651,#38652,#38653,#38654,#38655,#38656,#38657,#38658,
#38659,#38660,#38661,#38662,#38663,#38664,#38665,#38666,#38667,#38668,#38669,
#38670,#38671,#38672,#38673,#38674,#38675,#38676,#38677,#38678,#38679,#38680,
#38681,#38682,#38683,#38684,#38685,#38686,#38687,#38688,#38689,#38690,#38691,
#38692,#38693,#38694,#38695,#38696),.UNSPECIFIED.,.F.,.F.,(4,3,3,3,3,3,
3,3,3,3,3,3,3,3,3,3,3,3,3,3,3,3,3,3,3,3,3,3,3,3,3,3,3,3,3,3,3,3,3,3,3,3,
3,3,3,3,3,4),(354.999969855647,355.096451305071,355.193049126282,355.28986323818,
355.3867981232,355.483945074556,355.51705571041,355.610128654686,355.703075494323,
355.795923865508,355.888704370163,355.981449692319,356.074184657421,356.166934075762,
356.259782716497,356.352683157109,356.445739053193,356.516770365883,356.609843310159,
356.702790149796,356.795638520981,356.888419025636,356.981164347793,357.073899312894,
357.166648731235,357.25949737197,357.352397812582,357.445453708666,357.516485021356,
357.609557965632,357.702504805269,357.795353176454,357.888133681109,357.980879003266,
358.073613968367,358.166363386708,358.259212027443,358.352112468055,358.445168364139,
358.516199676829,358.609250019074,358.70218389026,358.795026308277,358.887802206273,
358.980552664654,359.073285531874,359.166063108531,359.23634059125),
 .UNSPECIFIED.);
#221=B_SPLINE_CURVE_WITH_KNOTS('',3,(#38701,#38702,#38703,#38704,#38705,
#38706,#38707,#38708,#38709,#38710,#38711,#38712,#38713,#38714,#38715,#38716,
#38717,#38718,#38719,#38720,#38721,#38722,#38723,#38724,#38725,#38726,#38727,
#38728,#38729,#38730,#38731,#38732,#38733,#38734,#38735,#38736,#38737,#38738,
#38739,#38740,#38741,#38742,#38743,#38744,#38745,#38746,#38747,#38748,#38749,
#38750,#38751,#38752,#38753,#38754,#38755,#38756,#38757,#38758,#38759,#38760,
#38761,#38762,#38763,#38764,#38765,#38766,#38767,#38768,#38769,#38770,#38771,
#38772,#38773,#38774,#38775,#38776,#38777,#38778,#38779,#38780,#38781,#38782,
#38783,#38784,#38785,#38786,#38787,#38788,#38789,#38790,#38791,#38792,#38793,
#38794,#38795,#38796,#38797,#38798,#38799,#38800,#38801,#38802,#38803,#38804,
#38805,#38806,#38807,#38808,#38809,#38810,#38811,#38812,#38813,#38814,#38815,
#38816,#38817,#38818,#38819,#38820,#38821,#38822,#38823,#38824,#38825,#38826,
#38827,#38828,#38829,#38830,#38831,#38832,#38833,#38834,#38835,#38836,#38837,
#38838,#38839,#38840,#38841,#38842,#38843,#38844,#38845,#38846,#38847,#38848,
#38849,#38850,#38851,#38852,#38853,#38854,#38855,#38856,#38857,#38858,#38859,
#38860,#38861,#38862,#38863,#38864,#38865,#38866,#38867,#38868,#38869,#38870,
#38871,#38872,#38873,#38874,#38875,#38876,#38877,#38878,#38879,#38880,#38881,
#38882,#38883,#38884,#38885,#38886,#38887,#38888,#38889,#38890,#38891,#38892,
#38893,#38894,#38895,#38896,#38897,#38898,#38899,#38900,#38901,#38902,#38903,
#38904,#38905,#38906,#38907,#38908,#38909,#38910,#38911,#38912,#38913,#38914,
#38915,#38916,#38917,#38918,#38919,#38920,#38921,#38922,#38923,#38924,#38925,
#38926,#38927,#38928,#38929,#38930,#38931,#38932,#38933,#38934,#38935,#38936,
#38937,#38938,#38939,#38940,#38941,#38942,#38943,#38944,#38945,#38946,#38947,
#38948,#38949,#38950,#38951,#38952,#38953,#38954,#38955,#38956,#38957,#38958),
 .UNSPECIFIED.,.F.,.F.,(4,2,2,2,2,2,2,2,2,2,2,2,2,2,2,2,2,2,2,2,2,2,2,2,
2,2,2,2,2,2,2,2,2,2,2,2,2,2,2,2,2,2,2,2,2,2,2,2,2,2,2,2,2,2,2,2,2,2,2,2,
2,2,2,2,2,2,2,2,2,2,2,2,2,2,2,2,2,2,2,2,2,2,2,2,2,2,2,2,2,2,2,2,2,2,2,2,
2,2,2,2,2,2,2,2,2,2,2,2,2,2,2,2,2,2,2,2,2,2,2,2,2,2,2,2,2,2,2,2,4),(-3.39966259726345,
-3.34930942753569,-3.31835551769945,-3.30796621344053,-3.30250707491916,
-3.30133043712181,-3.30067315117589,-3.30016925944657,-3.29959723048155,
-3.29851896952887,-3.29483097986264,-3.29391970540771,-3.21843406511585,
-3.17019305653192,-3.15241167225209,-3.14610953319681,-3.14319626496594,
-3.14087828645481,-3.13965918791189,-3.1386646026662,-3.13752068832588,
-3.13557426401416,-3.12886346311778,-3.12507957653716,-3.1212290071838,
-3.12074785294598,-3.11864305497853,-3.02730976720726,-2.98428094326636,
-2.97951874705186,-2.97839235471009,-2.97774611860352,-2.9771853137359,
-2.97648820486979,-2.97541552952473,-2.97060467065372,-2.87750633584063,
-2.82270276397698,-2.81998370831462,-2.8177945207525,-2.8166026652889,-2.81559853805938,
-2.81458194984785,-2.81269990762598,-2.80654611364521,-2.70052542053249,
-2.66105566960581,-2.65641638241295,-2.65529959453582,-2.65465545496267,
-2.65409437674978,-2.65339423272582,-2.65231190760501,-2.647381515798,-2.55198711800444,
-2.49953759627428,-2.49684569794216,-2.49467151645231,-2.49348430031026,
-2.49248973891235,-2.49147256993718,-2.4895879043092,-2.48341298356492,
-2.38029504463951,-2.33429109004294,-2.33256748712646,-2.33179998638969,
-2.33123027725755,-2.33069547636651,-2.32995116947577,-2.32802544855145,
-2.3010694682733,-2.21146565449179,-2.18667608153743,-2.17392844281765,
-2.17164750401975,-2.17043020308167,-2.16942589087345,-2.16840953665211,
-2.16652915723888,-2.16039072651125,-2.05471432427409,-2.03046112007357,
-2.02927466374306,-2.02588143178242,-2.02483194507878,-2.01111686453133,
-2.00962147771019,-2.00888170501469,-2.00834808070855,-2.00777758873436,
-2.00700559963059,-2.00525750351294,-2.00290604398428,-1.97970645259788,
-1.95470635180935,-1.89978433188292,-1.89427779205259,-1.87763177298475,
-1.87138136987099,-1.85176289547256,-1.84925018966872,-1.84796483708003,
-1.84701730856382,-1.84599103934444,-1.84459668839262,-1.84141487999575,
-1.79845660312388,-1.699760571375,-1.6880232200218,-1.68643309421035,-1.68569840762128,
-1.68513170402537,-1.68451423739202,-1.68353764249069,-1.68035029188592,
-1.6322065708271,-1.54782539366473,-1.54455141498501,-1.52839826913049,
-1.52576155176459,-1.5244703805501,-1.5234595343635,-1.52234015515182,-1.52050498035741,
-1.51419121737665,-1.47468704401601,-1.3960678521665,-1.36942377060857),
 .UNSPECIFIED.);
#222=B_SPLINE_CURVE_WITH_KNOTS('',3,(#38960,#38961,#38962,#38963,#38964,
#38965,#38966,#38967,#38968,#38969,#38970,#38971,#38972,#38973,#38974,#38975,
#38976,#38977,#38978,#38979,#38980,#38981,#38982,#38983,#38984,#38985,#38986,
#38987,#38988,#38989,#38990,#38991,#38992,#38993,#38994,#38995,#38996,#38997,
#38998,#38999,#39000,#39001,#39002,#39003,#39004,#39005,#39006,#39007,#39008,
#39009,#39010,#39011,#39012,#39013,#39014,#39015,#39016,#39017,#39018,#39019,
#39020,#39021,#39022,#39023,#39024,#39025,#39026,#39027,#39028,#39029),
 .UNSPECIFIED.,.F.,.F.,(4,3,3,3,3,3,3,3,3,3,3,3,3,3,3,3,3,3,3,3,3,3,3,4),
(359.23634059125,359.329226379691,359.422570355996,359.515914332302,359.608987276577,
359.701934116215,359.7947824874,359.887562992055,359.980308314211,360.073043279312,
360.165792697653,360.258641338388,360.351541779,360.444597675084,360.515628987774,
360.61156975962,360.703295257999,360.794935418517,360.886516342147,360.978064063546,
361.069633525802,361.161216235208,361.252875332287,361.283155162539),
 .UNSPECIFIED.);
#223=B_SPLINE_CURVE_WITH_KNOTS('',3,(#39030,#39031,#39032,#39033,#39034,
#39035,#39036,#39037,#39038,#39039,#39040,#39041,#39042,#39043,#39044,#39045,
#39046,#39047,#39048,#39049,#39050,#39051,#39052,#39053,#39054,#39055,#39056,
#39057,#39058,#39059,#39060,#39061,#39062,#39063,#39064,#39065,#39066,#39067,
#39068,#39069,#39070,#39071,#39072,#39073,#39074,#39075,#39076,#39077,#39078,
#39079,#39080,#39081,#39082,#39083,#39084,#39085,#39086,#39087,#39088,#39089,
#39090,#39091,#39092,#39093,#39094,#39095,#39096,#39097,#39098,#39099,#39100,
#39101,#39102,#39103,#39104,#39105,#39106,#39107,#39108,#39109,#39110,#39111,
#39112,#39113,#39114,#39115,#39116,#39117,#39118,#39119,#39120,#39121,#39122,
#39123,#39124,#39125,#39126,#39127,#39128,#39129,#39130,#39131,#39132,#39133,
#39134,#39135,#39136,#39137,#39138,#39139,#39140,#39141,#39142,#39143,#39144,
#39145,#39146,#39147,#39148,#39149,#39150,#39151,#39152,#39153,#39154,#39155,
#39156,#39157,#39158,#39159,#39160,#39161,#39162,#39163,#39164,#39165,#39166,
#39167,#39168,#39169,#39170,#39171,#39172,#39173,#39174,#39175,#39176,#39177,
#39178,#39179,#39180,#39181,#39182,#39183,#39184,#39185,#39186,#39187,#39188,
#39189,#39190,#39191,#39192,#39193,#39194,#39195,#39196,#39197,#39198,#39199,
#39200,#39201,#39202,#39203,#39204,#39205,#39206,#39207,#39208,#39209,#39210,
#39211,#39212,#39213,#39214,#39215,#39216,#39217,#39218,#39219,#39220,#39221,
#39222,#39223,#39224,#39225),.UNSPECIFIED.,.F.,.F.,(4,2,2,2,2,2,2,2,2,2,
2,2,2,2,2,2,2,2,2,2,2,2,2,2,2,2,2,2,2,2,2,2,2,2,2,2,2,2,2,2,2,2,2,2,2,2,
2,2,2,2,2,2,2,2,2,2,2,2,2,2,2,2,2,2,2,2,2,2,2,2,2,2,2,2,2,2,2,2,2,2,2,2,
2,2,2,2,2,2,2,2,2,2,2,2,2,2,2,4),(-4.05985780112435,-3.9949188893063,-3.9899681927845,
-3.98788643122196,-3.98678473053978,-3.9860779547586,-3.98541016780942,
-3.98490562802089,-3.9842559994703,-3.98314418791168,-3.97902447548922,
-3.9112993717401,-3.8976739749491,-3.88421896989649,-3.84577120163737,-3.82906339179991,
-3.82694368550262,-3.82561383237739,-3.82436839526673,-3.82345818728114,
-3.82248093233968,-3.82079566012486,-3.81611704303792,-3.74261159482878,
-3.71880170592077,-3.69371240009228,-3.6733179866591,-3.66756832562051,
-3.66406807968174,-3.66331705850079,-3.66261750579369,-3.662056414542,-3.66141171689633,
-3.66032105294822,-3.65640508645385,-3.59218123965039,-3.54245757420453,
-3.50987479613646,-3.50402667469848,-3.50271028705841,-3.50147457377119,
-3.50056554787565,-3.49958386064442,-3.49817075923631,-3.49422057437485,
-3.42993477408235,-3.39613394437811,-3.3639375637965,-3.34983104687737,
-3.34448532492474,-3.34117476045616,-3.34043623779244,-3.33974567376057,
-3.33918519144089,-3.33861880583541,-3.33756906627434,-3.33412769522635,
-3.27949665326839,-3.2315054257684,-3.19736196418451,-3.18229363118905,
-3.17992323803511,-3.17867341078234,-3.17776263876735,-3.17678728865184,
-3.17539716436698,-3.17159796048124,-3.11418552568979,-3.06090380541502,
-3.03377434140109,-3.02693480855402,-3.01891594981985,-3.01760520781451,
-3.01691326496517,-3.01640654066568,-3.01585515188944,-3.01487982933241,
-3.01201908616973,-2.96731958466446,-2.90687826760608,-2.88556733372441,
-2.8602803746977,-2.85738732761159,-2.85603039769741,-2.85501042254602,
-2.8540532863847,-2.85273076520681,-2.84935115540602,-2.80307511721189,
-2.73410379436719,-2.70772127423793,-2.6962464668446,-2.69481911634679,
-2.69410274546337,-2.69359277789063,-2.69305187597094,-2.69228507760071,
-2.69182724913245),.UNSPECIFIED.);
#224=B_SPLINE_CURVE_WITH_KNOTS('',3,(#39231,#39232,#39233,#39234,#39235,
#39236,#39237,#39238,#39239,#39240,#39241,#39242,#39243,#39244,#39245,#39246,
#39247,#39248,#39249,#39250,#39251,#39252,#39253,#39254,#39255,#39256,#39257,
#39258,#39259,#39260,#39261,#39262,#39263,#39264,#39265,#39266,#39267,#39268,
#39269,#39270,#39271,#39272,#39273,#39274,#39275,#39276,#39277,#39278,#39279,
#39280,#39281,#39282,#39283,#39284,#39285,#39286,#39287,#39288,#39289,#39290,
#39291,#39292,#39293,#39294,#39295,#39296,#39297,#39298,#39299,#39300,#39301,
#39302,#39303,#39304,#39305,#39306,#39307,#39308,#39309,#39310,#39311,#39312,
#39313,#39314,#39315,#39316,#39317,#39318,#39319,#39320,#39321,#39322,#39323,
#39324,#39325,#39326,#39327,#39328,#39329,#39330,#39331,#39332,#39333,#39334,
#39335,#39336,#39337,#39338,#39339,#39340,#39341,#39342,#39343,#39344,#39345,
#39346,#39347,#39348,#39349,#39350,#39351,#39352,#39353,#39354,#39355,#39356,
#39357,#39358,#39359,#39360,#39361,#39362,#39363,#39364,#39365,#39366,#39367,
#39368,#39369,#39370,#39371,#39372,#39373,#39374,#39375,#39376,#39377,#39378,
#39379,#39380,#39381,#39382,#39383,#39384,#39385,#39386,#39387,#39388,#39389,
#39390,#39391,#39392,#39393,#39394,#39395,#39396,#39397,#39398,#39399,#39400,
#39401,#39402,#39403,#39404,#39405,#39406,#39407,#39408,#39409,#39410,#39411,
#39412,#39413,#39414,#39415,#39416,#39417,#39418,#39419,#39420,#39421,#39422,
#39423,#39424,#39425,#39426,#39427,#39428,#39429,#39430,#39431,#39432,#39433,
#39434,#39435,#39436,#39437,#39438,#39439,#39440),.UNSPECIFIED.,.F.,.F.,
(4,2,2,2,2,2,2,2,2,2,2,2,2,2,2,2,2,2,2,2,2,2,2,2,2,2,2,2,2,2,2,2,2,2,2,
2,2,2,2,2,2,2,2,2,2,2,2,2,2,2,2,2,2,2,2,2,2,2,2,2,2,2,2,2,2,2,2,2,2,2,2,
2,2,2,2,2,2,2,2,2,2,2,2,2,2,2,2,2,2,2,2,2,2,2,2,2,2,2,2,2,2,2,2,2,4),(-1.37031440543437,
-1.34985354582264,-1.3438291591212,-1.34196249922411,-1.34094886086762,
-1.33994426827501,-1.33874711848388,-1.33652773334125,-1.33376719865848,
-1.28542360784259,-1.19094435320615,-1.18958082640232,-1.18800304602631,
-1.18534912746519,-1.18097453191006,-1.17983734857757,-1.17918177336801,
-1.17862147635709,-1.17793579652214,-1.17662820256177,-1.16876650062564,
-1.1540884961261,-1.14096899212298,-1.03960529394694,-1.03548316042706,
-1.03341370898517,-1.03259656691607,-1.03076767472717,-1.0268368247659,
-1.02072296182719,-1.01884541548855,-1.01782956487744,-1.01682510437983,
-1.01563126972847,-1.01343137992386,-1.01069800495569,-1.00491525643778,
-0.989074744870986,-0.958690409897572,-0.862853286709799,-0.85794230843511,
-0.856861347755493,-0.856161534428666,-0.855600350758997,-0.854955677235901,
-0.85383694889709,-0.849175704344511,-0.82672368350558,-0.814053521446936,
-0.73031131485283,-0.699755447923921,-0.696925857829539,-0.695561004061509,
-0.694592504495004,-0.693618888355921,-0.692346674735723,-0.689777192123046,
-0.686472387413955,-0.679005711864414,-0.656773472916899,-0.621359921809086,
-0.544497083646594,-0.543626192470129,-0.541439523851208,-0.541133172326015,
-0.535116267439142,-0.533955068482497,-0.533230540814627,-0.532666907973655,
-0.53203794461443,-0.53098960464022,-0.527135506865875,-0.438542204284299,
-0.406785890764745,-0.376732074824184,-0.373914056312083,-0.372552022913521,
-0.371584275156491,-0.370611178305843,-0.36962843616908,-0.367483554618584,
-0.357080181678513,-0.337311734680935,-0.313369220878766,-0.216672402140462,
-0.211855842791534,-0.210782373639322,-0.210084841892462,-0.20952375867137,
-0.208877269918677,-0.20775060802432,-0.202989665487318,-0.160059907314356,
-0.0970476351608282,-0.0912954534780944,-0.0755067392938426,-0.0533397442101704,
-0.0507380336612936,-0.0494298080432169,-0.0484762518739942,-0.0475127683795713,
-0.0465193091884311,-0.0452243237816687,-0.0431876943653371,-0.000960726247794841),
 .UNSPECIFIED.);
#225=B_SPLINE_CURVE_WITH_KNOTS('',3,(#39441,#39442,#39443,#39444,#39445,
#39446,#39447,#39448,#39449,#39450,#39451,#39452,#39453,#39454,#39455,#39456,
#39457,#39458,#39459,#39460,#39461,#39462,#39463,#39464,#39465,#39466,#39467,
#39468,#39469,#39470,#39471,#39472,#39473,#39474,#39475,#39476,#39477,#39478,
#39479,#39480,#39481,#39482,#39483,#39484,#39485,#39486,#39487,#39488,#39489,
#39490,#39491,#39492,#39493,#39494,#39495,#39496,#39497,#39498,#39499,#39500,
#39501,#39502,#39503,#39504,#39505,#39506,#39507,#39508,#39509,#39510,#39511,
#39512,#39513,#39514,#39515,#39516,#39517,#39518,#39519,#39520,#39521,#39522,
#39523,#39524,#39525,#39526,#39527,#39528,#39529,#39530,#39531,#39532,#39533,
#39534,#39535,#39536,#39537,#39538,#39539,#39540,#39541,#39542,#39543,#39544,
#39545,#39546,#39547,#39548,#39549,#39550,#39551,#39552),.UNSPECIFIED.,
 .F.,.F.,(4,2,2,2,2,2,2,2,2,2,2,2,2,2,2,2,2,2,2,2,2,2,2,2,2,2,2,2,2,2,2,
2,2,2,2,2,2,2,2,2,2,2,2,2,2,2,2,2,2,2,2,2,2,2,2,4),(-4.06033398351104,-3.99325575896065,
-3.96396145968547,-3.95370949610167,-3.94830325600619,-3.94713020088203,
-3.94647370673597,-3.94596984710917,-3.94539724101121,-3.94431608714047,
-3.94060237696248,-3.93972944119854,-3.83744482629944,-3.8179274018609,
-3.79121622778603,-3.78734223937179,-3.78618092764658,-3.78522774447348,
-3.7843235507462,-3.78316526685376,-3.7812052663126,-3.77415490574808,-3.7705556292229,
-3.7690612398609,-3.76852616508363,-3.76713549856036,-3.76652172219038,
-3.76444091178738,-3.76293807605746,-3.76173350473988,-3.76034818210871,
-3.75414547491261,-3.74649070751717,-3.71764773498423,-3.628871923601,-3.62638330375413,
-3.6245544633291,-3.62376823392448,-3.62319542396173,-3.62266567489052,
-3.62194024562897,-3.62012493316739,-3.61641298369729,-3.53035523667217,
-3.49938106983598,-3.47718630595116,-3.46972951891099,-3.4664282436174,
-3.46386466595557,-3.46259203876634,-3.4616191592552,-3.4606515175096,-3.45928887386699,
-3.4564671156655,-3.42621010760946,-3.39966259726345),.UNSPECIFIED.);
#226=B_SPLINE_CURVE_WITH_KNOTS('',3,(#39553,#39554,#39555,#39556,#39557,
#39558,#39559,#39560,#39561,#39562,#39563,#39564,#39565,#39566,#39567,#39568,
#39569,#39570,#39571,#39572,#39573,#39574,#39575,#39576,#39577,#39578,#39579,
#39580,#39581,#39582,#39583,#39584,#39585,#39586,#39587,#39588,#39589,#39590,
#39591,#39592,#39593,#39594,#39595,#39596,#39597,#39598,#39599,#39600,#39601,
#39602,#39603,#39604,#39605,#39606,#39607,#39608,#39609,#39610,#39611,#39612,
#39613,#39614,#39615,#39616,#39617,#39618,#39619,#39620,#39621,#39622,#39623,
#39624,#39625,#39626,#39627,#39628,#39629,#39630,#39631,#39632,#39633,#39634,
#39635,#39636,#39637,#39638,#39639,#39640,#39641,#39642,#39643,#39644,#39645,
#39646,#39647,#39648,#39649,#39650,#39651,#39652,#39653,#39654,#39655,#39656,
#39657,#39658,#39659,#39660,#39661,#39662,#39663,#39664,#39665,#39666,#39667,
#39668,#39669,#39670,#39671,#39672,#39673,#39674,#39675,#39676,#39677,#39678,
#39679,#39680,#39681,#39682,#39683,#39684,#39685,#39686,#39687,#39688,#39689,
#39690,#39691,#39692,#39693,#39694,#39695,#39696,#39697,#39698,#39699,#39700,
#39701,#39702,#39703,#39704,#39705,#39706,#39707,#39708,#39709,#39710,#39711,
#39712,#39713,#39714,#39715,#39716,#39717,#39718,#39719,#39720,#39721,#39722,
#39723,#39724,#39725,#39726,#39727,#39728,#39729,#39730,#39731,#39732,#39733,
#39734,#39735,#39736,#39737,#39738,#39739,#39740,#39741,#39742,#39743,#39744,
#39745,#39746,#39747,#39748,#39749,#39750,#39751,#39752,#39753,#39754,#39755,
#39756,#39757,#39758,#39759,#39760,#39761,#39762,#39763,#39764,#39765,#39766,
#39767,#39768,#39769,#39770,#39771,#39772,#39773,#39774,#39775,#39776,#39777,
#39778,#39779,#39780,#39781,#39782,#39783,#39784,#39785,#39786,#39787,#39788,
#39789,#39790,#39791,#39792,#39793,#39794,#39795,#39796,#39797,#39798,#39799,
#39800,#39801,#39802,#39803,#39804,#39805,#39806,#39807,#39808,#39809,#39810,
#39811,#39812),.UNSPECIFIED.,.F.,.F.,(4,2,2,2,2,2,2,2,2,2,2,2,2,2,2,2,2,
2,2,2,2,2,2,2,2,2,2,2,2,2,2,2,2,2,2,2,2,2,2,2,2,2,2,2,2,2,2,2,2,2,2,2,2,
2,2,2,2,2,2,2,2,2,2,2,2,2,2,2,2,2,2,2,2,2,2,2,2,2,2,2,2,2,2,2,2,2,2,2,2,
2,2,2,2,2,2,2,2,2,2,2,2,2,2,2,2,2,2,2,2,2,2,2,2,2,2,2,2,2,2,2,2,2,2,2,2,
2,2,2,2,4),(-2.69182724913245,-2.69021737643475,-2.65825795739905,-2.58460862661745,
-2.5513781104368,-2.53654745415856,-2.53417896831157,-2.53293286373868,
-2.53202255858695,-2.5310455713401,-2.52964951869221,-2.52581178359971,
-2.46691997400996,-2.43153893675863,-2.37467763143315,-2.37233389942129,
-2.37145652546998,-2.37086544010598,-2.37029203612731,-2.36960073746184,
-2.3678748722168,-2.35205643839174,-2.25827162252114,-2.23179160703465,
-2.21375645601447,-2.21126584275741,-2.21000449770419,-2.20909223143685,
-2.20812175254827,-2.20647051929564,-2.20201530441772,-2.1326794421864,
-2.08667222427382,-2.07343427550269,-2.05292010699533,-2.04962053808891,
-2.04862944571759,-2.04801338910414,-2.04744645650479,-2.04670938370279,
-2.04510591528097,-2.03300961099021,-2.03099285405789,-2.00468313915824,
-1.89580293195177,-1.88965815615834,-1.887777118519,-1.8867606914821,-1.88575648341966,
-1.88453956264867,-1.88226008588713,-1.8695389105778,-1.844744687504,-1.75519720363045,
-1.72812297591816,-1.72619548948106,-1.72545091285084,-1.72491605790831,
-1.72434642649189,-1.72357925631012,-1.72185733255494,-1.6765735312575,
-1.57285830927401,-1.5666330997393,-1.56474248673439,-1.56372414675436,
-1.5627297013904,-1.56154438010085,-1.55937933600542,-1.55670073861329,
-1.50534955500438,-1.40863938801605,-1.40382981982381,-1.40275715439446,
-1.40205999887493,-1.40149911974161,-1.40085275541368,-1.39972603475847,
-1.39496095513637,-1.35185545785978,-1.24975298892972,-1.24354362058159,
-1.24165484025532,-1.24063684132499,-1.23964232899484,-1.23845653272119,
-1.23629636849744,-1.23362041078573,-1.18249410735551,-1.08552437079673,
-1.08073283531703,-1.079661584516,-1.0789648530639,-1.07840398075966,-1.07775725014604,
-1.0766289597187,-1.07184405632949,-1.01702452278643,-0.940451079906658,
-0.939255584957217,-0.936220686212519,-0.934619133470207,-0.933976813784099,
-0.931943668374321,-0.929789509926258,-0.921025844263873,-0.919090103766099,
-0.917834448831157,-0.916827531551712,-0.915710145911843,-0.913963815691909,
-0.911821803790093,-0.907667747491708,-0.897515209060679,-0.862092713898233,
-0.767623998352655,-0.76627917751271,-0.764704803620338,-0.762086748279053,
-0.761612423217398,-0.757606402994916,-0.756506206240144,-0.755859241638221,
-0.755298313520025,-0.754601701909895,-0.753241932916879,-0.744076720849981,
-0.721632892976202,-0.680949136162185,-0.661764158671516),.UNSPECIFIED.);
#227=B_SPLINE_CURVE_WITH_KNOTS('',3,(#39817,#39818,#39819,#39820,#39821,
#39822,#39823,#39824,#39825,#39826,#39827,#39828,#39829,#39830,#39831,#39832,
#39833,#39834,#39835,#39836,#39837,#39838,#39839,#39840,#39841,#39842,#39843,
#39844,#39845,#39846,#39847,#39848,#39849,#39850,#39851,#39852,#39853,#39854,
#39855,#39856,#39857,#39858,#39859,#39860,#39861,#39862,#39863,#39864,#39865,
#39866,#39867,#39868,#39869,#39870,#39871,#39872,#39873,#39874,#39875,#39876,
#39877,#39878,#39879,#39880,#39881,#39882,#39883,#39884,#39885,#39886,#39887,
#39888,#39889,#39890,#39891,#39892,#39893,#39894,#39895,#39896,#39897,#39898,
#39899,#39900,#39901,#39902,#39903,#39904,#39905,#39906,#39907,#39908,#39909,
#39910,#39911,#39912,#39913,#39914,#39915,#39916,#39917,#39918,#39919,#39920,
#39921,#39922,#39923,#39924,#39925,#39926,#39927,#39928,#39929,#39930,#39931,
#39932,#39933,#39934,#39935,#39936,#39937,#39938,#39939,#39940,#39941,#39942,
#39943,#39944,#39945,#39946,#39947,#39948,#39949,#39950,#39951,#39952,#39953,
#39954,#39955,#39956,#39957,#39958,#39959,#39960,#39961,#39962,#39963,#39964,
#39965,#39966,#39967,#39968,#39969,#39970,#39971,#39972,#39973,#39974,#39975,
#39976,#39977,#39978,#39979,#39980,#39981,#39982,#39983,#39984,#39985,#39986,
#39987,#39988,#39989,#39990,#39991,#39992,#39993,#39994,#39995,#39996,#39997,
#39998,#39999,#40000,#40001,#40002,#40003,#40004,#40005,#40006,#40007,#40008,
#40009,#40010,#40011,#40012,#40013,#40014,#40015,#40016,#40017,#40018,#40019,
#40020,#40021,#40022,#40023,#40024,#40025,#40026,#40027,#40028,#40029,#40030,
#40031,#40032,#40033,#40034,#40035,#40036,#40037,#40038,#40039,#40040,#40041,
#40042,#40043,#40044,#40045,#40046,#40047,#40048,#40049,#40050,#40051,#40052,
#40053,#40054,#40055,#40056,#40057,#40058,#40059,#40060,#40061,#40062,#40063,
#40064,#40065,#40066,#40067,#40068,#40069,#40070,#40071,#40072,#40073,#40074,
#40075,#40076,#40077,#40078),.UNSPECIFIED.,.F.,.F.,(4,2,2,2,2,2,2,2,2,2,
2,2,2,2,2,2,2,2,2,2,2,2,2,2,2,2,2,2,2,2,2,2,2,2,2,2,2,2,2,2,2,2,2,2,2,2,
2,2,2,2,2,2,2,2,2,2,2,2,2,2,2,2,2,2,2,2,2,2,2,2,2,2,2,2,2,2,2,2,2,2,2,2,
2,2,2,2,2,2,2,2,2,2,2,2,2,2,2,2,2,2,2,2,2,2,2,2,2,2,2,2,2,2,2,2,2,2,2,2,
2,2,2,2,2,2,2,2,2,2,2,2,4),(-3.40032058230379,-3.3799374648879,-3.34212549608457,
-3.28371974346358,-3.28073584446632,-3.27937774803398,-3.27835761528463,
-3.27740085619244,-3.27607968493925,-3.27270795511768,-3.22697058758892,
-3.15481958391072,-3.14172149518491,-3.12656532004299,-3.12178848192617,
-3.11976092952867,-3.11868003839966,-3.11798199532822,-3.11736468867488,
-3.11681555214059,-3.1162460720554,-3.11518103684641,-3.11161020969522,
-3.11044465586696,-3.00830715877538,-2.97902495345214,-2.95997636602871,
-2.9574547972874,-2.95618713308082,-2.95527400905678,-2.95430606855141,
-2.9529428766579,-2.95011956829779,-2.91981856057307,-2.83266407016917,
-2.81944117769823,-2.79902457581346,-2.79684334916451,-2.79570373891997,
-2.79498104536503,-2.79431129292489,-2.79376200880038,-2.79319442855792,
-2.7921387796893,-2.78864783713265,-2.73263644232016,-2.68233283131275,
-2.65115325770841,-2.63679326515295,-2.6344379654432,-2.63320476495985,
-2.63219948154276,-2.63104290751681,-2.62909155825207,-2.62212785911985,
-2.61799868843131,-2.61678846863385,-2.58912004283622,-2.52818601040035,
-2.47600489618271,-2.47390490216913,-2.47279620947344,-2.47208648515507,
-2.47142644307641,-2.4708774781524,-2.47030379223922,-2.46921788872494,
-2.4654638611272,-2.46464692613671,-2.36205448220919,-2.33345152231888,
-2.31406318767361,-2.31153168751624,-2.31026198281973,-2.30934855518638,
-2.30838137302403,-2.3070210161324,-2.30420931445073,-2.27440655411847,
-2.18680257734629,-2.17357027870461,-2.15309788328493,-2.14980231753782,
-2.14881162771975,-2.14819563541882,-2.14762863130534,-2.14689128659541,
-2.14534427281589,-2.13418932717296,-2.03162347160407,-2.01504796289966,
-2.01252810491902,-1.99149525183495,-1.98868385030345,-1.98735267401199,
-1.98633321310056,-1.98524379103596,-1.98354191542762,-1.97828351202086,
-1.94902102029486,-1.90511091655736,-1.83131928365065,-1.82706733137248,
-1.82594229323562,-1.82528960350133,-1.82472923295969,-1.82404027880153,
-1.82271682839484,-1.81448117532174,-1.79686936304596,-1.77200100434899,
-1.70502744633313,-1.66925042616225,-1.66605040947304,-1.66475857200075,
-1.6638094604679,-1.66280508606322,-1.66146073442565,-1.65996835715344,
-1.65745923748942,-1.59973184090697,-1.50904827671948,-1.50420563682844,
-1.50313018707631,-1.50243210645491,-1.50187107856831,-1.5012252082698,
-1.50010100022417,-1.49536973071829,-1.45335850041969,-1.37031440543437),
 .UNSPECIFIED.);
#228=B_SPLINE_CURVE_WITH_KNOTS('',3,(#40080,#40081,#40082,#40083,#40084,
#40085,#40086,#40087,#40088,#40089,#40090,#40091,#40092,#40093,#40094,#40095,
#40096,#40097,#40098,#40099,#40100,#40101,#40102,#40103,#40104,#40105,#40106,
#40107,#40108,#40109,#40110,#40111,#40112,#40113,#40114,#40115,#40116,#40117,
#40118,#40119,#40120,#40121,#40122,#40123,#40124,#40125,#40126,#40127,#40128,
#40129,#40130,#40131,#40132,#40133,#40134,#40135,#40136,#40137,#40138,#40139,
#40140,#40141,#40142,#40143,#40144,#40145,#40146,#40147,#40148,#40149,#40150,
#40151,#40152,#40153,#40154,#40155,#40156,#40157,#40158,#40159,#40160,#40161,
#40162,#40163,#40164,#40165,#40166,#40167,#40168,#40169,#40170,#40171,#40172,
#40173,#40174,#40175,#40176,#40177,#40178,#40179,#40180,#40181,#40182,#40183,
#40184,#40185),.UNSPECIFIED.,.F.,.F.,(4,2,2,2,2,2,2,2,2,2,2,2,2,2,2,2,2,
2,2,2,2,2,2,2,2,2,2,2,2,2,2,2,2,2,2,2,2,2,2,2,2,2,2,2,2,2,2,2,2,2,2,2,4),
(-0.661764158671516,-0.630026095972386,-0.599660466607192,-0.596835164668896,
-0.595471330715412,-0.594503080907936,-0.593529626220461,-0.592547164926349,
-0.590405266744127,-0.580052738956178,-0.560411913828406,-0.525764839858332,
-0.439582547517306,-0.435716517236515,-0.434138317250194,-0.433378007457329,
-0.432838805051148,-0.432327994870582,-0.431606577921066,-0.430125216079379,
-0.416603358644276,-0.391670308022166,-0.357240898860935,-0.318533321754957,
-0.301470244379321,-0.295599217891707,-0.294040538114015,-0.292806344971613,
-0.291799484974881,-0.275951448748212,-0.27332999752129,-0.272041805663648,
-0.271031222873681,-0.27008822001604,-0.268988646385686,-0.265758570119385,
-0.234624138347925,-0.214725054536103,-0.136351665805889,-0.132958720863464,
-0.128284081036437,-0.125800160660937,-0.124997715274561,-0.123538298531019,
-0.112513858500062,-0.111107523597831,-0.11039017572697,-0.109862278437131,
-0.109287353238062,-0.108491022215696,-0.106605911173784,-0.07180074640157,
-0.000962423497023393),.UNSPECIFIED.);
#229=B_SPLINE_CURVE_WITH_KNOTS('',3,(#40186,#40187,#40188,#40189,#40190,
#40191,#40192,#40193,#40194,#40195,#40196,#40197,#40198,#40199,#40200,#40201,
#40202,#40203,#40204,#40205,#40206,#40207,#40208,#40209,#40210,#40211,#40212,
#40213,#40214,#40215,#40216,#40217,#40218,#40219,#40220,#40221,#40222,#40223,
#40224,#40225,#40226,#40227,#40228,#40229,#40230,#40231,#40232,#40233,#40234,
#40235,#40236,#40237,#40238,#40239,#40240,#40241,#40242,#40243,#40244,#40245,
#40246,#40247,#40248,#40249,#40250,#40251,#40252,#40253,#40254,#40255,#40256,
#40257,#40258,#40259,#40260,#40261,#40262,#40263,#40264,#40265,#40266,#40267,
#40268,#40269,#40270,#40271,#40272,#40273,#40274,#40275,#40276,#40277,#40278,
#40279,#40280,#40281,#40282,#40283,#40284,#40285,#40286,#40287,#40288,#40289,
#40290,#40291,#40292,#40293,#40294,#40295,#40296,#40297,#40298,#40299,#40300,
#40301,#40302,#40303,#40304,#40305,#40306,#40307,#40308,#40309,#40310,#40311,
#40312,#40313,#40314,#40315,#40316,#40317,#40318,#40319,#40320,#40321,#40322,
#40323,#40324,#40325,#40326,#40327,#40328,#40329,#40330,#40331,#40332,#40333,
#40334,#40335,#40336,#40337,#40338,#40339,#40340,#40341,#40342,#40343,#40344,
#40345,#40346,#40347,#40348,#40349,#40350,#40351,#40352,#40353,#40354,#40355,
#40356,#40357,#40358,#40359,#40360,#40361,#40362,#40363,#40364,#40365,#40366,
#40367,#40368,#40369,#40370,#40371,#40372,#40373,#40374,#40375,#40376,#40377,
#40378,#40379,#40380,#40381,#40382,#40383,#40384,#40385,#40386,#40387,#40388,
#40389,#40390,#40391,#40392,#40393,#40394,#40395,#40396,#40397,#40398,#40399,
#40400,#40401,#40402,#40403,#40404,#40405,#40406,#40407,#40408,#40409,#40410,
#40411,#40412,#40413,#40414,#40415,#40416,#40417,#40418,#40419,#40420,#40421),
 .UNSPECIFIED.,.F.,.F.,(4,2,2,2,2,2,2,2,2,2,2,2,2,2,2,2,2,2,2,2,2,2,2,2,
2,2,2,2,2,2,2,2,2,2,2,2,2,2,2,2,2,2,2,2,2,2,2,2,2,2,2,2,2,2,2,2,2,2,2,2,
2,2,2,2,2,2,2,2,2,2,2,2,2,2,2,2,2,2,2,2,2,2,2,2,2,2,2,2,2,2,2,2,2,2,2,2,
2,2,2,2,2,2,2,2,2,2,2,2,2,2,2,2,2,2,2,2,2,4),(-4.06265665564838,-4.01519207432212,
-4.01312846426963,-4.01182202416978,-4.01082448393246,-4.0098637311164,
-4.00891442534306,-4.00762310520072,-4.00442831954379,-3.96896057723717,
-3.96159857501236,-3.95572730743425,-3.87447110344671,-3.85351777991439,
-3.85017457363714,-3.84917829964622,-3.84856084631634,-3.84799390674043,
-3.84725857468516,-3.84603571530434,-3.84154145631612,-3.74737549969145,
-3.71602071727454,-3.69960251958336,-3.69055151222796,-3.68849643895652,
-3.68752229726192,-3.68660861106297,-3.68564020162565,-3.68427655733553,
-3.68145298825952,-3.67386870545059,-3.67205408430674,-3.66999013349106,
-3.66953427855102,-3.66751656089206,-3.6648165736704,-3.66361930774808,
-3.66204427725642,-3.65565080301116,-3.63933102626431,-3.59296419710499,
-3.58744400935408,-3.58103705971439,-3.57343088445997,-3.56401678258572,
-3.52848687925774,-3.52665033373977,-3.52586240098824,-3.52528896068898,
-3.5247590761432,-3.52403411954358,-3.52259811093182,-3.51074294975861,
-3.50996875811447,-3.50953532939472,-3.50859699339859,-3.43816279370622,
-3.40053927180154,-3.38126183450086,-3.37255915196901,-3.36885476382934,
-3.36603541399257,-3.36471280953938,-3.36375216849599,-3.36280302016574,
-3.36151224651823,-3.35832048859493,-3.32299411929447,-3.25034085396535,
-3.20546319800254,-3.20362474100503,-3.20283645387427,-3.20226293217564,
-3.20173310177316,-3.20100840944919,-3.19957349920323,-3.18775142581656,
-3.18695135266194,-3.18656364930523,-3.18556377061379,-3.18435838907648,
-3.18181166115263,-3.18048004752747,-3.12627571859425,-3.07335676548773,
-3.05466697981168,-3.04812455278461,-3.04512857599523,-3.04275761795701,
-3.04152606603022,-3.04061399866939,-3.03964089161196,-3.03826001314669,
-3.03452285622337,-2.97386610832818,-2.9560773992344,-2.91021452722237,
-2.89029214015917,-2.88170964771827,-2.88037158935712,-2.87967934896861,
-2.87917238701352,-2.87862072002632,-2.87764485514921,-2.8747821939702,
-2.82554661290418,-2.76830619470589,-2.74655226678981,-2.72497761090541,
-2.7220572100284,-2.71973327591102,-2.71851277221316,-2.71760218473921,
-2.71662420842439,-2.71522558550321,-2.71137354925264,-2.69339729397568),
 .UNSPECIFIED.);
#230=B_SPLINE_CURVE_WITH_KNOTS('',3,(#40427,#40428,#40429,#40430,#40431,
#40432,#40433,#40434,#40435,#40436,#40437,#40438,#40439,#40440,#40441,#40442,
#40443,#40444,#40445,#40446,#40447,#40448,#40449,#40450,#40451,#40452,#40453,
#40454,#40455,#40456,#40457,#40458,#40459,#40460,#40461,#40462,#40463,#40464,
#40465,#40466,#40467,#40468,#40469,#40470,#40471,#40472,#40473,#40474,#40475,
#40476,#40477,#40478,#40479,#40480,#40481,#40482,#40483,#40484,#40485,#40486,
#40487,#40488,#40489,#40490,#40491,#40492,#40493,#40494,#40495,#40496,#40497,
#40498,#40499,#40500,#40501,#40502,#40503,#40504,#40505,#40506,#40507,#40508,
#40509,#40510,#40511,#40512,#40513,#40514,#40515,#40516,#40517,#40518,#40519,
#40520,#40521,#40522,#40523,#40524,#40525,#40526,#40527,#40528,#40529,#40530,
#40531,#40532,#40533,#40534,#40535,#40536,#40537,#40538,#40539,#40540,#40541,
#40542,#40543,#40544,#40545,#40546,#40547,#40548,#40549,#40550,#40551,#40552,
#40553,#40554,#40555,#40556,#40557,#40558,#40559,#40560,#40561,#40562,#40563,
#40564,#40565,#40566,#40567,#40568,#40569,#40570,#40571,#40572,#40573,#40574,
#40575,#40576,#40577,#40578,#40579,#40580,#40581,#40582,#40583,#40584,#40585,
#40586,#40587,#40588,#40589,#40590,#40591,#40592,#40593,#40594,#40595,#40596,
#40597,#40598,#40599,#40600,#40601,#40602,#40603,#40604,#40605,#40606,#40607,
#40608,#40609,#40610,#40611,#40612,#40613,#40614,#40615,#40616,#40617,#40618,
#40619,#40620,#40621,#40622,#40623,#40624,#40625,#40626,#40627,#40628,#40629,
#40630,#40631,#40632,#40633,#40634,#40635,#40636,#40637,#40638,#40639,#40640,
#40641,#40642,#40643,#40644,#40645,#40646,#40647,#40648,#40649,#40650,#40651,
#40652,#40653,#40654,#40655,#40656,#40657,#40658,#40659,#40660,#40661,#40662,
#40663,#40664),.UNSPECIFIED.,.F.,.F.,(4,2,2,2,2,2,2,2,2,2,2,2,2,2,2,2,2,
2,2,2,2,2,2,2,2,2,2,2,2,2,2,2,2,2,2,2,2,2,2,2,2,2,2,2,2,2,2,2,2,2,2,2,2,
2,2,2,2,2,2,2,2,2,2,2,2,2,2,2,2,2,2,2,2,2,2,2,2,2,2,2,2,2,2,2,2,2,2,2,2,
2,2,2,2,2,2,2,2,2,2,2,2,2,2,2,2,2,2,2,2,2,2,2,2,2,2,2,2,2,4),(-1.3698304902262,
-1.32428933057399,-1.31948879307245,-1.31841674433939,-1.31771971518298,
-1.31717135303647,-1.31654222567829,-1.31547285221714,-1.31417946860804,
-1.31158485767664,-1.2840220018988,-1.16451499058872,-1.15890834890452,
-1.15709434131001,-1.15609137329208,-1.15508576708868,-1.15384555596996,
-1.1514563645641,-1.13626793975227,-1.10172225938852,-1.00079513260847,
-0.998376629750531,-0.99574636522065,-0.994804438739867,-0.994259713517067,
-0.99370580272964,-0.992989698771978,-0.992202556689252,-0.990908733506069,
-0.988312875516995,-0.981635028675933,-0.95563725752181,-0.869883529481548,
-0.862521488314064,-0.857018663457017,-0.855690476526718,-0.854487391421601,
-0.852873042988626,-0.850804291411659,-0.8498630066506,-0.849491825407147,
-0.847431178471495,-0.845617153848005,-0.837977650807255,-0.834888443722276,
-0.833648636533639,-0.832618767657051,-0.831566462010941,-0.830037065949472,
-0.826039354092153,-0.773354181536859,-0.76274030407169,-0.678200182203252,
-0.673237596030051,-0.672152565430984,-0.671451498336876,-0.67092123295971,
-0.670301084612403,-0.669271749185127,-0.668036921857623,-0.665601659217542,
-0.659478618965444,-0.647031632655781,-0.614395319742399,-0.547883827271349,
-0.540079567403126,-0.533987894744303,-0.532580789880052,-0.53136665663084,
-0.530217523221808,-0.514314784954095,-0.511690887189617,-0.510402340048761,
-0.509391868369516,-0.508271178459762,-0.506429917338288,-0.499923277918778,
-0.458617353545733,-0.446872452661901,-0.437624566661491,-0.429964520777408,
-0.423435890055808,-0.417766307164819,-0.412773069448065,-0.366078554089945,
-0.351170915829155,-0.349494262709317,-0.348799838132352,-0.348225596507305,
-0.347699321671372,-0.346892330567366,-0.344930194891345,-0.342189945104828,
-0.335002121289331,-0.310825373154438,-0.260371136784263,-0.216497556505191,
-0.211505644306274,-0.191756062727765,-0.189238465608133,-0.187951828889098,
-0.187003947342121,-0.185977866981315,-0.184584787014969,-0.181410256467709,
-0.139156688342432,-0.0509635004110096,-0.0473269913994285,-0.0443169920642124,
-0.0417706281933888,-0.02815904282542,-0.0266665397668058,-0.0259274181360774,
-0.0253939015293733,-0.0248569146346794,-0.0243003809023242,-0.0235698893386271,
-0.0224118256069681,-0.00096066158750924),.UNSPECIFIED.);
#231=B_SPLINE_CURVE_WITH_KNOTS('',3,(#40665,#40666,#40667,#40668,#40669,
#40670,#40671,#40672,#40673,#40674,#40675,#40676,#40677,#40678,#40679,#40680,
#40681,#40682,#40683,#40684,#40685,#40686,#40687,#40688,#40689,#40690,#40691,
#40692,#40693,#40694,#40695,#40696,#40697,#40698,#40699,#40700,#40701,#40702,
#40703,#40704,#40705,#40706,#40707,#40708,#40709,#40710,#40711,#40712,#40713,
#40714,#40715,#40716,#40717,#40718,#40719,#40720,#40721,#40722,#40723,#40724,
#40725,#40726,#40727,#40728,#40729,#40730,#40731,#40732,#40733,#40734,#40735,
#40736,#40737,#40738,#40739,#40740,#40741,#40742,#40743,#40744,#40745,#40746,
#40747,#40748,#40749,#40750,#40751,#40752,#40753,#40754,#40755,#40756,#40757,
#40758,#40759,#40760,#40761,#40762),.UNSPECIFIED.,.F.,.F.,(4,2,2,2,2,2,
2,2,2,2,2,2,2,2,2,2,2,2,2,2,2,2,2,2,2,2,2,2,2,2,2,2,2,2,2,2,2,2,2,2,2,2,
2,2,2,2,2,2,4),(-4.06158090041823,-3.96121984395872,-3.94175624083592,-3.92850692032922,
-3.92620208661939,-3.92497983597762,-3.92397549030708,-3.92296254403926,
-3.92109844107742,-3.91509238718933,-3.79931151758472,-3.78072060932732,
-3.77030457747063,-3.76670833095255,-3.76506418274644,-3.76376375652012,
-3.76308350811494,-3.76252493050456,-3.76187714026647,-3.76077308870359,
-3.75672863766171,-3.75630672469111,-3.75368472373727,-3.75211090308495,
-3.7186870091084,-3.69906245647009,-3.6615266660199,-3.62218340155293,-3.60572584072176,
-3.60328849763299,-3.60203816178099,-3.6011273659431,-3.60015231899455,
-3.59876317750513,-3.59497005068115,-3.53315354605583,-3.47742059325199,
-3.4643646876459,-3.45012892852547,-3.44492118037184,-3.44276017708284,
-3.44162825491389,-3.44066874520663,-3.44006500874364,-3.43949809933791,
-3.43876121291962,-3.43715876353481,-3.42508993849536,-3.40032058230379),
 .UNSPECIFIED.);
#232=B_SPLINE_CURVE_WITH_KNOTS('',3,(#40763,#40764,#40765,#40766,#40767,
#40768,#40769,#40770,#40771,#40772,#40773,#40774,#40775,#40776,#40777,#40778,
#40779,#40780,#40781,#40782,#40783,#40784,#40785,#40786,#40787,#40788,#40789,
#40790,#40791,#40792,#40793,#40794,#40795,#40796,#40797,#40798,#40799,#40800,
#40801,#40802,#40803,#40804,#40805,#40806,#40807,#40808,#40809,#40810,#40811,
#40812,#40813,#40814,#40815,#40816,#40817,#40818,#40819,#40820,#40821,#40822,
#40823,#40824,#40825,#40826,#40827,#40828,#40829,#40830,#40831,#40832,#40833,
#40834,#40835,#40836,#40837,#40838,#40839,#40840,#40841,#40842,#40843,#40844,
#40845,#40846,#40847,#40848,#40849,#40850,#40851,#40852,#40853,#40854,#40855,
#40856,#40857,#40858,#40859,#40860,#40861,#40862,#40863,#40864,#40865,#40866,
#40867,#40868,#40869,#40870,#40871,#40872,#40873,#40874,#40875,#40876,#40877,
#40878,#40879,#40880,#40881,#40882,#40883,#40884,#40885,#40886,#40887,#40888,
#40889,#40890,#40891,#40892,#40893,#40894,#40895,#40896,#40897,#40898,#40899,
#40900,#40901,#40902,#40903,#40904,#40905,#40906,#40907,#40908,#40909,#40910,
#40911,#40912,#40913,#40914,#40915,#40916,#40917,#40918,#40919,#40920,#40921,
#40922,#40923,#40924,#40925,#40926,#40927,#40928,#40929,#40930,#40931,#40932,
#40933,#40934,#40935,#40936,#40937,#40938,#40939,#40940,#40941,#40942,#40943,
#40944,#40945,#40946,#40947,#40948,#40949,#40950,#40951,#40952,#40953,#40954,
#40955,#40956,#40957,#40958,#40959,#40960,#40961,#40962,#40963,#40964,#40965,
#40966,#40967,#40968,#40969,#40970,#40971,#40972,#40973,#40974,#40975,#40976,
#40977,#40978,#40979,#40980,#40981,#40982,#40983,#40984,#40985,#40986,#40987,
#40988,#40989,#40990,#40991,#40992,#40993,#40994,#40995,#40996,#40997,#40998,
#40999,#41000,#41001,#41002,#41003,#41004,#41005,#41006,#41007,#41008,#41009,
#41010,#41011,#41012,#41013,#41014,#41015,#41016,#41017,#41018,#41019,#41020,
#41021,#41022,#41023,#41024,#41025,#41026,#41027,#41028,#41029,#41030,#41031,
#41032,#41033,#41034,#41035,#41036,#41037,#41038,#41039,#41040,#41041,#41042,
#41043,#41044,#41045,#41046,#41047,#41048,#41049,#41050,#41051,#41052,#41053,
#41054,#41055,#41056,#41057,#41058),.UNSPECIFIED.,.F.,.F.,(4,2,2,2,2,2,
2,2,2,2,2,2,2,2,2,2,2,2,2,2,2,2,2,2,2,2,2,2,2,2,2,2,2,2,2,2,2,2,2,2,2,2,
2,2,2,2,2,2,2,2,2,2,2,2,2,2,2,2,2,2,2,2,2,2,2,2,2,2,2,2,2,2,2,2,2,2,2,2,
2,2,2,2,2,2,2,2,2,2,2,2,2,2,2,2,2,2,2,2,2,2,2,2,2,2,2,2,2,2,2,2,2,2,2,2,
2,2,2,2,2,2,2,2,2,2,2,2,2,2,2,2,2,2,2,2,2,2,2,2,2,2,2,2,2,2,2,2,2,4),(-2.69339729397568,
-2.65070256896701,-2.56185162080011,-2.55807568284471,-2.55703458106043,
-2.55640704715056,-2.55584276078045,-2.5551147496108,-2.55360096451557,
-2.54369393474394,-2.54119861290314,-2.53936703346992,-2.44851580038719,
-2.42584793755402,-2.40210297604234,-2.39901597915292,-2.39658428836075,
-2.39534086308734,-2.39442706667613,-2.39345864486377,-2.39209515421873,
-2.38927245944913,-2.38168588342074,-2.37987037215632,-2.37780613827738,
-2.37735648789383,-2.37649300859573,-2.37442117695808,-2.37282220936172,
-2.37161790754733,-2.37030672687911,-2.36235115980645,-2.33342087300233,
-2.31416461982431,-2.27869168641303,-2.25063483858677,-2.24057872494133,
-2.23524708131059,-2.23407845254968,-2.23342259462732,-2.23291834450145,
-2.23234435389043,-2.23125780484793,-2.22750093263263,-2.16716361119526,
-2.1183454568295,-2.08100995136657,-2.07488664936594,-2.07308485763927,
-2.07197270132617,-2.07095969105062,-2.06965359577783,-2.06694310145696,
-2.04923703472158,-2.04477511220494,-2.03186986825692,-1.98640636545065,
-1.91635069540718,-1.9121484407553,-1.91102789463409,-1.91037599913304,
-1.90981518559431,-1.90912426906663,-1.9077927286498,-1.89937547193282,
-1.88034893507459,-1.85494792524301,-1.77779876797247,-1.77405237696026,
-1.75357098639904,-1.75074352732453,-1.74942894204689,-1.74841158346819,
-1.74731393013775,-1.74557713694573,-1.74003359769068,-1.70820883303056,
-1.66242401709319,-1.59300021985711,-1.58903215274263,-1.58793558484484,
-1.58728927389974,-1.58673904526217,-1.58608698590166,-1.58536324197837,
-1.58422148544993,-1.58203512981867,-1.56154817337327,-1.54089963874239,
-1.43501694765643,-1.42878156302234,-1.42688894239053,-1.4258697553289,
-1.42487462764692,-1.42366435536843,-1.42141816436874,-1.40936838489987,
-1.38559989939009,-1.34014581549528,-1.27589427376871,-1.27453722731701,
-1.27295923601943,-1.27031187285776,-1.26592902817596,-1.26479078675474,
-1.26413482703853,-1.26358537257141,-1.26291828704283,-1.26219941874474,
-1.26106920273423,-1.25891313556766,-1.20527170670429,-1.11115614921505,
-1.10552052161462,-1.10370220460565,-1.10269804146774,-1.10169200819346,
-1.10045241260208,-1.09806796051367,-1.08302059758581,-1.04902629263222,
-0.94726209072256,-0.946065598114438,-0.942512328583506,-0.941448974233042,
-0.940879632521123,-0.94037299481827,-0.939723257934841,-0.93856497078791,
-0.937137595362479,-0.934170310341013,-0.926161130851365,-0.900140778734837,
-0.809725910550172,-0.803510070067896,-0.80203686444722,-0.800827345210138,
-0.799526136163081,-0.78369314250953,-0.78107207453701,-0.77978380027982,
-0.778773028119492,-0.777651475659123,-0.775807586722291,-0.769279502083752,
-0.727753271970297,-0.68465412528036,-0.662515798853911),.UNSPECIFIED.);
#233=B_SPLINE_CURVE_WITH_KNOTS('',3,(#41063,#41064,#41065,#41066,#41067,
#41068,#41069,#41070,#41071,#41072,#41073,#41074,#41075,#41076,#41077,#41078,
#41079,#41080,#41081,#41082,#41083,#41084,#41085,#41086,#41087,#41088,#41089,
#41090,#41091,#41092,#41093,#41094,#41095,#41096,#41097,#41098,#41099,#41100,
#41101,#41102,#41103,#41104,#41105,#41106,#41107,#41108,#41109,#41110,#41111,
#41112,#41113,#41114,#41115,#41116,#41117,#41118,#41119,#41120,#41121,#41122,
#41123,#41124,#41125,#41126,#41127,#41128,#41129,#41130,#41131,#41132,#41133,
#41134,#41135,#41136,#41137,#41138,#41139,#41140,#41141,#41142,#41143,#41144,
#41145,#41146,#41147,#41148,#41149,#41150,#41151,#41152,#41153,#41154,#41155,
#41156,#41157,#41158,#41159,#41160,#41161,#41162,#41163,#41164,#41165,#41166,
#41167,#41168,#41169,#41170,#41171,#41172,#41173,#41174,#41175,#41176,#41177,
#41178,#41179,#41180,#41181,#41182,#41183,#41184,#41185,#41186,#41187,#41188,
#41189,#41190,#41191,#41192,#41193,#41194,#41195,#41196,#41197,#41198,#41199,
#41200,#41201,#41202,#41203,#41204,#41205,#41206,#41207,#41208,#41209,#41210,
#41211,#41212,#41213,#41214,#41215,#41216,#41217,#41218,#41219,#41220,#41221,
#41222,#41223,#41224,#41225,#41226,#41227,#41228,#41229,#41230,#41231,#41232,
#41233,#41234,#41235,#41236,#41237,#41238,#41239,#41240,#41241,#41242,#41243,
#41244,#41245,#41246,#41247,#41248,#41249,#41250,#41251,#41252,#41253,#41254,
#41255,#41256,#41257,#41258,#41259,#41260,#41261,#41262,#41263,#41264,#41265,
#41266,#41267,#41268,#41269,#41270,#41271,#41272,#41273,#41274,#41275,#41276,
#41277,#41278,#41279,#41280,#41281,#41282,#41283,#41284,#41285,#41286,#41287,
#41288,#41289,#41290,#41291,#41292,#41293,#41294,#41295,#41296,#41297,#41298,
#41299,#41300,#41301,#41302,#41303,#41304,#41305,#41306,#41307,#41308,#41309,
#41310,#41311,#41312,#41313,#41314),.UNSPECIFIED.,.F.,.F.,(4,2,2,2,2,2,
2,2,2,2,2,2,2,2,2,2,2,2,2,2,2,2,2,2,2,2,2,2,2,2,2,2,2,2,2,2,2,2,2,2,2,2,
2,2,2,2,2,2,2,2,2,2,2,2,2,2,2,2,2,2,2,2,2,2,2,2,2,2,2,2,2,2,2,2,2,2,2,2,
2,2,2,2,2,2,2,2,2,2,2,2,2,2,2,2,2,2,2,2,2,2,2,2,2,2,2,2,2,2,2,2,2,2,2,2,
2,2,2,2,2,2,2,2,2,2,2,4),(-3.40051625466855,-3.38690541455584,-3.29044724348338,
-3.26182515764191,-3.25917667588228,-3.25725462489775,-3.25645194662039,
-3.25587582132367,-3.25534925660727,-3.25463722419276,-3.25325163385757,
-3.2427742022924,-3.14888251686569,-3.1259149138765,-3.10185442059904,-3.09719754494597,
-3.09557286172972,-3.09463097013533,-3.0936578702247,-3.09240296646104,
-3.08995249069854,-3.07631855204624,-3.0759108883163,-3.06280325578392,
-2.9944847485952,-2.9396157336949,-2.93482999960508,-2.93370135045011,-2.93305438698172,
-2.93249329577895,-2.93179627242911,-2.9307245383389,-2.92593024470862,
-2.83839821057211,-2.77826275267882,-2.77398055322274,-2.77240850017005,
-2.77146704313098,-2.77046947700221,-2.76916901166849,-2.76650486519096,
-2.76340131264863,-2.68466730315942,-2.63581402890625,-2.61638155158392,
-2.61169127291663,-2.61057010115868,-2.60992480882675,-2.60936356912183,
-2.60866430825142,-2.60758535187923,-2.60270114104014,-2.50661658037635,
-2.47325099501405,-2.45267365450566,-2.45010863753982,-2.44884889051031,
-2.44787079423109,-2.44678664156047,-2.44507940440876,-2.44000822910834,
-2.35754081200886,-2.33411547965245,-2.30175434425609,-2.29327589962243,
-2.28857373653641,-2.28745166784889,-2.28680619727978,-2.28624500924613,
-2.28554607851144,-2.28446812165807,-2.27959593184768,-2.18513398554553,
-2.13165235681725,-2.12763911299052,-2.12610717286206,-2.12505420270318,
-2.12402453156198,-2.12278598363417,-2.1197052715485,-2.09153095940257,
-2.06180893345821,-2.03079833106906,-1.9788587385233,-1.97780567351586,
-1.96630110262639,-1.96472011759108,-1.96398719463192,-1.96342079068491,
-1.96280255116963,-1.96180209855782,-1.95841829966425,-1.93704358169982,
-1.91325698683968,-1.81122573363896,-1.80528287711341,-1.80342611911971,
-1.80241441768905,-1.801409562889,-1.80018416514624,-1.79786580618383,-1.78433969447462,
-1.76281990219557,-1.71774508637011,-1.64652664800121,-1.64247609741258,
-1.6413712992311,-1.64072326773154,-1.6401735004104,-1.63949812202562,-1.63876695437737,
-1.63760719800645,-1.63537281832261,-1.61410789402183,-1.59053766742233,
-1.48825184801937,-1.4822503421835,-1.48038647250649,-1.47937339283081,
-1.47836874925764,-1.47714589771116,-1.47483921777996,-1.46156089437542,
-1.44368541513119,-1.41935152810288,-1.3698304902262),.UNSPECIFIED.);
#234=B_SPLINE_CURVE_WITH_KNOTS('',3,(#41316,#41317,#41318,#41319,#41320,
#41321,#41322,#41323,#41324,#41325,#41326,#41327,#41328,#41329,#41330,#41331,
#41332,#41333,#41334,#41335,#41336,#41337,#41338,#41339,#41340,#41341,#41342,
#41343,#41344,#41345,#41346,#41347,#41348,#41349,#41350,#41351,#41352,#41353,
#41354,#41355,#41356,#41357,#41358,#41359,#41360,#41361,#41362,#41363,#41364,
#41365,#41366,#41367,#41368,#41369,#41370,#41371,#41372,#41373,#41374,#41375,
#41376,#41377,#41378,#41379,#41380,#41381,#41382,#41383,#41384,#41385,#41386,
#41387,#41388,#41389,#41390,#41391,#41392,#41393,#41394,#41395,#41396,#41397,
#41398,#41399,#41400,#41401,#41402,#41403,#41404,#41405,#41406,#41407,#41408,
#41409,#41410,#41411,#41412,#41413,#41414,#41415),.UNSPECIFIED.,.F.,.F.,
(4,2,2,2,2,2,2,2,2,2,2,2,2,2,2,2,2,2,2,2,2,2,2,2,2,2,2,2,2,2,2,2,2,2,2,
2,2,2,2,2,2,2,2,2,2,2,2,2,2,4),(-0.662515798853911,-0.622949123215544,-0.619410428437198,
-0.618348821592143,-0.617779855577449,-0.61727348175795,-0.61662335073915,
-0.615461241975333,-0.614029492323155,-0.611049758161222,-0.602994553941927,
-0.582591376448421,-0.464885700533223,-0.459078084680766,-0.457237914063416,
-0.456229405836154,-0.455324525615237,-0.454136371618478,-0.451991683794027,
-0.441691859967688,-0.422235387403578,-0.369406626324371,-0.346797847004858,
-0.315359670773203,-0.31176284413968,-0.311165310532351,-0.309750598088807,
-0.308997290185044,-0.297114933102574,-0.295519246214448,-0.294783510064955,
-0.294216647726752,-0.293691522326338,-0.292801384326984,-0.290312890080721,
-0.28660728759925,-0.275758530936159,-0.256353821445812,-0.177202364163881,
-0.161461846237226,-0.15888819944909,-0.137860606717043,-0.135012274995971,
-0.133694002962819,-0.132676353075674,-0.131580919887413,-0.129852994620517,
-0.124381467664199,-0.0326164518727757,-0.000962543441835597),
 .UNSPECIFIED.);
#235=B_SPLINE_CURVE_WITH_KNOTS('',3,(#41416,#41417,#41418,#41419,#41420,
#41421,#41422,#41423,#41424,#41425,#41426,#41427,#41428,#41429,#41430,#41431,
#41432,#41433,#41434,#41435,#41436,#41437,#41438,#41439,#41440,#41441,#41442,
#41443,#41444,#41445,#41446,#41447,#41448,#41449,#41450,#41451,#41452,#41453,
#41454,#41455,#41456,#41457,#41458,#41459,#41460,#41461,#41462,#41463,#41464,
#41465,#41466,#41467,#41468,#41469,#41470,#41471,#41472,#41473,#41474,#41475,
#41476,#41477,#41478,#41479,#41480,#41481,#41482,#41483,#41484,#41485,#41486,
#41487,#41488,#41489,#41490,#41491,#41492,#41493,#41494,#41495,#41496,#41497,
#41498,#41499,#41500,#41501,#41502,#41503,#41504,#41505,#41506,#41507,#41508,
#41509,#41510,#41511,#41512,#41513,#41514,#41515,#41516,#41517,#41518,#41519,
#41520,#41521,#41522,#41523,#41524,#41525,#41526,#41527,#41528,#41529,#41530,
#41531,#41532,#41533,#41534,#41535,#41536,#41537,#41538,#41539,#41540,#41541,
#41542,#41543,#41544,#41545,#41546,#41547,#41548,#41549,#41550,#41551,#41552,
#41553,#41554,#41555,#41556,#41557,#41558,#41559,#41560,#41561,#41562,#41563,
#41564,#41565,#41566,#41567,#41568,#41569,#41570,#41571,#41572,#41573,#41574,
#41575,#41576,#41577,#41578,#41579,#41580,#41581,#41582,#41583,#41584,#41585,
#41586,#41587,#41588,#41589,#41590,#41591,#41592,#41593,#41594,#41595,#41596,
#41597,#41598,#41599,#41600,#41601,#41602,#41603,#41604,#41605,#41606,#41607,
#41608,#41609,#41610,#41611,#41612,#41613,#41614,#41615,#41616,#41617,#41618,
#41619,#41620,#41621,#41622,#41623,#41624,#41625,#41626,#41627,#41628,#41629,
#41630,#41631,#41632,#41633,#41634,#41635,#41636,#41637,#41638,#41639,#41640,
#41641,#41642,#41643,#41644,#41645,#41646,#41647,#41648,#41649,#41650,#41651,
#41652,#41653,#41654,#41655,#41656,#41657,#41658,#41659,#41660,#41661,#41662,
#41663,#41664,#41665),.UNSPECIFIED.,.F.,.F.,(4,2,2,2,2,2,2,2,2,2,2,2,2,
2,2,2,2,2,2,2,2,2,2,2,2,2,2,2,2,2,2,2,2,2,2,2,2,2,2,2,2,2,2,2,2,2,2,2,2,
2,2,2,2,2,2,2,2,2,2,2,2,2,2,2,2,2,2,2,2,2,2,2,2,2,2,2,2,2,2,2,2,2,2,2,2,
2,2,2,2,2,2,2,2,2,2,2,2,2,2,2,2,2,2,2,2,2,2,2,2,2,2,2,2,2,2,2,2,2,2,2,2,
2,2,2,4),(-4.0596306034683,-4.03408001543506,-4.03284230580221,-4.03170089899201,
-4.03097756808815,-4.03042373629631,-4.02988513142353,-4.02934905080663,
-4.02859941912943,-4.02706360203124,-4.01191427368421,-4.01088880758094,
-4.00695556671887,-4.00259288122757,-3.99879678480457,-3.92038330815872,
-3.88759839889834,-3.87286396112631,-3.87049385401555,-3.86925792642461,
-3.86834927503052,-3.86736850537898,-3.86595760047595,-3.86201915130986,
-3.79801492584274,-3.74918338795194,-3.72749401875158,-3.71549138511218,
-3.71150146194004,-3.70886194487888,-3.70795327373198,-3.70742801778671,
-3.70686347063613,-3.706141292649,-3.70461486335358,-3.69439946013216,-3.6922147214184,
-3.69124229647514,-3.68257061893155,-3.63689995490928,-3.63161815457147,
-3.62553548874142,-3.61841228804763,-3.60985877235864,-3.59913723358057,
-3.56525610322083,-3.55024196353418,-3.54786034373455,-3.54662196201688,
-3.54561678399208,-3.5446133657065,-3.54279609643532,-3.53716148935955,
-3.44334607352452,-3.41156627664411,-3.39501784720514,-3.38962202868366,
-3.38740390849395,-3.38625045409914,-3.38527079066045,-3.38466502365465,
-3.38409903877816,-3.38336721957741,-3.38179077893482,-3.37038791533419,
-3.36830240252975,-3.36680624056531,-3.28754070723922,-3.24331774492344,
-3.22744220416606,-3.22502692419042,-3.22378145826932,-3.22278492279516,
-3.22164145714426,-3.21969672018744,-3.2129999374358,-3.20920949631288,
-3.20516314771942,-3.20475690458286,-3.20267336689837,-3.20146592327029,
-3.20025443429063,-3.19873737695966,-3.19251620843431,-3.10217498483601,
-3.07620828638405,-3.06816710065458,-3.06519197002561,-3.06376218451645,
-3.06260272101135,-3.06195296993781,-3.06144715052437,-3.06079310040788,
-3.05966177859417,-3.05534404352915,-2.95177595452284,-2.91911179588142,
-2.90440680881616,-2.9020377769674,-2.90080201522956,-2.89979698349377,
-2.89879206137503,-2.89696744076646,-2.89127597270991,-2.88911797889175,
-2.88479916972265,-2.88410396155892,-2.88257827035607,-2.88049092384788,
-2.87865122004206,-2.87742741771214,-2.87593728901736,-2.86991356312346,
-2.86204544015667,-2.82739388957354,-2.74398120228353,-2.74169769204191,
-2.74051959611997,-2.73978085024382,-2.73911187661108,-2.73856146983336,
-2.73800409849907,-2.73699845355724,-2.73390788155705,-2.69171368309219),
 .UNSPECIFIED.);
#236=B_SPLINE_CURVE_WITH_KNOTS('',3,(#41671,#41672,#41673,#41674,#41675,
#41676,#41677,#41678,#41679,#41680,#41681,#41682,#41683,#41684,#41685,#41686,
#41687,#41688,#41689,#41690,#41691,#41692,#41693,#41694,#41695,#41696,#41697,
#41698,#41699,#41700,#41701,#41702,#41703,#41704,#41705,#41706,#41707,#41708,
#41709,#41710,#41711,#41712,#41713,#41714,#41715,#41716,#41717,#41718,#41719,
#41720,#41721,#41722,#41723,#41724,#41725,#41726,#41727,#41728,#41729,#41730,
#41731,#41732,#41733,#41734,#41735,#41736,#41737,#41738,#41739,#41740,#41741,
#41742,#41743,#41744,#41745,#41746,#41747,#41748,#41749,#41750,#41751,#41752,
#41753,#41754,#41755,#41756,#41757,#41758,#41759,#41760,#41761,#41762,#41763,
#41764,#41765,#41766,#41767,#41768,#41769,#41770,#41771,#41772,#41773,#41774,
#41775,#41776,#41777,#41778,#41779,#41780,#41781,#41782,#41783,#41784,#41785,
#41786,#41787,#41788,#41789,#41790,#41791,#41792,#41793,#41794,#41795,#41796,
#41797,#41798,#41799,#41800,#41801,#41802,#41803,#41804,#41805,#41806,#41807,
#41808,#41809,#41810,#41811,#41812,#41813,#41814,#41815,#41816,#41817,#41818,
#41819,#41820,#41821,#41822,#41823,#41824,#41825,#41826,#41827,#41828,#41829,
#41830,#41831,#41832,#41833,#41834,#41835,#41836,#41837,#41838,#41839,#41840,
#41841,#41842,#41843,#41844,#41845,#41846,#41847,#41848,#41849,#41850,#41851,
#41852,#41853,#41854,#41855,#41856,#41857,#41858,#41859,#41860,#41861,#41862,
#41863,#41864,#41865,#41866,#41867,#41868,#41869,#41870,#41871,#41872,#41873,
#41874,#41875,#41876,#41877,#41878),.UNSPECIFIED.,.F.,.F.,(4,2,2,2,2,2,
2,2,2,2,2,2,2,2,2,2,2,2,2,2,2,2,2,2,2,2,2,2,2,2,2,2,2,2,2,2,2,2,2,2,2,2,
2,2,2,2,2,2,2,2,2,2,2,2,2,2,2,2,2,2,2,2,2,2,2,2,2,2,2,2,2,2,2,2,2,2,2,2,
2,2,2,2,2,2,2,2,2,2,2,2,2,2,2,2,2,2,2,2,2,2,2,2,2,4),(-1.36987613430623,
-1.30423436574626,-1.29811626324107,-1.29627565662543,-1.29513741718348,
-1.29415021048094,-1.29292585758167,-1.29160164608747,-1.28551314135413,
-1.22912540670448,-1.1514675610177,-1.15039164910677,-1.14999982222173,
-1.14917565738476,-1.14856659640192,-1.14757758861731,-1.13599509150043,
-1.13456888154719,-1.1338465289113,-1.1333174206724,-1.13274368225986,-1.13195336291943,
-1.13010235918765,-1.07879156098914,-1.01183753385623,-0.977350897628902,
-0.974177654777872,-0.972890327588509,-0.971942249931243,-0.970936837811205,
-0.969587134846786,-0.96808762884725,-0.958704957096693,-0.941527649371185,
-0.920577195061325,-0.86947729467201,-0.828095524617837,-0.825345004238373,
-0.822496376121744,-0.820889035414862,-0.819416935803335,-0.816869616095077,
-0.815885577195018,-0.812241128523552,-0.811167542563649,-0.810596304375256,
-0.810041485613778,-0.809361030782193,-0.808078076187776,-0.800752014359733,
-0.785412099906747,-0.767208555586726,-0.755505275941498,-0.745623005829675,
-0.684287783424875,-0.654336071043674,-0.651269518831263,-0.650000965646211,
-0.649057624431322,-0.648048804984938,-0.646677074345568,-0.645148759473659,
-0.635073861785818,-0.616181333057069,-0.592577846690027,-0.506035342388049,
-0.490351704678072,-0.488629633387516,-0.487938871576626,-0.487365525035434,
-0.486774079505288,-0.48589541586769,-0.483487625313566,-0.444383945728644,
-0.421291102608374,-0.390511981655186,-0.332109263843609,-0.328527432577969,
-0.327171470527913,-0.326205262954542,-0.32520973250963,-0.32391924591181,
-0.322503597214568,-0.314871297805738,-0.237897467758746,-0.179515446691896,
-0.17767097291996,-0.167086050594585,-0.16569637141602,-0.164983313387578,
-0.164456516221019,-0.163880677574938,-0.163079355626802,-0.161165052577766,
-0.158530029303512,-0.130180035919145,-0.0517939334688018,-0.0100431515482136,
-0.00573742005696059,-0.00410925369192486,-0.00314308150865512,-0.00217102557994161,
-0.00115611315314765,-0.000961498652879823),.UNSPECIFIED.);
#237=B_SPLINE_CURVE_WITH_KNOTS('',3,(#41879,#41880,#41881,#41882,#41883,
#41884,#41885,#41886,#41887,#41888,#41889,#41890,#41891,#41892,#41893,#41894,
#41895,#41896,#41897,#41898,#41899,#41900,#41901,#41902,#41903,#41904,#41905,
#41906,#41907,#41908,#41909,#41910,#41911,#41912,#41913,#41914,#41915,#41916,
#41917,#41918,#41919,#41920,#41921,#41922,#41923,#41924,#41925,#41926,#41927,
#41928,#41929,#41930,#41931,#41932,#41933,#41934,#41935,#41936,#41937,#41938,
#41939,#41940,#41941,#41942,#41943,#41944,#41945,#41946,#41947,#41948,#41949,
#41950,#41951,#41952,#41953,#41954,#41955,#41956,#41957,#41958,#41959,#41960,
#41961,#41962,#41963,#41964,#41965,#41966,#41967,#41968,#41969,#41970,#41971,
#41972),.UNSPECIFIED.,.F.,.F.,(4,2,2,2,2,2,2,2,2,2,2,2,2,2,2,2,2,2,2,2,
2,2,2,2,2,2,2,2,2,2,2,2,2,2,2,2,2,2,2,2,2,2,2,2,2,2,4),(-4.06152144056539,
-4.06068140455345,-4.05639989610793,-3.99939524463301,-3.93815796338596,
-3.91398161098074,-3.90439152400712,-3.90301674327762,-3.90231701789723,
-3.90176099769942,-3.90120101898099,-3.90018324148975,-3.89700056397345,
-3.84186610269507,-3.79113917844855,-3.76884803001755,-3.74759770649987,
-3.74328295757049,-3.74170635388609,-3.74076506738686,-3.7397684490541,
-3.73847187051845,-3.73582568920672,-3.71833684272978,-3.62662415397337,
-3.58209910484305,-3.58026263986025,-3.57947481607542,-3.57890148332518,
-3.57837171917564,-3.57764695854626,-3.57621143270756,-3.56436424142731,
-3.5642206697547,-3.56283798950838,-3.5614878900379,-3.55907159397315,-3.51970491019132,
-3.46869822090784,-3.42394639885459,-3.42010894945472,-3.41860420573156,
-3.41766132551795,-3.41665409833314,-3.41529737921832,-3.41235685579398,
-3.40051625466855),.UNSPECIFIED.);
#238=B_SPLINE_CURVE_WITH_KNOTS('',3,(#41973,#41974,#41975,#41976,#41977,
#41978,#41979,#41980,#41981,#41982,#41983,#41984,#41985,#41986,#41987,#41988,
#41989,#41990,#41991,#41992,#41993,#41994,#41995,#41996,#41997,#41998,#41999,
#42000,#42001,#42002,#42003,#42004,#42005,#42006,#42007,#42008,#42009,#42010,
#42011,#42012,#42013,#42014,#42015,#42016,#42017,#42018,#42019,#42020,#42021,
#42022,#42023,#42024,#42025,#42026,#42027,#42028,#42029,#42030,#42031,#42032,
#42033,#42034,#42035,#42036,#42037,#42038,#42039,#42040,#42041,#42042,#42043,
#42044,#42045,#42046,#42047,#42048,#42049,#42050,#42051,#42052,#42053,#42054,
#42055,#42056,#42057,#42058,#42059,#42060,#42061,#42062,#42063,#42064,#42065,
#42066,#42067,#42068,#42069,#42070,#42071,#42072,#42073,#42074,#42075,#42076,
#42077,#42078,#42079,#42080,#42081,#42082,#42083,#42084,#42085,#42086,#42087,
#42088,#42089,#42090,#42091,#42092,#42093,#42094,#42095,#42096,#42097,#42098,
#42099,#42100,#42101,#42102,#42103,#42104,#42105,#42106,#42107,#42108,#42109,
#42110,#42111,#42112,#42113,#42114,#42115,#42116,#42117,#42118,#42119,#42120,
#42121,#42122,#42123,#42124,#42125,#42126,#42127,#42128,#42129,#42130,#42131,
#42132,#42133,#42134,#42135,#42136,#42137,#42138,#42139,#42140,#42141,#42142,
#42143,#42144,#42145,#42146,#42147,#42148,#42149,#42150,#42151,#42152,#42153,
#42154,#42155,#42156,#42157,#42158,#42159,#42160,#42161,#42162,#42163,#42164,
#42165,#42166,#42167,#42168,#42169,#42170,#42171,#42172,#42173,#42174,#42175,
#42176,#42177,#42178,#42179,#42180,#42181,#42182,#42183,#42184,#42185,#42186,
#42187,#42188,#42189,#42190,#42191,#42192,#42193,#42194,#42195,#42196,#42197,
#42198,#42199,#42200,#42201,#42202,#42203,#42204,#42205,#42206,#42207,#42208,
#42209,#42210,#42211,#42212,#42213,#42214,#42215,#42216,#42217,#42218,#42219,
#42220,#42221,#42222,#42223,#42224,#42225,#42226,#42227,#42228,#42229,#42230,
#42231,#42232,#42233,#42234,#42235,#42236,#42237,#42238,#42239,#42240,#42241,
#42242,#42243,#42244,#42245,#42246,#42247,#42248,#42249,#42250,#42251,#42252,
#42253,#42254,#42255,#42256,#42257,#42258),.UNSPECIFIED.,.F.,.F.,(4,2,2,
2,2,2,2,2,2,2,2,2,2,2,2,2,2,2,2,2,2,2,2,2,2,2,2,2,2,2,2,2,2,2,2,2,2,2,2,
2,2,2,2,2,2,2,2,2,2,2,2,2,2,2,2,2,2,2,2,2,2,2,2,2,2,2,2,2,2,2,2,2,2,2,2,
2,2,2,2,2,2,2,2,2,2,2,2,2,2,2,2,2,2,2,2,2,2,2,2,2,2,2,2,2,2,2,2,2,2,2,2,
2,2,2,2,2,2,2,2,2,2,2,2,2,2,2,2,2,2,2,2,2,2,2,2,2,2,2,2,2,2,2,4),(-2.69171368309219,
-2.6834459837058,-2.62982931510195,-2.60083134579719,-2.58189109315544,
-2.57937317708939,-2.57810643031875,-2.57719360280117,-2.5762256382986,
-2.57486185784924,-2.57203552430532,-2.54158207936534,-2.454598442427,-2.44138213204764,
-2.4209882973397,-2.41880871173648,-2.41766979496211,-2.41670601595081,
-2.41610116601716,-2.41553478118276,-2.41480076821842,-2.41321311081192,
-2.40152586189933,-2.35729451210967,-2.33133511868389,-2.3037434151305,
-2.27880070171448,-2.25914273988751,-2.25660374311802,-2.25533258187017,
-2.25441901382055,-2.2534525218016,-2.25209450490336,-2.24929207125282,
-2.24168527229027,-2.23979352264476,-2.2387547465452,-2.23833373698779,
-2.23706899470299,-2.23497867901234,-2.23268535126204,-2.23148756544026,
-2.22987949183382,-2.22349992178107,-2.14631344688755,-2.12141405431791,
-2.103777826941,-2.0955399947309,-2.09421653519785,-2.09352761440454,-2.09296729079571,
-2.09240005695671,-2.09134588304041,-2.08786663208743,-2.03131222958311,
-1.94041243609069,-1.9349097120671,-1.93310937127585,-1.93210921061048,
-1.93111289840147,-1.92987223042552,-1.92748056084247,-1.91222587243804,
-1.87742633311048,-1.78406204017884,-1.77292496318781,-1.77137877748411,
-1.77064164004646,-1.77007471007355,-1.76945870983849,-1.76846782122739,
-1.76516993242197,-1.7446757700911,-1.73145330775892,-1.64370152734678,
-1.61413261114428,-1.61132657432292,-1.60996765292093,-1.60900090085964,
-1.60800709318742,-1.60672037194052,-1.60530979442929,-1.60299736826935,
-1.59838630961833,-1.55115064625895,-1.45409036483056,-1.44924778746479,
-1.4481025931723,-1.44744519233895,-1.44689039812731,-1.44620942153864,
-1.444923850799,-1.4375413673796,-1.42208245677764,-1.40892146603893,-1.32515132758051,
-1.29127709173573,-1.2881181894425,-1.28683348005702,-1.28588616742654,
-1.28488042266633,-1.28352630486411,-1.28202242438181,-1.27948550867864,
-1.20143317623793,-1.13856807004486,-1.12697225249683,-1.12554567628525,
-1.12482326565083,-1.12429417622832,-1.1237205199338,-1.12293042043797,
-1.12108041317263,-1.07111078932753,-1.0129160316982,-0.9686256971168,-0.965274849938421,
-0.963957142455952,-0.963001250848394,-0.962002107085687,-0.960680606096423,
-0.959221909953988,-0.956794172854803,-0.951868502983901,-0.860647303969667,
-0.822429623753632,-0.820723462521068,-0.818454479535298,-0.817277380238017,
-0.816400074058821,-0.814712279699945,-0.803955067175405,-0.802558983640366,
-0.801844346802657,-0.801317216677441,-0.800741869241858,-0.799942738954365,
-0.798040720255703,-0.795426806270093,-0.767488954905554,-0.716580306283524,
-0.686214775624197,-0.662215315077933),.UNSPECIFIED.);
#239=B_SPLINE_CURVE_WITH_KNOTS('',3,(#42263,#42264,#42265,#42266,#42267,
#42268,#42269,#42270,#42271,#42272,#42273,#42274,#42275,#42276,#42277,#42278,
#42279,#42280,#42281,#42282,#42283,#42284,#42285,#42286,#42287,#42288,#42289,
#42290,#42291,#42292,#42293,#42294,#42295,#42296,#42297,#42298,#42299,#42300,
#42301,#42302,#42303,#42304,#42305,#42306,#42307,#42308,#42309,#42310,#42311,
#42312,#42313,#42314,#42315,#42316,#42317,#42318,#42319,#42320,#42321,#42322,
#42323,#42324,#42325,#42326,#42327,#42328,#42329,#42330,#42331,#42332,#42333,
#42334,#42335,#42336,#42337,#42338,#42339,#42340,#42341,#42342,#42343,#42344,
#42345,#42346,#42347,#42348,#42349,#42350,#42351,#42352,#42353,#42354,#42355,
#42356,#42357,#42358,#42359,#42360,#42361,#42362,#42363,#42364,#42365,#42366,
#42367,#42368,#42369,#42370,#42371,#42372,#42373,#42374,#42375,#42376,#42377,
#42378,#42379,#42380,#42381,#42382,#42383,#42384,#42385,#42386,#42387,#42388,
#42389,#42390,#42391,#42392,#42393,#42394,#42395,#42396,#42397,#42398,#42399,
#42400,#42401,#42402,#42403,#42404,#42405,#42406,#42407,#42408,#42409,#42410,
#42411,#42412,#42413,#42414,#42415,#42416,#42417,#42418,#42419,#42420,#42421,
#42422,#42423,#42424,#42425,#42426,#42427,#42428,#42429,#42430,#42431,#42432,
#42433,#42434,#42435,#42436,#42437,#42438,#42439,#42440,#42441,#42442,#42443,
#42444,#42445,#42446,#42447,#42448,#42449,#42450,#42451,#42452,#42453,#42454,
#42455,#42456,#42457,#42458,#42459,#42460,#42461,#42462,#42463,#42464,#42465,
#42466,#42467,#42468,#42469,#42470,#42471,#42472,#42473,#42474,#42475,#42476,
#42477,#42478,#42479,#42480,#42481,#42482,#42483,#42484,#42485,#42486,#42487,
#42488,#42489,#42490,#42491,#42492,#42493,#42494,#42495,#42496,#42497,#42498,
#42499,#42500,#42501,#42502,#42503,#42504,#42505,#42506,#42507,#42508,#42509,
#42510,#42511,#42512,#42513,#42514,#42515,#42516,#42517,#42518,#42519,#42520,
#42521,#42522,#42523,#42524,#42525,#42526,#42527,#42528,#42529,#42530,#42531,
#42532,#42533,#42534,#42535,#42536,#42537,#42538,#42539,#42540,#42541,#42542,
#42543,#42544,#42545,#42546,#42547,#42548,#42549,#42550,#42551,#42552,#42553,
#42554,#42555,#42556,#42557,#42558,#42559,#42560,#42561,#42562,#42563,#42564,
#42565,#42566,#42567,#42568,#42569,#42570,#42571,#42572,#42573,#42574),
 .UNSPECIFIED.,.F.,.F.,(4,2,2,2,2,2,2,2,2,2,2,2,2,2,2,2,2,2,2,2,2,2,2,2,
2,2,2,2,2,2,2,2,2,2,2,2,2,2,2,2,2,2,2,2,2,2,2,2,2,2,2,2,2,2,2,2,2,2,2,2,
2,2,2,2,2,2,2,2,2,2,2,2,2,2,2,2,2,2,2,2,2,2,2,2,2,2,2,2,2,2,2,2,2,2,2,2,
2,2,2,2,2,2,2,2,2,2,2,2,2,2,2,2,2,2,2,2,2,2,2,2,2,2,2,2,2,2,2,2,2,2,2,2,
2,2,2,2,2,2,2,2,2,2,2,2,2,2,2,2,2,2,2,2,2,2,2,4),(-3.39995023952435,-3.39790066675237,
-3.39647554338721,-3.39531839591686,-3.39466939020519,-3.3941628559474,
-3.39350747895038,-3.39237083965205,-3.38800052013932,-3.30986736661366,
-3.29781501467423,-3.28589623440827,-3.25653148664586,-3.23745178257696,
-3.23492925938281,-3.23366138561753,-3.23274821767803,-3.23178032992174,
-3.23041737502309,-3.22759508668623,-3.22001540203264,-3.21820233110779,
-3.2161395714001,-3.21567962739949,-3.21482505227885,-3.21275437897285,
-3.21115770714825,-3.20995415177942,-3.20864383704753,-3.20247849077143,
-3.11188475322385,-3.08566910456112,-3.07783672016234,-3.07491821067812,
-3.07350834455919,-3.07267325509279,-3.07194060851529,-3.0713794764826,
-3.07084909896983,-3.07012169343935,-3.06829568553229,-3.0468612763854,
-2.97110392994944,-2.91666198446861,-2.91263174144541,-2.91109740062427,
-2.9100440823094,-2.90901508542667,-2.90777856998407,-2.90470928590416,
-2.89704322219085,-2.8952264563716,-2.89316585723297,-2.89279820480907,
-2.89185203346652,-2.88978292200772,-2.8881673481913,-2.88696397865985,
-2.88563624672462,-2.88010094240642,-2.86297139255846,-2.78642153828411,
-2.77330338809929,-2.75347857185489,-2.75133473475138,-2.75020931701263,
-2.74949256999691,-2.7488274144646,-2.74827825173216,-2.74770796380214,
-2.74663894992142,-2.74303386040555,-2.6853016252567,-2.63817349918101,
-2.59689095850564,-2.59038589670011,-2.58854486466318,-2.58742426732301,
-2.58641384871073,-2.58512532742226,-2.58250133730334,-2.56659436911881,
-2.5654522657683,-2.5642375553304,-2.56258903137233,-2.55631849527417,-2.47888185542894,
-2.43052788453324,-2.4283984213266,-2.42727845525793,-2.42656397839662,
-2.42590048476646,-2.42534242960493,-2.42476832422689,-2.42368047003734,
-2.41990938144759,-2.35831457109675,-2.33530954161544,-2.31072021846032,
-2.26971802830651,-2.26649592541021,-2.26509431412158,-2.26406670460222,
-2.26312074881111,-2.26184179621844,-2.25871643895931,-2.22632332949083,
-2.14107475443467,-2.12155743592282,-2.10992376517262,-2.10469937808016,
-2.10353846530059,-2.10288442504077,-2.10238036608172,-2.10180529809044,
-2.10071285584473,-2.09690098697674,-2.03157418266106,-1.94931965694971,
-1.94419670464287,-1.9424475215289,-1.94145739602333,-1.94055004817484,
-1.93933081508783,-1.93704185324756,-1.92414092186055,-1.89947793153787,
-1.80970500212944,-1.7828437948926,-1.78091909972448,-1.7801748175239,-1.77963990868748,
-1.77906996196085,-1.77830193509584,-1.77657629368887,-1.72982597768656,
-1.627302407254,-1.62125144730327,-1.61941870818423,-1.61828230243568,-1.61729473534568,
-1.61606910124171,-1.6147415703603,-1.60860350461782,-1.57110518123865,
-1.49079653385519,-1.45978295883548,-1.45779756346203,-1.45704348083467,
-1.45650596722624,-1.45599441638679,-1.45526822408518,-1.45376275383313,
-1.4390395989317,-1.41136436481419,-1.36987613430623),.UNSPECIFIED.);
#240=B_SPLINE_CURVE_WITH_KNOTS('',3,(#42576,#42577,#42578,#42579,#42580,
#42581,#42582,#42583,#42584,#42585,#42586,#42587,#42588,#42589,#42590,#42591,
#42592,#42593,#42594,#42595,#42596,#42597,#42598,#42599,#42600,#42601,#42602,
#42603,#42604,#42605,#42606,#42607,#42608,#42609,#42610,#42611,#42612,#42613,
#42614,#42615,#42616,#42617,#42618,#42619,#42620,#42621,#42622,#42623,#42624,
#42625,#42626,#42627,#42628,#42629,#42630,#42631,#42632,#42633,#42634,#42635,
#42636,#42637,#42638,#42639,#42640,#42641,#42642,#42643,#42644,#42645,#42646,
#42647,#42648,#42649,#42650,#42651,#42652,#42653,#42654,#42655,#42656,#42657,
#42658,#42659,#42660,#42661,#42662,#42663),.UNSPECIFIED.,.F.,.F.,(4,2,2,
2,2,2,2,2,2,2,2,2,2,2,2,2,2,2,2,2,2,2,2,2,2,2,2,2,2,2,2,2,2,2,2,2,2,2,2,
2,2,2,2,4),(-0.662215315077933,-0.645592509828678,-0.642300582460812,-0.640992787899431,
-0.640039418585149,-0.639037417660101,-0.637705679394495,-0.636232911803243,
-0.633771387936118,-0.628752756583026,-0.537544025971857,-0.497362414649182,
-0.495732165966819,-0.494945917470169,-0.481158980150784,-0.479661225169226,
-0.478920780711691,-0.478386904589461,-0.477816371141681,-0.477044709800266,
-0.475298974857173,-0.43425624349702,-0.39102377666103,-0.365785242715528,
-0.322667312670379,-0.319333571761,-0.318018579878763,-0.317063257448861,
-0.316062233502055,-0.314736831577171,-0.31327294134718,-0.310832948545832,
-0.305873943794809,-0.250575977325575,-0.162097704334626,-0.157377156307122,
-0.15631141826443,-0.155616244542065,-0.155111329213675,-0.154482503161208,
-0.153435247639401,-0.149594333680469,-0.0609460746495673,-0.0009618072526365),
 .UNSPECIFIED.);
#241=B_SPLINE_CURVE_WITH_KNOTS('',3,(#42664,#42665,#42666,#42667,#42668,
#42669,#42670,#42671,#42672,#42673,#42674,#42675,#42676,#42677,#42678,#42679,
#42680,#42681,#42682,#42683,#42684,#42685,#42686,#42687,#42688,#42689,#42690,
#42691,#42692,#42693,#42694,#42695,#42696,#42697,#42698,#42699,#42700,#42701,
#42702,#42703,#42704,#42705,#42706,#42707,#42708,#42709,#42710,#42711,#42712,
#42713,#42714,#42715,#42716,#42717,#42718,#42719,#42720,#42721,#42722,#42723,
#42724,#42725,#42726,#42727,#42728,#42729,#42730,#42731,#42732,#42733,#42734,
#42735,#42736,#42737,#42738,#42739,#42740,#42741,#42742,#42743,#42744,#42745,
#42746,#42747,#42748,#42749,#42750,#42751,#42752,#42753,#42754,#42755,#42756,
#42757,#42758,#42759,#42760,#42761,#42762,#42763,#42764,#42765,#42766,#42767,
#42768,#42769,#42770,#42771,#42772,#42773,#42774,#42775,#42776,#42777,#42778,
#42779,#42780,#42781,#42782,#42783,#42784,#42785,#42786,#42787,#42788,#42789,
#42790,#42791,#42792,#42793,#42794,#42795,#42796,#42797,#42798,#42799,#42800,
#42801,#42802,#42803,#42804,#42805,#42806,#42807,#42808,#42809,#42810,#42811,
#42812,#42813,#42814,#42815,#42816,#42817,#42818,#42819,#42820,#42821,#42822,
#42823,#42824,#42825,#42826,#42827,#42828,#42829,#42830,#42831,#42832,#42833,
#42834,#42835,#42836,#42837,#42838,#42839,#42840,#42841,#42842,#42843,#42844,
#42845,#42846,#42847,#42848,#42849),.UNSPECIFIED.,.F.,.F.,(4,2,2,2,2,2,
2,2,2,2,2,2,2,2,2,2,2,2,2,2,2,2,2,2,2,2,2,2,2,2,2,2,2,2,2,2,2,2,2,2,2,2,
2,2,2,2,2,2,2,2,2,2,2,2,2,2,2,2,2,2,2,2,2,2,2,2,2,2,2,2,2,2,2,2,2,2,2,2,
2,2,2,2,2,2,2,2,2,2,2,2,2,2,4),(-4.06324807418118,-4.06094680439846,-4.05858802674299,
-4.05743017218569,-4.05647707394084,-4.05557150509894,-4.05455859235606,
-4.05269756427623,-4.04602351267091,-3.9560165188871,-3.90112033625435,
-3.89633682194676,-3.89520810170527,-3.89456099549257,-3.89399971838414,
-3.89330238398713,-3.89223002456045,-3.88743057944171,-3.79320381259422,
-3.74333625913723,-3.73859711219189,-3.73623708003318,-3.73480629904628,
-3.73350489678219,-3.73250745586161,-3.73154450131164,-3.73020139324132,
-3.72670012948254,-3.66984168053083,-3.64056688350185,-3.63219371423025,
-3.57838329923819,-3.57322085695561,-3.57206404631861,-3.5714107631116,
-3.57090653822118,-3.57033047369,-3.56923372198927,-3.56538483513116,-3.56431884460312,
-3.46653181268291,-3.41988304625247,-3.41529988356628,-3.41299732211902,
-3.41159057004845,-3.41030648973064,-3.40931169938866,-3.40834295326624,
-3.40697809916241,-3.40414963036706,-3.37371225266012,-3.31275956994051,
-3.30288401391805,-3.29122817984202,-3.25194345633793,-3.24953258999275,
-3.24865335104612,-3.24806168285134,-3.24748825129421,-3.24679753825605,
-3.24507637353263,-3.22943568266711,-3.13069947995998,-3.09548497151522,
-3.09158280970419,-3.08953620295569,-3.08823696927282,-3.08703167687051,
-3.08604565638335,-3.08504226193537,-3.08322778285318,-3.07762183505614,
-2.95863497131182,-2.9496534646441,-2.92962944604377,-2.92637728262097,
-2.92539103621352,-2.92477578614392,-2.92420803549647,-2.9234677481213,
-2.92222823477204,-2.91776441721149,-2.82033351201189,-2.77338243199341,
-2.76878373967125,-2.76647540710207,-2.76506621725414,-2.76378032655481,
-2.76278523414449,-2.76181702812809,-2.76017936177847,-2.75581548862038,
-2.69329048899296),.UNSPECIFIED.);
#242=B_SPLINE_CURVE_WITH_KNOTS('',3,(#42855,#42856,#42857,#42858,#42859,
#42860,#42861,#42862,#42863,#42864,#42865,#42866,#42867,#42868,#42869,#42870,
#42871,#42872,#42873,#42874,#42875,#42876,#42877,#42878,#42879,#42880,#42881,
#42882,#42883,#42884,#42885,#42886,#42887,#42888,#42889,#42890,#42891,#42892,
#42893,#42894,#42895,#42896,#42897,#42898,#42899,#42900,#42901,#42902,#42903,
#42904,#42905,#42906,#42907,#42908,#42909,#42910,#42911,#42912,#42913,#42914,
#42915,#42916,#42917,#42918,#42919,#42920,#42921,#42922,#42923,#42924,#42925,
#42926,#42927,#42928,#42929,#42930,#42931,#42932,#42933,#42934,#42935,#42936,
#42937,#42938,#42939,#42940,#42941,#42942,#42943,#42944,#42945,#42946,#42947,
#42948,#42949,#42950,#42951,#42952,#42953,#42954,#42955,#42956,#42957,#42958,
#42959,#42960,#42961,#42962,#42963,#42964,#42965,#42966,#42967,#42968,#42969,
#42970,#42971,#42972,#42973,#42974,#42975,#42976,#42977,#42978,#42979,#42980,
#42981,#42982,#42983,#42984,#42985,#42986,#42987,#42988,#42989,#42990,#42991,
#42992,#42993,#42994,#42995,#42996,#42997,#42998,#42999,#43000,#43001,#43002,
#43003,#43004,#43005,#43006,#43007,#43008,#43009,#43010,#43011,#43012,#43013,
#43014,#43015,#43016,#43017,#43018,#43019,#43020,#43021,#43022,#43023,#43024,
#43025,#43026,#43027,#43028,#43029,#43030,#43031,#43032,#43033,#43034,#43035,
#43036,#43037,#43038,#43039,#43040,#43041,#43042,#43043,#43044,#43045,#43046),
 .UNSPECIFIED.,.F.,.F.,(4,2,2,2,2,2,2,2,2,2,2,2,2,2,2,2,2,2,2,2,2,2,2,2,
2,2,2,2,2,2,2,2,2,2,2,2,2,2,2,2,2,2,2,2,2,2,2,2,2,2,2,2,2,2,2,2,2,2,2,2,
2,2,2,2,2,2,2,2,2,2,2,2,2,2,2,2,2,2,2,2,2,2,2,2,2,2,2,2,2,2,2,2,2,2,2,4),
(-1.37066776653293,-1.33460806111142,-1.27843454625838,-1.27490538137125,
-1.27384494186462,-1.27327623849506,-1.2727443671615,-1.27208334308297,
-1.27137291597215,-1.27026278909526,-1.26815939788736,-1.21596749878615,
-1.15521930543116,-1.13785427222667,-1.13190929371174,-1.12982047984096,
-1.12926390242655,-1.12716725051053,-1.12548600189073,-1.12166452679788,
-1.11501792324622,-1.11307777832825,-1.11193472432678,-1.1109371540384,
-1.10968858488817,-1.1072614968637,-1.0911110942554,-1.05294827720473,-0.962790991629515,
-0.952600010708145,-0.951073492853772,-0.950343005611409,-0.949797106800045,
-0.94918931220958,-0.948213923797306,-0.947058410422206,-0.944835683636722,
-0.939426774461917,-0.922634630263533,-0.898152765055203,-0.826470251911123,
-0.81694246631414,-0.814468380251856,-0.79341426243295,-0.790600678741848,
-0.789268542665083,-0.788248379364131,-0.787158238475457,-0.785455305656051,
-0.780194144236855,-0.75091903178753,-0.696364997018037,-0.649346778261375,
-0.629995686466905,-0.628214493999182,-0.627494609689144,-0.626965990794584,
-0.6264029513512,-0.625632585884956,-0.624769891471457,-0.623292990596328,
-0.620184827786322,-0.61165270590269,-0.590785794557204,-0.474514607689977,
-0.468486227620434,-0.466618637232425,-0.465604561675056,-0.464599578763892,
-0.463377251188843,-0.461074359188197,-0.447889849426173,-0.425643715760829,
-0.37423412107745,-0.350802150871196,-0.310066575548288,-0.305712847800284,
-0.304577554132952,-0.303922336486818,-0.303415819498663,-0.302766161483592,
-0.301605990347403,-0.300177104416431,-0.297205264114373,-0.289178564973308,
-0.268815189127441,-0.151039005620794,-0.145239288404627,-0.143400332558613,
-0.142392196218494,-0.141386955515489,-0.140155348982315,-0.137807807080494,
-0.123630343973804,-0.0933395015526071,-0.000962437203753903),
 .UNSPECIFIED.);
#243=B_SPLINE_CURVE_WITH_KNOTS('',3,(#43047,#43048,#43049,#43050,#43051,
#43052,#43053,#43054,#43055,#43056,#43057,#43058,#43059,#43060,#43061,#43062,
#43063,#43064,#43065,#43066,#43067,#43068,#43069,#43070,#43071,#43072,#43073,
#43074,#43075,#43076,#43077,#43078,#43079,#43080,#43081,#43082,#43083,#43084,
#43085,#43086,#43087,#43088,#43089,#43090,#43091,#43092,#43093,#43094,#43095,
#43096,#43097,#43098,#43099,#43100,#43101,#43102,#43103,#43104,#43105,#43106,
#43107,#43108,#43109,#43110,#43111,#43112,#43113,#43114,#43115,#43116,#43117,
#43118,#43119,#43120,#43121,#43122,#43123,#43124,#43125,#43126,#43127,#43128,
#43129,#43130,#43131,#43132,#43133,#43134,#43135,#43136,#43137,#43138,#43139,
#43140,#43141,#43142,#43143,#43144,#43145,#43146,#43147,#43148,#43149,#43150,
#43151,#43152,#43153,#43154,#43155,#43156,#43157,#43158,#43159,#43160,#43161,
#43162),.UNSPECIFIED.,.F.,.F.,(4,2,2,2,2,2,2,2,2,2,2,2,2,2,2,2,2,2,2,2,
2,2,2,2,2,2,2,2,2,2,2,2,2,2,2,2,2,2,2,2,2,2,2,2,2,2,2,2,2,2,2,2,2,2,2,2,
2,4),(-4.06083114761616,-4.0435233454223,-4.04221098063693,-4.04141623662022,
-4.04083602012308,-4.04031019513466,-4.03973720305329,-4.03904698337022,
-4.03732685989293,-4.02168752395455,-4.01814001032623,-3.91800909934794,
-3.89465292189995,-3.88278521731068,-3.88055013050155,-3.87934287788983,
-3.8784371303106,-3.87729590673197,-3.87536118579213,-3.86875344233555,
-3.86410513177538,-3.86073828272011,-3.86031560717704,-3.85666346852078,
-3.85546887946217,-3.85380973961977,-3.84939833018316,-3.77132316705227,
-3.74620865332801,-3.72801157574431,-3.72252461606231,-3.72027891342914,
-3.71860615325555,-3.71785089510409,-3.71731835358458,-3.71679147311905,
-3.71607711037126,-3.71468137529038,-3.70391995690264,-3.65357828612443,
-3.64839558307956,-3.64251557028934,-3.63574432833506,-3.62778950622246,
-3.61815234105673,-3.60580757540362,-3.5746238042843,-3.5602655900665,-3.55791098872309,
-3.55667819868517,-3.5556732725962,-3.5546665232428,-3.55283313261629,-3.54707368807194,
-3.42900386082964,-3.40885334500813,-3.40086235155439,-3.39995023952435),
 .UNSPECIFIED.);
#244=B_SPLINE_CURVE_WITH_KNOTS('',3,(#43163,#43164,#43165,#43166,#43167,
#43168,#43169,#43170,#43171,#43172,#43173,#43174,#43175,#43176,#43177,#43178,
#43179,#43180,#43181,#43182,#43183,#43184,#43185,#43186,#43187,#43188,#43189,
#43190,#43191,#43192,#43193,#43194,#43195,#43196,#43197,#43198,#43199,#43200,
#43201,#43202,#43203,#43204,#43205,#43206,#43207,#43208,#43209,#43210,#43211,
#43212,#43213,#43214,#43215,#43216,#43217,#43218,#43219,#43220,#43221,#43222,
#43223,#43224,#43225,#43226,#43227,#43228,#43229,#43230,#43231,#43232,#43233,
#43234,#43235,#43236,#43237,#43238,#43239,#43240,#43241,#43242,#43243,#43244,
#43245,#43246,#43247,#43248,#43249,#43250,#43251,#43252,#43253,#43254,#43255,
#43256,#43257,#43258,#43259,#43260,#43261,#43262,#43263,#43264,#43265,#43266,
#43267,#43268,#43269,#43270,#43271,#43272,#43273,#43274,#43275,#43276,#43277,
#43278,#43279,#43280,#43281,#43282,#43283,#43284,#43285,#43286,#43287,#43288,
#43289,#43290,#43291,#43292,#43293,#43294,#43295,#43296,#43297,#43298,#43299,
#43300,#43301,#43302,#43303,#43304,#43305,#43306,#43307,#43308,#43309,#43310,
#43311,#43312,#43313,#43314,#43315,#43316,#43317,#43318,#43319,#43320,#43321,
#43322,#43323,#43324,#43325,#43326,#43327,#43328,#43329,#43330,#43331,#43332,
#43333,#43334,#43335,#43336,#43337,#43338,#43339,#43340,#43341,#43342,#43343,
#43344,#43345,#43346,#43347,#43348,#43349,#43350,#43351,#43352,#43353,#43354,
#43355,#43356,#43357,#43358,#43359,#43360,#43361,#43362,#43363,#43364,#43365,
#43366,#43367,#43368,#43369,#43370,#43371,#43372,#43373,#43374,#43375,#43376,
#43377,#43378,#43379,#43380,#43381,#43382,#43383,#43384,#43385,#43386,#43387,
#43388,#43389,#43390,#43391,#43392,#43393,#43394,#43395,#43396,#43397,#43398,
#43399,#43400,#43401,#43402,#43403,#43404,#43405,#43406,#43407,#43408,#43409,
#43410,#43411,#43412,#43413,#43414,#43415,#43416,#43417,#43418,#43419,#43420,
#43421,#43422,#43423,#43424,#43425,#43426,#43427,#43428,#43429,#43430,#43431,
#43432,#43433,#43434,#43435,#43436,#43437,#43438,#43439,#43440,#43441,#43442,
#43443,#43444,#43445,#43446,#43447,#43448,#43449,#43450,#43451,#43452),
 .UNSPECIFIED.,.F.,.F.,(4,2,2,2,2,2,2,2,2,2,2,2,2,2,2,2,2,2,2,2,2,2,2,2,
2,2,2,2,2,2,2,2,2,2,2,2,2,2,2,2,2,2,2,2,2,2,2,2,2,2,2,2,2,2,2,2,2,2,2,2,
2,2,2,2,2,2,2,2,2,2,2,2,2,2,2,2,2,2,2,2,2,2,2,2,2,2,2,2,2,2,2,2,2,2,2,2,
2,2,2,2,2,2,2,2,2,2,2,2,2,2,2,2,2,2,2,2,2,2,2,2,2,2,2,2,2,2,2,2,2,2,2,2,
2,2,2,2,2,2,2,2,2,2,2,2,4),(-2.69329048899296,-2.68518151524453,-2.63587705543086,
-2.613600490668,-2.60388411526308,-2.60250455754033,-2.60180365388543,-2.60124730553122,
-2.6006047816103,-2.59952435690388,-2.59570739418735,-2.59497548295562,
-2.49206004011417,-2.44971113826612,-2.44536321179857,-2.44314808030844,
-2.44177795228913,-2.44052152797007,-2.43953026098175,-2.43855164307469,
-2.43686092373885,-2.43214789649179,-2.35865987348145,-2.33667142779089,
-2.31482413970386,-2.2935533968185,-2.28500219987506,-2.28027004736997,
-2.27914550992267,-2.27849943023687,-2.27793820750385,-2.27723986834876,
-2.27616399245107,-2.27131899187077,-2.17490631430192,-2.15086749756722,
-2.13422238242691,-2.12082884661321,-2.11851609227305,-2.11729165256605,
-2.11638361779359,-2.1153958713777,-2.11365916027295,-2.10862790806344,
-2.0315412755472,-1.96135779946775,-1.95712473463824,-1.95600121671346,
-1.95534868475304,-1.95478800101291,-1.95409809694128,-1.95277110478572,
-1.94446177464751,-1.92618277154543,-1.9010482540412,-1.82292578135086,
-1.81880679027884,-1.81543657725583,-1.81395000771291,-1.81186558831238,
-1.81127500109984,-1.80963057796859,-1.80876504964641,-1.80285017221233,
-1.79691850516882,-1.79506270729554,-1.79405095953352,-1.79304569682694,
-1.79181927582225,-1.78949739676563,-1.77590849560258,-1.75197219639686,
-1.66214625200846,-1.6353238906885,-1.63339945282677,-1.63265510770978,
-1.63212009858896,-1.63156141219875,-1.63081574006164,-1.62998721837318,
-1.62859364379587,-1.59678532059277,-1.47937774035837,-1.4735561446105,
-1.4717141905978,-1.47070530759669,-1.46980043858811,-1.46861279208966,
-1.46647050711416,-1.45620912691655,-1.43684953741174,-1.41300802459559,
-1.3294468087224,-1.32821474143486,-1.32609752549758,-1.3257023279389,-1.32252085187905,
-1.31145351653741,-1.30990962763432,-1.30917275851862,-1.3086187909282,
-1.30801857257907,-1.30739381187667,-1.30648860949183,-1.30490690183153,
-1.24931038148874,-1.15601490001656,-1.15037992759812,-1.1485617808286,
-1.14755770206493,-1.14655174706372,-1.14531223865232,-1.14292792546519,
-1.12788054567231,-1.0938842988396,-0.992106753281869,-0.991021816513099,
-0.987399600618392,-0.986328310916322,-0.985757398585146,-0.985208084871823,
-0.984589180503195,-0.983891906375962,-0.982813131861444,-0.980791479443496,
-0.976034457111498,-0.96095183161327,-0.947879637922346,-0.881832770804898,
-0.829975828478919,-0.82652672863915,-0.825192294252787,-0.824231715878857,
-0.823212862961879,-0.821865548914382,-0.818941276088402,-0.772217816359426,
-0.759674536721786,-0.748551528660825,-0.669062549622139,-0.667893878600024,
-0.664322310816838,-0.663256833094503,-0.662687068250773,-0.662206116423806),
 .UNSPECIFIED.);
#245=B_SPLINE_CURVE_WITH_KNOTS('',3,(#43457,#43458,#43459,#43460,#43461,
#43462,#43463,#43464,#43465,#43466,#43467,#43468,#43469,#43470,#43471,#43472,
#43473,#43474,#43475,#43476,#43477,#43478,#43479,#43480,#43481,#43482,#43483,
#43484,#43485,#43486,#43487,#43488,#43489,#43490,#43491,#43492,#43493,#43494,
#43495,#43496,#43497,#43498,#43499,#43500,#43501,#43502,#43503,#43504,#43505,
#43506,#43507,#43508,#43509,#43510,#43511,#43512,#43513,#43514,#43515,#43516,
#43517,#43518,#43519,#43520,#43521,#43522,#43523,#43524,#43525,#43526,#43527,
#43528,#43529,#43530,#43531,#43532,#43533,#43534,#43535,#43536,#43537,#43538,
#43539,#43540,#43541,#43542,#43543,#43544,#43545,#43546,#43547,#43548,#43549,
#43550,#43551,#43552,#43553,#43554,#43555,#43556,#43557,#43558,#43559,#43560,
#43561,#43562,#43563,#43564,#43565,#43566,#43567,#43568,#43569,#43570,#43571,
#43572,#43573,#43574,#43575,#43576,#43577,#43578,#43579,#43580,#43581,#43582,
#43583,#43584,#43585,#43586,#43587,#43588,#43589,#43590,#43591,#43592,#43593,
#43594,#43595,#43596,#43597,#43598,#43599,#43600,#43601,#43602,#43603,#43604,
#43605,#43606,#43607,#43608,#43609,#43610,#43611,#43612,#43613,#43614,#43615,
#43616,#43617,#43618,#43619,#43620,#43621,#43622,#43623,#43624,#43625,#43626,
#43627,#43628,#43629,#43630,#43631,#43632,#43633,#43634,#43635,#43636,#43637,
#43638,#43639,#43640,#43641,#43642,#43643,#43644,#43645,#43646,#43647,#43648,
#43649,#43650,#43651,#43652,#43653,#43654,#43655,#43656,#43657,#43658,#43659,
#43660,#43661,#43662,#43663,#43664,#43665,#43666,#43667,#43668,#43669,#43670,
#43671,#43672,#43673,#43674,#43675,#43676,#43677,#43678,#43679,#43680,#43681,
#43682,#43683,#43684,#43685,#43686,#43687,#43688,#43689,#43690,#43691,#43692,
#43693,#43694,#43695,#43696,#43697,#43698,#43699,#43700,#43701,#43702,#43703,
#43704,#43705,#43706,#43707,#43708,#43709,#43710,#43711,#43712,#43713,#43714,
#43715,#43716,#43717,#43718,#43719,#43720,#43721,#43722,#43723,#43724,#43725,
#43726,#43727,#43728,#43729,#43730,#43731,#43732,#43733,#43734,#43735,#43736,
#43737,#43738,#43739,#43740,#43741,#43742,#43743,#43744,#43745,#43746,#43747,
#43748,#43749,#43750,#43751,#43752,#43753,#43754,#43755,#43756,#43757,#43758,
#43759,#43760,#43761,#43762,#43763,#43764,#43765,#43766,#43767,#43768,#43769,
#43770,#43771,#43772,#43773,#43774,#43775,#43776,#43777,#43778),
 .UNSPECIFIED.,.F.,.F.,(4,2,2,2,2,2,2,2,2,2,2,2,2,2,2,2,2,2,2,2,2,2,2,2,
2,2,2,2,2,2,2,2,2,2,2,2,2,2,2,2,2,2,2,2,2,2,2,2,2,2,2,2,2,2,2,2,2,2,2,2,
2,2,2,2,2,2,2,2,2,2,2,2,2,2,2,2,2,2,2,2,2,2,2,2,2,2,2,2,2,2,2,2,2,2,2,2,
2,2,2,2,2,2,2,2,2,2,2,2,2,2,2,2,2,2,2,2,2,2,2,2,2,2,2,2,2,2,2,2,2,2,2,2,
2,2,2,2,2,2,2,2,2,2,2,2,2,2,2,2,2,2,2,2,2,2,2,2,2,2,2,2,4),(-3.40146716175795,
-3.38592178780429,-3.38007580434383,-3.37600311457039,-3.37446646634171,
-3.37352479071898,-3.37250403191549,-3.37116799921537,-3.36892196149448,
-3.35537875389731,-3.35495807869944,-3.3511536937879,-3.34995803509296,
-3.34845852843925,-3.34145898012805,-3.25321113534674,-3.23986682318901,
-3.22229394875692,-3.21405681300377,-3.2127326555314,-3.21204328367722,
-3.2114825480802,-3.21091485883035,-3.20985972982115,-3.20637643641239,
-3.14996442247769,-3.06263767938197,-3.05683586693267,-3.05409536856676,
-3.05189007844652,-3.05069489981988,-3.04968985447596,-3.04867387658602,
-3.04679744857865,-3.04069804112289,-2.93618631090365,-2.89509228270947,
-2.89039017743441,-2.88926780684782,-2.8886221077132,-2.88806068739338,
-2.887361424203,-2.88628287502378,-2.88140679187724,-2.79080447414862,-2.73296079275012,
-2.73046413792708,-2.72897660470029,-2.72763526878433,-2.7266310505314,
-2.72568018745772,-2.72438314297515,-2.7218261917289,-2.70100602609924,
-2.69892741079334,-2.68920742524319,-2.63669427867626,-2.59090078038923,
-2.57512376986321,-2.56753094498153,-2.56623499306395,-2.56555157834579,
-2.56499637896063,-2.56434035788042,-2.56320208178509,-2.55881987950936,
-2.55617163538544,-2.55459409623113,-2.55324070785018,-2.45875739536967,
-2.40973754566531,-2.40727320983504,-2.40579911294765,-2.40446756058742,
-2.403465031549,-2.40251171218893,-2.40120491893475,-2.39792036932,-2.35781981441189,
-2.32113634392463,-2.28999636926658,-2.24523770428675,-2.24339978367346,
-2.2426115934094,-2.24203809175711,-2.24150824322023,-2.24078347253271,
-2.23934824538023,-2.22751683458497,-2.22672374948812,-2.22625590958104,
-2.22534800975359,-2.22502344831907,-2.22113716132625,-2.18275914630555,
-2.13176431553918,-2.09043712840539,-2.08392676831173,-2.08208469087454,
-2.0809635546848,-2.07995271338379,-2.07866373999067,-2.07603913084501,
-2.06013541600145,-2.05912597775413,-2.05789746442295,-2.05637984014076,
-2.05038603877782,-2.03165219500241,-1.98163923476699,-1.92445196027978,
-1.92098419639131,-1.91993098190839,-1.91936371563633,-1.91880300556955,
-1.91811309626095,-1.91678617685548,-1.90847981233839,-1.89022752324672,
-1.86510097871217,-1.78698163973076,-1.78271435085037,-1.78047239538417,
-1.77925380751239,-1.7774899168109,-1.77541488075755,-1.77202302902228,
-1.76895602377055,-1.76688930463986,-1.76092432549067,-1.75906436135799,
-1.75805174185547,-1.75704650091625,-1.75582139500518,-1.75350588082379,
-1.74005698106839,-1.72772965008905,-1.71007710929056,-1.66077617355242,
-1.60153062805088,-1.59796854243598,-1.59690422779246,-1.59633472984669,
-1.59578534133915,-1.59511830953969,-1.59439907699419,-1.59326799968654,
-1.59110967661637,-1.57106541423971,-1.55791393435228,-1.47568369615516,
-1.44015068004721,-1.43695458447562,-1.43566306983383,-1.43471374148678,
-1.43368815381629,-1.43229938483529,-1.42915028519991,-1.42494178434964,
-1.38492566727802,-1.37066776653293),.UNSPECIFIED.);
#246=B_SPLINE_CURVE_WITH_KNOTS('',3,(#43780,#43781,#43782,#43783,#43784,
#43785,#43786,#43787,#43788,#43789,#43790,#43791,#43792,#43793,#43794,#43795,
#43796,#43797,#43798,#43799,#43800,#43801,#43802,#43803,#43804,#43805,#43806,
#43807,#43808,#43809,#43810,#43811,#43812,#43813,#43814,#43815,#43816,#43817,
#43818,#43819,#43820,#43821,#43822,#43823,#43824,#43825,#43826,#43827,#43828,
#43829,#43830,#43831,#43832,#43833,#43834,#43835,#43836,#43837,#43838,#43839,
#43840,#43841,#43842,#43843,#43844,#43845,#43846,#43847,#43848,#43849,#43850,
#43851,#43852,#43853,#43854,#43855,#43856,#43857,#43858,#43859,#43860,#43861,
#43862,#43863,#43864,#43865,#43866,#43867,#43868,#43869,#43870,#43871,#43872,
#43873,#43874,#43875,#43876,#43877,#43878,#43879,#43880,#43881,#43882,#43883,
#43884,#43885,#43886,#43887,#43888,#43889,#43890,#43891),.UNSPECIFIED.,
 .F.,.F.,(4,2,2,2,2,2,2,2,2,2,2,2,2,2,2,2,2,2,2,2,2,2,2,2,2,2,2,2,2,2,2,
2,2,2,2,2,2,2,2,2,2,2,2,2,2,2,2,2,2,2,2,2,2,2,2,4),(-0.662206116423806,
-0.662137559750041,-0.661470855298611,-0.660752004993613,-0.659621891659609,
-0.657466178368891,-0.652277035860876,-0.63744171206928,-0.624293750850653,
-0.542500520295884,-0.506513522013831,-0.503307672129327,-0.502014398124426,
-0.501064561315932,-0.500039175347543,-0.498652004379523,-0.495512173336552,
-0.440164470154991,-0.429877117309386,-0.421441133205797,-0.414280150821569,
-0.408066434356903,-0.390096250308862,-0.36430290480305,-0.34258084571345,
-0.340748638878288,-0.3400199847707,-0.339489128833762,-0.338927878080486,
-0.33821177337931,-0.33738592326876,-0.33599879987426,-0.333144731416516,
-0.325548652403063,-0.303261682945464,-0.187046472407577,-0.181019307651192,
-0.179151964421858,-0.178137994222143,-0.17713309747737,-0.175910848293904,
-0.173608024962096,-0.16042186776298,-0.138243228604426,-0.100181521156588,
-0.0328147580883714,-0.0293606617536357,-0.0188857287964917,-0.0175003670608609,
-0.0167884398410369,-0.0162619461170664,-0.0157295202875011,-0.0151663174959569,
-0.0144172166227127,-0.0132147540621359,-0.00096088211313939),
 .UNSPECIFIED.);
#247=B_SPLINE_CURVE_WITH_KNOTS('',3,(#43892,#43893,#43894,#43895,#43896,
#43897,#43898,#43899,#43900,#43901,#43902,#43903,#43904,#43905,#43906,#43907,
#43908,#43909,#43910,#43911,#43912,#43913,#43914,#43915,#43916,#43917,#43918,
#43919,#43920,#43921,#43922,#43923,#43924,#43925,#43926,#43927,#43928,#43929,
#43930,#43931,#43932,#43933,#43934,#43935,#43936,#43937,#43938,#43939,#43940,
#43941,#43942,#43943,#43944,#43945,#43946,#43947,#43948,#43949,#43950,#43951,
#43952,#43953,#43954,#43955,#43956,#43957,#43958,#43959,#43960,#43961,#43962,
#43963,#43964,#43965,#43966,#43967,#43968,#43969,#43970,#43971,#43972,#43973,
#43974,#43975,#43976,#43977,#43978,#43979,#43980,#43981,#43982,#43983,#43984,
#43985,#43986,#43987,#43988,#43989,#43990,#43991,#43992,#43993,#43994,#43995,
#43996,#43997,#43998,#43999,#44000,#44001,#44002,#44003,#44004,#44005,#44006,
#44007,#44008,#44009,#44010,#44011,#44012,#44013,#44014,#44015,#44016,#44017,
#44018,#44019,#44020,#44021,#44022,#44023,#44024,#44025,#44026,#44027,#44028,
#44029,#44030,#44031,#44032,#44033,#44034,#44035,#44036,#44037,#44038,#44039,
#44040,#44041,#44042,#44043,#44044,#44045,#44046,#44047,#44048,#44049,#44050,
#44051,#44052,#44053,#44054,#44055,#44056,#44057,#44058,#44059,#44060,#44061,
#44062,#44063,#44064,#44065,#44066,#44067,#44068,#44069,#44070,#44071,#44072,
#44073,#44074,#44075,#44076,#44077,#44078,#44079,#44080,#44081,#44082,#44083,
#44084,#44085,#44086,#44087,#44088,#44089,#44090,#44091,#44092,#44093,#44094,
#44095,#44096,#44097,#44098,#44099,#44100,#44101,#44102,#44103,#44104,#44105,
#44106,#44107),.UNSPECIFIED.,.F.,.F.,(4,2,2,2,2,2,2,2,2,2,2,2,2,2,2,2,2,
2,2,2,2,2,2,2,2,2,2,2,2,2,2,2,2,2,2,2,2,2,2,2,2,2,2,2,2,2,2,2,2,2,2,2,2,
2,2,2,2,2,2,2,2,2,2,2,2,2,2,2,2,2,2,2,2,2,2,2,2,2,2,2,2,2,2,2,2,2,2,2,2,
2,2,2,2,2,2,2,2,2,2,2,2,2,2,2,2,2,2,4),(-4.06206535738935,-3.97005035195392,
-3.93532834806842,-3.92009277866108,-3.91770192381126,-3.91646144925626,
-3.9154651797298,-3.91431787006135,-3.9123564003393,-3.90551022367957,-3.90179718679256,
-3.90021178661866,-3.89942353102071,-3.89828306951866,-3.89763928331943,
-3.89556052258089,-3.89404019770954,-3.89283571977218,-3.89152072187029,
-3.88537296495507,-3.79474634673191,-3.76845098056662,-3.76069391311167,
-3.75779617436791,-3.75639375423261,-3.75556177277186,-3.7548135137795,
-3.75425472747258,-3.75372088014253,-3.75298003247016,-3.75148007628766,
-3.73760814400221,-3.7121544153632,-3.6897927442744,-3.64578019267646,-3.61652637292871,
-3.59748865186431,-3.59496743894511,-3.59369986043141,-3.5927867611743,
-3.59181881259745,-3.59045555303582,-3.58763192109274,-3.5573149981734,
-3.47018363921452,-3.45696206231222,-3.44163717599157,-3.43648127401355,
-3.43433616112414,-3.43321027622464,-3.43225493001972,-3.43165208672577,
-3.43109949803665,-3.43036873264978,-3.42879866431127,-3.41756485950941,
-3.36523111801977,-3.3133785512979,-3.27907545344096,-3.27326642996472,
-3.27149976574654,-3.27039584794461,-3.26938126812184,-3.26808216638591,
-3.26533331483837,-3.2467336421036,-3.24521126105597,-3.23855574869198,
-3.14938095713286,-3.12410205319073,-3.11540569192217,-3.11225435038609,
-3.11076259053383,-3.10989396181372,-3.10911978216742,-3.10855609704119,
-3.10802882251451,-3.10731356852286,-3.10591503667278,-3.0950923809918,
-3.09346368105756,-3.09303336517969,-3.08481470087977,-3.04234389695859,
-2.98311607405423,-2.96482869096398,-2.95134638946022,-2.94902993315509,
-2.94780488744436,-2.94679998408651,-2.94578794757581,-2.94392975562866,
-2.93797589985788,-2.82139320316555,-2.80387383085411,-2.78970630072558,
-2.78794202482143,-2.78696383546038,-2.78611149818159,-2.78553171105634,
-2.78495840664869,-2.7842679874125,-2.78254828931893,-2.76695288708008,
-2.76594527306988,-2.76304764473065,-2.6999573776292,-2.69323737458904),
 .UNSPECIFIED.);
#248=B_SPLINE_CURVE_WITH_KNOTS('',3,(#44113,#44114,#44115,#44116,#44117,
#44118,#44119,#44120,#44121,#44122,#44123,#44124,#44125,#44126,#44127,#44128,
#44129,#44130,#44131,#44132,#44133,#44134,#44135,#44136,#44137,#44138,#44139,
#44140,#44141,#44142,#44143,#44144,#44145,#44146,#44147,#44148,#44149,#44150,
#44151,#44152,#44153,#44154,#44155,#44156,#44157,#44158,#44159,#44160,#44161,
#44162,#44163,#44164,#44165,#44166,#44167,#44168,#44169,#44170,#44171,#44172,
#44173,#44174,#44175,#44176,#44177,#44178,#44179,#44180,#44181,#44182,#44183,
#44184,#44185,#44186,#44187,#44188,#44189,#44190,#44191,#44192,#44193,#44194,
#44195,#44196,#44197,#44198,#44199,#44200,#44201,#44202,#44203,#44204,#44205,
#44206,#44207,#44208,#44209,#44210,#44211,#44212,#44213,#44214,#44215,#44216,
#44217,#44218,#44219,#44220,#44221,#44222,#44223,#44224,#44225,#44226,#44227,
#44228,#44229,#44230,#44231,#44232,#44233,#44234,#44235,#44236,#44237,#44238,
#44239,#44240,#44241,#44242,#44243,#44244,#44245,#44246,#44247,#44248,#44249,
#44250,#44251,#44252,#44253,#44254,#44255,#44256,#44257,#44258,#44259,#44260,
#44261,#44262,#44263,#44264,#44265,#44266,#44267,#44268,#44269,#44270,#44271,
#44272,#44273,#44274,#44275,#44276,#44277,#44278,#44279,#44280,#44281,#44282,
#44283,#44284,#44285,#44286,#44287,#44288,#44289,#44290,#44291,#44292,#44293,
#44294,#44295,#44296,#44297,#44298,#44299,#44300,#44301,#44302,#44303,#44304),
 .UNSPECIFIED.,.F.,.F.,(4,2,2,2,2,2,2,2,2,2,2,2,2,2,2,2,2,2,2,2,2,2,2,2,
2,2,2,2,2,2,2,2,2,2,2,2,2,2,2,2,2,2,2,2,2,2,2,2,2,2,2,2,2,2,2,2,2,2,2,2,
2,2,2,2,2,2,2,2,2,2,2,2,2,2,2,2,2,2,2,2,2,2,2,2,2,2,2,2,2,2,2,2,2,2,2,4),
(-1.36992249076833,-1.36011110780835,-1.25889637125947,-1.25294780947012,
-1.2510904907751,-1.25007875752745,-1.24917412830259,-1.24801559320514,
-1.24597610048891,-1.24348253171853,-1.18581330666231,-1.09496916055279,
-1.09043233882278,-1.08923357519539,-1.08850558129432,-1.087939951584,-1.08731938653578,
-1.08630835283231,-1.08282480737874,-1.06039988309063,-1.03573485910554,
-0.937333701723687,-0.935904705376236,-0.929870643654192,-0.928002805115158,
-0.926988929954721,-0.926082840215784,-0.924926547731394,-0.922893745984984,
-0.920412645899742,-0.915339463228706,-0.902057370512905,-0.870245011814187,
-0.782618756168538,-0.781186474648235,-0.779696680472317,-0.767794444789422,
-0.766198215635278,-0.765462459288475,-0.764895679749286,-0.76427890352718,
-0.763284785671746,-0.759958400337259,-0.739174741858444,-0.690284340083477,
-0.628460401749236,-0.626947282274918,-0.625752345461889,-0.62222189780312,
-0.621688193249525,-0.617945436550069,-0.614474046058225,-0.613068644374581,
-0.606955283329361,-0.605077698695959,-0.604061785125997,-0.603154284414437,
-0.601999893488966,-0.600115643836136,-0.59776079546241,-0.593034763496795,
-0.580960922147294,-0.557852139939544,-0.450972812757739,-0.446286472258731,
-0.443614844829819,-0.442666671045137,-0.442120612001335,-0.441612255071038,
-0.440908125447865,-0.439512379391033,-0.42929114893009,-0.402499694111724,
-0.36393595292225,-0.343766784911088,-0.314011641336004,-0.285879911581213,
-0.282799963399097,-0.28156141959571,-0.280531630626738,-0.27958552795347,
-0.278555517000745,-0.27597202056229,-0.254197331456896,-0.231034098351554,
-0.180770198187209,-0.124383207341576,-0.120907155426492,-0.119853034392882,
-0.119285629371723,-0.11872500801893,-0.118035535392214,-0.116710451095787,
-0.108445529041699,-0.0905574676002597,-0.000962469125110394),
 .UNSPECIFIED.);
#249=B_SPLINE_CURVE_WITH_KNOTS('',3,(#44305,#44306,#44307,#44308,#44309,
#44310,#44311,#44312,#44313,#44314,#44315,#44316,#44317,#44318,#44319,#44320,
#44321,#44322,#44323,#44324,#44325,#44326,#44327,#44328,#44329,#44330,#44331,
#44332,#44333,#44334,#44335,#44336,#44337,#44338,#44339,#44340,#44341,#44342,
#44343,#44344,#44345,#44346,#44347,#44348,#44349,#44350,#44351,#44352,#44353,
#44354,#44355,#44356,#44357,#44358,#44359,#44360,#44361,#44362,#44363,#44364,
#44365,#44366,#44367,#44368,#44369,#44370,#44371,#44372,#44373,#44374,#44375,
#44376,#44377,#44378,#44379,#44380,#44381,#44382,#44383,#44384,#44385,#44386,
#44387,#44388,#44389,#44390,#44391,#44392,#44393,#44394,#44395,#44396,#44397,
#44398,#44399,#44400,#44401,#44402,#44403,#44404,#44405,#44406,#44407,#44408,
#44409,#44410,#44411,#44412,#44413,#44414,#44415,#44416,#44417,#44418,#44419,
#44420,#44421,#44422,#44423,#44424,#44425,#44426),.UNSPECIFIED.,.F.,.F.,
(4,2,2,2,2,2,2,2,2,2,2,2,2,2,2,2,2,2,2,2,2,2,2,2,2,2,2,2,2,2,2,2,2,2,2,
2,2,2,2,2,2,2,2,2,2,2,2,2,2,2,2,2,2,2,2,2,2,2,2,2,4),(-4.06307029976562,
-4.02621299276285,-4.02351802668358,-4.02194888577496,-4.02084961439851,
-4.01990644418212,-4.01889549160324,-4.01760594727514,-4.01497868571737,
-3.99902422831513,-3.99585419476142,-3.99241343008694,-3.98020157012189,
-3.97450569539038,-3.95242825469067,-3.86361183675127,-3.85981994263567,
-3.85877727241304,-3.85814938065569,-3.85758516285388,-3.85685777469768,
-3.85534718577422,-3.84551021456565,-3.84321483263195,-3.84105582799669,
-3.84059377470798,-3.7501971763093,-3.71980593390042,-3.70724718831045,
-3.69985500085665,-3.69793344300521,-3.69697150209076,-3.69596631676996,
-3.69495132848865,-3.6930800092665,-3.6870233357477,-3.6810663273813,-3.67866874590036,
-3.67658730112641,-3.67479280671131,-3.67357143020716,-3.66934688360038,
-3.658927640011,-3.61079023431505,-3.60549406522702,-3.59946617655345,-3.59250114127332,
-3.5842550103788,-3.55574833781797,-3.54329178305896,-3.53705746829144,
-3.53583174019658,-3.53516340804141,-3.53465857398292,-3.53409334467418,
-3.53305032356407,-3.52966759537004,-3.52804086828078,-3.44207330605695,
-3.40199142588857,-3.40146716175795),.UNSPECIFIED.);
#250=B_SPLINE_CURVE_WITH_KNOTS('',3,(#44427,#44428,#44429,#44430,#44431,
#44432,#44433,#44434,#44435,#44436,#44437,#44438,#44439,#44440,#44441,#44442,
#44443,#44444,#44445,#44446,#44447,#44448,#44449,#44450,#44451,#44452,#44453,
#44454,#44455,#44456,#44457,#44458,#44459,#44460,#44461,#44462,#44463,#44464,
#44465,#44466,#44467,#44468,#44469,#44470,#44471,#44472,#44473,#44474,#44475,
#44476,#44477,#44478,#44479,#44480,#44481,#44482,#44483,#44484,#44485,#44486,
#44487,#44488,#44489,#44490,#44491,#44492,#44493,#44494,#44495,#44496,#44497,
#44498,#44499,#44500,#44501,#44502,#44503,#44504,#44505,#44506,#44507,#44508,
#44509,#44510,#44511,#44512,#44513,#44514,#44515,#44516,#44517,#44518,#44519,
#44520,#44521,#44522,#44523,#44524,#44525,#44526,#44527,#44528,#44529,#44530,
#44531,#44532,#44533,#44534,#44535,#44536,#44537,#44538,#44539,#44540,#44541,
#44542,#44543,#44544,#44545,#44546,#44547,#44548,#44549,#44550,#44551,#44552,
#44553,#44554,#44555,#44556,#44557,#44558,#44559,#44560,#44561,#44562,#44563,
#44564,#44565,#44566,#44567,#44568,#44569,#44570,#44571,#44572,#44573,#44574,
#44575,#44576,#44577,#44578,#44579,#44580,#44581,#44582,#44583,#44584,#44585,
#44586,#44587,#44588,#44589,#44590,#44591,#44592,#44593,#44594,#44595,#44596,
#44597,#44598,#44599,#44600,#44601,#44602,#44603,#44604,#44605,#44606,#44607,
#44608,#44609,#44610,#44611,#44612,#44613,#44614,#44615,#44616,#44617,#44618,
#44619,#44620,#44621,#44622,#44623,#44624,#44625,#44626,#44627,#44628,#44629,
#44630,#44631,#44632,#44633,#44634,#44635,#44636,#44637,#44638,#44639,#44640,
#44641,#44642,#44643,#44644,#44645,#44646,#44647,#44648,#44649,#44650,#44651,
#44652,#44653,#44654,#44655,#44656,#44657,#44658,#44659,#44660,#44661,#44662,
#44663,#44664,#44665,#44666,#44667,#44668,#44669,#44670,#44671,#44672,#44673,
#44674,#44675,#44676,#44677,#44678,#44679,#44680,#44681,#44682,#44683,#44684,
#44685,#44686,#44687,#44688,#44689,#44690,#44691,#44692,#44693,#44694,#44695,
#44696,#44697,#44698,#44699,#44700,#44701,#44702,#44703,#44704,#44705,#44706,
#44707,#44708,#44709,#44710,#44711,#44712,#44713,#44714,#44715,#44716,#44717,
#44718,#44719,#44720,#44721,#44722,#44723,#44724,#44725,#44726,#44727,#44728,
#44729,#44730,#44731,#44732,#44733,#44734,#44735,#44736,#44737,#44738,#44739,
#44740,#44741,#44742,#44743,#44744,#44745,#44746,#44747,#44748,#44749,#44750,
#44751,#44752),.UNSPECIFIED.,.F.,.F.,(4,2,2,2,2,2,2,2,2,2,2,2,2,2,2,2,2,
2,2,2,2,2,2,2,2,2,2,2,2,2,2,2,2,2,2,2,2,2,2,2,2,2,2,2,2,2,2,2,2,2,2,2,2,
2,2,2,2,2,2,2,2,2,2,2,2,2,2,2,2,2,2,2,2,2,2,2,2,2,2,2,2,2,2,2,2,2,2,2,2,
2,2,2,2,2,2,2,2,2,2,2,2,2,2,2,2,2,2,2,2,2,2,2,2,2,2,2,2,2,2,2,2,2,2,2,2,
2,2,2,2,2,2,2,2,2,2,2,2,2,2,2,2,2,2,2,2,2,2,2,2,2,2,2,2,2,2,2,2,2,2,2,2,
2,4),(-2.69323737458904,-2.66695066000876,-2.64182901214515,-2.62819742798369,
-2.62587365866223,-2.62464686156451,-2.62364161081488,-2.62263014466621,
-2.62077563918824,-2.61485408885999,-2.61340434843227,-2.60983489595764,
-2.60626296557934,-2.60577036973392,-2.60366771636178,-2.60264295115914,
-2.60140188674851,-2.59960099323394,-2.59336206742085,-2.50234334390139,
-2.48184443833446,-2.4667959525035,-2.46496963966017,-2.46396693279606,
-2.46330158542213,-2.46267277427215,-2.46212425303578,-2.46142625489302,
-2.46035153700574,-2.45552133442309,-2.36172357025586,-2.3377499186391,
-2.309067134064,-2.30387260323175,-2.30217804510313,-2.30108986212082,-2.30006911586781,
-2.29873274159437,-2.29648534228126,-2.28291394277717,-2.28085154492269,
-2.27898490544721,-2.27442044479301,-2.27357292427173,-2.26183265851919,
-2.25616222555116,-2.19069619573504,-2.16639214407842,-2.14457891796077,
-2.14115312409478,-2.14014798829007,-2.13952859952953,-2.13896235204922,
-2.13823127332206,-2.13666057307168,-2.1254234763837,-2.0321312895758,-2.01041273211509,
-2.00163695316889,-1.99852579826467,-1.982476473502,-1.97984477492052,-1.97855448196252,
-1.97754359859112,-1.97642343478984,-1.97458527985579,-1.96811198895223,
-1.92716989925069,-1.87634647579663,-1.86635080849869,-1.82087757123191,
-1.81804251040804,-1.81707074987542,-1.81651995602071,-1.8160128740924,
-1.81531908673249,-1.81397335733894,-1.8051904272082,-1.78434856242143,
-1.73562894792959,-1.66236926545113,-1.65778956345497,-1.65611895174762,
-1.65514439910985,-1.65415199122443,-1.65288549578109,-1.65150174381603,
-1.64925396753122,-1.64481821807107,-1.60091271802256,-1.50929577850373,
-1.50837720442649,-1.50653385129321,-1.49594631052236,-1.4945563899444,
-1.49384321864254,-1.49331634294621,-1.49274042350044,-1.49193899746327,
-1.49002448480513,-1.48738919481383,-1.45903719466622,-1.34043780707141,
-1.33476307113318,-1.33293987105367,-1.33193481456781,-1.33094916436177,
-1.32974697238497,-1.32845219750689,-1.32641600555728,-1.32254078035876,
-1.28772232709118,-1.1905936034179,-1.18943639177376,-1.18809675704507,
-1.18640008761606,-1.17277676271892,-1.17128371566986,-1.17054439268769,
-1.1700107624716,-1.16943993991893,-1.1686669546663,-1.16691428134074,-1.13222330163187,
-1.01799281189823,-1.01162488132412,-1.00971696749924,-1.00858130290577,
-1.00759102564218,-1.00636135633456,-1.00399381690932,-1.00100551847271,
-0.994484739329017,-0.975873751621818,-0.92554955569963,-0.882694056078951,
-0.850188952980269,-0.848184973688339,-0.847427826112266,-0.846889503149032,
-0.846378360691303,-0.845654623392182,-0.844161440014647,-0.830065530139632,
-0.803250616064687,-0.793092442361747,-0.707915666286649,-0.706669354137044,
-0.705616502074262,-0.703532826701615,-0.70294124217594,-0.70131107551983,
-0.700467005634569,-0.695091100936416,-0.688697051917372,-0.686786176338426,
-0.685649896998808,-0.68465931120268,-0.683430427098059,-0.681066347591054,
-0.678083554983827,-0.67157879553533,-0.662484546563834),.UNSPECIFIED.);
#251=B_SPLINE_CURVE_WITH_KNOTS('',3,(#44757,#44758,#44759,#44760,#44761,
#44762,#44763,#44764,#44765,#44766,#44767,#44768,#44769,#44770,#44771,#44772,
#44773,#44774,#44775,#44776,#44777,#44778,#44779,#44780,#44781,#44782,#44783,
#44784,#44785,#44786,#44787,#44788,#44789,#44790,#44791,#44792,#44793,#44794,
#44795,#44796,#44797,#44798,#44799,#44800,#44801,#44802,#44803,#44804,#44805,
#44806,#44807,#44808,#44809,#44810,#44811,#44812,#44813,#44814,#44815,#44816,
#44817,#44818,#44819,#44820,#44821,#44822,#44823,#44824,#44825,#44826,#44827,
#44828,#44829,#44830,#44831,#44832,#44833,#44834,#44835,#44836,#44837,#44838,
#44839,#44840,#44841,#44842,#44843,#44844,#44845,#44846,#44847,#44848,#44849,
#44850,#44851,#44852,#44853,#44854,#44855,#44856,#44857,#44858,#44859,#44860,
#44861,#44862,#44863,#44864,#44865,#44866,#44867,#44868,#44869,#44870,#44871,
#44872,#44873,#44874,#44875,#44876,#44877,#44878,#44879,#44880,#44881,#44882,
#44883,#44884,#44885,#44886,#44887,#44888,#44889,#44890,#44891,#44892,#44893,
#44894,#44895,#44896,#44897,#44898,#44899,#44900,#44901,#44902,#44903,#44904,
#44905,#44906,#44907,#44908,#44909,#44910,#44911,#44912,#44913,#44914,#44915,
#44916,#44917,#44918,#44919,#44920,#44921,#44922,#44923,#44924,#44925,#44926,
#44927,#44928,#44929,#44930,#44931,#44932,#44933,#44934,#44935,#44936,#44937,
#44938,#44939,#44940,#44941,#44942,#44943,#44944,#44945,#44946,#44947,#44948,
#44949,#44950,#44951,#44952,#44953,#44954,#44955,#44956,#44957,#44958,#44959,
#44960,#44961,#44962,#44963,#44964,#44965,#44966,#44967,#44968,#44969,#44970,
#44971,#44972,#44973,#44974,#44975,#44976,#44977,#44978,#44979,#44980,#44981,
#44982,#44983,#44984,#44985,#44986,#44987,#44988,#44989,#44990,#44991,#44992,
#44993,#44994,#44995,#44996,#44997,#44998,#44999,#45000,#45001,#45002,#45003,
#45004,#45005,#45006,#45007,#45008,#45009,#45010,#45011,#45012,#45013,#45014,
#45015,#45016,#45017,#45018,#45019,#45020,#45021,#45022,#45023,#45024,#45025,
#45026,#45027,#45028,#45029,#45030,#45031,#45032,#45033,#45034,#45035,#45036,
#45037,#45038,#45039,#45040,#45041,#45042,#45043,#45044,#45045,#45046,#45047,
#45048,#45049,#45050,#45051,#45052,#45053,#45054),.UNSPECIFIED.,.F.,.F.,
(4,2,2,2,2,2,2,2,2,2,2,2,2,2,2,2,2,2,2,2,2,2,2,2,2,2,2,2,2,2,2,2,2,2,2,
2,2,2,2,2,2,2,2,2,2,2,2,2,2,2,2,2,2,2,2,2,2,2,2,2,2,2,2,2,2,2,2,2,2,2,2,
2,2,2,2,2,2,2,2,2,2,2,2,2,2,2,2,2,2,2,2,2,2,2,2,2,2,2,2,2,2,2,2,2,2,2,2,
2,2,2,2,2,2,2,2,2,2,2,2,2,2,2,2,2,2,2,2,2,2,2,2,2,2,2,2,2,2,2,2,2,2,2,2,
2,2,2,2,2,4),(-3.39990203970593,-3.37568906292057,-3.36178630294155,-3.35163759979921,
-3.35024913805766,-3.34968079191137,-3.34910709431136,-3.34857802843084,
-3.34785574102047,-3.3464296852929,-3.33484958607241,-3.30149814682876,
-3.26159896141466,-3.22265935806477,-3.20455103077339,-3.19201001310503,
-3.18964468023475,-3.18840929853978,-3.18750023590305,-3.18651823802952,
-3.18510422651216,-3.18114853425714,-3.11655674766835,-3.06673347130353,
-3.0404772553221,-3.02884269113632,-3.027411557059,-3.02669438297866,-3.02618427136127,
-3.02564362271037,-3.02472231361015,-3.02223352100496,-2.98260003124754,
-2.91609331838607,-2.88373338373485,-2.8692239675763,-2.86683869631314,
-2.86556825167259,-2.86465458301084,-2.86368741516949,-2.86232751883703,
-2.85951819628024,-2.82983250978034,-2.80928534262578,-2.74762095988082,
-2.72413258429119,-2.7079193107732,-2.70601309502644,-2.70454878279257,
-2.70383327423822,-2.70332112551669,-2.70278506082854,-2.70203621458432,
-2.70008318562765,-2.67136002289411,-2.58879484883179,-2.55129231134297,
-2.54517484565672,-2.5433610484862,-2.54224655677649,-2.54123476772663,
-2.53993493394394,-2.53725417524231,-2.52907243441431,-2.52671370613265,
-2.52388209052998,-2.52339295894234,-2.5209792169163,-2.51741852649105,
-2.4345715629149,-2.3841832292528,-2.38189930753702,-2.38104096065967,-2.38045008863287,
-2.37987642844745,-2.3791842871541,-2.37745351298012,-2.36146004118226,
-2.33219007892715,-2.31235187782139,-2.27212882893557,-2.24263988041179,
-2.22351154050838,-2.22098709892768,-2.21971864546848,-2.21880521223288,
-2.21783718462719,-2.21619915865981,-2.21183064819459,-2.2058618658656,
-2.09688310266205,-2.06056329815115,-2.0586677209403,-2.05786957990353,
-2.0572943119063,-2.05676679756776,-2.05605098037175,-2.05465064338855,
-2.04378747323072,-2.0421904443236,-2.04176360829486,-2.04056307446308,
-2.04007259737402,-2.03788385830732,-2.03673449151926,-2.03136324915038,
-2.01007514577286,-1.90535919762152,-1.89910701639322,-1.89721265573857,
-1.89619325713786,-1.89519837114668,-1.89398902825268,-1.89174642253287,
-1.87975764426959,-1.85612378776406,-1.81078635856992,-1.77840572855741,
-1.75067383698808,-1.73713546906084,-1.73550164719207,-1.73481480908172,
-1.73424250003767,-1.73364971557648,-1.73276468552204,-1.73031223694464,
-1.68808944411968,-1.58218257604977,-1.576018733314,-1.57413511759528,-1.57311800875414,
-1.57213365790823,-1.57095013865604,-1.56879308827265,-1.56612741964831,
-1.51587941804059,-1.4514926255499,-1.43579834140671,-1.42815852180856,
-1.42502264431835,-1.41391464536443,-1.41236949675846,-1.41163251925625,
-1.41106556036876,-1.41044937286506,-1.40945785552894,-1.40615495541566,
-1.38561133259827,-1.36992249076833),.UNSPECIFIED.);
#252=B_SPLINE_CURVE_WITH_KNOTS('',3,(#45056,#45057,#45058,#45059,#45060,
#45061,#45062,#45063,#45064,#45065,#45066,#45067,#45068,#45069,#45070,#45071,
#45072,#45073,#45074,#45075,#45076,#45077,#45078,#45079,#45080,#45081,#45082,
#45083,#45084,#45085,#45086,#45087,#45088,#45089,#45090,#45091,#45092,#45093,
#45094,#45095,#45096,#45097,#45098,#45099,#45100,#45101,#45102,#45103,#45104,
#45105,#45106,#45107,#45108,#45109,#45110,#45111,#45112,#45113,#45114,#45115,
#45116,#45117,#45118,#45119,#45120,#45121,#45122,#45123,#45124,#45125,#45126,
#45127,#45128,#45129,#45130,#45131,#45132,#45133,#45134,#45135,#45136,#45137,
#45138,#45139,#45140,#45141,#45142,#45143,#45144,#45145,#45146,#45147,#45148,
#45149,#45150,#45151,#45152,#45153),.UNSPECIFIED.,.F.,.F.,(4,2,2,2,2,2,
2,2,2,2,2,2,2,2,2,2,2,2,2,2,2,2,2,2,2,2,2,2,2,2,2,2,2,2,2,2,2,2,2,2,2,2,
2,2,2,2,2,2,4),(-0.662484546563834,-0.653028498095685,-0.616296305791393,
-0.530572689536388,-0.52585539356106,-0.524790056139435,-0.524095078273972,
-0.523590265262604,-0.522961522669115,-0.521914295862368,-0.518072303520396,
-0.429445501281873,-0.389416394524991,-0.385848483951991,-0.382043981007247,
-0.379961831561385,-0.377784719650975,-0.375951484981409,-0.371982876524711,
-0.3656451265558,-0.363740750107707,-0.362605883695746,-0.361616042869752,
-0.360645537328616,-0.358626092820093,-0.350040855825288,-0.334735425516253,
-0.31016377779759,-0.207094952442866,-0.206424747570049,-0.202563246583696,
-0.201478129244575,-0.200834573400788,-0.200278453904849,-0.199579284473267,
-0.198207774530163,-0.188721050710403,-0.161933511971421,-0.0786882112168834,
-0.0730623105976422,-0.0444561768123828,-0.0413632162909043,-0.0401225427657687,
-0.039092206450294,-0.038145925876914,-0.0371166700067285,-0.0357235945869139,
-0.0334535663773804,-0.000960739771948738),.UNSPECIFIED.);
#253=B_SPLINE_CURVE_WITH_KNOTS('',3,(#45154,#45155,#45156,#45157,#45158,
#45159,#45160,#45161,#45162,#45163,#45164,#45165,#45166,#45167,#45168,#45169,
#45170,#45171,#45172,#45173,#45174,#45175,#45176,#45177,#45178,#45179,#45180,
#45181,#45182,#45183,#45184,#45185,#45186,#45187,#45188,#45189,#45190,#45191,
#45192,#45193,#45194,#45195,#45196,#45197,#45198,#45199,#45200,#45201,#45202,
#45203,#45204,#45205,#45206,#45207,#45208,#45209,#45210,#45211,#45212,#45213,
#45214,#45215,#45216,#45217,#45218,#45219,#45220,#45221,#45222,#45223,#45224,
#45225,#45226,#45227,#45228,#45229,#45230,#45231,#45232,#45233,#45234,#45235,
#45236,#45237,#45238,#45239,#45240,#45241,#45242,#45243,#45244,#45245,#45246,
#45247,#45248,#45249,#45250,#45251,#45252,#45253,#45254,#45255,#45256,#45257,
#45258,#45259,#45260,#45261,#45262,#45263,#45264,#45265,#45266,#45267,#45268,
#45269,#45270,#45271,#45272,#45273,#45274,#45275,#45276,#45277,#45278,#45279,
#45280,#45281,#45282,#45283,#45284,#45285,#45286,#45287,#45288,#45289,#45290,
#45291,#45292,#45293,#45294,#45295,#45296,#45297,#45298,#45299,#45300,#45301,
#45302,#45303,#45304,#45305,#45306,#45307,#45308,#45309,#45310,#45311,#45312,
#45313,#45314,#45315,#45316,#45317,#45318,#45319,#45320,#45321,#45322,#45323,
#45324,#45325,#45326,#45327,#45328,#45329,#45330,#45331,#45332,#45333,#45334,
#45335,#45336,#45337,#45338,#45339,#45340,#45341,#45342,#45343,#45344,#45345,
#45346,#45347,#45348,#45349,#45350,#45351,#45352,#45353,#45354,#45355,#45356,
#45357,#45358,#45359,#45360,#45361,#45362,#45363,#45364,#45365),
 .UNSPECIFIED.,.F.,.F.,(4,2,2,2,2,2,2,2,2,2,2,2,2,2,2,2,2,2,2,2,2,2,2,2,
2,2,2,2,2,2,2,2,2,2,2,2,2,2,2,2,2,2,2,2,2,2,2,2,2,2,2,2,2,2,2,2,2,2,2,2,
2,2,2,2,2,2,2,2,2,2,2,2,2,2,2,2,2,2,2,2,2,2,2,2,2,2,2,2,2,2,2,2,2,2,2,2,
2,2,2,2,2,2,2,2,2,4),(-4.06127014542011,-3.96345360342496,-3.94283348390587,
-3.93952285030901,-3.93853020035635,-3.93791358486381,-3.93734642573133,
-3.93660945330883,-3.93500775257484,-3.92297456255997,-3.91964322838868,
-3.91553485159133,-3.89332821618906,-3.82371342826044,-3.80332568387682,
-3.78837019164686,-3.77993305323193,-3.77792396121982,-3.77695419739667,
-3.77596229970356,-3.77482384076671,-3.77290436873306,-3.76643966492423,
-3.76252733835516,-3.76075659642063,-3.75861228680896,-3.75805872741368,
-3.75596890550248,-3.754513394651,-3.75330689379693,-3.75179249796371,-3.74654907053496,
-3.70546252060252,-3.67647570978518,-3.621584694545,-3.61680442532471,-3.61567611640045,
-3.61502918521708,-3.61446802297562,-3.61377078399619,-3.61269848456357,
-3.60789793005972,-3.5208927820507,-3.48975277665014,-3.46828555572928,
-3.46101937772421,-3.45778043762926,-3.45525407182727,-3.45398962808627,
-3.45301291496556,-3.45204014380962,-3.4503788919813,-3.44586142558242,
-3.37946486463497,-3.34335078923876,-3.31435012516755,-3.30199884003998,
-3.29406530542728,-3.29275426149695,-3.29206772633116,-3.29150722679693,
-3.29085198323463,-3.28971675234639,-3.2853641766045,-3.28489194433908,
-3.18717767572461,-3.15487352585317,-3.14146202439485,-3.13635137493903,
-3.13385646301956,-3.13181366392817,-3.13065513031136,-3.12974977265603,
-3.12873708912742,-3.12687639160503,-3.12090421733095,-3.0222096922247,
-2.97149035506671,-2.9697574436245,-2.96898801170755,-2.96841775426936,
-2.96788310458741,-2.96714002102135,-2.96563200765558,-2.96164652392502,
-2.86405329816224,-2.81726354181658,-2.81267347325761,-2.81036844251205,
-2.80896071799233,-2.80767583868822,-2.80668106832067,-2.8057127240601,
-2.80434905875503,-2.8015250793395,-2.79394275524369,-2.79213031421433,
-2.79006698799704,-2.78959526099725,-2.78776832304441,-2.78486689438122,
-2.78367028196406,-2.78211136428351,-2.77497173158081,-2.70666089636562,
-2.69202105007084),.UNSPECIFIED.);
#254=B_SPLINE_CURVE_WITH_KNOTS('',3,(#45371,#45372,#45373,#45374,#45375,
#45376,#45377,#45378,#45379,#45380,#45381,#45382,#45383,#45384,#45385,#45386,
#45387,#45388,#45389,#45390,#45391,#45392,#45393,#45394,#45395,#45396,#45397,
#45398,#45399,#45400,#45401,#45402,#45403,#45404,#45405,#45406,#45407,#45408,
#45409,#45410,#45411,#45412,#45413,#45414,#45415,#45416,#45417,#45418,#45419,
#45420,#45421,#45422,#45423,#45424,#45425,#45426,#45427,#45428,#45429,#45430,
#45431,#45432,#45433,#45434,#45435,#45436,#45437,#45438,#45439,#45440,#45441,
#45442,#45443,#45444,#45445,#45446,#45447,#45448,#45449,#45450,#45451,#45452,
#45453,#45454,#45455,#45456,#45457,#45458,#45459,#45460,#45461,#45462,#45463,
#45464,#45465,#45466,#45467,#45468,#45469,#45470,#45471,#45472,#45473,#45474,
#45475,#45476,#45477,#45478,#45479,#45480,#45481,#45482,#45483,#45484,#45485,
#45486,#45487,#45488,#45489,#45490,#45491,#45492,#45493,#45494,#45495,#45496,
#45497,#45498,#45499,#45500,#45501,#45502,#45503,#45504,#45505,#45506,#45507,
#45508,#45509,#45510,#45511,#45512,#45513,#45514,#45515,#45516,#45517,#45518,
#45519,#45520,#45521,#45522,#45523,#45524,#45525,#45526,#45527,#45528,#45529,
#45530,#45531,#45532,#45533,#45534,#45535,#45536,#45537,#45538,#45539,#45540,
#45541,#45542,#45543,#45544,#45545,#45546,#45547,#45548,#45549,#45550,#45551,
#45552,#45553,#45554,#45555,#45556,#45557,#45558,#45559,#45560,#45561,#45562,
#45563,#45564,#45565,#45566),.UNSPECIFIED.,.F.,.F.,(4,2,2,2,2,2,2,2,2,2,
2,2,2,2,2,2,2,2,2,2,2,2,2,2,2,2,2,2,2,2,2,2,2,2,2,2,2,2,2,2,2,2,2,2,2,2,
2,2,2,2,2,2,2,2,2,2,2,2,2,2,2,2,2,2,2,2,2,2,2,2,2,2,2,2,2,2,2,2,2,2,2,2,
2,2,2,2,2,2,2,2,2,2,2,2,2,2,2,4),(-1.37006013660576,-1.36813097394664,-1.32932735761755,
-1.25858965367075,-1.23057258816633,-1.2286296907977,-1.22788241632752,
-1.22734671185576,-1.22683424142332,-1.22628381396108,-1.22506538691945,
-1.21891329741473,-1.20664598041326,-1.18447910256005,-1.12913574310777,
-1.07220127763863,-1.06843097000159,-1.06704509530975,-1.06607074681383,
-1.06515933446729,-1.06390617936786,-1.06145644709069,-1.0449600251339,
-1.00540499266253,-0.948642773372128,-0.923369959339648,-0.921576008121546,
-0.921013266749065,-0.907176292643627,-0.905677023241927,-0.904936188773754,
-0.904402198413551,-0.903831706534511,-0.903269252454078,-0.901936509723686,
-0.893379634416647,-0.873530442476435,-0.82285787511113,-0.782778572925608,
-0.769472551448452,-0.747892324998544,-0.745023163405022,-0.743700878407185,
-0.742682511269694,-0.741588650353387,-0.73986813003035,-0.734576219552312,
-0.726427642784752,-0.7019191579815,-0.638150144149182,-0.593104736606286,
-0.592026402197716,-0.590438525618296,-0.587691367670873,-0.583398584783547,
-0.582269252407768,-0.581615414219628,-0.581054885802996,-0.580366775684865,
-0.579631751813795,-0.576372713280065,-0.551120999278779,-0.509290951689597,
-0.428199055692575,-0.426948300765325,-0.422686678420152,-0.421065428990359,
-0.420100607840701,-0.419185764988364,-0.417908260011066,-0.415339804907564,
-0.401805544246659,-0.373160373205551,-0.344796516450849,-0.318729689397913,
-0.2634067526509,-0.260186303972084,-0.259163340098403,-0.258602253954898,
-0.258040943342226,-0.257499355794066,-0.256814437868253,-0.255764953036627,
-0.242117344300038,-0.213585554864005,-0.202494970741812,-0.190429095569164,
-0.105563197169878,-0.10007101334907,-0.0982715601255558,-0.0972712814648368,
-0.0962744536600228,-0.0950325528330217,-0.0926366420268566,-0.0896360550492344,
-0.0830792676873454,-0.064331162693157,-0.000961908199084628),
 .UNSPECIFIED.);
#255=B_SPLINE_CURVE_WITH_KNOTS('',3,(#45567,#45568,#45569,#45570,#45571,
#45572,#45573,#45574,#45575,#45576,#45577,#45578,#45579,#45580,#45581,#45582,
#45583,#45584,#45585,#45586,#45587,#45588,#45589,#45590,#45591,#45592,#45593,
#45594,#45595,#45596,#45597,#45598,#45599,#45600,#45601,#45602,#45603,#45604,
#45605,#45606,#45607,#45608,#45609,#45610,#45611,#45612,#45613,#45614,#45615,
#45616,#45617,#45618,#45619,#45620,#45621,#45622,#45623,#45624,#45625,#45626,
#45627,#45628,#45629,#45630,#45631,#45632,#45633,#45634,#45635,#45636,#45637,
#45638,#45639,#45640,#45641,#45642,#45643,#45644,#45645,#45646,#45647,#45648,
#45649,#45650,#45651,#45652,#45653,#45654,#45655,#45656,#45657,#45658,#45659,
#45660,#45661,#45662,#45663,#45664,#45665,#45666),.UNSPECIFIED.,.F.,.F.,
(4,2,2,2,2,2,2,2,2,2,2,2,2,2,2,2,2,2,2,2,2,2,2,2,2,2,2,2,2,2,2,2,2,2,2,
2,2,2,2,2,2,2,2,2,2,2,2,2,2,4),(-4.06049778996915,-3.99904159918256,-3.99731369694622,
-3.9963500425661,-3.99570114292148,-3.99507440656776,-3.99451040376592,
-3.99378216471943,-3.99226578783663,-3.9822865548596,-3.97986840961498,
-3.9306046388084,-3.92206896077134,-3.91472479405678,-3.89982315449474,
-3.85857816609013,-3.84034738026085,-3.83756243007123,-3.83530728122348,
-3.83409538755797,-3.83318886045351,-3.83219501848855,-3.83042688977888,
-3.82516666684674,-3.74360937424023,-3.72094211655588,-3.6948261901867,
-3.6809871027978,-3.67654913659154,-3.67368182493792,-3.67297483167414,
-3.67230687904806,-3.67180230047736,-3.67123732474311,-3.67019468043799,
-3.66681244995404,-3.61070253090208,-3.5656812649305,-3.55851304448269,
-3.53012041321281,-3.51497189534137,-3.51324871903817,-3.51172019812485,
-3.51066802158057,-3.50963790876059,-3.50839735908715,-3.5053039533476,
-3.47665769918529,-3.42568494445762,-3.39990203970593),.UNSPECIFIED.);
#256=B_SPLINE_CURVE_WITH_KNOTS('',3,(#45667,#45668,#45669,#45670,#45671,
#45672,#45673,#45674,#45675,#45676,#45677,#45678,#45679,#45680,#45681,#45682,
#45683,#45684,#45685,#45686,#45687,#45688,#45689,#45690,#45691,#45692,#45693,
#45694,#45695,#45696,#45697,#45698,#45699,#45700,#45701,#45702,#45703,#45704,
#45705,#45706,#45707,#45708,#45709,#45710,#45711,#45712,#45713,#45714,#45715,
#45716,#45717,#45718,#45719,#45720,#45721,#45722,#45723,#45724,#45725,#45726,
#45727,#45728,#45729,#45730,#45731,#45732,#45733,#45734,#45735,#45736,#45737,
#45738,#45739,#45740,#45741,#45742,#45743,#45744,#45745,#45746,#45747,#45748,
#45749,#45750,#45751,#45752,#45753,#45754,#45755,#45756,#45757,#45758,#45759,
#45760,#45761,#45762,#45763,#45764,#45765,#45766,#45767,#45768,#45769,#45770,
#45771,#45772,#45773,#45774,#45775,#45776,#45777,#45778,#45779,#45780,#45781,
#45782,#45783,#45784,#45785,#45786,#45787,#45788,#45789,#45790,#45791,#45792,
#45793,#45794,#45795,#45796,#45797,#45798,#45799,#45800,#45801,#45802,#45803,
#45804,#45805,#45806,#45807,#45808,#45809,#45810,#45811,#45812,#45813,#45814,
#45815,#45816,#45817,#45818,#45819,#45820,#45821,#45822,#45823,#45824,#45825,
#45826,#45827,#45828,#45829,#45830,#45831,#45832,#45833,#45834,#45835,#45836,
#45837,#45838,#45839,#45840,#45841,#45842,#45843,#45844,#45845,#45846,#45847,
#45848,#45849,#45850,#45851,#45852,#45853,#45854,#45855,#45856,#45857,#45858,
#45859,#45860,#45861,#45862,#45863,#45864,#45865,#45866,#45867,#45868,#45869,
#45870,#45871,#45872,#45873,#45874,#45875,#45876,#45877,#45878,#45879,#45880,
#45881,#45882,#45883,#45884,#45885,#45886,#45887,#45888,#45889,#45890,#45891,
#45892,#45893,#45894,#45895,#45896,#45897,#45898,#45899,#45900,#45901,#45902,
#45903,#45904,#45905,#45906,#45907,#45908,#45909,#45910,#45911,#45912,#45913,
#45914,#45915,#45916,#45917,#45918,#45919,#45920,#45921,#45922,#45923,#45924,
#45925,#45926,#45927,#45928,#45929,#45930,#45931,#45932,#45933,#45934,#45935,
#45936,#45937,#45938,#45939,#45940,#45941,#45942,#45943,#45944,#45945,#45946,
#45947,#45948),.UNSPECIFIED.,.F.,.F.,(4,2,2,2,2,2,2,2,2,2,2,2,2,2,2,2,2,
2,2,2,2,2,2,2,2,2,2,2,2,2,2,2,2,2,2,2,2,2,2,2,2,2,2,2,2,2,2,2,2,2,2,2,2,
2,2,2,2,2,2,2,2,2,2,2,2,2,2,2,2,2,2,2,2,2,2,2,2,2,2,2,2,2,2,2,2,2,2,2,2,
2,2,2,2,2,2,2,2,2,2,2,2,2,2,2,2,2,2,2,2,2,2,2,2,2,2,2,2,2,2,2,2,2,2,2,2,
2,2,2,2,2,2,2,2,2,2,2,2,2,2,2,4),(-2.69202105007084,-2.67637090133286,-2.65637037866237,
-2.64777232613318,-2.64643376474545,-2.64574146514728,-2.64518068180451,
-2.64461493810627,-2.64356905343837,-2.64016175042675,-2.58417962508604,
-2.49236389261529,-2.48873407707181,-2.48679243105214,-2.4855375012887,
-2.48436394594113,-2.48339573593312,-2.48237690288973,-2.48048552825973,
-2.47425903859647,-2.37060199419344,-2.32512857865517,-2.3234053116582,
-2.32263764893346,-2.3220676944243,-2.32153256847504,-2.32078766442116,
-2.31885960261658,-2.29180228064014,-2.26247520627152,-2.21160057356583,
-2.17951306019635,-2.16494208962872,-2.16257706111159,-2.16134147544218,
-2.16043211083388,-2.15944964019619,-2.15773967311286,-2.15289502066276,
-2.07862949008025,-2.03048944366382,-2.0025030824272,-2.00056034096373,
-1.99981299937901,-1.99927720455529,-1.99876461073467,-1.99803262773462,
-1.99649828049752,-1.98013761675789,-1.9603771836387,-1.85813758678381,
-1.84218690862827,-1.83956015703157,-1.83827085419179,-1.8372600867883,
-1.83613937391657,-1.83429877160718,-1.8278014284482,-1.78660207471037,
-1.73982688039598,-1.6815587408051,-1.67793942706893,-1.67686856181613,
-1.67629778421996,-1.67574279109273,-1.67507500176655,-1.6738371268906,
-1.67228700913496,-1.62187513142653,-1.54134795702907,-1.51955535959255,
-1.51667830774077,-1.51535453285432,-1.51433592340918,-1.51324269140768,
-1.51152502210243,-1.50625720071857,-1.47671042021872,-1.43252373522405,
-1.35915993022716,-1.35500585577259,-1.3538902961392,-1.35323964348548,
-1.35267886510016,-1.35200063022764,-1.35071461268247,-1.34909031512334,
-1.30950824919143,-1.25004042332307,-1.19750726677646,-1.19405203127634,
-1.19271667212103,-1.19175591929405,-1.19073733436559,-1.18939113966707,
-1.18647229515132,-1.15796750572267,-1.1340816293789,-1.06800353798191,
-1.05722705358869,-1.04973291550621,-1.0492251916827,-1.04851384707806,
-1.04626003378184,-1.044359600219,-1.03278622751438,-1.03136008722975,-1.03063766358717,
-1.03010845215822,-1.02953454985487,-1.02875979935458,-1.02699350535245,
-1.02458536933109,-1.0185552975402,-0.996419769794486,-0.945406318091502,
-0.87600117345941,-0.87146755725909,-0.869803893627545,-0.868830681569409,
-0.867918793205846,-0.86666258270707,-0.864198434959429,-0.849932637340456,
-0.831667938344258,-0.791538111422328,-0.750258920160955,-0.719205976205605,
-0.717667213459995,-0.716147696271361,-0.713413425993598,-0.709108967610019,
-0.707978475174131,-0.707324358782129,-0.706763833995119,-0.706225584158187,
-0.705132288003572,-0.700761372263859,-0.693046552444917,-0.67402532894375,
-0.6616833794075),.UNSPECIFIED.);
#257=B_SPLINE_CURVE_WITH_KNOTS('',3,(#45953,#45954,#45955,#45956,#45957,
#45958,#45959,#45960,#45961,#45962,#45963,#45964,#45965,#45966,#45967,#45968,
#45969,#45970,#45971,#45972,#45973,#45974,#45975,#45976,#45977,#45978,#45979,
#45980,#45981,#45982,#45983,#45984,#45985,#45986,#45987,#45988,#45989,#45990,
#45991,#45992,#45993,#45994,#45995,#45996,#45997,#45998,#45999,#46000,#46001,
#46002,#46003,#46004,#46005,#46006,#46007,#46008,#46009,#46010,#46011,#46012,
#46013,#46014,#46015,#46016,#46017,#46018,#46019,#46020,#46021,#46022,#46023,
#46024,#46025,#46026,#46027,#46028,#46029,#46030,#46031,#46032,#46033,#46034,
#46035,#46036,#46037,#46038,#46039,#46040,#46041,#46042,#46043,#46044,#46045,
#46046,#46047,#46048,#46049,#46050,#46051,#46052,#46053,#46054,#46055,#46056,
#46057,#46058,#46059,#46060,#46061,#46062,#46063,#46064,#46065,#46066,#46067,
#46068,#46069,#46070,#46071,#46072,#46073,#46074,#46075,#46076,#46077,#46078,
#46079,#46080,#46081,#46082,#46083,#46084,#46085,#46086,#46087,#46088,#46089,
#46090,#46091,#46092,#46093,#46094,#46095,#46096,#46097,#46098,#46099,#46100,
#46101,#46102,#46103,#46104,#46105,#46106,#46107,#46108,#46109,#46110,#46111,
#46112,#46113,#46114,#46115,#46116,#46117,#46118,#46119,#46120,#46121,#46122,
#46123,#46124,#46125,#46126,#46127,#46128,#46129,#46130,#46131,#46132,#46133,
#46134,#46135,#46136,#46137,#46138,#46139,#46140,#46141,#46142,#46143,#46144,
#46145,#46146,#46147,#46148,#46149,#46150,#46151,#46152,#46153,#46154,#46155,
#46156,#46157,#46158,#46159,#46160,#46161,#46162,#46163,#46164,#46165,#46166,
#46167,#46168,#46169,#46170,#46171,#46172,#46173,#46174,#46175,#46176,#46177,
#46178,#46179,#46180,#46181,#46182,#46183,#46184,#46185,#46186,#46187,#46188,
#46189,#46190,#46191,#46192,#46193,#46194,#46195,#46196,#46197,#46198,#46199,
#46200,#46201,#46202,#46203,#46204,#46205,#46206,#46207,#46208,#46209,#46210,
#46211,#46212,#46213,#46214,#46215,#46216,#46217,#46218,#46219,#46220,#46221,
#46222,#46223,#46224,#46225,#46226,#46227,#46228,#46229,#46230,#46231,#46232,
#46233,#46234,#46235,#46236,#46237,#46238,#46239,#46240,#46241,#46242,#46243,
#46244,#46245,#46246,#46247,#46248,#46249,#46250),.UNSPECIFIED.,.F.,.F.,
(4,2,2,2,2,2,2,2,2,2,2,2,2,2,2,2,2,2,2,2,2,2,2,2,2,2,2,2,2,2,2,2,2,2,2,
2,2,2,2,2,2,2,2,2,2,2,2,2,2,2,2,2,2,2,2,2,2,2,2,2,2,2,2,2,2,2,2,2,2,2,2,
2,2,2,2,2,2,2,2,2,2,2,2,2,2,2,2,2,2,2,2,2,2,2,2,2,2,2,2,2,2,2,2,2,2,2,2,
2,2,2,2,2,2,2,2,2,2,2,2,2,2,2,2,2,2,2,2,2,2,2,2,2,2,2,2,2,2,2,2,2,2,2,2,
2,2,2,2,2,4),(-3.40012302419576,-3.37861334262547,-3.34579899185165,-3.33610177007071,
-3.33004195076119,-3.32871108386029,-3.32746487717585,-3.32655447371831,
-3.32557735840309,-3.32418108479873,-3.32034250606838,-3.26146241461163,
-3.22320876765789,-3.19078378981384,-3.17513349868171,-3.16771973785196,
-3.16639615940618,-3.16570143700626,-3.16519434472901,-3.16464420346138,
-3.16367528205086,-3.16085796620878,-3.11308161352822,-3.05477603609166,
-3.03415185758079,-3.00895599202059,-3.00611480359512,-3.00476870275954,
-3.00375033480509,-3.00278989370851,-3.0014551386442,-2.99800240725392,
-2.94565709566628,-2.88854784681887,-2.86805022209868,-2.85231307014278,
-2.84483303039476,-2.84350668033969,-2.84281136630035,-2.8423041998841,
-2.84175433096262,-2.84078678305751,-2.83797917564052,-2.83528322908094,
-2.83312817911436,-2.83202818388997,-2.83026317398034,-2.79929098781733,
-2.72323024410347,-2.68983907210442,-2.68414918219515,-2.68238221026046,
-2.68127815831811,-2.68026349465707,-2.67896433999295,-2.67684162955999,
-2.66833575876634,-2.66627108514545,-2.66326697862997,-2.66275479712366,
-2.66065798419631,-2.65924868955021,-2.65804177490019,-2.65670792233358,
-2.65103544889531,-2.57662863793531,-2.52440097262526,-2.52123326133197,
-2.52025949593115,-2.51964277934739,-2.51907591266816,-2.51833984913381,
-2.51674219396669,-2.50480547905618,-2.50258112562136,-2.49958903003775,
-2.49828230529027,-2.49563047774737,-2.40971579781369,-2.37697100434725,
-2.36226105715761,-2.35989798772356,-2.35865299156287,-2.35765604384067,
-2.35651123194105,-2.35456207155334,-2.34783107068032,-2.24601113967426,
-2.19934920865369,-2.1976237774855,-2.19685581049498,-2.19628589478337,
-2.19575100514431,-2.19500673503428,-2.19308198898683,-2.16621472459157,
-2.0765055780489,-2.05171264319719,-2.03893917846921,-2.03665648112952,
-2.03543859090952,-2.03443397522464,-2.03326480631814,-2.03125990607609,
-2.02262118832324,-1.93087174442665,-1.88513055578382,-1.88384468416953,
-1.88234125631277,-1.8795674442905,-1.87529898367295,-1.87417209604471,
-1.87351885482268,-1.87295833295722,-1.87226959712096,-1.87094779146292,
-1.86275879724286,-1.84578604323859,-1.82120768036863,-1.72149480130843,
-1.71510902070917,-1.71319908548693,-1.71206300391871,-1.71115603126582,
-1.70994034851928,-1.70766789306571,-1.69533672190733,-1.67096468076081,
-1.58840793056682,-1.57713687452599,-1.55340688833401,-1.55153587690203,
-1.55080067290155,-1.55026819298299,-1.54969680319072,-1.54893565986218,
-1.54723524242552,-1.54494219917007,-1.52272075775901,-1.48347283921691,
-1.45229438530185,-1.39518153748121,-1.39139941994582,-1.39001175284679,
-1.38903694143529,-1.38812573059702,-1.38687383870859,-1.38443002320154,
-1.37006013660576),.UNSPECIFIED.);
#258=B_SPLINE_CURVE_WITH_KNOTS('',3,(#46252,#46253,#46254,#46255,#46256,
#46257,#46258,#46259,#46260,#46261,#46262,#46263,#46264,#46265,#46266,#46267,
#46268,#46269,#46270,#46271,#46272,#46273,#46274,#46275,#46276,#46277,#46278,
#46279,#46280,#46281,#46282,#46283,#46284,#46285,#46286,#46287,#46288,#46289,
#46290,#46291,#46292,#46293,#46294,#46295,#46296,#46297,#46298,#46299,#46300,
#46301,#46302,#46303,#46304,#46305,#46306,#46307,#46308,#46309,#46310,#46311,
#46312,#46313,#46314,#46315,#46316,#46317,#46318,#46319,#46320,#46321,#46322,
#46323,#46324,#46325,#46326,#46327,#46328,#46329,#46330,#46331,#46332,#46333,
#46334,#46335,#46336,#46337,#46338,#46339,#46340,#46341,#46342,#46343,#46344,
#46345,#46346,#46347,#46348,#46349,#46350,#46351,#46352,#46353,#46354,#46355,
#46356,#46357,#46358,#46359,#46360,#46361,#46362,#46363,#46364,#46365),
 .UNSPECIFIED.,.F.,.F.,(4,2,2,2,2,2,2,2,2,2,2,2,2,2,2,2,2,2,2,2,2,2,2,2,
2,2,2,2,2,2,2,2,2,2,2,2,2,2,2,2,2,2,2,2,2,2,2,2,2,2,2,2,2,2,2,2,4),(-0.6616833794075,
-0.633519355641761,-0.553700338753454,-0.548654798757302,-0.546915998544686,
-0.545927856781506,-0.545019944085586,-0.543796394971753,-0.541487706829025,
-0.528435400209994,-0.496753872514348,-0.488959980766652,-0.440615735169355,
-0.39615433077254,-0.394753254177924,-0.393185845516869,-0.390632909549094,
-0.389668267567501,-0.386011451872719,-0.384936331763941,-0.384364718594659,
-0.383809812505389,-0.383273501548794,-0.382607035395432,-0.380239967606707,
-0.376766082641168,-0.366833410867302,-0.33969611399129,-0.317592235843124,
-0.286335335341935,-0.229126154888774,-0.225338024910644,-0.223949348797695,
-0.222974202204585,-0.222062975147677,-0.220811522225008,-0.218370173106285,
-0.203298971359929,-0.154582171133134,-0.137981420406505,-0.129808968100797,
-0.120663247761598,-0.0831107177687953,-0.0819792174880646,-0.0808112520371773,
-0.0786142737099887,-0.0781351865346779,-0.076049215856738,-0.0640002776834103,
-0.0623982044538862,-0.0616612422995186,-0.0610941687298086,-0.0604777258993715,
-0.05984370999712,-0.0589160478804281,-0.0572784915626611,-0.000961098116046245),
 .UNSPECIFIED.);
#259=B_SPLINE_CURVE_WITH_KNOTS('',3,(#46366,#46367,#46368,#46369,#46370,
#46371,#46372,#46373,#46374,#46375,#46376,#46377,#46378,#46379,#46380,#46381,
#46382,#46383,#46384,#46385,#46386,#46387,#46388,#46389,#46390,#46391,#46392,
#46393,#46394,#46395,#46396,#46397,#46398,#46399,#46400,#46401,#46402,#46403,
#46404,#46405,#46406,#46407,#46408,#46409,#46410,#46411,#46412,#46413,#46414,
#46415,#46416,#46417,#46418,#46419,#46420,#46421,#46422,#46423,#46424,#46425,
#46426,#46427,#46428,#46429,#46430,#46431,#46432,#46433,#46434,#46435,#46436,
#46437,#46438,#46439,#46440,#46441,#46442,#46443,#46444,#46445,#46446,#46447,
#46448,#46449,#46450,#46451,#46452,#46453,#46454,#46455,#46456,#46457,#46458,
#46459,#46460,#46461,#46462,#46463,#46464,#46465,#46466,#46467,#46468,#46469,
#46470,#46471,#46472,#46473,#46474,#46475,#46476,#46477,#46478,#46479,#46480,
#46481,#46482,#46483,#46484,#46485,#46486,#46487,#46488,#46489,#46490,#46491,
#46492,#46493,#46494,#46495,#46496,#46497,#46498,#46499,#46500,#46501,#46502,
#46503,#46504,#46505,#46506,#46507,#46508,#46509,#46510,#46511,#46512,#46513,
#46514,#46515,#46516,#46517,#46518,#46519,#46520,#46521,#46522,#46523,#46524,
#46525,#46526,#46527,#46528,#46529,#46530,#46531,#46532,#46533,#46534,#46535,
#46536,#46537,#46538,#46539,#46540,#46541,#46542,#46543,#46544,#46545,#46546,
#46547,#46548,#46549,#46550,#46551,#46552,#46553,#46554,#46555,#46556,#46557,
#46558,#46559,#46560,#46561,#46562,#46563,#46564,#46565,#46566,#46567,#46568,
#46569,#46570,#46571,#46572,#46573),.UNSPECIFIED.,.F.,.F.,(4,2,2,2,2,2,
2,2,2,2,2,2,2,2,2,2,2,2,2,2,2,2,2,2,2,2,2,2,2,2,2,2,2,2,2,2,2,2,2,2,2,2,
2,2,2,2,2,2,2,2,2,2,2,2,2,2,2,2,2,2,2,2,2,2,2,2,2,2,2,2,2,2,2,2,2,2,2,2,
2,2,2,2,2,2,2,2,2,2,2,2,2,2,2,2,2,2,2,2,2,2,2,2,2,4),(-4.06158273434959,
-3.97420622812104,-3.96761257703122,-3.96459963285439,-3.96219581524972,
-3.96095248705518,-3.95994658566313,-3.95894516826372,-3.9571390927473,
-3.95159394576926,-3.86025076436609,-3.83856009378895,-3.80404285256712,
-3.80058164618932,-3.79983338456754,-3.79927056717153,-3.79869995771594,
-3.79816656668134,-3.79742763591341,-3.79593557459257,-3.7823309133433,
-3.78117891838724,-3.776240538024,-3.77317095138678,-3.74396438168119,-3.71771267133179,
-3.69067255668897,-3.65672368201556,-3.64170630826169,-3.63931231914721,
-3.63807096085153,-3.63707434586623,-3.63607409245784,-3.63427416910932,
-3.62877685704939,-3.54375756011914,-3.50416247952578,-3.47999253353542,
-3.47747584937258,-3.47679695223411,-3.47625721178888,-3.47575022767063,
-3.47519969300442,-3.47422878012438,-3.47139846478066,-3.42645777395488,
-3.37725738439123,-3.3358629998132,-3.32465482137048,-3.31787933940221,
-3.31599760187107,-3.31486784211023,-3.31385910059109,-3.31258617973585,
-3.31059517296258,-3.30240069342843,-3.29959029770863,-3.29860212401218,
-3.29815449599997,-3.29695289162195,-3.29486139561577,-3.29299577315764,
-3.29037522239285,-3.28212478639441,-3.23009736128573,-3.17871522451368,
-3.16294943826784,-3.15794390128001,-3.15479704971341,-3.15382429265853,
-3.15320781532365,-3.15264089246671,-3.15190437683198,-3.15030425577346,
-3.13830171993643,-3.13605070114259,-3.12848599246595,-3.1128587367408,
-3.05103229435915,-3.01229485671835,-2.99601000142188,-2.99356819195577,
-2.99231679785426,-2.99140573310728,-2.99043087349067,-2.98904279419967,
-2.98525745091578,-2.92440760089031,-2.83548121806865,-2.83310632575522,
-2.8313634762985,-2.83059091875818,-2.83001746616947,-2.82948782178933,
-2.82876356343905,-2.82733005470431,-2.81554215353034,-2.81471769752239,
-2.81421692335681,-2.81093890670191,-2.80845585143538,-2.79794857969055,
-2.71276901798617,-2.69260920664919),.UNSPECIFIED.);
#260=B_SPLINE_CURVE_WITH_KNOTS('',3,(#46579,#46580,#46581,#46582,#46583,
#46584,#46585,#46586,#46587,#46588,#46589,#46590,#46591,#46592,#46593,#46594,
#46595,#46596,#46597,#46598,#46599,#46600,#46601,#46602,#46603,#46604,#46605,
#46606,#46607,#46608,#46609,#46610,#46611,#46612,#46613,#46614,#46615,#46616,
#46617,#46618,#46619,#46620,#46621,#46622,#46623,#46624,#46625,#46626,#46627,
#46628,#46629,#46630,#46631,#46632,#46633,#46634,#46635,#46636,#46637,#46638,
#46639,#46640,#46641,#46642,#46643,#46644,#46645,#46646,#46647,#46648,#46649,
#46650,#46651,#46652,#46653,#46654,#46655,#46656,#46657,#46658,#46659,#46660,
#46661,#46662,#46663,#46664,#46665,#46666,#46667,#46668,#46669,#46670,#46671,
#46672,#46673,#46674,#46675,#46676,#46677,#46678,#46679,#46680,#46681,#46682,
#46683,#46684,#46685,#46686,#46687,#46688,#46689,#46690,#46691,#46692,#46693,
#46694,#46695,#46696,#46697,#46698,#46699,#46700,#46701,#46702,#46703,#46704,
#46705,#46706,#46707,#46708,#46709,#46710,#46711,#46712,#46713,#46714,#46715,
#46716,#46717,#46718,#46719,#46720),.UNSPECIFIED.,.F.,.F.,(4,3,3,3,3,3,
3,3,3,3,3,3,3,3,3,3,3,3,3,3,3,3,3,3,3,3,3,3,3,3,3,3,3,3,3,3,3,3,3,3,3,3,
3,3,3,3,3,4),(442.964564156161,443.090567200826,443.190607880541,443.283680824817,
443.376627664454,443.469476035639,443.562256540294,443.65500186245,443.747736827552,
443.840486245893,443.933334886628,444.026235327239,444.119291223324,444.190322536014,
444.28339548029,444.376342319927,444.469190691112,444.561971195768,444.654716517924,
444.747451483025,444.840200901366,444.933049542101,445.025949982713,445.119005878797,
445.190037191487,445.283110135763,445.3760569754,445.468905346585,445.56168585124,
445.654431173396,445.747166138497,445.839915556838,445.932764197574,446.025664638185,
446.118720534269,446.18975184696,446.282824791236,446.375771630873,446.468620002057,
446.561400506713,446.654145828869,446.74688079397,446.839630212311,446.932478853046,
447.025379293658,447.118435189742,447.189466502432,447.201562196418),
 .UNSPECIFIED.);
#261=B_SPLINE_CURVE_WITH_KNOTS('',3,(#46721,#46722,#46723,#46724,#46725,
#46726,#46727,#46728,#46729,#46730,#46731,#46732,#46733,#46734,#46735,#46736,
#46737,#46738,#46739,#46740,#46741,#46742,#46743,#46744,#46745,#46746,#46747,
#46748,#46749,#46750,#46751,#46752,#46753,#46754,#46755,#46756,#46757,#46758,
#46759,#46760,#46761,#46762,#46763,#46764,#46765,#46766,#46767,#46768,#46769,
#46770,#46771,#46772,#46773,#46774,#46775,#46776,#46777,#46778,#46779,#46780,
#46781,#46782,#46783,#46784,#46785,#46786,#46787,#46788,#46789,#46790,#46791,
#46792,#46793,#46794,#46795,#46796,#46797,#46798,#46799,#46800,#46801,#46802,
#46803,#46804,#46805,#46806,#46807,#46808,#46809,#46810,#46811,#46812),
 .UNSPECIFIED.,.F.,.F.,(4,2,2,2,2,2,2,2,2,2,2,2,2,2,2,2,2,2,2,2,2,2,2,2,
2,2,2,2,2,2,2,2,2,2,2,2,2,2,2,2,2,2,2,2,2,4),(-4.06137741686604,-3.99244122652865,
-3.97783305728595,-3.97576200001466,-3.97445258916643,-3.97322188765454,
-3.97231337392283,-3.97132916066007,-3.96960925355752,-3.96469234100141,
-3.88543273855108,-3.87230650744425,-3.85982632668212,-3.82739462143055,
-3.81374768679741,-3.8126935780148,-3.81200676306689,-3.81135321091697,
-3.81084922261485,-3.81027390667018,-3.8091800117638,-3.80535417760358,
-3.74350391913571,-3.716221641308,-3.68217997260114,-3.66349339697952,-3.65351999156419,
-3.65198792907096,-3.65059635891916,-3.64957051608242,-3.64862223466532,
-3.64733410810473,-3.64415627562183,-3.60945297852893,-3.56635458729749,
-3.52084856892669,-3.49327576726163,-3.48999748318605,-3.48926125500055,
-3.48857231955999,-3.48801186084446,-3.48744438482214,-3.48638946126764,
-3.48290528090794,-3.42650123911179,-3.40012302419576),.UNSPECIFIED.);
#262=B_SPLINE_CURVE_WITH_KNOTS('',3,(#46813,#46814,#46815,#46816,#46817,
#46818,#46819,#46820,#46821,#46822,#46823,#46824,#46825,#46826,#46827,#46828,
#46829,#46830,#46831,#46832,#46833,#46834,#46835,#46836,#46837,#46838,#46839,
#46840,#46841,#46842,#46843,#46844,#46845,#46846,#46847,#46848,#46849,#46850,
#46851,#46852,#46853,#46854,#46855,#46856,#46857,#46858,#46859,#46860,#46861,
#46862,#46863,#46864,#46865,#46866,#46867,#46868,#46869,#46870,#46871,#46872,
#46873,#46874,#46875,#46876,#46877,#46878,#46879,#46880,#46881,#46882,#46883,
#46884,#46885,#46886,#46887,#46888,#46889,#46890,#46891,#46892,#46893,#46894,
#46895,#46896,#46897,#46898,#46899,#46900,#46901,#46902,#46903,#46904,#46905,
#46906,#46907,#46908,#46909,#46910,#46911,#46912,#46913,#46914,#46915,#46916,
#46917,#46918,#46919,#46920,#46921,#46922,#46923,#46924,#46925,#46926,#46927,
#46928,#46929,#46930,#46931,#46932,#46933,#46934,#46935,#46936,#46937,#46938,
#46939,#46940,#46941,#46942,#46943,#46944,#46945,#46946,#46947,#46948,#46949,
#46950,#46951,#46952,#46953,#46954,#46955,#46956,#46957,#46958,#46959,#46960,
#46961,#46962,#46963,#46964,#46965,#46966,#46967,#46968,#46969,#46970,#46971,
#46972,#46973,#46974,#46975,#46976,#46977,#46978,#46979,#46980,#46981,#46982,
#46983,#46984,#46985,#46986,#46987,#46988,#46989,#46990,#46991,#46992,#46993,
#46994,#46995,#46996,#46997,#46998,#46999,#47000,#47001,#47002,#47003,#47004,
#47005,#47006,#47007,#47008,#47009,#47010,#47011,#47012,#47013,#47014,#47015,
#47016,#47017,#47018,#47019,#47020,#47021,#47022,#47023,#47024,#47025,#47026,
#47027,#47028,#47029,#47030,#47031,#47032,#47033,#47034,#47035,#47036,#47037,
#47038,#47039,#47040,#47041,#47042,#47043,#47044,#47045,#47046,#47047,#47048,
#47049,#47050,#47051,#47052,#47053,#47054,#47055,#47056,#47057,#47058,#47059,
#47060,#47061,#47062,#47063,#47064,#47065,#47066,#47067,#47068,#47069,#47070,
#47071,#47072,#47073,#47074,#47075,#47076,#47077,#47078,#47079,#47080,#47081,
#47082,#47083,#47084,#47085,#47086,#47087,#47088,#47089,#47090,#47091,#47092,
#47093,#47094,#47095,#47096,#47097,#47098,#47099,#47100,#47101,#47102,#47103,
#47104,#47105,#47106,#47107,#47108,#47109,#47110,#47111,#47112,#47113,#47114,
#47115,#47116,#47117,#47118,#47119,#47120,#47121,#47122,#47123,#47124,#47125,
#47126,#47127,#47128),.UNSPECIFIED.,.F.,.F.,(4,2,2,2,2,2,2,2,2,2,2,2,2,
2,2,2,2,2,2,2,2,2,2,2,2,2,2,2,2,2,2,2,2,2,2,2,2,2,2,2,2,2,2,2,2,2,2,2,2,
2,2,2,2,2,2,2,2,2,2,2,2,2,2,2,2,2,2,2,2,2,2,2,2,2,2,2,2,2,2,2,2,2,2,2,2,
2,2,2,2,2,2,2,2,2,2,2,2,2,2,2,2,2,2,2,2,2,2,2,2,2,2,2,2,2,2,2,2,2,2,2,2,
2,2,2,2,2,2,2,2,2,2,2,2,2,2,2,2,2,2,2,2,2,2,2,2,2,2,2,2,2,2,2,2,2,2,2,2,
4),(-2.69260920664919,-2.67763674653355,-2.67176324183407,-2.66997502699727,
-2.66886614602402,-2.66785270904156,-2.66656286434162,-2.66447142094702,
-2.65591514778885,-2.65384153972032,-2.65179951033141,-2.65117928142298,
-2.65041421580929,-2.64834048870591,-2.64676862082328,-2.64556437200839,
-2.64420939283802,-2.63871008129024,-2.62159890845879,-2.55268304811074,
-2.52875760229896,-2.51171616816116,-2.50878175250194,-2.50791027689039,
-2.50728250291302,-2.50671856254485,-2.50599176596797,-2.50448323569302,
-2.49468099198248,-2.49208949919983,-2.49105599491558,-2.48816679722052,
-2.4868950361405,-2.48462555139554,-2.40391644403388,-2.36602626955723,
-2.34994754262373,-2.34752357938152,-2.34627585393287,-2.34527858710773,
-2.3441354717486,-2.34219422737738,-2.33553506620722,-2.33172097424639,
-2.33004648135274,-2.32946397507851,-2.32802917588539,-2.3267349511877,
-2.23169726048984,-2.20970923576285,-2.18910300373577,-2.1857939642572,
-2.18480160446349,-2.18418512568023,-2.18361806169099,-2.18288117091588,
-2.18127948300773,-2.16924111125431,-2.16702118317221,-2.16562836640768,
-2.16451530608415,-2.162084280249,-2.16037042977011,-2.06564724714904,-2.03143318959107,
-2.02574908723052,-2.02392471087765,-2.02291943261526,-2.02191372626778,
-2.02067666652283,-2.01830369855196,-2.00353072834094,-1.97060579635047,
-1.86733016050763,-1.86677787999703,-1.86282896011432,-1.86173452183488,
-1.86108877483065,-1.86052752276194,-1.85982873809891,-1.85845914701179,
-1.84902827089104,-1.82459313315582,-1.72268973052317,-1.70409025305998,
-1.70134082942828,-1.70004139605516,-1.69902653009182,-1.69792227372657,
-1.69619032962716,-1.69064997161795,-1.65864456829686,-1.58099763669536,
-1.55000953999101,-1.54808380998953,-1.54021297382923,-1.53882048656305,
-1.53810752529616,-1.53754507165666,-1.53690901942732,-1.53585098150237,
-1.53213332945732,-1.44333173079549,-1.38260938618233,-1.37882414239492,
-1.37743596941246,-1.37646100284262,-1.37554980619682,-1.37429818105601,
-1.37190457230173,-1.3573768709386,-1.3251376969961,-1.25832144221263,-1.22800523221603,
-1.21737476605993,-1.21598337572553,-1.21526989229473,-1.21474300223839,
-1.21416728940651,-1.21336654376172,-1.21151792008218,-1.18917973712711,
-1.16782054189269,-1.10817219810253,-1.08575624444076,-1.07724835809942,
-1.07394024981145,-1.05790520569507,-1.05527430194043,-1.05398420173171,
-1.05297337895456,-1.05185318951687,-1.05005152804996,-1.04390313422098,
-1.03401720716491,-1.00010448362752,-0.946998185270369,-0.911513168698875,
-0.910605883831881,-0.894756765868944,-0.893029901550993,-0.892338332840257,
-0.891764757081677,-0.891173549966945,-0.890296095326423,-0.88795936487484,
-0.829349700561649,-0.790619811328917,-0.736408991355979,-0.7328812553212,
-0.731534035486197,-0.730570157917393,-0.729654904793902,-0.728374727961411,
-0.725844741972436,-0.706222593187417,-0.675377349731977,-0.662344877873636),
 .UNSPECIFIED.);
#263=B_SPLINE_CURVE_WITH_KNOTS('',3,(#47134,#47135,#47136,#47137,#47138,
#47139,#47140,#47141),.UNSPECIFIED.,.F.,.F.,(4,1,1,1,1,4),(449.247756666875,
450.188610468851,451.188325124324,452.188039779797,453.187754435269,453.485536920593),
 .UNSPECIFIED.);
#264=B_SPLINE_CURVE_WITH_KNOTS('',3,(#47142,#47143,#47144,#47145,#47146,
#47147,#47148,#47149,#47150,#47151,#47152,#47153,#47154,#47155,#47156,#47157,
#47158,#47159,#47160,#47161,#47162,#47163,#47164,#47165,#47166,#47167,#47168,
#47169,#47170,#47171,#47172,#47173,#47174,#47175,#47176,#47177,#47178,#47179,
#47180,#47181,#47182,#47183,#47184,#47185,#47186,#47187,#47188,#47189,#47190,
#47191,#47192,#47193,#47194,#47195,#47196,#47197,#47198,#47199,#47200,#47201,
#47202,#47203,#47204,#47205,#47206,#47207,#47208,#47209,#47210,#47211),
 .UNSPECIFIED.,.F.,.F.,(4,3,3,3,3,3,3,3,3,3,3,3,3,3,3,3,3,3,3,3,3,3,3,4),
(447.201562196418,447.294617197158,447.387549689525,447.480387294148,447.573161825754,
447.665904400597,447.75863984103,447.851392956841,447.94424706055,448.03715586022,
448.130216493826,448.189181157905,448.282254102181,448.375200941818,448.468049313003,
448.560829817658,448.653575139815,448.746310104916,448.839059523257,448.931908163992,
449.024808604604,449.117864500688,449.188895813378,449.247749463341),
 .UNSPECIFIED.);
#265=B_SPLINE_CURVE_WITH_KNOTS('',3,(#47213,#47214,#47215,#47216,#47217,
#47218,#47219,#47220,#47221,#47222,#47223,#47224,#47225,#47226,#47227,#47228,
#47229,#47230,#47231,#47232,#47233,#47234,#47235,#47236,#47237,#47238,#47239,
#47240,#47241,#47242,#47243,#47244,#47245,#47246,#47247,#47248,#47249,#47250,
#47251,#47252,#47253,#47254,#47255,#47256,#47257,#47258,#47259,#47260,#47261,
#47262,#47263,#47264,#47265,#47266,#47267,#47268,#47269,#47270,#47271,#47272,
#47273,#47274,#47275,#47276,#47277,#47278,#47279,#47280,#47281,#47282,#47283,
#47284,#47285,#47286,#47287,#47288,#47289,#47290,#47291,#47292,#47293,#47294,
#47295,#47296,#47297,#47298,#47299,#47300,#47301,#47302,#47303,#47304,#47305,
#47306,#47307,#47308,#47309,#47310),.UNSPECIFIED.,.F.,.F.,(4,2,2,2,2,2,
2,2,2,2,2,2,2,2,2,2,2,2,2,2,2,2,2,2,2,2,2,2,2,2,2,2,2,2,2,2,2,2,2,2,2,2,
2,2,2,2,2,2,4),(-0.662344877873636,-0.634147804424907,-0.580833096738116,
-0.579501825629761,-0.57793739142578,-0.575409913535667,-0.574376360467817,
-0.57075434030301,-0.569683207783907,-0.569112400137223,-0.568557448608283,
-0.567876046496436,-0.567150355838213,-0.564025633865396,-0.534619709700243,
-0.48611105310166,-0.414665807901001,-0.411359875691538,-0.409358109351963,
-0.408081752476541,-0.407072501748034,-0.40594448752745,-0.404778786662001,
-0.403049163865885,-0.386425478526341,-0.346370971119457,-0.318766618052582,
-0.251801668323609,-0.247851111192788,-0.246756581152906,-0.246110859141434,
-0.245549679194623,-0.244851049071112,-0.244101387738018,-0.242897603552263,
-0.22898075842022,-0.194229241459736,-0.180761196698222,-0.166723996205132,
-0.0922711416211886,-0.0874323107877999,-0.085723351157587,-0.084741187830486,
-0.0838319376635584,-0.0825962488813401,-0.0812799986883665,-0.0791929123388455,
-0.0646429522359529,-0.0009614827507557),.UNSPECIFIED.);
#266=B_SPLINE_CURVE_WITH_KNOTS('',3,(#47311,#47312,#47313,#47314,#47315,
#47316,#47317,#47318,#47319,#47320,#47321,#47322,#47323,#47324,#47325,#47326,
#47327,#47328,#47329,#47330,#47331,#47332,#47333,#47334,#47335,#47336,#47337,
#47338,#47339,#47340,#47341,#47342,#47343,#47344,#47345,#47346,#47347,#47348,
#47349,#47350,#47351,#47352,#47353,#47354,#47355,#47356,#47357,#47358,#47359,
#47360,#47361,#47362,#47363,#47364,#47365,#47366,#47367,#47368,#47369,#47370,
#47371,#47372,#47373,#47374,#47375,#47376,#47377,#47378,#47379,#47380,#47381,
#47382,#47383,#47384,#47385,#47386,#47387,#47388,#47389,#47390,#47391,#47392,
#47393,#47394,#47395,#47396,#47397,#47398,#47399,#47400,#47401,#47402,#47403,
#47404,#47405,#47406,#47407,#47408,#47409,#47410,#47411,#47412,#47413,#47414,
#47415,#47416,#47417,#47418,#47419,#47420,#47421,#47422,#47423,#47424,#47425,
#47426,#47427,#47428,#47429,#47430,#47431,#47432,#47433,#47434,#47435,#47436,
#47437,#47438,#47439,#47440,#47441,#47442,#47443,#47444,#47445,#47446,#47447,
#47448,#47449,#47450,#47451,#47452,#47453,#47454,#47455,#47456,#47457,#47458,
#47459,#47460,#47461,#47462,#47463,#47464,#47465,#47466,#47467,#47468,#47469,
#47470,#47471,#47472,#47473,#47474,#47475,#47476,#47477,#47478,#47479,#47480,
#47481,#47482,#47483,#47484,#47485,#47486,#47487,#47488,#47489,#47490,#47491,
#47492,#47493,#47494,#47495,#47496,#47497,#47498,#47499,#47500,#47501,#47502,
#47503,#47504,#47505,#47506),.UNSPECIFIED.,.F.,.F.,(4,2,2,2,2,2,2,2,2,2,
2,2,2,2,2,2,2,2,2,2,2,2,2,2,2,2,2,2,2,2,2,2,2,2,2,2,2,2,2,2,2,2,2,2,2,2,
2,2,2,2,2,2,2,2,2,2,2,2,2,2,2,2,2,2,2,2,2,2,2,2,2,2,2,2,2,2,2,2,2,2,2,2,
2,2,2,2,2,2,2,2,2,2,2,2,2,2,2,4),(-4.06034582511648,-3.99445104399732,-3.9852077296334,
-3.98403038375232,-3.98329179980511,-3.98260114528172,-3.9820405063354,
-3.98138876972932,-3.98026839366226,-3.97606571068478,-3.90531020465583,
-3.89193171359876,-3.87882062793399,-3.84018575303294,-3.82511646498073,
-3.82341085472919,-3.82225519304645,-3.82113421344775,-3.82012358057946,
-3.8188349654214,-3.81621140624214,-3.80032149281129,-3.79913113519368,
-3.79791814480669,-3.7965260135535,-3.79042953041537,-3.74282049438889,
-3.71746008945393,-3.69060442945423,-3.67037832085652,-3.66465286922078,
-3.66116367131339,-3.66041322675799,-3.65971404865467,-3.65915285791271,
-3.65850760070165,-3.65741496289121,-3.65348196872246,-3.58638920721675,
-3.53832647296154,-3.50731664735932,-3.50114898008441,-3.49981117853225,
-3.49855992756465,-3.49764878688548,-3.49667367546273,-3.49528495217581,
-3.49149610080983,-3.42982922814949,-3.3947579156103,-3.36142725529963,
-3.34660045227513,-3.34141186054972,-3.33817611134175,-3.33744254027057,
-3.33675549489367,-3.33619506909819,-3.33562632917131,-3.33456534674392,
-3.33103043557557,-3.27352017837254,-3.2247167536341,-3.19766910855078,
-3.17945186096262,-3.17696967049981,-3.17569614944256,-3.17478192134963,
-3.17381568673515,-3.17245958834097,-3.16887623835524,-3.11411314341179,
-3.05930644977589,-3.03868505862885,-3.02319418247306,-3.0158090537654,
-3.01452621991955,-3.01384016723687,-3.01333397662759,-3.01277938234999,
-3.01178855538521,-3.00881240037603,-2.95992484481501,-2.89573188099968,
-2.88183452553617,-2.85745824304657,-2.85437088914118,-2.85297736317385,
-2.85195109045097,-2.85100312665893,-2.84971652378462,-2.84719941705113,
-2.82746988099277,-2.82240507141891,-2.80186097571615,-2.72952413268572,
-2.70315217311971,-2.6930409546565,-2.69200921985429),.UNSPECIFIED.);
#267=B_SPLINE_CURVE_WITH_KNOTS('',3,(#47512,#47513,#47514,#47515,#47516,
#47517,#47518,#47519,#47520,#47521,#47522,#47523,#47524,#47525,#47526,#47527,
#47528,#47529,#47530,#47531,#47532,#47533,#47534,#47535,#47536,#47537,#47538,
#47539,#47540,#47541,#47542,#47543,#47544,#47545,#47546,#47547,#47548,#47549,
#47550,#47551,#47552,#47553,#47554,#47555,#47556,#47557,#47558,#47559,#47560,
#47561,#47562,#47563,#47564,#47565,#47566,#47567,#47568,#47569,#47570,#47571,
#47572,#47573,#47574,#47575,#47576,#47577,#47578,#47579,#47580,#47581,#47582,
#47583,#47584,#47585,#47586,#47587,#47588,#47589,#47590,#47591,#47592,#47593,
#47594,#47595,#47596,#47597,#47598,#47599,#47600,#47601,#47602,#47603,#47604,
#47605,#47606,#47607,#47608,#47609,#47610,#47611,#47612,#47613,#47614,#47615,
#47616,#47617,#47618,#47619,#47620,#47621,#47622,#47623,#47624,#47625,#47626,
#47627,#47628,#47629,#47630,#47631,#47632,#47633,#47634,#47635,#47636,#47637,
#47638,#47639,#47640,#47641,#47642,#47643,#47644,#47645,#47646,#47647,#47648,
#47649,#47650,#47651,#47652,#47653,#47654,#47655,#47656,#47657,#47658,#47659,
#47660,#47661,#47662,#47663,#47664,#47665,#47666,#47667,#47668,#47669,#47670,
#47671,#47672,#47673,#47674,#47675,#47676,#47677,#47678,#47679,#47680,#47681,
#47682,#47683,#47684,#47685,#47686,#47687,#47688,#47689,#47690,#47691,#47692,
#47693,#47694,#47695,#47696,#47697,#47698,#47699,#47700,#47701,#47702,#47703,
#47704,#47705,#47706,#47707,#47708,#47709,#47710,#47711,#47712,#47713,#47714,
#47715,#47716,#47717,#47718,#47719,#47720,#47721,#47722,#47723,#47724,#47725,
#47726,#47727,#47728,#47729,#47730,#47731,#47732,#47733,#47734,#47735,#47736,
#47737),.UNSPECIFIED.,.F.,.F.,(4,2,2,2,2,2,2,2,2,2,2,2,2,2,2,2,2,2,2,2,
2,2,2,2,2,2,2,2,2,2,2,2,2,2,2,2,2,2,2,2,2,2,2,2,2,2,2,2,2,2,2,2,2,2,2,2,
2,2,2,2,2,2,2,2,2,2,2,2,2,2,2,2,2,2,2,2,2,2,2,2,2,2,2,2,2,2,2,2,2,2,2,2,
2,2,2,2,2,2,2,2,2,2,2,2,2,2,2,2,2,2,2,2,4),(-1.37005249657453,-1.34947742657622,
-1.34606802935087,-1.34474042282689,-1.34378184118414,-1.3428150238564,
-1.34151935588637,-1.33883083194066,-1.33533913332211,-1.3060739226842,
-1.24370437695282,-1.18739402378087,-1.18392903894686,-1.18287633209735,
-1.18230926608889,-1.18174870665093,-1.18105891401461,-1.17973201011291,
-1.17141942514509,-1.15310303345706,-1.12795810155243,-1.04050191887311,
-1.03843372157579,-1.02498010866747,-1.02273937652417,-1.02140514142119,
-1.02038496355219,-1.01931834570073,-1.01775811421082,-1.01321564832487,
-1.00650593044383,-0.987171779782808,-0.935326323447163,-0.878303078665348,
-0.875250910405159,-0.873767488080319,-0.871404444155965,-0.869351236206721,
-0.861560025770046,-0.8601722176098,-0.859460340846227,-0.858898082677647,
-0.858261537691823,-0.85717932823904,-0.852955908365347,-0.82145192471196,
-0.737718877608971,-0.721308065905467,-0.718017355768539,-0.715913176560136,
-0.715428920456607,-0.711650108398861,-0.707916802208063,-0.70110522376816,
-0.699147113526778,-0.698000293069543,-0.697003558202362,-0.695786298577297,
-0.693480028775742,-0.690584024033379,-0.684332867718261,-0.666745044899952,
-0.625891942391485,-0.550172923607249,-0.538841001798487,-0.537266785476882,
-0.536535150672556,-0.535968941154943,-0.535350081477446,-0.534346848098215,
-0.530937230737147,-0.509293406041016,-0.48468382235598,-0.477431376513894,
-0.471256915294787,-0.465899268150126,-0.419827025605223,-0.403252692531126,
-0.400738152790972,-0.37969749135209,-0.376885145738053,-0.375553533517467,
-0.374533743684087,-0.373592365508861,-0.372523950765309,-0.369522007840247,
-0.365550490408535,-0.355993501683274,-0.324036484670031,-0.307980280253675,
-0.2200381163081,-0.215762052327458,-0.214272243730014,-0.213549111289099,
-0.212985560230024,-0.212355627141011,-0.211303259550368,-0.207408163838918,
-0.118889757535656,-0.103732932298317,-0.0979144688668333,-0.0840904985382303,
-0.0756962699386087,-0.0723811977320567,-0.0562807987276871,-0.053646672577637,
-0.0523559451565651,-0.0513450680913494,-0.0504022073920895,-0.0493040090954308,
-0.0477372101345243,-0.045047651856617,-0.000960743384126951),
 .UNSPECIFIED.);
#268=B_SPLINE_CURVE_WITH_KNOTS('',3,(#47738,#47739,#47740,#47741,#47742,
#47743),.UNSPECIFIED.,.F.,.F.,(4,1,1,4),(453.485536920593,454.187469090742,
455.187183746215,455.530927222854),.UNSPECIFIED.);
#269=B_SPLINE_CURVE_WITH_KNOTS('',3,(#47744,#47745,#47746,#47747,#47748,
#47749,#47750,#47751,#47752,#47753,#47754,#47755,#47756,#47757,#47758,#47759,
#47760,#47761,#47762,#47763,#47764,#47765,#47766,#47767,#47768,#47769,#47770,
#47771,#47772,#47773,#47774,#47775,#47776,#47777,#47778,#47779,#47780,#47781,
#47782,#47783,#47784,#47785,#47786,#47787,#47788,#47789,#47790,#47791,#47792,
#47793,#47794,#47795,#47796,#47797,#47798,#47799,#47800,#47801,#47802,#47803,
#47804,#47805,#47806,#47807,#47808,#47809,#47810,#47811,#47812,#47813,#47814,
#47815,#47816,#47817,#47818,#47819,#47820,#47821,#47822,#47823,#47824,#47825,
#47826,#47827,#47828,#47829,#47830,#47831,#47832,#47833,#47834,#47835,#47836,
#47837,#47838,#47839,#47840,#47841,#47842,#47843,#47844,#47845,#47846,#47847,
#47848,#47849,#47850,#47851,#47852,#47853,#47854,#47855,#47856,#47857,#47858,
#47859,#47860,#47861,#47862,#47863,#47864,#47865,#47866,#47867,#47868,#47869,
#47870,#47871,#47872,#47873,#47874,#47875,#47876,#47877,#47878,#47879,#47880,
#47881,#47882,#47883,#47884,#47885,#47886,#47887,#47888,#47889,#47890,#47891,
#47892,#47893,#47894,#47895,#47896,#47897,#47898,#47899,#47900,#47901,#47902,
#47903,#47904,#47905,#47906,#47907,#47908,#47909,#47910,#47911,#47912,#47913,
#47914,#47915,#47916,#47917,#47918,#47919,#47920,#47921,#47922,#47923,#47924,
#47925,#47926,#47927,#47928,#47929,#47930,#47931,#47932,#47933,#47934,#47935,
#47936,#47937,#47938,#47939,#47940,#47941,#47942,#47943,#47944,#47945,#47946,
#47947,#47948,#47949,#47950,#47951,#47952,#47953,#47954,#47955,#47956,#47957,
#47958,#47959,#47960,#47961,#47962,#47963,#47964,#47965,#47966,#47967,#47968,
#47969,#47970,#47971,#47972,#47973,#47974,#47975,#47976,#47977,#47978,#47979,
#47980,#47981,#47982,#47983,#47984,#47985,#47986,#47987,#47988,#47989,#47990,
#47991,#47992,#47993,#47994,#47995,#47996,#47997,#47998,#47999,#48000,#48001,
#48002,#48003,#48004,#48005,#48006,#48007,#48008,#48009,#48010,#48011,#48012,
#48013),.UNSPECIFIED.,.F.,.F.,(4,2,2,2,2,2,2,2,2,2,2,2,2,2,2,2,2,2,2,2,
2,2,2,2,2,2,2,2,2,2,2,2,2,2,2,2,2,2,2,2,2,2,2,2,2,2,2,2,2,2,2,2,2,2,2,2,
2,2,2,2,2,2,2,2,2,2,2,2,2,2,2,2,2,2,2,2,2,2,2,2,2,2,2,2,2,2,2,2,2,2,2,2,
2,2,2,2,2,2,2,2,2,2,2,2,2,2,2,2,2,2,2,2,2,2,2,2,2,2,2,2,2,2,2,2,2,2,2,2,
2,2,2,2,2,2,4),(-2.69200921985429,-2.69165321726174,-2.69094492855103,-2.69043602228833,
-2.68989173778862,-2.68911289351126,-2.68696659719547,-2.65386039208112,
-2.58216715875224,-2.53909144951289,-2.5347021149539,-2.53146748021361,
-2.53006771374992,-2.52903514301789,-2.52809474322263,-2.5268383893358,
-2.52377637728473,-2.49480666964021,-2.40388668536287,-2.39339612428702,
-2.37261064295925,-2.36929745269862,-2.36829632460508,-2.36767785309433,
-2.36711136523722,-2.36637850861288,-2.36479834071029,-2.35332202431041,
-2.35001553946594,-2.25876051509073,-2.22950881806805,-2.21046852014313,
-2.20794641268655,-2.20667833707885,-2.20576486098085,-2.20479649551643,
-2.20343262027594,-2.20060762028636,-2.17026987433493,-2.15993609144862,
-2.08376853296493,-2.04768000709782,-2.0457860202543,-2.04498816166278,
-2.04441295433481,-2.04388539197335,-2.04316935936716,-2.04176815597483,
-2.03088139231954,-2.00015673704151,-1.89231080395764,-1.88618497250253,
-1.88430574483263,-1.88328942155656,-1.88228476780398,-1.88106651957949,
-1.87878222896055,-1.86597725092406,-1.84118862290925,-1.75132733423306,
-1.72457965587552,-1.7226567568446,-1.72191276475521,-1.72137792715382,
-1.72080792251254,-1.72003959242045,-1.71831233261279,-1.67074170691629,
-1.56899289622534,-1.56298881875898,-1.5611243857828,-1.56011105215202,
-1.55910618972366,-1.55790771252357,-1.55568457569179,-1.55291786275152,
-1.49383231944649,-1.42461989541395,-1.40427278527274,-1.40014892190999,
-1.39903652947395,-1.39838667546102,-1.39788202393566,-1.39721416841314,
-1.39599002547766,-1.38977804068478,-1.37738240180472,-1.35388154729539,
-1.249132390923,-1.24040456449739,-1.23847166115012,-1.23721680900121,-1.23620985098609,
-1.23509181032965,-1.23327109109389,-1.23107158491522,-1.2267647527842,
-1.18509966529055,-1.1327460959081,-1.08701879002559,-1.0857060874427,-1.08418438433995,
-1.08150988702066,-1.07715400133105,-1.07601867342492,-1.07536354798018,
-1.07480325559912,-1.07411710724616,-1.07280719997668,-1.06489171719722,
-1.05176581656063,-1.02524132766951,-0.946818656505899,-0.918992858982936,
-0.915922201012758,-0.914685432211556,-0.913656341989606,-0.912710674531701,
-0.911285265281233,-0.907903263444656,-0.903264508743662,-0.89148934009968,
-0.865710076516489,-0.825415060322478,-0.766528317792936,-0.754991821724399,
-0.753409752631514,-0.752676686519284,-0.752110326950788,-0.751492296094884,
-0.750492521751862,-0.747114141450464,-0.725793593103464,-0.681591163627844,
-0.661698739247463),.UNSPECIFIED.);
#270=B_SPLINE_CURVE_WITH_KNOTS('',3,(#48018,#48019,#48020,#48021,#48022,
#48023,#48024,#48025,#48026,#48027,#48028,#48029,#48030,#48031,#48032,#48033,
#48034,#48035,#48036,#48037,#48038,#48039,#48040,#48041,#48042,#48043,#48044,
#48045,#48046,#48047,#48048,#48049,#48050,#48051,#48052,#48053,#48054,#48055,
#48056,#48057,#48058,#48059,#48060,#48061,#48062,#48063,#48064,#48065,#48066,
#48067,#48068,#48069,#48070,#48071,#48072,#48073,#48074,#48075,#48076,#48077,
#48078,#48079,#48080,#48081,#48082,#48083,#48084,#48085,#48086,#48087,#48088,
#48089,#48090,#48091,#48092,#48093,#48094,#48095,#48096,#48097,#48098,#48099,
#48100,#48101,#48102,#48103,#48104,#48105,#48106,#48107,#48108,#48109,#48110,
#48111,#48112,#48113,#48114,#48115,#48116,#48117,#48118,#48119,#48120,#48121,
#48122,#48123,#48124,#48125,#48126,#48127,#48128,#48129,#48130,#48131,#48132,
#48133,#48134,#48135,#48136,#48137,#48138,#48139,#48140,#48141,#48142,#48143,
#48144,#48145,#48146,#48147,#48148,#48149,#48150,#48151,#48152,#48153,#48154,
#48155,#48156,#48157,#48158,#48159,#48160,#48161,#48162,#48163,#48164,#48165,
#48166,#48167,#48168,#48169,#48170,#48171,#48172,#48173,#48174,#48175,#48176,
#48177,#48178,#48179,#48180,#48181,#48182,#48183,#48184,#48185,#48186,#48187,
#48188,#48189,#48190,#48191,#48192,#48193,#48194,#48195,#48196,#48197,#48198,
#48199,#48200,#48201,#48202,#48203,#48204,#48205,#48206,#48207,#48208,#48209,
#48210,#48211,#48212,#48213,#48214,#48215,#48216,#48217,#48218,#48219,#48220,
#48221,#48222,#48223,#48224,#48225,#48226,#48227,#48228,#48229,#48230,#48231,
#48232,#48233,#48234,#48235,#48236,#48237,#48238,#48239,#48240,#48241,#48242,
#48243,#48244,#48245,#48246,#48247,#48248,#48249,#48250,#48251,#48252,#48253,
#48254,#48255,#48256,#48257,#48258,#48259,#48260,#48261,#48262,#48263,#48264,
#48265,#48266,#48267,#48268,#48269,#48270,#48271,#48272,#48273,#48274,#48275,
#48276,#48277,#48278,#48279,#48280,#48281,#48282,#48283,#48284,#48285,#48286,
#48287,#48288,#48289,#48290,#48291,#48292,#48293,#48294,#48295,#48296,#48297,
#48298,#48299,#48300,#48301,#48302,#48303,#48304,#48305,#48306,#48307,#48308,
#48309,#48310,#48311,#48312,#48313,#48314,#48315,#48316,#48317,#48318,#48319,
#48320,#48321,#48322,#48323,#48324,#48325,#48326,#48327,#48328,#48329,#48330,
#48331,#48332,#48333,#48334,#48335,#48336,#48337,#48338,#48339),
 .UNSPECIFIED.,.F.,.F.,(4,2,2,2,2,2,2,2,2,2,2,2,2,2,2,2,2,2,2,2,2,2,2,2,
2,2,2,2,2,2,2,2,2,2,2,2,2,2,2,2,2,2,2,2,2,2,2,2,2,2,2,2,2,2,2,2,2,2,2,2,
2,2,2,2,2,2,2,2,2,2,2,2,2,2,2,2,2,2,2,2,2,2,2,2,2,2,2,2,2,2,2,2,2,2,2,2,
2,2,2,2,2,2,2,2,2,2,2,2,2,2,2,2,2,2,2,2,2,2,2,2,2,2,2,2,2,2,2,2,2,2,2,2,
2,2,2,2,2,2,2,2,2,2,2,2,2,2,2,2,2,2,2,2,2,2,2,2,2,2,2,2,4),(-3.40020803169445,
-3.35398570630315,-3.29013598947784,-3.28471453628915,-3.2829927101431,
-3.2818987238525,-3.28088073172867,-3.27955963004755,-3.27669578807702,
-3.26875965935094,-3.26642402437193,-3.26563970565285,-3.2640494092677,
-3.26345428659867,-3.2613705723809,-3.25988002549393,-3.25867461756904,
-3.25735496832278,-3.25121029429168,-3.16052920749821,-3.13420323739372,
-3.12646157331662,-3.12356779444746,-3.12216665504375,-3.12133511339737,
-3.12061412057079,-3.12005234574844,-3.11952264061871,-3.1187980366879,
-3.11736305085652,-3.10552991326149,-3.10474106284485,-3.10427868228702,
-3.10336680774234,-3.10300764822804,-3.02159881000798,-2.98002503432068,
-2.96300453254703,-2.96054706496354,-2.9592924114776,-2.95838090468532,
-2.95740739439603,-2.95574146390953,-2.95119144571076,-2.87770004397311,
-2.82219124676294,-2.80210250940144,-2.79994180147395,-2.79880992330032,
-2.79785040550319,-2.79724658336112,-2.79667953399562,-2.79594238529268,
-2.79433905002222,-2.78225339741649,-2.78100941024525,-2.77864282286437,
-2.7772112825547,-2.74661315305248,-2.67621596014387,-2.64429393188747,
-2.63874000431064,-2.63700241192106,-2.63590485381464,-2.63488799813024,
-2.63357464424756,-2.63075209409682,-2.62275996417313,-2.62090398579852,
-2.61897589381954,-2.61819339237392,-2.61748186929377,-2.61540608505668,
-2.61450914757871,-2.61045109072549,-2.60840357286315,-2.59613601351232,
-2.52087870550378,-2.4965222512257,-2.47885259714141,-2.47684851220761,
-2.47577661299671,-2.47508230041829,-2.47445948346121,-2.47391039702322,
-2.47324873384539,-2.47208539630559,-2.46727602544291,-2.37043576878027,
-2.35211470484474,-2.32857141440818,-2.31662110282314,-2.31438070669267,
-2.31317191075265,-2.312265585865,-2.3111244023118,-2.3091916117794,-2.30260670372054,
-2.29875568237016,-2.29480499064254,-2.29273362907647,-2.29098857853584,
-2.28977151563447,-2.28754665537073,-2.283254116112,-2.20645379036111,-2.15407249799104,
-2.15233768703452,-2.15156803611938,-2.15099786563572,-2.15046348525701,
-2.14972106161175,-2.14780728535993,-2.12161250245554,-2.03136322932114,
-1.99518731497887,-1.99197842230844,-1.99068493155661,-1.98973529863622,
-1.9887104799783,-1.98732468840064,-1.98419058145667,-1.93429768311864,
-1.83989692624847,-1.83858202211452,-1.83705663898469,-1.83455798955058,
-1.8335118803677,-1.82987556844279,-1.8288028172068,-1.82823169499027,-1.82767678252558,
-1.82699591944879,-1.82571132828652,-1.81835395861684,-1.80294688438215,
-1.78979566029935,-1.70646181409129,-1.69248356428609,-1.67146520918019,
-1.66861722691605,-1.66729901650909,-1.66628137167775,-1.66520797260919,
-1.66353771887348,-1.66158690583593,-1.65793330710152,-1.6263682433561,
-1.58074957163203,-1.55120522810682,-1.50931439754957,-1.50666690459669,
-1.50572235870822,-1.5051770655646,-1.50466854905917,-1.50396285739634,
-1.50255925117531,-1.49208045462941,-1.46417818883468,-1.39796080861194,
-1.37005249657453),.UNSPECIFIED.);
#271=B_SPLINE_CURVE_WITH_KNOTS('',3,(#48341,#48342,#48343,#48344,#48345,
#48346,#48347,#48348,#48349,#48350,#48351,#48352,#48353,#48354,#48355,#48356,
#48357,#48358,#48359,#48360,#48361,#48362,#48363,#48364,#48365,#48366,#48367,
#48368,#48369,#48370,#48371,#48372,#48373,#48374,#48375,#48376,#48377,#48378,
#48379,#48380,#48381,#48382,#48383,#48384,#48385,#48386,#48387,#48388,#48389,
#48390,#48391,#48392,#48393,#48394,#48395,#48396,#48397,#48398,#48399,#48400,
#48401,#48402,#48403,#48404,#48405,#48406,#48407,#48408,#48409,#48410,#48411,
#48412,#48413,#48414,#48415,#48416,#48417,#48418,#48419,#48420,#48421,#48422,
#48423,#48424,#48425,#48426,#48427,#48428,#48429,#48430,#48431,#48432,#48433,
#48434),.UNSPECIFIED.,.F.,.F.,(4,2,2,2,2,2,2,2,2,2,2,2,2,2,2,2,2,2,2,2,
2,2,2,2,2,2,2,2,2,2,2,2,2,2,2,2,2,2,2,2,2,2,2,2,2,2,4),(-0.661698739247463,
-0.63155827478073,-0.596440654951037,-0.593254201436511,-0.59196463836349,
-0.591016042432585,-0.590055886256616,-0.589058467814166,-0.586771017828778,
-0.573748051955903,-0.549672423321915,-0.51894174027973,-0.442624554119548,
-0.432068640809763,-0.43068029678856,-0.429967659942444,-0.429441044648925,
-0.428865271497753,-0.428063804292975,-0.426148043269977,-0.423510346780509,
-0.395101611831078,-0.357958254519825,-0.339759849144639,-0.315622408306712,
-0.299752363421774,-0.292937832283236,-0.291438612422854,-0.272844813936617,
-0.270095870077907,-0.268796622041962,-0.267781882656786,-0.266840258423881,
-0.265757452267252,-0.262689961811862,-0.229166499655505,-0.208869859261655,
-0.113498928485787,-0.108564664346256,-0.107481722724927,-0.106781224964328,
-0.106219892526339,-0.105575491922326,-0.104458328543778,-0.0998185169514192,
-0.0603751173097801,-0.000962380706964255),.UNSPECIFIED.);
#272=B_SPLINE_CURVE_WITH_KNOTS('',3,(#48435,#48436,#48437,#48438,#48439,
#48440,#48441,#48442,#48443,#48444,#48445,#48446,#48447,#48448,#48449,#48450,
#48451,#48452,#48453,#48454,#48455,#48456,#48457,#48458,#48459,#48460,#48461,
#48462,#48463,#48464,#48465,#48466,#48467,#48468,#48469,#48470,#48471,#48472,
#48473,#48474,#48475,#48476,#48477,#48478,#48479,#48480,#48481,#48482,#48483,
#48484,#48485,#48486,#48487,#48488,#48489,#48490,#48491,#48492,#48493,#48494,
#48495,#48496,#48497,#48498,#48499,#48500,#48501,#48502,#48503,#48504,#48505,
#48506,#48507,#48508,#48509,#48510,#48511,#48512,#48513,#48514,#48515,#48516,
#48517,#48518,#48519,#48520,#48521,#48522,#48523,#48524,#48525,#48526,#48527,
#48528,#48529,#48530,#48531,#48532,#48533,#48534,#48535,#48536,#48537,#48538,
#48539,#48540,#48541,#48542,#48543,#48544,#48545,#48546,#48547,#48548,#48549,
#48550,#48551,#48552,#48553,#48554,#48555,#48556,#48557,#48558,#48559,#48560,
#48561,#48562,#48563,#48564,#48565,#48566,#48567,#48568,#48569,#48570,#48571,
#48572,#48573,#48574,#48575,#48576),.UNSPECIFIED.,.F.,.F.,(4,3,3,3,3,3,
3,3,3,3,3,3,3,3,3,3,3,3,3,3,3,3,3,3,3,3,3,3,3,3,3,3,3,3,3,3,3,3,3,3,3,3,
3,3,3,3,3,4),(461.814120077699,461.906710520206,461.999282389779,462.091860611502,
462.184470108962,462.277191924903,462.369980696409,462.462916807322,462.486523846003,
462.579596790279,462.672543629916,462.765392001101,462.858172505756,462.950917827912,
463.043652793014,463.136402211355,463.22925085209,463.322151292702,463.415207188786,
463.486238501476,463.579311445752,463.672258285389,463.765106656574,463.857887161229,
463.950632483385,464.043367448486,464.136116866827,464.228965507563,464.321865948174,
464.414921844258,464.485953156949,464.579026101225,464.671972940862,464.764821312047,
464.857601816702,464.950347138859,465.04308210396,465.135831522301,465.228680163036,
465.321580603648,465.414636499732,465.485667812422,465.578733049488,465.671678204188,
465.766469833072,465.859244858906,465.955044789315,466.050844719725),
 .UNSPECIFIED.);
#273=B_SPLINE_CURVE_WITH_KNOTS('',3,(#48582,#48583,#48584,#48585,#48586,
#48587,#48588,#48589,#48590),.UNSPECIFIED.,.F.,.F.,(4,1,1,1,1,1,4),(468.097305384879,
468.183474267362,469.183188922835,470.182903578308,471.18261823378,472.182332889253,
472.335020342325),.UNSPECIFIED.);
#274=B_SPLINE_CURVE_WITH_KNOTS('',3,(#48591,#48592,#48593,#48594,#48595,
#48596,#48597,#48598,#48599,#48600,#48601,#48602,#48603,#48604,#48605,#48606,
#48607,#48608,#48609,#48610,#48611,#48612,#48613,#48614,#48615,#48616,#48617,
#48618,#48619,#48620,#48621,#48622,#48623,#48624,#48625,#48626,#48627,#48628,
#48629,#48630,#48631,#48632,#48633,#48634,#48635,#48636,#48637,#48638,#48639,
#48640,#48641,#48642,#48643,#48644,#48645,#48646,#48647,#48648,#48649,#48650,
#48651,#48652,#48653,#48654,#48655,#48656,#48657,#48658,#48659,#48660,#48661,
#48662,#48663,#48664,#48665,#48666,#48667,#48668,#48669,#48670,#48671,#48672,
#48673,#48674,#48675,#48676,#48677,#48678,#48679,#48680),.UNSPECIFIED.,
 .F.,.F.,(4,2,2,2,2,2,2,2,2,2,2,2,2,2,2,2,2,2,2,2,2,2,2,2,2,2,2,2,2,2,2,
2,2,2,2,2,2,2,2,2,2,2,2,2,4),(-4.0615787133633,-3.96620177886682,-3.94503108919774,
-3.93181765514419,-3.92951421756921,-3.92829213342944,-3.92728762705765,
-3.92627426614759,-3.92440867070688,-3.91839205846606,-3.80196330535944,
-3.77967963236435,-3.77222240536503,-3.76940715944143,-3.76740557751464,
-3.76659008987622,-3.76606427033867,-3.7654919740136,-3.76480504787816,
-3.763170536333,-3.74960832598282,-3.71984875033243,-3.70071937502966,-3.66351880813675,
-3.61123877065554,-3.60724819991789,-3.60571977798997,-3.60466757844447,
-3.60363737175628,-3.60239662282504,-3.599302266991,-3.57062615652089,-3.52079054086545,
-3.4737166867985,-3.45405731627538,-3.4484113590116,-3.44611753151641,-3.4449354149033,
-3.44394137526668,-3.44332964851857,-3.44276496805675,-3.44204401693983,
-3.4405253381659,-3.43049852344022,-3.40020803169445),.UNSPECIFIED.);
#275=B_SPLINE_CURVE_WITH_KNOTS('',3,(#48682,#48683,#48684,#48685,#48686,
#48687,#48688,#48689,#48690,#48691,#48692,#48693,#48694,#48695,#48696,#48697,
#48698,#48699,#48700,#48701,#48702,#48703,#48704,#48705,#48706,#48707,#48708,
#48709,#48710,#48711,#48712,#48713,#48714,#48715,#48716,#48717,#48718,#48719,
#48720,#48721,#48722,#48723,#48724,#48725,#48726,#48727,#48728,#48729,#48730,
#48731,#48732,#48733,#48734,#48735,#48736,#48737,#48738,#48739,#48740,#48741,
#48742,#48743,#48744,#48745,#48746,#48747,#48748,#48749,#48750,#48751),
 .UNSPECIFIED.,.F.,.F.,(4,3,3,3,3,3,3,3,3,3,3,3,3,3,3,3,3,3,3,3,3,3,3,4),
(466.050844719725,466.143596562294,466.236448811706,466.329354796081,466.422413806425,
466.485382467895,466.578455412171,466.671402251808,466.764250622992,466.857031127648,
466.949776449804,467.042511414905,467.135260833247,467.228109473982,467.321009914593,
467.414065810677,467.485097123367,467.579229131387,467.673226742089,467.767113320224,
467.860900400145,467.95462914991,468.048328493834,468.097305384879),
 .UNSPECIFIED.);
#276=B_SPLINE_CURVE_WITH_KNOTS('',3,(#48752,#48753,#48754,#48755,#48756,
#48757,#48758,#48759,#48760,#48761,#48762,#48763,#48764,#48765,#48766,#48767,
#48768,#48769,#48770,#48771,#48772,#48773,#48774,#48775,#48776,#48777,#48778,
#48779,#48780,#48781,#48782,#48783,#48784,#48785,#48786,#48787,#48788,#48789,
#48790,#48791,#48792,#48793,#48794,#48795,#48796,#48797,#48798,#48799,#48800,
#48801,#48802,#48803,#48804,#48805,#48806,#48807,#48808,#48809,#48810,#48811,
#48812,#48813,#48814,#48815,#48816,#48817,#48818,#48819,#48820,#48821,#48822,
#48823,#48824,#48825,#48826,#48827,#48828,#48829,#48830,#48831,#48832,#48833,
#48834,#48835,#48836,#48837,#48838,#48839,#48840,#48841,#48842,#48843,#48844,
#48845,#48846,#48847,#48848,#48849,#48850,#48851,#48852,#48853,#48854,#48855,
#48856,#48857,#48858,#48859,#48860,#48861,#48862,#48863,#48864,#48865,#48866,
#48867,#48868,#48869,#48870,#48871,#48872,#48873,#48874,#48875,#48876,#48877,
#48878,#48879,#48880,#48881,#48882,#48883,#48884,#48885,#48886,#48887,#48888,
#48889,#48890,#48891,#48892,#48893,#48894,#48895,#48896,#48897,#48898,#48899,
#48900,#48901,#48902,#48903,#48904,#48905,#48906,#48907,#48908,#48909,#48910,
#48911,#48912,#48913,#48914,#48915,#48916,#48917,#48918,#48919,#48920,#48921,
#48922,#48923,#48924,#48925,#48926,#48927,#48928,#48929,#48930,#48931,#48932,
#48933,#48934,#48935,#48936,#48937),.UNSPECIFIED.,.F.,.F.,(4,2,2,2,2,2,
2,2,2,2,2,2,2,2,2,2,2,2,2,2,2,2,2,2,2,2,2,2,2,2,2,2,2,2,2,2,2,2,2,2,2,2,
2,2,2,2,2,2,2,2,2,2,2,2,2,2,2,2,2,2,2,2,2,2,2,2,2,2,2,2,2,2,2,2,2,2,2,2,
2,2,2,2,2,2,2,2,2,2,2,2,2,2,4),(-4.06102333513819,-3.96661297328627,-3.94683356885609,
-3.93828133537681,-3.93694479057649,-3.93625299686735,-3.9356923494225,
-3.9351265088338,-3.9340797865513,-3.93066447296231,-3.87155298263716,-3.82222574212027,
-3.8034392971281,-3.78718506566586,-3.7812897165891,-3.77719386933177,-3.77565164006015,
-3.77471029304505,-3.77369065752855,-3.77235988113401,-3.76955160478619,
-3.74861391313929,-3.74647686426005,-3.70429585091037,-3.67504670677928,
-3.61689596049452,-3.61452905408814,-3.61365635747988,-3.61306620414351,
-3.61249191978958,-3.61179749555171,-3.61012108741465,-3.59522644760756,
-3.5935481312716,-3.59239646518981,-3.51645285402837,-3.4827428536277,-3.46497190228762,
-3.45867175374597,-3.45575880576181,-3.45344224045727,-3.45222227852344,
-3.45122729886878,-3.45022924412357,-3.44844062621916,-3.44302958760913,
-3.37028995110029,-3.32493451580695,-3.29600822902595,-3.29334502975947,
-3.29141458258231,-3.29061058507698,-3.29003430706728,-3.28950817212511,
-3.28879753654037,-3.28741705157541,-3.27706424183957,-3.27534818489528,
-3.18270236713388,-3.15246530018486,-3.13959001225012,-3.13463234365715,
-3.13219291099084,-3.13018735644553,-3.12903744098369,-3.12812711588652,
-3.12710706113729,-3.12520905938198,-3.11892483816865,-3.00433252195369,
-2.98767310454523,-2.97719508497035,-2.96919318877411,-2.96787925868693,
-2.96719214813878,-2.96663166474445,-2.96597699694161,-2.96484410785524,
-2.9605150234889,-2.88625559350889,-2.84263187020004,-2.81580431920211,
-2.81117914581305,-2.80886118231187,-2.80744807022002,-2.80615930686291,
-2.80516399782833,-2.80419706420858,-2.80283854552623,-2.80003546021256,
-2.77063181171653,-2.70090609820099,-2.6921555152646),.UNSPECIFIED.);
#277=B_SPLINE_CURVE_WITH_KNOTS('',3,(#48943,#48944,#48945,#48946,#48947,
#48948,#48949,#48950,#48951,#48952,#48953,#48954,#48955,#48956,#48957,#48958,
#48959,#48960,#48961,#48962,#48963,#48964,#48965,#48966,#48967,#48968,#48969,
#48970,#48971,#48972,#48973,#48974,#48975,#48976,#48977,#48978,#48979,#48980,
#48981,#48982,#48983,#48984,#48985,#48986,#48987,#48988,#48989,#48990,#48991,
#48992,#48993,#48994,#48995,#48996,#48997,#48998,#48999,#49000,#49001,#49002,
#49003,#49004,#49005,#49006,#49007,#49008,#49009,#49010,#49011,#49012,#49013,
#49014,#49015,#49016,#49017,#49018,#49019,#49020,#49021,#49022,#49023,#49024,
#49025,#49026,#49027,#49028,#49029,#49030,#49031,#49032,#49033,#49034,#49035,
#49036,#49037,#49038,#49039,#49040,#49041,#49042,#49043,#49044,#49045,#49046,
#49047,#49048,#49049,#49050,#49051,#49052,#49053,#49054,#49055,#49056,#49057,
#49058,#49059,#49060,#49061,#49062,#49063,#49064,#49065,#49066,#49067,#49068,
#49069,#49070,#49071,#49072,#49073,#49074,#49075,#49076,#49077,#49078,#49079,
#49080,#49081,#49082,#49083,#49084,#49085,#49086,#49087,#49088,#49089,#49090,
#49091,#49092,#49093,#49094,#49095,#49096,#49097,#49098,#49099,#49100,#49101,
#49102,#49103,#49104,#49105,#49106,#49107,#49108,#49109,#49110,#49111,#49112,
#49113,#49114,#49115,#49116,#49117,#49118,#49119,#49120,#49121,#49122,#49123,
#49124,#49125,#49126,#49127,#49128,#49129,#49130,#49131,#49132,#49133,#49134,
#49135,#49136),.UNSPECIFIED.,.F.,.F.,(4,2,2,2,2,2,2,2,2,2,2,2,2,2,2,2,2,
2,2,2,2,2,2,2,2,2,2,2,2,2,2,2,2,2,2,2,2,2,2,2,2,2,2,2,2,2,2,2,2,2,2,2,2,
2,2,2,2,2,2,2,2,2,2,2,2,2,2,2,2,2,2,2,2,2,2,2,2,2,2,2,2,2,2,2,2,2,2,2,2,
2,2,2,2,2,2,2,4),(-1.36992344699479,-1.33960600328324,-1.26228671155231,
-1.23213459145953,-1.23016072994359,-1.2294085412778,-1.22887155089048,
-1.22835978497847,-1.22764679456012,-1.22618974112011,-1.21350048378456,
-1.18806983696264,-1.13244453543704,-1.07382188127391,-1.06998499640528,
-1.06858894017261,-1.06761185348278,-1.06670137986705,-1.06545492751759,
-1.06303707312315,-1.04740332913328,-1.01112232314901,-0.950033619719869,
-0.922931174911829,-0.922605097521007,-0.921691854054946,-0.921230660763885,
-0.920442522312564,-0.908606070033288,-0.90717097083674,-0.906446336991062,
-0.905916622286234,-0.905343299170856,-0.904775673089278,-0.903394366543461,
-0.893473916510318,-0.867904806572996,-0.823313541315134,-0.789348744931029,
-0.786232056619268,-0.750048493467329,-0.746839117141523,-0.745545445941268,
-0.744595685753544,-0.743570734734431,-0.742184772950679,-0.739050318367336,
-0.734865950220565,-0.72461480256142,-0.688649671775339,-0.636737754195658,
-0.587525744593009,-0.584662443851755,-0.583686635801761,-0.583135068269418,
-0.582628240192152,-0.582088947190191,-0.581411745210198,-0.578916009252255,
-0.55346583158862,-0.512237808824646,-0.429930139050887,-0.424603356767535,
-0.422826019385017,-0.421830220116047,-0.420923835426037,-0.419714958969524,
-0.417474413467056,-0.405748283319039,-0.382678751118875,-0.348368915438273,
-0.3191046067704,-0.277362426122141,-0.276979030294106,-0.273870193803622,
-0.262733693484774,-0.261187272214194,-0.26044998771106,-0.25988292888482,
-0.259266772920944,-0.25863313562572,-0.257706302058061,-0.25004211900516,
-0.217471255943138,-0.206023129562492,-0.193655928435844,-0.1623328410385,
-0.105044923905998,-0.101252073628557,-0.0998627891717248,-0.0988875652544676,
-0.097976544012608,-0.0967258052425551,-0.0942873535456371,-0.0912209017053736,
-0.0844695428702945,-0.000961974495844116),.UNSPECIFIED.);
#278=B_SPLINE_CURVE_WITH_KNOTS('',3,(#49137,#49138,#49139,#49140,#49141,
#49142),.UNSPECIFIED.,.F.,.F.,(4,1,1,4),(472.335020342325,473.182047544726,
474.181762200199,474.380490692059),.UNSPECIFIED.);
#279=B_SPLINE_CURVE_WITH_KNOTS('',3,(#49143,#49144,#49145,#49146,#49147,
#49148,#49149,#49150,#49151,#49152,#49153,#49154,#49155,#49156,#49157,#49158,
#49159,#49160,#49161,#49162,#49163,#49164,#49165,#49166,#49167,#49168,#49169,
#49170,#49171,#49172,#49173,#49174,#49175,#49176,#49177,#49178,#49179,#49180,
#49181,#49182,#49183,#49184,#49185,#49186,#49187,#49188,#49189,#49190,#49191,
#49192,#49193,#49194,#49195,#49196,#49197,#49198,#49199,#49200,#49201,#49202,
#49203,#49204,#49205,#49206,#49207,#49208,#49209,#49210,#49211,#49212,#49213,
#49214,#49215,#49216,#49217,#49218,#49219,#49220,#49221,#49222,#49223,#49224,
#49225,#49226,#49227,#49228,#49229,#49230,#49231,#49232,#49233,#49234,#49235,
#49236,#49237,#49238,#49239,#49240,#49241,#49242,#49243,#49244,#49245,#49246,
#49247,#49248,#49249,#49250,#49251,#49252,#49253,#49254,#49255,#49256,#49257,
#49258,#49259,#49260,#49261,#49262,#49263,#49264,#49265,#49266,#49267,#49268,
#49269,#49270,#49271,#49272,#49273,#49274,#49275,#49276,#49277,#49278,#49279,
#49280,#49281,#49282,#49283,#49284,#49285,#49286,#49287,#49288,#49289,#49290,
#49291,#49292,#49293,#49294,#49295,#49296,#49297,#49298,#49299,#49300,#49301,
#49302,#49303,#49304,#49305,#49306,#49307,#49308,#49309,#49310,#49311,#49312,
#49313,#49314,#49315,#49316,#49317,#49318,#49319,#49320,#49321,#49322,#49323,
#49324,#49325,#49326,#49327,#49328,#49329,#49330,#49331,#49332,#49333,#49334,
#49335,#49336,#49337,#49338,#49339,#49340,#49341,#49342,#49343,#49344,#49345,
#49346,#49347,#49348,#49349,#49350,#49351,#49352,#49353,#49354,#49355,#49356,
#49357,#49358,#49359,#49360,#49361,#49362,#49363,#49364,#49365,#49366,#49367,
#49368,#49369,#49370,#49371,#49372,#49373,#49374,#49375,#49376,#49377,#49378,
#49379,#49380,#49381,#49382,#49383,#49384,#49385,#49386,#49387,#49388,#49389,
#49390,#49391,#49392,#49393,#49394,#49395,#49396,#49397,#49398,#49399,#49400,
#49401,#49402,#49403,#49404,#49405,#49406,#49407,#49408,#49409,#49410,#49411,
#49412,#49413,#49414,#49415,#49416,#49417,#49418,#49419,#49420,#49421,#49422,
#49423,#49424,#49425,#49426,#49427,#49428,#49429,#49430,#49431,#49432,#49433,
#49434,#49435,#49436,#49437,#49438,#49439,#49440,#49441,#49442,#49443,#49444,
#49445,#49446,#49447,#49448,#49449,#49450,#49451,#49452,#49453,#49454,#49455,
#49456,#49457,#49458,#49459,#49460,#49461,#49462,#49463,#49464,#49465,#49466),
 .UNSPECIFIED.,.F.,.F.,(4,2,2,2,2,2,2,2,2,2,2,2,2,2,2,2,2,2,2,2,2,2,2,2,
2,2,2,2,2,2,2,2,2,2,2,2,2,2,2,2,2,2,2,2,2,2,2,2,2,2,2,2,2,2,2,2,2,2,2,2,
2,2,2,2,2,2,2,2,2,2,2,2,2,2,2,2,2,2,2,2,2,2,2,2,2,2,2,2,2,2,2,2,2,2,2,2,
2,2,2,2,2,2,2,2,2,2,2,2,2,2,2,2,2,2,2,2,2,2,2,2,2,2,2,2,2,2,2,2,2,2,2,2,
2,2,2,2,2,2,2,2,2,2,2,2,2,2,2,2,2,2,2,2,2,2,2,2,2,2,2,2,2,4),(-2.6921555152646,
-2.64872518836412,-2.64556828097275,-2.64459303618737,-2.64398035314961,
-2.6434118967061,-2.64266641215536,-2.64107969144127,-2.62889557859108,
-2.62680371756745,-2.62565101194808,-2.62384307272071,-2.62365651231036,
-2.62173630501906,-2.61783628235704,-2.56533226983517,-2.52079374687381,
-2.49078619247967,-2.48724121356062,-2.48533250295622,-2.48409141163039,
-2.48292768953092,-2.48198564837255,-2.48096706012537,-2.47907729353888,
-2.47286552646328,-2.36936543701896,-2.32387011012541,-2.32202891283071,
-2.32124010998656,-2.32066646266215,-2.32013669900715,-2.31941236655072,
-2.31797897979877,-2.3062032700755,-2.30454171834748,-2.21542816650337,
-2.17912023648743,-2.16345935447878,-2.16105056887395,-2.15980578344754,
-2.15889528835548,-2.15791699652451,-2.1562280876479,-2.15152772817747,
-2.08015996604046,-2.0305930422031,-2.01993183746673,-2.01786541763354,
-2.01765403785961,-2.01557440502413,-2.01441867610367,-2.01323285592272,
-2.01281808440065,-2.01133220265145,-2.0003366081747,-1.99893119223079,
-1.99821402542402,-1.99768612160929,-1.99711104658864,-1.99631425752895,
-1.99442690601696,-1.9593387143366,-1.85873970573516,-1.85750761155556,
-1.85650250987388,-1.85562547822162,-1.85353222682329,-1.85266089977613,
-1.85087566958439,-1.84889985721392,-1.84064446174111,-1.83801547658754,
-1.8367257094214,-1.83571486839475,-1.83459437209975,-1.83275480607629,
-1.82626791825706,-1.78518121937992,-1.73793799932418,-1.67997671180798,
-1.67638419090264,-1.67531640161721,-1.67474623576602,-1.6741911881303,
-1.6735224257443,-1.6722798977157,-1.67072279480498,-1.61924445570903,-1.53812099080982,
-1.53535101509222,-1.51773605791126,-1.51503005334933,-1.51373899616501,
-1.51272527997245,-1.51161678169669,-1.50983069829253,-1.50437161932364,
-1.47242999474235,-1.4025288931549,-1.36879892504244,-1.36842534310419,
-1.36512993607868,-1.35417583929333,-1.35277211337036,-1.35205543157192,
-1.35152770129138,-1.35095262783457,-1.35017155766544,-1.34836067021856,
-1.34588154857607,-1.25703859919527,-1.1963341120859,-1.1925483604652,-1.19116008665413,
-1.19018507594113,-1.18927385925297,-1.18802223952348,-1.18557993324279,
-1.17023199432998,-1.13482311869531,-1.06576464974758,-1.05453164154305,
-1.05172575296958,-1.04990779043298,-1.04569784063563,-1.04526278381138,
-1.0434941167533,-1.04147447029399,-1.03107390752925,-1.0296914158473,-1.02898021464825,
-1.02845388991006,-1.02787763998223,-1.02709024401996,-1.02525195861575,
-1.02272156276118,-1.01627201777475,-0.991647314633338,-0.943471253523264,
-0.87419101170161,-0.86979847852409,-0.868156561251958,-0.867187678760253,
-0.866274382593825,-0.865007614322277,-0.862491927153914,-0.848277472618057,
-0.829682272329004,-0.795526610535457,-0.749605233450531,-0.721912434360655,
-0.70833121763364,-0.7066958769758,-0.70600872976013,-0.705436304376229,
-0.704843552490359,-0.704244592522621,-0.702570163952914,-0.686510926297019,
-0.673230566397562,-0.661737441512864),.UNSPECIFIED.);
#280=B_SPLINE_CURVE_WITH_KNOTS('',3,(#49471,#49472,#49473,#49474,#49475,
#49476,#49477,#49478,#49479,#49480,#49481,#49482,#49483,#49484,#49485,#49486,
#49487,#49488,#49489,#49490,#49491,#49492,#49493,#49494,#49495,#49496,#49497,
#49498,#49499,#49500,#49501,#49502,#49503,#49504,#49505,#49506,#49507,#49508,
#49509,#49510,#49511,#49512,#49513,#49514,#49515,#49516,#49517,#49518,#49519,
#49520,#49521,#49522,#49523,#49524,#49525,#49526,#49527,#49528,#49529,#49530,
#49531,#49532,#49533,#49534,#49535,#49536,#49537,#49538,#49539,#49540,#49541,
#49542,#49543,#49544,#49545,#49546,#49547,#49548,#49549,#49550,#49551,#49552,
#49553,#49554,#49555,#49556,#49557,#49558,#49559,#49560,#49561,#49562,#49563,
#49564,#49565,#49566,#49567,#49568,#49569,#49570,#49571,#49572,#49573,#49574,
#49575,#49576,#49577,#49578,#49579,#49580,#49581,#49582,#49583,#49584,#49585,
#49586,#49587,#49588,#49589,#49590,#49591,#49592,#49593,#49594,#49595,#49596,
#49597,#49598,#49599,#49600,#49601,#49602,#49603,#49604,#49605,#49606,#49607,
#49608,#49609,#49610,#49611,#49612,#49613,#49614,#49615,#49616,#49617,#49618,
#49619,#49620,#49621,#49622,#49623,#49624,#49625,#49626,#49627,#49628,#49629,
#49630,#49631,#49632,#49633,#49634,#49635,#49636,#49637,#49638,#49639,#49640,
#49641,#49642,#49643,#49644,#49645,#49646,#49647,#49648,#49649,#49650,#49651,
#49652,#49653,#49654,#49655,#49656,#49657,#49658,#49659,#49660,#49661,#49662,
#49663,#49664,#49665,#49666,#49667,#49668,#49669,#49670,#49671,#49672,#49673,
#49674,#49675,#49676,#49677,#49678,#49679,#49680,#49681,#49682,#49683,#49684,
#49685,#49686,#49687,#49688,#49689,#49690,#49691,#49692,#49693,#49694,#49695,
#49696,#49697,#49698,#49699,#49700,#49701,#49702,#49703,#49704,#49705,#49706,
#49707,#49708,#49709,#49710,#49711,#49712,#49713,#49714,#49715,#49716,#49717,
#49718,#49719,#49720,#49721,#49722,#49723,#49724,#49725,#49726,#49727,#49728,
#49729,#49730,#49731,#49732,#49733,#49734,#49735,#49736,#49737,#49738,#49739,
#49740,#49741,#49742,#49743,#49744,#49745,#49746,#49747,#49748,#49749,#49750,
#49751,#49752,#49753,#49754,#49755,#49756,#49757,#49758,#49759,#49760),
 .UNSPECIFIED.,.F.,.F.,(4,2,2,2,2,2,2,2,2,2,2,2,2,2,2,2,2,2,2,2,2,2,2,2,
2,2,2,2,2,2,2,2,2,2,2,2,2,2,2,2,2,2,2,2,2,2,2,2,2,2,2,2,2,2,2,2,2,2,2,2,
2,2,2,2,2,2,2,2,2,2,2,2,2,2,2,2,2,2,2,2,2,2,2,2,2,2,2,2,2,2,2,2,2,2,2,2,
2,2,2,2,2,2,2,2,2,2,2,2,2,2,2,2,2,2,2,2,2,2,2,2,2,2,2,2,2,2,2,2,2,2,2,2,
2,2,2,2,2,2,2,2,2,2,2,2,4),(-3.39933093202269,-3.37192198667737,-3.34555669939565,
-3.33656741287575,-3.33085434678425,-3.32954715876053,-3.32831814166208,
-3.32741003340446,-3.32642544409237,-3.32500147328314,-3.32097765256483,
-3.25608502982255,-3.20763744545644,-3.18876498070904,-3.16966887255641,
-3.16766495064862,-3.16703165411933,-3.1664158000156,-3.16584890998672,
-3.16511169560703,-3.16350714531025,-3.15137772444024,-3.15019968139962,
-3.1495584970972,-3.14912169980331,-3.14833936930078,-3.14688098146186,
-3.1434594199651,-3.11133797412728,-3.04912620331292,-3.0346819883484,-3.00991267076312,
-3.00708486451187,-3.00574159691272,-3.00472391142747,-3.0037630332796,
-3.0024259410061,-2.99895763695626,-2.94491069838879,-2.8839406110529,-2.85784052800934,
-2.84606905885733,-2.84460458268249,-2.84388073922162,-2.84336971631137,
-2.84283170168635,-2.84207527354128,-2.84007473352634,-2.80781205622302,
-2.74465182173471,-2.70340576480221,-2.68729556970097,-2.68434059223959,
-2.68297088216897,-2.68194898125437,-2.68099559361925,-2.67968695080073,
-2.67638859904298,-2.63536793261566,-2.60759610125953,-2.52602947581608,
-2.5224403278124,-2.52142100233404,-2.52079395768511,-2.52023007006467,
-2.51950251754791,-2.51798948763603,-2.50808226364076,-2.44483239826897,
-2.39929628029919,-2.36779597278997,-2.36414698181158,-2.36141352378903,
-2.3600620797709,-2.35904303963629,-2.35808444191119,-2.3567561905675,-2.35334176492262,
-2.30435529145259,-2.27766751052459,-2.22533734471887,-2.20304516325834,
-2.19957465058036,-2.19856508039139,-2.19794489736446,-2.19737925953787,
-2.1966507764747,-2.19545020276176,-2.19091826658226,-2.09747291938542,
-2.06215084063773,-2.04087387003158,-2.03829155567975,-2.03701157738786,
-2.0360966803647,-2.03513337386174,-2.03378726759814,-2.031033219116,-1.98038202712003,
-1.8876861202532,-1.87742622297775,-1.87589726717593,-1.87517437624013,
-1.87460948754367,-1.87398633475508,-1.87296366286417,-1.86936772705566,
-1.78782010630006,-1.74261155588595,-1.73846423448186,-1.73533475790599,
-1.73264165982437,-1.73062221889132,-1.73016494516652,-1.72810240212397,
-1.72628919413808,-1.71870939431408,-1.71588743981392,-1.71452452662425,
-1.71355661623871,-1.71264338533304,-1.71137535790882,-1.70885229179558,
-1.69024767153786,-1.66209718108382,-1.56647665098842,-1.5545092071133,
-1.55291039753953,-1.5521741179042,-1.5516072198842,-1.55099060811522,-1.55001729567529,
-1.54685757238908,-1.49466855338194,-1.42247621071353,-1.41477893170555,
-1.39516709891951,-1.39265453294616,-1.39136917882915,-1.39042161353809,
-1.38939527015229,-1.38800075739516,-1.38481831589471,-1.38055397574252,
-1.36992344699479),.UNSPECIFIED.);
#281=B_SPLINE_CURVE_WITH_KNOTS('',3,(#49762,#49763,#49764,#49765,#49766,
#49767,#49768,#49769,#49770,#49771,#49772,#49773,#49774,#49775,#49776,#49777,
#49778,#49779,#49780,#49781,#49782,#49783,#49784,#49785,#49786,#49787,#49788,
#49789,#49790,#49791,#49792,#49793,#49794,#49795,#49796,#49797,#49798,#49799,
#49800,#49801,#49802,#49803,#49804,#49805,#49806,#49807,#49808,#49809,#49810,
#49811,#49812,#49813,#49814,#49815,#49816,#49817,#49818,#49819,#49820,#49821,
#49822,#49823,#49824,#49825,#49826,#49827,#49828,#49829,#49830,#49831,#49832,
#49833,#49834,#49835,#49836,#49837,#49838,#49839,#49840,#49841,#49842,#49843,
#49844,#49845,#49846,#49847,#49848,#49849,#49850,#49851,#49852,#49853,#49854,
#49855,#49856,#49857,#49858,#49859,#49860,#49861,#49862,#49863,#49864,#49865,
#49866,#49867,#49868,#49869,#49870,#49871),.UNSPECIFIED.,.F.,.F.,(4,2,2,
2,2,2,2,2,2,2,2,2,2,2,2,2,2,2,2,2,2,2,2,2,2,2,2,2,2,2,2,2,2,2,2,2,2,2,2,
2,2,2,2,2,2,2,2,2,2,2,2,2,2,2,4),(-0.661737441512864,-0.633222867219186,
-0.552295341085543,-0.5470940973112,-0.54533405193584,-0.544341694208613,
-0.543434672279343,-0.542219387795267,-0.539949171077573,-0.527667983114906,
-0.443085223762492,-0.423299550443007,-0.406769898725888,-0.402909764926324,
-0.40166206152074,-0.385418117027195,-0.383853040257971,-0.383095921295719,
-0.382557565193185,-0.382046345475579,-0.381498197152693,-0.380792463753194,
-0.377943262255727,-0.373541880672581,-0.359854716308531,-0.337183918662043,
-0.316966016825565,-0.285254450557795,-0.227493595042903,-0.223676619841762,
-0.222283506076079,-0.221307147094467,-0.220396296814355,-0.219147698643439,
-0.216720038907084,-0.201636398544457,-0.172564307606687,-0.143837926692173,
-0.131165460430137,-0.124661871041258,-0.117035008391087,-0.0713093049919375,
-0.0701815573747394,-0.0686406194917836,-0.0662570601790751,-0.0636784513378337,
-0.0611606696905414,-0.0602355252090651,-0.059694050841081,-0.0591841257063379,
-0.0586384187966496,-0.05794023835713,-0.056859184314074,-0.0548314519699521,
-0.000961045134699609),.UNSPECIFIED.);
#282=B_SPLINE_CURVE_WITH_KNOTS('',3,(#49872,#49873,#49874,#49875,#49876,
#49877,#49878,#49879,#49880,#49881,#49882,#49883,#49884,#49885,#49886,#49887,
#49888,#49889,#49890,#49891,#49892,#49893,#49894,#49895,#49896,#49897,#49898,
#49899,#49900,#49901,#49902,#49903,#49904,#49905,#49906,#49907,#49908,#49909,
#49910,#49911,#49912,#49913,#49914,#49915,#49916,#49917,#49918,#49919,#49920,
#49921,#49922,#49923,#49924,#49925,#49926,#49927,#49928,#49929,#49930,#49931,
#49932,#49933,#49934,#49935,#49936,#49937,#49938,#49939,#49940,#49941,#49942,
#49943,#49944,#49945,#49946,#49947,#49948,#49949,#49950,#49951,#49952,#49953,
#49954,#49955,#49956,#49957,#49958,#49959,#49960,#49961,#49962,#49963,#49964,
#49965,#49966,#49967,#49968,#49969,#49970,#49971,#49972,#49973,#49974,#49975,
#49976,#49977,#49978,#49979,#49980,#49981,#49982,#49983,#49984,#49985,#49986,
#49987,#49988,#49989,#49990,#49991,#49992,#49993,#49994,#49995,#49996,#49997,
#49998,#49999,#50000,#50001,#50002,#50003,#50004,#50005,#50006,#50007,#50008,
#50009,#50010,#50011,#50012,#50013,#50014,#50015,#50016,#50017,#50018,#50019,
#50020,#50021,#50022,#50023,#50024,#50025,#50026,#50027,#50028,#50029,#50030,
#50031,#50032,#50033,#50034,#50035,#50036,#50037,#50038,#50039,#50040,#50041,
#50042,#50043,#50044,#50045,#50046,#50047,#50048,#50049,#50050,#50051,#50052,
#50053,#50054,#50055,#50056,#50057,#50058,#50059),.UNSPECIFIED.,.F.,.F.,
(4,2,2,2,2,2,2,2,2,2,2,2,2,2,2,2,2,2,2,2,2,2,2,2,2,2,2,2,2,2,2,2,2,2,2,
2,2,2,2,2,2,2,2,2,2,2,2,2,2,2,2,2,2,2,2,2,2,2,2,2,2,2,2,2,2,2,2,2,2,2,2,
2,2,2,2,2,2,2,2,2,2,2,2,2,2,2,2,2,2,2,2,2,2,4),(-4.06145248375961,-3.97227698131646,
-3.96575458039436,-3.96276577754912,-3.96037755022854,-3.95913741308972,
-3.95813165300121,-3.95712835315958,-3.95531325104445,-3.94969960193822,
-3.85707818763002,-3.83745890205865,-3.81177955682372,-3.79954551730999,
-3.79851433989304,-3.79783715127806,-3.7972979055941,-3.79679113678703,
-3.79623967881305,-3.79526418067788,-3.7924025756618,-3.7431169932631,-3.71159709513579,
-3.67510577031043,-3.65154328374339,-3.63960344985516,-3.63735150872766,
-3.63614022025778,-3.63523365786259,-3.63423929074326,-3.63246891421817,
-3.62719307134317,-3.54546048711246,-3.51954730742542,-3.49120503024035,
-3.48136954807898,-3.47614059758234,-3.47497951316494,-3.47443491034768,
-3.47392558497026,-3.47338274516004,-3.47245047712617,-3.46988524819966,
-3.42835767694418,-3.3867396155417,-3.3406605563784,-3.32504332345435,-3.31932059606169,
-3.31529515802321,-3.31376135947242,-3.31270800327187,-3.31167864965621,
-3.31044132063389,-3.30736801013771,-3.27945993694265,-3.23099597452038,
-3.18840303656109,-3.16988497079114,-3.15424909093175,-3.15252411167739,
-3.15173696962351,-3.15116083330467,-3.15063455741361,-3.14992334393174,
-3.14854060213908,-3.13206683580295,-3.12680923623964,-3.11054758627852,
-3.04052752538214,-2.99952780033866,-2.99304887730472,-2.99121038035081,
-2.99009027879397,-2.9890796273541,-2.9877898726544,-2.98516011497382,-2.96914210582708,
-2.96530442110006,-2.95999782830021,-2.95110637699093,-2.93379038461465,
-2.88251293251839,-2.83208971347903,-2.82980879653136,-2.82894872561336,
-2.82835751757514,-2.82778408380062,-2.82709285196959,-2.82536769233764,
-2.80957264370983,-2.80799096768976,-2.79990499110941,-2.71753453449011,
-2.69253084801131),.UNSPECIFIED.);
#283=B_SPLINE_CURVE_WITH_KNOTS('',3,(#50065,#50066,#50067,#50068,#50069,
#50070,#50071,#50072,#50073,#50074,#50075,#50076,#50077,#50078,#50079,#50080,
#50081,#50082,#50083,#50084,#50085,#50086,#50087,#50088,#50089,#50090,#50091,
#50092,#50093,#50094,#50095,#50096,#50097,#50098,#50099,#50100,#50101,#50102,
#50103,#50104,#50105,#50106,#50107,#50108,#50109,#50110,#50111,#50112,#50113,
#50114,#50115,#50116,#50117,#50118,#50119,#50120,#50121,#50122,#50123,#50124,
#50125,#50126,#50127,#50128,#50129,#50130,#50131,#50132,#50133,#50134,#50135,
#50136,#50137,#50138,#50139,#50140,#50141,#50142,#50143,#50144,#50145,#50146,
#50147,#50148,#50149,#50150,#50151,#50152,#50153,#50154,#50155,#50156,#50157,
#50158,#50159,#50160,#50161,#50162,#50163,#50164,#50165,#50166,#50167,#50168,
#50169,#50170,#50171,#50172,#50173,#50174,#50175,#50176,#50177,#50178,#50179,
#50180,#50181,#50182,#50183,#50184,#50185,#50186,#50187,#50188,#50189,#50190,
#50191,#50192,#50193,#50194,#50195,#50196,#50197,#50198,#50199,#50200,#50201,
#50202,#50203,#50204,#50205,#50206,#50207,#50208,#50209,#50210,#50211,#50212,
#50213,#50214,#50215,#50216,#50217,#50218,#50219,#50220,#50221,#50222,#50223,
#50224,#50225,#50226,#50227,#50228,#50229,#50230,#50231,#50232,#50233,#50234,
#50235,#50236,#50237,#50238,#50239,#50240,#50241,#50242,#50243,#50244,#50245,
#50246,#50247,#50248,#50249,#50250,#50251,#50252,#50253,#50254,#50255,#50256,
#50257,#50258,#50259,#50260,#50261,#50262,#50263,#50264),.UNSPECIFIED.,
 .F.,.F.,(4,2,2,2,2,2,2,2,2,2,2,2,2,2,2,2,2,2,2,2,2,2,2,2,2,2,2,2,2,2,2,
2,2,2,2,2,2,2,2,2,2,2,2,2,2,2,2,2,2,2,2,2,2,2,2,2,2,2,2,2,2,2,2,2,2,2,2,
2,2,2,2,2,2,2,2,2,2,2,2,2,2,2,2,2,2,2,2,2,2,2,2,2,2,2,2,2,2,2,2,4),(-1.36933436101521,
-1.36849737424044,-1.36775242609568,-1.36721734441935,-1.36664751075481,
-1.36588013452935,-1.36419258443954,-1.35105890789208,-1.32617825355882,
-1.25775072372392,-1.2115088765732,-1.20812901691825,-1.20680626804603,
-1.20584892192528,-1.20482868117506,-1.20347132772782,-1.20057710288288,
-1.17520541615952,-1.15368424802282,-1.09318886372733,-1.04867423922206,
-1.0458506686294,-1.04488069969442,-1.04433029017226,-1.04382315898495,
-1.04312869847589,-1.04180666955098,-1.03352227312986,-1.01535355381888,
-0.951112133275545,-0.88913250968735,-0.885332240925437,-0.883941753980511,
-0.882966157361079,-0.882055162289823,-0.880805039758072,-0.878434126459346,
-0.863363712164514,-0.8292129522212,-0.780958762004757,-0.752088677245505,
-0.724534427175619,-0.72259881695029,-0.721852756331595,-0.721317391230185,
-0.720747756095872,-0.719981484735029,-0.718299757207449,-0.698511197228781,
-0.679998440108996,-0.635344910659248,-0.597670822203311,-0.565288731179293,
-0.562163285035677,-0.560884222258155,-0.559938157558921,-0.558910403333568,
-0.557508548738348,-0.555962244033717,-0.545632885144771,-0.516780383488332,
-0.468069109637877,-0.413919649883421,-0.413502609402084,-0.411995167406995,
-0.401027214061324,-0.399623058129805,-0.398906297470013,-0.398378577533726,
-0.397803585514048,-0.397006706012031,-0.396120208476993,-0.3897488305053,
-0.376886358482462,-0.345393146673643,-0.318802188693085,-0.244652875726976,
-0.23984351622686,-0.2381389682103,-0.237157707338317,-0.236248270584041,
-0.235010771603775,-0.233692000152381,-0.231598889120807,-0.21489450850021,
-0.176170901662155,-0.16263152946763,-0.148937304010521,-0.0896189000749925,
-0.0894252369788815,-0.0780966960099142,-0.076522504940367,-0.0757908323711787,
-0.0752245721751104,-0.074605634802611,-0.0739680068213746,-0.0730316125793512,
-0.0713722523270497,-0.0677313842462216,-0.000961580881731712),
 .UNSPECIFIED.);
#284=B_SPLINE_CURVE_WITH_KNOTS('',3,(#50265,#50266,#50267,#50268,#50269,
#50270,#50271,#50272,#50273,#50274,#50275,#50276,#50277,#50278,#50279,#50280,
#50281,#50282,#50283,#50284,#50285,#50286,#50287,#50288,#50289,#50290,#50291,
#50292,#50293,#50294,#50295,#50296,#50297,#50298,#50299,#50300,#50301,#50302,
#50303,#50304,#50305,#50306,#50307,#50308,#50309,#50310,#50311,#50312,#50313,
#50314,#50315,#50316,#50317,#50318,#50319,#50320,#50321,#50322,#50323,#50324,
#50325,#50326,#50327,#50328,#50329,#50330,#50331,#50332,#50333,#50334,#50335,
#50336,#50337,#50338,#50339,#50340,#50341,#50342,#50343,#50344,#50345,#50346,
#50347,#50348,#50349,#50350,#50351,#50352,#50353,#50354,#50355,#50356),
 .UNSPECIFIED.,.F.,.F.,(4,2,2,2,2,2,2,2,2,2,2,2,2,2,2,2,2,2,2,2,2,2,2,2,
2,2,2,2,2,2,2,2,2,2,2,2,2,2,2,2,2,2,2,2,2,4),(-4.06038694981303,-3.99311640574062,
-3.97853380020269,-3.97646565463749,-3.97515763148088,-3.9739280367631,
-3.97301993142903,-3.97203576334703,-3.97031490080506,-3.96538869257994,
-3.88768691103398,-3.87427744171466,-3.86147278894616,-3.82817857312513,
-3.81453214875378,-3.81347329767406,-3.81278458238728,-3.81212973769813,
-3.81162590216822,-3.81105199342522,-3.8099644426968,-3.80619378809069,
-3.74411185386278,-3.72381521715483,-3.70363940834911,-3.66978256971005,
-3.65990787219642,-3.65376312553043,-3.65242697435233,-3.65117705592305,
-3.65026645682214,-3.64929151893622,-3.64761713769636,-3.6430088738072,
-3.56858088678463,-3.52192994391434,-3.49251801522111,-3.49046629297178,
-3.48983092158467,-3.48921363645748,-3.48864722699388,-3.48791309633718,
-3.48632485137972,-3.4746228878599,-3.42502489138987,-3.39933093202269),
 .UNSPECIFIED.);
#285=B_SPLINE_CURVE_WITH_KNOTS('',3,(#50357,#50358,#50359,#50360,#50361,
#50362,#50363,#50364,#50365,#50366,#50367,#50368,#50369,#50370,#50371,#50372,
#50373,#50374,#50375,#50376,#50377,#50378,#50379,#50380,#50381,#50382,#50383,
#50384,#50385,#50386,#50387,#50388,#50389,#50390,#50391,#50392,#50393,#50394,
#50395,#50396,#50397,#50398,#50399,#50400,#50401,#50402,#50403,#50404,#50405,
#50406,#50407,#50408,#50409,#50410,#50411,#50412,#50413,#50414,#50415,#50416,
#50417,#50418,#50419,#50420,#50421,#50422,#50423,#50424,#50425,#50426,#50427,
#50428,#50429,#50430,#50431,#50432,#50433,#50434,#50435,#50436,#50437,#50438,
#50439,#50440,#50441,#50442,#50443,#50444,#50445,#50446,#50447,#50448,#50449,
#50450,#50451,#50452,#50453,#50454,#50455,#50456,#50457,#50458,#50459,#50460,
#50461,#50462,#50463,#50464,#50465,#50466,#50467,#50468,#50469,#50470,#50471,
#50472,#50473,#50474,#50475,#50476,#50477,#50478,#50479,#50480,#50481,#50482,
#50483,#50484,#50485,#50486,#50487,#50488,#50489,#50490,#50491,#50492,#50493,
#50494,#50495,#50496,#50497,#50498,#50499,#50500,#50501,#50502,#50503,#50504,
#50505,#50506,#50507,#50508,#50509,#50510,#50511,#50512,#50513,#50514,#50515,
#50516,#50517,#50518,#50519,#50520,#50521,#50522,#50523,#50524,#50525,#50526,
#50527,#50528,#50529,#50530,#50531,#50532,#50533,#50534,#50535,#50536,#50537,
#50538,#50539,#50540,#50541,#50542,#50543,#50544,#50545,#50546,#50547,#50548,
#50549,#50550,#50551,#50552,#50553,#50554,#50555,#50556,#50557,#50558,#50559,
#50560,#50561,#50562,#50563,#50564,#50565,#50566,#50567,#50568,#50569,#50570,
#50571,#50572,#50573,#50574,#50575,#50576,#50577,#50578,#50579,#50580,#50581,
#50582,#50583,#50584,#50585,#50586,#50587,#50588,#50589,#50590,#50591,#50592,
#50593,#50594,#50595,#50596,#50597,#50598,#50599,#50600,#50601,#50602,#50603,
#50604,#50605,#50606,#50607,#50608,#50609,#50610,#50611,#50612,#50613,#50614,
#50615,#50616,#50617,#50618,#50619,#50620,#50621,#50622,#50623,#50624,#50625,
#50626,#50627,#50628,#50629,#50630,#50631,#50632,#50633,#50634,#50635,#50636,
#50637,#50638),.UNSPECIFIED.,.F.,.F.,(4,2,2,2,2,2,2,2,2,2,2,2,2,2,2,2,2,
2,2,2,2,2,2,2,2,2,2,2,2,2,2,2,2,2,2,2,2,2,2,2,2,2,2,2,2,2,2,2,2,2,2,2,2,
2,2,2,2,2,2,2,2,2,2,2,2,2,2,2,2,2,2,2,2,2,2,2,2,2,2,2,2,2,2,2,2,2,2,2,2,
2,2,2,2,2,2,2,2,2,2,2,2,2,2,2,2,2,2,2,2,2,2,2,2,2,2,2,2,2,2,2,2,2,2,2,2,
2,2,2,2,2,2,2,2,2,2,2,2,2,2,2,4),(-2.69253084801131,-2.67659534086741,-2.67233115381611,
-2.66914873035905,-2.66775423401712,-2.6667279059203,-2.66578035629344,
-2.66449502550178,-2.66198250514788,-2.64237064541017,-2.63611734293786,
-2.62852150405745,-2.55863568053625,-2.51029591885371,-2.50709994609254,
-2.50612261201985,-2.50550508180648,-2.50493847869591,-2.50420413911534,
-2.50261560536728,-2.49091658965511,-2.42591608132343,-2.3817727875377,
-2.36129451684806,-2.34805899146598,-2.34575399205254,-2.34453134974085,
-2.34352652472138,-2.34251296128512,-2.3406473363834,-2.33463333419885,
-2.33319821706952,-2.32967900537661,-2.32824391131659,-2.23138521974221,
-2.18908152713744,-2.18434026469069,-2.1832151305322,-2.18256897880751,
-2.18200785859457,-2.18130985881933,-2.18023489535017,-2.17539990948672,
-2.08099343976646,-2.03138589052011,-2.02433449292952,-2.02237361535553,
-2.02121468562102,-2.02030991772038,-2.01912257097719,-2.01698133034504,
-2.00673403734971,-1.98740923246788,-1.96358538548088,-1.87442151254333,
-1.87290868157109,-1.86194672644113,-1.86054274605871,-1.85982601287126,
-1.85929828292596,-1.85872324884482,-1.85792625575665,-1.85603721608547,
-1.82066310716825,-1.71630543227848,-1.71564846989638,-1.71169838331268,
-1.70798984609041,-1.701130938443,-1.69916754919025,-1.69801950643693,-1.6970228349678,
-1.695782161338,-1.6936019133816,-1.69080170718674,-1.63172767613707,-1.55081761589049,
-1.5491636131825,-1.53874922309969,-1.53736623731261,-1.53665492620697,
-1.53612859101639,-1.53555240277751,-1.53474907888718,-1.53295087629794,
-1.53044950023309,-1.44169627237407,-1.38095680560618,-1.37717223247484,
-1.37578421655003,-1.37480933252135,-1.37389819093343,-1.37264660712492,
-1.37025296011532,-1.35600421121596,-1.32489912865048,-1.25821387302968,
-1.21701056136886,-1.2146020085772,-1.21378445093403,-1.21322938489348,
-1.21272329831184,-1.21203817763839,-1.21075961171867,-1.20347094815355,
-1.18818676320163,-1.16657696981207,-1.10568884124944,-1.08473325258402,
-1.05693412234813,-1.05386371607299,-1.0526268313482,-1.05159755851101,
-1.05054399100491,-1.04948791492806,-1.0466723966505,-1.02329703124528,
-1.00102766028182,-0.947179847137763,-0.901764928424828,-0.90109051379113,
-0.892679008728169,-0.891257475013047,-0.890538311895011,-0.889975253252021,
-0.889343101459854,-0.888686548103145,-0.886435297840818,-0.866468984714367,
-0.846571013924919,-0.796071607600607,-0.7351475487337,-0.73136564627348,
-0.729978010019495,-0.72900320518696,-0.728091988463089,-0.726840069756809,
-0.724444985742037,-0.708916508483105,-0.689335332262786,-0.662385834278714),
 .UNSPECIFIED.);
#286=B_SPLINE_CURVE_WITH_KNOTS('',3,(#50643,#50644,#50645,#50646,#50647,
#50648,#50649,#50650,#50651,#50652,#50653,#50654,#50655,#50656,#50657,#50658,
#50659,#50660,#50661,#50662,#50663,#50664,#50665,#50666,#50667,#50668,#50669,
#50670,#50671,#50672,#50673,#50674,#50675,#50676,#50677,#50678,#50679,#50680,
#50681,#50682,#50683,#50684,#50685,#50686,#50687,#50688,#50689,#50690,#50691,
#50692,#50693,#50694,#50695,#50696,#50697,#50698,#50699,#50700,#50701,#50702,
#50703,#50704,#50705,#50706,#50707,#50708,#50709,#50710,#50711,#50712,#50713,
#50714,#50715,#50716,#50717,#50718,#50719,#50720,#50721,#50722,#50723,#50724,
#50725,#50726,#50727,#50728,#50729,#50730,#50731,#50732,#50733,#50734,#50735,
#50736,#50737,#50738,#50739,#50740,#50741,#50742,#50743,#50744,#50745,#50746,
#50747,#50748,#50749,#50750,#50751,#50752,#50753,#50754,#50755,#50756,#50757,
#50758,#50759,#50760,#50761,#50762,#50763,#50764,#50765,#50766,#50767,#50768,
#50769,#50770,#50771,#50772,#50773,#50774,#50775,#50776,#50777,#50778,#50779,
#50780,#50781,#50782,#50783,#50784,#50785,#50786,#50787,#50788,#50789,#50790,
#50791,#50792,#50793,#50794,#50795,#50796,#50797,#50798,#50799,#50800,#50801,
#50802,#50803,#50804,#50805,#50806,#50807,#50808,#50809,#50810,#50811,#50812,
#50813,#50814,#50815,#50816,#50817,#50818,#50819,#50820,#50821,#50822,#50823,
#50824,#50825,#50826,#50827,#50828,#50829,#50830,#50831,#50832,#50833,#50834,
#50835,#50836,#50837,#50838,#50839,#50840,#50841,#50842,#50843,#50844,#50845,
#50846,#50847,#50848,#50849,#50850,#50851,#50852,#50853,#50854,#50855,#50856,
#50857,#50858,#50859,#50860,#50861,#50862,#50863,#50864,#50865,#50866,#50867,
#50868,#50869,#50870,#50871,#50872,#50873,#50874,#50875,#50876,#50877,#50878,
#50879,#50880,#50881,#50882,#50883,#50884,#50885,#50886,#50887,#50888,#50889,
#50890,#50891,#50892,#50893,#50894,#50895,#50896,#50897,#50898,#50899,#50900,
#50901,#50902,#50903,#50904,#50905,#50906,#50907,#50908,#50909,#50910,#50911,
#50912,#50913,#50914),.UNSPECIFIED.,.F.,.F.,(4,2,2,2,2,2,2,2,2,2,2,2,2,
2,2,2,2,2,2,2,2,2,2,2,2,2,2,2,2,2,2,2,2,2,2,2,2,2,2,2,2,2,2,2,2,2,2,2,2,
2,2,2,2,2,2,2,2,2,2,2,2,2,2,2,2,2,2,2,2,2,2,2,2,2,2,2,2,2,2,2,2,2,2,2,2,
2,2,2,2,2,2,2,2,2,2,2,2,2,2,2,2,2,2,2,2,2,2,2,2,2,2,2,2,2,2,2,2,2,2,2,2,
2,2,2,2,2,2,2,2,2,2,2,2,2,2,4),(-3.39926360491999,-3.37688241372124,-3.33085573661026,
-3.31010026402408,-3.30677728275198,-3.30578369970508,-3.30516714426549,
-3.30460048952005,-3.30386478859867,-3.30226826225606,-3.2903558594644,
-3.22820951070095,-3.18531822881361,-3.16057808733654,-3.15216052732146,
-3.14673164470306,-3.14507118593755,-3.14397477139313,-3.14296430139436,
-3.14167364520367,-3.13903810015613,-3.12289522043311,-3.11735249035576,
-3.03665523616719,-2.98532150665199,-2.98347087261955,-2.98268073535315,
-2.98210713837037,-2.98157816748161,-2.98085601297705,-2.97943022933864,
-2.96785273615781,-2.91813389651933,-2.86174859280646,-2.82946421244397,
-2.82576099653129,-2.82379112754816,-2.822106214782,-2.82103043473098,-2.82001412530571,
-2.81870288412083,-2.81589032349568,-2.80788806142458,-2.80603099107828,
-2.80397428507211,-2.80362661398097,-2.80265129205505,-2.80058279536987,
-2.79896228960569,-2.79775909773326,-2.79644032308168,-2.79026173475653,
-2.78256660812256,-2.72096822484289,-2.66613193654551,-2.66134527932127,
-2.66021689139954,-2.65957015969599,-2.65900931932337,-2.65831267132758,
-2.65724163125085,-2.6524523304737,-2.56586679466431,-2.50461836890784,
-2.50185387630215,-2.49963206463485,-2.49843421343516,-2.49742967552889,
-2.49641649826985,-2.49455186309526,-2.48854325080575,-2.38667680144655,
-2.33921581585797,-2.33748919651981,-2.33672111684828,-2.33615128429757,
-2.33561659838711,-2.33487280320976,-2.33295033390937,-2.30620406550764,
-2.21642171974538,-2.19165711740084,-2.17884348180368,-2.1765591866997,
-2.1753411230007,-2.17433671914366,-2.17332073123874,-2.17144236764913,
-2.16532128625365,-2.05773018496375,-2.03039004660336,-2.02972520199299,
-2.01600240165622,-2.0145066996429,-2.01376681935515,-2.01323313997103,
-2.01266261119445,-2.01189060958376,-2.01014264259688,-1.9697475378102,
-1.92491581213147,-1.88398118915712,-1.87617677930896,-1.8746832707421,
-1.87347293732362,-1.87221695572504,-1.85636444688795,-1.8537430315984,
-1.85245495788034,-1.85144451410148,-1.85032350200536,-1.84848090412271,
-1.84196143920366,-1.80051823707967,-1.70660310011969,-1.69300732646376,
-1.69137148575494,-1.69068424211526,-1.69011178515086,-1.68951905390723,
-1.68863447933368,-1.68624245150182,-1.64728549390265,-1.56130865834456,
-1.53391875099285,-1.53116564128081,-1.52981951327835,-1.52885597214535,
-1.52794067287848,-1.5266598426789,-1.52412640537889,-1.50778165212095,
-1.46816929180748,-1.39754399467805,-1.37042613031333,-1.36933436101521),
 .UNSPECIFIED.);
#287=B_SPLINE_CURVE_WITH_KNOTS('',3,(#50916,#50917,#50918,#50919,#50920,
#50921,#50922,#50923,#50924,#50925,#50926,#50927,#50928,#50929,#50930,#50931,
#50932,#50933,#50934,#50935,#50936,#50937,#50938,#50939,#50940,#50941,#50942,
#50943,#50944,#50945,#50946,#50947,#50948,#50949,#50950,#50951,#50952,#50953,
#50954,#50955,#50956,#50957,#50958,#50959,#50960,#50961,#50962,#50963,#50964,
#50965,#50966,#50967,#50968,#50969,#50970,#50971,#50972,#50973,#50974,#50975,
#50976,#50977,#50978,#50979,#50980,#50981,#50982,#50983,#50984,#50985,#50986,
#50987,#50988,#50989,#50990,#50991,#50992,#50993,#50994,#50995,#50996,#50997,
#50998,#50999,#51000,#51001,#51002,#51003),.UNSPECIFIED.,.F.,.F.,(4,2,2,
2,2,2,2,2,2,2,2,2,2,2,2,2,2,2,2,2,2,2,2,2,2,2,2,2,2,2,2,2,2,2,2,2,2,2,2,
2,2,2,2,4),(-0.662385834278714,-0.6362356243194,-0.572935159665514,-0.569148678402942,
-0.568059012042635,-0.567484485895362,-0.566980387874265,-0.566325587197284,
-0.565637065068376,-0.563004150181575,-0.532566945138726,-0.482984349394012,
-0.413161376047426,-0.408659520818866,-0.407000823382457,-0.406028669866761,
-0.405116581895032,-0.403858231629967,-0.402510593401049,-0.396194179924321,
-0.385961775075733,-0.350101223734935,-0.319129754774269,-0.250344510590648,
-0.246247922402608,-0.245138258140834,-0.24448901178997,-0.243984276130349,
-0.243315621913099,-0.242607710623799,-0.241503487429798,-0.227797881617593,
-0.191841775006461,-0.177979160749078,-0.163556726548981,-0.0902301732190564,
-0.0857084764994424,-0.0840467208243449,-0.0830739458307767,-0.0821620295674787,
-0.0809050969223434,-0.0795594306801829,-0.0774023951194937,-0.000961434712091559),
 .UNSPECIFIED.);
#288=B_SPLINE_CURVE_WITH_KNOTS('',3,(#51004,#51005,#51006,#51007,#51008,
#51009,#51010,#51011,#51012,#51013,#51014,#51015,#51016,#51017,#51018,#51019,
#51020,#51021,#51022,#51023,#51024,#51025,#51026,#51027,#51028,#51029,#51030,
#51031,#51032,#51033,#51034,#51035,#51036,#51037,#51038,#51039,#51040,#51041,
#51042,#51043,#51044,#51045,#51046,#51047,#51048,#51049,#51050,#51051,#51052,
#51053,#51054,#51055,#51056,#51057,#51058,#51059,#51060,#51061,#51062,#51063,
#51064,#51065,#51066,#51067,#51068,#51069,#51070,#51071,#51072,#51073,#51074,
#51075,#51076,#51077,#51078,#51079,#51080,#51081,#51082,#51083,#51084,#51085,
#51086,#51087,#51088,#51089,#51090,#51091,#51092,#51093,#51094,#51095,#51096,
#51097,#51098,#51099,#51100,#51101,#51102,#51103,#51104,#51105,#51106,#51107,
#51108,#51109,#51110,#51111,#51112,#51113,#51114,#51115,#51116,#51117,#51118,
#51119,#51120,#51121,#51122,#51123,#51124,#51125,#51126,#51127,#51128,#51129,
#51130,#51131,#51132,#51133,#51134,#51135,#51136,#51137,#51138,#51139,#51140,
#51141,#51142,#51143,#51144,#51145,#51146,#51147,#51148,#51149,#51150,#51151,
#51152,#51153,#51154,#51155,#51156,#51157,#51158,#51159,#51160,#51161,#51162,
#51163,#51164,#51165,#51166,#51167,#51168,#51169,#51170,#51171,#51172,#51173,
#51174,#51175,#51176,#51177,#51178,#51179,#51180,#51181,#51182,#51183,#51184,
#51185,#51186,#51187,#51188,#51189,#51190,#51191,#51192,#51193,#51194,#51195,
#51196,#51197,#51198,#51199,#51200,#51201,#51202,#51203,#51204,#51205,#51206,
#51207),.UNSPECIFIED.,.F.,.F.,(4,2,2,2,2,2,2,2,2,2,2,2,2,2,2,2,2,2,2,2,
2,2,2,2,2,2,2,2,2,2,2,2,2,2,2,2,2,2,2,2,2,2,2,2,2,2,2,2,2,2,2,2,2,2,2,2,
2,2,2,2,2,2,2,2,2,2,2,2,2,2,2,2,2,2,2,2,2,2,2,2,2,2,2,2,2,2,2,2,2,2,2,2,
2,2,2,2,2,2,2,2,2,4),(-4.06003779901135,-3.99247556607899,-3.98327642325354,
-3.98208888839531,-3.98134609672055,-3.98065245603443,-3.98014552290343,
-3.9795949306341,-3.97862362860304,-3.97579052428501,-3.93036375229143,
-3.90194261785647,-3.8890182780983,-3.87655885592633,-3.84124223908723,
-3.82447698249938,-3.82227339468324,-3.82090826587115,-3.81963730940153,
-3.81872357918545,-3.81775662978758,-3.8161238148827,-3.81178792007458,
-3.74248608791876,-3.71631051501777,-3.68854256132202,-3.66846246694046,
-3.66275864953244,-3.65927967300459,-3.6585299818593,-3.65783137461025,
-3.6572703191131,-3.65662485749805,-3.65553104185684,-3.651585727485,-3.58310780442706,
-3.53581135400636,-3.50541525174032,-3.49928585799241,-3.49795071432104,
-3.4967014360209,-3.49579068843143,-3.49481500812085,-3.49342381552868,
-3.48961800283801,-3.42950415014912,-3.39384110001399,-3.3599735440906,
-3.34473815102985,-3.33957445804294,-3.3363507935214,-3.3356181468158,-3.33493179506936,
-3.33437149984588,-3.33380251675499,-3.33274000228331,-3.32919097722671,
-3.27127493342399,-3.22503303473745,-3.19218976146052,-3.17745427151142,
-3.17509716129976,-3.17385011450039,-3.17293965334823,-3.1719630053122,
-3.17056829007569,-3.16673954333308,-3.10865322532429,-3.03993717606383,
-3.02229796519031,-3.01406910841555,-3.01274937087468,-3.01205546542262,
-3.01154846939859,-3.01099793794804,-3.01002707181006,-3.00719712643014,
-2.96305619733515,-2.90900303525728,-2.87079345129595,-2.85464749899698,
-2.85226144617692,-2.85099423460073,-2.85008100834707,-2.84911256177796,
-2.84774800496388,-2.84491974598542,-2.84232414505121,-2.83584593539642,
-2.83454804119756,-2.83406271689407,-2.83272207328595,-2.83210249487991,
-2.83002100191228,-2.82851452043185,-2.82730933543043,-2.82599193201632,
-2.81984425319159,-2.80373155241326,-2.73262190960314,-2.70560877785445,
-2.69193413772045),.UNSPECIFIED.);
#289=B_SPLINE_CURVE_WITH_KNOTS('',3,(#51213,#51214,#51215,#51216,#51217,
#51218,#51219,#51220,#51221,#51222,#51223,#51224,#51225,#51226,#51227,#51228,
#51229,#51230,#51231,#51232,#51233,#51234,#51235,#51236,#51237,#51238,#51239,
#51240,#51241,#51242,#51243,#51244,#51245,#51246,#51247,#51248,#51249,#51250,
#51251,#51252,#51253,#51254,#51255,#51256,#51257,#51258,#51259,#51260,#51261,
#51262,#51263,#51264,#51265,#51266,#51267,#51268,#51269,#51270,#51271,#51272,
#51273,#51274,#51275,#51276,#51277,#51278,#51279,#51280,#51281,#51282,#51283,
#51284,#51285,#51286,#51287,#51288,#51289,#51290,#51291,#51292,#51293,#51294,
#51295,#51296,#51297,#51298,#51299,#51300,#51301,#51302,#51303,#51304,#51305,
#51306,#51307,#51308,#51309,#51310,#51311,#51312,#51313,#51314,#51315,#51316,
#51317,#51318,#51319,#51320,#51321,#51322,#51323,#51324,#51325,#51326,#51327,
#51328,#51329,#51330,#51331,#51332,#51333,#51334,#51335,#51336,#51337,#51338,
#51339,#51340,#51341,#51342,#51343,#51344,#51345,#51346,#51347,#51348,#51349,
#51350,#51351,#51352,#51353,#51354,#51355,#51356,#51357,#51358,#51359,#51360,
#51361,#51362,#51363,#51364,#51365,#51366,#51367,#51368,#51369,#51370,#51371,
#51372,#51373,#51374,#51375,#51376,#51377,#51378,#51379,#51380,#51381,#51382,
#51383,#51384,#51385,#51386,#51387,#51388,#51389,#51390,#51391,#51392,#51393,
#51394,#51395,#51396,#51397,#51398,#51399,#51400,#51401,#51402,#51403,#51404,
#51405,#51406,#51407,#51408,#51409,#51410,#51411,#51412,#51413,#51414,#51415,
#51416,#51417,#51418,#51419,#51420,#51421,#51422,#51423,#51424,#51425,#51426,
#51427,#51428,#51429,#51430,#51431,#51432,#51433,#51434,#51435,#51436,#51437,
#51438,#51439,#51440,#51441,#51442,#51443,#51444,#51445,#51446),
 .UNSPECIFIED.,.F.,.F.,(4,2,2,2,2,2,2,2,2,2,2,2,2,2,2,2,2,2,2,2,2,2,2,2,
2,2,2,2,2,2,2,2,2,2,2,2,2,2,2,2,2,2,2,2,2,2,2,2,2,2,2,2,2,2,2,2,2,2,2,2,
2,2,2,2,2,2,2,2,2,2,2,2,2,2,2,2,2,2,2,2,2,2,2,2,2,2,2,2,2,2,2,2,2,2,2,2,
2,2,2,2,2,2,2,2,2,2,2,2,2,2,2,2,2,2,2,2,4),(-1.36972866115331,-1.35430997194401,
-1.34824564483208,-1.3463740748379,-1.34535941941148,-1.3443548579261,-1.34315921423531,
-1.34094750382271,-1.33819824590719,-1.30755377187864,-1.24482795670056,
-1.18871876451973,-1.18528938116151,-1.18424106017695,-1.18367494902106,
-1.18311441967272,-1.18242333485335,-1.18108988449808,-1.17261141508242,
-1.15321542119109,-1.10725524971504,-1.08816458999835,-1.02832567851039,
-1.02464529336729,-1.02327378458777,-1.02230350597661,-1.02139105455907,
-1.02015430931416,-1.01775710142411,-1.01472024774376,-1.00805610257389,
-0.988895949462919,-0.936479395883524,-0.889634430730174,-0.863873931128287,
-0.861967648233763,-0.861226542788088,-0.860692564459935,-0.860122288233946,
-0.859351593287961,-0.857610646815456,-0.798810394935583,-0.736376151537241,
-0.726177069204377,-0.721845007348821,-0.720607127498751,-0.719591456642548,
-0.716275734628755,-0.715959719896745,-0.713927816557707,-0.711758767888483,
-0.703007404921325,-0.701072580514405,-0.699817149858467,-0.698810168581269,
-0.697864975882884,-0.696172878102653,-0.690960368653594,-0.68296913169701,
-0.65889523211027,-0.623738112729008,-0.544101845241873,-0.539706736579721,
-0.538567489342269,-0.537911436083862,-0.537356528611114,-0.536673868668313,
-0.535380527024604,-0.527834103198571,-0.512107466612118,-0.487307428114523,
-0.480047917714727,-0.473886023098427,-0.468551835964313,-0.423129430094186,
-0.406241631322227,-0.400629073897618,-0.399308419013051,-0.398103093096133,
-0.396621153826891,-0.394536539994629,-0.393952577968948,-0.392230805156151,
-0.391239845868998,-0.388424203790562,-0.380359797592356,-0.378305904868506,
-0.377013593761457,-0.376002636694435,-0.375059986445843,-0.373962860224534,
-0.370744318807546,-0.366379415448304,-0.355529411918452,-0.340986550386828,
-0.31516807346096,-0.229282002589889,-0.217509081185714,-0.216076102678238,
-0.215351982415232,-0.214822376013614,-0.214248900941553,-0.213460338640914,
-0.211619718701249,-0.166140578246789,-0.107086394450611,-0.101230681528391,
-0.08751281178236,-0.0586609609909284,-0.0556019951975356,-0.0543461603031945,
-0.0534058746940949,-0.0524508639835445,-0.0514444330553131,-0.0501127305584683,
-0.0479889044122154,-0.000960757701424912),.UNSPECIFIED.);
#290=B_SPLINE_CURVE_WITH_KNOTS('',3,(#51447,#51448,#51449,#51450,#51451,
#51452,#51453,#51454,#51455,#51456,#51457,#51458,#51459,#51460,#51461,#51462,
#51463,#51464,#51465,#51466,#51467,#51468,#51469,#51470,#51471,#51472,#51473,
#51474,#51475,#51476,#51477,#51478,#51479,#51480,#51481,#51482,#51483,#51484,
#51485,#51486,#51487,#51488,#51489,#51490,#51491,#51492,#51493,#51494,#51495,
#51496,#51497,#51498,#51499,#51500,#51501,#51502,#51503,#51504,#51505,#51506,
#51507,#51508,#51509,#51510,#51511,#51512,#51513,#51514,#51515,#51516,#51517,
#51518,#51519,#51520,#51521,#51522,#51523,#51524,#51525,#51526,#51527,#51528,
#51529,#51530,#51531,#51532,#51533,#51534,#51535,#51536,#51537,#51538,#51539,
#51540),.UNSPECIFIED.,.F.,.F.,(4,2,2,2,2,2,2,2,2,2,2,2,2,2,2,2,2,2,2,2,
2,2,2,2,2,2,2,2,2,2,2,2,2,2,2,2,2,2,2,2,2,2,2,2,2,2,4),(-4.05994418293563,
-3.97742496221251,-3.95591745462113,-3.9525215555251,-3.95151995039704,
-3.95090154938977,-3.95033538017432,-3.94960328200121,-3.94802608413189,
-3.93661304150904,-3.93453421145722,-3.84551619506739,-3.82564574588448,
-3.79443721997479,-3.79150927338425,-3.79044126209591,-3.78950021289165,
-3.78848076094066,-3.78714953891444,-3.78433783030483,-3.76329528977208,
-3.76075139198099,-3.74413037407835,-3.71360142990771,-3.68952365920941,
-3.63466645529907,-3.62988884968352,-3.62876121806178,-3.62811468361164,
-3.62755387073336,-3.62685707313564,-3.62578546608493,-3.62098822636374,
-3.53372871152031,-3.49647925483208,-3.47947062628942,-3.47337348946682,
-3.46916689058546,-3.46760843225411,-3.46666742301656,-3.46565026235607,
-3.4643330366156,-3.46148858414917,-3.440538193069,-3.4383865921133,-3.43013952628577,
-3.39926360491999),.UNSPECIFIED.);
#291=B_SPLINE_CURVE_WITH_KNOTS('',3,(#51541,#51542,#51543,#51544,#51545,
#51546,#51547,#51548,#51549,#51550,#51551,#51552,#51553,#51554,#51555,#51556,
#51557,#51558,#51559,#51560,#51561,#51562,#51563,#51564,#51565,#51566,#51567,
#51568,#51569,#51570,#51571,#51572,#51573,#51574,#51575,#51576,#51577,#51578,
#51579,#51580,#51581,#51582,#51583,#51584,#51585,#51586,#51587,#51588,#51589,
#51590,#51591,#51592,#51593,#51594,#51595,#51596,#51597,#51598,#51599,#51600,
#51601,#51602,#51603,#51604,#51605,#51606,#51607,#51608,#51609,#51610,#51611,
#51612,#51613,#51614,#51615,#51616,#51617,#51618,#51619,#51620,#51621,#51622,
#51623,#51624,#51625,#51626,#51627,#51628,#51629,#51630,#51631,#51632,#51633,
#51634,#51635,#51636,#51637,#51638,#51639,#51640,#51641,#51642,#51643,#51644,
#51645,#51646,#51647,#51648,#51649,#51650,#51651,#51652,#51653,#51654,#51655,
#51656,#51657,#51658,#51659,#51660,#51661,#51662,#51663,#51664,#51665,#51666,
#51667,#51668,#51669,#51670,#51671,#51672,#51673,#51674,#51675,#51676,#51677,
#51678,#51679,#51680,#51681,#51682,#51683,#51684,#51685,#51686,#51687,#51688,
#51689,#51690,#51691,#51692,#51693,#51694,#51695,#51696,#51697,#51698,#51699,
#51700,#51701,#51702,#51703,#51704,#51705,#51706,#51707,#51708,#51709,#51710,
#51711,#51712,#51713,#51714,#51715,#51716,#51717,#51718,#51719,#51720,#51721,
#51722,#51723,#51724,#51725,#51726,#51727,#51728,#51729,#51730,#51731,#51732,
#51733,#51734,#51735,#51736,#51737,#51738,#51739,#51740,#51741,#51742,#51743,
#51744,#51745,#51746,#51747,#51748,#51749,#51750,#51751,#51752,#51753,#51754,
#51755,#51756,#51757,#51758,#51759,#51760,#51761,#51762,#51763,#51764,#51765,
#51766,#51767,#51768,#51769,#51770,#51771,#51772,#51773,#51774,#51775,#51776,
#51777,#51778,#51779,#51780,#51781,#51782,#51783,#51784,#51785,#51786,#51787,
#51788,#51789,#51790,#51791,#51792,#51793,#51794,#51795,#51796,#51797,#51798,
#51799,#51800,#51801,#51802,#51803,#51804,#51805,#51806,#51807,#51808,#51809,
#51810,#51811,#51812,#51813,#51814,#51815,#51816,#51817,#51818,#51819,#51820,
#51821,#51822,#51823,#51824,#51825,#51826,#51827,#51828,#51829,#51830),
 .UNSPECIFIED.,.F.,.F.,(4,2,2,2,2,2,2,2,2,2,2,2,2,2,2,2,2,2,2,2,2,2,2,2,
2,2,2,2,2,2,2,2,2,2,2,2,2,2,2,2,2,2,2,2,2,2,2,2,2,2,2,2,2,2,2,2,2,2,2,2,
2,2,2,2,2,2,2,2,2,2,2,2,2,2,2,2,2,2,2,2,2,2,2,2,2,2,2,2,2,2,2,2,2,2,2,2,
2,2,2,2,2,2,2,2,2,2,2,2,2,2,2,2,2,2,2,2,2,2,2,2,2,2,2,2,2,2,2,2,2,2,2,2,
2,2,2,2,2,2,2,2,2,2,2,2,4),(-2.69193413772045,-2.69145735838593,-2.68997330443083,
-2.689245374593,-2.68873357346072,-2.68819670361825,-2.68744492800286,-2.68547352272114,
-2.65547796781937,-2.58680177411471,-2.53793584450239,-2.53081688926782,
-2.52892101604539,-2.52777943479029,-2.52677244192067,-2.52551797818855,
-2.52358647665744,-2.51487666090906,-2.41866994866227,-2.39383860033977,
-2.3711108516713,-2.36878748635319,-2.36710217097525,-2.36631506648136,
-2.36574186136412,-2.36521192442235,-2.3644864991012,-2.36267253648183,
-2.34181123097501,-2.32155688579686,-2.2984761144842,-2.25060622600615,
-2.20985362330253,-2.2066949263751,-2.20530455198635,-2.20427880639,-2.20333005938109,
-2.20204044995278,-2.19885468445759,-2.16379390000003,-2.08376281744099,
-2.0587291815934,-2.04545922109416,-2.0439831998168,-2.04326280772771,-2.04275211728246,
-2.0422124695452,-2.0412966561262,-2.03883963564719,-2.03618409062887,-2.03379751553649,
-2.03225553339583,-2.03093709017565,-2.00248582245845,-1.91232972498501,
-1.90601777440918,-1.90141821870513,-1.89935694711617,-1.88577672316944,
-1.88352910702193,-1.88219278083537,-1.88117217700993,-1.88008424839063,
-1.87839029714646,-1.87319923415328,-1.84453990410164,-1.80139608419535,
-1.72629628467729,-1.72568563910069,-1.72178063192054,-1.72069092094317,
-1.72004632358291,-1.719485022662,-1.71878482700419,-1.71740818559085,-1.70776985487326,
-1.68340336932087,-1.56734170257267,-1.56143825524245,-1.55958632079397,
-1.55857556097066,-1.55757056809375,-1.55636811426141,-1.55412671294974,
-1.55133198730227,-1.48499792005256,-1.40829010296201,-1.40733533400589,
-1.40547462430765,-1.39894469299867,-1.39775076067882,-1.39702416468783,
-1.39645868207639,-1.39583729281005,-1.39482278049122,-1.39130678663127,
-1.36853667619183,-1.34371030455154,-1.24750417382756,-1.2388898378797,
-1.23696624828831,-1.23571429689888,-1.2347075842021,-1.23358761238405,
-1.23173395940765,-1.22950363705495,-1.22511433500846,-1.18202525858585,
-1.13012824151556,-1.08563731704082,-1.08426648713809,-1.08268971798973,
-1.08004892132688,-1.07566294774228,-1.07452467646683,-1.07386886761162,
-1.07331397416925,-1.07263109249877,-1.07133661740354,-1.06376473483138,
-1.04801334067934,-1.02517119407404,-0.947801484228192,-0.917594331509372,
-0.914772900805758,-0.913410080182123,-0.91244216292318,-0.911528866612556,
-0.910286191833184,-0.908004867281879,-0.905059220870743,-0.898663123076397,
-0.880525896394444,-0.830366330299761,-0.75689749657802,-0.752708020055922,
-0.751589096091725,-0.750937769931712,-0.750377213351687,-0.749686319658207,
-0.748353925318702,-0.739903514870463,-0.720666292987405,-0.679396098858072,
-0.661817785846039),.UNSPECIFIED.);
#292=B_SPLINE_CURVE_WITH_KNOTS('',3,(#51835,#51836,#51837,#51838,#51839,
#51840,#51841,#51842,#51843,#51844,#51845,#51846,#51847,#51848,#51849,#51850,
#51851,#51852,#51853,#51854,#51855,#51856,#51857,#51858,#51859,#51860,#51861,
#51862,#51863,#51864,#51865,#51866,#51867,#51868,#51869,#51870,#51871,#51872,
#51873,#51874,#51875,#51876,#51877,#51878,#51879,#51880,#51881,#51882,#51883,
#51884,#51885,#51886,#51887,#51888,#51889,#51890,#51891,#51892,#51893,#51894,
#51895,#51896,#51897,#51898,#51899,#51900,#51901,#51902,#51903,#51904,#51905,
#51906,#51907,#51908,#51909,#51910,#51911,#51912,#51913,#51914,#51915,#51916,
#51917,#51918,#51919,#51920,#51921,#51922,#51923,#51924,#51925,#51926,#51927,
#51928,#51929,#51930,#51931,#51932,#51933,#51934,#51935,#51936,#51937,#51938,
#51939,#51940,#51941,#51942,#51943,#51944,#51945,#51946,#51947,#51948,#51949,
#51950,#51951,#51952,#51953,#51954,#51955,#51956,#51957,#51958,#51959,#51960,
#51961,#51962,#51963,#51964,#51965,#51966,#51967,#51968,#51969,#51970,#51971,
#51972,#51973,#51974,#51975,#51976,#51977,#51978,#51979,#51980,#51981,#51982,
#51983,#51984,#51985,#51986,#51987,#51988,#51989,#51990,#51991,#51992,#51993,
#51994,#51995,#51996,#51997,#51998,#51999,#52000,#52001,#52002,#52003,#52004,
#52005,#52006,#52007,#52008,#52009,#52010,#52011,#52012,#52013,#52014,#52015,
#52016,#52017,#52018,#52019,#52020,#52021,#52022,#52023,#52024,#52025,#52026,
#52027,#52028,#52029,#52030,#52031,#52032,#52033,#52034,#52035,#52036,#52037,
#52038,#52039,#52040,#52041,#52042,#52043,#52044,#52045,#52046,#52047,#52048,
#52049,#52050,#52051,#52052,#52053,#52054,#52055,#52056,#52057,#52058,#52059,
#52060,#52061,#52062,#52063,#52064,#52065,#52066,#52067,#52068,#52069,#52070,
#52071,#52072,#52073,#52074,#52075,#52076,#52077,#52078,#52079,#52080,#52081,
#52082,#52083,#52084,#52085,#52086,#52087,#52088,#52089,#52090,#52091,#52092,
#52093,#52094,#52095,#52096,#52097,#52098,#52099,#52100,#52101,#52102,#52103,
#52104,#52105,#52106,#52107,#52108,#52109,#52110,#52111,#52112,#52113,#52114,
#52115,#52116,#52117,#52118,#52119,#52120),.UNSPECIFIED.,.F.,.F.,(4,2,2,
2,2,2,2,2,2,2,2,2,2,2,2,2,2,2,2,2,2,2,2,2,2,2,2,2,2,2,2,2,2,2,2,2,2,2,2,
2,2,2,2,2,2,2,2,2,2,2,2,2,2,2,2,2,2,2,2,2,2,2,2,2,2,2,2,2,2,2,2,2,2,2,2,
2,2,2,2,2,2,2,2,2,2,2,2,2,2,2,2,2,2,2,2,2,2,2,2,2,2,2,2,2,2,2,2,2,2,2,2,
2,2,2,2,2,2,2,2,2,2,2,2,2,2,2,2,2,2,2,2,2,2,2,2,2,2,2,2,2,2,2,4),(-3.39932589205789,
-3.37664605276613,-3.33295005406636,-3.2922924414732,-3.28584711476626,
-3.28401270198473,-3.28289391097012,-3.28188367621363,-3.28059339678401,
-3.27795888724217,-3.26182941768803,-3.25854352732134,-3.2501482751672,
-3.16035385444002,-3.13374173424251,-3.12696445228955,-3.12434056697558,
-3.12303667873142,-3.12224545155251,-3.1215607898935,-3.12100373609016,
-3.12046707377518,-3.11971550236055,-3.11774414646171,-3.08770282907068,
-3.04408149950909,-2.99901702339878,-2.97707835448093,-2.96389188932416,
-2.96158992126389,-2.96036823343809,-2.95936385397638,-2.95835045222884,
-2.95648429361429,-2.95046201323023,-2.83443153499172,-2.80156898383306,
-2.80016498238844,-2.79933231530872,-2.79858354750263,-2.7980246637177,
-2.79749087020683,-2.79675040081671,-2.79525216218959,-2.7814394592779,
-2.78069164271035,-2.69139489710344,-2.66071135190701,-2.64113548415316,
-2.63859862684412,-2.63732783164102,-2.63641424884816,-2.63544748443947,
-2.63408866568762,-2.63128322143616,-2.62367957697548,-2.62186819852085,
-2.61980666134163,-2.61931247891372,-2.61725799075544,-2.6161829955101,
-2.61493598432529,-2.61372534546638,-2.61191326750068,-2.60707292528718,
-2.59795311166414,-2.52116909785941,-2.50047192530725,-2.48018784835006,
-2.47801500043262,-2.4768785810965,-2.4761572361015,-2.47551133018969,-2.47496141507606,
-2.47439949256615,-2.47337181747351,-2.47011069813522,-2.41411707647133,
-2.36371688839609,-2.33721627341591,-2.31824934452656,-2.31573004842992,
-2.3144627939536,-2.31354967459111,-2.31258146936232,-2.31121746253311,
-2.30839102732551,-2.27796120448242,-2.20436367923814,-2.18221998976322,
-2.163095659562,-2.15466518881887,-2.15333368516879,-2.15264301525351,-2.15208251873872,
-2.15143112418033,-2.15031175623636,-2.14611723157317,-2.07656356484937,
-2.03100061670361,-2.01462487206545,-2.01142762061337,-1.99552442799153,
-1.99290069612477,-1.99161226131537,-1.99060189192565,-1.98948133006069,
-1.98764031266588,-1.98113486872217,-1.93983882958115,-1.88882762583447,
-1.85036284286612,-1.84917067840476,-1.8482683523753,-1.83242037978032,
-1.83069392683666,-1.83000254770983,-1.82942913899719,-1.82883811501782,
-1.82796095243577,-1.82556262826323,-1.78705880990871,-1.73588563058796,
-1.67478639615717,-1.67077489374424,-1.66935260643082,-1.66836837506511,
-1.66745997306896,-1.66625436838632,-1.66399768651868,-1.6611798828565,
-1.64090394484499,-1.60353131948829,-1.51343043652783,-1.5086107781585,
-1.50753715947562,-1.50683963513011,-1.5062786283345,-1.50563230640225,
-1.50450613090255,-1.49974999936329,-1.45696013432009,-1.36972866115331),
 .UNSPECIFIED.);
#293=B_SPLINE_CURVE_WITH_KNOTS('',3,(#52122,#52123,#52124,#52125,#52126,
#52127,#52128,#52129,#52130,#52131,#52132,#52133,#52134,#52135,#52136,#52137,
#52138,#52139,#52140,#52141,#52142,#52143,#52144,#52145,#52146,#52147,#52148,
#52149,#52150,#52151,#52152,#52153,#52154,#52155,#52156,#52157,#52158,#52159,
#52160,#52161,#52162,#52163,#52164,#52165,#52166,#52167,#52168,#52169,#52170,
#52171,#52172,#52173,#52174,#52175,#52176,#52177,#52178,#52179,#52180,#52181,
#52182,#52183,#52184,#52185,#52186,#52187,#52188,#52189,#52190,#52191,#52192,
#52193,#52194,#52195,#52196,#52197,#52198,#52199,#52200,#52201,#52202,#52203,
#52204,#52205,#52206,#52207,#52208,#52209,#52210,#52211,#52212,#52213,#52214,
#52215),.UNSPECIFIED.,.F.,.F.,(4,2,2,2,2,2,2,2,2,2,2,2,2,2,2,2,2,2,2,2,
2,2,2,2,2,2,2,2,2,2,2,2,2,2,2,2,2,2,2,2,2,2,2,2,2,2,4),(-0.661817785846039,
-0.631446402549966,-0.594936698900035,-0.591720851839081,-0.590426142407845,
-0.589476182966453,-0.588451554667015,-0.587443401341402,-0.58507720331537,
-0.57005418523331,-0.536081981121245,-0.511038236961451,-0.434371763132626,
-0.433334741118563,-0.429713493102654,-0.428642525482714,-0.428071792347138,
-0.427516904834903,-0.426835569337568,-0.425548596991163,-0.418139527423193,
-0.402628039054871,-0.36025705268546,-0.341038272571705,-0.316338706676212,
-0.297203327417526,-0.290954043984244,-0.271336657129702,-0.268823687320345,
-0.267538157236581,-0.266590477115374,-0.26556402366529,-0.264552679137309,
-0.263207389113299,-0.256922756022098,-0.226064499166746,-0.205907523735348,
-0.111736952927014,-0.107489642422549,-0.105981692504411,-0.105254940934071,
-0.104690929687764,-0.104062964051209,-0.103019489520687,-0.0992174504771558,
-0.0104838575317579,-0.000962328596166258),.UNSPECIFIED.);
#294=B_SPLINE_CURVE_WITH_KNOTS('',3,(#52216,#52217,#52218,#52219,#52220,
#52221,#52222,#52223,#52224,#52225,#52226,#52227,#52228,#52229,#52230,#52231,
#52232,#52233,#52234,#52235,#52236,#52237,#52238,#52239,#52240,#52241,#52242,
#52243,#52244,#52245,#52246,#52247,#52248,#52249,#52250,#52251,#52252,#52253,
#52254,#52255,#52256,#52257,#52258,#52259,#52260,#52261,#52262,#52263,#52264,
#52265,#52266,#52267,#52268,#52269,#52270,#52271,#52272,#52273,#52274,#52275,
#52276,#52277,#52278,#52279,#52280,#52281,#52282,#52283,#52284,#52285,#52286,
#52287,#52288,#52289,#52290,#52291,#52292,#52293,#52294,#52295,#52296,#52297,
#52298,#52299,#52300,#52301,#52302,#52303,#52304,#52305,#52306,#52307,#52308,
#52309,#52310,#52311,#52312,#52313,#52314,#52315,#52316,#52317,#52318,#52319,
#52320,#52321,#52322,#52323,#52324,#52325,#52326,#52327,#52328,#52329,#52330,
#52331,#52332,#52333,#52334,#52335,#52336,#52337,#52338,#52339,#52340,#52341,
#52342,#52343,#52344,#52345,#52346,#52347,#52348,#52349,#52350,#52351,#52352,
#52353,#52354,#52355,#52356,#52357,#52358,#52359,#52360,#52361,#52362,#52363,
#52364,#52365,#52366,#52367,#52368,#52369,#52370,#52371,#52372,#52373,#52374,
#52375,#52376,#52377,#52378,#52379,#52380,#52381,#52382,#52383,#52384,#52385,
#52386,#52387,#52388,#52389,#52390,#52391,#52392,#52393,#52394,#52395,#52396,
#52397,#52398,#52399,#52400,#52401,#52402,#52403,#52404,#52405,#52406,#52407,
#52408,#52409,#52410,#52411,#52412,#52413,#52414,#52415,#52416,#52417,#52418,
#52419,#52420,#52421,#52422,#52423,#52424,#52425,#52426,#52427,#52428,#52429),
 .UNSPECIFIED.,.F.,.F.,(4,2,2,2,2,2,2,2,2,2,2,2,2,2,2,2,2,2,2,2,2,2,2,2,
2,2,2,2,2,2,2,2,2,2,2,2,2,2,2,2,2,2,2,2,2,2,2,2,2,2,2,2,2,2,2,2,2,2,2,2,
2,2,2,2,2,2,2,2,2,2,2,2,2,2,2,2,2,2,2,2,2,2,2,2,2,2,2,2,2,2,2,2,2,2,2,2,
2,2,2,2,2,2,2,2,2,2,4),(-4.06236830518179,-4.01128230784337,-4.00860916091127,
-4.00704905561026,-4.00595357167427,-4.00501093552446,-4.00399938511821,
-4.00270339750265,-4.00013206854681,-3.99184181669663,-3.98994577632168,
-3.98800630375214,-3.98659213524642,-3.98249844406454,-3.98000829183565,
-3.97510366934702,-3.96600766868781,-3.95141074503959,-3.94540833280247,
-3.89508138093323,-3.84637846026233,-3.84452919536455,-3.84373909705527,
-3.84316532270155,-3.84263603764128,-3.84191323327071,-3.84048550189996,
-3.82886490519833,-3.74707957015382,-3.72030872139708,-3.70213371050775,
-3.68607289248382,-3.68365782899963,-3.68264670893793,-3.68162035132604,
-3.6806724144489,-3.67938600890634,-3.67686976370155,-3.65716555553687,
-3.63783979127214,-3.62869838268935,-3.58079267930138,-3.57471057746759,
-3.56747826151506,-3.54205667472033,-3.53055871425514,-3.52261530716523,
-3.52130399711088,-3.52061747540546,-3.52005706631424,-3.51940201963884,
-3.51826735020328,-3.51391931341309,-3.43952122246206,-3.40733610049415,
-3.37717529654029,-3.36303954199801,-3.36070043932541,-3.3596974279773,
-3.35867552560362,-3.3577210476806,-3.35640920602911,-3.35309389099396,
-3.31112875033255,-3.23255705536707,-3.21840971952123,-3.20578194360784,
-3.19948533541297,-3.19825621823781,-3.19758724679695,-3.19708247993021,
-3.19651789758148,-3.19547766980306,-3.19211666374425,-3.13380261064229,
-3.09118375963743,-3.05560503048395,-3.0454221370737,-3.04125824992219,
-3.03815917116431,-3.03678344746364,-3.03575529140895,-3.03480958861689,
-3.03353212264099,-3.03041602661921,-2.99846025627691,-2.90688671050272,
-2.88555454356852,-2.8766574036631,-2.87530720213329,-2.87461243359211,
-2.87410518784067,-2.8735547614057,-2.87258503620628,-2.86976368789951,
-2.82305473929898,-2.76615661413109,-2.74447225970692,-2.72031992525608,
-2.71720227428073,-2.71475117466605,-2.71350358027369,-2.71258924446251,
-2.71162254860925,-2.70999232954388,-2.70567525048565,-2.69332373186839),
 .UNSPECIFIED.);
#295=B_SPLINE_CURVE_WITH_KNOTS('',3,(#52435,#52436,#52437,#52438,#52439,
#52440,#52441,#52442,#52443,#52444,#52445,#52446,#52447,#52448,#52449,#52450,
#52451,#52452,#52453,#52454,#52455,#52456,#52457,#52458,#52459,#52460,#52461,
#52462,#52463,#52464,#52465,#52466,#52467,#52468,#52469,#52470,#52471,#52472,
#52473,#52474,#52475,#52476,#52477,#52478,#52479,#52480,#52481,#52482,#52483,
#52484,#52485,#52486,#52487,#52488,#52489,#52490,#52491,#52492,#52493,#52494,
#52495,#52496,#52497,#52498,#52499,#52500,#52501,#52502,#52503,#52504,#52505,
#52506,#52507,#52508,#52509,#52510,#52511,#52512,#52513,#52514,#52515,#52516,
#52517,#52518,#52519,#52520,#52521,#52522,#52523,#52524,#52525,#52526,#52527,
#52528,#52529,#52530,#52531,#52532,#52533,#52534,#52535,#52536,#52537,#52538,
#52539,#52540,#52541,#52542,#52543,#52544,#52545,#52546,#52547,#52548,#52549,
#52550,#52551,#52552,#52553,#52554,#52555,#52556,#52557,#52558,#52559,#52560,
#52561,#52562,#52563,#52564,#52565,#52566,#52567,#52568,#52569,#52570,#52571,
#52572,#52573,#52574,#52575,#52576),.UNSPECIFIED.,.F.,.F.,(4,3,3,3,3,3,
3,3,3,3,3,3,3,3,3,3,3,3,3,3,3,3,3,3,3,3,3,3,3,3,3,3,3,3,3,3,3,3,3,3,3,3,
3,3,3,3,3,4),(512.079602535136,512.170919108167,512.263992052284,512.356938891763,
512.44978726279,512.542567767289,512.63531308929,512.728048054237,512.820797472426,
512.913646113011,513.006546553474,513.099602449414,513.17063376364,513.263706707811,
513.356653547343,513.449501918419,513.542282422965,513.63502774501,513.727762709999,
513.820512128227,513.913360768848,514.006261209345,514.099317105315,514.170348419112,
514.263421364159,514.35636820457,514.449216576529,514.541997081958,514.634742404887,
514.727477370759,514.820226789868,514.913075431362,515.005975872729,515.099031769554,
515.170063074585,515.263136017659,515.356082856097,515.448931226086,515.541711729555,
515.634457050532,515.727192014461,515.819941431639,515.912790071233,516.005690510712,
516.098746405693,516.169777730058,516.262840343893,516.317081157972),
 .UNSPECIFIED.);
#296=B_SPLINE_CURVE_WITH_KNOTS('',3,(#52577,#52578,#52579,#52580,#52581,
#52582,#52583,#52584,#52585,#52586,#52587,#52588,#52589,#52590,#52591,#52592,
#52593,#52594,#52595,#52596,#52597,#52598,#52599,#52600,#52601,#52602,#52603,
#52604,#52605,#52606,#52607,#52608,#52609,#52610,#52611,#52612,#52613,#52614,
#52615,#52616,#52617,#52618,#52619,#52620,#52621,#52622,#52623,#52624,#52625,
#52626,#52627,#52628,#52629,#52630,#52631,#52632,#52633,#52634,#52635,#52636,
#52637,#52638,#52639,#52640,#52641,#52642,#52643,#52644,#52645,#52646,#52647,
#52648,#52649,#52650,#52651,#52652,#52653,#52654,#52655,#52656,#52657,#52658,
#52659,#52660,#52661,#52662,#52663,#52664,#52665,#52666,#52667,#52668,#52669,
#52670,#52671,#52672,#52673,#52674,#52675,#52676),.UNSPECIFIED.,.F.,.F.,
(4,2,2,2,2,2,2,2,2,2,2,2,2,2,2,2,2,2,2,2,2,2,2,2,2,2,2,2,2,2,2,2,2,2,2,
2,2,2,2,2,2,2,2,2,2,2,2,2,2,4),(-4.06019064732414,-3.96551133596624,-3.93627764245022,
-3.9310228429966,-3.92932187488524,-3.92823296741668,-3.9272139411775,-3.92588326496817,
-3.92307267248462,-3.90203731571564,-3.89950321675288,-3.88289828236199,
-3.80458145762543,-3.78548988001597,-3.77445220310783,-3.77070040604564,
-3.76818790684858,-3.76729489216759,-3.76677007295134,-3.76620400855292,
-3.76547131563236,-3.76389001694167,-3.75235839834927,-3.74884301231658,
-3.74662501750788,-3.71614948388614,-3.69486242393203,-3.64856163202697,
-3.6142754661495,-3.60846921195793,-3.60670336502825,-3.6055999521817,-3.60458583260201,
-3.60328731492125,-3.60053967969616,-3.58194776095191,-3.58042908630198,
-3.57382290133506,-3.49690215555902,-3.46464457663389,-3.45229160446695,
-3.44821598516339,-3.44641292349166,-3.44501142041935,-3.44431005195053,
-3.44376196090874,-3.44321245953694,-3.44224578809134,-3.43944223418908,
-3.39932589205789),.UNSPECIFIED.);
#297=B_SPLINE_CURVE_WITH_KNOTS('',3,(#52677,#52678,#52679,#52680,#52681,
#52682,#52683,#52684,#52685,#52686,#52687,#52688,#52689,#52690,#52691,#52692,
#52693,#52694,#52695,#52696,#52697,#52698,#52699,#52700,#52701,#52702,#52703,
#52704,#52705,#52706,#52707,#52708,#52709,#52710,#52711,#52712,#52713,#52714,
#52715,#52716,#52717,#52718,#52719,#52720,#52721,#52722,#52723,#52724,#52725,
#52726,#52727,#52728,#52729,#52730,#52731,#52732,#52733,#52734,#52735,#52736,
#52737,#52738,#52739,#52740,#52741,#52742,#52743,#52744,#52745,#52746,#52747,
#52748,#52749,#52750,#52751,#52752,#52753,#52754,#52755,#52756,#52757,#52758,
#52759,#52760,#52761,#52762,#52763,#52764,#52765,#52766,#52767,#52768,#52769,
#52770,#52771,#52772,#52773,#52774,#52775,#52776,#52777,#52778,#52779,#52780,
#52781,#52782,#52783,#52784,#52785,#52786,#52787,#52788,#52789,#52790,#52791,
#52792,#52793,#52794,#52795,#52796,#52797,#52798,#52799,#52800,#52801,#52802,
#52803,#52804,#52805,#52806,#52807,#52808,#52809,#52810,#52811,#52812,#52813,
#52814,#52815,#52816,#52817,#52818,#52819,#52820,#52821,#52822,#52823,#52824,
#52825,#52826,#52827,#52828,#52829,#52830,#52831,#52832,#52833,#52834,#52835,
#52836,#52837,#52838,#52839,#52840,#52841,#52842,#52843,#52844,#52845,#52846,
#52847,#52848,#52849,#52850,#52851,#52852,#52853,#52854,#52855,#52856,#52857,
#52858,#52859,#52860,#52861,#52862,#52863,#52864,#52865,#52866,#52867,#52868,
#52869,#52870,#52871,#52872,#52873,#52874,#52875,#52876,#52877,#52878,#52879,
#52880,#52881,#52882,#52883,#52884,#52885,#52886,#52887,#52888,#52889,#52890,
#52891,#52892,#52893,#52894,#52895,#52896,#52897,#52898,#52899,#52900,#52901,
#52902,#52903,#52904,#52905,#52906,#52907,#52908,#52909,#52910,#52911,#52912,
#52913,#52914,#52915,#52916,#52917,#52918,#52919,#52920,#52921,#52922,#52923,
#52924,#52925,#52926,#52927,#52928,#52929,#52930,#52931,#52932,#52933,#52934,
#52935,#52936,#52937,#52938,#52939,#52940,#52941,#52942,#52943,#52944,#52945,
#52946,#52947,#52948),.UNSPECIFIED.,.F.,.F.,(4,2,2,2,2,2,2,2,2,2,2,2,2,
2,2,2,2,2,2,2,2,2,2,2,2,2,2,2,2,2,2,2,2,2,2,2,2,2,2,2,2,2,2,2,2,2,2,2,2,
2,2,2,2,2,2,2,2,2,2,2,2,2,2,2,2,2,2,2,2,2,2,2,2,2,2,2,2,2,2,2,2,2,2,2,2,
2,2,2,2,2,2,2,2,2,2,2,2,2,2,2,2,2,2,2,2,2,2,2,2,2,2,2,2,2,2,2,2,2,2,2,2,
2,2,2,2,2,2,2,2,2,2,2,2,2,2,4),(-2.69332373186839,-2.63590056303955,-2.59806115287555,
-2.57696081092695,-2.55633179412,-2.55302030257022,-2.55202756390987,-2.55141093236035,
-2.55084378590168,-2.55010686759453,-2.54850543205393,-2.53647896298135,
-2.53424559805585,-2.53356139770569,-2.53178653827847,-2.53063530704833,
-2.52405211013857,-2.51354138754007,-2.4731948785474,-2.42847837585149,
-2.39823559538545,-2.39467385090571,-2.39275854985133,-2.39111355398828,
-2.39004547753411,-2.38902535560524,-2.38769319623464,-2.38487928018183,
-2.363812889089,-2.36146198758775,-2.32627655806885,-2.30286396483439,-2.2539710811715,
-2.23339320988599,-2.2300867051748,-2.22909450837485,-2.2284779923434,-2.22791079669378,
-2.22717360116059,-2.22594435968902,-2.21881994646708,-2.12181547515734,
-2.09091683479816,-2.07125626509458,-2.06871605093705,-2.06744420702026,
-2.06653011952601,-2.0655630513402,-2.06420418141462,-2.06139984690182,
-2.0319497580756,-2.0077183012875,-1.91219803341816,-1.90726791750861,-1.90618514411705,
-1.90548461391946,-1.90492316096849,-1.90427851704085,-1.90316067369496,
-1.89851451677803,-1.87424082566735,-1.82662170535717,-1.81308605501974,
-1.75018670688178,-1.746325956503,-1.74492594377872,-1.74394753995088,-1.74303698448542,
-1.74179218349189,-1.73938360035058,-1.72373175461307,-1.68745316548452,
-1.59432399182279,-1.59227809682013,-1.58447714029863,-1.58321097944092,
-1.58246284549766,-1.58189380053572,-1.58129429297067,-1.58035562690714,
-1.57925316911031,-1.57717004566508,-1.55830257712428,-1.54540281725048,
-1.42958403681793,-1.4235771773282,-1.42171203890487,-1.42069835710753,
-1.41969317171171,-1.41846974060338,-1.41616220645593,-1.40288512962007,
-1.38435686890064,-1.34456156946301,-1.27205622854209,-1.261404885607,-1.26001244020086,
-1.25929859360713,-1.25877152233286,-1.25820745791169,-1.2574305703082,
-1.25655874189117,-1.25505942866704,-1.21168957205603,-1.10651447290484,
-1.10039821345671,-1.09851990419571,-1.09750363473058,-1.09649875622884,
-1.09527983596344,-1.09299310275094,-1.08014531899821,-1.05538661335461,
-0.965473652922269,-0.938761057845499,-0.936838413369243,-0.936094375934143,
-0.935559456860022,-0.935021473923919,-0.934287539974073,-0.932728829940132,
-0.93067138694473,-0.925799967028894,-0.910335530259787,-0.866752418091578,
-0.782554567270362,-0.777096263670779,-0.77530104640451,-0.774301476686873,
-0.773304280652919,-0.772060322566885,-0.769655380994483,-0.754093001055015,
-0.718148387247962,-0.679321467808541,-0.662369123431852),.UNSPECIFIED.);
#298=B_SPLINE_CURVE_WITH_KNOTS('',3,(#52954,#52955,#52956,#52957,#52958,
#52959,#52960,#52961,#52962,#52963,#52964,#52965,#52966,#52967,#52968,#52969,
#52970,#52971,#52972,#52973,#52974,#52975,#52976,#52977,#52978,#52979,#52980,
#52981,#52982,#52983,#52984,#52985,#52986,#52987,#52988,#52989,#52990,#52991,
#52992,#52993,#52994,#52995,#52996,#52997,#52998,#52999,#53000,#53001,#53002,
#53003,#53004,#53005,#53006,#53007,#53008,#53009,#53010,#53011,#53012,#53013,
#53014,#53015,#53016,#53017,#53018,#53019,#53020,#53021,#53022,#53023,#53024,
#53025,#53026,#53027,#53028,#53029,#53030,#53031,#53032,#53033,#53034,#53035,
#53036,#53037,#53038,#53039,#53040,#53041,#53042,#53043,#53044,#53045,#53046,
#53047,#53048,#53049,#53050,#53051,#53052,#53053,#53054,#53055,#53056,#53057,
#53058,#53059,#53060,#53061,#53062,#53063,#53064,#53065,#53066,#53067,#53068,
#53069,#53070,#53071,#53072,#53073,#53074,#53075,#53076,#53077,#53078,#53079,
#53080,#53081,#53082,#53083,#53084,#53085,#53086,#53087,#53088,#53089,#53090,
#53091,#53092,#53093,#53094,#53095,#53096,#53097,#53098,#53099,#53100,#53101,
#53102,#53103,#53104,#53105,#53106,#53107,#53108,#53109,#53110,#53111,#53112,
#53113,#53114,#53115,#53116,#53117,#53118,#53119,#53120,#53121,#53122,#53123,
#53124,#53125,#53126,#53127,#53128,#53129,#53130,#53131,#53132,#53133,#53134,
#53135),.UNSPECIFIED.,.F.,.F.,(4,2,2,2,2,2,2,2,2,2,2,2,2,2,2,2,2,2,2,2,
2,2,2,2,2,2,2,2,2,2,2,2,2,2,2,2,2,2,2,2,2,2,2,2,2,2,2,2,2,2,2,2,2,2,2,2,
2,2,2,2,2,2,2,2,2,2,2,2,2,2,2,2,2,2,2,2,2,2,2,2,2,2,2,2,2,2,2,2,2,2,4),
(-1.37013824341392,-1.34237747191845,-1.26296548255655,-1.25536130056935,
-1.24659540766556,-1.24586959228131,-1.23317991477552,-1.23171711750194,
-1.230999393659,-1.23043646945422,-1.22980340814454,-1.22875837730866,-1.22493445215964,
-1.13629518515779,-1.07548947616176,-1.071705691954,-1.0703177875468,-1.0693429263559,
-1.06843176200177,-1.06718007845695,-1.06473717415751,-1.04842685445754,
-1.00958701002103,-0.949541861280324,-0.920595253380862,-0.910248997532136,
-0.908868742418837,-0.908158155007743,-0.907632020484454,-0.907055704647409,
-0.906482907996922,-0.905053682495817,-0.893500756336844,-0.867187556378256,
-0.824917914430684,-0.753413761330077,-0.74899295524278,-0.747346767872416,
-0.746377109018273,-0.74546421707459,-0.744199804330603,-0.741695247766714,
-0.723585523021593,-0.696841802838405,-0.637649801136975,-0.589168997767841,
-0.586328345886029,-0.585355819349327,-0.584804912645701,-0.584297932530326,
-0.583758288439846,-0.583079869336424,-0.58056957833095,-0.555694178605008,
-0.515219253535521,-0.431711702631918,-0.426296719322435,-0.424507560325197,
-0.423509389672865,-0.422512296152171,-0.421266537180775,-0.418851978487372,
-0.403317567111448,-0.367406759777754,-0.342783674404433,-0.318345898600323,
-0.273498021158975,-0.272245526021084,-0.270739915235589,-0.267961432113831,
-0.263697864826172,-0.262571534646786,-0.261918464415451,-0.261357995163237,
-0.260819564611093,-0.260145265755279,-0.259121007977705,-0.246896917217738,
-0.219095594500449,-0.198237662155218,-0.165635642675342,-0.106771597814053,
-0.102935312594607,-0.101539357531473,-0.100562305560897,-0.099651835767735,
-0.0984053446425378,-0.0959872631004007,-0.0929523634159408,-0.0862943093706694,
-0.000962145650915263),.UNSPECIFIED.);
#299=B_SPLINE_CURVE_WITH_KNOTS('',3,(#53136,#53137,#53138,#53139,#53140,
#53141,#53142,#53143,#53144,#53145,#53146,#53147,#53148,#53149,#53150,#53151,
#53152,#53153,#53154,#53155,#53156,#53157,#53158,#53159,#53160,#53161,#53162,
#53163,#53164,#53165,#53166,#53167,#53168,#53169,#53170,#53171,#53172,#53173,
#53174,#53175,#53176,#53177,#53178,#53179,#53180,#53181,#53182,#53183,#53184,
#53185,#53186,#53187,#53188,#53189,#53190,#53191,#53192,#53193,#53194,#53195,
#53196,#53197,#53198,#53199,#53200,#53201,#53202,#53203,#53204,#53205),
 .UNSPECIFIED.,.F.,.F.,(4,3,3,3,3,3,3,3,3,3,3,3,3,3,3,3,3,3,3,3,3,3,3,4),
(516.317081157972,516.409967208446,516.504907855582,516.597664063071,516.690400143587,
516.783140911013,516.879728779642,516.972608388968,517.065554242249,517.158638357035,
517.169492385531,517.262565334695,517.355512179238,517.44836055534,517.54114106491,
517.633886391977,517.72662136198,517.819370785208,517.912219430777,518.005119876201,
518.098175777011,518.169207041004,518.305071793348,518.362787842316),
 .UNSPECIFIED.);
#300=B_SPLINE_CURVE_WITH_KNOTS('',3,(#53207,#53208,#53209,#53210,#53211,
#53212,#53213,#53214,#53215,#53216,#53217,#53218,#53219,#53220,#53221,#53222,
#53223,#53224,#53225,#53226,#53227,#53228,#53229,#53230,#53231,#53232,#53233,
#53234,#53235,#53236,#53237,#53238,#53239,#53240,#53241,#53242,#53243,#53244,
#53245,#53246,#53247,#53248,#53249,#53250,#53251,#53252,#53253,#53254,#53255,
#53256,#53257,#53258,#53259,#53260,#53261,#53262,#53263,#53264,#53265,#53266,
#53267,#53268,#53269,#53270,#53271,#53272,#53273,#53274,#53275,#53276,#53277,
#53278,#53279,#53280,#53281,#53282,#53283,#53284,#53285,#53286,#53287,#53288,
#53289,#53290,#53291,#53292,#53293,#53294,#53295,#53296,#53297,#53298,#53299,
#53300,#53301,#53302,#53303,#53304,#53305,#53306,#53307,#53308,#53309,#53310,
#53311,#53312,#53313,#53314),.UNSPECIFIED.,.F.,.F.,(4,2,2,2,2,2,2,2,2,2,
2,2,2,2,2,2,2,2,2,2,2,2,2,2,2,2,2,2,2,2,2,2,2,2,2,2,2,2,2,2,2,2,2,2,2,2,
2,2,2,2,2,2,2,4),(-0.662369123431852,-0.62745144403119,-0.624894961586772,
-0.615051491018097,-0.613540831864279,-0.612813519464919,-0.612249410799109,
-0.611634339945498,-0.610626291022457,-0.607162547734505,-0.601490992264344,
-0.581649228413477,-0.55393564927306,-0.459707160818077,-0.454073598566679,
-0.452255559620789,-0.45125145906371,-0.450245429418516,-0.449005750843542,
-0.446620867262244,-0.431562342388669,-0.397524861332346,-0.359405694182378,
-0.340783500053336,-0.315020908576646,-0.31191617739949,-0.309633211910726,
-0.309361695135919,-0.308471664010906,-0.307011722181371,-0.305834854723347,
-0.292248539947005,-0.290612998170837,-0.289925803729212,-0.28935335498504,
-0.28882742131339,-0.288245553991981,-0.286732332052735,-0.27124294091145,
-0.249295311213617,-0.158289237902776,-0.152178623612308,-0.150806701167426,
-0.149596139756178,-0.148344922412134,-0.13248898497981,-0.129867251400714,
-0.128579052407423,-0.127568524631218,-0.126447433991131,-0.12460474039766,
-0.118085269625875,-0.0766441399792139,-0.000962579226033729),
 .UNSPECIFIED.);
#301=B_SPLINE_CURVE_WITH_KNOTS('',3,(#53315,#53316,#53317,#53318,#53319,
#53320,#53321,#53322,#53323,#53324,#53325,#53326,#53327,#53328,#53329,#53330,
#53331,#53332,#53333,#53334,#53335,#53336,#53337,#53338,#53339,#53340,#53341,
#53342,#53343,#53344,#53345,#53346,#53347,#53348,#53349,#53350,#53351,#53352,
#53353,#53354,#53355,#53356,#53357,#53358,#53359,#53360,#53361,#53362,#53363,
#53364,#53365,#53366,#53367,#53368,#53369,#53370,#53371,#53372,#53373,#53374,
#53375,#53376,#53377,#53378,#53379,#53380,#53381,#53382,#53383,#53384,#53385,
#53386,#53387,#53388,#53389,#53390,#53391,#53392,#53393,#53394,#53395,#53396,
#53397,#53398,#53399,#53400,#53401,#53402,#53403,#53404,#53405,#53406,#53407,
#53408,#53409,#53410,#53411,#53412,#53413,#53414,#53415,#53416,#53417,#53418,
#53419,#53420,#53421,#53422,#53423,#53424,#53425,#53426,#53427,#53428,#53429,
#53430,#53431,#53432,#53433,#53434,#53435,#53436,#53437,#53438,#53439,#53440,
#53441,#53442,#53443,#53444,#53445,#53446,#53447,#53448,#53449,#53450,#53451,
#53452,#53453,#53454,#53455,#53456,#53457,#53458,#53459,#53460,#53461,#53462,
#53463,#53464,#53465,#53466,#53467,#53468,#53469,#53470,#53471,#53472,#53473,
#53474,#53475,#53476,#53477,#53478,#53479,#53480,#53481,#53482,#53483,#53484,
#53485,#53486,#53487,#53488,#53489,#53490,#53491,#53492,#53493,#53494,#53495,
#53496,#53497,#53498,#53499,#53500,#53501,#53502,#53503,#53504,#53505,#53506,
#53507,#53508,#53509,#53510,#53511,#53512,#53513,#53514,#53515,#53516,#53517,
#53518,#53519,#53520,#53521,#53522,#53523,#53524,#53525,#53526,#53527,#53528,
#53529,#53530,#53531,#53532,#53533,#53534),.UNSPECIFIED.,.F.,.F.,(4,2,2,
2,2,2,2,2,2,2,2,2,2,2,2,2,2,2,2,2,2,2,2,2,2,2,2,2,2,2,2,2,2,2,2,2,2,2,2,
2,2,2,2,2,2,2,2,2,2,2,2,2,2,2,2,2,2,2,2,2,2,2,2,2,2,2,2,2,2,2,2,2,2,2,2,
2,2,2,2,2,2,2,2,2,2,2,2,2,2,2,2,2,2,2,2,2,2,2,2,2,2,2,2,2,2,2,2,2,2,4),
(-4.06149001195427,-4.03430084075442,-4.02977258884284,-4.02861683066207,
-4.02788745406436,-4.02733148857688,-4.02679461843254,-4.026261124383,-4.02552132882982,
-4.0240252627134,-4.01027274796171,-4.00596483989454,-3.99467961431301,
-3.99071061390817,-3.90714195909425,-3.88237788159706,-3.86958043597391,
-3.86729753140544,-3.86608002678159,-3.86517331928053,-3.86403968739449,
-3.86213891302951,-3.85582587781367,-3.74921804381687,-3.72811942667567,
-3.71330537273624,-3.70621129912855,-3.70494359438975,-3.70438826729269,
-3.70385075405932,-3.70331633483153,-3.70257319468605,-3.70065396998791,
-3.67408357459449,-3.63177721987689,-3.62675265488348,-3.6209528511424,
-3.61415174664876,-3.60598534833864,-3.59577693627203,-3.56189537819281,
-3.5468795548363,-3.54449741845942,-3.54325874171467,-3.54225331094599,
-3.54124962932948,-3.53943185231182,-3.53379544543375,-3.44006046768866,
-3.40660510040486,-3.39091792117336,-3.38596044878126,-3.38387664956146,
-3.38230212462293,-3.38156531356056,-3.38102852077311,-3.38049520577073,
-3.37975639214039,-3.37826460419857,-3.36466423763384,-3.36267115939298,
-3.36095443124507,-3.35920947213016,-3.35611519840963,-3.2742723284145,
-3.26070926712454,-3.23619314107547,-3.22375222098135,-3.22148674059388,
-3.2202727793912,-3.21936621866287,-3.21837384312357,-3.21661236562687,
-3.21139771615466,-3.1303180441815,-3.08397060084227,-3.06821989416106,
-3.06314202052297,-3.06102098153343,-3.05990430519525,-3.0589553434277,
-3.05835411470745,-3.0577864242783,-3.05704427519897,-3.05579742965874,
-3.04834617983115,-3.04581822934454,-2.9451099789324,-2.90218874050175,
-2.89900821338615,-2.89761435505547,-2.89658842155797,-2.8956411833345,
-2.89435619424656,-2.89184410346205,-2.87222633116237,-2.86696597218873,
-2.85995248443672,-2.77377371676683,-2.73873789556053,-2.73731231196971,
-2.73647081687014,-2.73573073418203,-2.73516918636213,-2.73463967760853,
-2.73391536676175,-2.73248103515623,-2.72065634548908,-2.7182387527232,
-2.69318633084655),.UNSPECIFIED.);
#302=B_SPLINE_CURVE_WITH_KNOTS('',3,(#53539,#53540,#53541,#53542,#53543,
#53544,#53545,#53546,#53547,#53548,#53549,#53550,#53551,#53552,#53553,#53554,
#53555,#53556,#53557,#53558,#53559,#53560,#53561,#53562,#53563,#53564,#53565,
#53566,#53567,#53568,#53569,#53570,#53571,#53572,#53573,#53574,#53575,#53576,
#53577,#53578,#53579,#53580,#53581,#53582,#53583,#53584,#53585,#53586,#53587,
#53588,#53589,#53590,#53591,#53592,#53593,#53594,#53595,#53596,#53597,#53598,
#53599,#53600,#53601,#53602,#53603,#53604,#53605,#53606,#53607,#53608,#53609,
#53610,#53611,#53612,#53613,#53614,#53615,#53616,#53617,#53618,#53619,#53620,
#53621,#53622,#53623,#53624,#53625,#53626,#53627,#53628,#53629,#53630,#53631,
#53632,#53633,#53634,#53635,#53636,#53637,#53638,#53639,#53640,#53641,#53642,
#53643,#53644,#53645,#53646,#53647,#53648,#53649,#53650,#53651,#53652,#53653,
#53654,#53655,#53656,#53657,#53658,#53659,#53660,#53661,#53662,#53663,#53664,
#53665,#53666,#53667,#53668,#53669,#53670,#53671,#53672,#53673,#53674,#53675,
#53676,#53677,#53678,#53679,#53680,#53681,#53682,#53683,#53684,#53685,#53686,
#53687,#53688,#53689,#53690,#53691,#53692,#53693,#53694,#53695,#53696,#53697,
#53698,#53699,#53700,#53701,#53702,#53703,#53704,#53705,#53706,#53707,#53708,
#53709,#53710,#53711,#53712,#53713,#53714,#53715,#53716,#53717,#53718,#53719,
#53720,#53721,#53722,#53723,#53724,#53725,#53726,#53727,#53728,#53729,#53730,
#53731,#53732,#53733,#53734,#53735,#53736,#53737,#53738,#53739,#53740,#53741,
#53742,#53743,#53744,#53745,#53746,#53747,#53748,#53749,#53750,#53751,#53752,
#53753,#53754,#53755,#53756,#53757,#53758,#53759,#53760,#53761,#53762,#53763,
#53764,#53765,#53766,#53767,#53768,#53769,#53770,#53771,#53772,#53773,#53774,
#53775,#53776,#53777,#53778,#53779,#53780,#53781,#53782,#53783,#53784,#53785,
#53786,#53787,#53788,#53789,#53790,#53791,#53792,#53793,#53794,#53795,#53796,
#53797,#53798,#53799,#53800,#53801,#53802,#53803,#53804,#53805,#53806,#53807,
#53808,#53809,#53810,#53811,#53812,#53813,#53814,#53815,#53816,#53817,#53818,
#53819,#53820,#53821,#53822,#53823,#53824,#53825,#53826,#53827,#53828,#53829,
#53830,#53831,#53832,#53833,#53834),.UNSPECIFIED.,.F.,.F.,(4,2,2,2,2,2,
2,2,2,2,2,2,2,2,2,2,2,2,2,2,2,2,2,2,2,2,2,2,2,2,2,2,2,2,2,2,2,2,2,2,2,2,
2,2,2,2,2,2,2,2,2,2,2,2,2,2,2,2,2,2,2,2,2,2,2,2,2,2,2,2,2,2,2,2,2,2,2,2,
2,2,2,2,2,2,2,2,2,2,2,2,2,2,2,2,2,2,2,2,2,2,2,2,2,2,2,2,2,2,2,2,2,2,2,2,
2,2,2,2,2,2,2,2,2,2,2,2,2,2,2,2,2,2,2,2,2,2,2,2,2,2,2,2,2,2,2,2,2,4),(-3.39990807077895,
-3.38040660328844,-3.34866766661436,-3.33914485573359,-3.33316968616272,
-3.33184440072165,-3.33060222175386,-3.32969230693305,-3.32871336946001,
-3.32731052388335,-3.32342893520583,-3.26359940006235,-3.22172400779769,
-3.1716315570116,-3.16977654414896,-3.16897668541224,-3.16840125339318,
-3.16787438866942,-3.16716057016105,-3.16576744110638,-3.15508367140835,
-3.11251470375477,-3.05238795228073,-3.03637952601627,-3.01212308458557,
-3.00923325288756,-3.00787791706218,-3.00685822535848,-3.0059006862434,
-3.00457655017696,-3.0011871397329,-2.95416996011485,-2.8979467095119,-2.84863583019543,
-2.84683654492155,-2.84604889145538,-2.84547568407799,-2.84494596089086,
-2.84422127502957,-2.84278595387785,-2.83094280495201,-2.83016267713157,
-2.8297733276619,-2.82706156377725,-2.82536928172015,-2.82362717237232,
-2.81880760933122,-2.80805950114032,-2.74525323139849,-2.70512836055002,
-2.68932956373854,-2.68636256433413,-2.68499024746307,-2.6839675989178,
-2.68301437624201,-2.68170730361202,-2.67841990809102,-2.63808502327443,
-2.55934942475775,-2.54642007452257,-2.53283966987829,-2.52497447856393,
-2.52364952353526,-2.5229544202497,-2.52239350017703,-2.52182944595065,
-2.52079169904626,-2.51745058121227,-2.5133094474349,-2.51216770457176,
-2.51042068833676,-2.50761096435117,-2.50491026473328,-2.50081370012467,
-2.49086450692796,-2.4035980887951,-2.36996552231238,-2.36616982633216,
-2.36329490059547,-2.36194440115669,-2.36092534309872,-2.35996619185918,
-2.35863632018816,-2.35521309223996,-2.30554112729674,-2.2786093836318,
-2.22511129654473,-2.20943281412998,-2.20192717358904,-2.20063573008572,
-2.19995347531968,-2.19939858885528,-2.19882852159025,-2.19776072359094,
-2.19416654971323,-2.13515068532766,-2.08586228671401,-2.04325549219508,
-2.04036258537386,-2.03902150996979,-2.0380039144187,-2.03704195638369,
-2.03543484447454,-2.03126032968916,-2.01045218997788,-1.98781184729252,
-1.93712022100112,-1.88177086144202,-1.87854146259793,-1.87751750538504,
-1.87695627175528,-1.87639506981587,-1.8756950394239,-1.87431887846997,
-1.86468977114958,-1.84035880938954,-1.74981029116488,-1.7205967840737,
-1.71779876424528,-1.71644165901951,-1.71547525974014,-1.71456132708982,
-1.71328893729937,-1.71074485705234,-1.6918941968336,-1.66302596664332,
-1.56477314682159,-1.55617688403716,-1.55474568459255,-1.55403214436791,
-1.55346835826835,-1.5528397679191,-1.55181425263314,-1.54816927035647,
-1.49540073323149,-1.42244268210306,-1.41643427660268,-1.41490473331247,
-1.41367568772917,-1.41267045482983,-1.3967854237545,-1.39416199335293,
-1.3928734568801,-1.39186289285044,-1.39074199697456,-1.38890016081082,
-1.3825248885946,-1.37013824341392),.UNSPECIFIED.);
#303=B_SPLINE_CURVE_WITH_KNOTS('',3,(#53835,#53836,#53837,#53838,#53839,
#53840,#53841,#53842,#53843,#53844,#53845,#53846,#53847,#53848,#53849,#53850,
#53851,#53852,#53853,#53854,#53855,#53856,#53857,#53858,#53859,#53860,#53861,
#53862,#53863,#53864,#53865,#53866,#53867,#53868,#53869,#53870,#53871,#53872,
#53873,#53874,#53875,#53876,#53877,#53878,#53879,#53880,#53881,#53882,#53883,
#53884,#53885,#53886,#53887,#53888,#53889,#53890,#53891,#53892,#53893,#53894,
#53895,#53896,#53897,#53898,#53899,#53900,#53901,#53902,#53903,#53904,#53905,
#53906,#53907,#53908,#53909,#53910,#53911,#53912,#53913,#53914,#53915,#53916,
#53917,#53918,#53919,#53920,#53921,#53922,#53923,#53924,#53925,#53926,#53927,
#53928,#53929,#53930,#53931,#53932,#53933,#53934,#53935,#53936,#53937,#53938,
#53939,#53940,#53941,#53942,#53943,#53944,#53945,#53946,#53947,#53948,#53949,
#53950,#53951,#53952,#53953,#53954,#53955,#53956,#53957,#53958,#53959,#53960,
#53961,#53962,#53963,#53964,#53965,#53966,#53967,#53968,#53969,#53970,#53971,
#53972,#53973,#53974,#53975,#53976,#53977,#53978,#53979,#53980,#53981,#53982,
#53983,#53984,#53985,#53986,#53987,#53988,#53989,#53990,#53991,#53992,#53993,
#53994,#53995,#53996,#53997,#53998,#53999,#54000,#54001,#54002,#54003,#54004,
#54005,#54006,#54007,#54008,#54009,#54010,#54011,#54012,#54013,#54014,#54015,
#54016,#54017,#54018,#54019,#54020,#54021,#54022,#54023,#54024,#54025,#54026,
#54027,#54028,#54029,#54030,#54031,#54032,#54033,#54034,#54035,#54036,#54037,
#54038,#54039,#54040,#54041,#54042,#54043,#54044,#54045,#54046,#54047,#54048,
#54049,#54050,#54051,#54052,#54053,#54054,#54055,#54056,#54057,#54058,#54059,
#54060,#54061,#54062,#54063,#54064,#54065,#54066,#54067,#54068,#54069,#54070,
#54071,#54072,#54073,#54074,#54075,#54076,#54077,#54078,#54079,#54080,#54081,
#54082,#54083,#54084,#54085,#54086,#54087,#54088,#54089,#54090,#54091,#54092,
#54093,#54094,#54095,#54096,#54097,#54098,#54099,#54100,#54101,#54102,#54103,
#54104,#54105,#54106,#54107,#54108,#54109,#54110,#54111,#54112,#54113,#54114,
#54115,#54116,#54117,#54118,#54119,#54120,#54121,#54122),.UNSPECIFIED.,
 .F.,.F.,(4,2,2,2,2,2,2,2,2,2,2,2,2,2,2,2,2,2,2,2,2,2,2,2,2,2,2,2,2,2,2,
2,2,2,2,2,2,2,2,2,2,2,2,2,2,2,2,2,2,2,2,2,2,2,2,2,2,2,2,2,2,2,2,2,2,2,2,
2,2,2,2,2,2,2,2,2,2,2,2,2,2,2,2,2,2,2,2,2,2,2,2,2,2,2,2,2,2,2,2,2,2,2,2,
2,2,2,2,2,2,2,2,2,2,2,2,2,2,2,2,2,2,2,2,2,2,2,2,2,2,2,2,2,2,2,2,2,2,2,2,
2,2,2,2,4),(-2.69318633084655,-2.68468189971131,-2.62901886980189,-2.59358385261486,
-2.57815888471765,-2.57576037604458,-2.57451821440602,-2.57351246849581,
-2.57251055381831,-2.5707017714161,-2.56513527608284,-2.47342691501159,
-2.41619156214142,-2.41460209223925,-2.41333750240447,-2.41269922255045,
-2.41214846386,-2.41159184424319,-2.41059046552659,-2.407533750704,-2.3580483760135,
-2.32737650073408,-2.2926250573767,-2.26783909042529,-2.25505787256037,
-2.25277505005589,-2.25155724634622,-2.25055278214558,-2.24953649855788,
-2.24765690425763,-2.24152630608467,-2.1334703514287,-2.1061900057124,-2.09196065723888,
-2.0904647881606,-2.08974051398886,-2.08922928407664,-2.08869114322145,
-2.08793467795128,-2.08593475518338,-2.08451547365857,-2.03241931032881,
-1.95849902994206,-1.95229565717286,-1.95090908787588,-1.94970350773231,
-1.94820413214907,-1.94612142112026,-1.94550970731586,-1.9440935927618,
-1.94353075188207,-1.94193049841695,-1.93819732358864,-1.931382205116,-1.92942365180125,
-1.92827670120633,-1.92727993124663,-1.92603778776043,-1.92364041427127,
-1.90825815619092,-1.87298490227813,-1.77853232995525,-1.7767398253688,
-1.77573850044467,-1.77430844652868,-1.77243137117405,-1.76829925197024,
-1.76718595702541,-1.76653585629744,-1.76603117125563,-1.76536346649817,
-1.76414018999852,-1.75794442464571,-1.74559339366462,-1.72211834279851,
-1.61415189567692,-1.60802408774217,-1.60614466948463,-1.60512833425635,
-1.60414383647961,-1.60295883475556,-1.60168921461032,-1.59971259122766,
-1.59599216804081,-1.56345809253146,-1.47561408669336,-1.46704572282714,
-1.46399299293052,-1.46280719644719,-1.46201637039835,-1.45915605143732,
-1.45826620015512,-1.4565340040094,-1.44582585880636,-1.44443152638571,
-1.4437172976525,-1.44319023010916,-1.44261469843859,-1.441814879094,-1.4399092042381,
-1.43728906151824,-1.40923195361318,-1.29023571293427,-1.28464740773419,
-1.28283561186476,-1.28183298996764,-1.28084765808855,-1.27964078075811,
-1.27834061043929,-1.27629139472202,-1.27238181543328,-1.23704138054412,
-1.13764055517906,-1.13448748439908,-1.12261122048989,-1.12101582918796,
-1.12028017225954,-1.11971334997043,-1.11909641257351,-1.11810176608883,
-1.114771190778,-1.09394592935953,-1.03630271046631,-0.965617323296009,
-0.961241320247126,-0.959602150303799,-0.958633919089758,-0.957640265737019,
-0.956356591841733,-0.954950286968531,-0.952648400346053,-0.948066379927323,
-0.936484854562949,-0.892272423768784,-0.803605205890611,-0.798912359964746,
-0.797849018916853,-0.797154649172445,-0.796649853878687,-0.796020666371372,
-0.794971525543444,-0.791109871842227,-0.702525002647637,-0.662616381948172),
 .UNSPECIFIED.);
#304=B_SPLINE_CURVE_WITH_KNOTS('',3,(#54128,#54129,#54130,#54131,#54132,
#54133,#54134,#54135,#54136,#54137,#54138,#54139,#54140,#54141,#54142,#54143,
#54144,#54145,#54146,#54147,#54148,#54149,#54150,#54151,#54152,#54153,#54154,
#54155,#54156,#54157,#54158,#54159,#54160,#54161,#54162,#54163,#54164,#54165,
#54166,#54167,#54168,#54169,#54170,#54171,#54172,#54173,#54174,#54175,#54176,
#54177,#54178,#54179,#54180,#54181,#54182,#54183,#54184,#54185,#54186,#54187,
#54188,#54189,#54190,#54191,#54192,#54193,#54194,#54195,#54196,#54197,#54198,
#54199,#54200,#54201,#54202,#54203,#54204,#54205,#54206,#54207,#54208,#54209,
#54210,#54211,#54212,#54213,#54214,#54215,#54216,#54217,#54218,#54219,#54220,
#54221,#54222,#54223,#54224,#54225,#54226,#54227,#54228,#54229,#54230,#54231,
#54232,#54233,#54234,#54235,#54236,#54237,#54238,#54239,#54240,#54241,#54242,
#54243,#54244,#54245,#54246,#54247,#54248,#54249,#54250,#54251,#54252,#54253,
#54254,#54255,#54256,#54257,#54258,#54259,#54260,#54261,#54262,#54263,#54264,
#54265,#54266,#54267,#54268,#54269),.UNSPECIFIED.,.F.,.F.,(4,3,3,3,3,3,
3,3,3,3,3,3,3,3,3,3,3,3,3,3,3,3,3,3,3,3,3,3,3,3,3,3,3,3,3,3,3,3,3,3,3,3,
3,3,3,3,3,4),(530.929158456835,531.052637619016,531.16549756215,531.258593500593,
531.351563238514,531.444434384569,531.537237389033,531.630005035794,531.72276212552,
531.815533443563,531.908403502849,532.001325128654,532.09440160901,532.165212217623,
532.25831400871,532.351290023229,532.44416785562,532.536978127893,532.629753395939,
532.722518449069,532.815298061554,532.908176871882,533.001107515518,533.094193352236,
533.164926873096,533.257859329747,533.350665369314,533.443372805973,533.536012735091,
533.628617739324,533.72121280114,533.813822888242,533.906533935418,533.999297525186,
534.092219217153,534.164641528569,534.257899915445,534.351031676825,534.444064216637,
534.537027017635,534.629953427148,534.722868062142,534.81579552324,534.908818599269,
535.001891738338,535.095115714291,535.164356184042,535.166163310789),
 .UNSPECIFIED.);
#305=B_SPLINE_CURVE_WITH_KNOTS('',3,(#54270,#54271,#54272,#54273,#54274,
#54275,#54276,#54277,#54278,#54279,#54280,#54281,#54282,#54283,#54284,#54285,
#54286,#54287,#54288,#54289,#54290,#54291,#54292,#54293,#54294,#54295,#54296,
#54297,#54298,#54299,#54300,#54301,#54302,#54303,#54304,#54305,#54306,#54307,
#54308,#54309,#54310,#54311,#54312,#54313,#54314,#54315,#54316,#54317,#54318,
#54319,#54320,#54321,#54322,#54323,#54324,#54325,#54326,#54327,#54328,#54329,
#54330,#54331,#54332,#54333,#54334,#54335,#54336,#54337,#54338,#54339,#54340,
#54341,#54342,#54343,#54344,#54345,#54346,#54347,#54348,#54349,#54350,#54351,
#54352,#54353,#54354,#54355,#54356,#54357,#54358,#54359),.UNSPECIFIED.,
 .F.,.F.,(4,2,2,2,2,2,2,2,2,2,2,2,2,2,2,2,2,2,2,2,2,2,2,2,2,2,2,2,2,2,2,
2,2,2,2,2,2,2,2,2,2,2,2,2,4),(-4.06120165931072,-3.99556616212286,-3.98100786531949,
-3.97893812531483,-3.9776297672892,-3.97640015224412,-3.97549263921484,
-3.97450970358573,-3.97279253435601,-3.96788668347697,-3.89165199918798,
-3.87798823616661,-3.86490937232147,-3.83116870365376,-3.81724161128324,
-3.81603487504353,-3.81528433947467,-3.81458531640765,-3.81402452781977,
-3.81337990397929,-3.81228989916152,-3.80838144823366,-3.74246203805211,
-3.70730130462808,-3.67235221308252,-3.66228138304682,-3.65604127753915,
-3.65469821697044,-3.65344307205196,-3.65253117973898,-3.65155723056532,
-3.64989048068315,-3.64533780914025,-3.5723954348527,-3.52500010899046,
-3.49620307353646,-3.4930899070106,-3.49236473420255,-3.49168361836464,
-3.49112850877089,-3.49055724885437,-3.48948388855584,-3.48584250936362,
-3.42682380920632,-3.39990807077895),.UNSPECIFIED.);
#306=B_SPLINE_CURVE_WITH_KNOTS('',3,(#54361,#54362,#54363,#54364,#54365,
#54366,#54367,#54368,#54369,#54370,#54371,#54372,#54373,#54374,#54375,#54376,
#54377,#54378,#54379,#54380,#54381,#54382,#54383,#54384,#54385,#54386,#54387,
#54388,#54389,#54390,#54391,#54392,#54393,#54394,#54395,#54396,#54397,#54398,
#54399,#54400,#54401,#54402,#54403,#54404,#54405,#54406,#54407,#54408,#54409,
#54410,#54411,#54412,#54413,#54414,#54415,#54416,#54417,#54418,#54419,#54420,
#54421,#54422,#54423,#54424,#54425,#54426,#54427,#54428,#54429,#54430,#54431,
#54432,#54433,#54434,#54435,#54436,#54437,#54438,#54439,#54440,#54441,#54442,
#54443,#54444,#54445,#54446,#54447,#54448,#54449,#54450,#54451,#54452,#54453,
#54454,#54455,#54456,#54457,#54458),.UNSPECIFIED.,.F.,.F.,(4,2,2,2,2,2,
2,2,2,2,2,2,2,2,2,2,2,2,2,2,2,2,2,2,2,2,2,2,2,2,2,2,2,2,2,2,2,2,2,2,2,2,
2,2,2,2,2,2,4),(-0.662616381948172,-0.64164880803953,-0.637897976118936,
-0.636515187629546,-0.635541726181257,-0.634549081404025,-0.633278685576807,
-0.63189086355378,-0.629633248732558,-0.625170855294313,-0.61399416417033,
-0.572785370659433,-0.493947957375361,-0.493711805681332,-0.492791178666353,
-0.490673153084149,-0.488474518141173,-0.476513162116398,-0.474914391141096,
-0.474178044652392,-0.473611046546962,-0.47299424284865,-0.472000616741548,
-0.468680689247441,-0.447967400117738,-0.394237912593299,-0.366862630515129,
-0.318228718518348,-0.314817303857046,-0.313489208844909,-0.312530376067834,
-0.311531151009546,-0.310217224666995,-0.308769271225943,-0.306367744686909,
-0.30151465508055,-0.289003716759519,-0.260179951078527,-0.157145848280909,
-0.156458975464507,-0.152608438781245,-0.151524390496064,-0.150881020782156,
-0.150324841857773,-0.14962528217131,-0.148251833042149,-0.138708384617437,
-0.109414066723253,-0.00125715268977482),.UNSPECIFIED.);
#307=B_SPLINE_CURVE_WITH_KNOTS('',3,(#54459,#54460,#54461,#54462,#54463,
#54464,#54465,#54466,#54467,#54468,#54469,#54470,#54471,#54472,#54473,#54474,
#54475,#54476,#54477,#54478,#54479,#54480,#54481,#54482,#54483,#54484,#54485,
#54486,#54487,#54488,#54489,#54490,#54491,#54492,#54493,#54494,#54495,#54496,
#54497,#54498,#54499,#54500,#54501,#54502,#54503,#54504,#54505,#54506,#54507,
#54508,#54509,#54510,#54511,#54512,#54513,#54514,#54515,#54516,#54517,#54518,
#54519,#54520,#54521,#54522,#54523,#54524,#54525,#54526,#54527,#54528,#54529,
#54530,#54531,#54532,#54533,#54534,#54535,#54536,#54537,#54538,#54539,#54540,
#54541,#54542,#54543,#54544,#54545,#54546,#54547,#54548,#54549,#54550,#54551,
#54552,#54553,#54554,#54555,#54556,#54557,#54558,#54559,#54560,#54561,#54562,
#54563,#54564,#54565,#54566,#54567,#54568,#54569,#54570,#54571,#54572,#54573,
#54574,#54575,#54576,#54577,#54578,#54579,#54580,#54581,#54582,#54583,#54584,
#54585,#54586,#54587,#54588,#54589,#54590,#54591,#54592,#54593,#54594,#54595,
#54596,#54597,#54598,#54599,#54600,#54601,#54602,#54603,#54604,#54605,#54606,
#54607,#54608,#54609,#54610,#54611,#54612,#54613,#54614,#54615,#54616,#54617,
#54618,#54619,#54620,#54621,#54622,#54623,#54624,#54625,#54626,#54627,#54628,
#54629,#54630,#54631,#54632,#54633,#54634,#54635,#54636,#54637,#54638,#54639,
#54640,#54641,#54642,#54643,#54644,#54645,#54646,#54647,#54648,#54649,#54650,
#54651,#54652,#54653,#54654,#54655,#54656,#54657,#54658,#54659,#54660,#54661,
#54662,#54663,#54664,#54665,#54666,#54667,#54668,#54669,#54670,#54671,#54672,
#54673,#54674),.UNSPECIFIED.,.F.,.F.,(4,2,2,2,2,2,2,2,2,2,2,2,2,2,2,2,2,
2,2,2,2,2,2,2,2,2,2,2,2,2,2,2,2,2,2,2,2,2,2,2,2,2,2,2,2,2,2,2,2,2,2,2,2,
2,2,2,2,2,2,2,2,2,2,2,2,2,2,2,2,2,2,2,2,2,2,2,2,2,2,2,2,2,2,2,2,2,2,2,2,
2,2,2,2,2,2,2,2,2,2,2,2,2,2,2,2,2,2,4),(1.37016181069821,1.42817268469703,
1.43200789933298,1.4334043543174,1.43438203013633,1.43537430296662,1.43663677632357,
1.43801348135637,1.44024370600046,1.44463111947928,1.48764134481077,1.54213760195462,
1.57822754550834,1.59336649479065,1.59490244891858,1.59565235976803,1.59618873660573,
1.59670049655204,1.5974293882397,1.59895029045889,1.61458255189288,1.63988811921059,
1.66725202696257,1.69662547519539,1.75179430896636,1.75529151678636,1.75663302485728,
1.75759481634359,1.75859105417611,1.75988892862895,1.76131698188804,1.76367177007154,
1.76839864651118,1.78047706797543,1.80758781690462,1.85791906130342,1.91404750363126,
1.9174869532328,1.91853600457507,1.91910199293259,1.91966253425858,1.92035349183607,
1.92168516994251,1.93010503266359,1.94914762418543,2.02148620295153,2.07495196764682,
2.07841802830152,2.07975558937835,2.08071725606204,2.08171578725386,2.08302255946685,
2.08446068187745,2.08683800228604,2.09162384915754,2.10389959102975,2.13178495443518,
2.1826741908711,2.21568600659663,2.21886486444212,2.22407936510792,2.2262480248409,
2.22708150158334,2.22874362089204,2.23955254204174,2.24095159668956,2.24166736716192,
2.24219514445802,2.24277072113446,2.24356978772966,2.24547012952699,2.24808092581734,
2.27595191071345,2.30190133861818,2.31035013218035,2.33953350588949,2.39758232981042,
2.40117975856853,2.40253829688532,2.40350531502331,2.40450077042442,2.40578913804006,
2.40720226860933,2.4095201336109,2.41414480801579,2.42586936524387,2.45139749110119,
2.50069788894983,2.55973013283072,2.56333889153213,2.5644085081129,2.56497901478315,
2.56553397610908,2.5662158261787,2.56750507697796,2.57496088242439,2.59056097061397,
2.60402290728547,2.71272255386578,2.71880183510393,2.72385000642219,2.72558885160803,
2.72657683649139,2.72756438226155,2.72853609321891,2.72976473459772,2.73164427745407,
2.73916942421928),.UNSPECIFIED.);
#308=B_SPLINE_CURVE_WITH_KNOTS('',3,(#54678,#54679,#54680,#54681,#54682,
#54683,#54684,#54685,#54686,#54687,#54688,#54689,#54690,#54691,#54692,#54693,
#54694,#54695,#54696,#54697,#54698,#54699,#54700,#54701,#54702,#54703,#54704,
#54705,#54706,#54707,#54708,#54709,#54710,#54711,#54712,#54713,#54714,#54715,
#54716,#54717,#54718,#54719,#54720,#54721,#54722,#54723,#54724,#54725,#54726,
#54727,#54728,#54729,#54730,#54731,#54732,#54733,#54734,#54735,#54736,#54737,
#54738,#54739,#54740,#54741,#54742,#54743,#54744,#54745,#54746,#54747,#54748,
#54749,#54750),.UNSPECIFIED.,.F.,.F.,(4,3,3,3,3,3,3,3,3,3,3,3,3,3,3,3,3,
3,3,3,3,3,3,3,4),(-4.09274904019423,-3.99885862189133,-3.91013003463561,
-3.82151667028217,-3.73299492467159,-3.64126355488995,-3.55284687784964,
-3.46444494479893,-3.37603656732219,-3.28760055766733,-3.19906748037989,
-3.11047662341899,-3.02175922454557,-2.9991439664185,-2.9113117185417,-2.82359170340724,
-2.73595935458353,-2.64838791647642,-2.56084790305327,-2.47331725290167,
-2.38577391662778,-2.29814419020479,-2.21046845995505,-2.12265849831354,
-2.0615024666646),.UNSPECIFIED.);
#309=B_SPLINE_CURVE_WITH_KNOTS('',3,(#54754,#54755,#54756,#54757,#54758),
 .UNSPECIFIED.,.F.,.F.,(4,1,4),(0.,0.999714655472842,1.11004521091312),
 .UNSPECIFIED.);
#310=B_SPLINE_CURVE_WITH_KNOTS('',3,(#54760,#54761,#54762,#54763,#54764,
#54765,#54766,#54767,#54768,#54769,#54770,#54771,#54772,#54773,#54774,#54775,
#54776,#54777,#54778,#54779,#54780,#54781,#54782,#54783,#54784,#54785,#54786,
#54787,#54788,#54789,#54790,#54791,#54792,#54793,#54794,#54795,#54796,#54797,
#54798,#54799,#54800,#54801,#54802,#54803,#54804,#54805,#54806,#54807,#54808,
#54809,#54810,#54811,#54812,#54813,#54814,#54815,#54816,#54817,#54818,#54819,
#54820,#54821,#54822,#54823,#54824,#54825,#54826,#54827,#54828,#54829,#54830,
#54831,#54832,#54833,#54834,#54835,#54836,#54837,#54838,#54839,#54840,#54841,
#54842,#54843,#54844,#54845,#54846,#54847,#54848,#54849,#54850,#54851,#54852,
#54853,#54854,#54855,#54856,#54857,#54858,#54859,#54860,#54861,#54862,#54863,
#54864,#54865,#54866,#54867,#54868,#54869,#54870,#54871,#54872,#54873,#54874,
#54875,#54876,#54877,#54878,#54879,#54880,#54881,#54882,#54883,#54884,#54885,
#54886,#54887,#54888,#54889,#54890,#54891,#54892,#54893,#54894,#54895,#54896,
#54897,#54898,#54899,#54900,#54901,#54902,#54903,#54904,#54905,#54906,#54907,
#54908,#54909,#54910,#54911,#54912,#54913,#54914,#54915,#54916,#54917,#54918,
#54919,#54920,#54921,#54922,#54923,#54924,#54925,#54926,#54927,#54928,#54929,
#54930,#54931,#54932,#54933,#54934,#54935,#54936,#54937,#54938,#54939,#54940,
#54941,#54942,#54943,#54944,#54945,#54946,#54947,#54948,#54949,#54950,#54951,
#54952,#54953,#54954,#54955,#54956,#54957,#54958,#54959,#54960,#54961,#54962,
#54963,#54964,#54965,#54966,#54967,#54968,#54969,#54970,#54971,#54972,#54973,
#54974,#54975,#54976,#54977,#54978,#54979,#54980,#54981,#54982,#54983,#54984,
#54985),.UNSPECIFIED.,.F.,.F.,(4,3,3,3,3,3,3,3,3,3,3,3,3,3,3,3,3,3,3,3,
3,3,3,3,3,3,3,3,3,3,3,3,3,3,3,3,3,3,3,3,3,3,3,3,3,3,3,3,3,3,3,3,3,3,3,3,
3,3,3,3,3,3,3,3,3,3,3,3,3,3,3,3,3,3,3,4),(1.11004521091312,1.19650607737286,
1.28285954163267,1.37243076279679,1.45864998573532,1.54484568426876,1.63104074825189,
1.71725806627711,1.80356937260469,1.88993662696758,1.9764320828088,1.99942931094568,
2.08812745070002,2.17671106230774,2.26520376443174,2.35694628968009,2.44533579641836,
2.53371128164707,2.62209394913821,2.71050500255831,2.79901433144695,2.88758211323926,
2.97627757213889,2.99914396641851,3.08785485581244,3.17645390358261,3.26496469990875,
3.35670144015657,3.44511561604432,3.53351817191689,3.62193029548219,3.71037317610221,
3.79891771398502,3.88752272128331,3.97625809233711,3.99885862189134,4.08728386431003,
4.17559277707174,4.26380932330746,4.35565481756455,4.44376630278272,4.53186355987564,
4.61996809333743,4.70810140790274,4.79633499959244,4.88462787176457,4.97305177594552,
4.99857327736417,5.08715380295404,5.17561969285427,5.26399471606801,5.35578136816414,
5.4440540997554,5.53231335681461,5.6205804771028,5.70887679887865,5.79727320596014,
5.88572898664489,5.97431467292538,5.99828793283701,6.08685951668191,6.17531672428596,
6.26368333420257,6.35547324096598,6.44373829164684,6.53199015295223,6.62025017209036,
6.70853969699712,6.79692979659758,6.88537954726025,6.97395966042451,6.99800258830984,
7.09680951298944,7.19522907349122,7.29422968025973,7.39323028702825),
 .UNSPECIFIED.);
#311=B_SPLINE_CURVE_WITH_KNOTS('',3,(#54987,#54988,#54989,#54990,#54991,
#54992,#54993,#54994,#54995,#54996),.UNSPECIFIED.,.F.,.F.,(4,1,1,1,1,1,
1,4),(7.3932305180927,7.99771724378266,8.99743189925548,9.9971465547283,
10.9968612102011,11.9965758656739,12.9962905211468,13.6764158252723),
 .UNSPECIFIED.);
#312=B_SPLINE_CURVE_WITH_KNOTS('',3,(#54998,#54999,#55000,#55001,#55002,
#55003,#55004,#55005,#55006,#55007),.UNSPECIFIED.,.F.,.F.,(4,1,1,1,1,1,
1,4),(13.6764158252723,13.9960051766196,14.9957198320924,15.9954344875653,
16.9951491430381,17.994863798511,18.9945784539838,19.9595964226787),
 .UNSPECIFIED.);
#313=B_SPLINE_CURVE_WITH_KNOTS('',3,(#55009,#55010,#55011,#55012,#55013,
#55014,#55015,#55016,#55017,#55018,#55019,#55020,#55021,#55022,#55023,#55024,
#55025,#55026,#55027,#55028,#55029,#55030,#55031,#55032,#55033,#55034,#55035,
#55036,#55037,#55038,#55039,#55040,#55041,#55042,#55043,#55044,#55045,#55046,
#55047,#55048,#55049,#55050,#55051,#55052,#55053,#55054,#55055,#55056,#55057,
#55058,#55059,#55060,#55061,#55062,#55063,#55064,#55065,#55066,#55067,#55068,
#55069,#55070,#55071,#55072,#55073,#55074,#55075,#55076,#55077,#55078,#55079,
#55080,#55081,#55082,#55083,#55084,#55085,#55086,#55087,#55088,#55089,#55090,
#55091,#55092,#55093,#55094,#55095,#55096,#55097,#55098,#55099,#55100,#55101,
#55102,#55103,#55104,#55105,#55106,#55107,#55108,#55109,#55110,#55111,#55112,
#55113,#55114,#55115,#55116,#55117,#55118,#55119,#55120,#55121,#55122,#55123,
#55124,#55125,#55126,#55127,#55128,#55129,#55130,#55131,#55132,#55133,#55134,
#55135,#55136,#55137,#55138,#55139,#55140,#55141,#55142,#55143,#55144,#55145,
#55146,#55147,#55148,#55149,#55150,#55151,#55152,#55153,#55154,#55155,#55156,
#55157,#55158,#55159,#55160,#55161,#55162,#55163,#55164,#55165,#55166,#55167,
#55168,#55169,#55170,#55171,#55172,#55173,#55174,#55175,#55176,#55177,#55178,
#55179,#55180,#55181,#55182,#55183,#55184,#55185,#55186,#55187,#55188,#55189,
#55190,#55191,#55192,#55193,#55194,#55195,#55196,#55197,#55198,#55199,#55200,
#55201,#55202,#55203,#55204,#55205,#55206,#55207,#55208,#55209,#55210,#55211,
#55212,#55213,#55214,#55215,#55216,#55217,#55218,#55219,#55220,#55221,#55222,
#55223,#55224,#55225,#55226,#55227,#55228,#55229,#55230,#55231,#55232,#55233,
#55234,#55235,#55236,#55237),.UNSPECIFIED.,.F.,.F.,(4,3,3,3,3,3,3,3,3,3,
3,3,3,3,3,3,3,3,3,3,3,3,3,3,3,3,3,3,3,3,3,3,3,3,3,3,3,3,3,3,3,3,3,3,3,3,
3,3,3,3,3,3,3,3,3,3,3,3,3,3,3,3,3,3,3,3,3,3,3,3,3,3,3,3,3,3,4),(19.9596011324519,
19.9942931094567,20.0828452660075,20.1712826660522,20.2596291138166,20.3514264452057,
20.4396705717611,20.5279012623694,20.6161398857834,20.7044078113348,20.7927761166749,
20.8812039325379,20.9697620733111,20.9940077649295,21.0825599166399,21.1709973117995,
21.2593437546402,21.3511410878605,21.4393852094268,21.5276158950304,21.6158545134292,
21.7041224339604,21.792490734298,21.8809185451629,21.9694766809828,21.9937224204023,
22.0822745714392,22.1707119659024,22.2590584080244,22.3508557415058,22.4390998623023,
22.5273305471184,22.615569164713,22.7038370844238,22.7922053839211,22.8806331939328,
22.9691913288876,22.9934370758752,23.0819892286553,23.1704266248874,23.2587730688019,
23.3505704016202,23.4388145242568,23.5270452109275,23.6152838303892,23.7035517519777,
23.7919200533592,23.8803478652613,23.9689060021007,23.993151731348,24.0817038833189,
24.1701412787335,24.2584877218233,24.350285054948,24.438529176747,24.5267598625767,
24.614998481195,24.7032664019385,24.7916347024769,24.8800625135359,24.9686206495389,
24.9928663868208,25.0814185387661,25.1698559341527,25.258202377212,25.3499997103472,
25.4382438321097,25.5264745179007,25.6147131364782,25.7029810571788,25.7913493576714,
25.879777168683,25.9683353046363,25.9925810422937,26.108658292392,26.2221398067425,
26.2427863295604),.UNSPECIFIED.);
#314=B_SPLINE_CURVE_WITH_KNOTS('',3,(#55239,#55240,#55241,#55242,#55243,
#55244,#55245,#55246,#55247,#55248),.UNSPECIFIED.,.F.,.F.,(4,1,1,1,1,1,
1,4),(26.2427864396315,26.9922956977665,27.9920103532393,28.9917250087122,
29.991439664185,30.9911543196578,31.9908689751307,32.525971746811),
 .UNSPECIFIED.);
#315=B_SPLINE_CURVE_WITH_KNOTS('',3,(#55250,#55251,#55252,#55253,#55254,
#55255,#55256,#55257,#55258,#55259,#55260,#55261,#55262,#55263,#55264,#55265,
#55266,#55267,#55268,#55269,#55270,#55271,#55272,#55273,#55274,#55275,#55276,
#55277,#55278,#55279,#55280,#55281,#55282,#55283,#55284,#55285,#55286,#55287,
#55288,#55289,#55290,#55291,#55292,#55293,#55294,#55295,#55296,#55297,#55298,
#55299,#55300,#55301,#55302,#55303,#55304,#55305,#55306,#55307,#55308,#55309,
#55310,#55311,#55312,#55313,#55314,#55315,#55316,#55317,#55318,#55319,#55320,
#55321,#55322,#55323,#55324,#55325,#55326,#55327,#55328,#55329,#55330,#55331,
#55332,#55333,#55334,#55335,#55336,#55337,#55338,#55339,#55340,#55341,#55342,
#55343,#55344,#55345,#55346,#55347,#55348,#55349,#55350,#55351,#55352,#55353,
#55354,#55355,#55356,#55357,#55358,#55359,#55360,#55361,#55362,#55363,#55364,
#55365,#55366,#55367,#55368,#55369,#55370,#55371,#55372,#55373,#55374,#55375,
#55376,#55377,#55378,#55379,#55380,#55381,#55382,#55383,#55384,#55385,#55386,
#55387,#55388,#55389,#55390,#55391,#55392,#55393,#55394,#55395,#55396,#55397,
#55398,#55399,#55400,#55401,#55402,#55403,#55404,#55405,#55406,#55407,#55408,
#55409,#55410,#55411,#55412,#55413,#55414,#55415,#55416,#55417,#55418,#55419,
#55420,#55421,#55422,#55423,#55424,#55425,#55426,#55427,#55428,#55429,#55430,
#55431,#55432,#55433,#55434,#55435,#55436,#55437,#55438,#55439,#55440,#55441,
#55442,#55443,#55444,#55445,#55446,#55447,#55448,#55449,#55450,#55451,#55452,
#55453,#55454,#55455,#55456,#55457,#55458,#55459,#55460,#55461,#55462,#55463,
#55464,#55465,#55466,#55467,#55468,#55469,#55470,#55471,#55472,#55473,#55474,
#55475),.UNSPECIFIED.,.F.,.F.,(4,3,3,3,3,3,3,3,3,3,3,3,3,3,3,3,3,3,3,3,
3,3,3,3,3,3,3,3,3,3,3,3,3,3,3,3,3,3,3,3,3,3,3,3,3,3,3,3,3,3,3,3,3,3,3,3,
3,3,3,3,3,3,3,3,3,3,3,3,3,3,3,3,3,3,3,4),(32.5259719395726,32.6198747736003,
32.7140927372386,32.8084686989712,32.9031284200793,32.9905836306035,33.0791357826823,
33.1675731782046,33.2559196214019,33.3477169544862,33.4359610763914,33.5241917623266,
33.6124303810496,33.7006983018971,33.7890666025375,33.8774944136976,33.9660525497995,
33.9902982860763,34.0788504381557,34.1672878336786,34.2556342768766,34.3474316099607,
34.4356757318666,34.5239064178025,34.6121450365262,34.7004129573742,34.7887812580152,
34.877209069176,34.9657672052786,34.9900129415491,35.0785650936291,35.1670024891527,
35.2553489323512,35.347146265435,35.4353903873415,35.523621073278,35.6118596920023,
35.700127612851,35.7884959134927,35.876923724654,35.9654818607572,35.989727597022,
36.0782797491015,36.1667171446245,36.2550635878225,36.3468609209065,36.4351050428125,
36.5233357287484,36.6115743474721,36.6998422683203,36.7882105689614,36.8766383801223,
36.965196516225,36.9894422524948,37.0779944045744,37.1664318000975,37.2547782432956,
37.3465755763796,37.4348196982857,37.5230503842218,37.6112890029456,37.6995569237938,
37.787925224435,37.876353035596,37.9649111716988,37.9891569079676,38.0763924369636,
38.167988014092,38.2550056857047,38.3419692858987,38.4289013632082,38.5158244322685,
38.6027961903102,38.6897963120411,38.7768888180479,38.8091570539906),
 .UNSPECIFIED.);
#316=B_SPLINE_CURVE_WITH_KNOTS('',3,(#55477,#55478,#55479,#55480,#55481,
#55482,#55483,#55484,#55485,#55486,#55487),.UNSPECIFIED.,.F.,.F.,(4,1,1,
1,1,1,1,1,4),(38.8091570539906,38.9888715634404,39.9885862189133,40.9883008743861,
41.9880155298589,42.9877301853318,43.9874448408046,44.9871594962775,45.0923423611702),
 .UNSPECIFIED.);
#317=B_SPLINE_CURVE_WITH_KNOTS('',3,(#55489,#55490,#55491,#55492,#55493,
#55494,#55495,#55496,#55497,#55498),.UNSPECIFIED.,.F.,.F.,(4,1,1,1,1,1,
1,4),(45.0923423611702,45.9868741517503,46.9865888072231,47.986303462696,
48.9860181181688,49.9857327736416,50.9854474291144,51.3755276683498),
 .UNSPECIFIED.);
#318=B_SPLINE_CURVE_WITH_KNOTS('',3,(#55500,#55501,#55502,#55503,#55504,
#55505,#55506,#55507,#55508,#55509),.UNSPECIFIED.,.F.,.F.,(4,1,1,1,1,1,
1,4),(51.3755276683498,51.9851620845873,52.9848767400601,53.984591395533,
54.9843060510058,55.9840207064786,56.9837353619515,57.6587129755294),
 .UNSPECIFIED.);
#319=B_SPLINE_CURVE_WITH_KNOTS('',3,(#55511,#55512,#55513,#55514,#55515,
#55516,#55517,#55518,#55519,#55520),.UNSPECIFIED.,.F.,.F.,(4,1,1,1,1,1,
1,4),(57.6587129755294,57.9834500174243,58.9831646728971,59.98287932837,
60.9825939838428,61.9823086393156,62.9820232947885,63.9418930085214),
 .UNSPECIFIED.);
#320=B_SPLINE_CURVE_WITH_KNOTS('',3,(#55522,#55523,#55524,#55525,#55526,
#55527,#55528,#55529,#55530,#55531,#55532,#55533,#55534,#55535,#55536,#55537,
#55538,#55539,#55540,#55541,#55542,#55543,#55544,#55545,#55546,#55547,#55548,
#55549,#55550,#55551,#55552,#55553,#55554,#55555,#55556,#55557,#55558,#55559,
#55560,#55561,#55562,#55563,#55564,#55565,#55566,#55567,#55568,#55569,#55570,
#55571,#55572,#55573,#55574,#55575,#55576,#55577,#55578,#55579,#55580,#55581,
#55582,#55583,#55584,#55585,#55586,#55587,#55588,#55589,#55590,#55591,#55592,
#55593,#55594,#55595,#55596,#55597,#55598,#55599,#55600,#55601,#55602,#55603,
#55604,#55605,#55606,#55607,#55608,#55609,#55610,#55611,#55612,#55613,#55614,
#55615,#55616,#55617,#55618,#55619,#55620,#55621,#55622,#55623,#55624,#55625,
#55626,#55627,#55628,#55629,#55630,#55631,#55632,#55633,#55634,#55635,#55636,
#55637,#55638,#55639,#55640,#55641,#55642,#55643,#55644,#55645,#55646,#55647,
#55648,#55649,#55650,#55651,#55652,#55653,#55654,#55655,#55656,#55657,#55658,
#55659,#55660,#55661,#55662,#55663,#55664,#55665,#55666,#55667,#55668,#55669,
#55670,#55671,#55672,#55673,#55674,#55675,#55676,#55677,#55678,#55679,#55680,
#55681,#55682,#55683,#55684,#55685,#55686,#55687,#55688,#55689,#55690,#55691,
#55692,#55693,#55694,#55695,#55696,#55697,#55698,#55699,#55700,#55701,#55702,
#55703,#55704,#55705,#55706,#55707,#55708,#55709,#55710,#55711,#55712,#55713,
#55714,#55715,#55716,#55717,#55718,#55719,#55720,#55721,#55722,#55723,#55724,
#55725,#55726,#55727,#55728,#55729,#55730,#55731,#55732,#55733,#55734,#55735,
#55736,#55737,#55738,#55739,#55740,#55741,#55742,#55743,#55744,#55745,#55746,
#55747,#55748,#55749,#55750),.UNSPECIFIED.,.F.,.F.,(4,3,3,3,3,3,3,3,3,3,
3,3,3,3,3,3,3,3,3,3,3,3,3,3,3,3,3,3,3,3,3,3,3,3,3,3,3,3,3,3,3,3,3,3,3,3,
3,3,3,3,3,3,3,3,3,3,3,3,3,3,3,3,3,3,3,3,3,3,3,3,3,3,3,3,3,3,4),(63.941898282709,
63.9817379502613,64.0702901023407,64.1587274978637,64.2470739410617,64.3388712741458,
64.4271153960517,64.5153460819876,64.6035847007114,64.6918526215597,64.7802209222009,
64.8686487333618,64.9572068694644,64.9814526057341,65.0700047578135,65.1584421533364,
65.2467885965344,65.3385859296185,65.4268300515243,65.5150607374601,65.6032993561838,
65.6915672770317,65.7799355776727,65.8683633888335,65.956921524936,65.9811672612069,
66.0697194132867,66.1581568088099,66.2465032520082,66.3383005850922,66.4265447069984,
66.5147753929347,66.6030140116587,66.6912819325071,66.7796502331486,66.8680780443097,
66.9566361804127,66.9808819166798,67.0694340687594,67.1578714642826,67.2462179074807,
67.3380152405647,67.4262593624707,67.5144900484069,67.6027286671308,67.690996587979,
67.7793648886204,67.8677926997814,67.9563508358842,67.9805965721526,68.0691487242322,
68.1575861197554,68.2459325629534,68.3377298960374,68.4259740179435,68.5142047038796,
68.6024433226034,68.6907112434517,68.7790795440929,68.8675073552539,68.9560654913567,
68.9803112276255,69.0688633797051,69.1573007752283,69.2456472184266,69.3374445515105,
69.4256886734166,69.5139193593527,69.6021579780765,69.6904258989248,69.7787941995661,
69.867222010727,69.9557801468299,69.9800258830983,70.1025546974403,70.2168203982943,
70.2250835117824),.UNSPECIFIED.);
#321=B_SPLINE_CURVE_WITH_KNOTS('',3,(#55752,#55753,#55754,#55755,#55756,
#55757,#55758,#55759,#55760,#55761),.UNSPECIFIED.,.F.,.F.,(4,1,1,1,1,1,
1,4),(70.2250835898886,70.9797405385711,71.979455194044,72.9791698495168,
73.9788845049896,74.9785991604624,75.9783138159352,76.5082688970682),
 .UNSPECIFIED.);
#322=B_SPLINE_CURVE_WITH_KNOTS('',3,(#55763,#55764,#55765,#55766,#55767,
#55768,#55769,#55770,#55771,#55772),.UNSPECIFIED.,.F.,.F.,(4,1,1,1,1,1,
1,4),(76.5082688970682,76.9780284714081,77.9777431268809,78.9774577823538,
79.9771724378266,80.9768870932994,81.9766017487723,82.7914495005134),
 .UNSPECIFIED.);
#323=B_SPLINE_CURVE_WITH_KNOTS('',3,(#55774,#55775,#55776,#55777,#55778,
#55779,#55780,#55781,#55782,#55783,#55784,#55785,#55786,#55787,#55788,#55789,
#55790,#55791,#55792,#55793,#55794,#55795,#55796,#55797,#55798,#55799,#55800,
#55801,#55802,#55803,#55804,#55805,#55806,#55807,#55808,#55809,#55810,#55811,
#55812,#55813,#55814,#55815,#55816,#55817,#55818,#55819,#55820,#55821,#55822,
#55823,#55824,#55825,#55826,#55827,#55828,#55829,#55830,#55831,#55832,#55833,
#55834,#55835,#55836,#55837,#55838,#55839,#55840,#55841,#55842,#55843,#55844,
#55845,#55846,#55847,#55848,#55849,#55850,#55851,#55852,#55853,#55854,#55855,
#55856,#55857,#55858,#55859,#55860,#55861,#55862,#55863,#55864,#55865,#55866,
#55867,#55868,#55869,#55870,#55871,#55872,#55873,#55874,#55875,#55876,#55877,
#55878,#55879,#55880,#55881,#55882,#55883,#55884,#55885,#55886,#55887,#55888,
#55889,#55890,#55891,#55892,#55893,#55894,#55895,#55896,#55897,#55898,#55899,
#55900,#55901,#55902,#55903,#55904,#55905,#55906,#55907,#55908,#55909,#55910,
#55911,#55912,#55913,#55914,#55915,#55916,#55917,#55918,#55919,#55920,#55921,
#55922,#55923,#55924,#55925,#55926,#55927,#55928,#55929,#55930,#55931,#55932,
#55933,#55934,#55935,#55936,#55937,#55938,#55939,#55940,#55941,#55942,#55943,
#55944,#55945,#55946,#55947,#55948,#55949,#55950,#55951,#55952,#55953,#55954,
#55955,#55956,#55957,#55958,#55959,#55960,#55961,#55962,#55963,#55964,#55965,
#55966,#55967,#55968,#55969,#55970,#55971,#55972,#55973,#55974,#55975,#55976,
#55977,#55978,#55979,#55980,#55981,#55982,#55983,#55984,#55985,#55986,#55987,
#55988,#55989,#55990,#55991,#55992,#55993,#55994,#55995,#55996,#55997,#55998,
#55999),.UNSPECIFIED.,.F.,.F.,(4,3,3,3,3,3,3,3,3,3,3,3,3,3,3,3,3,3,3,3,
3,3,3,3,3,3,3,3,3,3,3,3,3,3,3,3,3,3,3,3,3,3,3,3,3,3,3,3,3,3,3,3,3,3,3,3,
3,3,3,3,3,3,3,3,3,3,3,3,3,3,3,3,3,3,3,4),(82.7914542042478,82.9239679358683,
82.9763164042451,83.0648685563247,83.1533059518479,83.2416523950459,83.3334497281299,
83.421693850036,83.5099245359721,83.5981631546961,83.6864310755445,83.7747993761859,
83.8632271873468,83.9517853234496,83.9760310597179,84.0645832117975,84.1530206073208,
84.2413670505189,84.3331643836029,84.4214085055091,84.5096391914452,84.5978778101692,
84.6861457310175,84.7745140316589,84.8629418428199,84.9514999789228,84.9757457151908,
85.0642978672704,85.1527352627935,85.2410817059916,85.3328790390756,85.4211231609817,
85.5093538469178,85.5975924656416,85.6858603864899,85.7742286871312,85.8626564982922,
85.9512146343949,85.9754603706636,86.0640125227432,86.1524499182664,86.2407963614645,
86.3325936945485,86.4208378164545,86.5090685023906,86.5973071211145,86.6855750419628,
86.7739433426041,86.8623711537651,86.9509292898679,86.9751750261364,87.063727178216,
87.1521645737392,87.2405110169374,87.3323083500214,87.4205524719275,87.5087831578636,
87.5970217765875,87.6852896974356,87.7736579980769,87.8620858092379,87.9506439453407,
87.9748896816092,88.0634418336888,88.151879229212,88.24022567241,88.332023005494,
88.4202671274001,88.5084978133362,88.5967364320601,88.6850043529082,88.7733726535495,
88.8618004647105,88.9503586008133,88.9746043370821,89.0746395114274),
 .UNSPECIFIED.);
#324=B_SPLINE_CURVE_WITH_KNOTS('',3,(#56001,#56002,#56003,#56004,#56005,
#56006,#56007,#56008,#56009,#56010),.UNSPECIFIED.,.F.,.F.,(4,1,1,1,1,1,
1,4),(89.0746484612627,89.9743189925549,90.9740336480277,91.9737483035006,
92.9734629589734,93.9731776144462,94.9728922699191,95.3578173614012),
 .UNSPECIFIED.);
#325=B_SPLINE_CURVE_WITH_KNOTS('',3,(#56012,#56013,#56014,#56015,#56016,
#56017,#56018,#56019,#56020,#56021,#56022,#56023,#56024,#56025,#56026,#56027,
#56028,#56029,#56030,#56031,#56032,#56033,#56034,#56035,#56036,#56037,#56038,
#56039,#56040,#56041,#56042,#56043,#56044,#56045,#56046,#56047,#56048,#56049,
#56050,#56051,#56052,#56053,#56054,#56055,#56056,#56057,#56058,#56059,#56060,
#56061,#56062,#56063,#56064,#56065,#56066,#56067,#56068,#56069,#56070,#56071,
#56072,#56073,#56074,#56075,#56076,#56077,#56078,#56079,#56080,#56081,#56082,
#56083,#56084,#56085,#56086,#56087,#56088,#56089,#56090,#56091,#56092,#56093,
#56094,#56095,#56096,#56097,#56098,#56099,#56100,#56101,#56102,#56103,#56104,
#56105,#56106,#56107,#56108,#56109,#56110,#56111,#56112,#56113,#56114,#56115,
#56116,#56117,#56118,#56119,#56120,#56121,#56122,#56123,#56124,#56125,#56126,
#56127,#56128,#56129,#56130,#56131,#56132,#56133,#56134,#56135,#56136,#56137,
#56138,#56139,#56140,#56141,#56142,#56143,#56144,#56145,#56146,#56147,#56148,
#56149,#56150,#56151,#56152,#56153,#56154,#56155,#56156,#56157,#56158,#56159,
#56160,#56161,#56162,#56163,#56164,#56165,#56166,#56167,#56168,#56169,#56170,
#56171,#56172,#56173,#56174,#56175,#56176,#56177,#56178,#56179,#56180,#56181,
#56182,#56183,#56184,#56185,#56186,#56187,#56188,#56189,#56190,#56191,#56192,
#56193,#56194,#56195,#56196,#56197,#56198,#56199,#56200,#56201,#56202,#56203,
#56204,#56205,#56206,#56207,#56208,#56209,#56210,#56211,#56212,#56213,#56214,
#56215,#56216,#56217,#56218,#56219,#56220,#56221,#56222,#56223,#56224,#56225,
#56226,#56227,#56228,#56229,#56230,#56231,#56232,#56233,#56234,#56235,#56236,
#56237),.UNSPECIFIED.,.F.,.F.,(4,3,3,3,3,3,3,3,3,3,3,3,3,3,3,3,3,3,3,3,
3,3,3,3,3,3,3,3,3,3,3,3,3,3,3,3,3,3,3,3,3,3,3,3,3,3,3,3,3,3,3,3,3,3,3,3,
3,3,3,3,3,3,3,3,3,3,3,3,3,3,3,3,3,3,3,4),(95.3578248186069,95.4469228467246,
95.5360360002453,95.6251842465887,95.7144518819726,95.8037810607741,95.8932749187053,
95.9726069253919,96.0611590774715,96.1495964729946,96.2379429161925,96.3297402492765,
96.4179843711827,96.5062150571188,96.5944536758426,96.6827215966912,96.7710898973325,
96.8595177084935,96.9480758445963,96.9723215808647,97.0608737329443,97.1493111284676,
97.2376575716657,97.3294549047497,97.4176990266558,97.505929712592,97.5941683313159,
97.6824362521645,97.7708045528058,97.8592323639669,97.9477905000696,97.9720362363376,
98.0605883884171,98.1490257839403,98.2373722271387,98.3291695602226,98.4174136821287,
98.5056443680648,98.5938829867886,98.6821509076364,98.7705192082777,98.8589470194386,
98.9475051555416,98.9717508918104,99.0603030438901,99.1487404394132,99.2370868826112,
99.3288842156952,99.4171283376014,99.5053590235375,99.5935976422613,99.6818655631093,
99.7702338637505,99.8586616749113,99.947219811014,99.9714655472833,100.060017699363,
100.148455094886,100.236801538084,100.328598871168,100.416842993074,100.50507367901,
100.593312297734,100.681580218582,100.769948519224,100.858376330385,100.946934466487,
100.971180202756,101.05961993014,101.147948157046,101.236186505253,101.324356520768,
101.412486320201,101.500591756939,101.58871623251,101.641010125787),
 .UNSPECIFIED.);
#326=B_SPLINE_CURVE_WITH_KNOTS('',3,(#56239,#56240,#56241,#56242,#56243,
#56244,#56245,#56246,#56247,#56248),.UNSPECIFIED.,.F.,.F.,(4,1,1,1,1,1,
1,4),(101.641017304817,101.970894858229,102.970609513702,103.970324169175,
104.970038824647,105.96975348012,106.969468135593,107.924195432966),
 .UNSPECIFIED.);
#327=B_SPLINE_CURVE_WITH_KNOTS('',3,(#56250,#56251,#56252,#56253,#56254,
#56255,#56256,#56257,#56258,#56259,#56260,#56261),.UNSPECIFIED.,.F.,.F.,
(4,2,1,1,1,1,1,1,4),(107.924195432966,107.969182791066,108.968897446539,
109.968612102012,110.968326757484,111.968041412957,112.96775606843,113.967470723903,
114.207380740146),.UNSPECIFIED.);
#328=B_SPLINE_CURVE_WITH_KNOTS('',3,(#56263,#56264,#56265,#56266,#56267,
#56268,#56269,#56270,#56271,#56272),.UNSPECIFIED.,.F.,.F.,(4,1,1,1,1,1,
1,4),(114.207380740146,114.967185379376,115.966900034849,116.966614690321,
117.966329345794,118.966044001267,119.96575865674,120.490566047325),
 .UNSPECIFIED.);
#329=B_SPLINE_CURVE_WITH_KNOTS('',3,(#56274,#56275,#56276,#56277,#56278,
#56279,#56280,#56281,#56282,#56283),.UNSPECIFIED.,.F.,.F.,(4,1,1,1,1,1,
1,4),(120.490566047325,120.965473312213,121.965187967686,122.964902623158,
123.964617278631,124.964331934104,125.964046589577,126.773747127373),
 .UNSPECIFIED.);
#330=B_SPLINE_CURVE_WITH_KNOTS('',3,(#56285,#56286,#56287,#56288,#56289,
#56290,#56291,#56292,#56293,#56294,#56295,#56296,#56297,#56298,#56299,#56300,
#56301,#56302,#56303,#56304,#56305,#56306,#56307,#56308,#56309,#56310,#56311,
#56312,#56313,#56314,#56315,#56316,#56317,#56318,#56319,#56320,#56321,#56322,
#56323,#56324,#56325,#56326,#56327,#56328,#56329,#56330,#56331,#56332,#56333,
#56334,#56335,#56336,#56337,#56338,#56339,#56340,#56341,#56342,#56343,#56344,
#56345,#56346,#56347,#56348,#56349,#56350,#56351,#56352,#56353,#56354,#56355,
#56356,#56357,#56358,#56359,#56360,#56361,#56362,#56363,#56364,#56365,#56366,
#56367,#56368,#56369,#56370,#56371,#56372,#56373,#56374,#56375,#56376,#56377,
#56378,#56379,#56380,#56381,#56382,#56383,#56384,#56385,#56386,#56387,#56388,
#56389,#56390,#56391,#56392,#56393,#56394,#56395,#56396,#56397,#56398,#56399,
#56400,#56401,#56402,#56403,#56404,#56405,#56406,#56407,#56408,#56409,#56410,
#56411,#56412,#56413,#56414,#56415,#56416,#56417,#56418,#56419,#56420,#56421,
#56422,#56423,#56424,#56425,#56426,#56427,#56428,#56429,#56430,#56431,#56432,
#56433,#56434,#56435,#56436,#56437,#56438,#56439,#56440,#56441,#56442,#56443,
#56444,#56445,#56446,#56447,#56448,#56449,#56450,#56451,#56452,#56453,#56454,
#56455,#56456,#56457,#56458,#56459,#56460,#56461,#56462,#56463,#56464,#56465,
#56466,#56467,#56468,#56469,#56470,#56471,#56472,#56473,#56474,#56475,#56476,
#56477,#56478,#56479,#56480,#56481,#56482,#56483,#56484,#56485,#56486,#56487,
#56488,#56489,#56490,#56491,#56492,#56493,#56494,#56495,#56496,#56497,#56498,
#56499,#56500,#56501,#56502,#56503,#56504,#56505,#56506,#56507,#56508,#56509,
#56510),.UNSPECIFIED.,.F.,.F.,(4,3,3,3,3,3,3,3,3,3,3,3,3,3,3,3,3,3,3,3,
3,3,3,3,3,3,3,3,3,3,3,3,3,3,3,3,3,3,3,3,3,3,3,3,3,3,3,3,3,3,3,3,3,3,3,3,
3,3,3,3,3,3,3,3,3,3,3,3,3,3,3,3,3,3,3,4),(126.773751354505,126.904300810836,
126.96376124505,127.05231339713,127.140750792653,127.229097235851,127.320894568935,
127.409138690841,127.497369376777,127.5856079955,127.673875916349,127.76224421699,
127.850672028151,127.939230164253,127.963475900523,128.052028052602,128.140465448125,
128.228811891323,128.320609224407,128.408853346313,128.497084032249,128.585322650973,
128.673590571821,128.761958872462,128.850386683623,128.938944819725,128.963190555995,
129.051742708075,129.140180103598,129.228526546796,129.32032387988,129.408568001786,
129.496798687722,129.585037306446,129.673305227294,129.761673527936,129.850101339097,
129.9386594752,129.962905211468,130.051457363548,130.139894759071,130.228241202269,
130.320038535353,130.408282657259,130.496513343196,130.58475196192,130.673019882768,
130.76138818341,130.849815994571,130.938374130674,130.962619866941,131.051172019021,
131.139609414544,131.227955857742,131.319753190826,131.407997312732,131.496227998668,
131.584466617392,131.67273453824,131.761102838881,131.849530650042,131.938088786145,
131.962334522414,132.050886674494,132.139324070017,132.227670513215,132.319467846299,
132.407711968205,132.495942654141,132.584181272865,132.672449193713,132.760817494355,
132.849245305516,132.937803441618,132.962049177887,133.056936661685),
 .UNSPECIFIED.);
#331=B_SPLINE_CURVE_WITH_KNOTS('',3,(#56512,#56513,#56514,#56515,#56516,
#56517,#56518,#56519,#56520,#56521),.UNSPECIFIED.,.F.,.F.,(4,1,1,1,1,1,
1,4),(133.056945554371,133.96176383336,134.961478488832,135.961193144305,
136.960907799778,137.960622455251,138.960337110724,139.340114405502),
 .UNSPECIFIED.);
#332=B_SPLINE_CURVE_WITH_KNOTS('',3,(#56523,#56524,#56525,#56526,#56527,
#56528,#56529,#56530,#56531,#56532,#56533,#56534,#56535,#56536,#56537,#56538,
#56539,#56540,#56541,#56542,#56543,#56544,#56545,#56546,#56547,#56548,#56549,
#56550,#56551,#56552,#56553,#56554,#56555,#56556,#56557,#56558,#56559,#56560,
#56561,#56562,#56563,#56564,#56565,#56566,#56567,#56568,#56569,#56570,#56571,
#56572,#56573,#56574,#56575,#56576,#56577,#56578,#56579,#56580,#56581,#56582,
#56583,#56584,#56585,#56586,#56587,#56588,#56589,#56590,#56591,#56592,#56593,
#56594,#56595,#56596,#56597,#56598,#56599,#56600,#56601,#56602,#56603,#56604,
#56605,#56606,#56607,#56608,#56609,#56610,#56611,#56612,#56613,#56614,#56615,
#56616,#56617,#56618,#56619,#56620,#56621,#56622,#56623,#56624,#56625,#56626,
#56627,#56628,#56629,#56630,#56631,#56632,#56633,#56634,#56635,#56636,#56637,
#56638,#56639,#56640,#56641,#56642,#56643,#56644,#56645,#56646,#56647,#56648,
#56649,#56650,#56651,#56652,#56653,#56654,#56655,#56656,#56657,#56658,#56659,
#56660,#56661,#56662,#56663,#56664,#56665,#56666,#56667,#56668,#56669,#56670,
#56671,#56672,#56673,#56674,#56675,#56676,#56677,#56678,#56679,#56680,#56681,
#56682,#56683,#56684,#56685,#56686,#56687,#56688,#56689,#56690,#56691,#56692,
#56693,#56694,#56695,#56696,#56697,#56698,#56699,#56700,#56701,#56702,#56703,
#56704,#56705,#56706,#56707,#56708,#56709,#56710,#56711,#56712,#56713,#56714,
#56715,#56716,#56717,#56718,#56719,#56720,#56721,#56722,#56723,#56724,#56725,
#56726,#56727,#56728,#56729,#56730,#56731,#56732,#56733,#56734,#56735,#56736,
#56737,#56738,#56739,#56740,#56741,#56742,#56743,#56744,#56745,#56746,#56747,
#56748),.UNSPECIFIED.,.F.,.F.,(4,3,3,3,3,3,3,3,3,3,3,3,3,3,3,3,3,3,3,3,
3,3,3,3,3,3,3,3,3,3,3,3,3,3,3,3,3,3,3,3,3,3,3,3,3,3,3,3,3,3,3,3,3,3,3,3,
3,3,3,3,3,3,3,3,3,3,3,3,3,3,3,3,3,3,3,4),(139.340121968864,139.429114310097,
139.51811844929,139.607154538274,139.696307192852,139.785518959188,139.874895927097,
139.960051766197,140.048603918276,140.137041313799,140.225387756997,140.317185090081,
140.405429211987,140.493659897922,140.581898516646,140.670166437494,140.758534738135,
140.846962549295,140.935520685398,140.959766421669,141.048318573749,141.136755969272,
141.22510241247,141.316899745554,141.40514386746,141.493374553396,141.58161317212,
141.669881092968,141.758249393609,141.84667720477,141.935235340873,141.959481077142,
142.048033229222,142.136470624745,142.224817067943,142.316614401027,142.404858522933,
142.49308920887,142.581327827594,142.669595748442,142.757964049084,142.846391860245,
142.934949996348,142.959195732615,143.047747884695,143.136185280218,143.224531723416,
143.3163290565,143.404573178406,143.492803864342,143.581042483066,143.669310403914,
143.757678704556,143.846106515716,143.934664651819,143.958910388088,144.047462540168,
144.135899935691,144.224246378889,144.316043711973,144.404287833879,144.492518519815,
144.580757138539,144.669025059388,144.757393360029,144.84582117119,144.934379307293,
144.958625043561,145.047148680272,145.135560075733,145.223880758912,145.312132182873,
145.400341173324,145.48852490424,145.576724249091,145.623307276044),
 .UNSPECIFIED.);
#333=B_SPLINE_CURVE_WITH_KNOTS('',3,(#56750,#56751,#56752,#56753,#56754,
#56755,#56756,#56757,#56758,#56759),.UNSPECIFIED.,.F.,.F.,(4,1,1,1,1,1,
1,4),(145.623314614479,145.958339699034,146.958054354506,147.957769009979,
148.957483665452,149.957198320925,150.956912976398,151.906492583223),
 .UNSPECIFIED.);
#334=B_SPLINE_CURVE_WITH_KNOTS('',3,(#56761,#56762,#56763,#56764,#56765,
#56766,#56767,#56768,#56769,#56770,#56771,#56772),.UNSPECIFIED.,.F.,.F.,
(4,2,1,1,1,1,1,1,4),(151.906492583223,151.956627631871,152.956342287343,
153.956056942816,154.955771598289,155.955486253762,156.955200909235,157.954915564708,
158.189677890403),.UNSPECIFIED.);
#335=B_SPLINE_CURVE_WITH_KNOTS('',3,(#56774,#56775,#56776,#56777,#56778,
#56779,#56780,#56781,#56782,#56783),.UNSPECIFIED.,.F.,.F.,(4,1,1,1,1,1,
1,4),(158.189677890403,158.95463022018,159.954344875653,160.954059531126,
161.953774186599,162.953488842072,163.953203497545,164.472863197582),
 .UNSPECIFIED.);
#336=B_SPLINE_CURVE_WITH_KNOTS('',3,(#56785,#56786,#56787,#56788,#56789,
#56790,#56791,#56792,#56793,#56794),.UNSPECIFIED.,.F.,.F.,(4,1,1,1,1,1,
1,4),(164.472863197582,164.952918153017,165.95263280849,166.952347463963,
167.952062119436,168.951776774909,169.951491430381,170.756044766746),
 .UNSPECIFIED.);
#337=B_SPLINE_CURVE_WITH_KNOTS('',3,(#56796,#56797,#56798,#56799,#56800,
#56801,#56802,#56803,#56804,#56805,#56806,#56807,#56808,#56809,#56810,#56811,
#56812,#56813,#56814,#56815,#56816,#56817,#56818,#56819,#56820,#56821,#56822,
#56823,#56824,#56825,#56826,#56827,#56828,#56829,#56830,#56831,#56832,#56833,
#56834,#56835,#56836,#56837,#56838,#56839,#56840,#56841,#56842,#56843,#56844,
#56845,#56846,#56847,#56848,#56849,#56850,#56851,#56852,#56853,#56854,#56855,
#56856,#56857,#56858,#56859,#56860,#56861,#56862,#56863,#56864,#56865,#56866,
#56867,#56868,#56869,#56870,#56871,#56872,#56873,#56874,#56875,#56876,#56877,
#56878,#56879,#56880,#56881,#56882,#56883,#56884,#56885,#56886,#56887,#56888,
#56889,#56890,#56891,#56892,#56893,#56894,#56895,#56896,#56897,#56898,#56899,
#56900,#56901,#56902,#56903,#56904,#56905,#56906,#56907,#56908,#56909,#56910,
#56911,#56912,#56913,#56914,#56915,#56916,#56917,#56918,#56919,#56920,#56921,
#56922,#56923,#56924,#56925,#56926,#56927,#56928,#56929,#56930,#56931,#56932,
#56933,#56934,#56935,#56936,#56937,#56938,#56939,#56940,#56941,#56942,#56943,
#56944,#56945,#56946,#56947,#56948,#56949,#56950,#56951,#56952,#56953,#56954,
#56955,#56956,#56957,#56958,#56959,#56960,#56961,#56962,#56963,#56964,#56965,
#56966,#56967,#56968,#56969,#56970,#56971,#56972,#56973,#56974,#56975,#56976,
#56977,#56978,#56979,#56980,#56981,#56982,#56983,#56984,#56985,#56986,#56987,
#56988,#56989,#56990,#56991,#56992,#56993,#56994,#56995,#56996,#56997,#56998,
#56999,#57000,#57001,#57002,#57003,#57004,#57005,#57006,#57007,#57008,#57009,
#57010,#57011,#57012,#57013,#57014,#57015,#57016,#57017,#57018,#57019,#57020,
#57021),.UNSPECIFIED.,.F.,.F.,(4,3,3,3,3,3,3,3,3,3,3,3,3,3,3,3,3,3,3,3,
3,3,3,3,3,3,3,3,3,3,3,3,3,3,3,3,3,3,3,3,3,3,3,3,3,3,3,3,3,3,3,3,3,3,3,3,
3,3,3,3,3,3,3,3,3,3,3,3,3,3,3,3,3,3,3,4),(170.756048504762,170.884766228992,
170.951206085854,171.039758237934,171.128195633458,171.216542076657,171.308339409741,
171.396583531648,171.484814217584,171.573052836309,171.661320757158,171.7496890578,
171.838116868962,171.926675005065,171.950920741327,172.039472893407,172.12791028893,
172.216256732128,172.308054065212,172.396298187118,172.484528873054,172.572767491778,
172.661035412626,172.749403713267,172.837831524428,172.926389660531,172.9506353968,
173.03918754888,173.127624944403,173.215971387601,173.307768720685,173.396012842591,
173.484243528527,173.57248214725,173.660750068099,173.74911836874,173.837546179901,
173.926104316003,173.950350052273,174.038902204353,174.127339599876,174.215686043074,
174.307483376158,174.395727498064,174.483958184,174.572196802724,174.660464723573,
174.748833024214,174.837260835375,174.925818971478,174.950064707746,175.038616859826,
175.127054255349,175.215400698547,175.307198031631,175.395442153537,175.483672839474,
175.571911458198,175.660179379046,175.748547679687,175.836975490849,175.925533626951,
175.949779363219,176.038331515298,176.126768910822,176.21511535402,176.306912687103,
176.395156809009,176.483387494945,176.571626113669,176.659894034517,176.748262335158,
176.836690146319,176.925248282422,176.949494018691,177.039233811941),
 .UNSPECIFIED.);
#338=B_SPLINE_CURVE_WITH_KNOTS('',3,(#57023,#57024,#57025,#57026,#57027,
#57028,#57029,#57030,#57031,#57032),.UNSPECIFIED.,.F.,.F.,(4,1,1,1,1,1,
1,4),(177.039242603138,177.949208674164,178.948923329637,179.94863798511,
180.948352640583,181.948067296056,182.947781951528,183.322411476105),
 .UNSPECIFIED.);
#339=B_SPLINE_CURVE_WITH_KNOTS('',3,(#57034,#57035,#57036,#57037,#57038,
#57039,#57040,#57041,#57042,#57043,#57044,#57045,#57046,#57047,#57048,#57049,
#57050,#57051,#57052,#57053,#57054,#57055,#57056,#57057,#57058,#57059,#57060,
#57061,#57062,#57063,#57064,#57065,#57066,#57067,#57068,#57069,#57070,#57071,
#57072,#57073,#57074,#57075,#57076,#57077,#57078,#57079,#57080,#57081,#57082,
#57083,#57084,#57085,#57086,#57087,#57088,#57089,#57090,#57091,#57092,#57093,
#57094,#57095,#57096,#57097,#57098,#57099,#57100,#57101,#57102,#57103,#57104,
#57105,#57106,#57107,#57108,#57109,#57110,#57111,#57112,#57113,#57114,#57115,
#57116,#57117,#57118,#57119,#57120,#57121,#57122,#57123,#57124,#57125,#57126,
#57127,#57128,#57129,#57130,#57131,#57132,#57133,#57134,#57135,#57136,#57137,
#57138,#57139,#57140,#57141,#57142,#57143,#57144,#57145,#57146,#57147,#57148,
#57149,#57150,#57151,#57152,#57153,#57154,#57155,#57156,#57157,#57158,#57159,
#57160,#57161,#57162,#57163,#57164,#57165,#57166,#57167,#57168,#57169,#57170,
#57171,#57172,#57173,#57174,#57175,#57176,#57177,#57178,#57179,#57180,#57181,
#57182,#57183,#57184,#57185,#57186,#57187,#57188,#57189,#57190,#57191,#57192,
#57193,#57194,#57195,#57196,#57197,#57198,#57199,#57200,#57201,#57202,#57203,
#57204,#57205,#57206,#57207,#57208,#57209,#57210,#57211,#57212,#57213,#57214,
#57215,#57216,#57217,#57218,#57219,#57220,#57221,#57222,#57223,#57224,#57225,
#57226,#57227,#57228,#57229,#57230,#57231,#57232,#57233,#57234,#57235,#57236,
#57237,#57238,#57239,#57240,#57241,#57242,#57243,#57244,#57245,#57246,#57247,
#57248,#57249,#57250,#57251,#57252,#57253,#57254,#57255,#57256,#57257,#57258,
#57259),.UNSPECIFIED.,.F.,.F.,(4,3,3,3,3,3,3,3,3,3,3,3,3,3,3,3,3,3,3,3,
3,3,3,3,3,3,3,3,3,3,3,3,3,3,3,3,3,3,3,3,3,3,3,3,3,3,3,3,3,3,3,3,3,3,3,3,
3,3,3,3,3,3,3,3,3,3,3,3,3,3,3,3,3,3,3,4),(183.322419119121,183.411309023726,
183.500207494653,183.589134856038,183.678725293779,183.767823606447,183.857660106724,
183.947496607001,184.036048759081,184.124486154604,184.212832597802,184.304629930886,
184.392874052792,184.481104738728,184.569343357452,184.6576112783,184.745979578942,
184.834407390103,184.922965526206,184.947211262474,185.035763414554,185.124200810077,
185.212547253275,185.304344586359,185.392588708265,185.480819394201,185.569058012925,
185.657325933774,185.745694234415,185.834122045576,185.922680181679,185.946925917947,
186.035478070027,186.12391546555,186.212261908748,186.304059241832,186.392303363738,
186.480534049674,186.568772668398,186.657040589246,186.745408889888,186.833836701049,
186.922394837152,186.94664057342,187.0351927255,187.123630121023,187.211976564221,
187.303773897305,187.392018019211,187.480248705148,187.568487323872,187.65675524472,
187.745123545362,187.833551356523,187.922109492626,187.946355228893,188.034907380972,
188.123344776495,188.211691219693,188.303488552777,188.391732674683,188.479963360619,
188.568201979342,188.656469900191,188.744838200832,188.833266011993,188.921824148096,
188.946069884365,189.034680468163,189.12317803393,189.211584011424,189.299919754286,
189.388210799519,189.476475634494,189.564752692411,189.605604426301),
 .UNSPECIFIED.);
#340=B_SPLINE_CURVE_WITH_KNOTS('',3,(#57261,#57262,#57263,#57264,#57265,
#57266,#57267,#57268,#57269,#57270),.UNSPECIFIED.,.F.,.F.,(4,1,1,1,1,1,
1,4),(189.605611896825,189.945784539838,190.945499195311,191.945213850784,
192.944928506257,193.94464316173,194.944357817202,195.88878973348),
 .UNSPECIFIED.);
#341=B_SPLINE_CURVE_WITH_KNOTS('',3,(#57272,#57273,#57274,#57275,#57276,
#57277,#57278,#57279,#57280,#57281,#57282),.UNSPECIFIED.,.F.,.F.,(4,1,1,
1,1,1,1,1,4),(195.88878973348,195.944072472675,196.943787128148,197.943501783621,
198.943216439094,199.942931094567,200.942645750039,201.942360405512,202.17197504066),
 .UNSPECIFIED.);
#342=B_SPLINE_CURVE_WITH_KNOTS('',3,(#57284,#57285,#57286,#57287,#57288,
#57289,#57290,#57291,#57292,#57293),.UNSPECIFIED.,.F.,.F.,(4,1,1,1,1,1,
1,4),(202.17197504066,202.942075060985,203.941789716458,204.941504371931,
205.941219027403,206.940933682876,207.940648338349,208.455160347839),
 .UNSPECIFIED.);
#343=B_SPLINE_CURVE_WITH_KNOTS('',3,(#57295,#57296,#57297,#57298,#57299,
#57300,#57301,#57302,#57303,#57304),.UNSPECIFIED.,.F.,.F.,(4,1,1,1,1,1,
1,4),(208.455160347839,208.940362993822,209.940077649295,210.939792304768,
211.939506960241,212.939221615713,213.938936271186,214.738345655019),
 .UNSPECIFIED.);
#344=B_SPLINE_CURVE_WITH_KNOTS('',3,(#57306,#57307,#57308,#57309,#57310,
#57311,#57312,#57313,#57314,#57315,#57316),.UNSPECIFIED.,.F.,.F.,(4,1,1,
1,1,1,1,1,4),(214.738345655019,214.938650926659,215.938365582132,216.938080237605,
217.937794893078,218.93750954855,219.937224204023,220.936938859496,221.021530962198),
 .UNSPECIFIED.);
#345=B_SPLINE_CURVE_WITH_KNOTS('',3,(#57318,#57319,#57320,#57321,#57322,
#57323,#57324,#57325,#57326,#57327),.UNSPECIFIED.,.F.,.F.,(4,1,1,1,1,1,
1,4),(221.021530962198,221.936653514969,222.936368170442,223.936082825914,
224.935797481387,225.93551213686,226.935226792333,227.304716269378),
 .UNSPECIFIED.);
#346=B_SPLINE_CURVE_WITH_KNOTS('',3,(#57329,#57330,#57331,#57332,#57333,
#57334,#57335,#57336,#57337,#57338),.UNSPECIFIED.,.F.,.F.,(4,1,1,1,1,1,
1,4),(227.304716269378,227.934941447806,228.934656103279,229.934370758752,
230.934085414224,231.933800069697,232.93351472517,233.587901576558),
 .UNSPECIFIED.);
#347=B_SPLINE_CURVE_WITH_KNOTS('',3,(#57340,#57341,#57342,#57343,#57344,
#57345,#57346,#57347,#57348,#57349,#57350,#57351,#57352,#57353,#57354,#57355,
#57356,#57357,#57358,#57359,#57360,#57361,#57362,#57363,#57364,#57365,#57366,
#57367,#57368,#57369,#57370,#57371,#57372,#57373,#57374,#57375,#57376,#57377,
#57378,#57379,#57380,#57381,#57382,#57383,#57384,#57385,#57386,#57387,#57388,
#57389,#57390,#57391,#57392,#57393,#57394,#57395,#57396,#57397,#57398,#57399,
#57400,#57401,#57402,#57403,#57404,#57405,#57406,#57407,#57408,#57409,#57410,
#57411,#57412,#57413,#57414,#57415,#57416,#57417,#57418,#57419,#57420,#57421,
#57422,#57423,#57424,#57425,#57426,#57427,#57428,#57429,#57430,#57431,#57432,
#57433,#57434,#57435,#57436,#57437,#57438,#57439,#57440,#57441,#57442,#57443,
#57444,#57445,#57446,#57447,#57448,#57449,#57450,#57451,#57452,#57453,#57454,
#57455,#57456,#57457,#57458,#57459,#57460,#57461,#57462,#57463,#57464,#57465,
#57466,#57467,#57468,#57469,#57470,#57471,#57472,#57473,#57474,#57475,#57476,
#57477,#57478,#57479,#57480,#57481,#57482,#57483,#57484,#57485,#57486,#57487,
#57488,#57489,#57490,#57491,#57492,#57493,#57494,#57495,#57496,#57497,#57498,
#57499,#57500,#57501,#57502,#57503,#57504,#57505,#57506,#57507,#57508,#57509,
#57510,#57511,#57512,#57513,#57514,#57515,#57516,#57517,#57518,#57519,#57520,
#57521,#57522,#57523,#57524,#57525,#57526,#57527,#57528,#57529,#57530,#57531,
#57532,#57533,#57534,#57535,#57536,#57537,#57538,#57539,#57540,#57541,#57542,
#57543,#57544,#57545,#57546,#57547,#57548,#57549,#57550,#57551,#57552,#57553,
#57554,#57555,#57556,#57557,#57558,#57559,#57560,#57561,#57562,#57563,#57564,
#57565),.UNSPECIFIED.,.F.,.F.,(4,3,3,3,3,3,3,3,3,3,3,3,3,3,3,3,3,3,3,3,
3,3,3,3,3,3,3,3,3,3,3,3,3,3,3,3,3,3,3,3,3,3,3,3,3,3,3,3,3,3,3,3,3,3,3,3,
3,3,3,3,3,3,3,3,3,3,3,3,3,3,3,3,3,3,3,4),(233.587901819524,233.689634913313,
233.791928180161,233.89488361089,233.933229380643,234.021781532723,234.110218928246,
234.198565371445,234.290362704529,234.378606826435,234.466837512371,234.555076131095,
234.643344051944,234.731712352586,234.820140163747,234.90869829985,234.932944036116,
235.021496188196,235.109933583719,235.198280026917,235.290077360001,235.378321481908,
235.466552167844,235.554790786568,235.643058707416,235.731427008058,235.819854819219,
235.908412955322,235.932658691589,236.021210843668,236.109648239191,236.197994682389,
236.289792015473,236.378036137379,236.466266823315,236.554505442038,236.642773362886,
236.731141663528,236.819569474688,236.908127610791,236.932373347061,237.020925499141,
237.109362894664,237.197709337862,237.289506670946,237.377750792852,237.465981478788,
237.554220097512,237.64248801836,237.730856319001,237.819284130162,237.907842266265,
237.932088002534,238.020640154614,238.109077550137,238.197423993335,238.289221326419,
238.377465448326,238.465696134262,238.553934752986,238.642202673834,238.730570974476,
238.818998785637,238.90755692174,238.931802658007,239.019567715922,239.107218672699,
239.194780175945,239.282278390013,239.369743686316,239.457198190576,239.544664015338,
239.632214924191,239.719810741112,239.807540789698,239.871086883737),
 .UNSPECIFIED.);
#348=B_SPLINE_CURVE_WITH_KNOTS('',3,(#57567,#57568,#57569,#57570,#57571,
#57572,#57573,#57574,#57575,#57576,#57577,#57578),.UNSPECIFIED.,.F.,.F.,
(4,2,1,1,1,1,1,1,4),(239.871086883737,239.93151731348,240.931231968953,
241.930946624426,242.930661279898,243.930375935371,244.930090590844,245.929805246317,
246.154272190917),.UNSPECIFIED.);
#349=B_SPLINE_CURVE_WITH_KNOTS('',3,(#57580,#57581,#57582,#57583,#57584,
#57585,#57586,#57587,#57588,#57589,#57590,#57591,#57592,#57593,#57594,#57595,
#57596,#57597,#57598,#57599,#57600,#57601,#57602,#57603,#57604,#57605,#57606,
#57607,#57608,#57609,#57610,#57611,#57612,#57613,#57614,#57615,#57616,#57617,
#57618,#57619,#57620,#57621,#57622,#57623,#57624,#57625,#57626,#57627,#57628,
#57629,#57630,#57631,#57632,#57633,#57634,#57635,#57636,#57637,#57638,#57639,
#57640,#57641,#57642,#57643,#57644,#57645,#57646,#57647,#57648,#57649,#57650,
#57651,#57652,#57653,#57654,#57655,#57656,#57657,#57658,#57659,#57660,#57661,
#57662,#57663,#57664,#57665,#57666,#57667,#57668,#57669,#57670,#57671,#57672,
#57673,#57674,#57675,#57676,#57677,#57678,#57679,#57680,#57681,#57682,#57683,
#57684,#57685,#57686,#57687,#57688,#57689,#57690,#57691,#57692,#57693,#57694,
#57695,#57696,#57697,#57698,#57699,#57700,#57701,#57702,#57703,#57704,#57705,
#57706,#57707,#57708,#57709,#57710,#57711,#57712,#57713,#57714,#57715,#57716,
#57717,#57718,#57719,#57720,#57721,#57722,#57723,#57724,#57725,#57726,#57727,
#57728,#57729,#57730,#57731,#57732,#57733,#57734,#57735,#57736,#57737,#57738,
#57739,#57740,#57741,#57742,#57743,#57744,#57745,#57746,#57747,#57748,#57749,
#57750,#57751,#57752,#57753,#57754,#57755,#57756,#57757,#57758,#57759,#57760,
#57761,#57762,#57763,#57764,#57765,#57766,#57767,#57768,#57769,#57770,#57771,
#57772,#57773,#57774,#57775,#57776,#57777,#57778,#57779,#57780,#57781,#57782,
#57783,#57784,#57785,#57786,#57787,#57788,#57789,#57790,#57791,#57792,#57793,
#57794,#57795,#57796,#57797,#57798,#57799,#57800,#57801,#57802,#57803,#57804,
#57805),.UNSPECIFIED.,.F.,.F.,(4,3,3,3,3,3,3,3,3,3,3,3,3,3,3,3,3,3,3,3,
3,3,3,3,3,3,3,3,3,3,3,3,3,3,3,3,3,3,3,3,3,3,3,3,3,3,3,3,3,3,3,3,3,3,3,3,
3,3,3,3,3,3,3,3,3,3,3,3,3,3,3,3,3,3,3,4),(246.154272190917,246.241451698402,
246.328564152085,246.415641150959,246.502705121084,246.58977847341,246.676938547938,
246.764142193271,246.851488540128,246.92951990179,247.01807205387,247.106509449393,
247.194855892591,247.286653225675,247.374897347581,247.463128033518,247.551366652242,
247.63963457309,247.728002873732,247.816430684893,247.904988820996,247.929234557263,
248.017786709342,248.106224104865,248.194570548063,248.286367881147,248.374612003053,
248.462842688989,248.551081307713,248.639349228561,248.727717529202,248.816145340363,
248.904703476466,248.928949212735,249.017501364815,249.105938760338,249.194285203536,
249.28608253662,249.374326658526,249.462557344462,249.550795963186,249.639063884034,
249.727432184675,249.815859995837,249.904418131939,249.928663868208,250.017216020288,
250.105653415811,250.193999859009,250.285797192093,250.374041313999,250.462271999935,
250.550510618659,250.638778539508,250.727146840149,250.81557465131,250.904132787413,
250.928378523681,251.016930675761,251.105368071284,251.193714514482,251.285511847566,
251.373755969472,251.461986655409,251.550225274133,251.63849319498,251.726861495621,
251.815289306782,251.903847442885,251.928093179154,252.020823214331,252.113389862077,
252.205749459193,252.297985132798,252.390068284817,252.437457498096),
 .UNSPECIFIED.);
#350=B_SPLINE_CURVE_WITH_KNOTS('',3,(#57807,#57808,#57809,#57810,#57811,
#57812,#57813,#57814,#57815,#57816,#57817,#57818,#57819,#57820,#57821,#57822,
#57823,#57824,#57825,#57826,#57827,#57828,#57829,#57830,#57831,#57832,#57833,
#57834,#57835,#57836,#57837,#57838,#57839,#57840,#57841,#57842,#57843,#57844,
#57845,#57846,#57847,#57848,#57849,#57850,#57851,#57852,#57853,#57854,#57855,
#57856,#57857,#57858,#57859,#57860,#57861,#57862,#57863,#57864,#57865,#57866,
#57867,#57868,#57869,#57870,#57871,#57872,#57873,#57874,#57875,#57876,#57877,
#57878,#57879,#57880,#57881,#57882,#57883,#57884,#57885,#57886,#57887,#57888,
#57889,#57890,#57891,#57892,#57893,#57894,#57895,#57896,#57897,#57898,#57899,
#57900,#57901,#57902,#57903,#57904,#57905,#57906,#57907,#57908,#57909,#57910,
#57911,#57912,#57913,#57914,#57915,#57916,#57917,#57918,#57919,#57920,#57921,
#57922,#57923,#57924,#57925,#57926,#57927,#57928,#57929,#57930,#57931,#57932,
#57933,#57934,#57935,#57936,#57937,#57938,#57939,#57940,#57941,#57942,#57943,
#57944,#57945,#57946,#57947,#57948,#57949,#57950,#57951,#57952,#57953,#57954,
#57955,#57956,#57957,#57958,#57959,#57960,#57961,#57962,#57963,#57964,#57965,
#57966,#57967,#57968,#57969,#57970,#57971,#57972,#57973,#57974,#57975,#57976,
#57977,#57978,#57979,#57980,#57981,#57982,#57983,#57984,#57985,#57986,#57987,
#57988,#57989,#57990,#57991,#57992,#57993,#57994,#57995,#57996,#57997,#57998,
#57999,#58000,#58001,#58002,#58003,#58004,#58005,#58006,#58007,#58008,#58009,
#58010,#58011,#58012,#58013,#58014,#58015,#58016,#58017,#58018,#58019,#58020,
#58021,#58022,#58023,#58024,#58025,#58026,#58027,#58028,#58029,#58030,#58031,
#58032),.UNSPECIFIED.,.F.,.F.,(4,3,3,3,3,3,3,3,3,3,3,3,3,3,3,3,3,3,3,3,
3,3,3,3,3,3,3,3,3,3,3,3,3,3,3,3,3,3,3,3,3,3,3,3,3,3,3,3,3,3,3,3,3,3,3,3,
3,3,3,3,3,3,3,3,3,3,3,3,3,3,3,3,3,3,3,4),(252.437457498304,252.530258428474,
252.623203058074,252.716386016105,252.809701689193,252.903229080169,252.927807834627,
253.016359986706,253.104797382229,253.193143825426,253.28494115851,253.373185280416,
253.461415966351,253.549654585075,253.637922505923,253.726290806563,253.814718617724,
253.903276753826,253.927522490099,254.016074642179,254.104512037702,254.1928584809,
254.284655813984,254.37289993589,254.461130621826,254.54936924055,254.637637161398,
254.72600546204,254.814433273201,254.902991409303,254.927237145572,255.015789297652,
255.104226693175,255.192573136374,255.284370469458,255.372614591364,255.4608452773,
255.549083896024,255.637351816873,255.725720117514,255.814147928676,255.902706064779,
255.926951801045,256.015503953125,256.103941348648,256.192287791846,256.28408512493,
256.372329246836,256.460559932772,256.548798551496,256.637066472344,256.725434772985,
256.813862584146,256.902420720249,256.926666456518,257.015218608598,257.103656004121,
257.192002447319,257.283799780403,257.372043902309,257.460274588245,257.548513206969,
257.636781127818,257.725149428459,257.81357723962,257.902135375723,257.926381111991,
258.013674483031,258.102045523312,258.189121133445,258.276140912924,258.363127375888,
258.452506233235,258.539523844794,258.630083325035,258.720642805276),
 .UNSPECIFIED.);
#351=B_SPLINE_CURVE_WITH_KNOTS('',3,(#58034,#58035,#58036,#58037,#58038,
#58039,#58040,#58041,#58042,#58043,#58044),.UNSPECIFIED.,.F.,.F.,(4,1,1,
1,1,1,1,1,4),(258.720642805276,258.926095767464,259.925810422936,260.925525078409,
261.925239733882,262.924954389355,263.924669044828,264.924383700301,265.003828112455),
 .UNSPECIFIED.);
#352=B_SPLINE_CURVE_WITH_KNOTS('',3,(#58046,#58047,#58048,#58049,#58050,
#58051,#58052,#58053,#58054,#58055),.UNSPECIFIED.,.F.,.F.,(4,1,1,1,1,1,
1,4),(265.003828112455,265.924098355773,266.923813011246,267.923527666719,
268.923242322192,269.922956977665,270.922671633138,271.287013419635),
 .UNSPECIFIED.);
#353=B_SPLINE_CURVE_WITH_KNOTS('',3,(#58057,#58058,#58059,#58060,#58061,
#58062,#58063,#58064,#58065,#58066),.UNSPECIFIED.,.F.,.F.,(4,1,1,1,1,1,
1,4),(271.287013419635,271.92238628861,272.922100944083,273.921815599556,
274.921530255029,275.921244910502,276.920959565975,277.570198726814),
 .UNSPECIFIED.);
#354=B_SPLINE_CURVE_WITH_KNOTS('',3,(#58068,#58069,#58070,#58071,#58072,
#58073,#58074,#58075,#58076,#58077,#58078,#58079,#58080,#58081,#58082,#58083,
#58084,#58085,#58086,#58087,#58088,#58089,#58090,#58091,#58092,#58093,#58094,
#58095,#58096,#58097,#58098,#58099,#58100,#58101,#58102,#58103,#58104,#58105,
#58106,#58107,#58108,#58109,#58110,#58111,#58112,#58113,#58114,#58115,#58116,
#58117,#58118,#58119,#58120,#58121,#58122,#58123,#58124,#58125,#58126,#58127,
#58128,#58129,#58130,#58131,#58132,#58133,#58134,#58135,#58136,#58137,#58138,
#58139,#58140,#58141,#58142,#58143,#58144,#58145,#58146,#58147,#58148,#58149,
#58150,#58151,#58152,#58153,#58154,#58155,#58156,#58157,#58158,#58159,#58160,
#58161,#58162,#58163,#58164,#58165,#58166,#58167,#58168,#58169,#58170,#58171,
#58172,#58173,#58174,#58175,#58176,#58177,#58178,#58179,#58180,#58181,#58182,
#58183,#58184,#58185,#58186,#58187,#58188,#58189,#58190,#58191,#58192,#58193,
#58194,#58195,#58196,#58197,#58198,#58199,#58200,#58201,#58202,#58203,#58204,
#58205,#58206,#58207,#58208,#58209,#58210,#58211,#58212,#58213,#58214,#58215,
#58216,#58217,#58218,#58219,#58220,#58221,#58222,#58223,#58224,#58225,#58226,
#58227,#58228,#58229,#58230,#58231,#58232,#58233,#58234,#58235,#58236,#58237,
#58238,#58239,#58240,#58241,#58242,#58243,#58244,#58245,#58246,#58247,#58248,
#58249,#58250,#58251,#58252,#58253,#58254,#58255,#58256,#58257,#58258,#58259,
#58260,#58261,#58262,#58263,#58264,#58265,#58266,#58267,#58268,#58269,#58270,
#58271,#58272,#58273,#58274,#58275,#58276,#58277,#58278,#58279,#58280,#58281,
#58282,#58283,#58284,#58285,#58286,#58287,#58288,#58289,#58290,#58291,#58292,
#58293),.UNSPECIFIED.,.F.,.F.,(4,3,3,3,3,3,3,3,3,3,3,3,3,3,3,3,3,3,3,3,
3,3,3,3,3,3,3,3,3,3,3,3,3,3,3,3,3,3,3,3,3,3,3,3,3,3,3,3,3,3,3,3,3,3,3,3,
3,3,3,3,3,3,3,3,3,3,3,3,3,3,3,3,3,3,3,4),(277.570198972254,277.671486989444,
277.773303087998,277.875759025028,277.920674221447,278.009226373527,278.09766376905,
278.186010212248,278.277807545332,278.366051667238,278.454282353174,278.542520971898,
278.630788892746,278.719157193388,278.807585004549,278.896143140652,278.92038887692,
279.008941029,279.097378424523,279.185724867721,279.277522200805,279.365766322711,
279.453997008647,279.542235627371,279.630503548219,279.718871848861,279.807299660022,
279.895857796125,279.920103532393,280.008655684473,280.097093079996,280.185439523194,
280.277236856278,280.365480978184,280.45371166412,280.541950282844,280.630218203692,
280.718586504333,280.807014315494,280.895572451597,280.919818187866,281.008370339946,
281.096807735469,281.185154178667,281.276951511751,281.365195633657,281.453426319593,
281.541664938317,281.629932859166,281.718301159807,281.806728970968,281.895287107071,
281.919532843339,282.008084995419,282.096522390942,282.18486883414,282.276666167224,
282.36491028913,282.453140975067,282.54137959379,282.629647514639,282.71801581528,
282.806443626441,282.895001762544,282.919247498812,283.006962242243,283.094562935591,
283.182074273176,283.269522395889,283.356937750207,283.444342502134,283.531758804621,
283.619259545184,283.706805501756,283.794483384449,283.853384033994),
 .UNSPECIFIED.);
#355=B_SPLINE_CURVE_WITH_KNOTS('',3,(#58295,#58296,#58297,#58298,#58299,
#58300,#58301,#58302,#58303,#58304,#58305,#58306),.UNSPECIFIED.,.F.,.F.,
(4,2,1,1,1,1,1,1,4),(283.853384033994,283.918962154284,284.918676809757,
285.91839146523,286.918106120703,287.917820776176,288.917535431649,289.917250087121,
290.136569341174),.UNSPECIFIED.);
#356=B_SPLINE_CURVE_WITH_KNOTS('',3,(#58308,#58309,#58310,#58311,#58312,
#58313,#58314,#58315,#58316,#58317,#58318,#58319,#58320,#58321,#58322,#58323,
#58324,#58325,#58326,#58327,#58328,#58329,#58330,#58331,#58332,#58333,#58334,
#58335,#58336,#58337,#58338,#58339,#58340,#58341,#58342,#58343,#58344,#58345,
#58346,#58347,#58348,#58349,#58350,#58351,#58352,#58353,#58354,#58355,#58356,
#58357,#58358,#58359,#58360,#58361,#58362,#58363,#58364,#58365,#58366,#58367,
#58368,#58369,#58370,#58371,#58372,#58373,#58374,#58375,#58376,#58377,#58378,
#58379,#58380,#58381,#58382,#58383,#58384,#58385,#58386,#58387,#58388,#58389,
#58390,#58391,#58392,#58393,#58394,#58395,#58396,#58397,#58398,#58399,#58400,
#58401,#58402,#58403,#58404,#58405,#58406,#58407,#58408,#58409,#58410,#58411,
#58412,#58413,#58414,#58415,#58416,#58417,#58418,#58419,#58420,#58421,#58422,
#58423,#58424,#58425,#58426,#58427,#58428,#58429,#58430,#58431,#58432,#58433,
#58434,#58435,#58436,#58437,#58438,#58439,#58440,#58441,#58442,#58443,#58444,
#58445,#58446,#58447,#58448,#58449,#58450,#58451,#58452,#58453,#58454,#58455,
#58456,#58457,#58458,#58459,#58460,#58461,#58462,#58463,#58464,#58465,#58466,
#58467,#58468,#58469,#58470,#58471,#58472,#58473,#58474,#58475,#58476,#58477,
#58478,#58479,#58480,#58481,#58482,#58483,#58484,#58485,#58486,#58487,#58488,
#58489,#58490,#58491,#58492,#58493,#58494,#58495,#58496,#58497,#58498,#58499,
#58500,#58501,#58502,#58503,#58504,#58505,#58506,#58507,#58508,#58509,#58510,
#58511,#58512,#58513,#58514,#58515,#58516,#58517,#58518,#58519,#58520,#58521,
#58522,#58523,#58524,#58525,#58526,#58527,#58528,#58529,#58530,#58531,#58532,
#58533),.UNSPECIFIED.,.F.,.F.,(4,3,3,3,3,3,3,3,3,3,3,3,3,3,3,3,3,3,3,3,
3,3,3,3,3,3,3,3,3,3,3,3,3,3,3,3,3,3,3,3,3,3,3,3,3,3,3,3,3,3,3,3,3,3,3,3,
3,3,3,3,3,3,3,3,3,3,3,3,3,3,3,3,3,3,3,4),(290.136569341174,290.223730192393,
290.310821510838,290.397875760146,290.484915386051,290.571962817726,290.659095926046,
290.746271223774,290.833590646189,290.916964742594,291.005516894674,291.093954290197,
291.182300733395,291.274098066479,291.362342188385,291.450572874322,291.538811493046,
291.627079413894,291.715447714535,291.803875525696,291.892433661799,291.916679398067,
292.005231550147,292.09366894567,292.182015388868,292.273812721952,292.362056843858,
292.450287529794,292.538526148518,292.626794069366,292.715162370007,292.803590181168,
292.892148317271,292.91639405354,293.00494620562,293.093383601143,293.181730044341,
293.273527377425,293.361771499331,293.450002185267,293.538240803991,293.626508724839,
293.714877025481,293.803304836642,293.891862972745,293.916108709013,294.004660861093,
294.093098256616,294.181444699814,294.273242032898,294.361486154804,294.44971684074,
294.537955459464,294.626223380313,294.714591680955,294.803019492116,294.891577628219,
294.915823364486,295.004375516565,295.092812912088,295.181159355286,295.27295668837,
295.361200810276,295.449431496212,295.537670114935,295.625938035784,295.714306336425,
295.802734147586,295.891292283689,295.915538019958,296.008475344092,296.10124593225,
296.193803345762,296.286232444007,296.378502206548,296.419754648353),
 .UNSPECIFIED.);
#357=B_SPLINE_CURVE_WITH_KNOTS('',3,(#58535,#58536,#58537,#58538,#58539,
#58540,#58541,#58542,#58543,#58544,#58545,#58546,#58547,#58548,#58549,#58550,
#58551,#58552,#58553,#58554,#58555,#58556,#58557,#58558,#58559,#58560,#58561,
#58562,#58563,#58564,#58565,#58566,#58567,#58568,#58569,#58570,#58571,#58572,
#58573,#58574,#58575,#58576,#58577,#58578,#58579,#58580,#58581,#58582,#58583,
#58584,#58585,#58586,#58587,#58588,#58589,#58590,#58591,#58592,#58593,#58594,
#58595,#58596,#58597,#58598,#58599,#58600,#58601,#58602,#58603,#58604,#58605,
#58606,#58607,#58608,#58609,#58610,#58611,#58612,#58613,#58614,#58615,#58616,
#58617,#58618,#58619,#58620,#58621,#58622,#58623,#58624,#58625,#58626,#58627,
#58628,#58629,#58630,#58631,#58632,#58633,#58634,#58635,#58636,#58637,#58638,
#58639,#58640,#58641,#58642,#58643,#58644,#58645,#58646,#58647,#58648,#58649,
#58650,#58651,#58652,#58653,#58654,#58655,#58656,#58657,#58658,#58659,#58660,
#58661,#58662,#58663,#58664,#58665,#58666,#58667,#58668,#58669,#58670,#58671,
#58672,#58673,#58674,#58675,#58676,#58677,#58678,#58679,#58680,#58681,#58682,
#58683,#58684,#58685,#58686,#58687,#58688,#58689,#58690,#58691,#58692,#58693,
#58694,#58695,#58696,#58697,#58698,#58699,#58700,#58701,#58702,#58703,#58704,
#58705,#58706,#58707,#58708,#58709,#58710,#58711,#58712,#58713,#58714,#58715,
#58716,#58717,#58718,#58719,#58720,#58721,#58722,#58723,#58724,#58725,#58726,
#58727,#58728,#58729,#58730,#58731,#58732,#58733,#58734,#58735,#58736,#58737,
#58738,#58739,#58740,#58741,#58742,#58743,#58744,#58745,#58746,#58747,#58748,
#58749,#58750,#58751,#58752,#58753,#58754,#58755,#58756,#58757,#58758,#58759,
#58760),.UNSPECIFIED.,.F.,.F.,(4,3,3,3,3,3,3,3,3,3,3,3,3,3,3,3,3,3,3,3,
3,3,3,3,3,3,3,3,3,3,3,3,3,3,3,3,3,3,3,3,3,3,3,3,3,3,3,3,3,3,3,3,3,3,3,3,
3,3,3,3,3,3,3,3,3,3,3,3,3,3,3,3,3,3,3,4),(296.419754648543,296.512351451628,
296.605083805464,296.698046710968,296.79113719593,296.884437934939,296.915252675431,
297.003804827511,297.092242223034,297.180588666232,297.272385999316,297.360630121222,
297.448860807159,297.537099425883,297.625367346731,297.713735647373,297.802163458534,
297.890721594637,297.914967330904,298.003519482984,298.091956878507,298.180303321705,
298.272100654789,298.360344776695,298.448575462631,298.536814081355,298.625082002203,
298.713450302845,298.801878114006,298.890436250109,298.914681986377,299.003234138457,
299.09167153398,299.180017977178,299.271815310262,299.360059432168,299.448290118104,
299.536528736828,299.624796657676,299.713164958317,299.801592769478,299.890150905581,
299.91439664185,300.00294879393,300.091386189453,300.179732632651,300.271529965735,
300.359774087641,300.448004773578,300.536243392302,300.62451131315,300.712879613792,
300.801307424953,300.889865561056,300.914111297323,301.002663449402,301.091100844925,
301.179447288123,301.271244621207,301.359488743113,301.447719429049,301.535958047772,
301.624225968621,301.712594269262,301.801022080423,301.889580216525,301.913825952795,
302.001138292507,302.088863500385,302.17595801984,302.262996307226,302.350000864675,
302.43823563739,302.525269190206,302.61410457287,302.702939955533),
 .UNSPECIFIED.);
#358=B_SPLINE_CURVE_WITH_KNOTS('',3,(#58762,#58763,#58764,#58765,#58766,
#58767,#58768,#58769,#58770,#58771,#58772),.UNSPECIFIED.,.F.,.F.,(4,1,1,
1,1,1,1,1,4),(302.702939955533,302.913540608268,303.913255263741,304.912969919214,
305.912684574687,306.91239923016,307.912113885632,308.911828541105,308.986125262712),
 .UNSPECIFIED.);
#359=B_SPLINE_CURVE_WITH_KNOTS('',3,(#58774,#58775,#58776,#58777,#58778,
#58779,#58780,#58781,#58782,#58783),.UNSPECIFIED.,.F.,.F.,(4,1,1,1,1,1,
1,4),(308.986125262712,309.911543196578,310.911257852051,311.910972507524,
312.910687162997,313.910401818469,314.910116473942,315.269310569892),
 .UNSPECIFIED.);
#360=B_SPLINE_CURVE_WITH_KNOTS('',3,(#58785,#58786,#58787,#58788,#58789,
#58790,#58791,#58792,#58793,#58794),.UNSPECIFIED.,.F.,.F.,(4,1,1,1,1,1,
1,4),(315.269310569892,315.909831129415,316.909545784888,317.909260440361,
318.908975095834,319.908689751306,320.908404406779,321.552495877071),
 .UNSPECIFIED.);
#361=B_SPLINE_CURVE_WITH_KNOTS('',3,(#58796,#58797,#58798,#58799,#58800,
#58801,#58802,#58803,#58804,#58805,#58806,#58807,#58808,#58809,#58810,#58811,
#58812,#58813,#58814,#58815,#58816,#58817,#58818,#58819,#58820,#58821,#58822,
#58823,#58824,#58825,#58826,#58827,#58828,#58829,#58830,#58831,#58832,#58833,
#58834,#58835,#58836,#58837,#58838,#58839,#58840,#58841,#58842,#58843,#58844,
#58845,#58846,#58847,#58848,#58849,#58850,#58851,#58852,#58853,#58854,#58855,
#58856,#58857,#58858,#58859,#58860,#58861,#58862,#58863,#58864,#58865,#58866,
#58867,#58868,#58869,#58870,#58871,#58872,#58873,#58874,#58875,#58876,#58877,
#58878,#58879,#58880,#58881,#58882,#58883,#58884,#58885,#58886,#58887,#58888,
#58889,#58890,#58891,#58892,#58893,#58894,#58895,#58896,#58897,#58898,#58899,
#58900,#58901,#58902,#58903,#58904,#58905,#58906,#58907,#58908,#58909,#58910,
#58911,#58912,#58913,#58914,#58915,#58916,#58917,#58918,#58919,#58920,#58921,
#58922,#58923,#58924,#58925,#58926,#58927,#58928,#58929,#58930,#58931,#58932,
#58933,#58934,#58935,#58936,#58937,#58938,#58939,#58940,#58941,#58942,#58943,
#58944,#58945,#58946,#58947,#58948,#58949,#58950,#58951,#58952,#58953,#58954,
#58955,#58956,#58957,#58958,#58959,#58960,#58961,#58962,#58963,#58964,#58965,
#58966,#58967,#58968,#58969,#58970,#58971,#58972,#58973,#58974,#58975,#58976,
#58977,#58978,#58979,#58980,#58981,#58982,#58983,#58984,#58985,#58986,#58987,
#58988,#58989,#58990,#58991,#58992,#58993,#58994,#58995,#58996,#58997,#58998,
#58999,#59000,#59001,#59002,#59003,#59004,#59005,#59006,#59007,#59008,#59009,
#59010,#59011,#59012,#59013,#59014,#59015,#59016,#59017,#59018,#59019,#59020,
#59021),.UNSPECIFIED.,.F.,.F.,(4,3,3,3,3,3,3,3,3,3,3,3,3,3,3,3,3,3,3,3,
3,3,3,3,3,3,3,3,3,3,3,3,3,3,3,3,3,3,3,3,3,3,3,3,3,3,3,3,3,3,3,3,3,3,3,3,
3,3,3,3,3,3,3,3,3,3,3,3,3,3,3,3,3,3,3,4),(321.55249612466,321.653352335466,
321.754706689964,321.856679710689,321.908119062252,321.996671214331,322.085108609854,
322.173455053052,322.265252386136,322.353496508042,322.441727193978,322.529965812702,
322.61823373355,322.706602034191,322.795029845352,322.883587981454,322.907833717725,
322.996385869805,323.084823265328,323.173169708526,323.26496704161,323.353211163516,
323.441441849452,323.529680468176,323.617948389025,323.706316689666,323.794744500827,
323.88330263693,323.907548373198,323.996100525278,324.084537920801,324.172884363999,
324.264681697083,324.35292581899,324.441156504926,324.52939512365,324.617663044498,
324.70603134514,324.794459156301,324.883017292404,324.907263028671,324.99581518075,
325.084252576273,325.172599019471,325.264396352555,325.352640474461,325.440871160397,
325.529109779121,325.617377699969,325.70574600061,325.794173811771,325.882731947873,
325.906977684143,325.995529836223,326.083967231746,326.172313674944,326.264111008028,
326.352355129934,326.44058581587,326.528824434594,326.617092355442,326.705460656083,
326.793888467244,326.882446603347,326.906692339616,326.994359313025,327.081912284458,
327.169375991889,327.256776540059,327.344144456776,327.431501945575,327.518871197051,
327.606324201979,327.693822711221,327.781450815237,327.835681184251),
 .UNSPECIFIED.);
#362=B_SPLINE_CURVE_WITH_KNOTS('',3,(#59023,#59024,#59025,#59026,#59027,
#59028,#59029,#59030,#59031,#59032,#59033),.UNSPECIFIED.,.F.,.F.,(4,1,1,
1,1,1,1,1,4),(327.835681184251,327.906406995089,328.906121650562,329.905836306035,
330.905550961508,331.90526561698,332.904980272453,333.904694927926,334.118866491431),
 .UNSPECIFIED.);
#363=B_SPLINE_CURVE_WITH_KNOTS('',3,(#59035,#59036,#59037,#59038,#59039,
#59040,#59041,#59042,#59043,#59044),.UNSPECIFIED.,.F.,.F.,(4,1,1,1,1,1,
1,4),(334.118866491431,334.904409583399,335.904124238872,336.903838894345,
337.903553549817,338.90326820529,339.902982860763,340.40205179861),
 .UNSPECIFIED.);
#364=B_SPLINE_CURVE_WITH_KNOTS('',3,(#59046,#59047,#59048,#59049,#59050,
#59051,#59052,#59053,#59054,#59055),.UNSPECIFIED.,.F.,.F.,(4,1,1,1,1,1,
1,4),(340.40205179861,340.902697516236,341.902412171709,342.902126827182,
343.901841482655,344.901556138127,345.9012707936,346.68523710579),
 .UNSPECIFIED.);
#365=B_SPLINE_CURVE_WITH_KNOTS('',3,(#59057,#59058,#59059,#59060,#59061,
#59062,#59063,#59064,#59065,#59066,#59067),.UNSPECIFIED.,.F.,.F.,(4,1,1,
1,1,1,1,1,4),(346.68523710579,346.900985449073,347.900700104546,348.900414760019,
349.900129415491,350.899844070964,351.899558726437,352.89927338191,352.968422412969),
 .UNSPECIFIED.);
#366=B_SPLINE_CURVE_WITH_KNOTS('',3,(#59069,#59070,#59071,#59072,#59073,
#59074,#59075,#59076,#59077,#59078,#59079,#59080,#59081,#59082,#59083,#59084,
#59085,#59086,#59087,#59088,#59089,#59090,#59091,#59092,#59093,#59094,#59095,
#59096,#59097,#59098,#59099,#59100,#59101,#59102,#59103,#59104,#59105,#59106,
#59107,#59108,#59109,#59110,#59111,#59112,#59113,#59114,#59115,#59116,#59117,
#59118,#59119,#59120,#59121,#59122,#59123,#59124,#59125,#59126,#59127,#59128,
#59129,#59130,#59131,#59132,#59133,#59134,#59135,#59136,#59137,#59138,#59139,
#59140,#59141,#59142,#59143,#59144,#59145,#59146,#59147,#59148,#59149,#59150,
#59151,#59152,#59153,#59154,#59155,#59156,#59157,#59158,#59159,#59160,#59161,
#59162,#59163,#59164,#59165,#59166,#59167,#59168,#59169,#59170,#59171,#59172,
#59173,#59174,#59175,#59176,#59177,#59178,#59179,#59180,#59181,#59182,#59183,
#59184,#59185,#59186,#59187,#59188,#59189,#59190,#59191,#59192,#59193,#59194,
#59195,#59196,#59197,#59198,#59199,#59200,#59201,#59202,#59203,#59204,#59205,
#59206,#59207,#59208,#59209,#59210,#59211,#59212,#59213,#59214,#59215,#59216,
#59217,#59218,#59219,#59220,#59221,#59222,#59223,#59224,#59225,#59226,#59227,
#59228,#59229,#59230,#59231,#59232,#59233,#59234,#59235,#59236,#59237,#59238,
#59239,#59240,#59241,#59242,#59243,#59244,#59245,#59246,#59247,#59248,#59249,
#59250,#59251,#59252,#59253,#59254,#59255,#59256,#59257,#59258,#59259,#59260,
#59261,#59262,#59263,#59264,#59265,#59266,#59267,#59268,#59269,#59270,#59271,
#59272,#59273,#59274,#59275,#59276,#59277,#59278,#59279,#59280,#59281,#59282,
#59283,#59284,#59285,#59286,#59287,#59288,#59289,#59290,#59291,#59292,#59293,
#59294),.UNSPECIFIED.,.F.,.F.,(4,3,3,3,3,3,3,3,3,3,3,3,3,3,3,3,3,3,3,3,
3,3,3,3,3,3,3,3,3,3,3,3,3,3,3,3,3,3,3,3,3,3,3,3,3,3,3,3,3,3,3,3,3,3,3,3,
3,3,3,3,3,3,3,3,3,3,3,3,3,3,3,3,3,3,3,4),(352.968422412969,353.056076536257,
353.143622164665,353.231083997544,353.318490920333,353.40587026875,353.493244230893,
353.580634986258,353.668117469944,353.755649754035,353.843319148401,353.898988037383,
353.987540189463,354.075977584986,354.164324028184,354.256121361268,354.344365483174,
354.43259616911,354.520834787834,354.609102708682,354.697471009324,354.785898820485,
354.874456956588,354.898702692856,354.987254844935,355.075692240458,355.164038683656,
355.25583601674,355.344080138646,355.432310824582,355.520549443305,355.608817364153,
355.697185664794,355.785613475955,355.874171612058,355.898417348328,355.986969500408,
356.075406895931,356.163753339129,356.255550672213,356.343794794119,356.432025480055,
356.520264098779,356.608532019628,356.696900320269,356.78532813143,356.873886267533,
356.898132003801,356.986684155881,357.075121551404,357.163467994602,357.255265327686,
357.343509449593,357.431740135529,357.519978754253,357.608246675101,357.696614975743,
357.785042786904,357.873600923007,357.897846659274,357.986398811353,358.074836206877,
358.163182650075,358.254979983159,358.343224105065,358.431454791001,358.519693409725,
358.607961330574,358.696329631215,358.784757442376,358.873315578479,358.897561314747,
358.999617211864,359.101261411547,359.202154318896,359.25160747295),
 .UNSPECIFIED.);
#367=B_SPLINE_CURVE_WITH_KNOTS('',3,(#59296,#59297,#59298,#59299,#59300,
#59301,#59302,#59303,#59304,#59305),.UNSPECIFIED.,.F.,.F.,(4,1,1,1,1,1,
1,4),(359.251607720149,359.89727597022,360.896990625693,361.896705281165,
362.896419936638,363.896134592111,364.895849247584,365.534793027328),
 .UNSPECIFIED.);
#368=B_SPLINE_CURVE_WITH_KNOTS('',3,(#59307,#59308,#59309,#59310,#59311,
#59312,#59313,#59314,#59315,#59316),.UNSPECIFIED.,.F.,.F.,(4,1,1,1,1,1,
1,4),(365.534793027328,365.895563903057,366.89527855853,367.894993214002,
368.894707869475,369.894422524948,370.894137180421,371.817978334508),
 .UNSPECIFIED.);
#369=B_SPLINE_CURVE_WITH_KNOTS('',3,(#59318,#59319,#59320,#59321,#59322,
#59323,#59324,#59325,#59326,#59327,#59328),.UNSPECIFIED.,.F.,.F.,(4,1,1,
1,1,1,1,1,4),(371.817978334508,371.893851835894,372.893566491367,373.893281146839,
374.892995802312,375.892710457785,376.892425113258,377.892139768731,378.101163641688),
 .UNSPECIFIED.);
#370=B_SPLINE_CURVE_WITH_KNOTS('',3,(#59330,#59331,#59332,#59333,#59334,
#59335,#59336,#59337,#59338,#59339,#59340,#59341,#59342,#59343,#59344,#59345,
#59346,#59347,#59348,#59349,#59350,#59351,#59352,#59353,#59354,#59355,#59356,
#59357,#59358,#59359,#59360,#59361,#59362,#59363,#59364,#59365,#59366,#59367,
#59368,#59369,#59370,#59371,#59372,#59373,#59374,#59375,#59376,#59377,#59378,
#59379,#59380,#59381,#59382,#59383,#59384,#59385,#59386,#59387,#59388,#59389,
#59390,#59391,#59392,#59393,#59394,#59395,#59396,#59397,#59398,#59399,#59400,
#59401,#59402,#59403,#59404,#59405,#59406,#59407,#59408,#59409,#59410,#59411,
#59412,#59413,#59414,#59415,#59416,#59417,#59418,#59419,#59420,#59421,#59422,
#59423,#59424,#59425,#59426,#59427,#59428,#59429,#59430,#59431,#59432,#59433,
#59434,#59435,#59436,#59437,#59438,#59439,#59440,#59441,#59442,#59443,#59444,
#59445,#59446,#59447,#59448,#59449,#59450,#59451,#59452,#59453,#59454,#59455,
#59456,#59457,#59458,#59459,#59460,#59461,#59462,#59463,#59464,#59465,#59466,
#59467,#59468,#59469,#59470,#59471,#59472,#59473,#59474,#59475,#59476,#59477,
#59478,#59479,#59480,#59481,#59482,#59483,#59484,#59485,#59486,#59487,#59488,
#59489,#59490,#59491,#59492,#59493,#59494,#59495,#59496,#59497,#59498,#59499,
#59500,#59501,#59502,#59503,#59504,#59505,#59506,#59507,#59508,#59509,#59510,
#59511,#59512,#59513,#59514,#59515,#59516,#59517,#59518,#59519,#59520,#59521,
#59522,#59523,#59524,#59525,#59526,#59527,#59528,#59529,#59530,#59531,#59532,
#59533,#59534,#59535,#59536,#59537,#59538,#59539,#59540,#59541,#59542,#59543,
#59544,#59545,#59546,#59547,#59548,#59549,#59550,#59551,#59552,#59553,#59554,
#59555),.UNSPECIFIED.,.F.,.F.,(4,3,3,3,3,3,3,3,3,3,3,3,3,3,3,3,3,3,3,3,
3,3,3,3,3,3,3,3,3,3,3,3,3,3,3,3,3,3,3,3,3,3,3,3,3,3,3,3,3,3,3,3,3,3,3,3,
3,3,3,3,3,3,3,3,3,3,3,3,3,3,3,3,3,3,3,4),(378.101163641688,378.188294434811,
378.276239433485,378.363255340551,378.45025374502,378.53725710691,378.625906436233,
378.71303415997,378.802444292087,378.891854424203,378.980406576283,379.068843971806,
379.157190415004,379.248987748088,379.337231869994,379.425462555931,379.513701174655,
379.601969095503,379.690337396145,379.778765207306,379.867323343409,379.891569079676,
379.980121231756,380.068558627279,380.156905070477,380.248702403561,380.336946525467,
380.425177211403,380.513415830127,380.601683750975,380.690052051617,380.778479862778,
380.867037998881,380.891283735149,380.979835887229,381.068273282752,381.15661972595,
381.248417059034,381.33666118094,381.424891866876,381.5131304856,381.601398406448,
381.68976670709,381.778194518251,381.866752654354,381.890998390622,381.979550542702,
382.067987938225,382.156334381423,382.248131714507,382.336375836413,382.424606522349,
382.512845141073,382.601113061921,382.689481362562,382.777909173723,382.866467309826,
382.890713046095,382.979265198175,383.067702593698,383.156049036896,383.24784636998,
383.336090491886,383.424321177823,383.512559796546,383.600827717395,383.689196018036,
383.777623829197,383.8661819653,383.890427701568,383.983796145665,384.076990602884,
384.169958800033,384.262789039653,384.355445853662,384.384348948737),
 .UNSPECIFIED.);
#371=B_SPLINE_CURVE_WITH_KNOTS('',3,(#59557,#59558,#59559,#59560,#59561,
#59562,#59563,#59564,#59565,#59566,#59567,#59568,#59569,#59570,#59571,#59572,
#59573,#59574,#59575,#59576,#59577,#59578,#59579,#59580,#59581,#59582,#59583,
#59584,#59585,#59586,#59587,#59588,#59589,#59590,#59591,#59592,#59593,#59594,
#59595,#59596,#59597,#59598,#59599,#59600,#59601,#59602,#59603,#59604,#59605,
#59606,#59607,#59608,#59609,#59610,#59611,#59612,#59613,#59614,#59615,#59616,
#59617,#59618,#59619,#59620,#59621,#59622,#59623,#59624,#59625,#59626,#59627,
#59628,#59629,#59630,#59631,#59632,#59633,#59634,#59635,#59636,#59637,#59638,
#59639,#59640,#59641,#59642,#59643,#59644,#59645,#59646,#59647,#59648,#59649,
#59650,#59651,#59652,#59653,#59654,#59655,#59656,#59657,#59658,#59659,#59660,
#59661,#59662,#59663,#59664,#59665,#59666,#59667,#59668,#59669,#59670,#59671,
#59672,#59673,#59674,#59675,#59676,#59677,#59678,#59679,#59680,#59681,#59682,
#59683,#59684,#59685,#59686,#59687,#59688,#59689,#59690,#59691,#59692,#59693,
#59694,#59695,#59696,#59697,#59698,#59699,#59700,#59701,#59702,#59703,#59704,
#59705,#59706,#59707,#59708,#59709,#59710,#59711,#59712,#59713,#59714,#59715,
#59716,#59717,#59718,#59719,#59720,#59721,#59722,#59723,#59724,#59725,#59726,
#59727,#59728,#59729,#59730,#59731,#59732,#59733,#59734,#59735,#59736,#59737,
#59738,#59739,#59740,#59741,#59742,#59743,#59744,#59745,#59746,#59747,#59748,
#59749,#59750,#59751,#59752,#59753,#59754,#59755,#59756,#59757,#59758,#59759,
#59760,#59761,#59762,#59763,#59764,#59765,#59766,#59767,#59768,#59769,#59770,
#59771,#59772,#59773,#59774,#59775,#59776,#59777,#59778,#59779,#59780,#59781,
#59782),.UNSPECIFIED.,.F.,.F.,(4,3,3,3,3,3,3,3,3,3,3,3,3,3,3,3,3,3,3,3,
3,3,3,3,3,3,3,3,3,3,3,3,3,3,3,3,3,3,3,3,3,3,3,3,3,3,3,3,3,3,3,3,3,3,3,3,
3,3,3,3,3,3,3,3,3,3,3,3,3,3,3,3,3,3,3,4),(384.384348948867,384.476552719823,
384.568876792834,384.661416748294,384.754074511718,384.846939805279,384.890142357041,
384.97869450912,385.067131904643,385.15547834784,385.247275680924,385.33551980283,
385.423750488766,385.511989107489,385.600257028336,385.688625328977,385.777053140138,
385.86561127624,385.889857012513,385.978409164593,386.066846560116,386.155193003314,
386.246990336398,386.335234458304,386.42346514424,386.511703762964,386.599971683812,
386.688339984454,386.776767795615,386.865325931717,386.889571667986,386.978123820066,
387.066561215589,387.154907658787,387.246704991871,387.334949113777,387.423179799714,
387.511418418438,387.599686339287,387.688054639928,387.776482451089,387.865040587192,
387.889286323459,387.977838475538,388.066275871061,388.15462231426,388.246419647344,
388.33466376925,388.422894455186,388.511133073909,388.599400994758,388.687769295399,
388.776197106561,388.864755242663,388.889000978932,388.977553131012,389.065990526535,
389.154336969733,389.246134302817,389.334378424723,389.422609110659,389.510847729383,
389.599115650232,389.687483950873,389.775911762034,389.864469898137,389.888715634405,
389.976073385051,390.063291913215,390.150431025801,390.237513252655,390.324561065973,
390.411628077518,390.498701051175,390.585857212418,390.667534256047),
 .UNSPECIFIED.);
#372=B_SPLINE_CURVE_WITH_KNOTS('',3,(#59784,#59785,#59786,#59787,#59788,
#59789,#59790,#59791,#59792,#59793,#59794),.UNSPECIFIED.,.F.,.F.,(4,1,1,
1,1,1,1,1,4),(390.667534256047,390.888430289877,391.88814494535,392.887859600823,
393.887574256296,394.887288911769,395.887003567242,396.886718222715,396.950719563226),
 .UNSPECIFIED.);
#373=B_SPLINE_CURVE_WITH_KNOTS('',3,(#59796,#59797,#59798,#59799,#59800,
#59801,#59802,#59803,#59804,#59805,#59806,#59807,#59808,#59809,#59810,#59811,
#59812,#59813,#59814,#59815,#59816,#59817,#59818,#59819,#59820,#59821,#59822,
#59823,#59824,#59825,#59826,#59827,#59828,#59829,#59830,#59831,#59832,#59833,
#59834,#59835,#59836,#59837,#59838,#59839,#59840,#59841,#59842,#59843,#59844,
#59845,#59846,#59847,#59848,#59849,#59850,#59851,#59852,#59853,#59854,#59855,
#59856,#59857,#59858,#59859,#59860,#59861,#59862,#59863,#59864,#59865,#59866,
#59867,#59868,#59869,#59870,#59871,#59872,#59873,#59874,#59875,#59876,#59877,
#59878,#59879,#59880,#59881,#59882,#59883,#59884,#59885,#59886,#59887,#59888,
#59889,#59890,#59891,#59892,#59893,#59894,#59895,#59896,#59897,#59898,#59899,
#59900,#59901,#59902,#59903,#59904,#59905,#59906,#59907,#59908,#59909,#59910,
#59911,#59912,#59913,#59914,#59915,#59916,#59917,#59918,#59919,#59920,#59921,
#59922,#59923,#59924,#59925,#59926,#59927,#59928,#59929,#59930,#59931,#59932,
#59933,#59934,#59935,#59936,#59937,#59938,#59939,#59940,#59941,#59942,#59943,
#59944,#59945,#59946,#59947,#59948,#59949,#59950,#59951,#59952,#59953,#59954,
#59955,#59956,#59957,#59958,#59959,#59960,#59961,#59962,#59963,#59964,#59965,
#59966,#59967,#59968,#59969,#59970,#59971,#59972,#59973,#59974,#59975,#59976,
#59977,#59978,#59979,#59980,#59981,#59982,#59983,#59984,#59985,#59986,#59987,
#59988,#59989,#59990,#59991,#59992,#59993,#59994,#59995,#59996,#59997,#59998,
#59999,#60000,#60001,#60002,#60003,#60004,#60005,#60006,#60007,#60008,#60009,
#60010,#60011,#60012,#60013,#60014,#60015,#60016,#60017,#60018,#60019,#60020,
#60021),.UNSPECIFIED.,.F.,.F.,(4,3,3,3,3,3,3,3,3,3,3,3,3,3,3,3,3,3,3,3,
3,3,3,3,3,3,3,3,3,3,3,3,3,3,3,3,3,3,3,3,3,3,3,3,3,3,3,3,3,3,3,3,3,3,3,3,
3,3,3,3,3,3,3,3,3,3,3,3,3,3,3,3,3,3,3,4),(396.950719563226,397.038425769189,
397.12602269023,397.213534984691,397.300991215638,397.388419047536,397.475840630628,
397.563278105804,397.650806974123,397.738384760113,397.826101134347,397.886432878187,
397.974985030267,398.06342242579,398.151768868988,398.243566202072,398.331810323978,
398.420041009914,398.508279628638,398.596547549487,398.684915850128,398.773343661289,
398.861901797392,398.88614753366,398.97469968574,399.063137081263,399.151483524461,
399.243280857545,399.331524979451,399.419755665387,399.507994284112,399.59626220496,
399.684630505601,399.773058316762,399.861616452865,399.885862189133,399.974414341213,
400.062851736736,400.151198179933,400.242995513018,400.331239634924,400.41947032086,
400.507708939584,400.595976860432,400.684345161073,400.772772972234,400.861331108337,
400.885576844606,400.974128996686,401.062566392209,401.150912835407,401.242710168491,
401.330954290397,401.419184976333,401.507423595057,401.595691515906,401.684059816547,
401.772487627708,401.861045763811,401.885291500079,401.973843652159,402.062281047682,
402.15062749088,402.242424823964,402.33066894587,402.418899631806,402.50713825053,
402.595406171378,402.683774472019,402.77220228318,402.860760419283,402.885006155552,
402.987537932938,403.089635708668,403.190946113391,403.233904625629),
 .UNSPECIFIED.);
#374=B_SPLINE_CURVE_WITH_KNOTS('',3,(#60023,#60024,#60025,#60026,#60027,
#60028,#60029,#60030,#60031,#60032),.UNSPECIFIED.,.F.,.F.,(4,1,1,1,1,1,
1,4),(403.233904870406,403.884720811024,404.884435466497,405.88415012197,
406.883864777443,407.883579432916,408.883294088388,409.517090177585),
 .UNSPECIFIED.);
#375=B_SPLINE_CURVE_WITH_KNOTS('',3,(#60034,#60035,#60036,#60037,#60038,
#60039,#60040,#60041,#60042,#60043),.UNSPECIFIED.,.F.,.F.,(4,1,1,1,1,1,
1,4),(409.517090177585,409.883008743861,410.882723399334,411.882438054807,
412.88215271028,413.881867365753,414.881582021225,415.800275484765),
 .UNSPECIFIED.);
#376=B_SPLINE_CURVE_WITH_KNOTS('',3,(#60045,#60046,#60047,#60048,#60049,
#60050,#60051,#60052,#60053,#60054,#60055),.UNSPECIFIED.,.F.,.F.,(4,1,1,
1,1,1,1,1,4),(415.800275484765,415.881296676698,416.881011332171,417.880725987644,
418.880440643117,419.88015529859,420.879869954062,421.879584609535,422.083460791944),
 .UNSPECIFIED.);
#377=B_SPLINE_CURVE_WITH_KNOTS('',3,(#60057,#60058,#60059,#60060,#60061,
#60062,#60063,#60064,#60065,#60066,#60067,#60068,#60069,#60070,#60071,#60072,
#60073,#60074,#60075,#60076,#60077,#60078,#60079,#60080,#60081,#60082,#60083,
#60084,#60085,#60086,#60087,#60088,#60089,#60090,#60091,#60092,#60093,#60094,
#60095,#60096,#60097,#60098,#60099,#60100,#60101,#60102,#60103,#60104,#60105,
#60106,#60107,#60108,#60109,#60110,#60111,#60112,#60113,#60114,#60115,#60116,
#60117,#60118,#60119,#60120,#60121,#60122,#60123,#60124,#60125,#60126,#60127,
#60128,#60129,#60130,#60131,#60132,#60133,#60134,#60135,#60136,#60137,#60138,
#60139,#60140,#60141,#60142,#60143,#60144,#60145,#60146,#60147,#60148,#60149,
#60150,#60151,#60152,#60153,#60154,#60155,#60156,#60157,#60158,#60159,#60160,
#60161,#60162,#60163,#60164,#60165,#60166,#60167,#60168,#60169,#60170,#60171,
#60172,#60173,#60174,#60175,#60176,#60177,#60178,#60179,#60180,#60181,#60182,
#60183,#60184,#60185,#60186,#60187,#60188,#60189,#60190,#60191,#60192,#60193,
#60194,#60195,#60196,#60197,#60198,#60199,#60200,#60201,#60202,#60203,#60204,
#60205,#60206,#60207,#60208,#60209,#60210,#60211,#60212,#60213,#60214,#60215,
#60216,#60217,#60218,#60219,#60220,#60221,#60222,#60223,#60224,#60225,#60226,
#60227,#60228,#60229,#60230,#60231,#60232,#60233,#60234,#60235,#60236,#60237,
#60238,#60239,#60240,#60241,#60242,#60243,#60244,#60245,#60246,#60247,#60248,
#60249,#60250,#60251,#60252,#60253,#60254,#60255,#60256,#60257,#60258,#60259,
#60260,#60261,#60262,#60263,#60264,#60265,#60266,#60267,#60268,#60269,#60270,
#60271,#60272,#60273,#60274,#60275,#60276,#60277,#60278,#60279,#60280,#60281,
#60282),.UNSPECIFIED.,.F.,.F.,(4,3,3,3,3,3,3,3,3,3,3,3,3,3,3,3,3,3,3,3,
3,3,3,3,3,3,3,3,3,3,3,3,3,3,3,3,3,3,3,3,3,3,3,3,3,3,3,3,3,3,3,3,3,3,3,3,
3,3,3,3,3,3,3,3,3,3,3,3,3,3,3,3,3,3,3,4),(422.083460791944,422.170580161418,
422.259170049367,422.346170390656,422.433151884973,422.520137005079,422.609927570061,
422.697035626069,422.788167445539,422.879299265008,422.967851417088,423.056288812611,
423.144635255809,423.236432588893,423.324676710799,423.412907396735,423.501146015459,
423.589413936308,423.677782236949,423.76621004811,423.854768184213,423.879013920481,
423.967566072561,424.056003468084,424.144349911282,424.236147244366,424.324391366272,
424.412622052208,424.500860670932,424.58912859178,424.677496892421,424.765924703583,
424.854482839685,424.878728575954,424.967280728034,425.055718123557,425.144064566756,
425.235861899839,425.324106021746,425.412336707682,425.500575326406,425.588843247254,
425.677211547896,425.765639359057,425.85419749516,425.878443231427,425.966995383506,
426.055432779029,426.143779222227,426.235576555311,426.323820677217,426.412051363153,
426.500289981877,426.588557902725,426.676926203366,426.765354014527,426.853912150629,
426.878157886899,426.966710038978,427.055147434502,427.1434938777,427.235291210784,
427.32353533269,427.411766018626,427.500004637349,427.588272558198,427.67664085884,
427.765068670001,427.853626806103,427.877872542372,427.971465113027,428.064879770433,
428.158061167363,428.251099314232,428.34395673494,428.366646098882),
 .UNSPECIFIED.);
#378=B_SPLINE_CURVE_WITH_KNOTS('',3,(#60284,#60285,#60286,#60287,#60288,
#60289,#60290,#60291,#60292,#60293,#60294,#60295,#60296,#60297,#60298,#60299,
#60300,#60301,#60302,#60303,#60304,#60305,#60306,#60307,#60308,#60309,#60310,
#60311,#60312,#60313,#60314,#60315,#60316,#60317,#60318,#60319,#60320,#60321,
#60322,#60323,#60324,#60325,#60326,#60327,#60328,#60329,#60330,#60331,#60332,
#60333,#60334,#60335,#60336,#60337,#60338,#60339,#60340,#60341,#60342,#60343,
#60344,#60345,#60346,#60347,#60348,#60349,#60350,#60351,#60352,#60353,#60354,
#60355,#60356,#60357,#60358,#60359,#60360,#60361,#60362,#60363,#60364,#60365,
#60366,#60367,#60368,#60369,#60370,#60371,#60372,#60373,#60374,#60375,#60376,
#60377,#60378,#60379,#60380,#60381,#60382,#60383,#60384,#60385,#60386,#60387,
#60388,#60389,#60390,#60391,#60392,#60393,#60394,#60395,#60396,#60397,#60398,
#60399,#60400,#60401,#60402,#60403,#60404,#60405,#60406,#60407,#60408,#60409,
#60410,#60411,#60412,#60413,#60414,#60415,#60416,#60417,#60418,#60419,#60420,
#60421,#60422,#60423,#60424,#60425,#60426,#60427,#60428,#60429,#60430,#60431,
#60432,#60433,#60434,#60435,#60436,#60437,#60438,#60439,#60440,#60441,#60442,
#60443,#60444,#60445,#60446,#60447,#60448,#60449,#60450,#60451,#60452,#60453,
#60454,#60455,#60456,#60457,#60458,#60459,#60460,#60461,#60462,#60463,#60464,
#60465,#60466,#60467,#60468,#60469,#60470,#60471,#60472,#60473,#60474,#60475,
#60476,#60477,#60478,#60479,#60480,#60481,#60482,#60483,#60484,#60485,#60486,
#60487,#60488,#60489,#60490,#60491,#60492,#60493,#60494,#60495,#60496,#60497,
#60498,#60499,#60500,#60501,#60502,#60503,#60504,#60505,#60506,#60507,#60508,
#60509),.UNSPECIFIED.,.F.,.F.,(4,3,3,3,3,3,3,3,3,3,3,3,3,3,3,3,3,3,3,3,
3,3,3,3,3,3,3,3,3,3,3,3,3,3,3,3,3,3,3,3,3,3,3,3,3,3,3,3,3,3,3,3,3,3,3,3,
3,3,3,3,3,3,3,3,3,3,3,3,3,3,3,3,3,3,3,4),(428.366646099124,428.458660731681,
428.550788526121,428.643125281989,428.735575195126,428.828231383776,428.877587197845,
428.966139349925,429.054576745448,429.142923188646,429.23472052173,429.322964643636,
429.411195329572,429.499433948296,429.587701869144,429.676070169786,429.764497980947,
429.85305611705,429.877301853318,429.965854005398,430.054291400921,430.142637844119,
430.234435177203,430.322679299109,430.410909985045,430.499148603769,430.587416524617,
430.675784825259,430.76421263642,430.852770772523,430.877016508791,430.965568660871,
431.054006056394,431.142352499592,431.234149832676,431.322393954582,431.410624640519,
431.498863259243,431.587131180091,431.675499480732,431.763927291893,431.852485427996,
431.876731164264,431.965283316343,432.053720711866,432.142067155064,432.233864488148,
432.322108610054,432.41033929599,432.498577914713,432.586845835561,432.675214136202,
432.763641947363,432.852200083466,432.876445819736,432.964997971815,433.053435367338,
433.141781810536,433.23357914362,433.321823265527,433.410053951463,433.498292570186,
433.586560491034,433.674928791675,433.763356602836,433.851914738939,433.876160475209,
433.963544690523,434.050789271289,434.137954171459,434.225061902882,434.312134919759,
434.399225629821,434.486322069984,434.573498400505,434.649831406304),
 .UNSPECIFIED.);
#379=B_SPLINE_CURVE_WITH_KNOTS('',3,(#60511,#60512,#60513,#60514,#60515,
#60516,#60517,#60518,#60519,#60520,#60521),.UNSPECIFIED.,.F.,.F.,(4,1,1,
1,1,1,1,1,4),(434.649831406304,434.875875130682,435.875589786155,436.875304441628,
437.875019097101,438.874733752573,439.874448408046,440.874163063519,440.933016713483),
 .UNSPECIFIED.);
#380=B_SPLINE_CURVE_WITH_KNOTS('',3,(#60523,#60524,#60525,#60526,#60527,
#60528,#60529,#60530,#60531,#60532,#60533,#60534,#60535,#60536,#60537,#60538,
#60539,#60540,#60541,#60542,#60543,#60544,#60545,#60546,#60547,#60548,#60549,
#60550,#60551,#60552,#60553,#60554,#60555,#60556,#60557,#60558,#60559,#60560,
#60561,#60562,#60563,#60564,#60565,#60566,#60567,#60568,#60569,#60570,#60571,
#60572,#60573,#60574,#60575,#60576,#60577,#60578,#60579,#60580,#60581,#60582,
#60583,#60584,#60585,#60586,#60587,#60588,#60589,#60590,#60591,#60592,#60593,
#60594,#60595,#60596,#60597,#60598,#60599,#60600,#60601,#60602,#60603,#60604,
#60605,#60606,#60607,#60608,#60609,#60610,#60611,#60612,#60613,#60614,#60615,
#60616,#60617,#60618,#60619,#60620,#60621,#60622,#60623,#60624,#60625,#60626,
#60627,#60628,#60629,#60630,#60631,#60632,#60633,#60634,#60635,#60636,#60637,
#60638,#60639,#60640,#60641,#60642,#60643,#60644,#60645,#60646,#60647,#60648,
#60649,#60650,#60651,#60652,#60653,#60654,#60655,#60656,#60657,#60658,#60659,
#60660,#60661,#60662,#60663,#60664,#60665,#60666,#60667,#60668,#60669,#60670,
#60671,#60672,#60673,#60674,#60675,#60676,#60677,#60678,#60679,#60680,#60681,
#60682,#60683,#60684,#60685,#60686,#60687,#60688,#60689,#60690,#60691,#60692,
#60693,#60694,#60695,#60696,#60697,#60698,#60699,#60700,#60701,#60702,#60703,
#60704,#60705,#60706,#60707,#60708,#60709,#60710,#60711,#60712,#60713,#60714,
#60715,#60716,#60717,#60718,#60719,#60720,#60721,#60722,#60723,#60724,#60725,
#60726,#60727,#60728,#60729,#60730,#60731,#60732,#60733,#60734,#60735,#60736,
#60737,#60738,#60739,#60740,#60741,#60742,#60743,#60744,#60745,#60746,#60747,
#60748),.UNSPECIFIED.,.F.,.F.,(4,3,3,3,3,3,3,3,3,3,3,3,3,3,3,3,3,3,3,3,
3,3,3,3,3,3,3,3,3,3,3,3,3,3,3,3,3,3,3,3,3,3,3,3,3,3,3,3,3,3,3,3,3,3,3,3,
3,3,3,3,3,3,3,3,3,3,3,3,3,3,3,3,3,3,3,4),(440.933016713483,441.020777353221,
441.108427962358,441.195993154872,441.283501177297,441.370980007062,441.458451753743,
441.545938516856,441.633516355183,441.721142246195,441.808908214733,441.873877718992,
441.962429871072,442.050867266595,442.139213709793,442.231011042877,442.319255164783,
442.407485850719,442.495724469443,442.583992390291,442.672360690933,442.760788502094,
442.849346638197,442.873592374465,442.962144526545,443.050581922068,443.138928365266,
443.23072569835,443.318969820256,443.407200506193,443.495439124917,443.583707045765,
443.672075346406,443.760503157567,443.84906129367,443.873307029938,443.961859182017,
444.05029657754,444.138643020738,444.230440353822,444.318684475728,444.406915161664,
444.495153780388,444.583421701236,444.671790001877,444.760217813038,444.84877594914,
444.87302168541,444.96157383749,445.050011233013,445.138357676211,445.230155009295,
445.318399131201,445.406629817137,445.49486843586,445.583136356709,445.67150465735,
445.759932468511,445.848490604614,445.872736340883,445.961288492963,446.049725888486,
446.138072331684,446.229869664768,446.318113786674,446.406344472611,446.494583091335,
446.582851012184,446.671219312825,446.759647123986,446.848205260089,446.872450996356,
446.975474402535,447.078039594968,447.179778915401,447.216201778632),
 .UNSPECIFIED.);
#381=B_SPLINE_CURVE_WITH_KNOTS('',3,(#60750,#60751,#60752,#60753,#60754,
#60755,#60756,#60757,#60758,#60759),.UNSPECIFIED.,.F.,.F.,(4,1,1,1,1,1,
1,4),(447.216202020663,447.872165651829,448.871880307302,449.871594962775,
450.871309618247,451.87102427372,452.870738929193,453.499387327842),
 .UNSPECIFIED.);
#382=B_SPLINE_CURVE_WITH_KNOTS('',3,(#60761,#60762,#60763,#60764,#60765,
#60766,#60767,#60768,#60769,#60770),.UNSPECIFIED.,.F.,.F.,(4,1,1,1,1,1,
1,4),(453.499387327842,453.870453584666,454.870168240139,455.869882895612,
456.869597551084,457.869312206557,458.86902686203,459.782563940701),
 .UNSPECIFIED.);
#383=B_SPLINE_CURVE_WITH_KNOTS('',3,(#60772,#60773,#60774,#60775,#60776,
#60777,#60778,#60779,#60780,#60781,#60782,#60783,#60784,#60785,#60786,#60787,
#60788,#60789,#60790,#60791,#60792,#60793,#60794,#60795,#60796,#60797,#60798,
#60799,#60800,#60801,#60802,#60803,#60804,#60805,#60806,#60807,#60808,#60809,
#60810,#60811,#60812,#60813,#60814,#60815,#60816,#60817,#60818,#60819,#60820,
#60821,#60822,#60823,#60824,#60825,#60826,#60827,#60828,#60829,#60830,#60831,
#60832,#60833,#60834,#60835,#60836,#60837,#60838,#60839,#60840,#60841,#60842,
#60843,#60844,#60845,#60846,#60847,#60848,#60849,#60850,#60851,#60852,#60853,
#60854,#60855,#60856,#60857,#60858,#60859,#60860,#60861,#60862,#60863,#60864,
#60865,#60866,#60867,#60868,#60869,#60870,#60871,#60872,#60873,#60874,#60875,
#60876,#60877,#60878,#60879,#60880,#60881,#60882,#60883,#60884,#60885,#60886,
#60887,#60888,#60889,#60890,#60891,#60892,#60893,#60894,#60895,#60896,#60897,
#60898,#60899,#60900,#60901,#60902,#60903,#60904,#60905,#60906,#60907,#60908,
#60909,#60910,#60911,#60912,#60913,#60914,#60915,#60916,#60917,#60918,#60919,
#60920,#60921,#60922,#60923,#60924,#60925,#60926,#60927,#60928,#60929,#60930,
#60931,#60932,#60933,#60934,#60935,#60936,#60937,#60938,#60939,#60940,#60941,
#60942,#60943,#60944,#60945,#60946,#60947,#60948,#60949,#60950,#60951,#60952,
#60953,#60954,#60955,#60956,#60957,#60958,#60959,#60960,#60961,#60962,#60963,
#60964,#60965,#60966,#60967,#60968,#60969,#60970,#60971,#60972,#60973,#60974,
#60975,#60976,#60977,#60978,#60979,#60980,#60981,#60982,#60983,#60984,#60985,
#60986,#60987,#60988,#60989,#60990,#60991,#60992,#60993,#60994,#60995,#60996,
#60997),.UNSPECIFIED.,.F.,.F.,(4,3,3,3,3,3,3,3,3,3,3,3,3,3,3,3,3,3,3,3,
3,3,3,3,3,3,3,3,3,3,3,3,3,3,3,3,3,3,3,3,3,3,3,3,3,3,3,3,3,3,3,3,3,3,3,3,
3,3,3,3,3,3,3,3,3,3,3,3,3,3,3,3,3,3,3,4),(459.782572635022,459.868741517503,
459.957293669583,460.045731065107,460.134077508305,460.225874841389,460.314118963296,
460.402349649232,460.490588267957,460.578856188805,460.667224489447,460.755652300609,
460.844210436712,460.868456172976,460.957008325056,461.045445720579,461.133792163777,
461.225589496861,461.313833618767,461.402064304703,461.490302923427,461.578570844275,
461.666939144917,461.755366956078,461.84392509218,461.868170828449,461.956722980528,
462.045160376051,462.133506819249,462.225304152333,462.313548274239,462.401778960175,
462.490017578899,462.578285499747,462.666653800388,462.755081611548,462.843639747651,
462.867885483921,462.956437636001,463.044875031524,463.133221474722,463.225018807806,
463.313262929712,463.401493615648,463.489732234372,463.57800015522,463.666368455862,
463.754796267023,463.843354403125,463.867600139394,463.956152291474,464.044589686997,
464.132936130195,464.224733463279,464.312977585185,464.401208271122,464.489446889846,
464.577714810694,464.666083111336,464.754510922497,464.8430690586,464.867314794867,
464.955866946947,465.04430434247,465.132650785668,465.224448118752,465.312692240658,
465.400922926594,465.489161545318,465.577429466167,465.665797766808,465.754225577969,
465.842783714072,465.86702945034,465.994547578253,466.065757942201),
 .UNSPECIFIED.);
#384=B_SPLINE_CURVE_WITH_KNOTS('',3,(#60999,#61000,#61001,#61002,#61003,
#61004,#61005,#61006,#61007,#61008),.UNSPECIFIED.,.F.,.F.,(4,1,1,1,1,1,
1,4),(466.065761334688,466.866744105813,467.866458761286,468.866173416758,
469.865888072231,470.865602727704,471.865317383177,472.348943249381),
 .UNSPECIFIED.);
#385=B_SPLINE_CURVE_WITH_KNOTS('',3,(#61010,#61011,#61012,#61013,#61014,
#61015,#61016,#61017,#61018,#61019),.UNSPECIFIED.,.F.,.F.,(4,1,1,1,1,1,
1,4),(472.348943249381,472.86503203865,473.864746694123,474.864461349595,
475.864176005068,476.863890660541,477.863605316014,478.632128556561),
 .UNSPECIFIED.);
#386=B_SPLINE_CURVE_WITH_KNOTS('',3,(#61021,#61022,#61023,#61024,#61025,
#61026,#61027,#61028,#61029,#61030,#61031),.UNSPECIFIED.,.F.,.F.,(4,1,1,
1,1,1,1,1,4),(478.632128556561,478.863319971487,479.86303462696,480.862749282432,
481.862463937905,482.862178593378,483.861893248851,484.861607904324,484.91531386374),
 .UNSPECIFIED.);
#387=B_SPLINE_CURVE_WITH_KNOTS('',3,(#61033,#61034,#61035,#61036,#61037,
#61038,#61039,#61040,#61041,#61042),.UNSPECIFIED.,.F.,.F.,(4,1,1,1,1,1,
1,4),(484.91531386374,485.861322559797,486.861037215269,487.860751870742,
488.860466526215,489.860181181688,490.859895837161,491.198491737937),
 .UNSPECIFIED.);
#388=B_SPLINE_CURVE_WITH_KNOTS('',3,(#61044,#61045,#61046,#61047,#61048,
#61049,#61050,#61051,#61052,#61053,#61054,#61055,#61056,#61057,#61058,#61059,
#61060,#61061,#61062,#61063,#61064,#61065,#61066,#61067,#61068,#61069,#61070,
#61071,#61072,#61073,#61074,#61075,#61076,#61077,#61078,#61079,#61080,#61081,
#61082,#61083,#61084,#61085,#61086,#61087,#61088,#61089,#61090,#61091,#61092,
#61093,#61094,#61095,#61096,#61097,#61098,#61099,#61100,#61101,#61102,#61103,
#61104,#61105,#61106,#61107,#61108,#61109,#61110,#61111,#61112,#61113,#61114,
#61115,#61116,#61117,#61118,#61119,#61120,#61121,#61122,#61123,#61124,#61125,
#61126,#61127,#61128,#61129,#61130,#61131,#61132,#61133,#61134,#61135,#61136,
#61137,#61138,#61139,#61140,#61141,#61142,#61143,#61144,#61145,#61146,#61147,
#61148,#61149,#61150,#61151,#61152,#61153,#61154,#61155,#61156,#61157,#61158,
#61159,#61160,#61161,#61162,#61163,#61164,#61165,#61166,#61167,#61168,#61169,
#61170,#61171,#61172,#61173,#61174,#61175,#61176,#61177,#61178,#61179,#61180,
#61181,#61182,#61183,#61184,#61185,#61186,#61187,#61188,#61189,#61190,#61191,
#61192,#61193,#61194,#61195,#61196,#61197,#61198,#61199,#61200,#61201,#61202,
#61203,#61204,#61205,#61206,#61207,#61208,#61209,#61210,#61211,#61212,#61213,
#61214,#61215,#61216,#61217,#61218,#61219,#61220,#61221,#61222,#61223,#61224,
#61225,#61226,#61227,#61228,#61229,#61230,#61231,#61232,#61233,#61234,#61235,
#61236,#61237,#61238,#61239,#61240,#61241,#61242,#61243,#61244,#61245,#61246,
#61247,#61248,#61249,#61250,#61251,#61252,#61253,#61254,#61255,#61256,#61257,
#61258,#61259,#61260,#61261,#61262,#61263,#61264,#61265,#61266,#61267,#61268,
#61269),.UNSPECIFIED.,.F.,.F.,(4,3,3,3,3,3,3,3,3,3,3,3,3,3,3,3,3,3,3,3,
3,3,3,3,3,3,3,3,3,3,3,3,3,3,3,3,3,3,3,3,3,3,3,3,3,3,3,3,3,3,3,3,3,3,3,3,
3,3,3,3,3,3,3,3,3,3,3,3,3,3,3,3,3,3,3,4),(491.19849917092,491.286759424022,
491.375007955342,491.463266018858,491.551554870329,491.639950591653,491.728406737234,
491.817005364184,491.859610492634,491.948162644713,492.036600040236,492.124946483433,
492.216743816518,492.304987938423,492.393218624359,492.481457243083,492.56972516393,
492.658093464571,492.746521275732,492.835079411834,492.859325148106,492.947877300185,
493.036314695709,493.124661138907,493.216458471991,493.304702593897,493.392933279833,
493.481171898557,493.569439819405,493.657808120046,493.746235931207,493.83479406731,
493.859039803579,493.947591955659,494.036029351183,494.124375794381,494.216173127465,
494.304417249372,494.392647935309,494.480886554033,494.569154474882,494.657522775524,
494.745950586686,494.834508722789,494.858754459052,494.947306611131,495.035744006654,
495.124090449852,495.215887782936,495.304131904842,495.392362590778,495.480601209502,
495.56886913035,495.657237430991,495.745665242152,495.834223378255,495.858469114525,
495.947021266604,496.035458662126,496.123805105323,496.215602438408,496.303846560313,
496.392077246248,496.480315864971,496.568583785819,496.65695208646,496.74537989762,
496.833938033722,496.858183769998,496.947491550541,497.036679717588,497.125768784926,
497.214770005954,497.303718316016,497.392701397058,497.481684478099),
 .UNSPECIFIED.);
#389=B_SPLINE_CURVE_WITH_KNOTS('',3,(#61271,#61272,#61273,#61274,#61275,
#61276,#61277,#61278,#61279,#61280),.UNSPECIFIED.,.F.,.F.,(4,1,1,1,1,1,
1,4),(497.481692099559,497.857898425471,498.857613080943,499.857327736416,
500.857042391889,501.856757047362,502.856471702835,503.76486095827),
 .UNSPECIFIED.);
#390=B_SPLINE_CURVE_WITH_KNOTS('',3,(#61282,#61283,#61284,#61285,#61286,
#61287,#61288,#61289,#61290,#61291,#61292,#61293,#61294,#61295,#61296,#61297,
#61298,#61299,#61300,#61301,#61302,#61303,#61304,#61305,#61306,#61307,#61308,
#61309,#61310,#61311,#61312,#61313,#61314,#61315,#61316,#61317,#61318,#61319,
#61320,#61321,#61322,#61323,#61324,#61325,#61326,#61327,#61328,#61329,#61330,
#61331,#61332,#61333,#61334,#61335,#61336,#61337,#61338,#61339,#61340,#61341,
#61342,#61343,#61344,#61345,#61346,#61347,#61348,#61349,#61350,#61351,#61352,
#61353,#61354,#61355,#61356,#61357,#61358,#61359,#61360,#61361,#61362,#61363,
#61364,#61365,#61366,#61367,#61368,#61369,#61370,#61371,#61372,#61373,#61374,
#61375,#61376,#61377,#61378,#61379,#61380,#61381,#61382,#61383,#61384,#61385,
#61386,#61387,#61388,#61389,#61390,#61391,#61392,#61393,#61394,#61395,#61396,
#61397,#61398,#61399,#61400,#61401,#61402,#61403,#61404,#61405,#61406,#61407,
#61408,#61409,#61410,#61411,#61412,#61413,#61414,#61415,#61416,#61417,#61418,
#61419,#61420,#61421,#61422,#61423,#61424,#61425,#61426,#61427,#61428,#61429,
#61430,#61431,#61432,#61433,#61434,#61435,#61436,#61437,#61438,#61439,#61440,
#61441,#61442,#61443,#61444,#61445,#61446,#61447,#61448,#61449,#61450,#61451,
#61452,#61453,#61454,#61455,#61456,#61457,#61458,#61459,#61460,#61461,#61462,
#61463,#61464,#61465,#61466,#61467,#61468,#61469,#61470,#61471,#61472,#61473,
#61474,#61475,#61476,#61477,#61478,#61479,#61480,#61481,#61482,#61483,#61484,
#61485,#61486,#61487,#61488,#61489,#61490,#61491,#61492,#61493,#61494,#61495,
#61496,#61497,#61498,#61499,#61500,#61501,#61502,#61503,#61504,#61505,#61506,
#61507),.UNSPECIFIED.,.F.,.F.,(4,3,3,3,3,3,3,3,3,3,3,3,3,3,3,3,3,3,3,3,
3,3,3,3,3,3,3,3,3,3,3,3,3,3,3,3,3,3,3,3,3,3,3,3,3,3,3,3,3,3,3,3,3,3,3,3,
3,3,3,3,3,3,3,3,3,3,3,3,3,3,3,3,3,3,3,4),(503.764869785279,503.856186358308,
503.944738510238,504.033175905611,504.12152234866,504.2133196818,504.30156380356,
504.38979448935,504.47803310793,504.566301028635,504.654669329136,504.743097140158,
504.831655276124,504.85590101378,504.94445316576,505.032890561183,505.121237004278,
505.2130343374,505.301278459201,505.38950914503,505.477747763647,505.566015684387,
505.654383984919,505.742811795971,505.831369931965,505.855615669253,505.944167822066,
506.032605218325,506.120951662261,506.212748995069,506.30099311771,506.38922380438,
506.477462423835,506.565730345411,506.654098646772,506.742526458648,506.831084595454,
506.855330324726,506.943882475663,507.032319870044,507.120666312104,507.212463645616,
507.300707766398,507.388938451218,507.477177068833,507.565444988583,507.653813288145,
507.742241098236,507.830799233292,507.855044980199,507.943597131997,508.032034527227,
508.120380970122,508.212178303315,508.300422424894,508.388653110495,508.476891728876,
508.565159649373,508.653527949655,508.74195576045,508.830513896182,508.854759635672,
508.943311792402,509.031749192592,509.120095640468,509.211892971802,509.300137098383,
509.388367788985,509.476606412361,509.564874337843,509.653242643066,509.741670458786,
509.830228599376,509.854474291144,509.983739743113,510.048055092458),
 .UNSPECIFIED.);
#391=B_SPLINE_CURVE_WITH_KNOTS('',3,(#61509,#61510,#61511,#61512,#61513,
#61514,#61515,#61516,#61517,#61518),.UNSPECIFIED.,.F.,.F.,(4,1,1,1,1,1,
1,4),(510.048058981494,510.854188946617,511.85390360209,512.853618257563,
513.853332913036,514.853047568509,515.852762223982,516.331240399638),
 .UNSPECIFIED.);
#392=B_SPLINE_CURVE_WITH_KNOTS('',3,(#61520,#61521,#61522,#61523,#61524,
#61525,#61526,#61527,#61528,#61529),.UNSPECIFIED.,.F.,.F.,(4,1,1,1,1,1,
1,4),(516.331240399638,516.852476879454,517.852191534927,518.8519061904,
519.851620845873,520.851335501346,521.851050156819,522.614425706818),
 .UNSPECIFIED.);
#393=B_SPLINE_CURVE_WITH_KNOTS('',3,(#61531,#61532,#61533,#61534,#61535,
#61536,#61537,#61538,#61539,#61540,#61541,#61542,#61543,#61544,#61545,#61546,
#61547,#61548,#61549,#61550,#61551,#61552,#61553,#61554,#61555,#61556,#61557,
#61558,#61559,#61560,#61561,#61562,#61563,#61564,#61565,#61566,#61567,#61568,
#61569,#61570,#61571,#61572,#61573,#61574,#61575,#61576,#61577,#61578,#61579,
#61580,#61581,#61582,#61583,#61584,#61585,#61586,#61587,#61588,#61589,#61590,
#61591,#61592,#61593,#61594,#61595,#61596,#61597,#61598,#61599,#61600,#61601,
#61602,#61603,#61604,#61605,#61606,#61607,#61608,#61609,#61610,#61611,#61612,
#61613,#61614,#61615,#61616,#61617,#61618,#61619,#61620,#61621,#61622,#61623,
#61624,#61625,#61626,#61627,#61628,#61629,#61630,#61631,#61632,#61633,#61634,
#61635,#61636,#61637,#61638,#61639,#61640,#61641,#61642,#61643,#61644,#61645,
#61646,#61647,#61648,#61649,#61650,#61651,#61652,#61653,#61654,#61655,#61656,
#61657,#61658,#61659,#61660,#61661,#61662,#61663,#61664,#61665,#61666,#61667,
#61668,#61669,#61670,#61671,#61672,#61673,#61674,#61675,#61676,#61677,#61678,
#61679,#61680,#61681,#61682,#61683,#61684,#61685,#61686,#61687,#61688,#61689,
#61690,#61691,#61692,#61693,#61694,#61695,#61696,#61697,#61698,#61699,#61700,
#61701,#61702,#61703,#61704,#61705,#61706,#61707,#61708,#61709,#61710,#61711,
#61712,#61713,#61714),.UNSPECIFIED.,.F.,.F.,(4,3,3,3,3,3,3,3,3,3,3,3,3,
3,3,3,3,3,3,3,3,3,3,3,3,3,3,3,3,3,3,3,3,3,3,3,3,3,3,3,3,3,3,3,3,3,3,3,3,
3,3,3,3,3,3,3,3,3,3,3,3,4),(522.614425731277,522.732595271784,522.850764812291,
522.939338841653,523.027798028275,523.116166152673,523.207955317059,523.296220715231,
523.384472493103,523.472731997983,523.561020577581,523.649409097732,523.737856897892,
523.826434531246,523.850479467764,523.939059065491,524.027524204539,524.115898653165,
524.207685586924,524.295958186708,524.384217475473,524.472484790942,524.560781471458,
524.649178477884,524.737634998707,524.826221625929,524.850194123237,524.938612611537,
525.026916056542,525.115128415847,525.206975961205,525.295086481409,525.383183961474,
525.471289905623,525.559425819224,525.647663761157,525.735962006623,525.824392749395,
525.84990877871,525.938637365966,526.02725073032,526.115772475931,526.207503845712,
526.295920522753,526.384322455804,526.472730833281,526.561166842936,526.649699920224,
526.738290777186,526.827008176059,526.849623434183,526.93745568206,527.025175697194,
527.112808046017,527.200379484124,527.287919497547,527.375450147699,527.462993483972,
527.550623210395,527.638298940645,527.726108902286,527.787264933936),
 .UNSPECIFIED.);
#394=B_SPLINE_CURVE_WITH_KNOTS('',3,(#61718,#61719,#61720,#61721,#61722,
#61723,#61724,#61725),.UNSPECIFIED.,.F.,.F.,(4,1,1,1,1,4),(-529.848767400601,
-528.849052745128,-527.849338089655,-526.849623434182,-525.84990877871,
-525.597129536099),.UNSPECIFIED.);
#395=B_SPLINE_CURVE_WITH_KNOTS('',3,(#61727,#61728,#61729,#61730,#61731,
#61732,#61733,#61734,#61735,#61736),.UNSPECIFIED.,.F.,.F.,(4,1,1,1,1,1,
1,4),(-525.597129536099,-524.850194123237,-523.850479467764,-522.850764812291,
-521.851050156818,-520.851335501345,-519.851620845873,-519.313944228919),
 .UNSPECIFIED.);
#396=B_SPLINE_CURVE_WITH_KNOTS('',3,(#61738,#61739,#61740,#61741,#61742,
#61743,#61744,#61745,#61746,#61747,#61748,#61749,#61750,#61751,#61752,#61753,
#61754,#61755,#61756,#61757,#61758,#61759,#61760,#61761,#61762,#61763,#61764,
#61765,#61766,#61767,#61768,#61769,#61770,#61771,#61772,#61773,#61774,#61775,
#61776,#61777,#61778,#61779,#61780,#61781,#61782,#61783,#61784,#61785,#61786,
#61787,#61788,#61789,#61790,#61791,#61792,#61793,#61794,#61795,#61796,#61797,
#61798,#61799,#61800,#61801,#61802,#61803,#61804,#61805,#61806,#61807,#61808,
#61809,#61810,#61811,#61812,#61813,#61814,#61815,#61816,#61817,#61818,#61819,
#61820,#61821,#61822,#61823,#61824,#61825,#61826,#61827,#61828,#61829,#61830,
#61831,#61832,#61833,#61834,#61835,#61836,#61837,#61838,#61839,#61840,#61841,
#61842,#61843,#61844,#61845,#61846,#61847,#61848,#61849,#61850,#61851,#61852,
#61853,#61854,#61855,#61856,#61857,#61858,#61859,#61860,#61861,#61862,#61863,
#61864,#61865,#61866,#61867,#61868,#61869,#61870,#61871,#61872,#61873,#61874,
#61875,#61876,#61877,#61878,#61879,#61880,#61881,#61882,#61883,#61884,#61885,
#61886,#61887,#61888,#61889,#61890,#61891,#61892,#61893,#61894,#61895,#61896,
#61897,#61898,#61899,#61900,#61901,#61902,#61903,#61904,#61905,#61906,#61907,
#61908,#61909,#61910,#61911,#61912,#61913,#61914,#61915,#61916,#61917,#61918,
#61919,#61920,#61921,#61922,#61923,#61924,#61925,#61926,#61927,#61928,#61929,
#61930,#61931,#61932,#61933,#61934,#61935,#61936,#61937,#61938,#61939,#61940,
#61941,#61942,#61943,#61944,#61945,#61946,#61947,#61948,#61949,#61950,#61951,
#61952,#61953,#61954,#61955,#61956,#61957,#61958,#61959,#61960,#61961,#61962,
#61963),.UNSPECIFIED.,.F.,.F.,(4,3,3,3,3,3,3,3,3,3,3,3,3,3,3,3,3,3,3,3,
3,3,3,3,3,3,3,3,3,3,3,3,3,3,3,3,3,3,3,3,3,3,3,3,3,3,3,3,3,3,3,3,3,3,3,3,
3,3,3,3,3,3,3,3,3,3,3,3,3,3,3,3,3,3,3,4),(-519.313944022838,-519.219926438778,
-519.125587303341,-519.031086436992,-518.936299770552,-518.8519061904,-518.763353055329,
-518.674914668526,-518.586567226996,-518.494770265487,-518.406525133958,
-518.318293435948,-518.230053803774,-518.141784869172,-518.053415559458,
-517.964986740699,-517.876427606999,-517.852191534927,-517.763639159473,
-517.675201534523,-517.586854856148,-517.495057609062,-517.40681323902,
-517.318582300568,-517.230343425196,-517.142075243814,-517.053706678148,
-516.965278599017,-516.876720192668,-516.852476879454,-516.763925130966,
-516.675488144823,-516.587142116275,-516.495344629738,-516.407100933068,
-516.318870675562,-516.23063248802,-516.142365000663,-516.053997134773,
-515.965569759635,-515.877012058054,-515.852762223981,-515.764209903475,
-515.675772337909,-515.587425723263,-515.495628453919,-515.407384158139,
-515.319153297728,-515.230914504112,-515.14264640814,-515.054277932913,
-514.965849947264,-514.877291638172,-514.853047568508,-514.764495399659,
-514.676057986669,-514.58771152533,-514.495914198794,-514.407670057167,
-514.319439350958,-514.231200711427,-514.142932769258,-514.054564446634,
-513.966136613078,-513.877578454143,-513.853332913036,-513.766099848692,
-513.678981063572,-513.591962273271,-513.504998644919,-513.418067626277,
-513.331146700021,-513.244177277615,-513.157180490533,-513.070089141411,
-513.03075892174),.UNSPECIFIED.);
#397=B_SPLINE_CURVE_WITH_KNOTS('',3,(#61965,#61966,#61967,#61968,#61969,
#61970,#61971,#61972,#61973,#61974,#61975),.UNSPECIFIED.,.F.,.F.,(4,1,1,
1,1,1,1,1,4),(-513.03075892174,-512.853618257563,-511.85390360209,-510.854188946617,
-509.854474291144,-508.854759635672,-507.855044980199,-506.855330324726,
-506.74757361456),.UNSPECIFIED.);
#398=B_SPLINE_CURVE_WITH_KNOTS('',3,(#61977,#61978,#61979,#61980,#61981,
#61982,#61983,#61984,#61985,#61986),.UNSPECIFIED.,.F.,.F.,(4,1,1,1,1,1,
1,4),(-506.74757361456,-505.855615669253,-504.85590101378,-503.856186358307,
-502.856471702834,-501.856757047362,-500.857042391889,-500.46438830738),
 .UNSPECIFIED.);
#399=B_SPLINE_CURVE_WITH_KNOTS('',3,(#61988,#61989,#61990,#61991,#61992,
#61993,#61994,#61995,#61996,#61997),.UNSPECIFIED.,.F.,.F.,(4,1,1,1,1,1,
1,4),(-500.46438830738,-499.857327736416,-498.857613080943,-497.85789842547,
-496.858183769998,-495.858469114525,-494.858754459052,-494.181203000201),
 .UNSPECIFIED.);
#400=B_SPLINE_CURVE_WITH_KNOTS('',3,(#61999,#62000,#62001,#62002,#62003,
#62004,#62005,#62006,#62007,#62008),.UNSPECIFIED.,.F.,.F.,(4,1,1,1,1,1,
1,4),(-494.181203000201,-493.859039803579,-492.859325148106,-491.859610492633,
-490.859895837161,-489.860181181688,-488.860466526215,-487.898022689968),
 .UNSPECIFIED.);
#401=B_SPLINE_CURVE_WITH_KNOTS('',3,(#62010,#62011,#62012,#62013,#62014,
#62015,#62016,#62017,#62018,#62019,#62020,#62021,#62022,#62023,#62024,#62025,
#62026,#62027,#62028,#62029,#62030,#62031,#62032,#62033,#62034,#62035,#62036,
#62037,#62038,#62039,#62040,#62041,#62042,#62043,#62044,#62045,#62046,#62047,
#62048,#62049,#62050,#62051,#62052,#62053,#62054,#62055,#62056,#62057,#62058,
#62059,#62060,#62061,#62062,#62063,#62064,#62065,#62066,#62067,#62068,#62069,
#62070,#62071,#62072,#62073,#62074,#62075,#62076,#62077,#62078,#62079,#62080,
#62081,#62082,#62083,#62084,#62085,#62086,#62087,#62088,#62089,#62090,#62091,
#62092,#62093,#62094,#62095,#62096,#62097,#62098,#62099,#62100,#62101,#62102,
#62103,#62104,#62105,#62106,#62107,#62108,#62109,#62110,#62111,#62112,#62113,
#62114,#62115,#62116,#62117,#62118,#62119,#62120,#62121,#62122,#62123,#62124,
#62125,#62126,#62127,#62128,#62129,#62130,#62131,#62132,#62133,#62134,#62135,
#62136,#62137,#62138,#62139,#62140,#62141,#62142,#62143,#62144,#62145,#62146,
#62147,#62148,#62149,#62150,#62151,#62152,#62153,#62154,#62155,#62156,#62157,
#62158,#62159,#62160,#62161,#62162,#62163,#62164,#62165,#62166,#62167,#62168,
#62169,#62170,#62171,#62172,#62173,#62174,#62175,#62176,#62177,#62178,#62179,
#62180,#62181,#62182,#62183,#62184,#62185,#62186,#62187,#62188,#62189,#62190,
#62191,#62192,#62193,#62194,#62195,#62196,#62197,#62198,#62199,#62200,#62201,
#62202,#62203,#62204,#62205,#62206,#62207,#62208,#62209,#62210,#62211,#62212,
#62213,#62214,#62215,#62216,#62217,#62218,#62219,#62220,#62221,#62222,#62223,
#62224,#62225,#62226,#62227,#62228,#62229,#62230,#62231,#62232,#62233,#62234,
#62235,#62236,#62237,#62238),.UNSPECIFIED.,.F.,.F.,(4,3,3,3,3,3,3,3,3,3,
3,3,3,3,3,3,3,3,3,3,3,3,3,3,3,3,3,3,3,3,3,3,3,3,3,3,3,3,3,3,3,3,3,3,3,3,
3,3,3,3,3,3,3,3,3,3,3,3,3,3,3,3,3,3,3,3,3,3,3,3,3,3,3,3,3,3,4),(-487.898017693021,
-487.860751870742,-487.772199718662,-487.683762323139,-487.595415879941,
-487.503618546857,-487.415374424951,-487.327143739015,-487.238905120291,
-487.150637199442,-487.062268898801,-486.97384108764,-486.885282951537,
-486.861037215269,-486.772485063189,-486.684047667666,-486.595701224468,
-486.503903891384,-486.415659769478,-486.327429083542,-486.239190464818,
-486.15092254397,-486.062554243328,-485.974126432167,-485.885568296064,
-485.861322559796,-485.772770407716,-485.684333012193,-485.595986568995,
-485.504189235911,-485.415945114005,-485.327714428068,-485.239475809344,
-485.151207888496,-485.062839587855,-484.974411776693,-484.885853640591,
-484.861607904323,-484.773055752244,-484.684618356721,-484.596271913523,
-484.504474580439,-484.416230458533,-484.327999772597,-484.239761153874,
-484.151493233026,-484.063124932385,-483.974697121224,-483.886138985121,
-483.861893248851,-483.773341096771,-483.684903701248,-483.59655725805,
-483.504759924966,-483.41651580306,-483.328285117124,-483.2400464984,-483.151778577551,
-483.06341027691,-482.974982465749,-482.886424329646,-482.862178593378,
-482.773626441298,-482.685189045775,-482.596842602576,-482.505045269492,
-482.416801147586,-482.32857046165,-482.240331842926,-482.152063922077,
-482.063695621436,-481.975267810275,-481.886709674172,-481.862463937905,
-481.745859209655,-481.631952730172,-481.614832480211),.UNSPECIFIED.);
#402=B_SPLINE_CURVE_WITH_KNOTS('',3,(#62240,#62241,#62242,#62243,#62244,
#62245,#62246,#62247,#62248,#62249),.UNSPECIFIED.,.F.,.F.,(4,1,1,1,1,1,
1,4),(-481.614832385842,-480.862749282432,-479.863034626959,-478.863319971486,
-477.863605316014,-476.863890660541,-475.864176005068,-475.331647078662),
 .UNSPECIFIED.);
#403=B_SPLINE_CURVE_WITH_KNOTS('',3,(#62251,#62252,#62253,#62254,#62255,
#62256,#62257,#62258,#62259,#62260),.UNSPECIFIED.,.F.,.F.,(4,1,1,1,1,1,
1,4),(-475.331647078662,-474.864461349595,-473.864746694122,-472.86503203865,
-471.865317383177,-470.865602727704,-469.865888072231,-469.048461771483),
 .UNSPECIFIED.);
#404=B_SPLINE_CURVE_WITH_KNOTS('',3,(#62262,#62263,#62264,#62265,#62266,
#62267,#62268,#62269,#62270,#62271,#62272),.UNSPECIFIED.,.F.,.F.,(4,1,1,
1,1,1,1,1,4),(-469.048461771483,-468.866173416758,-467.866458761285,-466.866744105813,
-465.86702945034,-464.867314794867,-463.867600139394,-462.867885483921,
-462.765276464303),.UNSPECIFIED.);
#405=B_SPLINE_CURVE_WITH_KNOTS('',3,(#62274,#62275,#62276,#62277,#62278,
#62279,#62280,#62281,#62282,#62283),.UNSPECIFIED.,.F.,.F.,(4,1,1,1,1,1,
1,4),(-462.765276464303,-461.868170828448,-460.868456172976,-459.868741517503,
-458.86902686203,-457.869312206557,-456.869597551084,-456.482098551466),
 .UNSPECIFIED.);
#406=B_SPLINE_CURVE_WITH_KNOTS('',3,(#62285,#62286,#62287,#62288,#62289,
#62290,#62291,#62292,#62293,#62294,#62295,#62296,#62297,#62298,#62299,#62300,
#62301,#62302,#62303,#62304,#62305,#62306,#62307,#62308,#62309,#62310,#62311,
#62312,#62313,#62314,#62315,#62316,#62317,#62318,#62319,#62320,#62321,#62322,
#62323,#62324,#62325,#62326,#62327,#62328,#62329,#62330,#62331,#62332,#62333,
#62334,#62335,#62336,#62337,#62338,#62339,#62340,#62341,#62342,#62343,#62344,
#62345,#62346,#62347,#62348,#62349,#62350,#62351,#62352,#62353,#62354,#62355,
#62356,#62357,#62358,#62359,#62360,#62361,#62362,#62363,#62364,#62365,#62366,
#62367,#62368,#62369,#62370,#62371,#62372,#62373,#62374,#62375,#62376,#62377,
#62378,#62379,#62380,#62381,#62382,#62383,#62384,#62385,#62386,#62387,#62388,
#62389,#62390,#62391,#62392,#62393,#62394,#62395,#62396,#62397,#62398,#62399,
#62400,#62401,#62402,#62403,#62404,#62405,#62406,#62407,#62408,#62409,#62410,
#62411,#62412,#62413,#62414,#62415,#62416,#62417,#62418,#62419,#62420,#62421,
#62422,#62423,#62424,#62425,#62426,#62427,#62428,#62429,#62430,#62431,#62432,
#62433,#62434,#62435,#62436,#62437,#62438,#62439,#62440,#62441,#62442,#62443,
#62444,#62445,#62446,#62447,#62448,#62449,#62450,#62451,#62452,#62453,#62454,
#62455,#62456,#62457,#62458,#62459,#62460,#62461,#62462,#62463,#62464,#62465,
#62466,#62467,#62468,#62469,#62470,#62471,#62472,#62473,#62474,#62475,#62476,
#62477,#62478,#62479,#62480,#62481,#62482,#62483,#62484,#62485,#62486,#62487,
#62488,#62489,#62490,#62491,#62492,#62493,#62494,#62495,#62496,#62497,#62498,
#62499,#62500,#62501,#62502,#62503,#62504,#62505,#62506,#62507,#62508,#62509,
#62510),.UNSPECIFIED.,.F.,.F.,(4,3,3,3,3,3,3,3,3,3,3,3,3,3,3,3,3,3,3,3,
3,3,3,3,3,3,3,3,3,3,3,3,3,3,3,3,3,3,3,3,3,3,3,3,3,3,3,3,3,3,3,3,3,3,3,3,
3,3,3,3,3,3,3,3,3,3,3,3,3,3,3,3,3,3,3,4),(-456.482091157123,-456.39293905207,
-456.303770120477,-456.214564491945,-456.12523803452,-456.035848798725,
-455.946295126569,-455.869882895611,-455.781330743532,-455.692893348009,
-455.604546904811,-455.512749571727,-455.424505449821,-455.336274763885,
-455.248036145161,-455.159768224313,-455.071399923672,-454.982972112511,
-454.894413976409,-454.870168240139,-454.781616088059,-454.693178692536,
-454.604832249338,-454.513034916254,-454.424790794348,-454.336560108412,
-454.248321489688,-454.160053568839,-454.071685268198,-453.983257457037,
-453.894699320934,-453.870453584666,-453.781901432586,-453.693464037063,
-453.605117593865,-453.513320260781,-453.425076138875,-453.336845452938,
-453.248606834214,-453.160338913365,-453.071970612724,-452.983542801563,
-452.89498466546,-452.870738929193,-452.782186777114,-452.69374938159,-452.605402938392,
-452.513605605308,-452.425361483402,-452.337130797466,-452.248892178742,
-452.160624257893,-452.072255957252,-451.983828146091,-451.895270009989,
-451.87102427372,-451.78247212164,-451.694034726117,-451.605688282919,-451.513890949835,
-451.425646827929,-451.337416141993,-451.249177523268,-451.160909602419,
-451.072541301778,-450.984113490617,-450.895555354514,-450.871309618247,
-450.782910718183,-450.694622961227,-450.60642468146,-450.518294288706,
-450.430203020071,-450.342135685022,-450.254047585887,-450.198905849944),
 .UNSPECIFIED.);
#407=B_SPLINE_CURVE_WITH_KNOTS('',3,(#62512,#62513,#62514,#62515,#62516,
#62517,#62518,#62519,#62520,#62521),.UNSPECIFIED.,.F.,.F.,(4,1,1,1,1,1,
1,4),(-450.198898760757,-449.871594962774,-448.871880307302,-447.872165651829,
-446.872450996356,-445.872736340883,-444.87302168541,-443.915726084063),
 .UNSPECIFIED.);
#408=B_SPLINE_CURVE_WITH_KNOTS('',3,(#62523,#62524,#62525,#62526,#62527,
#62528,#62529,#62530,#62531,#62532,#62533,#62534,#62535,#62536,#62537,#62538,
#62539,#62540,#62541,#62542,#62543,#62544,#62545,#62546,#62547,#62548,#62549,
#62550,#62551,#62552,#62553,#62554,#62555,#62556,#62557,#62558,#62559,#62560,
#62561,#62562,#62563,#62564,#62565,#62566,#62567,#62568,#62569,#62570,#62571,
#62572,#62573,#62574,#62575,#62576,#62577,#62578,#62579,#62580,#62581,#62582,
#62583,#62584,#62585,#62586,#62587,#62588,#62589,#62590,#62591,#62592,#62593,
#62594,#62595,#62596,#62597,#62598,#62599,#62600,#62601,#62602,#62603,#62604,
#62605,#62606,#62607,#62608,#62609,#62610,#62611,#62612,#62613,#62614,#62615,
#62616,#62617,#62618,#62619,#62620,#62621,#62622,#62623,#62624,#62625,#62626,
#62627,#62628,#62629,#62630,#62631,#62632,#62633,#62634,#62635,#62636,#62637,
#62638,#62639,#62640,#62641,#62642,#62643,#62644,#62645,#62646,#62647,#62648,
#62649,#62650,#62651,#62652,#62653,#62654,#62655,#62656,#62657,#62658,#62659,
#62660,#62661,#62662,#62663,#62664,#62665,#62666,#62667,#62668,#62669,#62670,
#62671,#62672,#62673,#62674,#62675,#62676,#62677,#62678,#62679,#62680,#62681,
#62682,#62683,#62684,#62685,#62686,#62687,#62688,#62689,#62690,#62691,#62692,
#62693,#62694,#62695,#62696,#62697,#62698,#62699,#62700,#62701,#62702,#62703,
#62704,#62705,#62706,#62707,#62708,#62709,#62710,#62711,#62712,#62713,#62714,
#62715,#62716,#62717,#62718,#62719,#62720,#62721,#62722,#62723,#62724,#62725,
#62726,#62727,#62728,#62729,#62730,#62731,#62732,#62733,#62734,#62735,#62736,
#62737,#62738,#62739,#62740,#62741,#62742,#62743,#62744,#62745,#62746,#62747,
#62748,#62749,#62750,#62751),.UNSPECIFIED.,.F.,.F.,(4,3,3,3,3,3,3,3,3,3,
3,3,3,3,3,3,3,3,3,3,3,3,3,3,3,3,3,3,3,3,3,3,3,3,3,3,3,3,3,3,3,3,3,3,3,3,
3,3,3,3,3,3,3,3,3,3,3,3,3,3,3,3,3,3,3,3,3,3,3,3,3,3,3,3,3,3,4),(-443.915720542764,
-443.873307029937,-443.784754877858,-443.696317482335,-443.607971039137,
-443.516173706053,-443.427929584147,-443.339698898211,-443.251460279487,
-443.163192358639,-443.074824057998,-442.986396246837,-442.897838110735,
-442.873592374465,-442.785040222385,-442.696602826862,-442.608256383664,
-442.51645905058,-442.428214928674,-442.339984242738,-442.251745624014,
-442.163477703165,-442.075109402524,-441.986681591363,-441.89812345526,
-441.873877718992,-441.785325566912,-441.696888171389,-441.608541728191,
-441.516744395107,-441.428500273201,-441.340269587264,-441.25203096854,
-441.163763047692,-441.075394747051,-440.986966935889,-440.898408799787,
-440.874163063519,-440.785610911439,-440.697173515916,-440.608827072718,
-440.517029739634,-440.428785617728,-440.340554931792,-440.252316313068,
-440.16404839222,-440.075680091579,-439.987252280418,-439.898694144315,
-439.874448408046,-439.785896255966,-439.697458860443,-439.609112417245,
-439.517315084161,-439.429070962255,-439.340840276319,-439.252601657595,
-439.164333736747,-439.075965436105,-438.987537624944,-438.898979488841,
-438.874733752573,-438.786181600493,-438.69774420497,-438.609397761772,
-438.517600428688,-438.429356306782,-438.341125620845,-438.252887002121,
-438.164619081273,-438.076250780631,-437.98782296947,-437.899264833367,
-437.8750190971,-437.75377719744,-437.639047704226,-437.632535297779),
 .UNSPECIFIED.);
#409=B_SPLINE_CURVE_WITH_KNOTS('',3,(#62753,#62754,#62755,#62756,#62757,
#62758,#62759,#62760,#62761,#62762),.UNSPECIFIED.,.F.,.F.,(4,1,1,1,1,1,
1,4),(-437.632535235585,-436.875304441628,-435.875589786155,-434.875875130682,
-433.876160475209,-432.876445819736,-431.876731164263,-431.349349928405),
 .UNSPECIFIED.);
#410=B_SPLINE_CURVE_WITH_KNOTS('',3,(#62764,#62765,#62766,#62767,#62768,
#62769,#62770,#62771,#62772,#62773),.UNSPECIFIED.,.F.,.F.,(4,1,1,1,1,1,
1,4),(-431.349349928405,-430.877016508791,-429.877301853318,-428.877587197845,
-427.877872542372,-426.878157886899,-425.878443231426,-425.066169088357),
 .UNSPECIFIED.);
#411=B_SPLINE_CURVE_WITH_KNOTS('',3,(#62775,#62776,#62777,#62778,#62779,
#62780,#62781,#62782,#62783,#62784,#62785,#62786,#62787,#62788,#62789,#62790,
#62791,#62792,#62793,#62794,#62795,#62796,#62797,#62798,#62799,#62800,#62801,
#62802,#62803,#62804,#62805,#62806,#62807,#62808,#62809,#62810,#62811,#62812,
#62813,#62814,#62815,#62816,#62817,#62818,#62819,#62820,#62821,#62822,#62823,
#62824,#62825,#62826,#62827,#62828,#62829,#62830,#62831,#62832,#62833,#62834,
#62835,#62836,#62837,#62838,#62839,#62840,#62841,#62842,#62843,#62844,#62845,
#62846,#62847,#62848,#62849,#62850,#62851,#62852,#62853,#62854,#62855,#62856,
#62857,#62858,#62859,#62860,#62861,#62862,#62863,#62864,#62865,#62866,#62867,
#62868,#62869,#62870,#62871,#62872,#62873,#62874,#62875,#62876,#62877,#62878,
#62879,#62880,#62881,#62882,#62883,#62884,#62885,#62886,#62887,#62888,#62889,
#62890,#62891,#62892,#62893,#62894,#62895,#62896,#62897,#62898,#62899,#62900,
#62901,#62902,#62903,#62904,#62905,#62906,#62907,#62908,#62909,#62910,#62911,
#62912,#62913,#62914,#62915,#62916,#62917,#62918,#62919,#62920,#62921,#62922,
#62923,#62924,#62925,#62926,#62927,#62928,#62929,#62930,#62931,#62932,#62933,
#62934,#62935,#62936,#62937,#62938,#62939,#62940,#62941,#62942,#62943,#62944,
#62945,#62946,#62947,#62948,#62949,#62950,#62951,#62952,#62953,#62954,#62955,
#62956,#62957,#62958,#62959,#62960,#62961,#62962,#62963,#62964,#62965,#62966,
#62967,#62968,#62969,#62970,#62971,#62972,#62973,#62974,#62975,#62976,#62977,
#62978,#62979,#62980,#62981,#62982,#62983,#62984,#62985,#62986,#62987,#62988,
#62989,#62990,#62991,#62992,#62993,#62994,#62995,#62996,#62997,#62998,#62999,
#63000),.UNSPECIFIED.,.F.,.F.,(4,3,3,3,3,3,3,3,3,3,3,3,3,3,3,3,3,3,3,3,
3,3,3,3,3,3,3,3,3,3,3,3,3,3,3,3,3,3,3,3,3,3,3,3,3,3,3,3,3,3,3,3,3,3,3,3,
3,3,3,3,3,3,3,3,3,3,3,3,3,3,3,3,3,3,3,4),(-425.066164621226,-424.934650446996,
-424.878728575954,-424.790176423874,-424.701739028351,-424.613392585153,
-424.521595252069,-424.433351130163,-424.345120444227,-424.256881825503,
-424.168613904655,-424.080245604013,-423.991817792852,-423.903259656749,
-423.879013920481,-423.790461768401,-423.702024372878,-423.61367792968,
-423.521880596596,-423.43363647469,-423.345405788754,-423.25716717003,-423.168899249181,
-423.08053094854,-422.992103137379,-422.903545001276,-422.879299265008,
-422.790747112928,-422.702309717405,-422.613963274207,-422.522165941123,
-422.433921819217,-422.345691133281,-422.257452514557,-422.169184593709,
-422.080816293068,-421.992388481907,-421.903830345804,-421.879584609535,
-421.791032457455,-421.702595061932,-421.614248618734,-421.52245128565,
-421.434207163744,-421.345976477808,-421.257737859084,-421.169469938235,
-421.081101637594,-420.992673826433,-420.90411569033,-420.879869954062,
-420.791317801982,-420.702880406459,-420.614533963261,-420.522736630177,
-420.434492508271,-420.346261822334,-420.25802320361,-420.169755282762,
-420.081386982121,-419.992959170959,-419.904401034857,-419.880155298589,
-419.79160314651,-419.703165750987,-419.614819307789,-419.523021974705,
-419.434777852799,-419.346547166863,-419.258308548139,-419.170040627291,
-419.08167232665,-418.993244515489,-418.904686379387,-418.880440643117,
-418.782979314046),.UNSPECIFIED.);
#412=B_SPLINE_CURVE_WITH_KNOTS('',3,(#63002,#63003,#63004,#63005,#63006,
#63007,#63008,#63009,#63010,#63011),.UNSPECIFIED.,.F.,.F.,(4,1,1,1,1,1,
1,4),(-418.782970387294,-417.880725987644,-416.881011332171,-415.881296676698,
-414.881582021225,-413.881867365752,-412.88215271028,-412.499801520433),
 .UNSPECIFIED.);
#413=B_SPLINE_CURVE_WITH_KNOTS('',3,(#63013,#63014,#63015,#63016,#63017,
#63018,#63019,#63020,#63021,#63022,#63023,#63024,#63025,#63026,#63027,#63028,
#63029,#63030,#63031,#63032,#63033,#63034,#63035,#63036,#63037,#63038,#63039,
#63040,#63041,#63042,#63043,#63044,#63045,#63046,#63047,#63048,#63049,#63050,
#63051,#63052,#63053,#63054,#63055,#63056,#63057,#63058,#63059,#63060,#63061,
#63062,#63063,#63064,#63065,#63066,#63067,#63068,#63069,#63070,#63071,#63072,
#63073,#63074,#63075,#63076,#63077,#63078,#63079,#63080,#63081,#63082,#63083,
#63084,#63085,#63086,#63087,#63088,#63089,#63090,#63091,#63092,#63093,#63094,
#63095,#63096,#63097,#63098,#63099,#63100,#63101,#63102,#63103,#63104,#63105,
#63106,#63107,#63108,#63109,#63110,#63111,#63112,#63113,#63114,#63115,#63116,
#63117,#63118,#63119,#63120,#63121,#63122,#63123,#63124,#63125,#63126,#63127,
#63128,#63129,#63130,#63131,#63132,#63133,#63134,#63135,#63136,#63137,#63138,
#63139,#63140,#63141,#63142,#63143,#63144,#63145,#63146,#63147,#63148,#63149,
#63150,#63151,#63152,#63153,#63154,#63155,#63156,#63157,#63158,#63159,#63160,
#63161,#63162,#63163,#63164,#63165,#63166,#63167,#63168,#63169,#63170,#63171,
#63172,#63173,#63174,#63175,#63176,#63177,#63178,#63179,#63180,#63181,#63182,
#63183,#63184,#63185,#63186,#63187,#63188,#63189,#63190,#63191,#63192,#63193,
#63194,#63195,#63196,#63197,#63198,#63199,#63200,#63201,#63202,#63203,#63204,
#63205,#63206,#63207,#63208,#63209,#63210,#63211,#63212,#63213,#63214,#63215,
#63216,#63217,#63218,#63219,#63220,#63221,#63222,#63223,#63224,#63225,#63226,
#63227,#63228,#63229,#63230,#63231,#63232,#63233,#63234,#63235,#63236,#63237,
#63238),.UNSPECIFIED.,.F.,.F.,(4,3,3,3,3,3,3,3,3,3,3,3,3,3,3,3,3,3,3,3,
3,3,3,3,3,3,3,3,3,3,3,3,3,3,3,3,3,3,3,3,3,3,3,3,3,3,3,3,3,3,3,3,3,3,3,3,
3,3,3,3,3,3,3,3,3,3,3,3,3,3,3,3,3,3,3,4),(-412.499794006866,-412.410749231375,
-412.321691006471,-412.232599270962,-412.143389567396,-412.054119542542,
-411.964684583505,-411.882438054807,-411.793885902727,-411.705448507204,
-411.617102064006,-411.525304730922,-411.437060609015,-411.348829923079,
-411.260591304355,-411.172323383506,-411.083955082865,-410.995527271704,
-410.906969135601,-410.882723399334,-410.794171247254,-410.705733851731,
-410.617387408533,-410.525590075449,-410.437345953543,-410.349115267606,
-410.260876648883,-410.172608728035,-410.084240427393,-409.995812616232,
-409.907254480129,-409.883008743861,-409.794456591781,-409.706019196258,
-409.61767275306,-409.525875419976,-409.43763129807,-409.349400612134,-409.26116199341,
-409.172894072562,-409.084525771921,-408.99609796076,-408.907539824657,
-408.883294088388,-408.794741936308,-408.706304540785,-408.617958097587,
-408.526160764503,-408.437916642597,-408.349685956661,-408.261447337937,
-408.173179417088,-408.084811116446,-407.996383305285,-407.907825169182,
-407.883579432915,-407.795027280835,-407.706589885313,-407.618243442115,
-407.526446109031,-407.438201987125,-407.349971301189,-407.261732682465,
-407.173464761617,-407.085096460976,-406.996668649815,-406.908110513712,
-406.883864777443,-406.795383472727,-406.707014034475,-406.618734886537,
-406.530524528595,-406.442355489767,-406.354211255501,-406.266049699108,
-406.216608699687),.UNSPECIFIED.);
#414=B_SPLINE_CURVE_WITH_KNOTS('',3,(#63240,#63241,#63242,#63243,#63244,
#63245,#63246,#63247,#63248,#63249),.UNSPECIFIED.,.F.,.F.,(4,1,1,1,1,1,
1,4),(-406.216601437559,-405.88415012197,-404.884435466497,-403.884720811024,
-402.885006155551,-401.885291500078,-400.885576844606,-399.933423392507),
 .UNSPECIFIED.);
#415=B_SPLINE_CURVE_WITH_KNOTS('',3,(#63251,#63252,#63253,#63254,#63255,
#63256,#63257,#63258,#63259,#63260,#63261,#63262),.UNSPECIFIED.,.F.,.F.,
(4,2,1,1,1,1,1,1,4),(-399.933423392507,-399.885862189133,-398.88614753366,
-397.886432878187,-396.886718222714,-395.887003567241,-394.887288911769,
-393.887574256296,-393.650238085328),.UNSPECIFIED.);
#416=B_SPLINE_CURVE_WITH_KNOTS('',3,(#63264,#63265,#63266,#63267,#63268,
#63269,#63270,#63271,#63272,#63273),.UNSPECIFIED.,.F.,.F.,(4,1,1,1,1,1,
1,4),(-393.650238085328,-392.887859600823,-391.88814494535,-390.888430289877,
-389.888715634404,-388.889000978932,-387.889286323459,-387.367052778148),
 .UNSPECIFIED.);
#417=B_SPLINE_CURVE_WITH_KNOTS('',3,(#63275,#63276,#63277,#63278,#63279,
#63280,#63281,#63282,#63283,#63284),.UNSPECIFIED.,.F.,.F.,(4,1,1,1,1,1,
1,4),(-387.367052778148,-386.889571667986,-385.889857012513,-384.89014235704,
-383.890427701567,-382.890713046095,-381.890998390622,-381.083871454974),
 .UNSPECIFIED.);
#418=B_SPLINE_CURVE_WITH_KNOTS('',3,(#63286,#63287,#63288,#63289,#63290,
#63291,#63292,#63293,#63294,#63295,#63296,#63297,#63298,#63299,#63300,#63301,
#63302,#63303,#63304,#63305,#63306,#63307,#63308,#63309,#63310,#63311,#63312,
#63313,#63314,#63315,#63316,#63317,#63318,#63319,#63320,#63321,#63322,#63323,
#63324,#63325,#63326,#63327,#63328,#63329,#63330,#63331,#63332,#63333,#63334,
#63335,#63336,#63337,#63338,#63339,#63340,#63341,#63342,#63343,#63344,#63345,
#63346,#63347,#63348,#63349,#63350,#63351,#63352,#63353,#63354,#63355,#63356,
#63357,#63358,#63359,#63360,#63361,#63362,#63363,#63364,#63365,#63366,#63367,
#63368,#63369,#63370,#63371,#63372,#63373,#63374,#63375,#63376,#63377,#63378,
#63379,#63380,#63381,#63382,#63383,#63384,#63385,#63386,#63387,#63388,#63389,
#63390,#63391,#63392,#63393,#63394,#63395,#63396,#63397,#63398,#63399,#63400,
#63401,#63402,#63403,#63404,#63405,#63406,#63407,#63408,#63409,#63410,#63411,
#63412,#63413,#63414,#63415,#63416,#63417,#63418,#63419,#63420,#63421,#63422,
#63423,#63424,#63425,#63426,#63427,#63428,#63429,#63430,#63431,#63432,#63433,
#63434,#63435,#63436,#63437,#63438,#63439,#63440,#63441,#63442,#63443,#63444,
#63445,#63446,#63447,#63448,#63449,#63450,#63451,#63452,#63453,#63454,#63455,
#63456,#63457,#63458,#63459,#63460,#63461,#63462,#63463,#63464,#63465,#63466,
#63467,#63468,#63469,#63470,#63471,#63472,#63473,#63474,#63475,#63476,#63477,
#63478,#63479,#63480,#63481,#63482,#63483,#63484,#63485,#63486,#63487,#63488,
#63489,#63490,#63491,#63492,#63493,#63494,#63495,#63496,#63497,#63498,#63499,
#63500,#63501,#63502,#63503,#63504,#63505,#63506,#63507,#63508,#63509,#63510,
#63511),.UNSPECIFIED.,.F.,.F.,(4,3,3,3,3,3,3,3,3,3,3,3,3,3,3,3,3,3,3,3,
3,3,3,3,3,3,3,3,3,3,3,3,3,3,3,3,3,3,3,3,3,3,3,3,3,3,3,3,3,3,3,3,3,3,3,3,
3,3,3,3,3,3,3,3,3,3,3,3,3,3,3,3,3,3,3,4),(-381.083867470969,-380.954249617554,
-380.891283735149,-380.80273158307,-380.714294187547,-380.625947744349,
-380.534150411265,-380.445906289359,-380.357675603423,-380.2694369847,-380.181169063852,
-380.092800763211,-380.00437295205,-379.915814815947,-379.891569079676,
-379.803016927596,-379.714579532073,-379.626233088875,-379.534435755791,
-379.446191633885,-379.357960947949,-379.269722329225,-379.181454408376,
-379.093086107735,-379.004658296574,-378.916100160471,-378.891854424203,
-378.803302272123,-378.7148648766,-378.626518433402,-378.534721100318,-378.446476978411,
-378.358246292475,-378.270007673751,-378.181739752903,-378.093371452261,
-378.0049436411,-377.916385504997,-377.89213976873,-377.803587616651,-377.715150221128,
-377.62680377793,-377.535006444846,-377.44676232294,-377.358531637004,-377.27029301828,
-377.182025097432,-377.093656796791,-377.005228985631,-376.916670849528,
-376.892425113258,-376.803872961178,-376.715435565655,-376.627089122457,
-376.535291789373,-376.447047667467,-376.358816981531,-376.270578362807,
-376.182310441959,-376.093942141318,-376.005514330157,-375.916956194054,
-375.892710457785,-375.804158305705,-375.715720910182,-375.627374466984,
-375.5355771339,-375.447333011993,-375.359102326057,-375.270863707333,-375.182595786484,
-375.094227485843,-375.005799674682,-374.917241538579,-374.892995802312,
-374.800682163789),.UNSPECIFIED.);
#419=B_SPLINE_CURVE_WITH_KNOTS('',3,(#63513,#63514,#63515,#63516,#63517,
#63518,#63519,#63520,#63521,#63522),.UNSPECIFIED.,.F.,.F.,(4,1,1,1,1,1,
1,4),(-374.800673316255,-373.893281146839,-372.893566491366,-371.893851835893,
-370.894137180421,-369.894422524948,-368.894707869475,-368.517504463139),
 .UNSPECIFIED.);
#420=B_SPLINE_CURVE_WITH_KNOTS('',3,(#63524,#63525,#63526,#63527,#63528,
#63529,#63530,#63531,#63532,#63533,#63534,#63535,#63536,#63537,#63538,#63539,
#63540,#63541,#63542,#63543,#63544,#63545,#63546,#63547,#63548,#63549,#63550,
#63551,#63552,#63553,#63554,#63555,#63556,#63557,#63558,#63559,#63560,#63561,
#63562,#63563,#63564,#63565,#63566,#63567,#63568,#63569,#63570,#63571,#63572,
#63573,#63574,#63575,#63576,#63577,#63578,#63579,#63580,#63581,#63582,#63583,
#63584,#63585,#63586,#63587,#63588,#63589,#63590,#63591,#63592,#63593,#63594,
#63595,#63596,#63597,#63598,#63599,#63600,#63601,#63602,#63603,#63604,#63605,
#63606,#63607,#63608,#63609,#63610,#63611,#63612,#63613,#63614,#63615,#63616,
#63617,#63618,#63619,#63620,#63621,#63622,#63623,#63624,#63625,#63626,#63627,
#63628,#63629,#63630,#63631,#63632,#63633,#63634,#63635,#63636,#63637,#63638,
#63639,#63640,#63641,#63642,#63643,#63644,#63645,#63646,#63647,#63648,#63649,
#63650,#63651,#63652,#63653,#63654,#63655,#63656,#63657,#63658,#63659,#63660,
#63661,#63662,#63663,#63664,#63665,#63666,#63667,#63668,#63669,#63670,#63671,
#63672,#63673,#63674,#63675,#63676,#63677,#63678,#63679,#63680,#63681,#63682,
#63683,#63684,#63685,#63686,#63687,#63688,#63689,#63690,#63691,#63692,#63693,
#63694,#63695,#63696,#63697,#63698,#63699,#63700,#63701,#63702,#63703,#63704,
#63705,#63706,#63707,#63708,#63709,#63710,#63711,#63712,#63713,#63714,#63715,
#63716,#63717,#63718,#63719,#63720,#63721,#63722,#63723,#63724,#63725,#63726,
#63727,#63728,#63729,#63730,#63731,#63732,#63733,#63734,#63735,#63736,#63737,
#63738,#63739,#63740,#63741,#63742,#63743,#63744,#63745,#63746,#63747,#63748,
#63749),.UNSPECIFIED.,.F.,.F.,(4,3,3,3,3,3,3,3,3,3,3,3,3,3,3,3,3,3,3,3,
3,3,3,3,3,3,3,3,3,3,3,3,3,3,3,3,3,3,3,3,3,3,3,3,3,3,3,3,3,3,3,3,3,3,3,3,
3,3,3,3,3,3,3,3,3,3,3,3,3,3,3,3,3,3,3,4),(-368.517496856609,-368.428556137099,
-368.339605247134,-368.250623947272,-368.161527466105,-368.072373070321,
-367.983053193189,-367.894993214002,-367.806441061922,-367.718003666399,
-367.629657223201,-367.537859890117,-367.44961576821,-367.361385082274,
-367.27314646355,-367.184878542702,-367.09651024206,-367.008082430899,-366.919524294796,
-366.895278558529,-366.80672640645,-366.718289010927,-366.629942567729,
-366.538145234645,-366.449901112739,-366.361670426803,-366.273431808079,
-366.18516388723,-366.096795586589,-366.008367775429,-365.919809639326,
-365.895563903057,-365.807011750977,-365.718574355454,-365.630227912257,
-365.538430579173,-365.450186457267,-365.361955771331,-365.273717152607,
-365.185449231759,-365.097080931118,-365.008653119957,-364.920094983854,
-364.895849247584,-364.807297095504,-364.718859699981,-364.630513256783,
-364.538715923699,-364.450471801793,-364.362241115856,-364.274002497132,
-364.185734576284,-364.097366275643,-364.008938464481,-363.920380328378,
-363.896134592111,-363.807582440031,-363.719145044508,-363.630798601311,
-363.539001268226,-363.45075714632,-363.362526460384,-363.27428784166,-363.186019920812,
-363.09765162017,-363.009223809009,-362.920665672906,-362.896419936638,
-362.807853208516,-362.719399105434,-362.631036147201,-362.542742929627,
-362.454493271629,-362.366269341606,-362.278031497364,-362.23431154943),
 .UNSPECIFIED.);
#421=B_SPLINE_CURVE_WITH_KNOTS('',3,(#63751,#63752,#63753,#63754,#63755,
#63756,#63757,#63758,#63759,#63760),.UNSPECIFIED.,.F.,.F.,(4,1,1,1,1,1,
1,4),(-362.234304141519,-361.896705281165,-360.896990625692,-359.89727597022,
-358.897561314747,-357.897846659274,-356.898132003801,-355.95112624225),
 .UNSPECIFIED.);
#422=B_SPLINE_CURVE_WITH_KNOTS('',3,(#63762,#63763,#63764,#63765,#63766,
#63767,#63768,#63769,#63770,#63771,#63772,#63773),.UNSPECIFIED.,.F.,.F.,
(4,2,1,1,1,1,1,1,4),(-355.95112624225,-355.898417348328,-354.898702692855,
-353.898988037383,-352.89927338191,-351.899558726437,-350.899844070964,
-349.900129415491,-349.667940935071),.UNSPECIFIED.);
#423=B_SPLINE_CURVE_WITH_KNOTS('',3,(#63775,#63776,#63777,#63778,#63779,
#63780,#63781,#63782,#63783,#63784),.UNSPECIFIED.,.F.,.F.,(4,1,1,1,1,1,
1,4),(-349.667940935071,-348.900414760018,-347.900700104546,-346.900985449073,
-345.9012707936,-344.901556138127,-343.901841482654,-343.384755627891),
 .UNSPECIFIED.);
#424=B_SPLINE_CURVE_WITH_KNOTS('',3,(#63786,#63787,#63788,#63789,#63790,
#63791,#63792,#63793,#63794,#63795),.UNSPECIFIED.,.F.,.F.,(4,1,1,1,1,1,
1,4),(-343.384755627891,-342.902126827181,-341.902412171709,-340.902697516236,
-339.902982860763,-338.90326820529,-337.903553549817,-337.101573810142),
 .UNSPECIFIED.);
#425=B_SPLINE_CURVE_WITH_KNOTS('',3,(#63797,#63798,#63799,#63800,#63801,
#63802,#63803,#63804,#63805,#63806,#63807,#63808,#63809,#63810,#63811,#63812,
#63813,#63814,#63815,#63816,#63817,#63818,#63819,#63820,#63821,#63822,#63823,
#63824,#63825,#63826,#63827,#63828,#63829,#63830,#63831,#63832,#63833,#63834,
#63835,#63836,#63837,#63838,#63839,#63840,#63841,#63842,#63843,#63844,#63845,
#63846,#63847,#63848,#63849,#63850,#63851,#63852,#63853,#63854,#63855,#63856,
#63857,#63858,#63859,#63860,#63861,#63862,#63863,#63864,#63865,#63866,#63867,
#63868,#63869,#63870,#63871,#63872,#63873,#63874,#63875,#63876,#63877,#63878,
#63879,#63880,#63881,#63882,#63883,#63884,#63885,#63886,#63887,#63888,#63889,
#63890,#63891,#63892,#63893,#63894,#63895,#63896,#63897,#63898,#63899,#63900,
#63901,#63902,#63903,#63904,#63905,#63906,#63907,#63908,#63909,#63910,#63911,
#63912,#63913,#63914,#63915,#63916,#63917,#63918,#63919,#63920,#63921,#63922,
#63923,#63924,#63925,#63926,#63927,#63928,#63929,#63930,#63931,#63932,#63933,
#63934,#63935,#63936,#63937,#63938,#63939,#63940,#63941,#63942,#63943,#63944,
#63945,#63946,#63947,#63948,#63949,#63950,#63951,#63952,#63953,#63954,#63955,
#63956,#63957,#63958,#63959,#63960,#63961,#63962,#63963,#63964,#63965,#63966,
#63967,#63968,#63969,#63970,#63971,#63972,#63973,#63974,#63975,#63976,#63977,
#63978,#63979,#63980,#63981,#63982,#63983,#63984,#63985,#63986,#63987,#63988,
#63989,#63990,#63991,#63992,#63993,#63994,#63995,#63996,#63997,#63998,#63999,
#64000,#64001,#64002,#64003,#64004,#64005,#64006,#64007,#64008,#64009,#64010,
#64011,#64012,#64013,#64014,#64015,#64016,#64017,#64018,#64019,#64020,#64021,
#64022),.UNSPECIFIED.,.F.,.F.,(4,3,3,3,3,3,3,3,3,3,3,3,3,3,3,3,3,3,3,3,
3,3,3,3,3,3,3,3,3,3,3,3,3,3,3,3,3,3,3,3,3,3,3,3,3,3,3,3,3,3,3,3,3,3,3,3,
3,3,3,3,3,3,3,3,3,3,3,3,3,3,3,3,3,3,3,4),(-337.101570320712,-336.973722808615,
-336.903838894344,-336.815286742266,-336.726849346744,-336.638502903547,
-336.546705570463,-336.458461448558,-336.370230762624,-336.281992143901,
-336.193724223054,-336.105355922414,-336.016928111255,-335.928369975154,
-335.904124238872,-335.815572086792,-335.727134691269,-335.63878824807,
-335.546990914986,-335.45874679308,-335.370516107144,-335.28227748842,-335.194009567571,
-335.10564126693,-335.017213455768,-334.928655319665,-334.904409583399,
-334.815857431319,-334.727420035796,-334.639073592597,-334.547276259513,
-334.459032137607,-334.370801451671,-334.282562832946,-334.194294912098,
-334.105926611456,-334.017498800295,-333.928940664192,-333.904694927926,
-333.816142775847,-333.727705380324,-333.639358937126,-333.547561604042,
-333.459317482136,-333.3710867962,-333.282848177476,-333.194580256628,-333.106211955987,
-333.017784144826,-332.929226008723,-332.904980272453,-332.816428120373,
-332.72799072485,-332.639644281652,-332.547846948568,-332.459602826662,
-332.371372140726,-332.283133522002,-332.194865601153,-332.106497300512,
-332.018069489351,-331.929511353248,-331.90526561698,-331.8167134649,-331.728276069377,
-331.639929626179,-331.548132293095,-331.459888171189,-331.371657485253,
-331.283418866529,-331.19515094568,-331.106782645039,-331.018354833878,
-330.929796697775,-330.905550961507,-330.818385013532),.UNSPECIFIED.);
#426=B_SPLINE_CURVE_WITH_KNOTS('',3,(#64024,#64025,#64026,#64027,#64028,
#64029,#64030,#64031,#64032,#64033),.UNSPECIFIED.,.F.,.F.,(4,1,1,1,1,1,
1,4),(-330.818376289941,-329.905836306035,-328.906121650562,-327.906406995089,
-326.906692339616,-325.906977684143,-324.90726302867,-324.535207379122),
 .UNSPECIFIED.);
#427=B_SPLINE_CURVE_WITH_KNOTS('',3,(#64035,#64036,#64037,#64038,#64039,
#64040,#64041,#64042,#64043,#64044,#64045,#64046,#64047,#64048,#64049,#64050,
#64051,#64052,#64053,#64054,#64055,#64056,#64057,#64058,#64059,#64060,#64061,
#64062,#64063,#64064,#64065,#64066,#64067,#64068,#64069,#64070,#64071,#64072,
#64073,#64074,#64075,#64076,#64077,#64078,#64079,#64080,#64081,#64082,#64083,
#64084,#64085,#64086,#64087,#64088,#64089,#64090,#64091,#64092,#64093,#64094,
#64095,#64096,#64097,#64098,#64099,#64100,#64101,#64102,#64103,#64104,#64105,
#64106,#64107,#64108,#64109,#64110,#64111,#64112,#64113,#64114,#64115,#64116,
#64117,#64118,#64119,#64120,#64121,#64122,#64123,#64124,#64125,#64126,#64127,
#64128,#64129,#64130,#64131,#64132,#64133,#64134,#64135,#64136,#64137,#64138,
#64139,#64140,#64141,#64142,#64143,#64144,#64145,#64146,#64147,#64148,#64149,
#64150,#64151,#64152,#64153,#64154,#64155,#64156,#64157,#64158,#64159,#64160,
#64161,#64162,#64163,#64164,#64165,#64166,#64167,#64168,#64169,#64170,#64171,
#64172,#64173,#64174,#64175,#64176,#64177,#64178,#64179,#64180,#64181,#64182,
#64183,#64184,#64185,#64186,#64187,#64188,#64189,#64190,#64191,#64192,#64193,
#64194,#64195,#64196,#64197,#64198,#64199,#64200,#64201,#64202,#64203,#64204,
#64205,#64206,#64207,#64208,#64209,#64210,#64211,#64212,#64213,#64214,#64215,
#64216,#64217,#64218,#64219,#64220,#64221,#64222,#64223,#64224,#64225,#64226,
#64227,#64228,#64229,#64230,#64231,#64232,#64233,#64234,#64235,#64236,#64237,
#64238,#64239,#64240,#64241,#64242,#64243,#64244,#64245,#64246,#64247,#64248,
#64249,#64250,#64251,#64252,#64253,#64254,#64255,#64256,#64257,#64258,#64259,
#64260),.UNSPECIFIED.,.F.,.F.,(4,3,3,3,3,3,3,3,3,3,3,3,3,3,3,3,3,3,3,3,
3,3,3,3,3,3,3,3,3,3,3,3,3,3,3,3,3,3,3,3,3,3,3,3,3,3,3,3,3,3,3,3,3,3,3,3,
3,3,3,3,3,3,3,3,3,3,3,3,3,3,3,3,3,3,3,4),(-324.535199706353,-324.446359815449,
-324.357512939538,-324.268638672611,-324.178366097758,-324.089322870752,
-323.998435621975,-323.907548373198,-323.818996221118,-323.730558825595,
-323.642212382397,-323.550415049313,-323.462170927407,-323.373940241471,
-323.285701622747,-323.197433701898,-323.109065401257,-323.020637590096,
-322.932079453993,-322.907833717725,-322.819281565645,-322.730844170122,
-322.642497726924,-322.55070039384,-322.462456271934,-322.374225585998,
-322.285986967274,-322.197719046425,-322.109350745784,-322.020922934623,
-321.93236479852,-321.908119062252,-321.819566910172,-321.731129514649,
-321.642783071451,-321.550985738367,-321.462741616461,-321.374510930525,
-321.286272311801,-321.198004390953,-321.109636090311,-321.021208279151,
-320.932650143048,-320.908404406779,-320.819852254699,-320.731414859176,
-320.643068415978,-320.551271082894,-320.463026960988,-320.374796275052,
-320.286557656327,-320.198289735479,-320.109921434838,-320.021493623676,
-319.932935487573,-319.908689751306,-319.820137599226,-319.731700203703,
-319.643353760505,-319.551556427421,-319.463312305515,-319.375081619579,
-319.286843000855,-319.198575080007,-319.110206779366,-319.021778968205,
-318.933220832102,-318.908975095833,-318.82031988714,-318.73177809888,-318.643328353439,
-318.554949349457,-318.46661619347,-318.37830974425,-318.289992754975,-318.252014399173),
 .UNSPECIFIED.);
#428=B_SPLINE_CURVE_WITH_KNOTS('',3,(#64262,#64263,#64264,#64265,#64266,
#64267,#64268,#64269,#64270,#64271,#64272,#64273,#64274,#64275,#64276,#64277,
#64278,#64279,#64280,#64281,#64282,#64283,#64284,#64285,#64286,#64287,#64288,
#64289,#64290,#64291,#64292,#64293,#64294,#64295,#64296,#64297,#64298,#64299,
#64300,#64301,#64302,#64303,#64304,#64305,#64306,#64307,#64308,#64309,#64310,
#64311,#64312,#64313,#64314,#64315,#64316,#64317,#64318,#64319,#64320,#64321,
#64322,#64323,#64324,#64325,#64326,#64327,#64328,#64329,#64330,#64331,#64332,
#64333,#64334,#64335,#64336,#64337,#64338,#64339,#64340,#64341,#64342,#64343,
#64344,#64345,#64346,#64347,#64348,#64349,#64350,#64351,#64352,#64353,#64354,
#64355,#64356,#64357,#64358,#64359,#64360,#64361,#64362,#64363,#64364,#64365,
#64366,#64367,#64368,#64369,#64370,#64371,#64372,#64373,#64374,#64375,#64376,
#64377,#64378,#64379,#64380,#64381,#64382,#64383,#64384,#64385,#64386,#64387,
#64388,#64389,#64390,#64391,#64392,#64393,#64394,#64395,#64396,#64397,#64398,
#64399,#64400,#64401,#64402,#64403,#64404,#64405,#64406,#64407,#64408,#64409,
#64410,#64411,#64412,#64413,#64414,#64415,#64416,#64417,#64418,#64419,#64420,
#64421,#64422,#64423,#64424,#64425,#64426,#64427,#64428,#64429,#64430,#64431,
#64432,#64433,#64434,#64435,#64436,#64437,#64438,#64439,#64440,#64441,#64442,
#64443,#64444,#64445,#64446,#64447,#64448,#64449,#64450,#64451,#64452,#64453,
#64454,#64455,#64456,#64457,#64458,#64459,#64460,#64461,#64462,#64463,#64464,
#64465,#64466,#64467,#64468,#64469,#64470,#64471,#64472,#64473,#64474,#64475,
#64476,#64477,#64478,#64479,#64480,#64481,#64482,#64483,#64484,#64485,#64486,
#64487),.UNSPECIFIED.,.F.,.F.,(4,3,3,3,3,3,3,3,3,3,3,3,3,3,3,3,3,3,3,3,
3,3,3,3,3,3,3,3,3,3,3,3,3,3,3,3,3,3,3,3,3,3,3,3,3,3,3,3,3,3,3,3,3,3,3,3,
3,3,3,3,3,3,3,3,3,3,3,3,3,3,3,3,3,3,3,4),(-318.252014398944,-318.150053608736,
-318.04751572947,-317.944304068901,-317.909260440361,-317.820708288281,
-317.732270892758,-317.643924449559,-317.552127116475,-317.463882994569,
-317.375652308632,-317.287413689908,-317.19914576906,-317.110777468418,
-317.022349657257,-316.933791521154,-316.909545784888,-316.820993632808,
-316.732556237285,-316.644209794087,-316.552412461003,-316.464168339097,
-316.375937653161,-316.287699034437,-316.199431113589,-316.111062812948,
-316.022635001787,-315.934076865684,-315.909831129415,-315.821278977335,
-315.732841581812,-315.644495138614,-315.55269780553,-315.464453683624,
-315.376222997688,-315.287984378964,-315.199716458116,-315.111348157475,
-315.022920346314,-314.934362210211,-314.910116473942,-314.821564321862,
-314.733126926339,-314.644780483141,-314.552983150057,-314.464739028151,
-314.376508342215,-314.288269723491,-314.200001802642,-314.111633502001,
-314.02320569084,-313.934647554737,-313.910401818469,-313.821849666389,
-313.733412270866,-313.645065827668,-313.553268494584,-313.465024372678,
-313.376793686742,-313.288555068018,-313.200287147169,-313.111918846528,
-313.023491035367,-312.934932899264,-312.910687162996,-312.822895988953,
-312.73521894255,-312.647631400734,-312.560107192341,-312.472615981098,
-312.3851356625,-312.297644145287,-312.210067236098,-312.12244558037,-312.034688551243,
-311.968829091993),.UNSPECIFIED.);
#429=B_SPLINE_CURVE_WITH_KNOTS('',3,(#64489,#64490,#64491,#64492,#64493,
#64494,#64495,#64496,#64497,#64498,#64499,#64500),.UNSPECIFIED.,.F.,.F.,
(4,2,1,1,1,1,1,1,4),(-311.968829091993,-311.910972507524,-310.911257852051,
-309.911543196578,-308.911828541105,-307.912113885632,-306.912399230159,
-305.912684574687,-305.685643784814),.UNSPECIFIED.);
#430=B_SPLINE_CURVE_WITH_KNOTS('',3,(#64502,#64503,#64504,#64505,#64506,
#64507,#64508,#64509,#64510,#64511,#64512,#64513,#64514,#64515,#64516,#64517,
#64518,#64519,#64520,#64521,#64522,#64523,#64524,#64525,#64526,#64527,#64528,
#64529,#64530,#64531,#64532,#64533,#64534,#64535,#64536,#64537,#64538,#64539,
#64540,#64541,#64542,#64543,#64544,#64545,#64546,#64547,#64548,#64549,#64550,
#64551,#64552,#64553,#64554,#64555,#64556,#64557,#64558,#64559,#64560,#64561,
#64562,#64563,#64564,#64565,#64566,#64567,#64568,#64569,#64570,#64571,#64572,
#64573,#64574,#64575,#64576,#64577,#64578,#64579,#64580,#64581,#64582,#64583,
#64584,#64585,#64586,#64587,#64588,#64589,#64590,#64591,#64592,#64593,#64594,
#64595,#64596,#64597,#64598,#64599,#64600,#64601,#64602,#64603,#64604,#64605,
#64606,#64607,#64608,#64609,#64610,#64611,#64612,#64613,#64614,#64615,#64616,
#64617,#64618,#64619,#64620,#64621,#64622,#64623,#64624,#64625,#64626,#64627,
#64628,#64629,#64630,#64631,#64632,#64633,#64634,#64635,#64636,#64637,#64638,
#64639,#64640,#64641,#64642,#64643,#64644,#64645,#64646,#64647,#64648,#64649,
#64650,#64651,#64652,#64653,#64654,#64655,#64656,#64657,#64658,#64659,#64660,
#64661,#64662,#64663,#64664,#64665,#64666,#64667,#64668,#64669,#64670,#64671,
#64672,#64673,#64674,#64675,#64676,#64677,#64678,#64679,#64680,#64681,#64682,
#64683,#64684,#64685,#64686,#64687,#64688,#64689,#64690,#64691,#64692,#64693,
#64694,#64695,#64696,#64697,#64698,#64699,#64700,#64701,#64702,#64703,#64704,
#64705,#64706,#64707,#64708,#64709,#64710,#64711,#64712,#64713,#64714,#64715,
#64716,#64717,#64718,#64719,#64720,#64721,#64722,#64723,#64724,#64725,#64726,
#64727),.UNSPECIFIED.,.F.,.F.,(4,3,3,3,3,3,3,3,3,3,3,3,3,3,3,3,3,3,3,3,
3,3,3,3,3,3,3,3,3,3,3,3,3,3,3,3,3,3,3,3,3,3,3,3,3,3,3,3,3,3,3,3,3,3,3,3,
3,3,3,3,3,3,3,3,3,3,3,3,3,3,3,3,3,3,3,4),(-305.685643784814,-305.598454037272,
-305.511330089946,-305.424240779258,-305.337163689709,-305.250076420172,
-305.162901898749,-305.075683108739,-304.988322318422,-304.912969919214,
-304.824417767134,-304.735980371611,-304.647633928413,-304.555836595329,
-304.467592473423,-304.379361787487,-304.291123168763,-304.202855247914,
-304.114486947273,-304.026059136112,-303.937501000009,-303.913255263741,
-303.824703111661,-303.736265716138,-303.64791927294,-303.556121939856,
-303.46787781795,-303.379647132014,-303.29140851329,-303.203140592442,-303.114772291801,
-303.02634448064,-302.937786344537,-302.913540608268,-302.824988456188,
-302.736551060665,-302.648204617467,-302.556407284383,-302.468163162477,
-302.379932476541,-302.291693857817,-302.203425936968,-302.115057636327,
-302.026629825166,-301.938071689063,-301.913825952795,-301.825273800715,
-301.736836405192,-301.648489961994,-301.55669262891,-301.468448507004,
-301.380217821067,-301.291979202343,-301.203711281495,-301.115342980854,
-301.026915169693,-300.93835703359,-300.914111297322,-300.825559145243,
-300.73712174972,-300.648775306523,-300.556977973439,-300.468733851533,
-300.380503165597,-300.292264546873,-300.203996626025,-300.115628325384,
-300.027200514223,-299.938642378121,-299.91439664185,-299.821768244774,
-299.72930162526,-299.637039091217,-299.54489838375,-299.45290684345,-299.402458477634),
 .UNSPECIFIED.);
#431=B_SPLINE_CURVE_WITH_KNOTS('',3,(#64729,#64730,#64731,#64732,#64733,
#64734,#64735,#64736,#64737,#64738,#64739,#64740,#64741,#64742,#64743,#64744,
#64745,#64746,#64747,#64748,#64749,#64750,#64751,#64752,#64753,#64754,#64755,
#64756,#64757,#64758,#64759,#64760,#64761,#64762,#64763,#64764,#64765,#64766,
#64767,#64768,#64769,#64770,#64771,#64772,#64773,#64774,#64775,#64776,#64777,
#64778,#64779,#64780,#64781,#64782,#64783,#64784,#64785,#64786,#64787,#64788,
#64789,#64790,#64791,#64792,#64793,#64794,#64795,#64796,#64797,#64798,#64799,
#64800,#64801,#64802,#64803,#64804,#64805,#64806,#64807,#64808,#64809,#64810,
#64811,#64812,#64813,#64814,#64815,#64816,#64817,#64818,#64819,#64820,#64821,
#64822,#64823,#64824,#64825,#64826,#64827,#64828,#64829,#64830,#64831,#64832,
#64833,#64834,#64835,#64836,#64837,#64838,#64839,#64840,#64841,#64842,#64843,
#64844,#64845,#64846,#64847,#64848,#64849,#64850,#64851,#64852,#64853,#64854,
#64855,#64856,#64857,#64858,#64859,#64860,#64861,#64862,#64863,#64864,#64865,
#64866,#64867,#64868,#64869,#64870,#64871,#64872,#64873,#64874,#64875,#64876,
#64877,#64878,#64879,#64880,#64881,#64882,#64883,#64884,#64885,#64886,#64887,
#64888,#64889,#64890,#64891,#64892,#64893,#64894,#64895,#64896,#64897,#64898,
#64899,#64900,#64901,#64902,#64903,#64904,#64905,#64906,#64907,#64908,#64909,
#64910,#64911,#64912,#64913,#64914,#64915,#64916,#64917,#64918,#64919,#64920,
#64921,#64922,#64923,#64924,#64925,#64926,#64927,#64928,#64929,#64930,#64931,
#64932,#64933,#64934,#64935,#64936,#64937,#64938,#64939,#64940,#64941,#64942,
#64943,#64944,#64945,#64946,#64947,#64948,#64949,#64950,#64951,#64952,#64953,
#64954),.UNSPECIFIED.,.F.,.F.,(4,3,3,3,3,3,3,3,3,3,3,3,3,3,3,3,3,3,3,3,
3,3,3,3,3,3,3,3,3,3,3,3,3,3,3,3,3,3,3,3,3,3,3,3,3,3,3,3,3,3,3,3,3,3,3,3,
3,3,3,3,3,3,3,3,3,3,3,3,3,3,3,3,3,3,3,4),(-299.402458477502,-299.309553527439,
-299.216500663027,-299.123205464595,-299.029774917432,-298.936131896398,
-298.914681986377,-298.826129834297,-298.737692438774,-298.649345995575,
-298.557548662491,-298.469304540585,-298.381073854649,-298.292835235925,
-298.204567315076,-298.116199014434,-298.027771203273,-297.93921306717,
-297.914967330904,-297.826415178824,-297.737977783301,-297.649631340103,
-297.557834007019,-297.469589885113,-297.381359199177,-297.293120580453,
-297.204852659604,-297.116484358963,-297.028056547802,-296.939498411699,
-296.915252675431,-296.826700523351,-296.738263127828,-296.64991668463,
-296.558119351546,-296.46987522964,-296.381644543704,-296.29340592498,-296.205138004132,
-296.116769703491,-296.02834189233,-295.939783756227,-295.915538019958,
-295.826985867878,-295.738548472355,-295.650202029157,-295.558404696073,
-295.470160574166,-295.38192988823,-295.293691269506,-295.205423348658,
-295.117055048016,-295.028627236855,-294.940069100752,-294.915823364485,
-294.827271212406,-294.738833816883,-294.650487373685,-294.558690040601,
-294.470445918695,-294.382215232759,-294.293976614035,-294.205708693187,
-294.117340392546,-294.028912581385,-293.940354445283,-293.916108709013,
-293.828823892562,-293.740130052298,-293.65306297726,-293.566051538638,
-293.479073216952,-293.389123205328,-293.30211266917,-293.210692919813,
-293.119273170455),.UNSPECIFIED.);
#432=B_SPLINE_CURVE_WITH_KNOTS('',3,(#64956,#64957,#64958,#64959,#64960,
#64961,#64962,#64963,#64964,#64965,#64966),.UNSPECIFIED.,.F.,.F.,(4,1,1,
1,1,1,1,1,4),(-293.119273170455,-292.91639405354,-291.916679398067,-290.916964742594,
-289.917250087121,-288.917535431648,-287.917820776176,-286.918106120703,
-286.836087863275),.UNSPECIFIED.);
#433=B_SPLINE_CURVE_WITH_KNOTS('',3,(#64968,#64969,#64970,#64971,#64972,
#64973,#64974,#64975,#64976,#64977),.UNSPECIFIED.,.F.,.F.,(4,1,1,1,1,1,
1,4),(-286.836087863275,-285.91839146523,-284.918676809757,-283.918962154284,
-282.919247498811,-281.919532843339,-280.919818187866,-280.552902556096),
 .UNSPECIFIED.);
#434=B_SPLINE_CURVE_WITH_KNOTS('',3,(#64979,#64980,#64981,#64982,#64983,
#64984,#64985,#64986,#64987,#64988),.UNSPECIFIED.,.F.,.F.,(4,1,1,1,1,1,
1,4),(-280.552902556096,-279.920103532393,-278.92038887692,-277.920674221447,
-276.920959565974,-275.921244910502,-274.921530255029,-274.269717248916),
 .UNSPECIFIED.);
#435=B_SPLINE_CURVE_WITH_KNOTS('',3,(#64990,#64991,#64992,#64993,#64994,
#64995,#64996,#64997,#64998,#64999,#65000,#65001,#65002,#65003,#65004,#65005,
#65006,#65007,#65008,#65009,#65010,#65011,#65012,#65013,#65014,#65015,#65016,
#65017,#65018,#65019,#65020,#65021,#65022,#65023,#65024,#65025,#65026,#65027,
#65028,#65029,#65030,#65031,#65032,#65033,#65034,#65035,#65036,#65037,#65038,
#65039,#65040,#65041,#65042,#65043,#65044,#65045,#65046,#65047,#65048,#65049,
#65050,#65051,#65052,#65053,#65054,#65055,#65056,#65057,#65058,#65059,#65060,
#65061,#65062,#65063,#65064,#65065,#65066,#65067,#65068,#65069,#65070,#65071,
#65072,#65073,#65074,#65075,#65076,#65077,#65078,#65079,#65080,#65081,#65082,
#65083,#65084,#65085,#65086,#65087,#65088,#65089,#65090,#65091,#65092,#65093,
#65094,#65095,#65096,#65097,#65098,#65099,#65100,#65101,#65102,#65103,#65104,
#65105,#65106,#65107,#65108,#65109,#65110,#65111,#65112,#65113,#65114,#65115,
#65116,#65117,#65118,#65119,#65120,#65121,#65122,#65123,#65124,#65125,#65126,
#65127,#65128,#65129,#65130,#65131,#65132,#65133,#65134,#65135,#65136,#65137,
#65138,#65139,#65140,#65141,#65142,#65143,#65144,#65145,#65146,#65147,#65148,
#65149,#65150,#65151,#65152,#65153,#65154,#65155,#65156,#65157,#65158,#65159,
#65160,#65161,#65162,#65163,#65164,#65165,#65166,#65167,#65168,#65169,#65170,
#65171,#65172,#65173,#65174,#65175,#65176,#65177,#65178,#65179,#65180,#65181,
#65182,#65183,#65184,#65185,#65186,#65187,#65188,#65189,#65190,#65191,#65192,
#65193,#65194,#65195,#65196,#65197,#65198,#65199,#65200,#65201,#65202,#65203,
#65204,#65205,#65206,#65207,#65208,#65209,#65210,#65211,#65212,#65213,#65214,
#65215),.UNSPECIFIED.,.F.,.F.,(4,3,3,3,3,3,3,3,3,3,3,3,3,3,3,3,3,3,3,3,
3,3,3,3,3,3,3,3,3,3,3,3,3,3,3,3,3,3,3,3,3,3,3,3,3,3,3,3,3,3,3,3,3,3,3,3,
3,3,3,3,3,3,3,3,3,3,3,3,3,3,3,3,3,3,3,4),(-274.269717004602,-274.168208143946,
-274.066155437434,-273.963451878141,-273.921815599556,-273.833263447476,
-273.744826051953,-273.656479608755,-273.564682275671,-273.476438153764,
-273.388207467828,-273.299968849104,-273.211700928256,-273.123332627614,
-273.034904816453,-272.94634668035,-272.922100944083,-272.833548792003,
-272.74511139648,-272.656764953282,-272.564967620198,-272.476723498292,
-272.388492812356,-272.300254193632,-272.211986272784,-272.123617972142,
-272.035190160981,-271.946632024879,-271.92238628861,-271.83383413653,-271.745396741007,
-271.657050297809,-271.565252964725,-271.477008842819,-271.388778156882,
-271.300539538159,-271.21227161731,-271.123903316669,-271.035475505508,
-270.946917369405,-270.922671633137,-270.834119481058,-270.745682085535,
-270.657335642337,-270.565538309253,-270.477294187347,-270.389063501411,
-270.300824882687,-270.212556961839,-270.124188661198,-270.035760850037,
-269.947202713935,-269.922956977665,-269.834404825585,-269.745967430062,
-269.657620986864,-269.56582365378,-269.477579531874,-269.389348845938,
-269.301110227215,-269.212842306366,-269.124474005725,-269.036046194564,
-268.947488058461,-268.923242322192,-268.835502740503,-268.747877234083,
-268.660341131574,-268.572868278738,-268.485428267421,-268.397998951407,
-268.310558197594,-268.223032677745,-268.135462093365,-268.047758426598,
-267.986531941736),.UNSPECIFIED.);
#436=B_SPLINE_CURVE_WITH_KNOTS('',3,(#65217,#65218,#65219,#65220,#65221,
#65222,#65223,#65224,#65225,#65226,#65227,#65228),.UNSPECIFIED.,.F.,.F.,
(4,2,1,1,1,1,1,1,4),(-267.986531941736,-267.923527666719,-266.923813011246,
-265.924098355773,-264.9243837003,-263.924669044828,-262.924954389355,-261.925239733882,
-261.703346634557),.UNSPECIFIED.);
#437=B_SPLINE_CURVE_WITH_KNOTS('',3,(#65230,#65231,#65232,#65233,#65234,
#65235,#65236,#65237,#65238,#65239,#65240,#65241,#65242,#65243,#65244,#65245,
#65246,#65247,#65248,#65249,#65250,#65251,#65252,#65253,#65254,#65255,#65256,
#65257,#65258,#65259,#65260,#65261,#65262,#65263,#65264,#65265,#65266,#65267,
#65268,#65269,#65270,#65271,#65272,#65273,#65274,#65275,#65276,#65277,#65278,
#65279,#65280,#65281,#65282,#65283,#65284,#65285,#65286,#65287,#65288,#65289,
#65290,#65291,#65292,#65293,#65294,#65295,#65296,#65297,#65298,#65299,#65300,
#65301,#65302,#65303,#65304,#65305,#65306,#65307,#65308,#65309,#65310,#65311,
#65312,#65313,#65314,#65315,#65316,#65317,#65318,#65319,#65320,#65321,#65322,
#65323,#65324,#65325,#65326,#65327,#65328,#65329,#65330,#65331,#65332,#65333,
#65334,#65335,#65336,#65337,#65338,#65339,#65340,#65341,#65342,#65343,#65344,
#65345,#65346,#65347,#65348,#65349,#65350,#65351,#65352,#65353,#65354,#65355,
#65356,#65357,#65358,#65359,#65360,#65361,#65362,#65363,#65364,#65365,#65366,
#65367,#65368,#65369,#65370,#65371,#65372,#65373,#65374,#65375,#65376,#65377,
#65378,#65379,#65380,#65381,#65382,#65383,#65384,#65385,#65386,#65387,#65388,
#65389,#65390,#65391,#65392,#65393,#65394,#65395,#65396,#65397,#65398,#65399,
#65400,#65401,#65402,#65403,#65404,#65405,#65406,#65407,#65408,#65409,#65410,
#65411,#65412,#65413,#65414,#65415,#65416,#65417,#65418,#65419,#65420,#65421,
#65422,#65423,#65424,#65425,#65426,#65427,#65428,#65429,#65430,#65431,#65432,
#65433,#65434,#65435,#65436,#65437,#65438,#65439,#65440,#65441,#65442,#65443,
#65444,#65445,#65446,#65447,#65448,#65449,#65450,#65451,#65452,#65453,#65454,
#65455),.UNSPECIFIED.,.F.,.F.,(4,3,3,3,3,3,3,3,3,3,3,3,3,3,3,3,3,3,3,3,
3,3,3,3,3,3,3,3,3,3,3,3,3,3,3,3,3,3,3,3,3,3,3,3,3,3,3,3,3,3,3,3,3,3,3,3,
3,3,3,3,3,3,3,3,3,3,3,3,3,3,3,3,3,3,3,4),(-261.703346634557,-261.616176758673,
-261.529075180752,-261.442009868448,-261.35495838563,-261.267898311999,
-261.180752041239,-261.093562892726,-261.006230334554,-260.925525078409,
-260.836972926329,-260.748535530806,-260.660189087608,-260.568391754524,
-260.480147632618,-260.391916946682,-260.303678327958,-260.21541040711,
-260.127042106468,-260.038614295307,-259.950056159204,-259.925810422936,
-259.837258270856,-259.748820875333,-259.660474432135,-259.568677099051,
-259.480432977145,-259.392202291209,-259.303963672485,-259.215695751636,
-259.127327450994,-259.038899639833,-258.95034150373,-258.926095767463,
-258.837543615383,-258.749106219861,-258.660759776663,-258.568962443579,
-258.480718321673,-258.392487635737,-258.304249017013,-258.215981096165,
-258.127612795524,-258.039184984363,-257.950626848261,-257.926381111991,
-257.837828959912,-257.749391564388,-257.66104512119,-257.569247788106,
-257.4810036662,-257.392772980264,-257.30453436154,-257.216266440692,-257.127898140051,
-257.03947032889,-256.950912192787,-256.926666456518,-256.838114304438,
-256.749676908915,-256.661330465717,-256.569533132633,-256.481289010727,
-256.393058324791,-256.304819706067,-256.216551785218,-256.128183484577,
-256.039755673416,-255.951197537313,-255.926951801045,-255.834118795862,
-255.741450830476,-255.648992944735,-255.556661144641,-255.46448525518,
-255.420161327377),.UNSPECIFIED.);
#438=B_SPLINE_CURVE_WITH_KNOTS('',3,(#65457,#65458,#65459,#65460,#65461,
#65462,#65463,#65464,#65465,#65466,#65467,#65468,#65469,#65470,#65471,#65472,
#65473,#65474,#65475,#65476,#65477,#65478,#65479,#65480,#65481,#65482,#65483,
#65484,#65485,#65486,#65487,#65488,#65489,#65490,#65491,#65492,#65493,#65494,
#65495,#65496,#65497,#65498,#65499,#65500,#65501,#65502,#65503,#65504,#65505,
#65506,#65507,#65508,#65509,#65510,#65511,#65512,#65513,#65514,#65515,#65516,
#65517,#65518,#65519,#65520,#65521,#65522,#65523,#65524,#65525,#65526,#65527,
#65528,#65529,#65530,#65531,#65532,#65533,#65534,#65535,#65536,#65537,#65538,
#65539,#65540,#65541,#65542,#65543,#65544,#65545,#65546,#65547,#65548,#65549,
#65550,#65551,#65552,#65553,#65554,#65555,#65556,#65557,#65558,#65559,#65560,
#65561,#65562,#65563,#65564,#65565,#65566,#65567,#65568,#65569,#65570,#65571,
#65572,#65573,#65574,#65575,#65576,#65577,#65578,#65579,#65580,#65581,#65582,
#65583,#65584,#65585,#65586,#65587,#65588,#65589,#65590,#65591,#65592,#65593,
#65594,#65595,#65596,#65597,#65598,#65599,#65600,#65601,#65602,#65603,#65604,
#65605,#65606,#65607,#65608,#65609,#65610,#65611,#65612,#65613,#65614,#65615,
#65616,#65617,#65618,#65619,#65620,#65621,#65622,#65623,#65624,#65625,#65626,
#65627,#65628,#65629,#65630,#65631,#65632,#65633,#65634,#65635,#65636,#65637,
#65638,#65639,#65640,#65641,#65642,#65643,#65644,#65645,#65646,#65647,#65648,
#65649,#65650,#65651,#65652,#65653,#65654,#65655,#65656,#65657,#65658,#65659,
#65660,#65661,#65662,#65663,#65664,#65665,#65666,#65667,#65668,#65669,#65670,
#65671,#65672,#65673,#65674,#65675,#65676,#65677,#65678,#65679,#65680,#65681,
#65682),.UNSPECIFIED.,.F.,.F.,(4,3,3,3,3,3,3,3,3,3,3,3,3,3,3,3,3,3,3,3,
3,3,3,3,3,3,3,3,3,3,3,3,3,3,3,3,3,3,3,3,3,3,3,3,3,3,3,3,3,3,3,3,3,3,3,3,
3,3,3,3,3,3,3,3,3,3,3,3,3,3,3,3,3,3,3,4),(-255.420161327226,-255.327463107471,
-255.234625308542,-255.141553107975,-255.048350781773,-254.954937477772,
-254.927237145572,-254.838684993492,-254.750247597969,-254.661901154771,
-254.570103821687,-254.48185969978,-254.393629013844,-254.30539039512,-254.217122474272,
-254.12875417363,-254.040326362469,-253.951768226366,-253.927522490099,
-253.838970338019,-253.750532942496,-253.662186499298,-253.570389166214,
-253.482145044308,-253.393914358371,-253.305675739647,-253.217407818799,
-253.129039518158,-253.040611706997,-252.952053570894,-252.927807834626,
-252.839255682547,-252.750818287024,-252.662471843826,-252.570674510742,
-252.482430388836,-252.3941997029,-252.305961084176,-252.217693163328,-252.129324862687,
-252.040897051527,-251.952338915424,-251.928093179154,-251.839541027074,
-251.751103631551,-251.662757188353,-251.570959855269,-251.482715733363,
-251.394485047427,-251.306246428703,-251.217978507855,-251.129610207213,
-251.041182396052,-250.95262425995,-250.928378523681,-250.839826371601,
-250.751388976078,-250.66304253288,-250.571245199796,-250.483001077889,
-250.394770391953,-250.306531773229,-250.218263852381,-250.129895551739,
-250.041467740578,-249.952909604475,-249.928663868208,-249.841361323148,
-249.753313160279,-249.666228402379,-249.579199673663,-249.492204465771,
-249.403397354378,-249.316372070933,-249.226674045566,-249.136976020198),
 .UNSPECIFIED.);
#439=B_SPLINE_CURVE_WITH_KNOTS('',3,(#65684,#65685,#65686,#65687,#65688,
#65689,#65690,#65691,#65692,#65693,#65694),.UNSPECIFIED.,.F.,.F.,(4,1,1,
1,1,1,1,1,4),(-249.136976020198,-248.928949212735,-247.929234557262,-246.92951990179,
-245.929805246317,-244.930090590844,-243.930375935371,-242.930661279898,
-242.853790713018),.UNSPECIFIED.);
#440=B_SPLINE_CURVE_WITH_KNOTS('',3,(#65696,#65697,#65698,#65699,#65700,
#65701,#65702,#65703,#65704,#65705),.UNSPECIFIED.,.F.,.F.,(4,1,1,1,1,1,
1,4),(-242.853790713018,-241.930946624425,-240.931231968953,-239.93151731348,
-238.931802658007,-237.932088002534,-236.932373347061,-236.570605405839),
 .UNSPECIFIED.);
#441=B_SPLINE_CURVE_WITH_KNOTS('',3,(#65707,#65708,#65709,#65710,#65711,
#65712,#65713,#65714,#65715,#65716),.UNSPECIFIED.,.F.,.F.,(4,1,1,1,1,1,
1,4),(-236.570605405839,-235.932658691588,-234.932944036115,-233.933229380643,
-232.93351472517,-231.933800069697,-230.934085414224,-230.287420098659),
 .UNSPECIFIED.);
#442=B_SPLINE_CURVE_WITH_KNOTS('',3,(#65718,#65719,#65720,#65721,#65722,
#65723,#65724,#65725,#65726,#65727,#65728,#65729,#65730,#65731,#65732,#65733,
#65734,#65735,#65736,#65737,#65738,#65739,#65740,#65741,#65742,#65743,#65744,
#65745,#65746,#65747,#65748,#65749,#65750,#65751,#65752,#65753,#65754,#65755,
#65756,#65757,#65758,#65759,#65760,#65761,#65762,#65763,#65764,#65765,#65766,
#65767,#65768,#65769,#65770,#65771,#65772,#65773,#65774,#65775,#65776,#65777,
#65778,#65779,#65780,#65781,#65782,#65783,#65784,#65785,#65786,#65787,#65788,
#65789,#65790,#65791,#65792,#65793,#65794,#65795,#65796,#65797,#65798,#65799,
#65800,#65801,#65802,#65803,#65804,#65805,#65806,#65807,#65808,#65809,#65810,
#65811,#65812,#65813,#65814,#65815,#65816,#65817,#65818,#65819,#65820,#65821,
#65822,#65823,#65824,#65825,#65826,#65827,#65828,#65829,#65830,#65831,#65832,
#65833,#65834,#65835,#65836,#65837,#65838,#65839,#65840,#65841,#65842,#65843,
#65844,#65845,#65846,#65847,#65848,#65849,#65850,#65851,#65852,#65853,#65854,
#65855,#65856,#65857,#65858,#65859,#65860,#65861,#65862,#65863,#65864,#65865,
#65866,#65867,#65868,#65869,#65870,#65871,#65872,#65873,#65874,#65875,#65876,
#65877,#65878,#65879,#65880,#65881,#65882,#65883,#65884,#65885,#65886,#65887,
#65888,#65889,#65890,#65891,#65892,#65893,#65894,#65895,#65896,#65897,#65898,
#65899,#65900,#65901,#65902,#65903,#65904,#65905,#65906,#65907,#65908,#65909,
#65910,#65911,#65912,#65913,#65914,#65915,#65916,#65917,#65918,#65919,#65920,
#65921,#65922,#65923,#65924,#65925,#65926,#65927,#65928,#65929,#65930,#65931,
#65932,#65933,#65934,#65935,#65936,#65937,#65938,#65939,#65940,#65941,#65942,
#65943),.UNSPECIFIED.,.F.,.F.,(4,3,3,3,3,3,3,3,3,3,3,3,3,3,3,3,3,3,3,3,
3,3,3,3,3,3,3,3,3,3,3,3,3,3,3,3,3,3,3,3,3,3,3,3,3,3,3,3,3,3,3,3,3,3,3,3,
3,3,3,3,3,3,3,3,3,3,3,3,3,3,3,3,3,3,3,4),(-230.287419852317,-230.186349361613,
-230.084766015855,-229.982553557715,-229.934370758751,-229.845818606672,
-229.757381211149,-229.669034767952,-229.577237434868,-229.488993312962,
-229.400762627027,-229.312524008303,-229.224256087456,-229.135887786815,
-229.047459975654,-228.958901839552,-228.934656103279,-228.846103951199,
-228.757666555676,-228.669320112478,-228.577522779394,-228.489278657488,
-228.401047971552,-228.312809352828,-228.224541431979,-228.136173131338,
-228.047745320177,-227.959187184074,-227.934941447806,-227.846389295726,
-227.757951900203,-227.669605457005,-227.577808123921,-227.489564002014,
-227.401333316078,-227.313094697354,-227.224826776505,-227.136458475864,
-227.048030664703,-226.9594725286,-226.935226792333,-226.846674640253,-226.75823724473,
-226.669890801532,-226.578093468448,-226.489849346542,-226.401618660606,
-226.313380041883,-226.225112121034,-226.136743820393,-226.048316009232,
-225.959757873129,-225.93551213686,-225.84695998478,-225.758522589257,-225.670176146059,
-225.578378812975,-225.490134691069,-225.401904005132,-225.313665386408,
-225.22539746556,-225.137029164918,-225.048601353757,-224.960043217654,
-224.935797481387,-224.848106940113,-224.760530424475,-224.673043217952,
-224.585619196174,-224.498227872774,-224.410847062648,-224.323454593684,
-224.235978024256,-224.148456092247,-224.060803396832,-224.00423479148),
 .UNSPECIFIED.);
#443=B_SPLINE_CURVE_WITH_KNOTS('',3,(#65945,#65946,#65947,#65948,#65949,
#65950,#65951,#65952,#65953,#65954,#65955,#65956),.UNSPECIFIED.,.F.,.F.,
(4,2,1,1,1,1,1,1,4),(-224.00423479148,-223.936082825914,-222.936368170442,
-221.936653514969,-220.936938859496,-219.937224204023,-218.93750954855,
-217.937794893077,-217.7210494843),.UNSPECIFIED.);
#444=B_SPLINE_CURVE_WITH_KNOTS('',3,(#65958,#65959,#65960,#65961,#65962,
#65963,#65964,#65965,#65966,#65967),.UNSPECIFIED.,.F.,.F.,(4,1,1,1,1,1,
1,4),(-217.7210494843,-216.938080237605,-215.938365582132,-214.938650926659,
-213.938936271186,-212.939221615713,-211.93950696024,-211.43786417712),
 .UNSPECIFIED.);
#445=B_SPLINE_CURVE_WITH_KNOTS('',3,(#65969,#65970,#65971,#65972,#65973,
#65974,#65975,#65976,#65977,#65978),.UNSPECIFIED.,.F.,.F.,(4,1,1,1,1,1,
1,4),(-211.43786417712,-210.939792304768,-209.940077649295,-208.940362993822,
-207.940648338349,-206.940933682876,-205.941219027403,-205.154678869941),
 .UNSPECIFIED.);
#446=B_SPLINE_CURVE_WITH_KNOTS('',3,(#65980,#65981,#65982,#65983,#65984,
#65985,#65986,#65987,#65988,#65989,#65990),.UNSPECIFIED.,.F.,.F.,(4,1,1,
1,1,1,1,1,4),(-205.154678869941,-204.941504371931,-203.941789716458,-202.942075060985,
-201.942360405512,-200.942645750039,-199.942931094566,-198.943216439094,
-198.871493562761),.UNSPECIFIED.);
#447=B_SPLINE_CURVE_WITH_KNOTS('',3,(#65992,#65993,#65994,#65995,#65996,
#65997,#65998,#65999,#66000,#66001,#66002,#66003,#66004,#66005,#66006,#66007,
#66008,#66009,#66010,#66011,#66012,#66013,#66014,#66015,#66016,#66017,#66018,
#66019,#66020,#66021,#66022,#66023,#66024,#66025,#66026,#66027,#66028,#66029,
#66030,#66031,#66032,#66033,#66034,#66035,#66036,#66037,#66038,#66039,#66040,
#66041,#66042,#66043,#66044,#66045,#66046,#66047,#66048,#66049,#66050,#66051,
#66052,#66053,#66054,#66055,#66056,#66057,#66058,#66059,#66060,#66061,#66062,
#66063,#66064,#66065,#66066,#66067,#66068,#66069,#66070,#66071,#66072,#66073,
#66074,#66075,#66076,#66077,#66078,#66079,#66080,#66081,#66082,#66083,#66084,
#66085,#66086,#66087,#66088,#66089,#66090,#66091,#66092,#66093,#66094,#66095,
#66096,#66097,#66098,#66099,#66100,#66101,#66102,#66103,#66104,#66105,#66106,
#66107,#66108,#66109,#66110,#66111,#66112,#66113,#66114,#66115,#66116,#66117,
#66118,#66119,#66120,#66121,#66122,#66123,#66124,#66125,#66126,#66127,#66128,
#66129,#66130,#66131,#66132,#66133,#66134,#66135,#66136,#66137,#66138,#66139,
#66140,#66141,#66142,#66143,#66144,#66145,#66146,#66147,#66148,#66149,#66150,
#66151,#66152,#66153,#66154,#66155,#66156,#66157,#66158,#66159,#66160,#66161,
#66162,#66163,#66164,#66165,#66166,#66167,#66168,#66169,#66170,#66171,#66172,
#66173,#66174,#66175,#66176,#66177,#66178,#66179,#66180,#66181,#66182,#66183,
#66184,#66185,#66186,#66187,#66188,#66189,#66190,#66191,#66192,#66193,#66194,
#66195,#66196,#66197,#66198,#66199,#66200,#66201,#66202,#66203,#66204,#66205,
#66206,#66207,#66208,#66209,#66210,#66211,#66212,#66213,#66214,#66215,#66216,
#66217),.UNSPECIFIED.,.F.,.F.,(4,3,3,3,3,3,3,3,3,3,3,3,3,3,3,3,3,3,3,3,
3,3,3,3,3,3,3,3,3,3,3,3,3,3,3,3,3,3,3,3,3,3,3,3,3,3,3,3,3,3,3,3,3,3,3,3,
3,3,3,3,3,3,3,3,3,3,3,3,3,3,3,3,3,3,3,4),(-198.871493562761,-198.783864600819,
-198.696343722576,-198.608906209389,-198.521523012626,-198.434166966534,
-198.346815865093,-198.259447510499,-198.171987253728,-198.084476748613,
-197.996829867738,-197.943501783621,-197.854949631541,-197.766512236018,
-197.67816579282,-197.586368459736,-197.49812433783,-197.409893651894,-197.32165503317,
-197.233387112322,-197.145018811681,-197.05659100052,-196.968032864417,
-196.943787128148,-196.855234976068,-196.766797580545,-196.678451137347,
-196.586653804263,-196.498409682357,-196.410178996421,-196.321940377697,
-196.233672456848,-196.145304156207,-196.056876345046,-195.968318208943,
-195.944072472675,-195.855520320595,-195.767082925072,-195.678736481874,
-195.58693914879,-195.498695026884,-195.410464340948,-195.322225722224,
-195.233957801376,-195.145589500735,-195.057161689573,-194.968603553471,
-194.944357817202,-194.855805665122,-194.767368269599,-194.679021826401,
-194.587224493317,-194.498980371411,-194.410749685474,-194.32251106675,
-194.234243145902,-194.14587484526,-194.057447034099,-193.968888897996,
-193.944643161729,-193.856091009649,-193.767653614126,-193.679307170928,
-193.587509837844,-193.499265715939,-193.411035030003,-193.322796411279,
-193.234528490431,-193.14616018979,-193.057732378629,-192.969174242526,
-192.944928506257,-192.843104874923,-192.741682446818,-192.640994115083,
-192.588308503375),.UNSPECIFIED.);
#448=B_SPLINE_CURVE_WITH_KNOTS('',3,(#66219,#66220,#66221,#66222,#66223,
#66224,#66225,#66226,#66227,#66228),.UNSPECIFIED.,.F.,.F.,(4,1,1,1,1,1,
1,4),(-192.588308255582,-191.945213850784,-190.945499195311,-189.945784539838,
-188.946069884365,-187.946355228892,-186.94664057342,-186.305122948402),
 .UNSPECIFIED.);
#449=B_SPLINE_CURVE_WITH_KNOTS('',3,(#66230,#66231,#66232,#66233,#66234,
#66235,#66236,#66237,#66238,#66239,#66240,#66241,#66242,#66243,#66244,#66245,
#66246,#66247,#66248,#66249,#66250,#66251,#66252,#66253,#66254,#66255,#66256,
#66257,#66258,#66259,#66260,#66261,#66262,#66263,#66264,#66265,#66266,#66267,
#66268,#66269,#66270,#66271,#66272,#66273,#66274,#66275,#66276,#66277,#66278,
#66279,#66280,#66281,#66282,#66283,#66284,#66285,#66286,#66287,#66288,#66289,
#66290,#66291,#66292,#66293,#66294,#66295,#66296,#66297,#66298,#66299,#66300,
#66301,#66302,#66303,#66304,#66305,#66306,#66307,#66308,#66309,#66310,#66311,
#66312,#66313,#66314,#66315,#66316,#66317,#66318,#66319,#66320,#66321,#66322,
#66323,#66324,#66325,#66326,#66327,#66328,#66329,#66330,#66331,#66332,#66333,
#66334,#66335,#66336,#66337,#66338,#66339,#66340,#66341,#66342,#66343,#66344,
#66345,#66346,#66347,#66348,#66349,#66350,#66351,#66352,#66353,#66354,#66355,
#66356,#66357,#66358,#66359,#66360,#66361,#66362,#66363,#66364,#66365,#66366,
#66367,#66368,#66369,#66370,#66371,#66372,#66373,#66374,#66375,#66376,#66377,
#66378,#66379,#66380,#66381,#66382,#66383,#66384,#66385,#66386,#66387,#66388,
#66389,#66390,#66391,#66392,#66393,#66394,#66395,#66396,#66397,#66398,#66399,
#66400,#66401,#66402,#66403,#66404,#66405,#66406,#66407,#66408,#66409,#66410,
#66411,#66412,#66413,#66414,#66415,#66416,#66417,#66418,#66419,#66420,#66421,
#66422,#66423,#66424,#66425,#66426,#66427,#66428,#66429,#66430,#66431,#66432,
#66433,#66434,#66435,#66436,#66437,#66438,#66439,#66440,#66441,#66442,#66443,
#66444,#66445,#66446,#66447,#66448,#66449,#66450,#66451,#66452,#66453,#66454,
#66455),.UNSPECIFIED.,.F.,.F.,(4,3,3,3,3,3,3,3,3,3,3,3,3,3,3,3,3,3,3,3,
3,3,3,3,3,3,3,3,3,3,3,3,3,3,3,3,3,3,3,3,3,3,3,3,3,3,3,3,3,3,3,3,3,3,3,3,
3,3,3,3,3,3,3,3,3,3,3,3,3,3,3,3,3,3,3,4),(-186.305122700355,-186.204477591045,
-186.103348556496,-186.0016110299,-185.946925917947,-185.858373765867,-185.769936370344,
-185.681589927145,-185.589792594061,-185.501548472155,-185.413317786219,
-185.325079167494,-185.236811246646,-185.148442946004,-185.060015134843,
-184.97145699874,-184.947211262474,-184.858659110394,-184.770221714871,
-184.681875271673,-184.590077938589,-184.501833816683,-184.413603130747,
-184.325364512023,-184.237096591174,-184.148728290533,-184.060300479372,
-183.971742343269,-183.947496607001,-183.858944454921,-183.770507059398,
-183.6821606162,-183.590363283116,-183.50211916121,-183.413888475274,-183.32564985655,
-183.237381935702,-183.149013635061,-183.0605858239,-182.972027687797,-182.947781951528,
-182.859229799448,-182.770792403925,-182.682445960727,-182.590648627643,
-182.502404505736,-182.4141738198,-182.325935201076,-182.237667280228,-182.149298979586,
-182.060871168425,-181.972313032322,-181.948067296055,-181.859515143976,
-181.771077748453,-181.682731305255,-181.590933972171,-181.502689850265,
-181.414459164329,-181.326220545605,-181.237952624757,-181.149584324116,
-181.061156512955,-180.972598376852,-180.948352640583,-180.860708602494,
-180.773178543556,-180.685737705076,-180.598360004986,-180.511014872504,
-180.42368008632,-180.336333438008,-180.248903392421,-180.161427705554,
-180.073823597944,-180.021937641223),.UNSPECIFIED.);
#450=B_SPLINE_CURVE_WITH_KNOTS('',3,(#66457,#66458,#66459,#66460,#66461,
#66462,#66463,#66464,#66465,#66466,#66467),.UNSPECIFIED.,.F.,.F.,(4,1,1,
1,1,1,1,1,4),(-180.021937641223,-179.94863798511,-178.948923329637,-177.949208674164,
-176.949494018691,-175.949779363218,-174.950064707746,-173.950350052273,
-173.738752334043),.UNSPECIFIED.);
#451=B_SPLINE_CURVE_WITH_KNOTS('',3,(#66469,#66470,#66471,#66472,#66473,
#66474,#66475,#66476,#66477,#66478,#66479,#66480,#66481,#66482,#66483,#66484,
#66485,#66486,#66487,#66488,#66489,#66490,#66491,#66492,#66493,#66494,#66495,
#66496,#66497,#66498,#66499,#66500,#66501,#66502,#66503,#66504,#66505,#66506,
#66507,#66508,#66509,#66510,#66511,#66512,#66513,#66514,#66515,#66516,#66517,
#66518,#66519,#66520,#66521,#66522,#66523,#66524,#66525,#66526,#66527,#66528,
#66529,#66530,#66531,#66532,#66533,#66534,#66535,#66536,#66537,#66538,#66539,
#66540,#66541,#66542,#66543,#66544,#66545,#66546,#66547,#66548,#66549,#66550,
#66551,#66552,#66553,#66554,#66555,#66556,#66557,#66558,#66559,#66560,#66561,
#66562,#66563,#66564,#66565,#66566,#66567,#66568,#66569,#66570,#66571,#66572,
#66573,#66574,#66575,#66576,#66577,#66578,#66579,#66580,#66581,#66582,#66583,
#66584,#66585,#66586,#66587,#66588,#66589,#66590,#66591,#66592,#66593,#66594,
#66595,#66596,#66597,#66598,#66599,#66600,#66601,#66602,#66603,#66604,#66605,
#66606,#66607,#66608,#66609,#66610,#66611,#66612,#66613,#66614,#66615,#66616,
#66617,#66618,#66619,#66620,#66621,#66622,#66623,#66624,#66625,#66626,#66627,
#66628,#66629,#66630,#66631,#66632,#66633,#66634,#66635,#66636,#66637,#66638,
#66639,#66640,#66641,#66642,#66643,#66644,#66645,#66646,#66647,#66648,#66649,
#66650,#66651,#66652,#66653,#66654,#66655,#66656,#66657,#66658,#66659,#66660,
#66661,#66662,#66663,#66664,#66665,#66666,#66667,#66668,#66669,#66670,#66671,
#66672,#66673,#66674,#66675,#66676,#66677,#66678,#66679,#66680,#66681,#66682,
#66683,#66684,#66685,#66686,#66687,#66688,#66689,#66690,#66691,#66692,#66693,
#66694),.UNSPECIFIED.,.F.,.F.,(4,3,3,3,3,3,3,3,3,3,3,3,3,3,3,3,3,3,3,3,
3,3,3,3,3,3,3,3,3,3,3,3,3,3,3,3,3,3,3,3,3,3,3,3,3,3,3,3,3,3,3,3,3,3,3,3,
3,3,3,3,3,3,3,3,3,3,3,3,3,3,3,3,3,3,3,4),(-173.738752334043,-173.651614929709,
-173.563992488095,-173.476967882539,-173.389960097741,-173.302946680709,
-173.214868859732,-173.127730364889,-173.039182880844,-172.9506353968,-172.86208324472,
-172.773645849197,-172.685299405999,-172.593502072915,-172.505257951009,
-172.417027265073,-172.328788646349,-172.240520725501,-172.152152424859,
-172.063724613698,-171.975166477595,-171.950920741327,-171.862368589247,
-171.773931193724,-171.685584750526,-171.593787417442,-171.505543295536,
-171.4173126096,-171.329073990876,-171.240806070027,-171.152437769386,-171.064009958225,
-170.975451822122,-170.951206085854,-170.862653933774,-170.774216538251,
-170.685870095053,-170.594072761969,-170.505828640062,-170.417597954126,
-170.329359335402,-170.241091414554,-170.152723113912,-170.064295302751,
-169.975737166648,-169.951491430381,-169.862939278302,-169.774501882779,
-169.686155439581,-169.594358106497,-169.506113984591,-169.417883298655,
-169.329644679931,-169.241376759083,-169.153008458442,-169.064580647281,
-168.976022511178,-168.951776774909,-168.86322462283,-168.774787227306,
-168.686440784108,-168.594643451024,-168.506399329118,-168.418168643182,
-168.329930024459,-168.241662103611,-168.15329380297,-168.064865991809,
-167.976307855706,-167.952062119436,-167.858803568459,-167.765717118764,
-167.672853547193,-167.580125408874,-167.487567112195,-167.455567027009),
 .UNSPECIFIED.);
#452=B_SPLINE_CURVE_WITH_KNOTS('',3,(#66696,#66697,#66698,#66699,#66700,
#66701,#66702,#66703,#66704,#66705,#66706,#66707,#66708,#66709,#66710,#66711,
#66712,#66713,#66714,#66715,#66716,#66717,#66718,#66719,#66720,#66721,#66722,
#66723,#66724,#66725,#66726,#66727,#66728,#66729,#66730,#66731,#66732,#66733,
#66734,#66735,#66736,#66737,#66738,#66739,#66740,#66741,#66742,#66743,#66744,
#66745,#66746,#66747,#66748,#66749,#66750,#66751,#66752,#66753,#66754,#66755,
#66756,#66757,#66758,#66759,#66760,#66761,#66762,#66763,#66764,#66765,#66766,
#66767,#66768,#66769,#66770,#66771,#66772,#66773,#66774,#66775,#66776,#66777,
#66778,#66779,#66780,#66781,#66782,#66783,#66784,#66785,#66786,#66787,#66788,
#66789,#66790,#66791,#66792,#66793,#66794,#66795,#66796,#66797,#66798,#66799,
#66800,#66801,#66802,#66803,#66804,#66805,#66806,#66807,#66808,#66809,#66810,
#66811,#66812,#66813,#66814,#66815,#66816,#66817,#66818,#66819,#66820,#66821,
#66822,#66823,#66824,#66825,#66826,#66827,#66828,#66829,#66830,#66831,#66832,
#66833,#66834,#66835,#66836,#66837,#66838,#66839,#66840,#66841,#66842,#66843,
#66844,#66845,#66846,#66847,#66848,#66849,#66850,#66851,#66852,#66853,#66854,
#66855,#66856,#66857,#66858,#66859,#66860,#66861,#66862,#66863,#66864,#66865,
#66866,#66867,#66868,#66869,#66870,#66871,#66872,#66873,#66874,#66875,#66876,
#66877,#66878,#66879,#66880,#66881,#66882,#66883,#66884,#66885,#66886,#66887,
#66888,#66889,#66890,#66891,#66892,#66893,#66894,#66895,#66896,#66897,#66898,
#66899,#66900,#66901,#66902,#66903,#66904,#66905,#66906,#66907,#66908,#66909,
#66910,#66911,#66912,#66913,#66914,#66915,#66916,#66917,#66918,#66919,#66920,
#66921),.UNSPECIFIED.,.F.,.F.,(4,3,3,3,3,3,3,3,3,3,3,3,3,3,3,3,3,3,3,3,
3,3,3,3,3,3,3,3,3,3,3,3,3,3,3,3,3,3,3,3,3,3,3,3,3,3,3,3,3,3,3,3,3,3,3,3,
3,3,3,3,3,3,3,3,3,3,3,3,3,3,3,3,3,3,3,4),(-167.455567026863,-167.363266863581,
-167.270842710716,-167.178199114077,-167.085435326711,-166.992463354601,
-166.952347463963,-166.863795311883,-166.77535791636,-166.687011473162,
-166.595214140078,-166.506970018171,-166.418739332235,-166.330500713511,
-166.242232792663,-166.153864492021,-166.06543668086,-165.976878544757,
-165.95263280849,-165.86408065641,-165.775643260887,-165.687296817689,-165.595499484605,
-165.507255362699,-165.419024676763,-165.330786058039,-165.24251813719,
-165.154149836549,-165.065722025388,-164.977163889285,-164.952918153017,
-164.864366000937,-164.775928605414,-164.687582162216,-164.595784829132,
-164.507540707226,-164.41931002129,-164.331071402566,-164.242803481717,
-164.154435181076,-164.066007369915,-163.977449233812,-163.953203497544,
-163.864651345465,-163.776213949942,-163.687867506743,-163.59607017366,
-163.507826051754,-163.419595365818,-163.331356747094,-163.243088826246,
-163.154720525604,-163.066292714444,-162.977734578341,-162.953488842072,
-162.864936689992,-162.776499294469,-162.688152851271,-162.596355518187,
-162.508111396281,-162.419880710345,-162.331642091621,-162.243374170773,
-162.155005870132,-162.066578058971,-161.978019922868,-161.953774186599,
-161.866428726277,-161.779222289971,-161.692095142986,-161.605024747212,
-161.517988622192,-161.430932553615,-161.343870414659,-161.256723427662,
-161.172381719684),.UNSPECIFIED.);
#453=B_SPLINE_CURVE_WITH_KNOTS('',3,(#66923,#66924,#66925,#66926,#66927,
#66928,#66929,#66930,#66931,#66932,#66933),.UNSPECIFIED.,.F.,.F.,(4,1,1,
1,1,1,1,1,4),(-161.172381719684,-160.954059531126,-159.954344875653,-158.95463022018,
-157.954915564707,-156.955200909235,-155.955486253762,-154.955771598289,
-154.889196412504),.UNSPECIFIED.);
#454=B_SPLINE_CURVE_WITH_KNOTS('',3,(#66935,#66936,#66937,#66938,#66939,
#66940,#66941,#66942,#66943,#66944,#66945,#66946,#66947,#66948,#66949,#66950,
#66951,#66952,#66953,#66954,#66955,#66956,#66957,#66958,#66959,#66960,#66961,
#66962,#66963,#66964,#66965,#66966,#66967,#66968,#66969,#66970,#66971,#66972,
#66973,#66974,#66975,#66976,#66977,#66978,#66979,#66980,#66981,#66982,#66983,
#66984,#66985,#66986,#66987,#66988,#66989,#66990,#66991,#66992,#66993,#66994,
#66995,#66996,#66997,#66998,#66999,#67000,#67001,#67002,#67003,#67004,#67005,
#67006,#67007,#67008,#67009,#67010,#67011,#67012,#67013,#67014,#67015,#67016,
#67017,#67018,#67019,#67020,#67021,#67022,#67023,#67024,#67025,#67026,#67027,
#67028,#67029,#67030,#67031,#67032,#67033,#67034,#67035,#67036,#67037,#67038,
#67039,#67040,#67041,#67042,#67043,#67044,#67045,#67046,#67047,#67048,#67049,
#67050,#67051,#67052,#67053,#67054,#67055,#67056,#67057,#67058,#67059,#67060,
#67061,#67062,#67063,#67064,#67065,#67066,#67067,#67068,#67069,#67070,#67071,
#67072,#67073,#67074,#67075,#67076,#67077,#67078,#67079,#67080,#67081,#67082,
#67083,#67084,#67085,#67086,#67087,#67088,#67089,#67090,#67091,#67092,#67093,
#67094,#67095,#67096,#67097,#67098,#67099,#67100,#67101,#67102,#67103,#67104,
#67105,#67106,#67107,#67108,#67109,#67110,#67111,#67112,#67113,#67114,#67115,
#67116,#67117,#67118,#67119,#67120,#67121,#67122,#67123,#67124,#67125,#67126,
#67127,#67128,#67129,#67130,#67131,#67132,#67133,#67134,#67135,#67136,#67137,
#67138,#67139,#67140,#67141,#67142,#67143,#67144,#67145,#67146,#67147,#67148,
#67149,#67150,#67151,#67152,#67153,#67154,#67155,#67156,#67157,#67158,#67159,
#67160),.UNSPECIFIED.,.F.,.F.,(4,3,3,3,3,3,3,3,3,3,3,3,3,3,3,3,3,3,3,3,
3,3,3,3,3,3,3,3,3,3,3,3,3,3,3,3,3,3,3,3,3,3,3,3,3,3,3,3,3,3,3,3,3,3,3,3,
3,3,3,3,3,3,3,3,3,3,3,3,3,3,3,3,3,3,3,4),(-154.889196412504,-154.801516541426,
-154.713945565697,-154.62645880606,-154.539027538957,-154.451624262389,
-154.364226806844,-154.276813011792,-154.189307658123,-154.101752947617,
-154.014060389313,-153.956056942816,-153.867504790736,-153.779067395213,
-153.690720952015,-153.598923618931,-153.510679497025,-153.422448811088,
-153.334210192364,-153.245942271516,-153.157573970875,-153.069146159713,
-152.98058802361,-152.956342287343,-152.867790135264,-152.779352739741,
-152.691006296543,-152.599208963459,-152.510964841553,-152.422734155617,
-152.334495536893,-152.246227616045,-152.157859315404,-152.069431504243,
-151.98087336814,-151.956627631871,-151.868075479791,-151.779638084268,
-151.69129164107,-151.599494307986,-151.51125018608,-151.423019500144,-151.33478088142,
-151.246512960572,-151.158144659931,-151.06971684877,-150.981158712667,
-150.956912976398,-150.868360824318,-150.779923428795,-150.691576985597,
-150.599779652513,-150.511535530607,-150.42330484467,-150.335066225946,
-150.246798305098,-150.158430004457,-150.070002193295,-149.981444057192,
-149.957198320925,-149.868646168845,-149.780208773322,-149.691862330124,
-149.60006499704,-149.511820875134,-149.423590189197,-149.335351570474,
-149.247083649626,-149.158715348984,-149.070287537824,-148.981729401721,
-148.957483665452,-148.855191749666,-148.753322456798,-148.652222206138,
-148.606011351141),.UNSPECIFIED.);
#455=B_SPLINE_CURVE_WITH_KNOTS('',3,(#67162,#67163,#67164,#67165,#67166,
#67167,#67168,#67169,#67170,#67171),.UNSPECIFIED.,.F.,.F.,(4,1,1,1,1,1,
1,4),(-148.606011105325,-147.957769009979,-146.958054354506,-145.958339699033,
-144.958625043561,-143.958910388088,-142.959195732615,-142.322825798145),
 .UNSPECIFIED.);
#456=B_SPLINE_CURVE_WITH_KNOTS('',3,(#67173,#67174,#67175,#67176,#67177,
#67178,#67179,#67180,#67181,#67182),.UNSPECIFIED.,.F.,.F.,(4,1,1,1,1,1,
1,4),(-142.322825798145,-141.959481077142,-140.959766421669,-139.960051766196,
-138.960337110724,-137.960622455251,-136.960907799778,-136.039640490966),
 .UNSPECIFIED.);
#457=B_SPLINE_CURVE_WITH_KNOTS('',3,(#67184,#67185,#67186,#67187,#67188,
#67189,#67190,#67191,#67192,#67193,#67194,#67195),.UNSPECIFIED.,.F.,.F.,
(4,2,1,1,1,1,1,1,4),(-136.039640490966,-135.961193144305,-134.961478488832,
-133.961763833359,-132.962049177887,-131.962334522414,-130.962619866941,
-129.962905211468,-129.756455183786),.UNSPECIFIED.);
#458=B_SPLINE_CURVE_WITH_KNOTS('',3,(#67197,#67198,#67199,#67200,#67201,
#67202,#67203,#67204,#67205,#67206,#67207,#67208,#67209,#67210,#67211,#67212,
#67213,#67214,#67215,#67216,#67217,#67218,#67219,#67220,#67221,#67222,#67223,
#67224,#67225,#67226,#67227,#67228,#67229,#67230,#67231,#67232,#67233,#67234,
#67235,#67236,#67237,#67238,#67239,#67240,#67241,#67242,#67243,#67244,#67245,
#67246,#67247,#67248,#67249,#67250,#67251,#67252,#67253,#67254,#67255,#67256,
#67257,#67258,#67259,#67260,#67261,#67262,#67263,#67264,#67265,#67266,#67267,
#67268,#67269,#67270,#67271,#67272,#67273,#67274,#67275,#67276,#67277,#67278,
#67279,#67280,#67281,#67282,#67283,#67284,#67285,#67286,#67287,#67288,#67289,
#67290,#67291,#67292,#67293,#67294,#67295,#67296,#67297,#67298,#67299,#67300,
#67301,#67302,#67303,#67304,#67305,#67306,#67307,#67308,#67309,#67310,#67311,
#67312,#67313,#67314,#67315,#67316,#67317,#67318,#67319,#67320,#67321,#67322,
#67323,#67324,#67325,#67326,#67327,#67328,#67329,#67330,#67331,#67332,#67333,
#67334,#67335,#67336,#67337,#67338,#67339,#67340,#67341,#67342,#67343,#67344,
#67345,#67346,#67347,#67348,#67349,#67350,#67351,#67352,#67353,#67354,#67355,
#67356,#67357,#67358,#67359,#67360,#67361,#67362,#67363,#67364,#67365,#67366,
#67367,#67368,#67369,#67370,#67371,#67372,#67373,#67374,#67375,#67376,#67377,
#67378,#67379,#67380,#67381,#67382,#67383,#67384,#67385,#67386,#67387,#67388,
#67389,#67390,#67391,#67392,#67393,#67394,#67395,#67396,#67397,#67398,#67399,
#67400,#67401,#67402,#67403,#67404,#67405,#67406,#67407,#67408,#67409,#67410,
#67411,#67412,#67413,#67414,#67415,#67416,#67417,#67418,#67419,#67420,#67421,
#67422),.UNSPECIFIED.,.F.,.F.,(4,3,3,3,3,3,3,3,3,3,3,3,3,3,3,3,3,3,3,3,
3,3,3,3,3,3,3,3,3,3,3,3,3,3,3,3,3,3,3,3,3,3,3,3,3,3,3,3,3,3,3,3,3,3,3,3,
3,3,3,3,3,3,3,3,3,3,3,3,3,3,3,3,3,3,3,4),(-129.756455183786,-129.669330401864,
-129.58106292113,-129.494055101733,-129.407065460323,-129.320071530291,
-129.230851286717,-129.143733708822,-129.053462132409,-128.963190555995,
-128.874638403916,-128.786201008393,-128.697854565195,-128.606057232111,
-128.517813110205,-128.429582424269,-128.341343805545,-128.253075884698,
-128.164707584056,-128.076279772896,-127.987721636793,-127.963475900523,
-127.874923748443,-127.78648635292,-127.698139909722,-127.606342576638,
-127.518098454732,-127.429867768796,-127.341629150072,-127.253361229224,
-127.164992928583,-127.076565117422,-126.988006981319,-126.96376124505,
-126.87520909297,-126.786771697447,-126.698425254249,-126.606627921165,
-126.518383799259,-126.430153113322,-126.341914494598,-126.25364657375,
-126.165278273108,-126.076850461947,-125.988292325844,-125.964046589577,
-125.875494437497,-125.787057041974,-125.698710598776,-125.606913265692,
-125.518669143786,-125.43043845785,-125.342199839126,-125.253931918278,
-125.165563617636,-125.077135806475,-124.988577670373,-124.964331934104,
-124.875779782024,-124.787342386501,-124.698995943303,-124.607198610219,
-124.518954488313,-124.430723802377,-124.342485183653,-124.254217262805,
-124.165848962164,-124.077421151002,-123.9888630149,-123.964617278631,-123.871137501164,
-123.777833647348,-123.684759513492,-123.591825941801,-123.49906942334,
-123.473269876792),.UNSPECIFIED.);
#459=B_SPLINE_CURVE_WITH_KNOTS('',3,(#67424,#67425,#67426,#67427,#67428,
#67429,#67430,#67431,#67432,#67433,#67434,#67435,#67436,#67437,#67438,#67439,
#67440,#67441,#67442,#67443,#67444,#67445,#67446,#67447,#67448,#67449,#67450,
#67451,#67452,#67453,#67454,#67455,#67456,#67457,#67458,#67459,#67460,#67461,
#67462,#67463,#67464,#67465,#67466,#67467,#67468,#67469,#67470,#67471,#67472,
#67473,#67474,#67475,#67476,#67477,#67478,#67479,#67480,#67481,#67482,#67483,
#67484,#67485,#67486,#67487,#67488,#67489,#67490,#67491,#67492,#67493,#67494,
#67495,#67496,#67497,#67498,#67499,#67500,#67501,#67502,#67503,#67504,#67505,
#67506,#67507,#67508,#67509,#67510,#67511,#67512,#67513,#67514,#67515,#67516,
#67517,#67518,#67519,#67520,#67521,#67522,#67523,#67524,#67525,#67526,#67527,
#67528,#67529,#67530,#67531,#67532,#67533,#67534,#67535,#67536,#67537,#67538,
#67539,#67540,#67541,#67542,#67543,#67544,#67545,#67546,#67547,#67548,#67549,
#67550,#67551,#67552,#67553,#67554,#67555,#67556,#67557,#67558,#67559,#67560,
#67561,#67562,#67563,#67564,#67565,#67566,#67567,#67568,#67569,#67570,#67571,
#67572,#67573,#67574,#67575,#67576,#67577,#67578,#67579,#67580,#67581,#67582,
#67583,#67584,#67585,#67586,#67587,#67588,#67589,#67590,#67591,#67592,#67593,
#67594,#67595,#67596,#67597,#67598,#67599,#67600,#67601,#67602,#67603,#67604,
#67605,#67606,#67607,#67608,#67609,#67610,#67611,#67612,#67613,#67614,#67615,
#67616,#67617,#67618,#67619,#67620,#67621,#67622,#67623,#67624,#67625,#67626,
#67627,#67628,#67629,#67630,#67631,#67632,#67633,#67634,#67635,#67636,#67637,
#67638,#67639,#67640,#67641,#67642,#67643,#67644,#67645,#67646,#67647,#67648,
#67649),.UNSPECIFIED.,.F.,.F.,(4,3,3,3,3,3,3,3,3,3,3,3,3,3,3,3,3,3,3,3,
3,3,3,3,3,3,3,3,3,3,3,3,3,3,3,3,3,3,3,3,3,3,3,3,3,3,3,3,3,3,3,3,3,3,3,3,
3,3,3,3,3,3,3,3,3,3,3,3,3,3,3,3,3,3,3,4),(-123.473269876606,-123.381161277955,
-123.288935985714,-123.196498304588,-123.103945159693,-123.011185121163,
-122.964902623158,-122.876350471079,-122.787913075556,-122.699566632358,
-122.607769299274,-122.519525177368,-122.431294491433,-122.343055872709,
-122.254787951861,-122.16641965122,-122.077991840059,-121.989433703957,
-121.965187967686,-121.876635815606,-121.788198420083,-121.699851976885,
-121.608054643801,-121.519810521895,-121.431579835959,-121.343341217235,
-121.255073296387,-121.166704995745,-121.078277184585,-120.989719048482,
-120.965473312213,-120.876921160133,-120.78848376461,-120.700137321412,
-120.608339988328,-120.520095866422,-120.431865180485,-120.343626561761,
-120.255358640913,-120.166990340271,-120.07856252911,-119.990004393007,
-119.96575865674,-119.87720650466,-119.788769109137,-119.700422665939,-119.608625332855,
-119.520381210949,-119.432150525013,-119.343911906289,-119.255643985441,
-119.167275684799,-119.078847873638,-118.990289737535,-118.966044001267,
-118.877491849187,-118.789054453664,-118.700708010466,-118.608910677382,
-118.520666555476,-118.43243586954,-118.344197250816,-118.255929329967,
-118.167561029326,-118.079133218164,-117.990575082061,-117.966329345794,
-117.878958677332,-117.791727434839,-117.704575738324,-117.61748106669,
-117.530420956491,-117.44334239818,-117.356257991148,-117.269092049149,
-117.190084569427),.UNSPECIFIED.);
#460=B_SPLINE_CURVE_WITH_KNOTS('',3,(#67651,#67652,#67653,#67654,#67655,
#67656,#67657,#67658,#67659,#67660,#67661),.UNSPECIFIED.,.F.,.F.,(4,1,1,
1,1,1,1,1,4),(-117.190084569427,-116.966614690321,-115.966900034849,-114.967185379376,
-113.967470723903,-112.96775606843,-111.968041412957,-110.968326757484,
-110.906899262247),.UNSPECIFIED.);
#461=B_SPLINE_CURVE_WITH_KNOTS('',3,(#67663,#67664,#67665,#67666,#67667,
#67668,#67669,#67670,#67671,#67672,#67673,#67674,#67675,#67676,#67677,#67678,
#67679,#67680,#67681,#67682,#67683,#67684,#67685,#67686,#67687,#67688,#67689,
#67690,#67691,#67692,#67693,#67694,#67695,#67696,#67697,#67698,#67699,#67700,
#67701,#67702,#67703,#67704,#67705,#67706,#67707,#67708,#67709,#67710,#67711,
#67712,#67713,#67714,#67715,#67716,#67717,#67718,#67719,#67720,#67721,#67722,
#67723,#67724,#67725,#67726,#67727,#67728,#67729,#67730,#67731,#67732,#67733,
#67734,#67735,#67736,#67737,#67738,#67739,#67740,#67741,#67742,#67743,#67744,
#67745,#67746,#67747,#67748,#67749,#67750,#67751,#67752,#67753,#67754,#67755,
#67756,#67757,#67758,#67759,#67760,#67761,#67762,#67763,#67764,#67765,#67766,
#67767,#67768,#67769,#67770,#67771,#67772,#67773,#67774,#67775,#67776,#67777,
#67778,#67779,#67780,#67781,#67782,#67783,#67784,#67785,#67786,#67787,#67788,
#67789,#67790,#67791,#67792,#67793,#67794,#67795,#67796,#67797,#67798,#67799,
#67800,#67801,#67802,#67803,#67804,#67805,#67806,#67807,#67808,#67809,#67810,
#67811,#67812,#67813,#67814,#67815,#67816,#67817,#67818,#67819,#67820,#67821,
#67822,#67823,#67824,#67825,#67826,#67827,#67828,#67829,#67830,#67831,#67832,
#67833,#67834,#67835,#67836,#67837,#67838,#67839,#67840,#67841,#67842,#67843,
#67844,#67845,#67846,#67847,#67848,#67849,#67850,#67851,#67852,#67853,#67854,
#67855,#67856,#67857,#67858,#67859,#67860,#67861,#67862,#67863,#67864,#67865,
#67866,#67867,#67868,#67869,#67870,#67871,#67872,#67873,#67874,#67875,#67876,
#67877,#67878,#67879,#67880,#67881,#67882,#67883,#67884,#67885,#67886,#67887,
#67888),.UNSPECIFIED.,.F.,.F.,(4,3,3,3,3,3,3,3,3,3,3,3,3,3,3,3,3,3,3,3,
3,3,3,3,3,3,3,3,3,3,3,3,3,3,3,3,3,3,3,3,3,3,3,3,3,3,3,3,3,3,3,3,3,3,3,3,
3,3,3,3,3,3,3,3,3,3,3,3,3,3,3,3,3,3,3,4),(-110.906899262247,-110.81916613363,
-110.73154266842,-110.644004230026,-110.556522414419,-110.469069398607,
-110.381623052323,-110.294161255007,-110.20660822571,-110.119006713472,
-110.031265869715,-109.968612102012,-109.880059949932,-109.791622554409,
-109.703276111211,-109.611478778127,-109.523234656221,-109.435003970284,
-109.34676535156,-109.258497430712,-109.170129130071,-109.081701318909,
-108.993143182807,-108.968897446539,-108.880345294459,-108.791907898936,
-108.703561455738,-108.611764122654,-108.523520000748,-108.435289314812,
-108.347050696088,-108.258782775239,-108.170414474598,-108.081986663437,
-107.993428527334,-107.969182791066,-107.880630638987,-107.792193243463,
-107.703846800265,-107.612049467181,-107.523805345275,-107.435574659339,
-107.347336040615,-107.259068119767,-107.170699819126,-107.082272007965,
-106.993713871862,-106.969468135593,-106.880915983513,-106.79247858799,
-106.704132144792,-106.612334811708,-106.524090689802,-106.435860003866,
-106.347621385142,-106.259353464294,-106.170985163653,-106.082557352492,
-105.993999216389,-105.96975348012,-105.88120132804,-105.792763932517,-105.704417489319,
-105.612620156235,-105.524376034329,-105.436145348392,-105.347906729668,
-105.25963880882,-105.171270508178,-105.082842697018,-104.994284560914,
-104.970038824647,-104.867263249388,-104.764933531125,-104.663410117904,
-104.623714198583),.UNSPECIFIED.);
#462=B_SPLINE_CURVE_WITH_KNOTS('',3,(#67890,#67891,#67892,#67893,#67894,
#67895,#67896,#67897,#67898,#67899),.UNSPECIFIED.,.F.,.F.,(4,1,1,1,1,1,
1,4),(-104.623713955068,-103.970324169175,-102.970609513702,-101.970894858229,
-100.971180202756,-99.9714655472832,-98.9717508918104,-98.3405286478881),
 .UNSPECIFIED.);
#463=B_SPLINE_CURVE_WITH_KNOTS('',3,(#67901,#67902,#67903,#67904,#67905,
#67906,#67907,#67908,#67909,#67910),.UNSPECIFIED.,.F.,.F.,(4,1,1,1,1,1,
1,4),(-98.3405286478881,-97.9720362363375,-96.9723215808647,-95.9726069253919,
-94.972892269919,-93.9731776144462,-92.9734629589734,-92.0573433407085),
 .UNSPECIFIED.);
#464=B_SPLINE_CURVE_WITH_KNOTS('',3,(#67912,#67913,#67914,#67915,#67916,
#67917,#67918,#67919,#67920,#67921,#67922),.UNSPECIFIED.,.F.,.F.,(4,1,1,
1,1,1,1,1,4),(-92.0573433407085,-91.9737483035005,-90.9740336480277,-89.9743189925549,
-88.974604337082,-87.9748896816092,-86.9751750261364,-85.9754603706636,
-85.7741580335289),.UNSPECIFIED.);
#465=B_SPLINE_CURVE_WITH_KNOTS('',3,(#67924,#67925,#67926,#67927,#67928,
#67929,#67930,#67931,#67932,#67933,#67934,#67935,#67936,#67937,#67938,#67939,
#67940,#67941,#67942,#67943,#67944,#67945,#67946,#67947,#67948,#67949,#67950,
#67951,#67952,#67953,#67954,#67955,#67956,#67957,#67958,#67959,#67960,#67961,
#67962,#67963,#67964,#67965,#67966,#67967,#67968,#67969,#67970,#67971,#67972,
#67973,#67974,#67975,#67976,#67977,#67978,#67979,#67980,#67981,#67982,#67983,
#67984,#67985,#67986,#67987,#67988,#67989,#67990,#67991,#67992,#67993,#67994,
#67995,#67996,#67997,#67998,#67999,#68000,#68001,#68002,#68003,#68004,#68005,
#68006,#68007,#68008,#68009,#68010,#68011,#68012,#68013,#68014,#68015,#68016,
#68017,#68018,#68019,#68020,#68021,#68022,#68023,#68024,#68025,#68026,#68027,
#68028,#68029,#68030,#68031,#68032,#68033,#68034,#68035,#68036,#68037,#68038,
#68039,#68040,#68041,#68042,#68043,#68044,#68045,#68046,#68047,#68048,#68049,
#68050,#68051,#68052,#68053,#68054,#68055,#68056,#68057,#68058,#68059,#68060,
#68061,#68062,#68063,#68064,#68065,#68066,#68067,#68068,#68069,#68070,#68071,
#68072,#68073,#68074,#68075,#68076,#68077,#68078,#68079,#68080,#68081,#68082,
#68083,#68084,#68085,#68086,#68087,#68088,#68089,#68090,#68091,#68092,#68093,
#68094,#68095,#68096,#68097,#68098,#68099,#68100,#68101,#68102,#68103,#68104,
#68105,#68106,#68107,#68108,#68109,#68110,#68111,#68112,#68113,#68114,#68115,
#68116,#68117,#68118,#68119,#68120,#68121,#68122,#68123,#68124,#68125,#68126,
#68127,#68128,#68129,#68130,#68131,#68132,#68133,#68134,#68135,#68136,#68137,
#68138,#68139,#68140,#68141,#68142,#68143,#68144,#68145,#68146,#68147,#68148,
#68149,#68150,#68151,#68152),.UNSPECIFIED.,.F.,.F.,(4,3,3,3,3,3,3,3,3,3,
3,3,3,3,3,3,3,3,3,3,3,3,3,3,3,3,3,3,3,3,3,3,3,3,3,3,3,3,3,3,3,3,3,3,3,3,
3,3,3,3,3,3,3,3,3,3,3,3,3,3,3,3,3,3,3,3,3,3,3,3,3,3,3,3,3,3,4),(-85.7741580335289,
-85.687043478963,-85.5981312584914,-85.511137786955,-85.4241638250235,-85.3371868942073,
-85.2468265994532,-85.1597274426246,-85.0725693580145,-84.9852878854184,
-84.9757457151907,-84.8871935631111,-84.798756167588,-84.71040972439,-84.618612391306,
-84.5303682693999,-84.4421375834636,-84.3538989647399,-84.2656310438917,
-84.1772627432505,-84.0888349320897,-84.000276795987,-83.9760310597179,
-83.8874789076383,-83.7990415121153,-83.7106950689173,-83.6188977358333,
-83.5306536139271,-83.4424229279909,-83.3541843092672,-83.2659163884184,
-83.1775480877771,-83.089120276616,-83.0005621405133,-82.9763164042451,
-82.8877642521655,-82.7993268566425,-82.7109804134444,-82.6191830803604,
-82.5309389584542,-82.442708272518,-82.3544696537941,-82.2662017329457,
-82.1778334323044,-82.0894056211431,-82.0008474850403,-81.9766017487722,
-81.8880495966926,-81.7996122011695,-81.7112657579712,-81.6194684248872,
-81.5312243029812,-81.442993617045,-81.3547549983213,-81.2664870774732,
-81.178118776832,-81.0896909656709,-81.0011328295681,-80.9768870932994,
-80.8883349412198,-80.7998975456966,-80.7115511024986,-80.6197537694146,
-80.5315096475084,-80.4432789615722,-80.3550403428486,-80.2667724219998,
-80.1784041213586,-80.0899763101974,-80.0014181740946,-79.9771724378266,
-79.88346559413,-79.785342377222,-79.6920597431561,-79.5989227576672,-79.5059681543834,
-79.4909727264982),.UNSPECIFIED.);
#466=B_SPLINE_CURVE_WITH_KNOTS('',3,(#68154,#68155,#68156,#68157,#68158,
#68159,#68160,#68161,#68162,#68163,#68164,#68165,#68166,#68167,#68168,#68169,
#68170,#68171,#68172,#68173,#68174,#68175,#68176,#68177,#68178,#68179,#68180,
#68181,#68182,#68183,#68184,#68185,#68186,#68187,#68188,#68189,#68190,#68191,
#68192,#68193,#68194,#68195,#68196,#68197,#68198,#68199,#68200,#68201,#68202,
#68203,#68204,#68205,#68206,#68207,#68208,#68209,#68210,#68211,#68212,#68213,
#68214,#68215,#68216,#68217,#68218,#68219,#68220,#68221,#68222,#68223,#68224,
#68225,#68226,#68227,#68228,#68229,#68230,#68231,#68232,#68233,#68234,#68235,
#68236,#68237,#68238,#68239,#68240,#68241,#68242,#68243,#68244,#68245,#68246,
#68247,#68248,#68249,#68250,#68251,#68252,#68253,#68254,#68255,#68256,#68257,
#68258,#68259,#68260,#68261,#68262,#68263,#68264,#68265,#68266,#68267,#68268,
#68269,#68270,#68271,#68272,#68273,#68274,#68275,#68276,#68277,#68278,#68279,
#68280,#68281,#68282,#68283,#68284,#68285,#68286,#68287,#68288,#68289,#68290,
#68291,#68292,#68293,#68294,#68295,#68296,#68297,#68298,#68299,#68300,#68301,
#68302,#68303,#68304,#68305,#68306,#68307,#68308,#68309,#68310,#68311,#68312,
#68313,#68314,#68315,#68316,#68317,#68318,#68319,#68320,#68321,#68322,#68323,
#68324,#68325,#68326,#68327,#68328,#68329,#68330,#68331,#68332,#68333,#68334,
#68335,#68336,#68337,#68338,#68339,#68340,#68341,#68342,#68343,#68344,#68345,
#68346,#68347,#68348,#68349,#68350,#68351,#68352,#68353,#68354,#68355,#68356,
#68357,#68358,#68359,#68360,#68361,#68362,#68363,#68364,#68365,#68366,#68367,
#68368,#68369,#68370,#68371,#68372,#68373,#68374,#68375,#68376,#68377,#68378,
#68379),.UNSPECIFIED.,.F.,.F.,(4,3,3,3,3,3,3,3,3,3,3,3,3,3,3,3,3,3,3,3,
3,3,3,3,3,3,3,3,3,3,3,3,3,3,3,3,3,3,3,3,3,3,3,3,3,3,3,3,3,3,3,3,3,3,3,3,
3,3,3,3,3,3,3,3,3,3,3,3,3,3,3,3,3,3,3,4),(-79.4909727263493,-79.3990508671971,
-79.3070193033341,-79.2147821410095,-79.1224340910687,-79.0298803650998,
-78.9774577823537,-78.8889056302741,-78.800468234751,-78.7121217915529,
-78.6203244584689,-78.5320803365628,-78.4438496506267,-78.3556110319029,
-78.2673431110545,-78.1789748104133,-78.0905469992525,-78.0019888631497,
-77.9777431268809,-77.8891909748013,-77.8007535792782,-77.7124071360799,
-77.620609802996,-77.5323656810899,-77.4441349951538,-77.3558963764299,
-77.267628455582,-77.1792601549407,-77.0908323437798,-77.0022742076771,
-76.9780284714081,-76.8894763193284,-76.8010389238053,-76.7126924806068,
-76.6208951475229,-76.5326510256168,-76.4444203396807,-76.3561817209568,
-76.2679138001086,-76.1795454994673,-76.0911176883063,-76.0025595522034,
-75.9783138159353,-75.8897616638556,-75.8013242683325,-75.7129778251343,
-75.6211804920503,-75.5329363701443,-75.444705684208,-75.3564670654841,
-75.2681991446358,-75.1798308439944,-75.0914030328337,-75.0028448967308,
-74.9785991604624,-74.8900470083828,-74.8016096128595,-74.7132631696616,
-74.6214658365776,-74.5332217146715,-74.4449910287354,-74.3567524100117,
-74.2684844891637,-74.1801161885225,-74.0916883773617,-74.0031302412588,
-73.9788845049896,-73.8914861121851,-73.8042275676723,-73.7170488426747,
-73.6299274350949,-73.5428409004767,-73.4557374324535,-73.3686283582785,
-73.2814410301796,-73.2077874191697),.UNSPECIFIED.);
#467=B_SPLINE_CURVE_WITH_KNOTS('',3,(#68381,#68382,#68383,#68384,#68385,
#68386,#68387,#68388,#68389,#68390,#68391),.UNSPECIFIED.,.F.,.F.,(4,1,1,
1,1,1,1,1,4),(-73.2077874191697,-72.9791698495167,-71.9794551940439,-70.9797405385711,
-69.9800258830982,-68.9803112276254,-67.9805965721526,-66.9808819166797,
-66.9246021119901),.UNSPECIFIED.);
#468=B_SPLINE_CURVE_WITH_KNOTS('',3,(#68393,#68394,#68395,#68396,#68397,
#68398,#68399,#68400,#68401,#68402),.UNSPECIFIED.,.F.,.F.,(4,1,1,1,1,1,
1,4),(-66.9246021119901,-65.9811672612069,-64.9814526057341,-63.9817379502612,
-62.9820232947884,-61.9823086393156,-60.9825939838428,-60.6414242977388),
 .UNSPECIFIED.);
#469=B_SPLINE_CURVE_WITH_KNOTS('',3,(#68404,#68405,#68406,#68407,#68408,
#68409,#68410,#68411,#68412,#68413,#68414,#68415,#68416,#68417,#68418,#68419,
#68420,#68421,#68422,#68423,#68424,#68425,#68426,#68427,#68428,#68429,#68430,
#68431,#68432,#68433,#68434,#68435,#68436,#68437,#68438,#68439,#68440,#68441,
#68442,#68443,#68444,#68445,#68446,#68447,#68448,#68449,#68450,#68451,#68452,
#68453,#68454,#68455,#68456,#68457,#68458,#68459,#68460,#68461,#68462,#68463,
#68464,#68465,#68466,#68467,#68468,#68469,#68470,#68471,#68472,#68473,#68474,
#68475,#68476,#68477,#68478,#68479,#68480,#68481,#68482,#68483,#68484,#68485,
#68486,#68487,#68488,#68489,#68490,#68491,#68492,#68493,#68494,#68495,#68496,
#68497,#68498,#68499,#68500,#68501,#68502,#68503,#68504,#68505,#68506,#68507,
#68508,#68509,#68510,#68511,#68512,#68513,#68514,#68515,#68516,#68517,#68518,
#68519,#68520,#68521,#68522,#68523,#68524,#68525,#68526,#68527,#68528,#68529,
#68530,#68531,#68532,#68533,#68534,#68535,#68536,#68537,#68538,#68539,#68540,
#68541,#68542,#68543,#68544,#68545,#68546,#68547,#68548,#68549,#68550,#68551,
#68552,#68553,#68554,#68555,#68556,#68557,#68558,#68559,#68560,#68561,#68562,
#68563,#68564,#68565,#68566,#68567,#68568,#68569,#68570,#68571,#68572,#68573,
#68574,#68575,#68576,#68577,#68578,#68579,#68580,#68581,#68582,#68583,#68584,
#68585,#68586,#68587,#68588,#68589,#68590,#68591,#68592,#68593,#68594,#68595,
#68596,#68597,#68598,#68599,#68600,#68601,#68602,#68603,#68604,#68605,#68606,
#68607,#68608,#68609,#68610,#68611,#68612,#68613,#68614,#68615,#68616,#68617,
#68618,#68619,#68620,#68621,#68622,#68623,#68624,#68625,#68626,#68627,#68628,
#68629),.UNSPECIFIED.,.F.,.F.,(4,3,3,3,3,3,3,3,3,3,3,3,3,3,3,3,3,3,3,3,
3,3,3,3,3,3,3,3,3,3,3,3,3,3,3,3,3,3,3,3,3,3,3,3,3,3,3,3,3,3,3,3,3,3,3,3,
3,3,3,3,3,3,3,3,3,3,3,3,3,3,3,3,3,3,3,4),(-60.6414168048105,-60.5531164885272,
-60.4648265653877,-60.3765258343915,-60.2881930918611,-60.1997525210904,
-60.1112505357928,-60.0226065066029,-59.9828793283699,-59.8943271762903,
-59.8058897807671,-59.717543337569,-59.625746004485,-59.5375018825789,-59.4492711966428,
-59.3610325779189,-59.272764657071,-59.1843963564296,-59.0959685452685,
-59.0074104091656,-58.9831646728971,-58.8946125208176,-58.8061751252944,
-58.7178286820963,-58.6260313490123,-58.5377872271062,-58.4495565411702,
-58.3613179224462,-58.2730500015979,-58.1846817009566,-58.0962538897957,
-58.007695753693,-57.9834500174243,-57.8948978653448,-57.8064604698214,
-57.7181140266232,-57.6263166935392,-57.5380725716331,-57.449841885697,
-57.3616032669731,-57.2733353461248,-57.1849670454835,-57.0965392343224,
-57.0079810982195,-56.9837353619514,-56.8951832098719,-56.8067458143486,
-56.7183993711503,-56.6266020380664,-56.5383579161603,-56.4501272302242,
-56.3618886115005,-56.2736206906521,-56.1852523900108,-56.0968245788499,
-56.008266442747,-55.9840207064786,-55.8954685543989,-55.807031158876,-55.7186847156778,
-55.6268873825938,-55.5386432606877,-55.4504125747516,-55.3621739560279,
-55.273906035179,-55.1855377345377,-55.0971099233766,-55.008551787274,-54.9843060510058,
-54.8950533954186,-54.8059198068906,-54.71688469093,-54.6272213926052,-54.5383253255974,
-54.4482784116142,-54.3582314976309),.UNSPECIFIED.);
#470=B_SPLINE_CURVE_WITH_KNOTS('',3,(#68631,#68632,#68633,#68634,#68635,
#68636,#68637,#68638,#68639,#68640),.UNSPECIFIED.,.F.,.F.,(4,1,1,1,1,1,
1,4),(-54.3582238422873,-53.9845913955329,-52.9848767400601,-51.9851620845873,
-50.9854474291144,-49.9857327736416,-48.9860181181688,-48.0750549567666),
 .UNSPECIFIED.);
#471=B_SPLINE_CURVE_WITH_KNOTS('',3,(#68642,#68643,#68644,#68645,#68646,
#68647,#68648,#68649,#68650,#68651,#68652,#68653,#68654,#68655,#68656,#68657,
#68658,#68659,#68660,#68661,#68662,#68663,#68664,#68665,#68666,#68667,#68668,
#68669,#68670,#68671,#68672,#68673,#68674,#68675,#68676,#68677,#68678,#68679,
#68680,#68681,#68682,#68683,#68684,#68685,#68686,#68687,#68688,#68689,#68690,
#68691,#68692,#68693,#68694,#68695,#68696,#68697,#68698,#68699,#68700,#68701,
#68702,#68703,#68704,#68705,#68706,#68707,#68708,#68709,#68710,#68711,#68712,
#68713,#68714,#68715,#68716,#68717,#68718,#68719,#68720,#68721,#68722,#68723,
#68724,#68725,#68726,#68727,#68728,#68729,#68730,#68731,#68732,#68733,#68734,
#68735,#68736,#68737,#68738,#68739,#68740,#68741,#68742,#68743,#68744,#68745,
#68746,#68747,#68748,#68749,#68750,#68751,#68752,#68753,#68754,#68755,#68756,
#68757,#68758,#68759,#68760,#68761,#68762,#68763,#68764,#68765,#68766,#68767,
#68768,#68769,#68770,#68771,#68772,#68773,#68774,#68775,#68776,#68777,#68778,
#68779,#68780,#68781,#68782,#68783,#68784,#68785,#68786,#68787,#68788,#68789,
#68790,#68791,#68792,#68793,#68794,#68795,#68796,#68797,#68798,#68799,#68800,
#68801,#68802,#68803,#68804,#68805,#68806,#68807,#68808,#68809,#68810,#68811,
#68812,#68813,#68814,#68815,#68816,#68817,#68818,#68819,#68820,#68821,#68822,
#68823,#68824,#68825,#68826,#68827,#68828,#68829,#68830,#68831,#68832,#68833,
#68834,#68835,#68836,#68837,#68838,#68839,#68840,#68841,#68842,#68843,#68844,
#68845,#68846,#68847,#68848,#68849,#68850,#68851,#68852,#68853,#68854,#68855,
#68856,#68857,#68858,#68859,#68860,#68861,#68862,#68863,#68864,#68865,#68866,
#68867),.UNSPECIFIED.,.F.,.F.,(4,3,3,3,3,3,3,3,3,3,3,3,3,3,3,3,3,3,3,3,
3,3,3,3,3,3,3,3,3,3,3,3,3,3,3,3,3,3,3,3,3,3,3,3,3,3,3,3,3,3,3,3,3,3,3,3,
3,3,3,3,3,3,3,3,3,3,3,3,3,3,3,3,3,3,3,4),(-48.0750461904513,-47.9863034626959,
-47.8977513106161,-47.8093139150928,-47.7209674718944,-47.6291701388105,
-47.5409260169042,-47.4526953309678,-47.3644567122437,-47.2761887913952,
-47.1878204907537,-47.0993926795925,-47.0108345434895,-46.9865888072231,
-46.8980366551436,-46.8095992596205,-46.7212528164225,-46.6294554833385,
-46.5412113614325,-46.4529806754964,-46.3647420567726,-46.2764741359245,
-46.1881058352832,-46.0996780241223,-46.0111198880196,-45.9868741517503,
-45.8983219996707,-45.8098846041475,-45.7215381609494,-45.6297408278654,
-45.5414967059593,-45.4532660200232,-45.3650274012992,-45.2767594804509,
-45.1883911798096,-45.0999633686486,-45.0114052325458,-44.9871594962774,
-44.8986073441978,-44.8101699486746,-44.7218235054764,-44.6300261723924,
-44.5417820504863,-44.4535513645502,-44.3653127458263,-44.277044824978,
-44.1886765243367,-44.1002487131756,-44.0116905770728,-43.9874448408046,
-43.898892688725,-43.8104552932019,-43.7221088500039,-43.6303115169199,
-43.5420673950138,-43.4538367090777,-43.3655980903539,-43.2773301695055,
-43.1889618688643,-43.1005340577032,-43.0119759216005,-42.9877301853318,
-42.8991780332522,-42.810740637729,-42.7223941945309,-42.6305968614469,
-42.5423527395408,-42.4541220536047,-42.3658834348808,-42.2776155140324,
-42.1892472133912,-42.1008194022302,-42.0122612661274,-41.9880155298589,
-41.8596383787935,-41.7918608832717),.UNSPECIFIED.);
#472=B_SPLINE_CURVE_WITH_KNOTS('',3,(#68869,#68870,#68871,#68872,#68873,
#68874,#68875,#68876,#68877,#68878),.UNSPECIFIED.,.F.,.F.,(4,1,1,1,1,1,
1,4),(-41.7918572412641,-40.9883008743861,-39.9885862189133,-38.9888715634405,
-37.9891569079676,-36.9894422524948,-35.989727597022,-35.5086755760922),
 .UNSPECIFIED.);
#473=B_SPLINE_CURVE_WITH_KNOTS('',3,(#68880,#68881,#68882,#68883,#68884,
#68885,#68886,#68887,#68888,#68889),.UNSPECIFIED.,.F.,.F.,(4,1,1,1,1,1,
1,4),(-35.5086755760922,-34.9900129415491,-33.9902982860763,-32.9905836306035,
-31.9908689751306,-30.9911543196578,-29.991439664185,-29.2254902689126),
 .UNSPECIFIED.);
#474=B_SPLINE_CURVE_WITH_KNOTS('',3,(#68891,#68892,#68893,#68894,#68895,
#68896,#68897,#68898,#68899,#68900,#68901),.UNSPECIFIED.,.F.,.F.,(4,1,1,
1,1,1,1,1,4),(-29.2254902689126,-28.9917250087121,-27.9920103532393,-26.9922956977665,
-25.9925810422936,-24.9928663868208,-23.993151731348,-22.9934370758751,
-22.942304961733),.UNSPECIFIED.);
#475=B_SPLINE_CURVE_WITH_KNOTS('',3,(#68903,#68904,#68905,#68906,#68907,
#68908,#68909,#68910,#68911,#68912),.UNSPECIFIED.,.F.,.F.,(4,1,1,1,1,1,
1,4),(-22.942304961733,-21.9937224204023,-20.9940077649295,-19.9942931094566,
-18.9945784539838,-17.994863798511,-16.9951491430381,-16.6591270207278),
 .UNSPECIFIED.);
#476=B_SPLINE_CURVE_WITH_KNOTS('',3,(#68914,#68915,#68916,#68917,#68918,
#68919,#68920,#68921,#68922,#68923,#68924,#68925,#68926,#68927,#68928,#68929,
#68930,#68931,#68932,#68933,#68934,#68935,#68936,#68937,#68938,#68939,#68940,
#68941,#68942,#68943,#68944,#68945,#68946,#68947,#68948,#68949,#68950,#68951,
#68952,#68953,#68954,#68955,#68956,#68957,#68958,#68959,#68960,#68961,#68962,
#68963,#68964,#68965,#68966,#68967,#68968,#68969,#68970,#68971,#68972,#68973,
#68974,#68975,#68976,#68977,#68978,#68979,#68980,#68981,#68982,#68983,#68984,
#68985,#68986,#68987,#68988,#68989,#68990,#68991,#68992,#68993,#68994,#68995,
#68996,#68997,#68998,#68999,#69000,#69001,#69002,#69003,#69004,#69005,#69006,
#69007,#69008,#69009,#69010,#69011,#69012,#69013,#69014,#69015,#69016,#69017,
#69018,#69019,#69020,#69021,#69022,#69023,#69024,#69025,#69026,#69027,#69028,
#69029,#69030,#69031,#69032,#69033,#69034,#69035,#69036,#69037,#69038,#69039,
#69040,#69041,#69042,#69043,#69044,#69045,#69046,#69047,#69048,#69049,#69050,
#69051,#69052,#69053,#69054,#69055,#69056,#69057,#69058,#69059,#69060,#69061,
#69062,#69063,#69064,#69065,#69066,#69067,#69068,#69069,#69070,#69071,#69072,
#69073,#69074,#69075,#69076,#69077,#69078,#69079,#69080,#69081,#69082,#69083,
#69084,#69085,#69086,#69087,#69088,#69089,#69090,#69091,#69092,#69093,#69094,
#69095,#69096,#69097,#69098,#69099,#69100,#69101,#69102,#69103,#69104,#69105,
#69106,#69107,#69108,#69109,#69110,#69111,#69112,#69113,#69114,#69115,#69116,
#69117,#69118,#69119,#69120,#69121,#69122,#69123,#69124,#69125,#69126,#69127,
#69128,#69129,#69130,#69131,#69132,#69133,#69134,#69135,#69136,#69137,#69138,
#69139),.UNSPECIFIED.,.F.,.F.,(4,3,3,3,3,3,3,3,3,3,3,3,3,3,3,3,3,3,3,3,
3,3,3,3,3,3,3,3,3,3,3,3,3,3,3,3,3,3,3,3,3,3,3,3,3,3,3,3,3,3,3,3,3,3,3,3,
3,3,3,3,3,3,3,3,3,3,3,3,3,3,3,3,3,3,3,4),(-16.6591196545534,-16.5708987836911,
-16.4826909463111,-16.39447483713,-16.3062291499716,-16.2178775403357,-16.1294664880442,
-16.0409125071688,-15.9954344875653,-15.9068823127741,-15.8184448949747,
-15.7300984299549,-15.6383011052221,-15.55005696275,-15.4618262567426,-15.3735876184608,
-15.2853196785869,-15.1969513597993,-15.1085235309808,-15.0199653780704,
-14.9957198320925,-14.9071675077305,-14.8187299390432,-14.7303833220088,
-14.6385860538351,-14.5503417575066,-14.4621108972267,-14.3738721044216,
-14.2856040099394,-14.1972355372029,-14.1088075546291,-14.0202492494465,
-13.9960051766197,-13.9074534571886,-13.819016494562,-13.7306704840109,
-13.6388729886529,-13.5506292961144,-13.4623990376217,-13.3741608439751,
-13.2858933453935,-13.1975254607428,-13.1090980624374,-13.020540331398,
-12.9962905211468,-12.9077381001238,-12.8193004382952,-12.7309537316963,
-12.6391564984435,-12.5509121219219,-12.4626811850177,-12.3744423192198,
-12.2861741554417,-12.1978056191965,-12.1093775763988,-12.0208192162486,
-11.996575865674,-11.908022720017,-11.8195843246472,-11.7312368765609,-11.639439918266,
-11.5511947852311,-11.4629630875814,-11.3747234576318,-11.2864545271203,
-11.1980852242406,-11.1096564139226,-11.021097290955,-10.9968612102012,
-10.9075004241338,-10.8182598130855,-10.7291189426381,-10.640067321383,
-10.5510692741881,-10.4620920011923,-10.3759343473738),.UNSPECIFIED.);
#477=B_SPLINE_CURVE_WITH_KNOTS('',3,(#69140,#69141,#69142,#69143,#69144,
#69145,#69146,#69147,#69148,#69149),.UNSPECIFIED.,.F.,.F.,(4,1,1,1,1,1,
1,4),(-10.3759267640895,-9.99714655472832,-8.99743189925549,-7.99771724378266,
-6.99800258830983,-5.99828793283699,-4.99857327736416,-4.0927579448374),
 .UNSPECIFIED.);
#478=B_SPLINE_CURVE_WITH_KNOTS('',3,(#69152,#69153,#69154,#69155,#69156,
#69157,#69158,#69159,#69160,#69161,#69162,#69163,#69164,#69165,#69166,#69167,
#69168,#69169,#69170,#69171,#69172,#69173,#69174,#69175,#69176,#69177,#69178,
#69179,#69180,#69181,#69182,#69183,#69184,#69185,#69186,#69187,#69188,#69189,
#69190,#69191,#69192,#69193,#69194,#69195,#69196,#69197,#69198,#69199,#69200,
#69201,#69202,#69203,#69204,#69205,#69206,#69207,#69208,#69209,#69210,#69211,
#69212,#69213,#69214,#69215,#69216,#69217,#69218,#69219,#69220,#69221,#69222,
#69223,#69224,#69225,#69226,#69227,#69228,#69229,#69230,#69231,#69232,#69233,
#69234,#69235,#69236,#69237,#69238,#69239,#69240,#69241,#69242,#69243,#69244,
#69245,#69246,#69247,#69248,#69249,#69250,#69251,#69252,#69253,#69254,#69255,
#69256,#69257,#69258,#69259,#69260,#69261,#69262,#69263,#69264,#69265,#69266,
#69267,#69268,#69269,#69270,#69271,#69272,#69273,#69274,#69275,#69276,#69277,
#69278,#69279,#69280,#69281,#69282,#69283,#69284,#69285,#69286,#69287,#69288,
#69289,#69290,#69291,#69292,#69293,#69294,#69295,#69296,#69297,#69298,#69299,
#69300,#69301,#69302,#69303,#69304,#69305,#69306,#69307,#69308,#69309,#69310,
#69311,#69312,#69313,#69314,#69315,#69316,#69317,#69318,#69319,#69320,#69321,
#69322,#69323,#69324,#69325),.UNSPECIFIED.,.F.,.F.,(4,2,2,2,2,2,2,2,2,2,
2,2,2,2,2,2,2,2,2,2,2,2,2,2,2,2,2,2,2,2,2,2,2,2,2,2,2,2,2,2,2,2,2,2,2,2,
2,2,2,2,2,2,2,2,2,2,2,2,2,2,2,2,2,2,2,2,2,2,2,2,2,2,2,2,2,2,2,2,2,2,2,2,
2,2,2,2,4),(0.00584818159483936,0.0833145403087904,0.119798541190528,0.141538318830421,
0.144170087014775,0.14547429476973,0.14640642714708,0.147387815864638,0.148759121781876,
0.151564746211207,0.17973329450901,0.228089013742081,0.273503294053368,
0.297374946185057,0.300084718010428,0.302053797000991,0.302879679694602,
0.303424952652158,0.304011448637213,0.30484292497825,0.306844998348911,
0.338167487368042,0.363754212317079,0.411681980848662,0.440764683950415,
0.459769203371667,0.462300484273235,0.463574433775327,0.464492643053152,
0.465466495291672,0.466838865743283,0.469683937477996,0.500400276153216,
0.501264789422534,0.574394376789672,0.603104757062347,0.6218330455912,0.624956632985009,
0.625928445141098,0.62653096481541,0.627084504034372,0.627803388533153,
0.629272470720125,0.639037815668281,0.693580567889972,0.753391160794976,
0.770644744200646,0.78401986068556,0.78631853951607,0.787534200465984,0.788531406216088,
0.789535684326634,0.791379603931896,0.797287122663885,0.914564704302383,
0.938494556661125,0.94800309566758,0.949366136088689,0.950050469151676,
0.950598288780364,0.951218819934483,0.952241022135733,0.955622252115452,
1.01353206910293,1.07220338839884,1.09604162916153,1.10812992399944,1.11038272606639,
1.11159650679142,1.11259449467071,1.11361659302962,1.11551456922664,1.12176740763345,
1.22748453082085,1.25144601047151,1.2685531134962,1.27151244538824,1.27246729746659,
1.27306771867178,1.27362609079136,1.2743617612658,1.2758957178046,1.28697388512726,
1.28934319240167,1.29049736874123,1.37002912032471,1.37016181069821),
 .UNSPECIFIED.);
#479=B_SPLINE_CURVE_WITH_KNOTS('',3,(#69329,#69330,#69331,#69332,#69333,
#69334,#69335,#69336,#69337,#69338,#69339,#69340,#69341,#69342,#69343,#69344,
#69345,#69346,#69347,#69348,#69349,#69350,#69351,#69352,#69353,#69354,#69355,
#69356,#69357,#69358,#69359),.UNSPECIFIED.,.F.,.F.,(4,3,3,3,3,3,3,3,3,3,
4),(537.212343764025,537.307206720962,537.401923457098,537.497120543768,
537.591603148533,537.686022182108,537.780399718832,537.876174826739,537.970560964813,
538.067030557636,538.16350015046),.UNSPECIFIED.);
#480=B_SPLINE_CURVE_WITH_KNOTS('',3,(#69360,#69361,#69362,#69363,#69364,
#69365,#69366,#69367,#69368,#69369,#69370,#69371,#69372,#69373,#69374,#69375,
#69376,#69377,#69378,#69379,#69380,#69381,#69382,#69383,#69384,#69385,#69386,
#69387,#69388,#69389,#69390,#69391,#69392,#69393,#69394,#69395,#69396,#69397,
#69398,#69399,#69400,#69401,#69402,#69403,#69404,#69405,#69406,#69407,#69408,
#69409,#69410,#69411,#69412,#69413,#69414,#69415,#69416,#69417,#69418,#69419,
#69420,#69421,#69422,#69423,#69424,#69425,#69426,#69427,#69428,#69429),
 .UNSPECIFIED.,.F.,.F.,(4,3,3,3,3,3,3,3,3,3,3,3,3,3,3,3,3,3,3,3,3,3,3,4),
(535.166163310789,535.259377415355,535.352468125424,535.44546285116,535.538392707924,
535.631289207834,535.724176983089,535.817080652029,535.910084313234,536.003140721908,
536.096351253059,536.164070839515,536.256098879168,536.348000065887,536.439803195721,
536.531542963888,536.623250393304,536.714951321204,536.806671573945,536.898504795489,
536.990395572781,537.082462154414,537.163785494987,537.212343763855),
 .UNSPECIFIED.);
#481=B_SPLINE_CURVE_WITH_KNOTS('',3,(#71562,#71563,#71564,#71565,#71566,
#71567,#71568,#71569,#71570,#71571,#71572,#71573,#71574,#71575,#71576,#71577,
#71578,#71579,#71580,#71581,#71582,#71583,#71584,#71585,#71586,#71587,#71588,
#71589,#71590,#71591,#71592,#71593,#71594,#71595,#71596,#71597,#71598,#71599,
#71600,#71601,#71602,#71603,#71604,#71605,#71606,#71607,#71608,#71609,#71610,
#71611,#71612,#71613,#71614,#71615,#71616,#71617,#71618,#71619,#71620,#71621,
#71622,#71623,#71624,#71625,#71626,#71627,#71628,#71629,#71630,#71631,#71632,
#71633,#71634,#71635,#71636,#71637,#71638,#71639,#71640,#71641,#71642,#71643,
#71644,#71645,#71646,#71647,#71648,#71649,#71650,#71651,#71652,#71653,#71654,
#71655,#71656,#71657,#71658),.UNSPECIFIED.,.F.,.F.,(4,3,3,3,3,3,3,3,3,3,
3,3,3,3,3,3,3,3,3,3,3,3,3,3,3,3,3,3,3,3,3,3,4),(0.,0.024358377757175,0.0606004463391366,
0.0979427454018428,0.135285044464549,0.147496336806586,0.153993564102934,
0.189847058097303,0.225532572426869,0.260944091043929,0.278511116143725,
0.288145210622836,0.295840256144695,0.300686689054012,0.335177193005298,
0.368740608710732,0.4014802918423,0.435215231454813,0.439494929020506,0.47314786573973,
0.507110508987375,0.540835061830413,0.566063267316088,0.571536025515506,
0.576790817926267,0.610135744437123,0.643480670947979,0.652892754403838,
0.658607915903714,0.664640539756856,0.696454722966971,0.727403443102524,
0.744397949170609),.UNSPECIFIED.);
#482=B_SPLINE_CURVE_WITH_KNOTS('',3,(#71659,#71660,#71661,#71662,#71663,
#71664,#71665,#71666,#71667,#71668,#71669,#71670,#71671,#71672,#71673,#71674,
#71675,#71676,#71677,#71678,#71679,#71680,#71681,#71682,#71683,#71684,#71685,
#71686,#71687,#71688,#71689,#71690,#71691,#71692,#71693,#71694,#71695,#71696,
#71697,#71698,#71699,#71700,#71701,#71702,#71703,#71704,#71705,#71706,#71707,
#71708,#71709,#71710,#71711,#71712,#71713,#71714,#71715,#71716,#71717,#71718,
#71719,#71720,#71721,#71722,#71723,#71724,#71725,#71726,#71727,#71728,#71729,
#71730,#71731,#71732,#71733,#71734,#71735,#71736,#71737,#71738,#71739,#71740,
#71741,#71742,#71743,#71744,#71745,#71746,#71747,#71748,#71749,#71750,#71751,
#71752),.UNSPECIFIED.,.F.,.F.,(4,3,3,3,3,3,3,3,3,3,3,3,3,3,3,3,3,3,3,3,
3,3,3,3,3,3,3,3,3,3,3,4),(0.,0.0201115232403622,0.0509103820036684,0.0827015579379697,
0.114480781419795,0.125233641024824,0.130996774529478,0.163645515795945,
0.196840351068161,0.230356207922839,0.247143998849504,0.25945135865808,
0.263664864268182,0.298048672203931,0.332324436198921,0.364116142924617,
0.387688307017233,0.395015510154993,0.401768807630668,0.435672330857666,
0.47020591900154,0.50544680147227,0.534532831369196,0.540976992820617,0.546669086825655,
0.582618106602,0.618832117278038,0.635189667272764,0.64457122033922,0.681413970877714,
0.717779744788314,0.741270768406475),.UNSPECIFIED.);
#483=B_SPLINE_CURVE_WITH_KNOTS('',3,(#73886,#73887,#73888,#73889,#73890,
#73891,#73892,#73893,#73894,#73895,#73896,#73897,#73898,#73899,#73900,#73901,
#73902,#73903,#73904,#73905,#73906,#73907,#73908,#73909,#73910,#73911,#73912,
#73913,#73914,#73915,#73916,#73917,#73918,#73919,#73920,#73921,#73922,#73923,
#73924,#73925,#73926,#73927,#73928,#73929,#73930,#73931,#73932,#73933,#73934,
#73935,#73936,#73937,#73938,#73939,#73940,#73941,#73942,#73943,#73944,#73945,
#73946,#73947,#73948,#73949,#73950,#73951,#73952,#73953,#73954,#73955,#73956,
#73957,#73958,#73959,#73960,#73961,#73962,#73963,#73964,#73965,#73966,#73967,
#73968,#73969,#73970,#73971,#73972,#73973,#73974,#73975,#73976,#73977,#73978,
#73979),.UNSPECIFIED.,.F.,.F.,(4,3,3,3,3,3,3,3,3,3,3,3,3,3,3,3,3,3,3,3,
3,3,3,3,3,3,3,3,3,3,3,4),(0.,0.0201115232402943,0.0509103821130776,0.0827015580720687,
0.114480781418801,0.125233641028996,0.130996774690604,0.163535076161932,
0.196984384449669,0.230433692737407,0.247143999010811,0.259451358570654,
0.265189960467916,0.299585032738881,0.333849079024935,0.364116142924638,
0.387688307017256,0.39501551015294,0.401768807899556,0.435672331184667,
0.470205918898849,0.505446801388904,0.534532831632145,0.540976995161682,
0.546669087389317,0.582793053609079,0.618874393635674,0.635189668141087,
0.644571220279675,0.681413970914885,0.717779744663936,0.741270768406529),
 .UNSPECIFIED.);
#484=B_SPLINE_CURVE_WITH_KNOTS('',3,(#73980,#73981,#73982,#73983),
 .UNSPECIFIED.,.F.,.F.,(4,4),(0.,0.0151734474062035),.UNSPECIFIED.);
#485=B_SPLINE_CURVE_WITH_KNOTS('',3,(#73984,#73985,#73986,#73987,#73988,
#73989,#73990,#73991,#73992,#73993,#73994,#73995,#73996,#73997,#73998,#73999,
#74000,#74001,#74002,#74003,#74004,#74005,#74006,#74007,#74008,#74009,#74010,
#74011,#74012,#74013,#74014,#74015,#74016,#74017,#74018,#74019,#74020,#74021,
#74022,#74023,#74024,#74025,#74026,#74027,#74028,#74029,#74030,#74031,#74032,
#74033,#74034,#74035,#74036,#74037,#74038,#74039,#74040,#74041,#74042,#74043,
#74044,#74045,#74046,#74047,#74048,#74049,#74050,#74051,#74052,#74053,#74054,
#74055,#74056,#74057,#74058,#74059,#74060,#74061,#74062,#74063,#74064,#74065,
#74066,#74067,#74068,#74069,#74070,#74071,#74072,#74073,#74074,#74075,#74076,
#74077,#74078,#74079,#74080),.UNSPECIFIED.,.F.,.F.,(4,3,3,3,3,3,3,3,3,3,
3,3,3,3,3,3,3,3,3,3,3,3,3,3,3,3,3,3,3,3,3,3,4),(0.,0.0243583777572955,0.0606004463128303,
0.0979427454027436,0.135285044492657,0.147496336813618,0.153993563998701,
0.189887631727371,0.225706497374811,0.260756281969611,0.288145210372972,
0.295840255200718,0.300686688874331,0.335177192775901,0.368740608421313,
0.401480291842367,0.422912645425388,0.435215231449938,0.439494929180684,
0.473147865916593,0.50711050909266,0.540835061994793,0.566063267486325,
0.571536022966052,0.576790817150764,0.609861602079571,0.642320376686977,
0.652892753239362,0.658607918910948,0.664640540296814,0.69645472327343,
0.727403443285381,0.744397949170614),.UNSPECIFIED.);
#486=SHAPE_REPRESENTATION_RELATIONSHIP('SRR','None',#74128,#490);
#487=SHAPE_REPRESENTATION_RELATIONSHIP('SRR','None',#74129,#491);
#488=SHAPE_REPRESENTATION_RELATIONSHIP('SRR','None',#74130,#492);
#489=SHAPE_REPRESENTATION_RELATIONSHIP('SRR','None',#74131,#493);
#490=ADVANCED_BREP_SHAPE_REPRESENTATION('',(#498),#74099);
#491=ADVANCED_BREP_SHAPE_REPRESENTATION('',(#499),#74100);
#492=ADVANCED_BREP_SHAPE_REPRESENTATION('',(#500),#74101);
#493=ADVANCED_BREP_SHAPE_REPRESENTATION('',(#501),#74102);
#494=STYLED_ITEM('',(#74157),#498);
#495=STYLED_ITEM('',(#74157),#499);
#496=STYLED_ITEM('',(#74158),#500);
#497=STYLED_ITEM('',(#74159),#501);
#498=MANIFOLD_SOLID_BREP('Body1',#4573);
#499=MANIFOLD_SOLID_BREP('Body1',#4574);
#500=MANIFOLD_SOLID_BREP('Body1',#4575);
#501=MANIFOLD_SOLID_BREP('Body1',#4576);
#502=TOROIDAL_SURFACE('',#4660,4.5,0.5);
#503=TOROIDAL_SURFACE('',#4667,4.5,0.5);
#504=TOROIDAL_SURFACE('',#4674,4.5,0.5);
#505=TOROIDAL_SURFACE('',#4681,20.5,0.5);
#506=TOROIDAL_SURFACE('',#4686,4.5,0.5);
#507=TOROIDAL_SURFACE('',#4716,4.5,0.5);
#508=TOROIDAL_SURFACE('',#4718,4.5,0.5);
#509=TOROIDAL_SURFACE('',#4720,4.5,0.5);
#510=TOROIDAL_SURFACE('',#4722,20.5,0.5);
#511=TOROIDAL_SURFACE('',#4724,4.5,0.5);
#512=TOROIDAL_SURFACE('',#4736,4.5,0.5);
#513=TOROIDAL_SURFACE('',#4747,4.5,0.5);
#514=TOROIDAL_SURFACE('',#4753,4.5,0.5);
#515=TOROIDAL_SURFACE('',#4759,20.5,0.5);
#516=TOROIDAL_SURFACE('',#4761,4.5,0.5);
#517=TOROIDAL_SURFACE('',#4791,4.5,0.5);
#518=TOROIDAL_SURFACE('',#4799,4.5,0.5);
#519=TOROIDAL_SURFACE('',#4801,20.5,0.5);
#520=TOROIDAL_SURFACE('',#4803,4.5,0.5);
#521=TOROIDAL_SURFACE('',#4821,4.5,0.5);
#522=TOROIDAL_SURFACE('',#4828,19.9,0.400000000000003);
#523=TOROIDAL_SURFACE('',#4833,20.1,0.399999999999996);
#524=TOROIDAL_SURFACE('',#4838,20.1,0.399999999999998);
#525=TOROIDAL_SURFACE('',#4843,19.9,0.400000000000003);
#526=ELLIPSE('',#4635,0.541196100146199,0.5);
#527=ELLIPSE('',#4636,0.541196100146197,0.5);
#528=ELLIPSE('',#4638,0.541196100146197,0.5);
#529=ELLIPSE('',#4640,0.541196100146199,0.5);
#530=ELLIPSE('',#4642,0.541196100146199,0.5);
#531=ELLIPSE('',#4643,0.541196100146197,0.5);
#532=ELLIPSE('',#4645,0.541196100146197,0.5);
#533=ELLIPSE('',#4648,0.541196100146199,0.5);
#534=ELLIPSE('',#4694,0.541196100146197,0.5);
#535=ELLIPSE('',#4695,0.541196100146197,0.5);
#536=ELLIPSE('',#4697,0.541196100146197,0.5);
#537=ELLIPSE('',#4699,0.541196100146197,0.5);
#538=ELLIPSE('',#4701,0.541196100146197,0.5);
#539=ELLIPSE('',#4703,0.541196100146197,0.5);
#540=ELLIPSE('',#4705,0.541196100146197,0.5);
#541=ELLIPSE('',#4707,0.541196100146197,0.5);
#542=ELLIPSE('',#4768,0.541196100146197,0.5);
#543=ELLIPSE('',#4769,0.541196100146199,0.5);
#544=ELLIPSE('',#4771,0.541196100146199,0.5);
#545=ELLIPSE('',#4773,0.541196100146197,0.5);
#546=ELLIPSE('',#4775,0.541196100146197,0.5);
#547=ELLIPSE('',#4776,0.541196100146197,0.5);
#548=ELLIPSE('',#4778,0.541196100146199,0.5);
#549=ELLIPSE('',#4781,0.541196100146197,0.5);
#550=ELLIPSE('',#4806,0.541196100146197,0.5);
#551=ELLIPSE('',#4807,0.541196100146198,0.5);
#552=ELLIPSE('',#4809,0.541196100146198,0.5);
#553=ELLIPSE('',#4811,0.541196100146197,0.5);
#554=ELLIPSE('',#4813,0.541196100146197,0.5);
#555=ELLIPSE('',#4814,0.541196100146197,0.5);
#556=ELLIPSE('',#4816,0.541196100146198,0.5);
#557=ELLIPSE('',#4819,0.541196100146197,0.5);
#558=FACE_BOUND('',#800,.T.);
#559=FACE_BOUND('',#802,.T.);
#560=FACE_BOUND('',#817,.T.);
#561=FACE_BOUND('',#818,.T.);
#562=FACE_BOUND('',#819,.T.);
#563=FACE_BOUND('',#820,.T.);
#564=FACE_BOUND('',#821,.T.);
#565=FACE_BOUND('',#842,.T.);
#566=FACE_BOUND('',#843,.T.);
#567=FACE_BOUND('',#844,.T.);
#568=FACE_BOUND('',#845,.T.);
#569=FACE_BOUND('',#846,.T.);
#570=FACE_BOUND('',#856,.T.);
#571=FACE_BOUND('',#858,.T.);
#572=FACE_BOUND('',#861,.T.);
#573=FACE_BOUND('',#862,.T.);
#574=FACE_BOUND('',#863,.T.);
#575=FACE_BOUND('',#864,.T.);
#576=FACE_BOUND('',#865,.T.);
#577=FACE_BOUND('',#892,.T.);
#578=FACE_BOUND('',#893,.T.);
#579=FACE_BOUND('',#894,.T.);
#580=FACE_BOUND('',#895,.T.);
#581=FACE_BOUND('',#896,.T.);
#582=FACE_BOUND('',#913,.T.);
#583=FACE_BOUND('',#918,.T.);
#584=PLANE('',#4627);
#585=PLANE('',#4629);
#586=PLANE('',#4650);
#587=PLANE('',#4651);
#588=PLANE('',#4652);
#589=PLANE('',#4653);
#590=PLANE('',#4654);
#591=PLANE('',#4709);
#592=PLANE('',#4710);
#593=PLANE('',#4726);
#594=PLANE('',#4727);
#595=PLANE('',#4728);
#596=PLANE('',#4730);
#597=PLANE('',#4733);
#598=PLANE('',#4740);
#599=PLANE('',#4783);
#600=PLANE('',#4784);
#601=PLANE('',#4785);
#602=PLANE('',#4786);
#603=PLANE('',#4787);
#604=PLANE('',#4788);
#605=PLANE('',#4789);
#606=PLANE('',#4790);
#607=PLANE('',#4794);
#608=PLANE('',#4831);
#609=PLANE('',#4841);
#610=PLANE('',#4936);
#611=PLANE('',#4937);
#612=FACE_OUTER_BOUND('',#798,.T.);
#613=FACE_OUTER_BOUND('',#799,.T.);
#614=FACE_OUTER_BOUND('',#801,.T.);
#615=FACE_OUTER_BOUND('',#803,.T.);
#616=FACE_OUTER_BOUND('',#804,.T.);
#617=FACE_OUTER_BOUND('',#805,.T.);
#618=FACE_OUTER_BOUND('',#806,.T.);
#619=FACE_OUTER_BOUND('',#807,.T.);
#620=FACE_OUTER_BOUND('',#808,.T.);
#621=FACE_OUTER_BOUND('',#809,.T.);
#622=FACE_OUTER_BOUND('',#810,.T.);
#623=FACE_OUTER_BOUND('',#811,.T.);
#624=FACE_OUTER_BOUND('',#812,.T.);
#625=FACE_OUTER_BOUND('',#813,.T.);
#626=FACE_OUTER_BOUND('',#814,.T.);
#627=FACE_OUTER_BOUND('',#815,.T.);
#628=FACE_OUTER_BOUND('',#816,.T.);
#629=FACE_OUTER_BOUND('',#822,.T.);
#630=FACE_OUTER_BOUND('',#823,.T.);
#631=FACE_OUTER_BOUND('',#824,.T.);
#632=FACE_OUTER_BOUND('',#825,.T.);
#633=FACE_OUTER_BOUND('',#826,.T.);
#634=FACE_OUTER_BOUND('',#827,.T.);
#635=FACE_OUTER_BOUND('',#828,.T.);
#636=FACE_OUTER_BOUND('',#829,.T.);
#637=FACE_OUTER_BOUND('',#830,.T.);
#638=FACE_OUTER_BOUND('',#831,.T.);
#639=FACE_OUTER_BOUND('',#832,.T.);
#640=FACE_OUTER_BOUND('',#833,.T.);
#641=FACE_OUTER_BOUND('',#834,.T.);
#642=FACE_OUTER_BOUND('',#835,.T.);
#643=FACE_OUTER_BOUND('',#836,.T.);
#644=FACE_OUTER_BOUND('',#837,.T.);
#645=FACE_OUTER_BOUND('',#838,.T.);
#646=FACE_OUTER_BOUND('',#839,.T.);
#647=FACE_OUTER_BOUND('',#840,.T.);
#648=FACE_OUTER_BOUND('',#841,.T.);
#649=FACE_OUTER_BOUND('',#847,.T.);
#650=FACE_OUTER_BOUND('',#848,.T.);
#651=FACE_OUTER_BOUND('',#849,.T.);
#652=FACE_OUTER_BOUND('',#850,.T.);
#653=FACE_OUTER_BOUND('',#851,.T.);
#654=FACE_OUTER_BOUND('',#852,.T.);
#655=FACE_OUTER_BOUND('',#853,.T.);
#656=FACE_OUTER_BOUND('',#854,.T.);
#657=FACE_OUTER_BOUND('',#855,.T.);
#658=FACE_OUTER_BOUND('',#857,.T.);
#659=FACE_OUTER_BOUND('',#859,.T.);
#660=FACE_OUTER_BOUND('',#860,.T.);
#661=FACE_OUTER_BOUND('',#866,.T.);
#662=FACE_OUTER_BOUND('',#867,.T.);
#663=FACE_OUTER_BOUND('',#868,.T.);
#664=FACE_OUTER_BOUND('',#869,.T.);
#665=FACE_OUTER_BOUND('',#870,.T.);
#666=FACE_OUTER_BOUND('',#871,.T.);
#667=FACE_OUTER_BOUND('',#872,.T.);
#668=FACE_OUTER_BOUND('',#873,.T.);
#669=FACE_OUTER_BOUND('',#874,.T.);
#670=FACE_OUTER_BOUND('',#875,.T.);
#671=FACE_OUTER_BOUND('',#876,.T.);
#672=FACE_OUTER_BOUND('',#877,.T.);
#673=FACE_OUTER_BOUND('',#878,.T.);
#674=FACE_OUTER_BOUND('',#879,.T.);
#675=FACE_OUTER_BOUND('',#880,.T.);
#676=FACE_OUTER_BOUND('',#881,.T.);
#677=FACE_OUTER_BOUND('',#882,.T.);
#678=FACE_OUTER_BOUND('',#883,.T.);
#679=FACE_OUTER_BOUND('',#884,.T.);
#680=FACE_OUTER_BOUND('',#885,.T.);
#681=FACE_OUTER_BOUND('',#886,.T.);
#682=FACE_OUTER_BOUND('',#887,.T.);
#683=FACE_OUTER_BOUND('',#888,.T.);
#684=FACE_OUTER_BOUND('',#889,.T.);
#685=FACE_OUTER_BOUND('',#890,.T.);
#686=FACE_OUTER_BOUND('',#891,.T.);
#687=FACE_OUTER_BOUND('',#897,.T.);
#688=FACE_OUTER_BOUND('',#898,.T.);
#689=FACE_OUTER_BOUND('',#899,.T.);
#690=FACE_OUTER_BOUND('',#900,.T.);
#691=FACE_OUTER_BOUND('',#901,.T.);
#692=FACE_OUTER_BOUND('',#902,.T.);
#693=FACE_OUTER_BOUND('',#903,.T.);
#694=FACE_OUTER_BOUND('',#904,.T.);
#695=FACE_OUTER_BOUND('',#905,.T.);
#696=FACE_OUTER_BOUND('',#906,.T.);
#697=FACE_OUTER_BOUND('',#907,.T.);
#698=FACE_OUTER_BOUND('',#908,.T.);
#699=FACE_OUTER_BOUND('',#909,.T.);
#700=FACE_OUTER_BOUND('',#910,.T.);
#701=FACE_OUTER_BOUND('',#911,.T.);
#702=FACE_OUTER_BOUND('',#912,.T.);
#703=FACE_OUTER_BOUND('',#914,.T.);
#704=FACE_OUTER_BOUND('',#915,.T.);
#705=FACE_OUTER_BOUND('',#916,.T.);
#706=FACE_OUTER_BOUND('',#917,.T.);
#707=FACE_OUTER_BOUND('',#919,.T.);
#708=FACE_OUTER_BOUND('',#920,.T.);
#709=FACE_OUTER_BOUND('',#921,.T.);
#710=FACE_OUTER_BOUND('',#922,.T.);
#711=FACE_OUTER_BOUND('',#923,.T.);
#712=FACE_OUTER_BOUND('',#924,.T.);
#713=FACE_OUTER_BOUND('',#925,.T.);
#714=FACE_OUTER_BOUND('',#926,.T.);
#715=FACE_OUTER_BOUND('',#927,.T.);
#716=FACE_OUTER_BOUND('',#928,.T.);
#717=FACE_OUTER_BOUND('',#929,.T.);
#718=FACE_OUTER_BOUND('',#930,.T.);
#719=FACE_OUTER_BOUND('',#931,.T.);
#720=FACE_OUTER_BOUND('',#932,.T.);
#721=FACE_OUTER_BOUND('',#933,.T.);
#722=FACE_OUTER_BOUND('',#934,.T.);
#723=FACE_OUTER_BOUND('',#935,.T.);
#724=FACE_OUTER_BOUND('',#936,.T.);
#725=FACE_OUTER_BOUND('',#937,.T.);
#726=FACE_OUTER_BOUND('',#938,.T.);
#727=FACE_OUTER_BOUND('',#939,.T.);
#728=FACE_OUTER_BOUND('',#940,.T.);
#729=FACE_OUTER_BOUND('',#941,.T.);
#730=FACE_OUTER_BOUND('',#942,.T.);
#731=FACE_OUTER_BOUND('',#943,.T.);
#732=FACE_OUTER_BOUND('',#944,.T.);
#733=FACE_OUTER_BOUND('',#945,.T.);
#734=FACE_OUTER_BOUND('',#946,.T.);
#735=FACE_OUTER_BOUND('',#947,.T.);
#736=FACE_OUTER_BOUND('',#948,.T.);
#737=FACE_OUTER_BOUND('',#949,.T.);
#738=FACE_OUTER_BOUND('',#950,.T.);
#739=FACE_OUTER_BOUND('',#951,.T.);
#740=FACE_OUTER_BOUND('',#952,.T.);
#741=FACE_OUTER_BOUND('',#953,.T.);
#742=FACE_OUTER_BOUND('',#954,.T.);
#743=FACE_OUTER_BOUND('',#955,.T.);
#744=FACE_OUTER_BOUND('',#956,.T.);
#745=FACE_OUTER_BOUND('',#957,.T.);
#746=FACE_OUTER_BOUND('',#958,.T.);
#747=FACE_OUTER_BOUND('',#959,.T.);
#748=FACE_OUTER_BOUND('',#960,.T.);
#749=FACE_OUTER_BOUND('',#961,.T.);
#750=FACE_OUTER_BOUND('',#962,.T.);
#751=FACE_OUTER_BOUND('',#963,.T.);
#752=FACE_OUTER_BOUND('',#964,.T.);
#753=FACE_OUTER_BOUND('',#965,.T.);
#754=FACE_OUTER_BOUND('',#966,.T.);
#755=FACE_OUTER_BOUND('',#967,.T.);
#756=FACE_OUTER_BOUND('',#968,.T.);
#757=FACE_OUTER_BOUND('',#969,.T.);
#758=FACE_OUTER_BOUND('',#970,.T.);
#759=FACE_OUTER_BOUND('',#971,.T.);
#760=FACE_OUTER_BOUND('',#972,.T.);
#761=FACE_OUTER_BOUND('',#973,.T.);
#762=FACE_OUTER_BOUND('',#974,.T.);
#763=FACE_OUTER_BOUND('',#975,.T.);
#764=FACE_OUTER_BOUND('',#976,.T.);
#765=FACE_OUTER_BOUND('',#977,.T.);
#766=FACE_OUTER_BOUND('',#978,.T.);
#767=FACE_OUTER_BOUND('',#979,.T.);
#768=FACE_OUTER_BOUND('',#980,.T.);
#769=FACE_OUTER_BOUND('',#981,.T.);
#770=FACE_OUTER_BOUND('',#982,.T.);
#771=FACE_OUTER_BOUND('',#983,.T.);
#772=FACE_OUTER_BOUND('',#984,.T.);
#773=FACE_OUTER_BOUND('',#985,.T.);
#774=FACE_OUTER_BOUND('',#986,.T.);
#775=FACE_OUTER_BOUND('',#987,.T.);
#776=FACE_OUTER_BOUND('',#988,.T.);
#777=FACE_OUTER_BOUND('',#989,.T.);
#778=FACE_OUTER_BOUND('',#990,.T.);
#779=FACE_OUTER_BOUND('',#991,.T.);
#780=FACE_OUTER_BOUND('',#992,.T.);
#781=FACE_OUTER_BOUND('',#993,.T.);
#782=FACE_OUTER_BOUND('',#994,.T.);
#783=FACE_OUTER_BOUND('',#995,.T.);
#784=FACE_OUTER_BOUND('',#996,.T.);
#785=FACE_OUTER_BOUND('',#997,.T.);
#786=FACE_OUTER_BOUND('',#998,.T.);
#787=FACE_OUTER_BOUND('',#999,.T.);
#788=FACE_OUTER_BOUND('',#1000,.T.);
#789=FACE_OUTER_BOUND('',#1001,.T.);
#790=FACE_OUTER_BOUND('',#1002,.T.);
#791=FACE_OUTER_BOUND('',#1003,.T.);
#792=FACE_OUTER_BOUND('',#1004,.T.);
#793=FACE_OUTER_BOUND('',#1005,.T.);
#794=FACE_OUTER_BOUND('',#1006,.T.);
#795=FACE_OUTER_BOUND('',#1007,.T.);
#796=FACE_OUTER_BOUND('',#1008,.T.);
#797=FACE_OUTER_BOUND('',#1009,.T.);
#798=EDGE_LOOP('',(#2771,#2772,#2773,#2774));
#799=EDGE_LOOP('',(#2775));
#800=EDGE_LOOP('',(#2776));
#801=EDGE_LOOP('',(#2777));
#802=EDGE_LOOP('',(#2778));
#803=EDGE_LOOP('',(#2779,#2780,#2781,#2782,#2783));
#804=EDGE_LOOP('',(#2784,#2785,#2786,#2787));
#805=EDGE_LOOP('',(#2788,#2789,#2790,#2791));
#806=EDGE_LOOP('',(#2792,#2793,#2794,#2795));
#807=EDGE_LOOP('',(#2796,#2797,#2798,#2799));
#808=EDGE_LOOP('',(#2800,#2801,#2802,#2803));
#809=EDGE_LOOP('',(#2804,#2805,#2806,#2807));
#810=EDGE_LOOP('',(#2808,#2809,#2810,#2811));
#811=EDGE_LOOP('',(#2812,#2813,#2814,#2815));
#812=EDGE_LOOP('',(#2816,#2817,#2818,#2819));
#813=EDGE_LOOP('',(#2820,#2821,#2822,#2823));
#814=EDGE_LOOP('',(#2824,#2825,#2826,#2827));
#815=EDGE_LOOP('',(#2828,#2829,#2830,#2831));
#816=EDGE_LOOP('',(#2832,#2833,#2834,#2835,#2836,#2837,#2838,#2839));
#817=EDGE_LOOP('',(#2840));
#818=EDGE_LOOP('',(#2841));
#819=EDGE_LOOP('',(#2842));
#820=EDGE_LOOP('',(#2843));
#821=EDGE_LOOP('',(#2844));
#822=EDGE_LOOP('',(#2845,#2846,#2847,#2848,#2849));
#823=EDGE_LOOP('',(#2850,#2851,#2852,#2853,#2854,#2855));
#824=EDGE_LOOP('',(#2856,#2857,#2858,#2859,#2860));
#825=EDGE_LOOP('',(#2861,#2862,#2863,#2864,#2865,#2866));
#826=EDGE_LOOP('',(#2867,#2868,#2869,#2870,#2871));
#827=EDGE_LOOP('',(#2872,#2873,#2874,#2875,#2876,#2877));
#828=EDGE_LOOP('',(#2878,#2879,#2880,#2881,#2882));
#829=EDGE_LOOP('',(#2883,#2884,#2885,#2886,#2887));
#830=EDGE_LOOP('',(#2888,#2889,#2890,#2891,#2892));
#831=EDGE_LOOP('',(#2893,#2894,#2895,#2896,#2897,#2898));
#832=EDGE_LOOP('',(#2899,#2900,#2901,#2902));
#833=EDGE_LOOP('',(#2903,#2904,#2905,#2906));
#834=EDGE_LOOP('',(#2907,#2908,#2909,#2910));
#835=EDGE_LOOP('',(#2911,#2912,#2913,#2914));
#836=EDGE_LOOP('',(#2915,#2916,#2917,#2918));
#837=EDGE_LOOP('',(#2919,#2920,#2921,#2922));
#838=EDGE_LOOP('',(#2923,#2924,#2925,#2926));
#839=EDGE_LOOP('',(#2927,#2928,#2929,#2930));
#840=EDGE_LOOP('',(#2931,#2932,#2933,#2934));
#841=EDGE_LOOP('',(#2935,#2936,#2937,#2938,#2939,#2940,#2941,#2942));
#842=EDGE_LOOP('',(#2943));
#843=EDGE_LOOP('',(#2944));
#844=EDGE_LOOP('',(#2945));
#845=EDGE_LOOP('',(#2946));
#846=EDGE_LOOP('',(#2947));
#847=EDGE_LOOP('',(#2948,#2949,#2950,#2951,#2952));
#848=EDGE_LOOP('',(#2953,#2954,#2955,#2956,#2957));
#849=EDGE_LOOP('',(#2958,#2959,#2960,#2961,#2962));
#850=EDGE_LOOP('',(#2963,#2964,#2965,#2966,#2967));
#851=EDGE_LOOP('',(#2968,#2969,#2970,#2971,#2972));
#852=EDGE_LOOP('',(#2973,#2974,#2975,#2976));
#853=EDGE_LOOP('',(#2977,#2978,#2979,#2980));
#854=EDGE_LOOP('',(#2981,#2982,#2983,#2984));
#855=EDGE_LOOP('',(#2985));
#856=EDGE_LOOP('',(#2986));
#857=EDGE_LOOP('',(#2987));
#858=EDGE_LOOP('',(#2988));
#859=EDGE_LOOP('',(#2989,#2990,#2991,#2992));
#860=EDGE_LOOP('',(#2993,#2994,#2995,#2996,#2997,#2998,#2999,#3000));
#861=EDGE_LOOP('',(#3001));
#862=EDGE_LOOP('',(#3002));
#863=EDGE_LOOP('',(#3003));
#864=EDGE_LOOP('',(#3004));
#865=EDGE_LOOP('',(#3005));
#866=EDGE_LOOP('',(#3006,#3007,#3008,#3009));
#867=EDGE_LOOP('',(#3010,#3011,#3012,#3013));
#868=EDGE_LOOP('',(#3014,#3015,#3016,#3017,#3018));
#869=EDGE_LOOP('',(#3019,#3020,#3021,#3022));
#870=EDGE_LOOP('',(#3023,#3024,#3025,#3026,#3027));
#871=EDGE_LOOP('',(#3028,#3029,#3030,#3031));
#872=EDGE_LOOP('',(#3032,#3033,#3034,#3035));
#873=EDGE_LOOP('',(#3036,#3037,#3038,#3039,#3040));
#874=EDGE_LOOP('',(#3041,#3042,#3043,#3044));
#875=EDGE_LOOP('',(#3045,#3046,#3047,#3048));
#876=EDGE_LOOP('',(#3049,#3050,#3051,#3052));
#877=EDGE_LOOP('',(#3053,#3054,#3055,#3056));
#878=EDGE_LOOP('',(#3057,#3058,#3059,#3060));
#879=EDGE_LOOP('',(#3061,#3062,#3063,#3064));
#880=EDGE_LOOP('',(#3065,#3066,#3067,#3068));
#881=EDGE_LOOP('',(#3069,#3070,#3071,#3072));
#882=EDGE_LOOP('',(#3073,#3074,#3075,#3076));
#883=EDGE_LOOP('',(#3077,#3078,#3079,#3080));
#884=EDGE_LOOP('',(#3081,#3082,#3083,#3084));
#885=EDGE_LOOP('',(#3085,#3086,#3087,#3088));
#886=EDGE_LOOP('',(#3089,#3090,#3091,#3092));
#887=EDGE_LOOP('',(#3093,#3094,#3095,#3096));
#888=EDGE_LOOP('',(#3097,#3098,#3099,#3100));
#889=EDGE_LOOP('',(#3101,#3102,#3103,#3104));
#890=EDGE_LOOP('',(#3105,#3106,#3107,#3108,#3109));
#891=EDGE_LOOP('',(#3110,#3111,#3112,#3113,#3114,#3115,#3116,#3117));
#892=EDGE_LOOP('',(#3118));
#893=EDGE_LOOP('',(#3119));
#894=EDGE_LOOP('',(#3120));
#895=EDGE_LOOP('',(#3121));
#896=EDGE_LOOP('',(#3122));
#897=EDGE_LOOP('',(#3123,#3124,#3125,#3126,#3127));
#898=EDGE_LOOP('',(#3128,#3129,#3130,#3131));
#899=EDGE_LOOP('',(#3132,#3133,#3134,#3135,#3136));
#900=EDGE_LOOP('',(#3137,#3138,#3139,#3140));
#901=EDGE_LOOP('',(#3141,#3142,#3143,#3144));
#902=EDGE_LOOP('',(#3145,#3146,#3147,#3148));
#903=EDGE_LOOP('',(#3149,#3150,#3151,#3152));
#904=EDGE_LOOP('',(#3153,#3154,#3155,#3156));
#905=EDGE_LOOP('',(#3157,#3158,#3159,#3160));
#906=EDGE_LOOP('',(#3161,#3162,#3163,#3164));
#907=EDGE_LOOP('',(#3165,#3166,#3167,#3168));
#908=EDGE_LOOP('',(#3169,#3170,#3171,#3172));
#909=EDGE_LOOP('',(#3173,#3174,#3175,#3176));
#910=EDGE_LOOP('',(#3177,#3178,#3179,#3180));
#911=EDGE_LOOP('',(#3181,#3182,#3183,#3184));
#912=EDGE_LOOP('',(#3185));
#913=EDGE_LOOP('',(#3186));
#914=EDGE_LOOP('',(#3187,#3188,#3189,#3190));
#915=EDGE_LOOP('',(#3191,#3192,#3193,#3194));
#916=EDGE_LOOP('',(#3195,#3196,#3197,#3198));
#917=EDGE_LOOP('',(#3199));
#918=EDGE_LOOP('',(#3200));
#919=EDGE_LOOP('',(#3201,#3202,#3203,#3204));
#920=EDGE_LOOP('',(#3205,#3206,#3207,#3208));
#921=EDGE_LOOP('',(#3209,#3210,#3211,#3212,#3213,#3214));
#922=EDGE_LOOP('',(#3215,#3216,#3217,#3218));
#923=EDGE_LOOP('',(#3219,#3220,#3221,#3222,#3223,#3224));
#924=EDGE_LOOP('',(#3225,#3226,#3227,#3228));
#925=EDGE_LOOP('',(#3229,#3230,#3231,#3232,#3233,#3234));
#926=EDGE_LOOP('',(#3235,#3236,#3237,#3238));
#927=EDGE_LOOP('',(#3239,#3240,#3241,#3242,#3243,#3244));
#928=EDGE_LOOP('',(#3245,#3246,#3247,#3248));
#929=EDGE_LOOP('',(#3249,#3250,#3251,#3252,#3253,#3254));
#930=EDGE_LOOP('',(#3255,#3256,#3257,#3258));
#931=EDGE_LOOP('',(#3259,#3260,#3261,#3262,#3263,#3264));
#932=EDGE_LOOP('',(#3265,#3266,#3267,#3268));
#933=EDGE_LOOP('',(#3269,#3270,#3271,#3272,#3273,#3274));
#934=EDGE_LOOP('',(#3275,#3276,#3277,#3278));
#935=EDGE_LOOP('',(#3279,#3280,#3281,#3282,#3283,#3284));
#936=EDGE_LOOP('',(#3285,#3286,#3287,#3288,#3289));
#937=EDGE_LOOP('',(#3290,#3291,#3292,#3293,#3294));
#938=EDGE_LOOP('',(#3295,#3296,#3297,#3298,#3299));
#939=EDGE_LOOP('',(#3300,#3301,#3302,#3303,#3304));
#940=EDGE_LOOP('',(#3305,#3306,#3307,#3308,#3309));
#941=EDGE_LOOP('',(#3310,#3311,#3312,#3313,#3314));
#942=EDGE_LOOP('',(#3315,#3316,#3317,#3318,#3319));
#943=EDGE_LOOP('',(#3320,#3321,#3322,#3323,#3324));
#944=EDGE_LOOP('',(#3325,#3326,#3327,#3328,#3329));
#945=EDGE_LOOP('',(#3330,#3331,#3332,#3333,#3334));
#946=EDGE_LOOP('',(#3335,#3336,#3337,#3338,#3339));
#947=EDGE_LOOP('',(#3340,#3341,#3342,#3343,#3344));
#948=EDGE_LOOP('',(#3345,#3346,#3347,#3348,#3349));
#949=EDGE_LOOP('',(#3350,#3351,#3352,#3353,#3354));
#950=EDGE_LOOP('',(#3355,#3356,#3357,#3358,#3359));
#951=EDGE_LOOP('',(#3360,#3361,#3362,#3363,#3364));
#952=EDGE_LOOP('',(#3365,#3366,#3367,#3368,#3369));
#953=EDGE_LOOP('',(#3370,#3371,#3372,#3373,#3374));
#954=EDGE_LOOP('',(#3375,#3376,#3377,#3378,#3379));
#955=EDGE_LOOP('',(#3380,#3381,#3382,#3383,#3384));
#956=EDGE_LOOP('',(#3385,#3386,#3387,#3388,#3389));
#957=EDGE_LOOP('',(#3390,#3391,#3392,#3393,#3394,#3395));
#958=EDGE_LOOP('',(#3396,#3397,#3398,#3399));
#959=EDGE_LOOP('',(#3400,#3401,#3402,#3403,#3404,#3405));
#960=EDGE_LOOP('',(#3406,#3407,#3408,#3409,#3410));
#961=EDGE_LOOP('',(#3411,#3412,#3413,#3414,#3415));
#962=EDGE_LOOP('',(#3416,#3417,#3418,#3419,#3420));
#963=EDGE_LOOP('',(#3421,#3422,#3423,#3424,#3425));
#964=EDGE_LOOP('',(#3426,#3427,#3428,#3429,#3430,#3431));
#965=EDGE_LOOP('',(#3432,#3433,#3434,#3435,#3436));
#966=EDGE_LOOP('',(#3437,#3438,#3439,#3440,#3441));
#967=EDGE_LOOP('',(#3442,#3443,#3444,#3445,#3446));
#968=EDGE_LOOP('',(#3447,#3448,#3449,#3450,#3451));
#969=EDGE_LOOP('',(#3452,#3453,#3454,#3455,#3456));
#970=EDGE_LOOP('',(#3457,#3458,#3459,#3460,#3461,#3462));
#971=EDGE_LOOP('',(#3463,#3464,#3465,#3466,#3467));
#972=EDGE_LOOP('',(#3468,#3469,#3470,#3471,#3472));
#973=EDGE_LOOP('',(#3473,#3474,#3475,#3476,#3477,#3478));
#974=EDGE_LOOP('',(#3479,#3480,#3481,#3482));
#975=EDGE_LOOP('',(#3483,#3484,#3485,#3486,#3487,#3488));
#976=EDGE_LOOP('',(#3489,#3490,#3491,#3492,#3493));
#977=EDGE_LOOP('',(#3494,#3495,#3496,#3497,#3498));
#978=EDGE_LOOP('',(#3499,#3500,#3501,#3502,#3503));
#979=EDGE_LOOP('',(#3504,#3505,#3506,#3507,#3508));
#980=EDGE_LOOP('',(#3509,#3510,#3511,#3512,#3513));
#981=EDGE_LOOP('',(#3514,#3515,#3516,#3517,#3518));
#982=EDGE_LOOP('',(#3519,#3520,#3521,#3522,#3523));
#983=EDGE_LOOP('',(#3524,#3525,#3526,#3527,#3528));
#984=EDGE_LOOP('',(#3529,#3530,#3531,#3532,#3533));
#985=EDGE_LOOP('',(#3534,#3535,#3536,#3537,#3538));
#986=EDGE_LOOP('',(#3539,#3540,#3541,#3542,#3543));
#987=EDGE_LOOP('',(#3544,#3545,#3546,#3547,#3548));
#988=EDGE_LOOP('',(#3549,#3550,#3551,#3552,#3553));
#989=EDGE_LOOP('',(#3554,#3555,#3556,#3557,#3558));
#990=EDGE_LOOP('',(#3559,#3560,#3561,#3562,#3563,#3564));
#991=EDGE_LOOP('',(#3565,#3566,#3567,#3568,#3569));
#992=EDGE_LOOP('',(#3570,#3571,#3572,#3573,#3574));
#993=EDGE_LOOP('',(#3575,#3576,#3577,#3578,#3579,#3580));
#994=EDGE_LOOP('',(#3581,#3582,#3583,#3584,#3585));
#995=EDGE_LOOP('',(#3586,#3587,#3588,#3589,#3590));
#996=EDGE_LOOP('',(#3591,#3592,#3593,#3594,#3595));
#997=EDGE_LOOP('',(#3596,#3597,#3598,#3599,#3600));
#998=EDGE_LOOP('',(#3601,#3602,#3603,#3604,#3605));
#999=EDGE_LOOP('',(#3606,#3607,#3608,#3609,#3610));
#1000=EDGE_LOOP('',(#3611,#3612,#3613,#3614,#3615));
#1001=EDGE_LOOP('',(#3616,#3617,#3618,#3619,#3620,#3621));
#1002=EDGE_LOOP('',(#3622,#3623,#3624,#3625));
#1003=EDGE_LOOP('',(#3626,#3627,#3628,#3629,#3630,#3631));
#1004=EDGE_LOOP('',(#3632,#3633,#3634,#3635,#3636,#3637,#3638,#3639,#3640,
#3641,#3642,#3643,#3644,#3645,#3646,#3647,#3648,#3649,#3650,#3651,#3652,
#3653,#3654,#3655,#3656,#3657,#3658,#3659,#3660,#3661,#3662,#3663,#3664,
#3665,#3666,#3667,#3668,#3669,#3670,#3671,#3672,#3673,#3674,#3675,#3676,
#3677,#3678,#3679,#3680,#3681,#3682,#3683,#3684,#3685,#3686,#3687,#3688,
#3689,#3690,#3691,#3692,#3693,#3694,#3695,#3696,#3697,#3698,#3699,#3700,
#3701,#3702,#3703,#3704,#3705,#3706,#3707,#3708,#3709,#3710,#3711,#3712,
#3713,#3714,#3715,#3716,#3717,#3718,#3719,#3720,#3721,#3722,#3723,#3724,
#3725,#3726,#3727,#3728,#3729,#3730,#3731,#3732,#3733,#3734,#3735,#3736,
#3737,#3738,#3739,#3740,#3741,#3742,#3743,#3744,#3745,#3746,#3747,#3748,
#3749,#3750,#3751,#3752,#3753,#3754,#3755,#3756,#3757,#3758,#3759,#3760,
#3761,#3762,#3763,#3764,#3765,#3766,#3767,#3768,#3769,#3770,#3771,#3772,
#3773,#3774,#3775,#3776,#3777,#3778,#3779,#3780,#3781,#3782,#3783,#3784,
#3785,#3786,#3787,#3788,#3789,#3790,#3791,#3792,#3793,#3794,#3795,#3796,
#3797,#3798,#3799,#3800,#3801,#3802,#3803));
#1005=EDGE_LOOP('',(#3804,#3805,#3806,#3807,#3808));
#1006=EDGE_LOOP('',(#3809,#3810,#3811,#3812,#3813,#3814,#3815,#3816,#3817,
#3818,#3819,#3820,#3821,#3822,#3823,#3824,#3825,#3826,#3827,#3828,#3829,
#3830,#3831,#3832,#3833,#3834,#3835,#3836,#3837,#3838,#3839,#3840,#3841,
#3842,#3843,#3844,#3845,#3846,#3847,#3848,#3849,#3850,#3851,#3852,#3853,
#3854,#3855,#3856,#3857,#3858,#3859,#3860,#3861,#3862,#3863,#3864,#3865,
#3866,#3867,#3868,#3869,#3870,#3871,#3872,#3873,#3874,#3875,#3876,#3877,
#3878,#3879,#3880,#3881,#3882,#3883,#3884,#3885,#3886,#3887,#3888,#3889,
#3890,#3891,#3892,#3893,#3894,#3895,#3896,#3897,#3898,#3899,#3900,#3901,
#3902,#3903,#3904,#3905,#3906,#3907,#3908,#3909,#3910,#3911,#3912,#3913,
#3914,#3915,#3916,#3917,#3918,#3919,#3920,#3921,#3922,#3923,#3924,#3925,
#3926,#3927,#3928,#3929,#3930,#3931,#3932,#3933,#3934,#3935,#3936,#3937,
#3938,#3939,#3940,#3941,#3942,#3943,#3944,#3945,#3946,#3947,#3948,#3949,
#3950,#3951,#3952,#3953,#3954,#3955,#3956,#3957,#3958,#3959,#3960,#3961,
#3962,#3963,#3964,#3965,#3966,#3967,#3968,#3969,#3970,#3971,#3972,#3973,
#3974,#3975,#3976,#3977,#3978,#3979,#3980,#3981,#3982,#3983,#3984,#3985,
#3986,#3987,#3988,#3989,#3990,#3991,#3992,#3993,#3994,#3995,#3996,#3997,
#3998,#3999,#4000,#4001,#4002,#4003,#4004,#4005,#4006,#4007,#4008,#4009,
#4010,#4011,#4012,#4013,#4014,#4015,#4016,#4017,#4018,#4019,#4020,#4021,
#4022,#4023,#4024,#4025,#4026));
#1007=EDGE_LOOP('',(#4027,#4028,#4029,#4030,#4031,#4032,#4033,#4034,#4035,
#4036,#4037,#4038,#4039,#4040,#4041,#4042,#4043,#4044,#4045,#4046,#4047,
#4048,#4049,#4050,#4051,#4052,#4053,#4054,#4055,#4056,#4057,#4058,#4059,
#4060,#4061,#4062,#4063,#4064,#4065,#4066,#4067,#4068,#4069,#4070,#4071,
#4072,#4073,#4074,#4075,#4076,#4077,#4078,#4079,#4080,#4081,#4082,#4083,
#4084,#4085,#4086,#4087,#4088,#4089,#4090,#4091,#4092,#4093,#4094,#4095,
#4096,#4097,#4098,#4099,#4100,#4101,#4102,#4103,#4104,#4105,#4106,#4107,
#4108,#4109,#4110,#4111,#4112,#4113,#4114,#4115,#4116,#4117,#4118,#4119,
#4120,#4121,#4122,#4123,#4124,#4125,#4126,#4127,#4128,#4129,#4130,#4131,
#4132,#4133,#4134,#4135,#4136,#4137,#4138,#4139,#4140,#4141,#4142,#4143,
#4144,#4145,#4146,#4147,#4148,#4149,#4150,#4151,#4152,#4153,#4154,#4155,
#4156,#4157,#4158,#4159,#4160,#4161,#4162,#4163,#4164,#4165,#4166,#4167,
#4168,#4169,#4170,#4171,#4172,#4173,#4174,#4175,#4176,#4177,#4178,#4179,
#4180,#4181,#4182,#4183,#4184,#4185,#4186,#4187,#4188,#4189,#4190,#4191,
#4192,#4193,#4194,#4195,#4196,#4197,#4198,#4199,#4200,#4201,#4202,#4203,
#4204,#4205,#4206,#4207,#4208,#4209,#4210,#4211,#4212,#4213,#4214,#4215,
#4216,#4217,#4218,#4219,#4220,#4221,#4222,#4223,#4224,#4225,#4226,#4227,
#4228,#4229,#4230,#4231,#4232,#4233,#4234,#4235,#4236,#4237,#4238,#4239,
#4240,#4241,#4242,#4243,#4244,#4245));
#1008=EDGE_LOOP('',(#4246,#4247,#4248,#4249,#4250));
#1009=EDGE_LOOP('',(#4251,#4252,#4253,#4254));
#1010=LINE('',#5781,#1188);
#1011=LINE('',#5794,#1189);
#1012=LINE('',#5798,#1190);
#1013=LINE('',#5802,#1191);
#1014=LINE('',#5806,#1192);
#1015=LINE('',#5809,#1193);
#1016=LINE('',#5812,#1194);
#1017=LINE('',#5815,#1195);
#1018=LINE('',#5819,#1196);
#1019=LINE('',#5823,#1197);
#1020=LINE('',#5827,#1198);
#1021=LINE('',#5829,#1199);
#1022=LINE('',#5832,#1200);
#1023=LINE('',#5833,#1201);
#1024=LINE('',#5836,#1202);
#1025=LINE('',#5838,#1203);
#1026=LINE('',#5841,#1204);
#1027=LINE('',#5842,#1205);
#1028=LINE('',#5845,#1206);
#1029=LINE('',#5847,#1207);
#1030=LINE('',#5848,#1208);
#1031=LINE('',#5851,#1209);
#1032=LINE('',#5852,#1210);
#1033=LINE('',#5855,#1211);
#1034=LINE('',#5856,#1212);
#1035=LINE('',#5859,#1213);
#1036=LINE('',#5860,#1214);
#1037=LINE('',#5880,#1215);
#1038=LINE('',#5892,#1216);
#1039=LINE('',#5904,#1217);
#1040=LINE('',#5912,#1218);
#1041=LINE('',#5924,#1219);
#1042=LINE('',#5931,#1220);
#1043=LINE('',#5934,#1221);
#1044=LINE('',#5938,#1222);
#1045=LINE('',#5941,#1223);
#1046=LINE('',#5944,#1224);
#1047=LINE('',#5947,#1225);
#1048=LINE('',#5950,#1226);
#1049=LINE('',#5952,#1227);
#1050=LINE('',#5955,#1228);
#1051=LINE('',#5959,#1229);
#1052=LINE('',#5963,#1230);
#1053=LINE('',#5966,#1231);
#1054=LINE('',#5968,#1232);
#1055=LINE('',#5991,#1233);
#1056=LINE('',#5993,#1234);
#1057=LINE('',#6015,#1235);
#1058=LINE('',#6017,#1236);
#1059=LINE('',#6019,#1237);
#1060=LINE('',#6021,#1238);
#1061=LINE('',#6023,#1239);
#1062=LINE('',#6025,#1240);
#1063=LINE('',#6027,#1241);
#1064=LINE('',#6028,#1242);
#1065=LINE('',#6039,#1243);
#1066=LINE('',#6047,#1244);
#1067=LINE('',#6057,#1245);
#1068=LINE('',#6069,#1246);
#1069=LINE('',#6077,#1247);
#1070=LINE('',#6082,#1248);
#1071=LINE('',#6086,#1249);
#1072=LINE('',#6091,#1250);
#1073=LINE('',#6095,#1251);
#1074=LINE('',#6098,#1252);
#1075=LINE('',#6101,#1253);
#1076=LINE('',#6104,#1254);
#1077=LINE('',#6107,#1255);
#1078=LINE('',#6109,#1256);
#1079=LINE('',#6110,#1257);
#1080=LINE('',#6113,#1258);
#1081=LINE('',#6114,#1259);
#1082=LINE('',#6117,#1260);
#1083=LINE('',#6118,#1261);
#1084=LINE('',#6121,#1262);
#1085=LINE('',#6122,#1263);
#1086=LINE('',#6125,#1264);
#1087=LINE('',#6127,#1265);
#1088=LINE('',#6128,#1266);
#1089=LINE('',#6130,#1267);
#1090=LINE('',#6133,#1268);
#1091=LINE('',#6134,#1269);
#1092=LINE('',#6136,#1270);
#1093=LINE('',#6144,#1271);
#1094=LINE('',#6146,#1272);
#1095=LINE('',#6148,#1273);
#1096=LINE('',#6150,#1274);
#1097=LINE('',#6152,#1275);
#1098=LINE('',#6154,#1276);
#1099=LINE('',#6156,#1277);
#1100=LINE('',#6157,#1278);
#1101=LINE('',#6191,#1279);
#1102=LINE('',#6197,#1280);
#1103=LINE('',#6213,#1281);
#1104=LINE('',#6227,#1282);
#1105=LINE('',#6416,#1283);
#1106=LINE('',#6989,#1284);
#1107=LINE('',#7567,#1285);
#1108=LINE('',#8159,#1286);
#1109=LINE('',#8711,#1287);
#1110=LINE('',#9319,#1288);
#1111=LINE('',#9901,#1289);
#1112=LINE('',#10517,#1290);
#1113=LINE('',#11063,#1291);
#1114=LINE('',#11697,#1292);
#1115=LINE('',#12261,#1293);
#1116=LINE('',#12875,#1294);
#1117=LINE('',#13439,#1295);
#1118=LINE('',#14047,#1296);
#1119=LINE('',#14615,#1297);
#1120=LINE('',#15207,#1298);
#1121=LINE('',#15798,#1299);
#1122=LINE('',#16429,#1300);
#1123=LINE('',#17070,#1301);
#1124=LINE('',#17613,#1302);
#1125=LINE('',#18324,#1303);
#1126=LINE('',#18929,#1304);
#1127=LINE('',#19652,#1305);
#1128=LINE('',#20219,#1306);
#1129=LINE('',#20836,#1307);
#1130=LINE('',#21423,#1308);
#1131=LINE('',#22026,#1309);
#1132=LINE('',#22619,#1310);
#1133=LINE('',#23222,#1311);
#1134=LINE('',#23827,#1312);
#1135=LINE('',#24392,#1313);
#1136=LINE('',#24967,#1314);
#1137=LINE('',#25560,#1315);
#1138=LINE('',#26111,#1316);
#1139=LINE('',#26700,#1317);
#1140=LINE('',#27311,#1318);
#1141=LINE('',#27902,#1319);
#1142=LINE('',#28488,#1320);
#1143=LINE('',#29136,#1321);
#1144=LINE('',#29644,#1322);
#1145=LINE('',#30202,#1323);
#1146=LINE('',#30813,#1324);
#1147=LINE('',#31392,#1325);
#1148=LINE('',#31945,#1326);
#1149=LINE('',#32463,#1327);
#1150=LINE('',#32990,#1328);
#1151=LINE('',#33615,#1329);
#1152=LINE('',#34196,#1330);
#1153=LINE('',#34863,#1331);
#1154=LINE('',#35396,#1332);
#1155=LINE('',#35886,#1333);
#1156=LINE('',#36445,#1334);
#1157=LINE('',#37032,#1335);
#1158=LINE('',#37622,#1336);
#1159=LINE('',#38172,#1337);
#1160=LINE('',#38700,#1338);
#1161=LINE('',#39229,#1339);
#1162=LINE('',#39816,#1340);
#1163=LINE('',#40425,#1341);
#1164=LINE('',#41062,#1342);
#1165=LINE('',#41669,#1343);
#1166=LINE('',#42262,#1344);
#1167=LINE('',#42853,#1345);
#1168=LINE('',#43456,#1346);
#1169=LINE('',#44111,#1347);
#1170=LINE('',#44756,#1348);
#1171=LINE('',#45369,#1349);
#1172=LINE('',#45952,#1350);
#1173=LINE('',#46577,#1351);
#1174=LINE('',#47132,#1352);
#1175=LINE('',#47510,#1353);
#1176=LINE('',#48017,#1354);
#1177=LINE('',#48580,#1355);
#1178=LINE('',#48941,#1356);
#1179=LINE('',#49470,#1357);
#1180=LINE('',#50063,#1358);
#1181=LINE('',#50642,#1359);
#1182=LINE('',#51211,#1360);
#1183=LINE('',#51834,#1361);
#1184=LINE('',#52433,#1362);
#1185=LINE('',#52952,#1363);
#1186=LINE('',#53538,#1364);
#1187=LINE('',#54126,#1365);
#1188=VECTOR('',#4955,20.5);
#1189=VECTOR('',#4972,20.);
#1190=VECTOR('',#4975,10.);
#1191=VECTOR('',#4978,10.);
#1192=VECTOR('',#4983,10.);
#1193=VECTOR('',#4986,9.99999999999999);
#1194=VECTOR('',#4989,10.);
#1195=VECTOR('',#4992,10.);
#1196=VECTOR('',#4995,10.);
#1197=VECTOR('',#4998,10.);
#1198=VECTOR('',#5003,9.99999999999999);
#1199=VECTOR('',#5004,10.);
#1200=VECTOR('',#5009,10.);
#1201=VECTOR('',#5010,9.99999999999999);
#1202=VECTOR('',#5013,10.);
#1203=VECTOR('',#5014,10.);
#1204=VECTOR('',#5019,9.99999999999999);
#1205=VECTOR('',#5020,10.);
#1206=VECTOR('',#5023,10.);
#1207=VECTOR('',#5024,9.99999999999999);
#1208=VECTOR('',#5025,10.);
#1209=VECTOR('',#5028,10.);
#1210=VECTOR('',#5029,10.);
#1211=VECTOR('',#5032,10.);
#1212=VECTOR('',#5033,9.99999999999999);
#1213=VECTOR('',#5036,10.);
#1214=VECTOR('',#5037,10.);
#1215=VECTOR('',#5060,4.);
#1216=VECTOR('',#5075,4.);
#1217=VECTOR('',#5090,4.);
#1218=VECTOR('',#5101,20.);
#1219=VECTOR('',#5116,4.);
#1220=VECTOR('',#5123,10.);
#1221=VECTOR('',#5126,10.);
#1222=VECTOR('',#5131,10.);
#1223=VECTOR('',#5134,9.99999999999999);
#1224=VECTOR('',#5137,10.);
#1225=VECTOR('',#5140,10.);
#1226=VECTOR('',#5143,10.);
#1227=VECTOR('',#5146,9.99999999999999);
#1228=VECTOR('',#5149,10.);
#1229=VECTOR('',#5154,10.);
#1230=VECTOR('',#5159,10.);
#1231=VECTOR('',#5164,10.);
#1232=VECTOR('',#5167,10.);
#1233=VECTOR('',#5202,10.);
#1234=VECTOR('',#5205,10.);
#1235=VECTOR('',#5232,10.);
#1236=VECTOR('',#5233,10.);
#1237=VECTOR('',#5234,10.);
#1238=VECTOR('',#5235,10.);
#1239=VECTOR('',#5236,10.);
#1240=VECTOR('',#5237,10.);
#1241=VECTOR('',#5238,10.);
#1242=VECTOR('',#5239,10.);
#1243=VECTOR('',#5250,4.);
#1244=VECTOR('',#5261,4.);
#1245=VECTOR('',#5274,4.);
#1246=VECTOR('',#5291,4.);
#1247=VECTOR('',#5300,9.99999999999999);
#1248=VECTOR('',#5307,10.);
#1249=VECTOR('',#5312,9.99999999999999);
#1250=VECTOR('',#5317,9.99999999999999);
#1251=VECTOR('',#5322,10.);
#1252=VECTOR('',#5327,10.);
#1253=VECTOR('',#5330,9.99999999999999);
#1254=VECTOR('',#5335,10.);
#1255=VECTOR('',#5338,10.);
#1256=VECTOR('',#5339,10.);
#1257=VECTOR('',#5340,10.);
#1258=VECTOR('',#5343,10.);
#1259=VECTOR('',#5344,9.99999999999999);
#1260=VECTOR('',#5347,10.);
#1261=VECTOR('',#5348,10.);
#1262=VECTOR('',#5351,10.);
#1263=VECTOR('',#5352,9.99999999999999);
#1264=VECTOR('',#5355,10.);
#1265=VECTOR('',#5356,9.99999999999999);
#1266=VECTOR('',#5357,10.);
#1267=VECTOR('',#5360,10.);
#1268=VECTOR('',#5363,10.);
#1269=VECTOR('',#5364,10.);
#1270=VECTOR('',#5367,9.99999999999999);
#1271=VECTOR('',#5376,10.);
#1272=VECTOR('',#5377,10.);
#1273=VECTOR('',#5378,10.);
#1274=VECTOR('',#5379,10.);
#1275=VECTOR('',#5380,10.);
#1276=VECTOR('',#5381,10.);
#1277=VECTOR('',#5382,10.);
#1278=VECTOR('',#5383,10.);
#1279=VECTOR('',#5442,20.5);
#1280=VECTOR('',#5449,19.5);
#1281=VECTOR('',#5472,20.5);
#1282=VECTOR('',#5491,3.22275);
#1283=VECTOR('',#5496,3.22275);
#1284=VECTOR('',#5499,3.22275);
#1285=VECTOR('',#5502,3.22275);
#1286=VECTOR('',#5505,3.22275);
#1287=VECTOR('',#5508,3.22275);
#1288=VECTOR('',#5511,3.22275);
#1289=VECTOR('',#5514,3.22275);
#1290=VECTOR('',#5517,3.22275);
#1291=VECTOR('',#5520,3.22275);
#1292=VECTOR('',#5523,3.22275);
#1293=VECTOR('',#5526,3.22275);
#1294=VECTOR('',#5529,3.22275);
#1295=VECTOR('',#5532,3.22275);
#1296=VECTOR('',#5535,3.22275);
#1297=VECTOR('',#5538,3.22275);
#1298=VECTOR('',#5541,3.22275);
#1299=VECTOR('',#5544,3.22275);
#1300=VECTOR('',#5547,3.22275);
#1301=VECTOR('',#5550,3.22275);
#1302=VECTOR('',#5553,3.22275);
#1303=VECTOR('',#5556,3.22275);
#1304=VECTOR('',#5559,3.22275);
#1305=VECTOR('',#5562,3.22275);
#1306=VECTOR('',#5565,3.22275);
#1307=VECTOR('',#5568,3.22275);
#1308=VECTOR('',#5571,3.22275);
#1309=VECTOR('',#5574,3.22275);
#1310=VECTOR('',#5577,3.22275);
#1311=VECTOR('',#5580,3.22275);
#1312=VECTOR('',#5583,3.22275);
#1313=VECTOR('',#5586,3.22275);
#1314=VECTOR('',#5589,3.22275);
#1315=VECTOR('',#5592,3.22275);
#1316=VECTOR('',#5595,3.22275);
#1317=VECTOR('',#5598,3.22275);
#1318=VECTOR('',#5601,3.22275);
#1319=VECTOR('',#5604,3.22275);
#1320=VECTOR('',#5607,3.22275);
#1321=VECTOR('',#5610,3.22275);
#1322=VECTOR('',#5613,3.22275);
#1323=VECTOR('',#5616,3.22275);
#1324=VECTOR('',#5619,3.22275);
#1325=VECTOR('',#5622,3.22275);
#1326=VECTOR('',#5625,3.22275);
#1327=VECTOR('',#5628,3.22275);
#1328=VECTOR('',#5631,3.22275);
#1329=VECTOR('',#5634,3.22275);
#1330=VECTOR('',#5637,3.22275);
#1331=VECTOR('',#5640,3.22275);
#1332=VECTOR('',#5643,3.22275);
#1333=VECTOR('',#5646,3.22275);
#1334=VECTOR('',#5649,3.22275);
#1335=VECTOR('',#5652,3.22275);
#1336=VECTOR('',#5655,3.22275);
#1337=VECTOR('',#5658,3.22275);
#1338=VECTOR('',#5661,3.22275);
#1339=VECTOR('',#5664,3.22275);
#1340=VECTOR('',#5667,3.22275);
#1341=VECTOR('',#5670,3.22275);
#1342=VECTOR('',#5673,3.22275);
#1343=VECTOR('',#5676,3.22275);
#1344=VECTOR('',#5679,3.22275);
#1345=VECTOR('',#5682,3.22275);
#1346=VECTOR('',#5685,3.22275);
#1347=VECTOR('',#5688,3.22275);
#1348=VECTOR('',#5691,3.22275);
#1349=VECTOR('',#5694,3.22275);
#1350=VECTOR('',#5697,3.22275);
#1351=VECTOR('',#5700,3.22275);
#1352=VECTOR('',#5703,3.22275);
#1353=VECTOR('',#5706,3.22275);
#1354=VECTOR('',#5709,3.22275);
#1355=VECTOR('',#5712,3.22275);
#1356=VECTOR('',#5715,3.22275);
#1357=VECTOR('',#5718,3.22275);
#1358=VECTOR('',#5721,3.22275);
#1359=VECTOR('',#5724,3.22275);
#1360=VECTOR('',#5727,3.22275);
#1361=VECTOR('',#5730,3.22275);
#1362=VECTOR('',#5733,3.22275);
#1363=VECTOR('',#5736,3.22275);
#1364=VECTOR('',#5739,3.22275);
#1365=VECTOR('',#5742,3.22275);
#1366=CIRCLE('',#4625,20.5);
#1367=CIRCLE('',#4626,20.5);
#1368=CIRCLE('',#4628,20.);
#1369=CIRCLE('',#4630,20.);
#1370=CIRCLE('',#4632,20.);
#1371=CIRCLE('',#4633,20.);
#1372=CIRCLE('',#4655,4.5);
#1373=CIRCLE('',#4656,4.5);
#1374=CIRCLE('',#4657,4.5);
#1375=CIRCLE('',#4658,20.5);
#1376=CIRCLE('',#4659,4.5);
#1377=CIRCLE('',#4661,4.);
#1378=CIRCLE('',#4662,0.5);
#1379=CIRCLE('',#4663,4.);
#1380=CIRCLE('',#4665,4.);
#1381=CIRCLE('',#4666,4.);
#1382=CIRCLE('',#4668,4.);
#1383=CIRCLE('',#4669,0.5);
#1384=CIRCLE('',#4670,4.);
#1385=CIRCLE('',#4672,4.);
#1386=CIRCLE('',#4673,4.);
#1387=CIRCLE('',#4675,4.);
#1388=CIRCLE('',#4676,0.5);
#1389=CIRCLE('',#4677,4.);
#1390=CIRCLE('',#4679,4.);
#1391=CIRCLE('',#4680,4.);
#1392=CIRCLE('',#4682,0.5);
#1393=CIRCLE('',#4684,20.);
#1394=CIRCLE('',#4685,20.);
#1395=CIRCLE('',#4687,4.);
#1396=CIRCLE('',#4688,0.5);
#1397=CIRCLE('',#4689,4.);
#1398=CIRCLE('',#4691,4.);
#1399=CIRCLE('',#4692,4.);
#1400=CIRCLE('',#4711,4.5);
#1401=CIRCLE('',#4712,4.5);
#1402=CIRCLE('',#4713,4.5);
#1403=CIRCLE('',#4714,20.5);
#1404=CIRCLE('',#4715,4.5);
#1405=CIRCLE('',#4717,0.5);
#1406=CIRCLE('',#4719,0.5);
#1407=CIRCLE('',#4721,0.5);
#1408=CIRCLE('',#4723,0.5);
#1409=CIRCLE('',#4725,0.5);
#1410=CIRCLE('',#4731,20.5);
#1411=CIRCLE('',#4732,20.);
#1412=CIRCLE('',#4734,20.5);
#1413=CIRCLE('',#4735,20.);
#1414=CIRCLE('',#4737,4.5);
#1415=CIRCLE('',#4738,0.5);
#1416=CIRCLE('',#4739,4.);
#1417=CIRCLE('',#4741,4.5);
#1418=CIRCLE('',#4742,20.5);
#1419=CIRCLE('',#4743,4.5);
#1420=CIRCLE('',#4744,4.5);
#1421=CIRCLE('',#4746,4.);
#1422=CIRCLE('',#4748,0.5);
#1423=CIRCLE('',#4749,4.);
#1424=CIRCLE('',#4751,4.);
#1425=CIRCLE('',#4752,4.);
#1426=CIRCLE('',#4754,0.5);
#1427=CIRCLE('',#4755,4.);
#1428=CIRCLE('',#4757,4.);
#1429=CIRCLE('',#4758,4.);
#1430=CIRCLE('',#4760,0.5);
#1431=CIRCLE('',#4762,0.5);
#1432=CIRCLE('',#4763,4.);
#1433=CIRCLE('',#4765,4.);
#1434=CIRCLE('',#4766,4.);
#1435=CIRCLE('',#4792,4.5);
#1436=CIRCLE('',#4793,0.5);
#1437=CIRCLE('',#4795,4.5);
#1438=CIRCLE('',#4796,4.5);
#1439=CIRCLE('',#4797,4.5);
#1440=CIRCLE('',#4798,20.5);
#1441=CIRCLE('',#4800,0.5);
#1442=CIRCLE('',#4802,0.5);
#1443=CIRCLE('',#4804,0.5);
#1444=CIRCLE('',#4822,0.5);
#1445=CIRCLE('',#4826,19.5);
#1446=CIRCLE('',#4827,19.5);
#1447=CIRCLE('',#4829,19.9);
#1448=CIRCLE('',#4830,0.400000000000003);
#1449=CIRCLE('',#4832,20.1);
#1450=CIRCLE('',#4834,20.5);
#1451=CIRCLE('',#4835,0.399999999999996);
#1452=CIRCLE('',#4837,20.5);
#1453=CIRCLE('',#4839,20.1);
#1454=CIRCLE('',#4840,0.399999999999998);
#1455=CIRCLE('',#4842,19.9);
#1456=CIRCLE('',#4844,0.400000000000003);
#1457=CIRCLE('',#4847,3.22275);
#1458=CIRCLE('',#4932,3.933);
#1459=CIRCLE('',#4933,3.933);
#1460=CIRCLE('',#4935,3.22275);
#1461=VERTEX_POINT('',#5778);
#1462=VERTEX_POINT('',#5780);
#1463=VERTEX_POINT('',#5784);
#1464=VERTEX_POINT('',#5787);
#1465=VERTEX_POINT('',#5790);
#1466=VERTEX_POINT('',#5791);
#1467=VERTEX_POINT('',#5796);
#1468=VERTEX_POINT('',#5797);
#1469=VERTEX_POINT('',#5799);
#1470=VERTEX_POINT('',#5801);
#1471=VERTEX_POINT('',#5805);
#1472=VERTEX_POINT('',#5807);
#1473=VERTEX_POINT('',#5811);
#1474=VERTEX_POINT('',#5813);
#1475=VERTEX_POINT('',#5817);
#1476=VERTEX_POINT('',#5818);
#1477=VERTEX_POINT('',#5820);
#1478=VERTEX_POINT('',#5822);
#1479=VERTEX_POINT('',#5826);
#1480=VERTEX_POINT('',#5828);
#1481=VERTEX_POINT('',#5835);
#1482=VERTEX_POINT('',#5837);
#1483=VERTEX_POINT('',#5844);
#1484=VERTEX_POINT('',#5846);
#1485=VERTEX_POINT('',#5850);
#1486=VERTEX_POINT('',#5854);
#1487=VERTEX_POINT('',#5858);
#1488=VERTEX_POINT('',#5862);
#1489=VERTEX_POINT('',#5864);
#1490=VERTEX_POINT('',#5866);
#1491=VERTEX_POINT('',#5868);
#1492=VERTEX_POINT('',#5870);
#1493=VERTEX_POINT('',#5873);
#1494=VERTEX_POINT('',#5874);
#1495=VERTEX_POINT('',#5879);
#1496=VERTEX_POINT('',#5881);
#1497=VERTEX_POINT('',#5885);
#1498=VERTEX_POINT('',#5886);
#1499=VERTEX_POINT('',#5891);
#1500=VERTEX_POINT('',#5893);
#1501=VERTEX_POINT('',#5897);
#1502=VERTEX_POINT('',#5898);
#1503=VERTEX_POINT('',#5903);
#1504=VERTEX_POINT('',#5905);
#1505=VERTEX_POINT('',#5911);
#1506=VERTEX_POINT('',#5913);
#1507=VERTEX_POINT('',#5917);
#1508=VERTEX_POINT('',#5918);
#1509=VERTEX_POINT('',#5923);
#1510=VERTEX_POINT('',#5925);
#1511=VERTEX_POINT('',#5929);
#1512=VERTEX_POINT('',#5930);
#1513=VERTEX_POINT('',#5932);
#1514=VERTEX_POINT('',#5937);
#1515=VERTEX_POINT('',#5939);
#1516=VERTEX_POINT('',#5943);
#1517=VERTEX_POINT('',#5945);
#1518=VERTEX_POINT('',#5949);
#1519=VERTEX_POINT('',#5954);
#1520=VERTEX_POINT('',#5958);
#1521=VERTEX_POINT('',#5962);
#1522=VERTEX_POINT('',#5970);
#1523=VERTEX_POINT('',#5972);
#1524=VERTEX_POINT('',#5974);
#1525=VERTEX_POINT('',#5976);
#1526=VERTEX_POINT('',#5978);
#1527=VERTEX_POINT('',#5997);
#1528=VERTEX_POINT('',#5999);
#1529=VERTEX_POINT('',#6002);
#1530=VERTEX_POINT('',#6004);
#1531=VERTEX_POINT('',#6007);
#1532=VERTEX_POINT('',#6009);
#1533=VERTEX_POINT('',#6013);
#1534=VERTEX_POINT('',#6014);
#1535=VERTEX_POINT('',#6016);
#1536=VERTEX_POINT('',#6018);
#1537=VERTEX_POINT('',#6020);
#1538=VERTEX_POINT('',#6022);
#1539=VERTEX_POINT('',#6024);
#1540=VERTEX_POINT('',#6026);
#1541=VERTEX_POINT('',#6029);
#1542=VERTEX_POINT('',#6031);
#1543=VERTEX_POINT('',#6033);
#1544=VERTEX_POINT('',#6035);
#1545=VERTEX_POINT('',#6038);
#1546=VERTEX_POINT('',#6042);
#1547=VERTEX_POINT('',#6046);
#1548=VERTEX_POINT('',#6048);
#1549=VERTEX_POINT('',#6052);
#1550=VERTEX_POINT('',#6056);
#1551=VERTEX_POINT('',#6058);
#1552=VERTEX_POINT('',#6064);
#1553=VERTEX_POINT('',#6068);
#1554=VERTEX_POINT('',#6070);
#1555=VERTEX_POINT('',#6074);
#1556=VERTEX_POINT('',#6076);
#1557=VERTEX_POINT('',#6080);
#1558=VERTEX_POINT('',#6084);
#1559=VERTEX_POINT('',#6088);
#1560=VERTEX_POINT('',#6090);
#1561=VERTEX_POINT('',#6094);
#1562=VERTEX_POINT('',#6100);
#1563=VERTEX_POINT('',#6106);
#1564=VERTEX_POINT('',#6108);
#1565=VERTEX_POINT('',#6112);
#1566=VERTEX_POINT('',#6116);
#1567=VERTEX_POINT('',#6120);
#1568=VERTEX_POINT('',#6124);
#1569=VERTEX_POINT('',#6126);
#1570=VERTEX_POINT('',#6132);
#1571=VERTEX_POINT('',#6138);
#1572=VERTEX_POINT('',#6142);
#1573=VERTEX_POINT('',#6143);
#1574=VERTEX_POINT('',#6145);
#1575=VERTEX_POINT('',#6147);
#1576=VERTEX_POINT('',#6149);
#1577=VERTEX_POINT('',#6151);
#1578=VERTEX_POINT('',#6153);
#1579=VERTEX_POINT('',#6155);
#1580=VERTEX_POINT('',#6158);
#1581=VERTEX_POINT('',#6160);
#1582=VERTEX_POINT('',#6162);
#1583=VERTEX_POINT('',#6164);
#1584=VERTEX_POINT('',#6194);
#1585=VERTEX_POINT('',#6196);
#1586=VERTEX_POINT('',#6200);
#1587=VERTEX_POINT('',#6204);
#1588=VERTEX_POINT('',#6207);
#1589=VERTEX_POINT('',#6211);
#1590=VERTEX_POINT('',#6215);
#1591=VERTEX_POINT('',#6219);
#1592=VERTEX_POINT('',#6225);
#1593=VERTEX_POINT('',#6226);
#1594=VERTEX_POINT('',#6228);
#1595=VERTEX_POINT('',#6341);
#1596=VERTEX_POINT('',#6414);
#1597=VERTEX_POINT('',#6415);
#1598=VERTEX_POINT('',#6417);
#1599=VERTEX_POINT('',#6709);
#1600=VERTEX_POINT('',#6987);
#1601=VERTEX_POINT('',#6988);
#1602=VERTEX_POINT('',#7565);
#1603=VERTEX_POINT('',#7566);
#1604=VERTEX_POINT('',#7568);
#1605=VERTEX_POINT('',#7879);
#1606=VERTEX_POINT('',#8157);
#1607=VERTEX_POINT('',#8158);
#1608=VERTEX_POINT('',#8709);
#1609=VERTEX_POINT('',#8710);
#1610=VERTEX_POINT('',#8712);
#1611=VERTEX_POINT('',#9017);
#1612=VERTEX_POINT('',#9317);
#1613=VERTEX_POINT('',#9318);
#1614=VERTEX_POINT('',#9899);
#1615=VERTEX_POINT('',#9900);
#1616=VERTEX_POINT('',#9902);
#1617=VERTEX_POINT('',#10209);
#1618=VERTEX_POINT('',#10515);
#1619=VERTEX_POINT('',#10516);
#1620=VERTEX_POINT('',#11061);
#1621=VERTEX_POINT('',#11062);
#1622=VERTEX_POINT('',#11064);
#1623=VERTEX_POINT('',#11371);
#1624=VERTEX_POINT('',#11695);
#1625=VERTEX_POINT('',#11696);
#1626=VERTEX_POINT('',#12259);
#1627=VERTEX_POINT('',#12260);
#1628=VERTEX_POINT('',#12262);
#1629=VERTEX_POINT('',#12565);
#1630=VERTEX_POINT('',#12873);
#1631=VERTEX_POINT('',#12874);
#1632=VERTEX_POINT('',#13437);
#1633=VERTEX_POINT('',#13438);
#1634=VERTEX_POINT('',#13440);
#1635=VERTEX_POINT('',#13761);
#1636=VERTEX_POINT('',#14045);
#1637=VERTEX_POINT('',#14046);
#1638=VERTEX_POINT('',#14613);
#1639=VERTEX_POINT('',#14614);
#1640=VERTEX_POINT('',#14616);
#1641=VERTEX_POINT('',#14955);
#1642=VERTEX_POINT('',#15205);
#1643=VERTEX_POINT('',#15206);
#1644=VERTEX_POINT('',#15494);
#1645=VERTEX_POINT('',#15796);
#1646=VERTEX_POINT('',#15797);
#1647=VERTEX_POINT('',#15799);
#1648=VERTEX_POINT('',#16427);
#1649=VERTEX_POINT('',#16428);
#1650=VERTEX_POINT('',#16724);
#1651=VERTEX_POINT('',#17068);
#1652=VERTEX_POINT('',#17069);
#1653=VERTEX_POINT('',#17071);
#1654=VERTEX_POINT('',#17611);
#1655=VERTEX_POINT('',#17612);
#1656=VERTEX_POINT('',#17908);
#1657=VERTEX_POINT('',#18322);
#1658=VERTEX_POINT('',#18323);
#1659=VERTEX_POINT('',#18325);
#1660=VERTEX_POINT('',#18927);
#1661=VERTEX_POINT('',#18928);
#1662=VERTEX_POINT('',#19270);
#1663=VERTEX_POINT('',#19650);
#1664=VERTEX_POINT('',#19651);
#1665=VERTEX_POINT('',#19653);
#1666=VERTEX_POINT('',#20217);
#1667=VERTEX_POINT('',#20218);
#1668=VERTEX_POINT('',#20504);
#1669=VERTEX_POINT('',#20834);
#1670=VERTEX_POINT('',#20835);
#1671=VERTEX_POINT('',#20837);
#1672=VERTEX_POINT('',#21421);
#1673=VERTEX_POINT('',#21422);
#1674=VERTEX_POINT('',#21736);
#1675=VERTEX_POINT('',#22024);
#1676=VERTEX_POINT('',#22025);
#1677=VERTEX_POINT('',#22027);
#1678=VERTEX_POINT('',#22617);
#1679=VERTEX_POINT('',#22618);
#1680=VERTEX_POINT('',#22910);
#1681=VERTEX_POINT('',#23220);
#1682=VERTEX_POINT('',#23221);
#1683=VERTEX_POINT('',#23223);
#1684=VERTEX_POINT('',#23825);
#1685=VERTEX_POINT('',#23826);
#1686=VERTEX_POINT('',#24104);
#1687=VERTEX_POINT('',#24390);
#1688=VERTEX_POINT('',#24391);
#1689=VERTEX_POINT('',#24393);
#1690=VERTEX_POINT('',#24965);
#1691=VERTEX_POINT('',#24966);
#1692=VERTEX_POINT('',#25236);
#1693=VERTEX_POINT('',#25558);
#1694=VERTEX_POINT('',#25559);
#1695=VERTEX_POINT('',#25561);
#1696=VERTEX_POINT('',#26109);
#1697=VERTEX_POINT('',#26110);
#1698=VERTEX_POINT('',#26412);
#1699=VERTEX_POINT('',#26698);
#1700=VERTEX_POINT('',#26699);
#1701=VERTEX_POINT('',#26701);
#1702=VERTEX_POINT('',#27309);
#1703=VERTEX_POINT('',#27310);
#1704=VERTEX_POINT('',#27640);
#1705=VERTEX_POINT('',#27900);
#1706=VERTEX_POINT('',#27901);
#1707=VERTEX_POINT('',#27903);
#1708=VERTEX_POINT('',#28190);
#1709=VERTEX_POINT('',#28486);
#1710=VERTEX_POINT('',#28487);
#1711=VERTEX_POINT('',#29134);
#1712=VERTEX_POINT('',#29135);
#1713=VERTEX_POINT('',#29137);
#1714=VERTEX_POINT('',#29408);
#1715=VERTEX_POINT('',#29642);
#1716=VERTEX_POINT('',#29643);
#1717=VERTEX_POINT('',#29937);
#1718=VERTEX_POINT('',#30200);
#1719=VERTEX_POINT('',#30201);
#1720=VERTEX_POINT('',#30203);
#1721=VERTEX_POINT('',#30811);
#1722=VERTEX_POINT('',#30812);
#1723=VERTEX_POINT('',#31078);
#1724=VERTEX_POINT('',#31390);
#1725=VERTEX_POINT('',#31391);
#1726=VERTEX_POINT('',#31393);
#1727=VERTEX_POINT('',#31943);
#1728=VERTEX_POINT('',#31944);
#1729=VERTEX_POINT('',#31946);
#1730=VERTEX_POINT('',#32211);
#1731=VERTEX_POINT('',#32461);
#1732=VERTEX_POINT('',#32462);
#1733=VERTEX_POINT('',#32734);
#1734=VERTEX_POINT('',#32988);
#1735=VERTEX_POINT('',#32989);
#1736=VERTEX_POINT('',#32991);
#1737=VERTEX_POINT('',#33613);
#1738=VERTEX_POINT('',#33614);
#1739=VERTEX_POINT('',#33900);
#1740=VERTEX_POINT('',#34194);
#1741=VERTEX_POINT('',#34195);
#1742=VERTEX_POINT('',#34197);
#1743=VERTEX_POINT('',#34861);
#1744=VERTEX_POINT('',#34862);
#1745=VERTEX_POINT('',#35148);
#1746=VERTEX_POINT('',#35394);
#1747=VERTEX_POINT('',#35395);
#1748=VERTEX_POINT('',#35397);
#1749=VERTEX_POINT('',#35634);
#1750=VERTEX_POINT('',#35884);
#1751=VERTEX_POINT('',#35885);
#1752=VERTEX_POINT('',#35887);
#1753=VERTEX_POINT('',#36443);
#1754=VERTEX_POINT('',#36444);
#1755=VERTEX_POINT('',#36766);
#1756=VERTEX_POINT('',#37030);
#1757=VERTEX_POINT('',#37031);
#1758=VERTEX_POINT('',#37033);
#1759=VERTEX_POINT('',#37328);
#1760=VERTEX_POINT('',#37620);
#1761=VERTEX_POINT('',#37621);
#1762=VERTEX_POINT('',#38170);
#1763=VERTEX_POINT('',#38171);
#1764=VERTEX_POINT('',#38173);
#1765=VERTEX_POINT('',#38468);
#1766=VERTEX_POINT('',#38698);
#1767=VERTEX_POINT('',#38699);
#1768=VERTEX_POINT('',#38959);
#1769=VERTEX_POINT('',#39227);
#1770=VERTEX_POINT('',#39228);
#1771=VERTEX_POINT('',#39230);
#1772=VERTEX_POINT('',#39814);
#1773=VERTEX_POINT('',#39815);
#1774=VERTEX_POINT('',#40079);
#1775=VERTEX_POINT('',#40423);
#1776=VERTEX_POINT('',#40424);
#1777=VERTEX_POINT('',#40426);
#1778=VERTEX_POINT('',#41060);
#1779=VERTEX_POINT('',#41061);
#1780=VERTEX_POINT('',#41315);
#1781=VERTEX_POINT('',#41667);
#1782=VERTEX_POINT('',#41668);
#1783=VERTEX_POINT('',#41670);
#1784=VERTEX_POINT('',#42260);
#1785=VERTEX_POINT('',#42261);
#1786=VERTEX_POINT('',#42575);
#1787=VERTEX_POINT('',#42851);
#1788=VERTEX_POINT('',#42852);
#1789=VERTEX_POINT('',#42854);
#1790=VERTEX_POINT('',#43454);
#1791=VERTEX_POINT('',#43455);
#1792=VERTEX_POINT('',#43779);
#1793=VERTEX_POINT('',#44109);
#1794=VERTEX_POINT('',#44110);
#1795=VERTEX_POINT('',#44112);
#1796=VERTEX_POINT('',#44754);
#1797=VERTEX_POINT('',#44755);
#1798=VERTEX_POINT('',#45055);
#1799=VERTEX_POINT('',#45367);
#1800=VERTEX_POINT('',#45368);
#1801=VERTEX_POINT('',#45370);
#1802=VERTEX_POINT('',#45950);
#1803=VERTEX_POINT('',#45951);
#1804=VERTEX_POINT('',#46251);
#1805=VERTEX_POINT('',#46575);
#1806=VERTEX_POINT('',#46576);
#1807=VERTEX_POINT('',#46578);
#1808=VERTEX_POINT('',#47130);
#1809=VERTEX_POINT('',#47131);
#1810=VERTEX_POINT('',#47133);
#1811=VERTEX_POINT('',#47212);
#1812=VERTEX_POINT('',#47508);
#1813=VERTEX_POINT('',#47509);
#1814=VERTEX_POINT('',#47511);
#1815=VERTEX_POINT('',#48015);
#1816=VERTEX_POINT('',#48016);
#1817=VERTEX_POINT('',#48340);
#1818=VERTEX_POINT('',#48578);
#1819=VERTEX_POINT('',#48579);
#1820=VERTEX_POINT('',#48581);
#1821=VERTEX_POINT('',#48681);
#1822=VERTEX_POINT('',#48939);
#1823=VERTEX_POINT('',#48940);
#1824=VERTEX_POINT('',#48942);
#1825=VERTEX_POINT('',#49468);
#1826=VERTEX_POINT('',#49469);
#1827=VERTEX_POINT('',#49761);
#1828=VERTEX_POINT('',#50061);
#1829=VERTEX_POINT('',#50062);
#1830=VERTEX_POINT('',#50064);
#1831=VERTEX_POINT('',#50640);
#1832=VERTEX_POINT('',#50641);
#1833=VERTEX_POINT('',#50915);
#1834=VERTEX_POINT('',#51209);
#1835=VERTEX_POINT('',#51210);
#1836=VERTEX_POINT('',#51212);
#1837=VERTEX_POINT('',#51832);
#1838=VERTEX_POINT('',#51833);
#1839=VERTEX_POINT('',#52121);
#1840=VERTEX_POINT('',#52431);
#1841=VERTEX_POINT('',#52432);
#1842=VERTEX_POINT('',#52434);
#1843=VERTEX_POINT('',#52950);
#1844=VERTEX_POINT('',#52951);
#1845=VERTEX_POINT('',#52953);
#1846=VERTEX_POINT('',#53206);
#1847=VERTEX_POINT('',#53536);
#1848=VERTEX_POINT('',#53537);
#1849=VERTEX_POINT('',#54124);
#1850=VERTEX_POINT('',#54125);
#1851=VERTEX_POINT('',#54127);
#1852=VERTEX_POINT('',#54360);
#1853=VERTEX_POINT('',#54676);
#1854=VERTEX_POINT('',#54677);
#1855=VERTEX_POINT('',#54751);
#1856=VERTEX_POINT('',#54753);
#1857=VERTEX_POINT('',#54759);
#1858=VERTEX_POINT('',#54986);
#1859=VERTEX_POINT('',#54997);
#1860=VERTEX_POINT('',#55008);
#1861=VERTEX_POINT('',#55238);
#1862=VERTEX_POINT('',#55249);
#1863=VERTEX_POINT('',#55476);
#1864=VERTEX_POINT('',#55488);
#1865=VERTEX_POINT('',#55499);
#1866=VERTEX_POINT('',#55510);
#1867=VERTEX_POINT('',#55521);
#1868=VERTEX_POINT('',#55751);
#1869=VERTEX_POINT('',#55762);
#1870=VERTEX_POINT('',#55773);
#1871=VERTEX_POINT('',#56000);
#1872=VERTEX_POINT('',#56011);
#1873=VERTEX_POINT('',#56238);
#1874=VERTEX_POINT('',#56249);
#1875=VERTEX_POINT('',#56262);
#1876=VERTEX_POINT('',#56273);
#1877=VERTEX_POINT('',#56284);
#1878=VERTEX_POINT('',#56511);
#1879=VERTEX_POINT('',#56522);
#1880=VERTEX_POINT('',#56749);
#1881=VERTEX_POINT('',#56760);
#1882=VERTEX_POINT('',#56773);
#1883=VERTEX_POINT('',#56784);
#1884=VERTEX_POINT('',#56795);
#1885=VERTEX_POINT('',#57022);
#1886=VERTEX_POINT('',#57033);
#1887=VERTEX_POINT('',#57260);
#1888=VERTEX_POINT('',#57271);
#1889=VERTEX_POINT('',#57283);
#1890=VERTEX_POINT('',#57294);
#1891=VERTEX_POINT('',#57305);
#1892=VERTEX_POINT('',#57317);
#1893=VERTEX_POINT('',#57328);
#1894=VERTEX_POINT('',#57339);
#1895=VERTEX_POINT('',#57566);
#1896=VERTEX_POINT('',#57579);
#1897=VERTEX_POINT('',#57806);
#1898=VERTEX_POINT('',#58033);
#1899=VERTEX_POINT('',#58045);
#1900=VERTEX_POINT('',#58056);
#1901=VERTEX_POINT('',#58067);
#1902=VERTEX_POINT('',#58294);
#1903=VERTEX_POINT('',#58307);
#1904=VERTEX_POINT('',#58534);
#1905=VERTEX_POINT('',#58761);
#1906=VERTEX_POINT('',#58773);
#1907=VERTEX_POINT('',#58784);
#1908=VERTEX_POINT('',#58795);
#1909=VERTEX_POINT('',#59022);
#1910=VERTEX_POINT('',#59034);
#1911=VERTEX_POINT('',#59045);
#1912=VERTEX_POINT('',#59056);
#1913=VERTEX_POINT('',#59068);
#1914=VERTEX_POINT('',#59295);
#1915=VERTEX_POINT('',#59306);
#1916=VERTEX_POINT('',#59317);
#1917=VERTEX_POINT('',#59329);
#1918=VERTEX_POINT('',#59556);
#1919=VERTEX_POINT('',#59783);
#1920=VERTEX_POINT('',#59795);
#1921=VERTEX_POINT('',#60022);
#1922=VERTEX_POINT('',#60033);
#1923=VERTEX_POINT('',#60044);
#1924=VERTEX_POINT('',#60056);
#1925=VERTEX_POINT('',#60283);
#1926=VERTEX_POINT('',#60510);
#1927=VERTEX_POINT('',#60522);
#1928=VERTEX_POINT('',#60749);
#1929=VERTEX_POINT('',#60760);
#1930=VERTEX_POINT('',#60771);
#1931=VERTEX_POINT('',#60998);
#1932=VERTEX_POINT('',#61009);
#1933=VERTEX_POINT('',#61020);
#1934=VERTEX_POINT('',#61032);
#1935=VERTEX_POINT('',#61043);
#1936=VERTEX_POINT('',#61270);
#1937=VERTEX_POINT('',#61281);
#1938=VERTEX_POINT('',#61508);
#1939=VERTEX_POINT('',#61519);
#1940=VERTEX_POINT('',#61530);
#1941=VERTEX_POINT('',#61715);
#1942=VERTEX_POINT('',#61717);
#1943=VERTEX_POINT('',#61726);
#1944=VERTEX_POINT('',#61737);
#1945=VERTEX_POINT('',#61964);
#1946=VERTEX_POINT('',#61976);
#1947=VERTEX_POINT('',#61987);
#1948=VERTEX_POINT('',#61998);
#1949=VERTEX_POINT('',#62009);
#1950=VERTEX_POINT('',#62239);
#1951=VERTEX_POINT('',#62250);
#1952=VERTEX_POINT('',#62261);
#1953=VERTEX_POINT('',#62273);
#1954=VERTEX_POINT('',#62284);
#1955=VERTEX_POINT('',#62511);
#1956=VERTEX_POINT('',#62522);
#1957=VERTEX_POINT('',#62752);
#1958=VERTEX_POINT('',#62763);
#1959=VERTEX_POINT('',#62774);
#1960=VERTEX_POINT('',#63001);
#1961=VERTEX_POINT('',#63012);
#1962=VERTEX_POINT('',#63239);
#1963=VERTEX_POINT('',#63250);
#1964=VERTEX_POINT('',#63263);
#1965=VERTEX_POINT('',#63274);
#1966=VERTEX_POINT('',#63285);
#1967=VERTEX_POINT('',#63512);
#1968=VERTEX_POINT('',#63523);
#1969=VERTEX_POINT('',#63750);
#1970=VERTEX_POINT('',#63761);
#1971=VERTEX_POINT('',#63774);
#1972=VERTEX_POINT('',#63785);
#1973=VERTEX_POINT('',#63796);
#1974=VERTEX_POINT('',#64023);
#1975=VERTEX_POINT('',#64034);
#1976=VERTEX_POINT('',#64261);
#1977=VERTEX_POINT('',#64488);
#1978=VERTEX_POINT('',#64501);
#1979=VERTEX_POINT('',#64728);
#1980=VERTEX_POINT('',#64955);
#1981=VERTEX_POINT('',#64967);
#1982=VERTEX_POINT('',#64978);
#1983=VERTEX_POINT('',#64989);
#1984=VERTEX_POINT('',#65216);
#1985=VERTEX_POINT('',#65229);
#1986=VERTEX_POINT('',#65456);
#1987=VERTEX_POINT('',#65683);
#1988=VERTEX_POINT('',#65695);
#1989=VERTEX_POINT('',#65706);
#1990=VERTEX_POINT('',#65717);
#1991=VERTEX_POINT('',#65944);
#1992=VERTEX_POINT('',#65957);
#1993=VERTEX_POINT('',#65968);
#1994=VERTEX_POINT('',#65979);
#1995=VERTEX_POINT('',#65991);
#1996=VERTEX_POINT('',#66218);
#1997=VERTEX_POINT('',#66229);
#1998=VERTEX_POINT('',#66456);
#1999=VERTEX_POINT('',#66468);
#2000=VERTEX_POINT('',#66695);
#2001=VERTEX_POINT('',#66922);
#2002=VERTEX_POINT('',#66934);
#2003=VERTEX_POINT('',#67161);
#2004=VERTEX_POINT('',#67172);
#2005=VERTEX_POINT('',#67183);
#2006=VERTEX_POINT('',#67196);
#2007=VERTEX_POINT('',#67423);
#2008=VERTEX_POINT('',#67650);
#2009=VERTEX_POINT('',#67662);
#2010=VERTEX_POINT('',#67889);
#2011=VERTEX_POINT('',#67900);
#2012=VERTEX_POINT('',#67911);
#2013=VERTEX_POINT('',#67923);
#2014=VERTEX_POINT('',#68153);
#2015=VERTEX_POINT('',#68380);
#2016=VERTEX_POINT('',#68392);
#2017=VERTEX_POINT('',#68403);
#2018=VERTEX_POINT('',#68630);
#2019=VERTEX_POINT('',#68641);
#2020=VERTEX_POINT('',#68868);
#2021=VERTEX_POINT('',#68879);
#2022=VERTEX_POINT('',#68890);
#2023=VERTEX_POINT('',#68902);
#2024=VERTEX_POINT('',#68913);
#2025=VERTEX_POINT('',#69151);
#2026=VERTEX_POINT('',#69326);
#2027=VERTEX_POINT('',#69328);
#2028=VERTEX_POINT('',#73885);
#2029=EDGE_CURVE('',#1461,#1461,#1366,.T.);
#2030=EDGE_CURVE('',#1461,#1462,#1010,.T.);
#2031=EDGE_CURVE('',#1462,#1462,#1367,.T.);
#2032=EDGE_CURVE('',#1463,#1463,#1368,.T.);
#2033=EDGE_CURVE('',#1464,#1464,#1369,.T.);
#2034=EDGE_CURVE('',#1465,#1466,#1370,.T.);
#2035=EDGE_CURVE('',#1466,#1465,#1371,.T.);
#2036=EDGE_CURVE('',#1466,#1464,#1011,.T.);
#2037=EDGE_CURVE('',#1467,#1468,#1012,.T.);
#2038=EDGE_CURVE('',#1468,#1469,#526,.T.);
#2039=EDGE_CURVE('',#1469,#1470,#1013,.T.);
#2040=EDGE_CURVE('',#1467,#1470,#527,.T.);
#2041=EDGE_CURVE('',#1468,#1471,#1014,.T.);
#2042=EDGE_CURVE('',#1471,#1472,#528,.T.);
#2043=EDGE_CURVE('',#1472,#1469,#1015,.T.);
#2044=EDGE_CURVE('',#1471,#1473,#1016,.T.);
#2045=EDGE_CURVE('',#1473,#1474,#529,.T.);
#2046=EDGE_CURVE('',#1474,#1472,#1017,.T.);
#2047=EDGE_CURVE('',#1475,#1476,#1018,.T.);
#2048=EDGE_CURVE('',#1476,#1477,#530,.T.);
#2049=EDGE_CURVE('',#1477,#1478,#1019,.T.);
#2050=EDGE_CURVE('',#1478,#1475,#531,.T.);
#2051=EDGE_CURVE('',#1479,#1477,#1020,.T.);
#2052=EDGE_CURVE('',#1476,#1480,#1021,.T.);
#2053=EDGE_CURVE('',#1480,#1479,#532,.T.);
#2054=EDGE_CURVE('',#1473,#1475,#1022,.T.);
#2055=EDGE_CURVE('',#1478,#1474,#1023,.T.);
#2056=EDGE_CURVE('',#1481,#1479,#1024,.T.);
#2057=EDGE_CURVE('',#1480,#1482,#1025,.T.);
#2058=EDGE_CURVE('',#1482,#1481,#533,.T.);
#2059=EDGE_CURVE('',#1470,#1481,#1026,.T.);
#2060=EDGE_CURVE('',#1482,#1467,#1027,.T.);
#2061=EDGE_CURVE('',#1472,#1483,#1028,.T.);
#2062=EDGE_CURVE('',#1484,#1483,#1029,.T.);
#2063=EDGE_CURVE('',#1469,#1484,#1030,.T.);
#2064=EDGE_CURVE('',#1474,#1485,#1031,.T.);
#2065=EDGE_CURVE('',#1483,#1485,#1032,.T.);
#2066=EDGE_CURVE('',#1478,#1486,#1033,.T.);
#2067=EDGE_CURVE('',#1485,#1486,#1034,.T.);
#2068=EDGE_CURVE('',#1477,#1487,#1035,.T.);
#2069=EDGE_CURVE('',#1486,#1487,#1036,.T.);
#2070=EDGE_CURVE('',#1488,#1488,#1372,.T.);
#2071=EDGE_CURVE('',#1489,#1489,#1373,.T.);
#2072=EDGE_CURVE('',#1490,#1490,#1374,.T.);
#2073=EDGE_CURVE('',#1491,#1491,#1375,.T.);
#2074=EDGE_CURVE('',#1492,#1492,#1376,.T.);
#2075=EDGE_CURVE('',#1493,#1494,#1377,.T.);
#2076=EDGE_CURVE('',#1494,#1488,#1378,.T.);
#2077=EDGE_CURVE('',#1494,#1493,#1379,.T.);
#2078=EDGE_CURVE('',#1493,#1495,#1037,.T.);
#2079=EDGE_CURVE('',#1496,#1495,#1380,.T.);
#2080=EDGE_CURVE('',#1495,#1496,#1381,.T.);
#2081=EDGE_CURVE('',#1497,#1498,#1382,.T.);
#2082=EDGE_CURVE('',#1498,#1492,#1383,.T.);
#2083=EDGE_CURVE('',#1498,#1497,#1384,.T.);
#2084=EDGE_CURVE('',#1497,#1499,#1038,.T.);
#2085=EDGE_CURVE('',#1500,#1499,#1385,.T.);
#2086=EDGE_CURVE('',#1499,#1500,#1386,.T.);
#2087=EDGE_CURVE('',#1501,#1502,#1387,.T.);
#2088=EDGE_CURVE('',#1502,#1489,#1388,.T.);
#2089=EDGE_CURVE('',#1502,#1501,#1389,.T.);
#2090=EDGE_CURVE('',#1501,#1503,#1039,.T.);
#2091=EDGE_CURVE('',#1504,#1503,#1390,.T.);
#2092=EDGE_CURVE('',#1503,#1504,#1391,.T.);
#2093=EDGE_CURVE('',#1465,#1491,#1392,.T.);
#2094=EDGE_CURVE('',#1463,#1505,#1040,.T.);
#2095=EDGE_CURVE('',#1506,#1505,#1393,.T.);
#2096=EDGE_CURVE('',#1505,#1506,#1394,.T.);
#2097=EDGE_CURVE('',#1507,#1508,#1395,.T.);
#2098=EDGE_CURVE('',#1508,#1490,#1396,.T.);
#2099=EDGE_CURVE('',#1508,#1507,#1397,.T.);
#2100=EDGE_CURVE('',#1507,#1509,#1041,.T.);
#2101=EDGE_CURVE('',#1510,#1509,#1398,.T.);
#2102=EDGE_CURVE('',#1509,#1510,#1399,.T.);
#2103=EDGE_CURVE('',#1511,#1512,#1042,.T.);
#2104=EDGE_CURVE('',#1512,#1513,#534,.T.);
#2105=EDGE_CURVE('',#1513,#1484,#1043,.T.);
#2106=EDGE_CURVE('',#1511,#1484,#535,.T.);
#2107=EDGE_CURVE('',#1512,#1514,#1044,.T.);
#2108=EDGE_CURVE('',#1514,#1515,#536,.T.);
#2109=EDGE_CURVE('',#1515,#1513,#1045,.T.);
#2110=EDGE_CURVE('',#1514,#1516,#1046,.T.);
#2111=EDGE_CURVE('',#1516,#1517,#537,.T.);
#2112=EDGE_CURVE('',#1517,#1515,#1047,.T.);
#2113=EDGE_CURVE('',#1516,#1518,#1048,.T.);
#2114=EDGE_CURVE('',#1518,#1487,#538,.T.);
#2115=EDGE_CURVE('',#1487,#1517,#1049,.T.);
#2116=EDGE_CURVE('',#1518,#1519,#1050,.T.);
#2117=EDGE_CURVE('',#1519,#1486,#539,.T.);
#2118=EDGE_CURVE('',#1519,#1520,#1051,.T.);
#2119=EDGE_CURVE('',#1520,#1485,#540,.T.);
#2120=EDGE_CURVE('',#1520,#1521,#1052,.T.);
#2121=EDGE_CURVE('',#1521,#1483,#541,.T.);
#2122=EDGE_CURVE('',#1521,#1511,#1053,.T.);
#2123=EDGE_CURVE('',#1470,#1513,#1054,.T.);
#2124=EDGE_CURVE('',#1522,#1522,#1400,.T.);
#2125=EDGE_CURVE('',#1523,#1523,#1401,.T.);
#2126=EDGE_CURVE('',#1524,#1524,#1402,.T.);
#2127=EDGE_CURVE('',#1525,#1525,#1403,.T.);
#2128=EDGE_CURVE('',#1526,#1526,#1404,.T.);
#2129=EDGE_CURVE('',#1522,#1496,#1405,.T.);
#2130=EDGE_CURVE('',#1526,#1500,#1406,.T.);
#2131=EDGE_CURVE('',#1523,#1504,#1407,.T.);
#2132=EDGE_CURVE('',#1525,#1506,#1408,.T.);
#2133=EDGE_CURVE('',#1524,#1510,#1409,.T.);
#2134=EDGE_CURVE('',#1481,#1515,#1055,.T.);
#2135=EDGE_CURVE('',#1479,#1517,#1056,.T.);
#2136=EDGE_CURVE('',#1527,#1527,#1410,.T.);
#2137=EDGE_CURVE('',#1528,#1528,#1411,.T.);
#2138=EDGE_CURVE('',#1529,#1529,#1412,.T.);
#2139=EDGE_CURVE('',#1530,#1530,#1413,.T.);
#2140=EDGE_CURVE('',#1531,#1531,#1414,.T.);
#2141=EDGE_CURVE('',#1531,#1532,#1415,.T.);
#2142=EDGE_CURVE('',#1532,#1532,#1416,.T.);
#2143=EDGE_CURVE('',#1533,#1534,#1057,.T.);
#2144=EDGE_CURVE('',#1535,#1533,#1058,.T.);
#2145=EDGE_CURVE('',#1536,#1535,#1059,.T.);
#2146=EDGE_CURVE('',#1537,#1536,#1060,.T.);
#2147=EDGE_CURVE('',#1538,#1537,#1061,.T.);
#2148=EDGE_CURVE('',#1539,#1538,#1062,.T.);
#2149=EDGE_CURVE('',#1540,#1539,#1063,.T.);
#2150=EDGE_CURVE('',#1534,#1540,#1064,.T.);
#2151=EDGE_CURVE('',#1541,#1541,#1417,.T.);
#2152=EDGE_CURVE('',#1542,#1542,#1418,.T.);
#2153=EDGE_CURVE('',#1543,#1543,#1419,.T.);
#2154=EDGE_CURVE('',#1544,#1544,#1420,.T.);
#2155=EDGE_CURVE('',#1532,#1545,#1065,.T.);
#2156=EDGE_CURVE('',#1545,#1545,#1421,.T.);
#2157=EDGE_CURVE('',#1541,#1546,#1422,.T.);
#2158=EDGE_CURVE('',#1546,#1546,#1423,.T.);
#2159=EDGE_CURVE('',#1546,#1547,#1066,.T.);
#2160=EDGE_CURVE('',#1548,#1547,#1424,.T.);
#2161=EDGE_CURVE('',#1547,#1548,#1425,.T.);
#2162=EDGE_CURVE('',#1544,#1549,#1426,.T.);
#2163=EDGE_CURVE('',#1549,#1549,#1427,.T.);
#2164=EDGE_CURVE('',#1549,#1550,#1067,.T.);
#2165=EDGE_CURVE('',#1551,#1550,#1428,.T.);
#2166=EDGE_CURVE('',#1550,#1551,#1429,.T.);
#2167=EDGE_CURVE('',#1542,#1528,#1430,.T.);
#2168=EDGE_CURVE('',#1543,#1552,#1431,.T.);
#2169=EDGE_CURVE('',#1552,#1552,#1432,.T.);
#2170=EDGE_CURVE('',#1552,#1553,#1068,.T.);
#2171=EDGE_CURVE('',#1554,#1553,#1433,.T.);
#2172=EDGE_CURVE('',#1553,#1554,#1434,.T.);
#2173=EDGE_CURVE('',#1537,#1555,#542,.T.);
#2174=EDGE_CURVE('',#1555,#1556,#1069,.T.);
#2175=EDGE_CURVE('',#1538,#1556,#543,.T.);
#2176=EDGE_CURVE('',#1536,#1557,#544,.T.);
#2177=EDGE_CURVE('',#1557,#1555,#1070,.T.);
#2178=EDGE_CURVE('',#1535,#1558,#545,.T.);
#2179=EDGE_CURVE('',#1558,#1557,#1071,.T.);
#2180=EDGE_CURVE('',#1534,#1559,#546,.T.);
#2181=EDGE_CURVE('',#1559,#1560,#1072,.T.);
#2182=EDGE_CURVE('',#1560,#1533,#547,.T.);
#2183=EDGE_CURVE('',#1561,#1559,#1073,.T.);
#2184=EDGE_CURVE('',#1540,#1561,#548,.T.);
#2185=EDGE_CURVE('',#1560,#1558,#1074,.T.);
#2186=EDGE_CURVE('',#1562,#1561,#1075,.T.);
#2187=EDGE_CURVE('',#1539,#1562,#549,.T.);
#2188=EDGE_CURVE('',#1556,#1562,#1076,.T.);
#2189=EDGE_CURVE('',#1557,#1563,#1077,.T.);
#2190=EDGE_CURVE('',#1564,#1563,#1078,.T.);
#2191=EDGE_CURVE('',#1555,#1564,#1079,.T.);
#2192=EDGE_CURVE('',#1558,#1565,#1080,.T.);
#2193=EDGE_CURVE('',#1563,#1565,#1081,.T.);
#2194=EDGE_CURVE('',#1560,#1566,#1082,.T.);
#2195=EDGE_CURVE('',#1565,#1566,#1083,.T.);
#2196=EDGE_CURVE('',#1559,#1567,#1084,.T.);
#2197=EDGE_CURVE('',#1566,#1567,#1085,.T.);
#2198=EDGE_CURVE('',#1562,#1568,#1086,.T.);
#2199=EDGE_CURVE('',#1569,#1568,#1087,.T.);
#2200=EDGE_CURVE('',#1561,#1569,#1088,.T.);
#2201=EDGE_CURVE('',#1567,#1569,#1089,.T.);
#2202=EDGE_CURVE('',#1556,#1570,#1090,.T.);
#2203=EDGE_CURVE('',#1568,#1570,#1091,.T.);
#2204=EDGE_CURVE('',#1570,#1564,#1092,.T.);
#2205=EDGE_CURVE('',#1571,#1571,#1435,.T.);
#2206=EDGE_CURVE('',#1571,#1548,#1436,.T.);
#2207=EDGE_CURVE('',#1572,#1573,#1093,.T.);
#2208=EDGE_CURVE('',#1574,#1572,#1094,.T.);
#2209=EDGE_CURVE('',#1575,#1574,#1095,.T.);
#2210=EDGE_CURVE('',#1576,#1575,#1096,.T.);
#2211=EDGE_CURVE('',#1577,#1576,#1097,.T.);
#2212=EDGE_CURVE('',#1578,#1577,#1098,.T.);
#2213=EDGE_CURVE('',#1579,#1578,#1099,.T.);
#2214=EDGE_CURVE('',#1573,#1579,#1100,.T.);
#2215=EDGE_CURVE('',#1580,#1580,#1437,.T.);
#2216=EDGE_CURVE('',#1581,#1581,#1438,.T.);
#2217=EDGE_CURVE('',#1582,#1582,#1439,.T.);
#2218=EDGE_CURVE('',#1583,#1583,#1440,.T.);
#2219=EDGE_CURVE('',#1580,#1551,#1441,.T.);
#2220=EDGE_CURVE('',#1583,#1530,#1442,.T.);
#2221=EDGE_CURVE('',#1581,#1554,#1443,.T.);
#2222=EDGE_CURVE('',#1576,#1563,#550,.T.);
#2223=EDGE_CURVE('',#1577,#1565,#551,.T.);
#2224=EDGE_CURVE('',#1575,#1564,#552,.T.);
#2225=EDGE_CURVE('',#1574,#1570,#553,.T.);
#2226=EDGE_CURVE('',#1573,#1569,#554,.T.);
#2227=EDGE_CURVE('',#1568,#1572,#555,.T.);
#2228=EDGE_CURVE('',#1579,#1567,#556,.T.);
#2229=EDGE_CURVE('',#1578,#1566,#557,.T.);
#2230=EDGE_CURVE('',#1545,#1582,#1444,.T.);
#2231=EDGE_CURVE('',#1527,#1529,#1101,.T.);
#2232=EDGE_CURVE('',#1584,#1584,#1445,.T.);
#2233=EDGE_CURVE('',#1584,#1585,#1102,.T.);
#2234=EDGE_CURVE('',#1585,#1585,#1446,.T.);
#2235=EDGE_CURVE('',#1586,#1586,#1447,.T.);
#2236=EDGE_CURVE('',#1586,#1584,#1448,.T.);
#2237=EDGE_CURVE('',#1587,#1587,#1449,.T.);
#2238=EDGE_CURVE('',#1588,#1588,#1450,.T.);
#2239=EDGE_CURVE('',#1588,#1587,#1451,.T.);
#2240=EDGE_CURVE('',#1589,#1589,#1452,.T.);
#2241=EDGE_CURVE('',#1589,#1588,#1103,.T.);
#2242=EDGE_CURVE('',#1590,#1590,#1453,.T.);
#2243=EDGE_CURVE('',#1590,#1589,#1454,.T.);
#2244=EDGE_CURVE('',#1591,#1591,#1455,.T.);
#2245=EDGE_CURVE('',#1585,#1591,#1456,.T.);
#2246=EDGE_CURVE('',#1592,#1593,#1104,.T.);
#2247=EDGE_CURVE('',#1594,#1592,#49,.T.);
#2248=EDGE_CURVE('',#1595,#1594,#1457,.T.);
#2249=EDGE_CURVE('',#1595,#1593,#50,.T.);
#2250=EDGE_CURVE('',#1596,#1597,#1105,.T.);
#2251=EDGE_CURVE('',#1598,#1596,#51,.F.);
#2252=EDGE_CURVE('',#1592,#1598,#52,.T.);
#2253=EDGE_CURVE('',#1593,#1599,#53,.T.);
#2254=EDGE_CURVE('',#1599,#1597,#54,.T.);
#2255=EDGE_CURVE('',#1600,#1601,#1106,.T.);
#2256=EDGE_CURVE('',#1596,#1600,#55,.F.);
#2257=EDGE_CURVE('',#1597,#1601,#56,.T.);
#2258=EDGE_CURVE('',#1602,#1603,#1107,.T.);
#2259=EDGE_CURVE('',#1604,#1602,#57,.F.);
#2260=EDGE_CURVE('',#1600,#1604,#58,.F.);
#2261=EDGE_CURVE('',#1601,#1605,#59,.T.);
#2262=EDGE_CURVE('',#1605,#1603,#60,.T.);
#2263=EDGE_CURVE('',#1606,#1607,#1108,.T.);
#2264=EDGE_CURVE('',#1602,#1606,#61,.F.);
#2265=EDGE_CURVE('',#1603,#1607,#62,.T.);
#2266=EDGE_CURVE('',#1608,#1609,#1109,.T.);
#2267=EDGE_CURVE('',#1610,#1608,#63,.F.);
#2268=EDGE_CURVE('',#1606,#1610,#64,.F.);
#2269=EDGE_CURVE('',#1607,#1611,#65,.T.);
#2270=EDGE_CURVE('',#1611,#1609,#66,.T.);
#2271=EDGE_CURVE('',#1612,#1613,#1110,.T.);
#2272=EDGE_CURVE('',#1608,#1612,#67,.F.);
#2273=EDGE_CURVE('',#1609,#1613,#68,.T.);
#2274=EDGE_CURVE('',#1614,#1615,#1111,.T.);
#2275=EDGE_CURVE('',#1616,#1614,#69,.F.);
#2276=EDGE_CURVE('',#1612,#1616,#70,.F.);
#2277=EDGE_CURVE('',#1613,#1617,#71,.T.);
#2278=EDGE_CURVE('',#1617,#1615,#72,.T.);
#2279=EDGE_CURVE('',#1618,#1619,#1112,.T.);
#2280=EDGE_CURVE('',#1614,#1618,#73,.F.);
#2281=EDGE_CURVE('',#1615,#1619,#74,.T.);
#2282=EDGE_CURVE('',#1620,#1621,#1113,.T.);
#2283=EDGE_CURVE('',#1622,#1620,#75,.F.);
#2284=EDGE_CURVE('',#1618,#1622,#76,.F.);
#2285=EDGE_CURVE('',#1619,#1623,#77,.T.);
#2286=EDGE_CURVE('',#1623,#1621,#78,.T.);
#2287=EDGE_CURVE('',#1624,#1625,#1114,.T.);
#2288=EDGE_CURVE('',#1620,#1624,#79,.F.);
#2289=EDGE_CURVE('',#1621,#1625,#80,.T.);
#2290=EDGE_CURVE('',#1626,#1627,#1115,.T.);
#2291=EDGE_CURVE('',#1628,#1626,#81,.F.);
#2292=EDGE_CURVE('',#1624,#1628,#82,.F.);
#2293=EDGE_CURVE('',#1625,#1629,#83,.T.);
#2294=EDGE_CURVE('',#1629,#1627,#84,.T.);
#2295=EDGE_CURVE('',#1630,#1631,#1116,.T.);
#2296=EDGE_CURVE('',#1626,#1630,#85,.F.);
#2297=EDGE_CURVE('',#1627,#1631,#86,.T.);
#2298=EDGE_CURVE('',#1632,#1633,#1117,.T.);
#2299=EDGE_CURVE('',#1634,#1632,#87,.F.);
#2300=EDGE_CURVE('',#1630,#1634,#88,.F.);
#2301=EDGE_CURVE('',#1631,#1635,#89,.T.);
#2302=EDGE_CURVE('',#1635,#1633,#90,.T.);
#2303=EDGE_CURVE('',#1636,#1637,#1118,.T.);
#2304=EDGE_CURVE('',#1632,#1636,#91,.F.);
#2305=EDGE_CURVE('',#1633,#1637,#92,.T.);
#2306=EDGE_CURVE('',#1638,#1639,#1119,.T.);
#2307=EDGE_CURVE('',#1640,#1638,#93,.F.);
#2308=EDGE_CURVE('',#1636,#1640,#94,.F.);
#2309=EDGE_CURVE('',#1637,#1641,#95,.T.);
#2310=EDGE_CURVE('',#1641,#1639,#96,.T.);
#2311=EDGE_CURVE('',#1642,#1643,#1120,.T.);
#2312=EDGE_CURVE('',#1638,#1642,#97,.F.);
#2313=EDGE_CURVE('',#1639,#1644,#98,.T.);
#2314=EDGE_CURVE('',#1644,#1643,#99,.T.);
#2315=EDGE_CURVE('',#1645,#1646,#1121,.T.);
#2316=EDGE_CURVE('',#1647,#1645,#100,.F.);
#2317=EDGE_CURVE('',#1642,#1647,#101,.F.);
#2318=EDGE_CURVE('',#1643,#1646,#102,.T.);
#2319=EDGE_CURVE('',#1648,#1649,#1122,.T.);
#2320=EDGE_CURVE('',#1645,#1648,#103,.F.);
#2321=EDGE_CURVE('',#1646,#1650,#104,.T.);
#2322=EDGE_CURVE('',#1650,#1649,#105,.T.);
#2323=EDGE_CURVE('',#1651,#1652,#1123,.T.);
#2324=EDGE_CURVE('',#1653,#1651,#106,.F.);
#2325=EDGE_CURVE('',#1648,#1653,#107,.F.);
#2326=EDGE_CURVE('',#1649,#1652,#108,.T.);
#2327=EDGE_CURVE('',#1654,#1655,#1124,.T.);
#2328=EDGE_CURVE('',#1651,#1654,#109,.F.);
#2329=EDGE_CURVE('',#1652,#1656,#110,.T.);
#2330=EDGE_CURVE('',#1656,#1655,#111,.T.);
#2331=EDGE_CURVE('',#1657,#1658,#1125,.T.);
#2332=EDGE_CURVE('',#1659,#1657,#112,.F.);
#2333=EDGE_CURVE('',#1654,#1659,#113,.F.);
#2334=EDGE_CURVE('',#1655,#1658,#114,.T.);
#2335=EDGE_CURVE('',#1660,#1661,#1126,.T.);
#2336=EDGE_CURVE('',#1657,#1660,#115,.F.);
#2337=EDGE_CURVE('',#1658,#1662,#116,.T.);
#2338=EDGE_CURVE('',#1662,#1661,#117,.T.);
#2339=EDGE_CURVE('',#1663,#1664,#1127,.T.);
#2340=EDGE_CURVE('',#1665,#1663,#118,.F.);
#2341=EDGE_CURVE('',#1660,#1665,#119,.F.);
#2342=EDGE_CURVE('',#1661,#1664,#120,.T.);
#2343=EDGE_CURVE('',#1666,#1667,#1128,.T.);
#2344=EDGE_CURVE('',#1663,#1666,#121,.F.);
#2345=EDGE_CURVE('',#1664,#1668,#122,.T.);
#2346=EDGE_CURVE('',#1668,#1667,#123,.T.);
#2347=EDGE_CURVE('',#1669,#1670,#1129,.T.);
#2348=EDGE_CURVE('',#1671,#1669,#124,.F.);
#2349=EDGE_CURVE('',#1666,#1671,#125,.F.);
#2350=EDGE_CURVE('',#1667,#1670,#126,.T.);
#2351=EDGE_CURVE('',#1672,#1673,#1130,.T.);
#2352=EDGE_CURVE('',#1669,#1672,#127,.F.);
#2353=EDGE_CURVE('',#1670,#1674,#128,.T.);
#2354=EDGE_CURVE('',#1674,#1673,#129,.T.);
#2355=EDGE_CURVE('',#1675,#1676,#1131,.T.);
#2356=EDGE_CURVE('',#1677,#1675,#130,.F.);
#2357=EDGE_CURVE('',#1672,#1677,#131,.F.);
#2358=EDGE_CURVE('',#1673,#1676,#132,.T.);
#2359=EDGE_CURVE('',#1678,#1679,#1132,.T.);
#2360=EDGE_CURVE('',#1675,#1678,#133,.F.);
#2361=EDGE_CURVE('',#1676,#1680,#134,.T.);
#2362=EDGE_CURVE('',#1680,#1679,#135,.T.);
#2363=EDGE_CURVE('',#1681,#1682,#1133,.T.);
#2364=EDGE_CURVE('',#1683,#1681,#136,.F.);
#2365=EDGE_CURVE('',#1678,#1683,#137,.F.);
#2366=EDGE_CURVE('',#1679,#1682,#138,.T.);
#2367=EDGE_CURVE('',#1684,#1685,#1134,.T.);
#2368=EDGE_CURVE('',#1681,#1684,#139,.F.);
#2369=EDGE_CURVE('',#1682,#1686,#140,.T.);
#2370=EDGE_CURVE('',#1686,#1685,#141,.T.);
#2371=EDGE_CURVE('',#1687,#1688,#1135,.T.);
#2372=EDGE_CURVE('',#1689,#1687,#142,.F.);
#2373=EDGE_CURVE('',#1684,#1689,#143,.F.);
#2374=EDGE_CURVE('',#1685,#1688,#144,.T.);
#2375=EDGE_CURVE('',#1690,#1691,#1136,.T.);
#2376=EDGE_CURVE('',#1687,#1690,#145,.F.);
#2377=EDGE_CURVE('',#1688,#1692,#146,.T.);
#2378=EDGE_CURVE('',#1692,#1691,#147,.T.);
#2379=EDGE_CURVE('',#1693,#1694,#1137,.T.);
#2380=EDGE_CURVE('',#1695,#1693,#148,.F.);
#2381=EDGE_CURVE('',#1690,#1695,#149,.F.);
#2382=EDGE_CURVE('',#1691,#1694,#150,.T.);
#2383=EDGE_CURVE('',#1696,#1697,#1138,.T.);
#2384=EDGE_CURVE('',#1693,#1696,#151,.F.);
#2385=EDGE_CURVE('',#1694,#1698,#152,.T.);
#2386=EDGE_CURVE('',#1698,#1697,#153,.T.);
#2387=EDGE_CURVE('',#1699,#1700,#1139,.T.);
#2388=EDGE_CURVE('',#1701,#1699,#154,.F.);
#2389=EDGE_CURVE('',#1696,#1701,#155,.F.);
#2390=EDGE_CURVE('',#1697,#1700,#156,.T.);
#2391=EDGE_CURVE('',#1702,#1703,#1140,.T.);
#2392=EDGE_CURVE('',#1699,#1702,#157,.F.);
#2393=EDGE_CURVE('',#1700,#1704,#158,.T.);
#2394=EDGE_CURVE('',#1704,#1703,#159,.T.);
#2395=EDGE_CURVE('',#1705,#1706,#1141,.T.);
#2396=EDGE_CURVE('',#1707,#1705,#160,.F.);
#2397=EDGE_CURVE('',#1702,#1707,#161,.F.);
#2398=EDGE_CURVE('',#1703,#1708,#162,.T.);
#2399=EDGE_CURVE('',#1708,#1706,#163,.T.);
#2400=EDGE_CURVE('',#1709,#1710,#1142,.T.);
#2401=EDGE_CURVE('',#1705,#1709,#164,.F.);
#2402=EDGE_CURVE('',#1706,#1710,#165,.T.);
#2403=EDGE_CURVE('',#1711,#1712,#1143,.T.);
#2404=EDGE_CURVE('',#1713,#1711,#166,.F.);
#2405=EDGE_CURVE('',#1709,#1713,#167,.F.);
#2406=EDGE_CURVE('',#1710,#1714,#168,.T.);
#2407=EDGE_CURVE('',#1714,#1712,#169,.T.);
#2408=EDGE_CURVE('',#1715,#1716,#1144,.T.);
#2409=EDGE_CURVE('',#1711,#1715,#170,.F.);
#2410=EDGE_CURVE('',#1712,#1717,#171,.T.);
#2411=EDGE_CURVE('',#1717,#1716,#172,.T.);
#2412=EDGE_CURVE('',#1718,#1719,#1145,.T.);
#2413=EDGE_CURVE('',#1720,#1718,#173,.F.);
#2414=EDGE_CURVE('',#1715,#1720,#174,.F.);
#2415=EDGE_CURVE('',#1716,#1719,#175,.T.);
#2416=EDGE_CURVE('',#1721,#1722,#1146,.T.);
#2417=EDGE_CURVE('',#1718,#1721,#176,.F.);
#2418=EDGE_CURVE('',#1719,#1723,#177,.T.);
#2419=EDGE_CURVE('',#1723,#1722,#178,.T.);
#2420=EDGE_CURVE('',#1724,#1725,#1147,.T.);
#2421=EDGE_CURVE('',#1726,#1724,#179,.T.);
#2422=EDGE_CURVE('',#1721,#1726,#180,.F.);
#2423=EDGE_CURVE('',#1722,#1725,#181,.T.);
#2424=EDGE_CURVE('',#1727,#1728,#1148,.T.);
#2425=EDGE_CURVE('',#1729,#1727,#182,.F.);
#2426=EDGE_CURVE('',#1724,#1729,#183,.T.);
#2427=EDGE_CURVE('',#1725,#1730,#184,.T.);
#2428=EDGE_CURVE('',#1730,#1728,#185,.T.);
#2429=EDGE_CURVE('',#1731,#1732,#1149,.T.);
#2430=EDGE_CURVE('',#1727,#1731,#186,.F.);
#2431=EDGE_CURVE('',#1728,#1733,#187,.T.);
#2432=EDGE_CURVE('',#1733,#1732,#188,.T.);
#2433=EDGE_CURVE('',#1734,#1735,#1150,.T.);
#2434=EDGE_CURVE('',#1736,#1734,#189,.F.);
#2435=EDGE_CURVE('',#1731,#1736,#190,.F.);
#2436=EDGE_CURVE('',#1732,#1735,#191,.T.);
#2437=EDGE_CURVE('',#1737,#1738,#1151,.T.);
#2438=EDGE_CURVE('',#1734,#1737,#192,.F.);
#2439=EDGE_CURVE('',#1735,#1739,#193,.T.);
#2440=EDGE_CURVE('',#1739,#1738,#194,.T.);
#2441=EDGE_CURVE('',#1740,#1741,#1152,.T.);
#2442=EDGE_CURVE('',#1742,#1740,#195,.F.);
#2443=EDGE_CURVE('',#1737,#1742,#196,.F.);
#2444=EDGE_CURVE('',#1738,#1741,#197,.T.);
#2445=EDGE_CURVE('',#1743,#1744,#1153,.T.);
#2446=EDGE_CURVE('',#1740,#1743,#198,.F.);
#2447=EDGE_CURVE('',#1741,#1745,#199,.T.);
#2448=EDGE_CURVE('',#1745,#1744,#200,.T.);
#2449=EDGE_CURVE('',#1746,#1747,#1154,.T.);
#2450=EDGE_CURVE('',#1748,#1746,#201,.T.);
#2451=EDGE_CURVE('',#1743,#1748,#202,.F.);
#2452=EDGE_CURVE('',#1744,#1749,#203,.T.);
#2453=EDGE_CURVE('',#1749,#1747,#204,.T.);
#2454=EDGE_CURVE('',#1750,#1751,#1155,.T.);
#2455=EDGE_CURVE('',#1752,#1750,#205,.F.);
#2456=EDGE_CURVE('',#1746,#1752,#206,.T.);
#2457=EDGE_CURVE('',#1747,#1751,#207,.T.);
#2458=EDGE_CURVE('',#1753,#1754,#1156,.T.);
#2459=EDGE_CURVE('',#1750,#1753,#208,.F.);
#2460=EDGE_CURVE('',#1751,#1755,#209,.T.);
#2461=EDGE_CURVE('',#1755,#1754,#210,.T.);
#2462=EDGE_CURVE('',#1756,#1757,#1157,.T.);
#2463=EDGE_CURVE('',#1758,#1756,#211,.F.);
#2464=EDGE_CURVE('',#1753,#1758,#212,.F.);
#2465=EDGE_CURVE('',#1754,#1759,#213,.T.);
#2466=EDGE_CURVE('',#1759,#1757,#214,.T.);
#2467=EDGE_CURVE('',#1760,#1761,#1158,.T.);
#2468=EDGE_CURVE('',#1756,#1760,#215,.F.);
#2469=EDGE_CURVE('',#1757,#1761,#216,.T.);
#2470=EDGE_CURVE('',#1762,#1763,#1159,.T.);
#2471=EDGE_CURVE('',#1764,#1762,#217,.F.);
#2472=EDGE_CURVE('',#1760,#1764,#218,.F.);
#2473=EDGE_CURVE('',#1761,#1765,#219,.T.);
#2474=EDGE_CURVE('',#1765,#1763,#220,.T.);
#2475=EDGE_CURVE('',#1766,#1767,#1160,.T.);
#2476=EDGE_CURVE('',#1762,#1766,#221,.F.);
#2477=EDGE_CURVE('',#1763,#1768,#222,.T.);
#2478=EDGE_CURVE('',#1768,#1767,#223,.T.);
#2479=EDGE_CURVE('',#1769,#1770,#1161,.T.);
#2480=EDGE_CURVE('',#1771,#1769,#224,.F.);
#2481=EDGE_CURVE('',#1766,#1771,#225,.F.);
#2482=EDGE_CURVE('',#1767,#1770,#226,.T.);
#2483=EDGE_CURVE('',#1772,#1773,#1162,.T.);
#2484=EDGE_CURVE('',#1769,#1772,#227,.F.);
#2485=EDGE_CURVE('',#1770,#1774,#228,.T.);
#2486=EDGE_CURVE('',#1774,#1773,#229,.T.);
#2487=EDGE_CURVE('',#1775,#1776,#1163,.T.);
#2488=EDGE_CURVE('',#1777,#1775,#230,.F.);
#2489=EDGE_CURVE('',#1772,#1777,#231,.F.);
#2490=EDGE_CURVE('',#1773,#1776,#232,.T.);
#2491=EDGE_CURVE('',#1778,#1779,#1164,.T.);
#2492=EDGE_CURVE('',#1775,#1778,#233,.F.);
#2493=EDGE_CURVE('',#1776,#1780,#234,.T.);
#2494=EDGE_CURVE('',#1780,#1779,#235,.T.);
#2495=EDGE_CURVE('',#1781,#1782,#1165,.T.);
#2496=EDGE_CURVE('',#1783,#1781,#236,.F.);
#2497=EDGE_CURVE('',#1778,#1783,#237,.F.);
#2498=EDGE_CURVE('',#1779,#1782,#238,.T.);
#2499=EDGE_CURVE('',#1784,#1785,#1166,.T.);
#2500=EDGE_CURVE('',#1781,#1784,#239,.F.);
#2501=EDGE_CURVE('',#1782,#1786,#240,.T.);
#2502=EDGE_CURVE('',#1786,#1785,#241,.T.);
#2503=EDGE_CURVE('',#1787,#1788,#1167,.T.);
#2504=EDGE_CURVE('',#1789,#1787,#242,.F.);
#2505=EDGE_CURVE('',#1784,#1789,#243,.F.);
#2506=EDGE_CURVE('',#1785,#1788,#244,.T.);
#2507=EDGE_CURVE('',#1790,#1791,#1168,.T.);
#2508=EDGE_CURVE('',#1787,#1790,#245,.F.);
#2509=EDGE_CURVE('',#1788,#1792,#246,.T.);
#2510=EDGE_CURVE('',#1792,#1791,#247,.T.);
#2511=EDGE_CURVE('',#1793,#1794,#1169,.T.);
#2512=EDGE_CURVE('',#1795,#1793,#248,.F.);
#2513=EDGE_CURVE('',#1790,#1795,#249,.F.);
#2514=EDGE_CURVE('',#1791,#1794,#250,.T.);
#2515=EDGE_CURVE('',#1796,#1797,#1170,.T.);
#2516=EDGE_CURVE('',#1793,#1796,#251,.F.);
#2517=EDGE_CURVE('',#1794,#1798,#252,.T.);
#2518=EDGE_CURVE('',#1798,#1797,#253,.T.);
#2519=EDGE_CURVE('',#1799,#1800,#1171,.T.);
#2520=EDGE_CURVE('',#1801,#1799,#254,.F.);
#2521=EDGE_CURVE('',#1796,#1801,#255,.F.);
#2522=EDGE_CURVE('',#1797,#1800,#256,.T.);
#2523=EDGE_CURVE('',#1802,#1803,#1172,.T.);
#2524=EDGE_CURVE('',#1799,#1802,#257,.F.);
#2525=EDGE_CURVE('',#1800,#1804,#258,.T.);
#2526=EDGE_CURVE('',#1804,#1803,#259,.T.);
#2527=EDGE_CURVE('',#1805,#1806,#1173,.T.);
#2528=EDGE_CURVE('',#1807,#1805,#260,.T.);
#2529=EDGE_CURVE('',#1802,#1807,#261,.F.);
#2530=EDGE_CURVE('',#1803,#1806,#262,.T.);
#2531=EDGE_CURVE('',#1808,#1809,#1174,.T.);
#2532=EDGE_CURVE('',#1810,#1808,#263,.T.);
#2533=EDGE_CURVE('',#1805,#1810,#264,.T.);
#2534=EDGE_CURVE('',#1806,#1811,#265,.T.);
#2535=EDGE_CURVE('',#1811,#1809,#266,.T.);
#2536=EDGE_CURVE('',#1812,#1813,#1175,.T.);
#2537=EDGE_CURVE('',#1814,#1812,#267,.F.);
#2538=EDGE_CURVE('',#1808,#1814,#268,.T.);
#2539=EDGE_CURVE('',#1809,#1813,#269,.T.);
#2540=EDGE_CURVE('',#1815,#1816,#1176,.T.);
#2541=EDGE_CURVE('',#1812,#1815,#270,.F.);
#2542=EDGE_CURVE('',#1813,#1817,#271,.T.);
#2543=EDGE_CURVE('',#1817,#1816,#272,.T.);
#2544=EDGE_CURVE('',#1818,#1819,#1177,.T.);
#2545=EDGE_CURVE('',#1820,#1818,#273,.T.);
#2546=EDGE_CURVE('',#1815,#1820,#274,.F.);
#2547=EDGE_CURVE('',#1816,#1821,#275,.T.);
#2548=EDGE_CURVE('',#1821,#1819,#276,.T.);
#2549=EDGE_CURVE('',#1822,#1823,#1178,.T.);
#2550=EDGE_CURVE('',#1824,#1822,#277,.F.);
#2551=EDGE_CURVE('',#1818,#1824,#278,.T.);
#2552=EDGE_CURVE('',#1819,#1823,#279,.T.);
#2553=EDGE_CURVE('',#1825,#1826,#1179,.T.);
#2554=EDGE_CURVE('',#1822,#1825,#280,.F.);
#2555=EDGE_CURVE('',#1823,#1827,#281,.T.);
#2556=EDGE_CURVE('',#1827,#1826,#282,.T.);
#2557=EDGE_CURVE('',#1828,#1829,#1180,.T.);
#2558=EDGE_CURVE('',#1830,#1828,#283,.F.);
#2559=EDGE_CURVE('',#1825,#1830,#284,.F.);
#2560=EDGE_CURVE('',#1826,#1829,#285,.T.);
#2561=EDGE_CURVE('',#1831,#1832,#1181,.T.);
#2562=EDGE_CURVE('',#1828,#1831,#286,.F.);
#2563=EDGE_CURVE('',#1829,#1833,#287,.T.);
#2564=EDGE_CURVE('',#1833,#1832,#288,.T.);
#2565=EDGE_CURVE('',#1834,#1835,#1182,.T.);
#2566=EDGE_CURVE('',#1836,#1834,#289,.F.);
#2567=EDGE_CURVE('',#1831,#1836,#290,.F.);
#2568=EDGE_CURVE('',#1832,#1835,#291,.T.);
#2569=EDGE_CURVE('',#1837,#1838,#1183,.T.);
#2570=EDGE_CURVE('',#1834,#1837,#292,.F.);
#2571=EDGE_CURVE('',#1835,#1839,#293,.T.);
#2572=EDGE_CURVE('',#1839,#1838,#294,.T.);
#2573=EDGE_CURVE('',#1840,#1841,#1184,.T.);
#2574=EDGE_CURVE('',#1842,#1840,#295,.T.);
#2575=EDGE_CURVE('',#1837,#1842,#296,.F.);
#2576=EDGE_CURVE('',#1838,#1841,#297,.T.);
#2577=EDGE_CURVE('',#1843,#1844,#1185,.T.);
#2578=EDGE_CURVE('',#1845,#1843,#298,.F.);
#2579=EDGE_CURVE('',#1840,#1845,#299,.T.);
#2580=EDGE_CURVE('',#1841,#1846,#300,.T.);
#2581=EDGE_CURVE('',#1846,#1844,#301,.T.);
#2582=EDGE_CURVE('',#1847,#1848,#1186,.T.);
#2583=EDGE_CURVE('',#1843,#1847,#302,.F.);
#2584=EDGE_CURVE('',#1844,#1848,#303,.T.);
#2585=EDGE_CURVE('',#1849,#1850,#1187,.T.);
#2586=EDGE_CURVE('',#1851,#1849,#304,.T.);
#2587=EDGE_CURVE('',#1847,#1851,#305,.F.);
#2588=EDGE_CURVE('',#1848,#1852,#306,.T.);
#2589=EDGE_CURVE('',#1852,#1850,#307,.F.);
#2590=EDGE_CURVE('',#1853,#1854,#308,.T.);
#2591=EDGE_CURVE('',#1855,#1854,#1458,.T.);
#2592=EDGE_CURVE('',#1855,#1856,#309,.T.);
#2593=EDGE_CURVE('',#1856,#1857,#310,.T.);
#2594=EDGE_CURVE('',#1857,#1858,#311,.T.);
#2595=EDGE_CURVE('',#1858,#1859,#312,.T.);
#2596=EDGE_CURVE('',#1859,#1860,#313,.T.);
#2597=EDGE_CURVE('',#1860,#1861,#314,.T.);
#2598=EDGE_CURVE('',#1861,#1862,#315,.T.);
#2599=EDGE_CURVE('',#1862,#1863,#316,.T.);
#2600=EDGE_CURVE('',#1863,#1864,#317,.T.);
#2601=EDGE_CURVE('',#1864,#1865,#318,.T.);
#2602=EDGE_CURVE('',#1865,#1866,#319,.T.);
#2603=EDGE_CURVE('',#1866,#1867,#320,.T.);
#2604=EDGE_CURVE('',#1867,#1868,#321,.T.);
#2605=EDGE_CURVE('',#1868,#1869,#322,.T.);
#2606=EDGE_CURVE('',#1869,#1870,#323,.T.);
#2607=EDGE_CURVE('',#1870,#1871,#324,.T.);
#2608=EDGE_CURVE('',#1871,#1872,#325,.T.);
#2609=EDGE_CURVE('',#1872,#1873,#326,.T.);
#2610=EDGE_CURVE('',#1873,#1874,#327,.T.);
#2611=EDGE_CURVE('',#1874,#1875,#328,.T.);
#2612=EDGE_CURVE('',#1875,#1876,#329,.T.);
#2613=EDGE_CURVE('',#1876,#1877,#330,.T.);
#2614=EDGE_CURVE('',#1877,#1878,#331,.T.);
#2615=EDGE_CURVE('',#1878,#1879,#332,.T.);
#2616=EDGE_CURVE('',#1879,#1880,#333,.T.);
#2617=EDGE_CURVE('',#1880,#1881,#334,.T.);
#2618=EDGE_CURVE('',#1881,#1882,#335,.T.);
#2619=EDGE_CURVE('',#1882,#1883,#336,.T.);
#2620=EDGE_CURVE('',#1883,#1884,#337,.T.);
#2621=EDGE_CURVE('',#1884,#1885,#338,.T.);
#2622=EDGE_CURVE('',#1885,#1886,#339,.T.);
#2623=EDGE_CURVE('',#1886,#1887,#340,.T.);
#2624=EDGE_CURVE('',#1887,#1888,#341,.T.);
#2625=EDGE_CURVE('',#1888,#1889,#342,.T.);
#2626=EDGE_CURVE('',#1889,#1890,#343,.T.);
#2627=EDGE_CURVE('',#1890,#1891,#344,.T.);
#2628=EDGE_CURVE('',#1891,#1892,#345,.T.);
#2629=EDGE_CURVE('',#1892,#1893,#346,.T.);
#2630=EDGE_CURVE('',#1893,#1894,#347,.T.);
#2631=EDGE_CURVE('',#1894,#1895,#348,.T.);
#2632=EDGE_CURVE('',#1895,#1896,#349,.T.);
#2633=EDGE_CURVE('',#1896,#1897,#350,.T.);
#2634=EDGE_CURVE('',#1897,#1898,#351,.T.);
#2635=EDGE_CURVE('',#1898,#1899,#352,.T.);
#2636=EDGE_CURVE('',#1899,#1900,#353,.T.);
#2637=EDGE_CURVE('',#1900,#1901,#354,.T.);
#2638=EDGE_CURVE('',#1901,#1902,#355,.T.);
#2639=EDGE_CURVE('',#1902,#1903,#356,.T.);
#2640=EDGE_CURVE('',#1903,#1904,#357,.T.);
#2641=EDGE_CURVE('',#1904,#1905,#358,.T.);
#2642=EDGE_CURVE('',#1905,#1906,#359,.T.);
#2643=EDGE_CURVE('',#1906,#1907,#360,.T.);
#2644=EDGE_CURVE('',#1907,#1908,#361,.T.);
#2645=EDGE_CURVE('',#1908,#1909,#362,.T.);
#2646=EDGE_CURVE('',#1909,#1910,#363,.T.);
#2647=EDGE_CURVE('',#1910,#1911,#364,.T.);
#2648=EDGE_CURVE('',#1911,#1912,#365,.T.);
#2649=EDGE_CURVE('',#1912,#1913,#366,.T.);
#2650=EDGE_CURVE('',#1913,#1914,#367,.T.);
#2651=EDGE_CURVE('',#1914,#1915,#368,.T.);
#2652=EDGE_CURVE('',#1915,#1916,#369,.T.);
#2653=EDGE_CURVE('',#1916,#1917,#370,.T.);
#2654=EDGE_CURVE('',#1917,#1918,#371,.T.);
#2655=EDGE_CURVE('',#1918,#1919,#372,.T.);
#2656=EDGE_CURVE('',#1919,#1920,#373,.T.);
#2657=EDGE_CURVE('',#1920,#1921,#374,.T.);
#2658=EDGE_CURVE('',#1921,#1922,#375,.T.);
#2659=EDGE_CURVE('',#1922,#1923,#376,.T.);
#2660=EDGE_CURVE('',#1923,#1924,#377,.T.);
#2661=EDGE_CURVE('',#1924,#1925,#378,.T.);
#2662=EDGE_CURVE('',#1925,#1926,#379,.T.);
#2663=EDGE_CURVE('',#1926,#1927,#380,.T.);
#2664=EDGE_CURVE('',#1927,#1928,#381,.T.);
#2665=EDGE_CURVE('',#1928,#1929,#382,.T.);
#2666=EDGE_CURVE('',#1929,#1930,#383,.T.);
#2667=EDGE_CURVE('',#1930,#1931,#384,.T.);
#2668=EDGE_CURVE('',#1931,#1932,#385,.T.);
#2669=EDGE_CURVE('',#1932,#1933,#386,.T.);
#2670=EDGE_CURVE('',#1933,#1934,#387,.T.);
#2671=EDGE_CURVE('',#1934,#1935,#388,.T.);
#2672=EDGE_CURVE('',#1935,#1936,#389,.T.);
#2673=EDGE_CURVE('',#1936,#1937,#390,.T.);
#2674=EDGE_CURVE('',#1937,#1938,#391,.T.);
#2675=EDGE_CURVE('',#1938,#1939,#392,.T.);
#2676=EDGE_CURVE('',#1939,#1940,#393,.T.);
#2677=EDGE_CURVE('',#1941,#1940,#1459,.F.);
#2678=EDGE_CURVE('',#1941,#1942,#394,.T.);
#2679=EDGE_CURVE('',#1942,#1943,#395,.T.);
#2680=EDGE_CURVE('',#1943,#1944,#396,.T.);
#2681=EDGE_CURVE('',#1944,#1945,#397,.T.);
#2682=EDGE_CURVE('',#1945,#1946,#398,.T.);
#2683=EDGE_CURVE('',#1946,#1947,#399,.T.);
#2684=EDGE_CURVE('',#1947,#1948,#400,.T.);
#2685=EDGE_CURVE('',#1948,#1949,#401,.T.);
#2686=EDGE_CURVE('',#1949,#1950,#402,.T.);
#2687=EDGE_CURVE('',#1950,#1951,#403,.T.);
#2688=EDGE_CURVE('',#1951,#1952,#404,.T.);
#2689=EDGE_CURVE('',#1952,#1953,#405,.T.);
#2690=EDGE_CURVE('',#1953,#1954,#406,.T.);
#2691=EDGE_CURVE('',#1954,#1955,#407,.T.);
#2692=EDGE_CURVE('',#1955,#1956,#408,.T.);
#2693=EDGE_CURVE('',#1956,#1957,#409,.T.);
#2694=EDGE_CURVE('',#1957,#1958,#410,.T.);
#2695=EDGE_CURVE('',#1958,#1959,#411,.T.);
#2696=EDGE_CURVE('',#1959,#1960,#412,.T.);
#2697=EDGE_CURVE('',#1960,#1961,#413,.T.);
#2698=EDGE_CURVE('',#1961,#1962,#414,.T.);
#2699=EDGE_CURVE('',#1962,#1963,#415,.T.);
#2700=EDGE_CURVE('',#1963,#1964,#416,.T.);
#2701=EDGE_CURVE('',#1964,#1965,#417,.T.);
#2702=EDGE_CURVE('',#1965,#1966,#418,.T.);
#2703=EDGE_CURVE('',#1966,#1967,#419,.T.);
#2704=EDGE_CURVE('',#1967,#1968,#420,.T.);
#2705=EDGE_CURVE('',#1968,#1969,#421,.T.);
#2706=EDGE_CURVE('',#1969,#1970,#422,.T.);
#2707=EDGE_CURVE('',#1970,#1971,#423,.T.);
#2708=EDGE_CURVE('',#1971,#1972,#424,.T.);
#2709=EDGE_CURVE('',#1972,#1973,#425,.T.);
#2710=EDGE_CURVE('',#1973,#1974,#426,.T.);
#2711=EDGE_CURVE('',#1974,#1975,#427,.T.);
#2712=EDGE_CURVE('',#1975,#1976,#428,.T.);
#2713=EDGE_CURVE('',#1976,#1977,#429,.T.);
#2714=EDGE_CURVE('',#1977,#1978,#430,.T.);
#2715=EDGE_CURVE('',#1978,#1979,#431,.T.);
#2716=EDGE_CURVE('',#1979,#1980,#432,.T.);
#2717=EDGE_CURVE('',#1980,#1981,#433,.T.);
#2718=EDGE_CURVE('',#1981,#1982,#434,.T.);
#2719=EDGE_CURVE('',#1982,#1983,#435,.T.);
#2720=EDGE_CURVE('',#1983,#1984,#436,.T.);
#2721=EDGE_CURVE('',#1984,#1985,#437,.T.);
#2722=EDGE_CURVE('',#1985,#1986,#438,.T.);
#2723=EDGE_CURVE('',#1986,#1987,#439,.T.);
#2724=EDGE_CURVE('',#1987,#1988,#440,.T.);
#2725=EDGE_CURVE('',#1988,#1989,#441,.T.);
#2726=EDGE_CURVE('',#1989,#1990,#442,.T.);
#2727=EDGE_CURVE('',#1990,#1991,#443,.T.);
#2728=EDGE_CURVE('',#1991,#1992,#444,.T.);
#2729=EDGE_CURVE('',#1992,#1993,#445,.T.);
#2730=EDGE_CURVE('',#1993,#1994,#446,.T.);
#2731=EDGE_CURVE('',#1994,#1995,#447,.T.);
#2732=EDGE_CURVE('',#1995,#1996,#448,.T.);
#2733=EDGE_CURVE('',#1996,#1997,#449,.T.);
#2734=EDGE_CURVE('',#1997,#1998,#450,.T.);
#2735=EDGE_CURVE('',#1998,#1999,#451,.T.);
#2736=EDGE_CURVE('',#1999,#2000,#452,.T.);
#2737=EDGE_CURVE('',#2000,#2001,#453,.T.);
#2738=EDGE_CURVE('',#2001,#2002,#454,.T.);
#2739=EDGE_CURVE('',#2002,#2003,#455,.T.);
#2740=EDGE_CURVE('',#2003,#2004,#456,.T.);
#2741=EDGE_CURVE('',#2004,#2005,#457,.T.);
#2742=EDGE_CURVE('',#2005,#2006,#458,.T.);
#2743=EDGE_CURVE('',#2006,#2007,#459,.T.);
#2744=EDGE_CURVE('',#2007,#2008,#460,.T.);
#2745=EDGE_CURVE('',#2008,#2009,#461,.T.);
#2746=EDGE_CURVE('',#2009,#2010,#462,.T.);
#2747=EDGE_CURVE('',#2010,#2011,#463,.T.);
#2748=EDGE_CURVE('',#2011,#2012,#464,.T.);
#2749=EDGE_CURVE('',#2012,#2013,#465,.T.);
#2750=EDGE_CURVE('',#2013,#2014,#466,.T.);
#2751=EDGE_CURVE('',#2014,#2015,#467,.T.);
#2752=EDGE_CURVE('',#2015,#2016,#468,.T.);
#2753=EDGE_CURVE('',#2016,#2017,#469,.T.);
#2754=EDGE_CURVE('',#2017,#2018,#470,.T.);
#2755=EDGE_CURVE('',#2018,#2019,#471,.T.);
#2756=EDGE_CURVE('',#2019,#2020,#472,.T.);
#2757=EDGE_CURVE('',#2020,#2021,#473,.T.);
#2758=EDGE_CURVE('',#2021,#2022,#474,.T.);
#2759=EDGE_CURVE('',#2022,#2023,#475,.T.);
#2760=EDGE_CURVE('',#2023,#2024,#476,.T.);
#2761=EDGE_CURVE('',#2024,#1853,#477,.T.);
#2762=EDGE_CURVE('',#1850,#2025,#478,.F.);
#2763=EDGE_CURVE('',#2026,#2025,#1460,.T.);
#2764=EDGE_CURVE('',#2027,#2026,#479,.T.);
#2765=EDGE_CURVE('',#1849,#2027,#480,.T.);
#2766=EDGE_CURVE('',#1940,#2026,#481,.T.);
#2767=EDGE_CURVE('',#1594,#1855,#482,.T.);
#2768=EDGE_CURVE('',#2028,#1941,#483,.T.);
#2769=EDGE_CURVE('',#2025,#2028,#484,.T.);
#2770=EDGE_CURVE('',#1854,#1595,#485,.T.);
#2771=ORIENTED_EDGE('',*,*,#2029,.F.);
#2772=ORIENTED_EDGE('',*,*,#2030,.T.);
#2773=ORIENTED_EDGE('',*,*,#2031,.T.);
#2774=ORIENTED_EDGE('',*,*,#2030,.F.);
#2775=ORIENTED_EDGE('',*,*,#2031,.F.);
#2776=ORIENTED_EDGE('',*,*,#2032,.F.);
#2777=ORIENTED_EDGE('',*,*,#2029,.T.);
#2778=ORIENTED_EDGE('',*,*,#2033,.F.);
#2779=ORIENTED_EDGE('',*,*,#2034,.F.);
#2780=ORIENTED_EDGE('',*,*,#2035,.F.);
#2781=ORIENTED_EDGE('',*,*,#2036,.T.);
#2782=ORIENTED_EDGE('',*,*,#2033,.T.);
#2783=ORIENTED_EDGE('',*,*,#2036,.F.);
#2784=ORIENTED_EDGE('',*,*,#2037,.T.);
#2785=ORIENTED_EDGE('',*,*,#2038,.T.);
#2786=ORIENTED_EDGE('',*,*,#2039,.T.);
#2787=ORIENTED_EDGE('',*,*,#2040,.F.);
#2788=ORIENTED_EDGE('',*,*,#2041,.T.);
#2789=ORIENTED_EDGE('',*,*,#2042,.T.);
#2790=ORIENTED_EDGE('',*,*,#2043,.T.);
#2791=ORIENTED_EDGE('',*,*,#2038,.F.);
#2792=ORIENTED_EDGE('',*,*,#2044,.T.);
#2793=ORIENTED_EDGE('',*,*,#2045,.T.);
#2794=ORIENTED_EDGE('',*,*,#2046,.T.);
#2795=ORIENTED_EDGE('',*,*,#2042,.F.);
#2796=ORIENTED_EDGE('',*,*,#2047,.T.);
#2797=ORIENTED_EDGE('',*,*,#2048,.T.);
#2798=ORIENTED_EDGE('',*,*,#2049,.T.);
#2799=ORIENTED_EDGE('',*,*,#2050,.T.);
#2800=ORIENTED_EDGE('',*,*,#2051,.T.);
#2801=ORIENTED_EDGE('',*,*,#2048,.F.);
#2802=ORIENTED_EDGE('',*,*,#2052,.T.);
#2803=ORIENTED_EDGE('',*,*,#2053,.T.);
#2804=ORIENTED_EDGE('',*,*,#2054,.T.);
#2805=ORIENTED_EDGE('',*,*,#2050,.F.);
#2806=ORIENTED_EDGE('',*,*,#2055,.T.);
#2807=ORIENTED_EDGE('',*,*,#2045,.F.);
#2808=ORIENTED_EDGE('',*,*,#2056,.T.);
#2809=ORIENTED_EDGE('',*,*,#2053,.F.);
#2810=ORIENTED_EDGE('',*,*,#2057,.T.);
#2811=ORIENTED_EDGE('',*,*,#2058,.T.);
#2812=ORIENTED_EDGE('',*,*,#2059,.T.);
#2813=ORIENTED_EDGE('',*,*,#2058,.F.);
#2814=ORIENTED_EDGE('',*,*,#2060,.T.);
#2815=ORIENTED_EDGE('',*,*,#2040,.T.);
#2816=ORIENTED_EDGE('',*,*,#2043,.F.);
#2817=ORIENTED_EDGE('',*,*,#2061,.T.);
#2818=ORIENTED_EDGE('',*,*,#2062,.F.);
#2819=ORIENTED_EDGE('',*,*,#2063,.F.);
#2820=ORIENTED_EDGE('',*,*,#2046,.F.);
#2821=ORIENTED_EDGE('',*,*,#2064,.T.);
#2822=ORIENTED_EDGE('',*,*,#2065,.F.);
#2823=ORIENTED_EDGE('',*,*,#2061,.F.);
#2824=ORIENTED_EDGE('',*,*,#2055,.F.);
#2825=ORIENTED_EDGE('',*,*,#2066,.T.);
#2826=ORIENTED_EDGE('',*,*,#2067,.F.);
#2827=ORIENTED_EDGE('',*,*,#2064,.F.);
#2828=ORIENTED_EDGE('',*,*,#2049,.F.);
#2829=ORIENTED_EDGE('',*,*,#2068,.T.);
#2830=ORIENTED_EDGE('',*,*,#2069,.F.);
#2831=ORIENTED_EDGE('',*,*,#2066,.F.);
#2832=ORIENTED_EDGE('',*,*,#2047,.F.);
#2833=ORIENTED_EDGE('',*,*,#2054,.F.);
#2834=ORIENTED_EDGE('',*,*,#2044,.F.);
#2835=ORIENTED_EDGE('',*,*,#2041,.F.);
#2836=ORIENTED_EDGE('',*,*,#2037,.F.);
#2837=ORIENTED_EDGE('',*,*,#2060,.F.);
#2838=ORIENTED_EDGE('',*,*,#2057,.F.);
#2839=ORIENTED_EDGE('',*,*,#2052,.F.);
#2840=ORIENTED_EDGE('',*,*,#2070,.F.);
#2841=ORIENTED_EDGE('',*,*,#2071,.F.);
#2842=ORIENTED_EDGE('',*,*,#2072,.F.);
#2843=ORIENTED_EDGE('',*,*,#2073,.F.);
#2844=ORIENTED_EDGE('',*,*,#2074,.F.);
#2845=ORIENTED_EDGE('',*,*,#2075,.T.);
#2846=ORIENTED_EDGE('',*,*,#2076,.T.);
#2847=ORIENTED_EDGE('',*,*,#2070,.T.);
#2848=ORIENTED_EDGE('',*,*,#2076,.F.);
#2849=ORIENTED_EDGE('',*,*,#2077,.T.);
#2850=ORIENTED_EDGE('',*,*,#2075,.F.);
#2851=ORIENTED_EDGE('',*,*,#2078,.T.);
#2852=ORIENTED_EDGE('',*,*,#2079,.F.);
#2853=ORIENTED_EDGE('',*,*,#2080,.F.);
#2854=ORIENTED_EDGE('',*,*,#2078,.F.);
#2855=ORIENTED_EDGE('',*,*,#2077,.F.);
#2856=ORIENTED_EDGE('',*,*,#2081,.T.);
#2857=ORIENTED_EDGE('',*,*,#2082,.T.);
#2858=ORIENTED_EDGE('',*,*,#2074,.T.);
#2859=ORIENTED_EDGE('',*,*,#2082,.F.);
#2860=ORIENTED_EDGE('',*,*,#2083,.T.);
#2861=ORIENTED_EDGE('',*,*,#2081,.F.);
#2862=ORIENTED_EDGE('',*,*,#2084,.T.);
#2863=ORIENTED_EDGE('',*,*,#2085,.F.);
#2864=ORIENTED_EDGE('',*,*,#2086,.F.);
#2865=ORIENTED_EDGE('',*,*,#2084,.F.);
#2866=ORIENTED_EDGE('',*,*,#2083,.F.);
#2867=ORIENTED_EDGE('',*,*,#2087,.T.);
#2868=ORIENTED_EDGE('',*,*,#2088,.T.);
#2869=ORIENTED_EDGE('',*,*,#2071,.T.);
#2870=ORIENTED_EDGE('',*,*,#2088,.F.);
#2871=ORIENTED_EDGE('',*,*,#2089,.T.);
#2872=ORIENTED_EDGE('',*,*,#2087,.F.);
#2873=ORIENTED_EDGE('',*,*,#2090,.T.);
#2874=ORIENTED_EDGE('',*,*,#2091,.F.);
#2875=ORIENTED_EDGE('',*,*,#2092,.F.);
#2876=ORIENTED_EDGE('',*,*,#2090,.F.);
#2877=ORIENTED_EDGE('',*,*,#2089,.F.);
#2878=ORIENTED_EDGE('',*,*,#2034,.T.);
#2879=ORIENTED_EDGE('',*,*,#2035,.T.);
#2880=ORIENTED_EDGE('',*,*,#2093,.T.);
#2881=ORIENTED_EDGE('',*,*,#2073,.T.);
#2882=ORIENTED_EDGE('',*,*,#2093,.F.);
#2883=ORIENTED_EDGE('',*,*,#2032,.T.);
#2884=ORIENTED_EDGE('',*,*,#2094,.T.);
#2885=ORIENTED_EDGE('',*,*,#2095,.F.);
#2886=ORIENTED_EDGE('',*,*,#2096,.F.);
#2887=ORIENTED_EDGE('',*,*,#2094,.F.);
#2888=ORIENTED_EDGE('',*,*,#2097,.T.);
#2889=ORIENTED_EDGE('',*,*,#2098,.T.);
#2890=ORIENTED_EDGE('',*,*,#2072,.T.);
#2891=ORIENTED_EDGE('',*,*,#2098,.F.);
#2892=ORIENTED_EDGE('',*,*,#2099,.T.);
#2893=ORIENTED_EDGE('',*,*,#2097,.F.);
#2894=ORIENTED_EDGE('',*,*,#2100,.T.);
#2895=ORIENTED_EDGE('',*,*,#2101,.F.);
#2896=ORIENTED_EDGE('',*,*,#2102,.F.);
#2897=ORIENTED_EDGE('',*,*,#2100,.F.);
#2898=ORIENTED_EDGE('',*,*,#2099,.F.);
#2899=ORIENTED_EDGE('',*,*,#2103,.T.);
#2900=ORIENTED_EDGE('',*,*,#2104,.T.);
#2901=ORIENTED_EDGE('',*,*,#2105,.T.);
#2902=ORIENTED_EDGE('',*,*,#2106,.F.);
#2903=ORIENTED_EDGE('',*,*,#2107,.T.);
#2904=ORIENTED_EDGE('',*,*,#2108,.T.);
#2905=ORIENTED_EDGE('',*,*,#2109,.T.);
#2906=ORIENTED_EDGE('',*,*,#2104,.F.);
#2907=ORIENTED_EDGE('',*,*,#2110,.T.);
#2908=ORIENTED_EDGE('',*,*,#2111,.T.);
#2909=ORIENTED_EDGE('',*,*,#2112,.T.);
#2910=ORIENTED_EDGE('',*,*,#2108,.F.);
#2911=ORIENTED_EDGE('',*,*,#2113,.T.);
#2912=ORIENTED_EDGE('',*,*,#2114,.T.);
#2913=ORIENTED_EDGE('',*,*,#2115,.T.);
#2914=ORIENTED_EDGE('',*,*,#2111,.F.);
#2915=ORIENTED_EDGE('',*,*,#2116,.T.);
#2916=ORIENTED_EDGE('',*,*,#2117,.T.);
#2917=ORIENTED_EDGE('',*,*,#2069,.T.);
#2918=ORIENTED_EDGE('',*,*,#2114,.F.);
#2919=ORIENTED_EDGE('',*,*,#2067,.T.);
#2920=ORIENTED_EDGE('',*,*,#2117,.F.);
#2921=ORIENTED_EDGE('',*,*,#2118,.T.);
#2922=ORIENTED_EDGE('',*,*,#2119,.T.);
#2923=ORIENTED_EDGE('',*,*,#2065,.T.);
#2924=ORIENTED_EDGE('',*,*,#2119,.F.);
#2925=ORIENTED_EDGE('',*,*,#2120,.T.);
#2926=ORIENTED_EDGE('',*,*,#2121,.T.);
#2927=ORIENTED_EDGE('',*,*,#2062,.T.);
#2928=ORIENTED_EDGE('',*,*,#2121,.F.);
#2929=ORIENTED_EDGE('',*,*,#2122,.T.);
#2930=ORIENTED_EDGE('',*,*,#2106,.T.);
#2931=ORIENTED_EDGE('',*,*,#2039,.F.);
#2932=ORIENTED_EDGE('',*,*,#2063,.T.);
#2933=ORIENTED_EDGE('',*,*,#2105,.F.);
#2934=ORIENTED_EDGE('',*,*,#2123,.F.);
#2935=ORIENTED_EDGE('',*,*,#2103,.F.);
#2936=ORIENTED_EDGE('',*,*,#2122,.F.);
#2937=ORIENTED_EDGE('',*,*,#2120,.F.);
#2938=ORIENTED_EDGE('',*,*,#2118,.F.);
#2939=ORIENTED_EDGE('',*,*,#2116,.F.);
#2940=ORIENTED_EDGE('',*,*,#2113,.F.);
#2941=ORIENTED_EDGE('',*,*,#2110,.F.);
#2942=ORIENTED_EDGE('',*,*,#2107,.F.);
#2943=ORIENTED_EDGE('',*,*,#2124,.F.);
#2944=ORIENTED_EDGE('',*,*,#2125,.F.);
#2945=ORIENTED_EDGE('',*,*,#2126,.F.);
#2946=ORIENTED_EDGE('',*,*,#2127,.F.);
#2947=ORIENTED_EDGE('',*,*,#2128,.F.);
#2948=ORIENTED_EDGE('',*,*,#2124,.T.);
#2949=ORIENTED_EDGE('',*,*,#2129,.T.);
#2950=ORIENTED_EDGE('',*,*,#2079,.T.);
#2951=ORIENTED_EDGE('',*,*,#2080,.T.);
#2952=ORIENTED_EDGE('',*,*,#2129,.F.);
#2953=ORIENTED_EDGE('',*,*,#2128,.T.);
#2954=ORIENTED_EDGE('',*,*,#2130,.T.);
#2955=ORIENTED_EDGE('',*,*,#2085,.T.);
#2956=ORIENTED_EDGE('',*,*,#2086,.T.);
#2957=ORIENTED_EDGE('',*,*,#2130,.F.);
#2958=ORIENTED_EDGE('',*,*,#2125,.T.);
#2959=ORIENTED_EDGE('',*,*,#2131,.T.);
#2960=ORIENTED_EDGE('',*,*,#2091,.T.);
#2961=ORIENTED_EDGE('',*,*,#2092,.T.);
#2962=ORIENTED_EDGE('',*,*,#2131,.F.);
#2963=ORIENTED_EDGE('',*,*,#2127,.T.);
#2964=ORIENTED_EDGE('',*,*,#2132,.T.);
#2965=ORIENTED_EDGE('',*,*,#2095,.T.);
#2966=ORIENTED_EDGE('',*,*,#2096,.T.);
#2967=ORIENTED_EDGE('',*,*,#2132,.F.);
#2968=ORIENTED_EDGE('',*,*,#2126,.T.);
#2969=ORIENTED_EDGE('',*,*,#2133,.T.);
#2970=ORIENTED_EDGE('',*,*,#2101,.T.);
#2971=ORIENTED_EDGE('',*,*,#2102,.T.);
#2972=ORIENTED_EDGE('',*,*,#2133,.F.);
#2973=ORIENTED_EDGE('',*,*,#2059,.F.);
#2974=ORIENTED_EDGE('',*,*,#2123,.T.);
#2975=ORIENTED_EDGE('',*,*,#2109,.F.);
#2976=ORIENTED_EDGE('',*,*,#2134,.F.);
#2977=ORIENTED_EDGE('',*,*,#2056,.F.);
#2978=ORIENTED_EDGE('',*,*,#2134,.T.);
#2979=ORIENTED_EDGE('',*,*,#2112,.F.);
#2980=ORIENTED_EDGE('',*,*,#2135,.F.);
#2981=ORIENTED_EDGE('',*,*,#2051,.F.);
#2982=ORIENTED_EDGE('',*,*,#2135,.T.);
#2983=ORIENTED_EDGE('',*,*,#2115,.F.);
#2984=ORIENTED_EDGE('',*,*,#2068,.F.);
#2985=ORIENTED_EDGE('',*,*,#2136,.T.);
#2986=ORIENTED_EDGE('',*,*,#2137,.F.);
#2987=ORIENTED_EDGE('',*,*,#2138,.F.);
#2988=ORIENTED_EDGE('',*,*,#2139,.F.);
#2989=ORIENTED_EDGE('',*,*,#2140,.T.);
#2990=ORIENTED_EDGE('',*,*,#2141,.T.);
#2991=ORIENTED_EDGE('',*,*,#2142,.T.);
#2992=ORIENTED_EDGE('',*,*,#2141,.F.);
#2993=ORIENTED_EDGE('',*,*,#2143,.F.);
#2994=ORIENTED_EDGE('',*,*,#2144,.F.);
#2995=ORIENTED_EDGE('',*,*,#2145,.F.);
#2996=ORIENTED_EDGE('',*,*,#2146,.F.);
#2997=ORIENTED_EDGE('',*,*,#2147,.F.);
#2998=ORIENTED_EDGE('',*,*,#2148,.F.);
#2999=ORIENTED_EDGE('',*,*,#2149,.F.);
#3000=ORIENTED_EDGE('',*,*,#2150,.F.);
#3001=ORIENTED_EDGE('',*,*,#2151,.F.);
#3002=ORIENTED_EDGE('',*,*,#2152,.F.);
#3003=ORIENTED_EDGE('',*,*,#2153,.F.);
#3004=ORIENTED_EDGE('',*,*,#2154,.F.);
#3005=ORIENTED_EDGE('',*,*,#2140,.F.);
#3006=ORIENTED_EDGE('',*,*,#2142,.F.);
#3007=ORIENTED_EDGE('',*,*,#2155,.T.);
#3008=ORIENTED_EDGE('',*,*,#2156,.F.);
#3009=ORIENTED_EDGE('',*,*,#2155,.F.);
#3010=ORIENTED_EDGE('',*,*,#2151,.T.);
#3011=ORIENTED_EDGE('',*,*,#2157,.T.);
#3012=ORIENTED_EDGE('',*,*,#2158,.T.);
#3013=ORIENTED_EDGE('',*,*,#2157,.F.);
#3014=ORIENTED_EDGE('',*,*,#2158,.F.);
#3015=ORIENTED_EDGE('',*,*,#2159,.T.);
#3016=ORIENTED_EDGE('',*,*,#2160,.F.);
#3017=ORIENTED_EDGE('',*,*,#2161,.F.);
#3018=ORIENTED_EDGE('',*,*,#2159,.F.);
#3019=ORIENTED_EDGE('',*,*,#2154,.T.);
#3020=ORIENTED_EDGE('',*,*,#2162,.T.);
#3021=ORIENTED_EDGE('',*,*,#2163,.T.);
#3022=ORIENTED_EDGE('',*,*,#2162,.F.);
#3023=ORIENTED_EDGE('',*,*,#2163,.F.);
#3024=ORIENTED_EDGE('',*,*,#2164,.T.);
#3025=ORIENTED_EDGE('',*,*,#2165,.F.);
#3026=ORIENTED_EDGE('',*,*,#2166,.F.);
#3027=ORIENTED_EDGE('',*,*,#2164,.F.);
#3028=ORIENTED_EDGE('',*,*,#2152,.T.);
#3029=ORIENTED_EDGE('',*,*,#2167,.T.);
#3030=ORIENTED_EDGE('',*,*,#2137,.T.);
#3031=ORIENTED_EDGE('',*,*,#2167,.F.);
#3032=ORIENTED_EDGE('',*,*,#2153,.T.);
#3033=ORIENTED_EDGE('',*,*,#2168,.T.);
#3034=ORIENTED_EDGE('',*,*,#2169,.T.);
#3035=ORIENTED_EDGE('',*,*,#2168,.F.);
#3036=ORIENTED_EDGE('',*,*,#2169,.F.);
#3037=ORIENTED_EDGE('',*,*,#2170,.T.);
#3038=ORIENTED_EDGE('',*,*,#2171,.F.);
#3039=ORIENTED_EDGE('',*,*,#2172,.F.);
#3040=ORIENTED_EDGE('',*,*,#2170,.F.);
#3041=ORIENTED_EDGE('',*,*,#2147,.T.);
#3042=ORIENTED_EDGE('',*,*,#2173,.T.);
#3043=ORIENTED_EDGE('',*,*,#2174,.T.);
#3044=ORIENTED_EDGE('',*,*,#2175,.F.);
#3045=ORIENTED_EDGE('',*,*,#2146,.T.);
#3046=ORIENTED_EDGE('',*,*,#2176,.T.);
#3047=ORIENTED_EDGE('',*,*,#2177,.T.);
#3048=ORIENTED_EDGE('',*,*,#2173,.F.);
#3049=ORIENTED_EDGE('',*,*,#2145,.T.);
#3050=ORIENTED_EDGE('',*,*,#2178,.T.);
#3051=ORIENTED_EDGE('',*,*,#2179,.T.);
#3052=ORIENTED_EDGE('',*,*,#2176,.F.);
#3053=ORIENTED_EDGE('',*,*,#2143,.T.);
#3054=ORIENTED_EDGE('',*,*,#2180,.T.);
#3055=ORIENTED_EDGE('',*,*,#2181,.T.);
#3056=ORIENTED_EDGE('',*,*,#2182,.T.);
#3057=ORIENTED_EDGE('',*,*,#2183,.T.);
#3058=ORIENTED_EDGE('',*,*,#2180,.F.);
#3059=ORIENTED_EDGE('',*,*,#2150,.T.);
#3060=ORIENTED_EDGE('',*,*,#2184,.T.);
#3061=ORIENTED_EDGE('',*,*,#2144,.T.);
#3062=ORIENTED_EDGE('',*,*,#2182,.F.);
#3063=ORIENTED_EDGE('',*,*,#2185,.T.);
#3064=ORIENTED_EDGE('',*,*,#2178,.F.);
#3065=ORIENTED_EDGE('',*,*,#2186,.T.);
#3066=ORIENTED_EDGE('',*,*,#2184,.F.);
#3067=ORIENTED_EDGE('',*,*,#2149,.T.);
#3068=ORIENTED_EDGE('',*,*,#2187,.T.);
#3069=ORIENTED_EDGE('',*,*,#2188,.T.);
#3070=ORIENTED_EDGE('',*,*,#2187,.F.);
#3071=ORIENTED_EDGE('',*,*,#2148,.T.);
#3072=ORIENTED_EDGE('',*,*,#2175,.T.);
#3073=ORIENTED_EDGE('',*,*,#2177,.F.);
#3074=ORIENTED_EDGE('',*,*,#2189,.T.);
#3075=ORIENTED_EDGE('',*,*,#2190,.F.);
#3076=ORIENTED_EDGE('',*,*,#2191,.F.);
#3077=ORIENTED_EDGE('',*,*,#2179,.F.);
#3078=ORIENTED_EDGE('',*,*,#2192,.T.);
#3079=ORIENTED_EDGE('',*,*,#2193,.F.);
#3080=ORIENTED_EDGE('',*,*,#2189,.F.);
#3081=ORIENTED_EDGE('',*,*,#2185,.F.);
#3082=ORIENTED_EDGE('',*,*,#2194,.T.);
#3083=ORIENTED_EDGE('',*,*,#2195,.F.);
#3084=ORIENTED_EDGE('',*,*,#2192,.F.);
#3085=ORIENTED_EDGE('',*,*,#2181,.F.);
#3086=ORIENTED_EDGE('',*,*,#2196,.T.);
#3087=ORIENTED_EDGE('',*,*,#2197,.F.);
#3088=ORIENTED_EDGE('',*,*,#2194,.F.);
#3089=ORIENTED_EDGE('',*,*,#2186,.F.);
#3090=ORIENTED_EDGE('',*,*,#2198,.T.);
#3091=ORIENTED_EDGE('',*,*,#2199,.F.);
#3092=ORIENTED_EDGE('',*,*,#2200,.F.);
#3093=ORIENTED_EDGE('',*,*,#2183,.F.);
#3094=ORIENTED_EDGE('',*,*,#2200,.T.);
#3095=ORIENTED_EDGE('',*,*,#2201,.F.);
#3096=ORIENTED_EDGE('',*,*,#2196,.F.);
#3097=ORIENTED_EDGE('',*,*,#2188,.F.);
#3098=ORIENTED_EDGE('',*,*,#2202,.T.);
#3099=ORIENTED_EDGE('',*,*,#2203,.F.);
#3100=ORIENTED_EDGE('',*,*,#2198,.F.);
#3101=ORIENTED_EDGE('',*,*,#2174,.F.);
#3102=ORIENTED_EDGE('',*,*,#2191,.T.);
#3103=ORIENTED_EDGE('',*,*,#2204,.F.);
#3104=ORIENTED_EDGE('',*,*,#2202,.F.);
#3105=ORIENTED_EDGE('',*,*,#2205,.T.);
#3106=ORIENTED_EDGE('',*,*,#2206,.T.);
#3107=ORIENTED_EDGE('',*,*,#2160,.T.);
#3108=ORIENTED_EDGE('',*,*,#2161,.T.);
#3109=ORIENTED_EDGE('',*,*,#2206,.F.);
#3110=ORIENTED_EDGE('',*,*,#2207,.F.);
#3111=ORIENTED_EDGE('',*,*,#2208,.F.);
#3112=ORIENTED_EDGE('',*,*,#2209,.F.);
#3113=ORIENTED_EDGE('',*,*,#2210,.F.);
#3114=ORIENTED_EDGE('',*,*,#2211,.F.);
#3115=ORIENTED_EDGE('',*,*,#2212,.F.);
#3116=ORIENTED_EDGE('',*,*,#2213,.F.);
#3117=ORIENTED_EDGE('',*,*,#2214,.F.);
#3118=ORIENTED_EDGE('',*,*,#2215,.F.);
#3119=ORIENTED_EDGE('',*,*,#2216,.F.);
#3120=ORIENTED_EDGE('',*,*,#2217,.F.);
#3121=ORIENTED_EDGE('',*,*,#2218,.F.);
#3122=ORIENTED_EDGE('',*,*,#2205,.F.);
#3123=ORIENTED_EDGE('',*,*,#2215,.T.);
#3124=ORIENTED_EDGE('',*,*,#2219,.T.);
#3125=ORIENTED_EDGE('',*,*,#2165,.T.);
#3126=ORIENTED_EDGE('',*,*,#2166,.T.);
#3127=ORIENTED_EDGE('',*,*,#2219,.F.);
#3128=ORIENTED_EDGE('',*,*,#2218,.T.);
#3129=ORIENTED_EDGE('',*,*,#2220,.T.);
#3130=ORIENTED_EDGE('',*,*,#2139,.T.);
#3131=ORIENTED_EDGE('',*,*,#2220,.F.);
#3132=ORIENTED_EDGE('',*,*,#2216,.T.);
#3133=ORIENTED_EDGE('',*,*,#2221,.T.);
#3134=ORIENTED_EDGE('',*,*,#2171,.T.);
#3135=ORIENTED_EDGE('',*,*,#2172,.T.);
#3136=ORIENTED_EDGE('',*,*,#2221,.F.);
#3137=ORIENTED_EDGE('',*,*,#2211,.T.);
#3138=ORIENTED_EDGE('',*,*,#2222,.T.);
#3139=ORIENTED_EDGE('',*,*,#2193,.T.);
#3140=ORIENTED_EDGE('',*,*,#2223,.F.);
#3141=ORIENTED_EDGE('',*,*,#2210,.T.);
#3142=ORIENTED_EDGE('',*,*,#2224,.T.);
#3143=ORIENTED_EDGE('',*,*,#2190,.T.);
#3144=ORIENTED_EDGE('',*,*,#2222,.F.);
#3145=ORIENTED_EDGE('',*,*,#2209,.T.);
#3146=ORIENTED_EDGE('',*,*,#2225,.T.);
#3147=ORIENTED_EDGE('',*,*,#2204,.T.);
#3148=ORIENTED_EDGE('',*,*,#2224,.F.);
#3149=ORIENTED_EDGE('',*,*,#2207,.T.);
#3150=ORIENTED_EDGE('',*,*,#2226,.T.);
#3151=ORIENTED_EDGE('',*,*,#2199,.T.);
#3152=ORIENTED_EDGE('',*,*,#2227,.T.);
#3153=ORIENTED_EDGE('',*,*,#2201,.T.);
#3154=ORIENTED_EDGE('',*,*,#2226,.F.);
#3155=ORIENTED_EDGE('',*,*,#2214,.T.);
#3156=ORIENTED_EDGE('',*,*,#2228,.T.);
#3157=ORIENTED_EDGE('',*,*,#2208,.T.);
#3158=ORIENTED_EDGE('',*,*,#2227,.F.);
#3159=ORIENTED_EDGE('',*,*,#2203,.T.);
#3160=ORIENTED_EDGE('',*,*,#2225,.F.);
#3161=ORIENTED_EDGE('',*,*,#2197,.T.);
#3162=ORIENTED_EDGE('',*,*,#2228,.F.);
#3163=ORIENTED_EDGE('',*,*,#2213,.T.);
#3164=ORIENTED_EDGE('',*,*,#2229,.T.);
#3165=ORIENTED_EDGE('',*,*,#2195,.T.);
#3166=ORIENTED_EDGE('',*,*,#2229,.F.);
#3167=ORIENTED_EDGE('',*,*,#2212,.T.);
#3168=ORIENTED_EDGE('',*,*,#2223,.T.);
#3169=ORIENTED_EDGE('',*,*,#2156,.T.);
#3170=ORIENTED_EDGE('',*,*,#2230,.T.);
#3171=ORIENTED_EDGE('',*,*,#2217,.T.);
#3172=ORIENTED_EDGE('',*,*,#2230,.F.);
#3173=ORIENTED_EDGE('',*,*,#2136,.F.);
#3174=ORIENTED_EDGE('',*,*,#2231,.T.);
#3175=ORIENTED_EDGE('',*,*,#2138,.T.);
#3176=ORIENTED_EDGE('',*,*,#2231,.F.);
#3177=ORIENTED_EDGE('',*,*,#2232,.F.);
#3178=ORIENTED_EDGE('',*,*,#2233,.T.);
#3179=ORIENTED_EDGE('',*,*,#2234,.T.);
#3180=ORIENTED_EDGE('',*,*,#2233,.F.);
#3181=ORIENTED_EDGE('',*,*,#2235,.F.);
#3182=ORIENTED_EDGE('',*,*,#2236,.T.);
#3183=ORIENTED_EDGE('',*,*,#2232,.T.);
#3184=ORIENTED_EDGE('',*,*,#2236,.F.);
#3185=ORIENTED_EDGE('',*,*,#2237,.F.);
#3186=ORIENTED_EDGE('',*,*,#2235,.T.);
#3187=ORIENTED_EDGE('',*,*,#2238,.F.);
#3188=ORIENTED_EDGE('',*,*,#2239,.T.);
#3189=ORIENTED_EDGE('',*,*,#2237,.T.);
#3190=ORIENTED_EDGE('',*,*,#2239,.F.);
#3191=ORIENTED_EDGE('',*,*,#2240,.F.);
#3192=ORIENTED_EDGE('',*,*,#2241,.T.);
#3193=ORIENTED_EDGE('',*,*,#2238,.T.);
#3194=ORIENTED_EDGE('',*,*,#2241,.F.);
#3195=ORIENTED_EDGE('',*,*,#2242,.F.);
#3196=ORIENTED_EDGE('',*,*,#2243,.T.);
#3197=ORIENTED_EDGE('',*,*,#2240,.T.);
#3198=ORIENTED_EDGE('',*,*,#2243,.F.);
#3199=ORIENTED_EDGE('',*,*,#2242,.T.);
#3200=ORIENTED_EDGE('',*,*,#2244,.F.);
#3201=ORIENTED_EDGE('',*,*,#2234,.F.);
#3202=ORIENTED_EDGE('',*,*,#2245,.T.);
#3203=ORIENTED_EDGE('',*,*,#2244,.T.);
#3204=ORIENTED_EDGE('',*,*,#2245,.F.);
#3205=ORIENTED_EDGE('',*,*,#2246,.F.);
#3206=ORIENTED_EDGE('',*,*,#2247,.F.);
#3207=ORIENTED_EDGE('',*,*,#2248,.F.);
#3208=ORIENTED_EDGE('',*,*,#2249,.T.);
#3209=ORIENTED_EDGE('',*,*,#2250,.F.);
#3210=ORIENTED_EDGE('',*,*,#2251,.F.);
#3211=ORIENTED_EDGE('',*,*,#2252,.F.);
#3212=ORIENTED_EDGE('',*,*,#2246,.T.);
#3213=ORIENTED_EDGE('',*,*,#2253,.T.);
#3214=ORIENTED_EDGE('',*,*,#2254,.T.);
#3215=ORIENTED_EDGE('',*,*,#2255,.F.);
#3216=ORIENTED_EDGE('',*,*,#2256,.F.);
#3217=ORIENTED_EDGE('',*,*,#2250,.T.);
#3218=ORIENTED_EDGE('',*,*,#2257,.T.);
#3219=ORIENTED_EDGE('',*,*,#2258,.F.);
#3220=ORIENTED_EDGE('',*,*,#2259,.F.);
#3221=ORIENTED_EDGE('',*,*,#2260,.F.);
#3222=ORIENTED_EDGE('',*,*,#2255,.T.);
#3223=ORIENTED_EDGE('',*,*,#2261,.T.);
#3224=ORIENTED_EDGE('',*,*,#2262,.T.);
#3225=ORIENTED_EDGE('',*,*,#2263,.F.);
#3226=ORIENTED_EDGE('',*,*,#2264,.F.);
#3227=ORIENTED_EDGE('',*,*,#2258,.T.);
#3228=ORIENTED_EDGE('',*,*,#2265,.T.);
#3229=ORIENTED_EDGE('',*,*,#2266,.F.);
#3230=ORIENTED_EDGE('',*,*,#2267,.F.);
#3231=ORIENTED_EDGE('',*,*,#2268,.F.);
#3232=ORIENTED_EDGE('',*,*,#2263,.T.);
#3233=ORIENTED_EDGE('',*,*,#2269,.T.);
#3234=ORIENTED_EDGE('',*,*,#2270,.T.);
#3235=ORIENTED_EDGE('',*,*,#2271,.F.);
#3236=ORIENTED_EDGE('',*,*,#2272,.F.);
#3237=ORIENTED_EDGE('',*,*,#2266,.T.);
#3238=ORIENTED_EDGE('',*,*,#2273,.T.);
#3239=ORIENTED_EDGE('',*,*,#2274,.F.);
#3240=ORIENTED_EDGE('',*,*,#2275,.F.);
#3241=ORIENTED_EDGE('',*,*,#2276,.F.);
#3242=ORIENTED_EDGE('',*,*,#2271,.T.);
#3243=ORIENTED_EDGE('',*,*,#2277,.T.);
#3244=ORIENTED_EDGE('',*,*,#2278,.T.);
#3245=ORIENTED_EDGE('',*,*,#2279,.F.);
#3246=ORIENTED_EDGE('',*,*,#2280,.F.);
#3247=ORIENTED_EDGE('',*,*,#2274,.T.);
#3248=ORIENTED_EDGE('',*,*,#2281,.T.);
#3249=ORIENTED_EDGE('',*,*,#2282,.F.);
#3250=ORIENTED_EDGE('',*,*,#2283,.F.);
#3251=ORIENTED_EDGE('',*,*,#2284,.F.);
#3252=ORIENTED_EDGE('',*,*,#2279,.T.);
#3253=ORIENTED_EDGE('',*,*,#2285,.T.);
#3254=ORIENTED_EDGE('',*,*,#2286,.T.);
#3255=ORIENTED_EDGE('',*,*,#2287,.F.);
#3256=ORIENTED_EDGE('',*,*,#2288,.F.);
#3257=ORIENTED_EDGE('',*,*,#2282,.T.);
#3258=ORIENTED_EDGE('',*,*,#2289,.T.);
#3259=ORIENTED_EDGE('',*,*,#2290,.F.);
#3260=ORIENTED_EDGE('',*,*,#2291,.F.);
#3261=ORIENTED_EDGE('',*,*,#2292,.F.);
#3262=ORIENTED_EDGE('',*,*,#2287,.T.);
#3263=ORIENTED_EDGE('',*,*,#2293,.T.);
#3264=ORIENTED_EDGE('',*,*,#2294,.T.);
#3265=ORIENTED_EDGE('',*,*,#2295,.F.);
#3266=ORIENTED_EDGE('',*,*,#2296,.F.);
#3267=ORIENTED_EDGE('',*,*,#2290,.T.);
#3268=ORIENTED_EDGE('',*,*,#2297,.T.);
#3269=ORIENTED_EDGE('',*,*,#2298,.F.);
#3270=ORIENTED_EDGE('',*,*,#2299,.F.);
#3271=ORIENTED_EDGE('',*,*,#2300,.F.);
#3272=ORIENTED_EDGE('',*,*,#2295,.T.);
#3273=ORIENTED_EDGE('',*,*,#2301,.T.);
#3274=ORIENTED_EDGE('',*,*,#2302,.T.);
#3275=ORIENTED_EDGE('',*,*,#2303,.F.);
#3276=ORIENTED_EDGE('',*,*,#2304,.F.);
#3277=ORIENTED_EDGE('',*,*,#2298,.T.);
#3278=ORIENTED_EDGE('',*,*,#2305,.T.);
#3279=ORIENTED_EDGE('',*,*,#2306,.F.);
#3280=ORIENTED_EDGE('',*,*,#2307,.F.);
#3281=ORIENTED_EDGE('',*,*,#2308,.F.);
#3282=ORIENTED_EDGE('',*,*,#2303,.T.);
#3283=ORIENTED_EDGE('',*,*,#2309,.T.);
#3284=ORIENTED_EDGE('',*,*,#2310,.T.);
#3285=ORIENTED_EDGE('',*,*,#2311,.F.);
#3286=ORIENTED_EDGE('',*,*,#2312,.F.);
#3287=ORIENTED_EDGE('',*,*,#2306,.T.);
#3288=ORIENTED_EDGE('',*,*,#2313,.T.);
#3289=ORIENTED_EDGE('',*,*,#2314,.T.);
#3290=ORIENTED_EDGE('',*,*,#2315,.F.);
#3291=ORIENTED_EDGE('',*,*,#2316,.F.);
#3292=ORIENTED_EDGE('',*,*,#2317,.F.);
#3293=ORIENTED_EDGE('',*,*,#2311,.T.);
#3294=ORIENTED_EDGE('',*,*,#2318,.T.);
#3295=ORIENTED_EDGE('',*,*,#2319,.F.);
#3296=ORIENTED_EDGE('',*,*,#2320,.F.);
#3297=ORIENTED_EDGE('',*,*,#2315,.T.);
#3298=ORIENTED_EDGE('',*,*,#2321,.T.);
#3299=ORIENTED_EDGE('',*,*,#2322,.T.);
#3300=ORIENTED_EDGE('',*,*,#2323,.F.);
#3301=ORIENTED_EDGE('',*,*,#2324,.F.);
#3302=ORIENTED_EDGE('',*,*,#2325,.F.);
#3303=ORIENTED_EDGE('',*,*,#2319,.T.);
#3304=ORIENTED_EDGE('',*,*,#2326,.T.);
#3305=ORIENTED_EDGE('',*,*,#2327,.F.);
#3306=ORIENTED_EDGE('',*,*,#2328,.F.);
#3307=ORIENTED_EDGE('',*,*,#2323,.T.);
#3308=ORIENTED_EDGE('',*,*,#2329,.T.);
#3309=ORIENTED_EDGE('',*,*,#2330,.T.);
#3310=ORIENTED_EDGE('',*,*,#2331,.F.);
#3311=ORIENTED_EDGE('',*,*,#2332,.F.);
#3312=ORIENTED_EDGE('',*,*,#2333,.F.);
#3313=ORIENTED_EDGE('',*,*,#2327,.T.);
#3314=ORIENTED_EDGE('',*,*,#2334,.T.);
#3315=ORIENTED_EDGE('',*,*,#2335,.F.);
#3316=ORIENTED_EDGE('',*,*,#2336,.F.);
#3317=ORIENTED_EDGE('',*,*,#2331,.T.);
#3318=ORIENTED_EDGE('',*,*,#2337,.T.);
#3319=ORIENTED_EDGE('',*,*,#2338,.T.);
#3320=ORIENTED_EDGE('',*,*,#2339,.F.);
#3321=ORIENTED_EDGE('',*,*,#2340,.F.);
#3322=ORIENTED_EDGE('',*,*,#2341,.F.);
#3323=ORIENTED_EDGE('',*,*,#2335,.T.);
#3324=ORIENTED_EDGE('',*,*,#2342,.T.);
#3325=ORIENTED_EDGE('',*,*,#2343,.F.);
#3326=ORIENTED_EDGE('',*,*,#2344,.F.);
#3327=ORIENTED_EDGE('',*,*,#2339,.T.);
#3328=ORIENTED_EDGE('',*,*,#2345,.T.);
#3329=ORIENTED_EDGE('',*,*,#2346,.T.);
#3330=ORIENTED_EDGE('',*,*,#2347,.F.);
#3331=ORIENTED_EDGE('',*,*,#2348,.F.);
#3332=ORIENTED_EDGE('',*,*,#2349,.F.);
#3333=ORIENTED_EDGE('',*,*,#2343,.T.);
#3334=ORIENTED_EDGE('',*,*,#2350,.T.);
#3335=ORIENTED_EDGE('',*,*,#2351,.F.);
#3336=ORIENTED_EDGE('',*,*,#2352,.F.);
#3337=ORIENTED_EDGE('',*,*,#2347,.T.);
#3338=ORIENTED_EDGE('',*,*,#2353,.T.);
#3339=ORIENTED_EDGE('',*,*,#2354,.T.);
#3340=ORIENTED_EDGE('',*,*,#2355,.F.);
#3341=ORIENTED_EDGE('',*,*,#2356,.F.);
#3342=ORIENTED_EDGE('',*,*,#2357,.F.);
#3343=ORIENTED_EDGE('',*,*,#2351,.T.);
#3344=ORIENTED_EDGE('',*,*,#2358,.T.);
#3345=ORIENTED_EDGE('',*,*,#2359,.F.);
#3346=ORIENTED_EDGE('',*,*,#2360,.F.);
#3347=ORIENTED_EDGE('',*,*,#2355,.T.);
#3348=ORIENTED_EDGE('',*,*,#2361,.T.);
#3349=ORIENTED_EDGE('',*,*,#2362,.T.);
#3350=ORIENTED_EDGE('',*,*,#2363,.F.);
#3351=ORIENTED_EDGE('',*,*,#2364,.F.);
#3352=ORIENTED_EDGE('',*,*,#2365,.F.);
#3353=ORIENTED_EDGE('',*,*,#2359,.T.);
#3354=ORIENTED_EDGE('',*,*,#2366,.T.);
#3355=ORIENTED_EDGE('',*,*,#2367,.F.);
#3356=ORIENTED_EDGE('',*,*,#2368,.F.);
#3357=ORIENTED_EDGE('',*,*,#2363,.T.);
#3358=ORIENTED_EDGE('',*,*,#2369,.T.);
#3359=ORIENTED_EDGE('',*,*,#2370,.T.);
#3360=ORIENTED_EDGE('',*,*,#2371,.F.);
#3361=ORIENTED_EDGE('',*,*,#2372,.F.);
#3362=ORIENTED_EDGE('',*,*,#2373,.F.);
#3363=ORIENTED_EDGE('',*,*,#2367,.T.);
#3364=ORIENTED_EDGE('',*,*,#2374,.T.);
#3365=ORIENTED_EDGE('',*,*,#2375,.F.);
#3366=ORIENTED_EDGE('',*,*,#2376,.F.);
#3367=ORIENTED_EDGE('',*,*,#2371,.T.);
#3368=ORIENTED_EDGE('',*,*,#2377,.T.);
#3369=ORIENTED_EDGE('',*,*,#2378,.T.);
#3370=ORIENTED_EDGE('',*,*,#2379,.F.);
#3371=ORIENTED_EDGE('',*,*,#2380,.F.);
#3372=ORIENTED_EDGE('',*,*,#2381,.F.);
#3373=ORIENTED_EDGE('',*,*,#2375,.T.);
#3374=ORIENTED_EDGE('',*,*,#2382,.T.);
#3375=ORIENTED_EDGE('',*,*,#2383,.F.);
#3376=ORIENTED_EDGE('',*,*,#2384,.F.);
#3377=ORIENTED_EDGE('',*,*,#2379,.T.);
#3378=ORIENTED_EDGE('',*,*,#2385,.T.);
#3379=ORIENTED_EDGE('',*,*,#2386,.T.);
#3380=ORIENTED_EDGE('',*,*,#2387,.F.);
#3381=ORIENTED_EDGE('',*,*,#2388,.F.);
#3382=ORIENTED_EDGE('',*,*,#2389,.F.);
#3383=ORIENTED_EDGE('',*,*,#2383,.T.);
#3384=ORIENTED_EDGE('',*,*,#2390,.T.);
#3385=ORIENTED_EDGE('',*,*,#2391,.F.);
#3386=ORIENTED_EDGE('',*,*,#2392,.F.);
#3387=ORIENTED_EDGE('',*,*,#2387,.T.);
#3388=ORIENTED_EDGE('',*,*,#2393,.T.);
#3389=ORIENTED_EDGE('',*,*,#2394,.T.);
#3390=ORIENTED_EDGE('',*,*,#2395,.F.);
#3391=ORIENTED_EDGE('',*,*,#2396,.F.);
#3392=ORIENTED_EDGE('',*,*,#2397,.F.);
#3393=ORIENTED_EDGE('',*,*,#2391,.T.);
#3394=ORIENTED_EDGE('',*,*,#2398,.T.);
#3395=ORIENTED_EDGE('',*,*,#2399,.T.);
#3396=ORIENTED_EDGE('',*,*,#2400,.F.);
#3397=ORIENTED_EDGE('',*,*,#2401,.F.);
#3398=ORIENTED_EDGE('',*,*,#2395,.T.);
#3399=ORIENTED_EDGE('',*,*,#2402,.T.);
#3400=ORIENTED_EDGE('',*,*,#2403,.F.);
#3401=ORIENTED_EDGE('',*,*,#2404,.F.);
#3402=ORIENTED_EDGE('',*,*,#2405,.F.);
#3403=ORIENTED_EDGE('',*,*,#2400,.T.);
#3404=ORIENTED_EDGE('',*,*,#2406,.T.);
#3405=ORIENTED_EDGE('',*,*,#2407,.T.);
#3406=ORIENTED_EDGE('',*,*,#2408,.F.);
#3407=ORIENTED_EDGE('',*,*,#2409,.F.);
#3408=ORIENTED_EDGE('',*,*,#2403,.T.);
#3409=ORIENTED_EDGE('',*,*,#2410,.T.);
#3410=ORIENTED_EDGE('',*,*,#2411,.T.);
#3411=ORIENTED_EDGE('',*,*,#2412,.F.);
#3412=ORIENTED_EDGE('',*,*,#2413,.F.);
#3413=ORIENTED_EDGE('',*,*,#2414,.F.);
#3414=ORIENTED_EDGE('',*,*,#2408,.T.);
#3415=ORIENTED_EDGE('',*,*,#2415,.T.);
#3416=ORIENTED_EDGE('',*,*,#2416,.F.);
#3417=ORIENTED_EDGE('',*,*,#2417,.F.);
#3418=ORIENTED_EDGE('',*,*,#2412,.T.);
#3419=ORIENTED_EDGE('',*,*,#2418,.T.);
#3420=ORIENTED_EDGE('',*,*,#2419,.T.);
#3421=ORIENTED_EDGE('',*,*,#2420,.F.);
#3422=ORIENTED_EDGE('',*,*,#2421,.F.);
#3423=ORIENTED_EDGE('',*,*,#2422,.F.);
#3424=ORIENTED_EDGE('',*,*,#2416,.T.);
#3425=ORIENTED_EDGE('',*,*,#2423,.T.);
#3426=ORIENTED_EDGE('',*,*,#2424,.F.);
#3427=ORIENTED_EDGE('',*,*,#2425,.F.);
#3428=ORIENTED_EDGE('',*,*,#2426,.F.);
#3429=ORIENTED_EDGE('',*,*,#2420,.T.);
#3430=ORIENTED_EDGE('',*,*,#2427,.T.);
#3431=ORIENTED_EDGE('',*,*,#2428,.T.);
#3432=ORIENTED_EDGE('',*,*,#2429,.F.);
#3433=ORIENTED_EDGE('',*,*,#2430,.F.);
#3434=ORIENTED_EDGE('',*,*,#2424,.T.);
#3435=ORIENTED_EDGE('',*,*,#2431,.T.);
#3436=ORIENTED_EDGE('',*,*,#2432,.T.);
#3437=ORIENTED_EDGE('',*,*,#2433,.F.);
#3438=ORIENTED_EDGE('',*,*,#2434,.F.);
#3439=ORIENTED_EDGE('',*,*,#2435,.F.);
#3440=ORIENTED_EDGE('',*,*,#2429,.T.);
#3441=ORIENTED_EDGE('',*,*,#2436,.T.);
#3442=ORIENTED_EDGE('',*,*,#2437,.F.);
#3443=ORIENTED_EDGE('',*,*,#2438,.F.);
#3444=ORIENTED_EDGE('',*,*,#2433,.T.);
#3445=ORIENTED_EDGE('',*,*,#2439,.T.);
#3446=ORIENTED_EDGE('',*,*,#2440,.T.);
#3447=ORIENTED_EDGE('',*,*,#2441,.F.);
#3448=ORIENTED_EDGE('',*,*,#2442,.F.);
#3449=ORIENTED_EDGE('',*,*,#2443,.F.);
#3450=ORIENTED_EDGE('',*,*,#2437,.T.);
#3451=ORIENTED_EDGE('',*,*,#2444,.T.);
#3452=ORIENTED_EDGE('',*,*,#2445,.F.);
#3453=ORIENTED_EDGE('',*,*,#2446,.F.);
#3454=ORIENTED_EDGE('',*,*,#2441,.T.);
#3455=ORIENTED_EDGE('',*,*,#2447,.T.);
#3456=ORIENTED_EDGE('',*,*,#2448,.T.);
#3457=ORIENTED_EDGE('',*,*,#2449,.F.);
#3458=ORIENTED_EDGE('',*,*,#2450,.F.);
#3459=ORIENTED_EDGE('',*,*,#2451,.F.);
#3460=ORIENTED_EDGE('',*,*,#2445,.T.);
#3461=ORIENTED_EDGE('',*,*,#2452,.T.);
#3462=ORIENTED_EDGE('',*,*,#2453,.T.);
#3463=ORIENTED_EDGE('',*,*,#2454,.F.);
#3464=ORIENTED_EDGE('',*,*,#2455,.F.);
#3465=ORIENTED_EDGE('',*,*,#2456,.F.);
#3466=ORIENTED_EDGE('',*,*,#2449,.T.);
#3467=ORIENTED_EDGE('',*,*,#2457,.T.);
#3468=ORIENTED_EDGE('',*,*,#2458,.F.);
#3469=ORIENTED_EDGE('',*,*,#2459,.F.);
#3470=ORIENTED_EDGE('',*,*,#2454,.T.);
#3471=ORIENTED_EDGE('',*,*,#2460,.T.);
#3472=ORIENTED_EDGE('',*,*,#2461,.T.);
#3473=ORIENTED_EDGE('',*,*,#2462,.F.);
#3474=ORIENTED_EDGE('',*,*,#2463,.F.);
#3475=ORIENTED_EDGE('',*,*,#2464,.F.);
#3476=ORIENTED_EDGE('',*,*,#2458,.T.);
#3477=ORIENTED_EDGE('',*,*,#2465,.T.);
#3478=ORIENTED_EDGE('',*,*,#2466,.T.);
#3479=ORIENTED_EDGE('',*,*,#2467,.F.);
#3480=ORIENTED_EDGE('',*,*,#2468,.F.);
#3481=ORIENTED_EDGE('',*,*,#2462,.T.);
#3482=ORIENTED_EDGE('',*,*,#2469,.T.);
#3483=ORIENTED_EDGE('',*,*,#2470,.F.);
#3484=ORIENTED_EDGE('',*,*,#2471,.F.);
#3485=ORIENTED_EDGE('',*,*,#2472,.F.);
#3486=ORIENTED_EDGE('',*,*,#2467,.T.);
#3487=ORIENTED_EDGE('',*,*,#2473,.T.);
#3488=ORIENTED_EDGE('',*,*,#2474,.T.);
#3489=ORIENTED_EDGE('',*,*,#2475,.F.);
#3490=ORIENTED_EDGE('',*,*,#2476,.F.);
#3491=ORIENTED_EDGE('',*,*,#2470,.T.);
#3492=ORIENTED_EDGE('',*,*,#2477,.T.);
#3493=ORIENTED_EDGE('',*,*,#2478,.T.);
#3494=ORIENTED_EDGE('',*,*,#2479,.F.);
#3495=ORIENTED_EDGE('',*,*,#2480,.F.);
#3496=ORIENTED_EDGE('',*,*,#2481,.F.);
#3497=ORIENTED_EDGE('',*,*,#2475,.T.);
#3498=ORIENTED_EDGE('',*,*,#2482,.T.);
#3499=ORIENTED_EDGE('',*,*,#2483,.F.);
#3500=ORIENTED_EDGE('',*,*,#2484,.F.);
#3501=ORIENTED_EDGE('',*,*,#2479,.T.);
#3502=ORIENTED_EDGE('',*,*,#2485,.T.);
#3503=ORIENTED_EDGE('',*,*,#2486,.T.);
#3504=ORIENTED_EDGE('',*,*,#2487,.F.);
#3505=ORIENTED_EDGE('',*,*,#2488,.F.);
#3506=ORIENTED_EDGE('',*,*,#2489,.F.);
#3507=ORIENTED_EDGE('',*,*,#2483,.T.);
#3508=ORIENTED_EDGE('',*,*,#2490,.T.);
#3509=ORIENTED_EDGE('',*,*,#2491,.F.);
#3510=ORIENTED_EDGE('',*,*,#2492,.F.);
#3511=ORIENTED_EDGE('',*,*,#2487,.T.);
#3512=ORIENTED_EDGE('',*,*,#2493,.T.);
#3513=ORIENTED_EDGE('',*,*,#2494,.T.);
#3514=ORIENTED_EDGE('',*,*,#2495,.F.);
#3515=ORIENTED_EDGE('',*,*,#2496,.F.);
#3516=ORIENTED_EDGE('',*,*,#2497,.F.);
#3517=ORIENTED_EDGE('',*,*,#2491,.T.);
#3518=ORIENTED_EDGE('',*,*,#2498,.T.);
#3519=ORIENTED_EDGE('',*,*,#2499,.F.);
#3520=ORIENTED_EDGE('',*,*,#2500,.F.);
#3521=ORIENTED_EDGE('',*,*,#2495,.T.);
#3522=ORIENTED_EDGE('',*,*,#2501,.T.);
#3523=ORIENTED_EDGE('',*,*,#2502,.T.);
#3524=ORIENTED_EDGE('',*,*,#2503,.F.);
#3525=ORIENTED_EDGE('',*,*,#2504,.F.);
#3526=ORIENTED_EDGE('',*,*,#2505,.F.);
#3527=ORIENTED_EDGE('',*,*,#2499,.T.);
#3528=ORIENTED_EDGE('',*,*,#2506,.T.);
#3529=ORIENTED_EDGE('',*,*,#2507,.F.);
#3530=ORIENTED_EDGE('',*,*,#2508,.F.);
#3531=ORIENTED_EDGE('',*,*,#2503,.T.);
#3532=ORIENTED_EDGE('',*,*,#2509,.T.);
#3533=ORIENTED_EDGE('',*,*,#2510,.T.);
#3534=ORIENTED_EDGE('',*,*,#2511,.F.);
#3535=ORIENTED_EDGE('',*,*,#2512,.F.);
#3536=ORIENTED_EDGE('',*,*,#2513,.F.);
#3537=ORIENTED_EDGE('',*,*,#2507,.T.);
#3538=ORIENTED_EDGE('',*,*,#2514,.T.);
#3539=ORIENTED_EDGE('',*,*,#2515,.F.);
#3540=ORIENTED_EDGE('',*,*,#2516,.F.);
#3541=ORIENTED_EDGE('',*,*,#2511,.T.);
#3542=ORIENTED_EDGE('',*,*,#2517,.T.);
#3543=ORIENTED_EDGE('',*,*,#2518,.T.);
#3544=ORIENTED_EDGE('',*,*,#2519,.F.);
#3545=ORIENTED_EDGE('',*,*,#2520,.F.);
#3546=ORIENTED_EDGE('',*,*,#2521,.F.);
#3547=ORIENTED_EDGE('',*,*,#2515,.T.);
#3548=ORIENTED_EDGE('',*,*,#2522,.T.);
#3549=ORIENTED_EDGE('',*,*,#2523,.F.);
#3550=ORIENTED_EDGE('',*,*,#2524,.F.);
#3551=ORIENTED_EDGE('',*,*,#2519,.T.);
#3552=ORIENTED_EDGE('',*,*,#2525,.T.);
#3553=ORIENTED_EDGE('',*,*,#2526,.T.);
#3554=ORIENTED_EDGE('',*,*,#2527,.F.);
#3555=ORIENTED_EDGE('',*,*,#2528,.F.);
#3556=ORIENTED_EDGE('',*,*,#2529,.F.);
#3557=ORIENTED_EDGE('',*,*,#2523,.T.);
#3558=ORIENTED_EDGE('',*,*,#2530,.T.);
#3559=ORIENTED_EDGE('',*,*,#2531,.F.);
#3560=ORIENTED_EDGE('',*,*,#2532,.F.);
#3561=ORIENTED_EDGE('',*,*,#2533,.F.);
#3562=ORIENTED_EDGE('',*,*,#2527,.T.);
#3563=ORIENTED_EDGE('',*,*,#2534,.T.);
#3564=ORIENTED_EDGE('',*,*,#2535,.T.);
#3565=ORIENTED_EDGE('',*,*,#2536,.F.);
#3566=ORIENTED_EDGE('',*,*,#2537,.F.);
#3567=ORIENTED_EDGE('',*,*,#2538,.F.);
#3568=ORIENTED_EDGE('',*,*,#2531,.T.);
#3569=ORIENTED_EDGE('',*,*,#2539,.T.);
#3570=ORIENTED_EDGE('',*,*,#2540,.F.);
#3571=ORIENTED_EDGE('',*,*,#2541,.F.);
#3572=ORIENTED_EDGE('',*,*,#2536,.T.);
#3573=ORIENTED_EDGE('',*,*,#2542,.T.);
#3574=ORIENTED_EDGE('',*,*,#2543,.T.);
#3575=ORIENTED_EDGE('',*,*,#2544,.F.);
#3576=ORIENTED_EDGE('',*,*,#2545,.F.);
#3577=ORIENTED_EDGE('',*,*,#2546,.F.);
#3578=ORIENTED_EDGE('',*,*,#2540,.T.);
#3579=ORIENTED_EDGE('',*,*,#2547,.T.);
#3580=ORIENTED_EDGE('',*,*,#2548,.T.);
#3581=ORIENTED_EDGE('',*,*,#2549,.F.);
#3582=ORIENTED_EDGE('',*,*,#2550,.F.);
#3583=ORIENTED_EDGE('',*,*,#2551,.F.);
#3584=ORIENTED_EDGE('',*,*,#2544,.T.);
#3585=ORIENTED_EDGE('',*,*,#2552,.T.);
#3586=ORIENTED_EDGE('',*,*,#2553,.F.);
#3587=ORIENTED_EDGE('',*,*,#2554,.F.);
#3588=ORIENTED_EDGE('',*,*,#2549,.T.);
#3589=ORIENTED_EDGE('',*,*,#2555,.T.);
#3590=ORIENTED_EDGE('',*,*,#2556,.T.);
#3591=ORIENTED_EDGE('',*,*,#2557,.F.);
#3592=ORIENTED_EDGE('',*,*,#2558,.F.);
#3593=ORIENTED_EDGE('',*,*,#2559,.F.);
#3594=ORIENTED_EDGE('',*,*,#2553,.T.);
#3595=ORIENTED_EDGE('',*,*,#2560,.T.);
#3596=ORIENTED_EDGE('',*,*,#2561,.F.);
#3597=ORIENTED_EDGE('',*,*,#2562,.F.);
#3598=ORIENTED_EDGE('',*,*,#2557,.T.);
#3599=ORIENTED_EDGE('',*,*,#2563,.T.);
#3600=ORIENTED_EDGE('',*,*,#2564,.T.);
#3601=ORIENTED_EDGE('',*,*,#2565,.F.);
#3602=ORIENTED_EDGE('',*,*,#2566,.F.);
#3603=ORIENTED_EDGE('',*,*,#2567,.F.);
#3604=ORIENTED_EDGE('',*,*,#2561,.T.);
#3605=ORIENTED_EDGE('',*,*,#2568,.T.);
#3606=ORIENTED_EDGE('',*,*,#2569,.F.);
#3607=ORIENTED_EDGE('',*,*,#2570,.F.);
#3608=ORIENTED_EDGE('',*,*,#2565,.T.);
#3609=ORIENTED_EDGE('',*,*,#2571,.T.);
#3610=ORIENTED_EDGE('',*,*,#2572,.T.);
#3611=ORIENTED_EDGE('',*,*,#2573,.F.);
#3612=ORIENTED_EDGE('',*,*,#2574,.F.);
#3613=ORIENTED_EDGE('',*,*,#2575,.F.);
#3614=ORIENTED_EDGE('',*,*,#2569,.T.);
#3615=ORIENTED_EDGE('',*,*,#2576,.T.);
#3616=ORIENTED_EDGE('',*,*,#2577,.F.);
#3617=ORIENTED_EDGE('',*,*,#2578,.F.);
#3618=ORIENTED_EDGE('',*,*,#2579,.F.);
#3619=ORIENTED_EDGE('',*,*,#2573,.T.);
#3620=ORIENTED_EDGE('',*,*,#2580,.T.);
#3621=ORIENTED_EDGE('',*,*,#2581,.T.);
#3622=ORIENTED_EDGE('',*,*,#2582,.F.);
#3623=ORIENTED_EDGE('',*,*,#2583,.F.);
#3624=ORIENTED_EDGE('',*,*,#2577,.T.);
#3625=ORIENTED_EDGE('',*,*,#2584,.T.);
#3626=ORIENTED_EDGE('',*,*,#2585,.F.);
#3627=ORIENTED_EDGE('',*,*,#2586,.F.);
#3628=ORIENTED_EDGE('',*,*,#2587,.F.);
#3629=ORIENTED_EDGE('',*,*,#2582,.T.);
#3630=ORIENTED_EDGE('',*,*,#2588,.T.);
#3631=ORIENTED_EDGE('',*,*,#2589,.T.);
#3632=ORIENTED_EDGE('',*,*,#2590,.T.);
#3633=ORIENTED_EDGE('',*,*,#2591,.F.);
#3634=ORIENTED_EDGE('',*,*,#2592,.T.);
#3635=ORIENTED_EDGE('',*,*,#2593,.T.);
#3636=ORIENTED_EDGE('',*,*,#2594,.T.);
#3637=ORIENTED_EDGE('',*,*,#2595,.T.);
#3638=ORIENTED_EDGE('',*,*,#2596,.T.);
#3639=ORIENTED_EDGE('',*,*,#2597,.T.);
#3640=ORIENTED_EDGE('',*,*,#2598,.T.);
#3641=ORIENTED_EDGE('',*,*,#2599,.T.);
#3642=ORIENTED_EDGE('',*,*,#2600,.T.);
#3643=ORIENTED_EDGE('',*,*,#2601,.T.);
#3644=ORIENTED_EDGE('',*,*,#2602,.T.);
#3645=ORIENTED_EDGE('',*,*,#2603,.T.);
#3646=ORIENTED_EDGE('',*,*,#2604,.T.);
#3647=ORIENTED_EDGE('',*,*,#2605,.T.);
#3648=ORIENTED_EDGE('',*,*,#2606,.T.);
#3649=ORIENTED_EDGE('',*,*,#2607,.T.);
#3650=ORIENTED_EDGE('',*,*,#2608,.T.);
#3651=ORIENTED_EDGE('',*,*,#2609,.T.);
#3652=ORIENTED_EDGE('',*,*,#2610,.T.);
#3653=ORIENTED_EDGE('',*,*,#2611,.T.);
#3654=ORIENTED_EDGE('',*,*,#2612,.T.);
#3655=ORIENTED_EDGE('',*,*,#2613,.T.);
#3656=ORIENTED_EDGE('',*,*,#2614,.T.);
#3657=ORIENTED_EDGE('',*,*,#2615,.T.);
#3658=ORIENTED_EDGE('',*,*,#2616,.T.);
#3659=ORIENTED_EDGE('',*,*,#2617,.T.);
#3660=ORIENTED_EDGE('',*,*,#2618,.T.);
#3661=ORIENTED_EDGE('',*,*,#2619,.T.);
#3662=ORIENTED_EDGE('',*,*,#2620,.T.);
#3663=ORIENTED_EDGE('',*,*,#2621,.T.);
#3664=ORIENTED_EDGE('',*,*,#2622,.T.);
#3665=ORIENTED_EDGE('',*,*,#2623,.T.);
#3666=ORIENTED_EDGE('',*,*,#2624,.T.);
#3667=ORIENTED_EDGE('',*,*,#2625,.T.);
#3668=ORIENTED_EDGE('',*,*,#2626,.T.);
#3669=ORIENTED_EDGE('',*,*,#2627,.T.);
#3670=ORIENTED_EDGE('',*,*,#2628,.T.);
#3671=ORIENTED_EDGE('',*,*,#2629,.T.);
#3672=ORIENTED_EDGE('',*,*,#2630,.T.);
#3673=ORIENTED_EDGE('',*,*,#2631,.T.);
#3674=ORIENTED_EDGE('',*,*,#2632,.T.);
#3675=ORIENTED_EDGE('',*,*,#2633,.T.);
#3676=ORIENTED_EDGE('',*,*,#2634,.T.);
#3677=ORIENTED_EDGE('',*,*,#2635,.T.);
#3678=ORIENTED_EDGE('',*,*,#2636,.T.);
#3679=ORIENTED_EDGE('',*,*,#2637,.T.);
#3680=ORIENTED_EDGE('',*,*,#2638,.T.);
#3681=ORIENTED_EDGE('',*,*,#2639,.T.);
#3682=ORIENTED_EDGE('',*,*,#2640,.T.);
#3683=ORIENTED_EDGE('',*,*,#2641,.T.);
#3684=ORIENTED_EDGE('',*,*,#2642,.T.);
#3685=ORIENTED_EDGE('',*,*,#2643,.T.);
#3686=ORIENTED_EDGE('',*,*,#2644,.T.);
#3687=ORIENTED_EDGE('',*,*,#2645,.T.);
#3688=ORIENTED_EDGE('',*,*,#2646,.T.);
#3689=ORIENTED_EDGE('',*,*,#2647,.T.);
#3690=ORIENTED_EDGE('',*,*,#2648,.T.);
#3691=ORIENTED_EDGE('',*,*,#2649,.T.);
#3692=ORIENTED_EDGE('',*,*,#2650,.T.);
#3693=ORIENTED_EDGE('',*,*,#2651,.T.);
#3694=ORIENTED_EDGE('',*,*,#2652,.T.);
#3695=ORIENTED_EDGE('',*,*,#2653,.T.);
#3696=ORIENTED_EDGE('',*,*,#2654,.T.);
#3697=ORIENTED_EDGE('',*,*,#2655,.T.);
#3698=ORIENTED_EDGE('',*,*,#2656,.T.);
#3699=ORIENTED_EDGE('',*,*,#2657,.T.);
#3700=ORIENTED_EDGE('',*,*,#2658,.T.);
#3701=ORIENTED_EDGE('',*,*,#2659,.T.);
#3702=ORIENTED_EDGE('',*,*,#2660,.T.);
#3703=ORIENTED_EDGE('',*,*,#2661,.T.);
#3704=ORIENTED_EDGE('',*,*,#2662,.T.);
#3705=ORIENTED_EDGE('',*,*,#2663,.T.);
#3706=ORIENTED_EDGE('',*,*,#2664,.T.);
#3707=ORIENTED_EDGE('',*,*,#2665,.T.);
#3708=ORIENTED_EDGE('',*,*,#2666,.T.);
#3709=ORIENTED_EDGE('',*,*,#2667,.T.);
#3710=ORIENTED_EDGE('',*,*,#2668,.T.);
#3711=ORIENTED_EDGE('',*,*,#2669,.T.);
#3712=ORIENTED_EDGE('',*,*,#2670,.T.);
#3713=ORIENTED_EDGE('',*,*,#2671,.T.);
#3714=ORIENTED_EDGE('',*,*,#2672,.T.);
#3715=ORIENTED_EDGE('',*,*,#2673,.T.);
#3716=ORIENTED_EDGE('',*,*,#2674,.T.);
#3717=ORIENTED_EDGE('',*,*,#2675,.T.);
#3718=ORIENTED_EDGE('',*,*,#2676,.T.);
#3719=ORIENTED_EDGE('',*,*,#2677,.F.);
#3720=ORIENTED_EDGE('',*,*,#2678,.T.);
#3721=ORIENTED_EDGE('',*,*,#2679,.T.);
#3722=ORIENTED_EDGE('',*,*,#2680,.T.);
#3723=ORIENTED_EDGE('',*,*,#2681,.T.);
#3724=ORIENTED_EDGE('',*,*,#2682,.T.);
#3725=ORIENTED_EDGE('',*,*,#2683,.T.);
#3726=ORIENTED_EDGE('',*,*,#2684,.T.);
#3727=ORIENTED_EDGE('',*,*,#2685,.T.);
#3728=ORIENTED_EDGE('',*,*,#2686,.T.);
#3729=ORIENTED_EDGE('',*,*,#2687,.T.);
#3730=ORIENTED_EDGE('',*,*,#2688,.T.);
#3731=ORIENTED_EDGE('',*,*,#2689,.T.);
#3732=ORIENTED_EDGE('',*,*,#2690,.T.);
#3733=ORIENTED_EDGE('',*,*,#2691,.T.);
#3734=ORIENTED_EDGE('',*,*,#2692,.T.);
#3735=ORIENTED_EDGE('',*,*,#2693,.T.);
#3736=ORIENTED_EDGE('',*,*,#2694,.T.);
#3737=ORIENTED_EDGE('',*,*,#2695,.T.);
#3738=ORIENTED_EDGE('',*,*,#2696,.T.);
#3739=ORIENTED_EDGE('',*,*,#2697,.T.);
#3740=ORIENTED_EDGE('',*,*,#2698,.T.);
#3741=ORIENTED_EDGE('',*,*,#2699,.T.);
#3742=ORIENTED_EDGE('',*,*,#2700,.T.);
#3743=ORIENTED_EDGE('',*,*,#2701,.T.);
#3744=ORIENTED_EDGE('',*,*,#2702,.T.);
#3745=ORIENTED_EDGE('',*,*,#2703,.T.);
#3746=ORIENTED_EDGE('',*,*,#2704,.T.);
#3747=ORIENTED_EDGE('',*,*,#2705,.T.);
#3748=ORIENTED_EDGE('',*,*,#2706,.T.);
#3749=ORIENTED_EDGE('',*,*,#2707,.T.);
#3750=ORIENTED_EDGE('',*,*,#2708,.T.);
#3751=ORIENTED_EDGE('',*,*,#2709,.T.);
#3752=ORIENTED_EDGE('',*,*,#2710,.T.);
#3753=ORIENTED_EDGE('',*,*,#2711,.T.);
#3754=ORIENTED_EDGE('',*,*,#2712,.T.);
#3755=ORIENTED_EDGE('',*,*,#2713,.T.);
#3756=ORIENTED_EDGE('',*,*,#2714,.T.);
#3757=ORIENTED_EDGE('',*,*,#2715,.T.);
#3758=ORIENTED_EDGE('',*,*,#2716,.T.);
#3759=ORIENTED_EDGE('',*,*,#2717,.T.);
#3760=ORIENTED_EDGE('',*,*,#2718,.T.);
#3761=ORIENTED_EDGE('',*,*,#2719,.T.);
#3762=ORIENTED_EDGE('',*,*,#2720,.T.);
#3763=ORIENTED_EDGE('',*,*,#2721,.T.);
#3764=ORIENTED_EDGE('',*,*,#2722,.T.);
#3765=ORIENTED_EDGE('',*,*,#2723,.T.);
#3766=ORIENTED_EDGE('',*,*,#2724,.T.);
#3767=ORIENTED_EDGE('',*,*,#2725,.T.);
#3768=ORIENTED_EDGE('',*,*,#2726,.T.);
#3769=ORIENTED_EDGE('',*,*,#2727,.T.);
#3770=ORIENTED_EDGE('',*,*,#2728,.T.);
#3771=ORIENTED_EDGE('',*,*,#2729,.T.);
#3772=ORIENTED_EDGE('',*,*,#2730,.T.);
#3773=ORIENTED_EDGE('',*,*,#2731,.T.);
#3774=ORIENTED_EDGE('',*,*,#2732,.T.);
#3775=ORIENTED_EDGE('',*,*,#2733,.T.);
#3776=ORIENTED_EDGE('',*,*,#2734,.T.);
#3777=ORIENTED_EDGE('',*,*,#2735,.T.);
#3778=ORIENTED_EDGE('',*,*,#2736,.T.);
#3779=ORIENTED_EDGE('',*,*,#2737,.T.);
#3780=ORIENTED_EDGE('',*,*,#2738,.T.);
#3781=ORIENTED_EDGE('',*,*,#2739,.T.);
#3782=ORIENTED_EDGE('',*,*,#2740,.T.);
#3783=ORIENTED_EDGE('',*,*,#2741,.T.);
#3784=ORIENTED_EDGE('',*,*,#2742,.T.);
#3785=ORIENTED_EDGE('',*,*,#2743,.T.);
#3786=ORIENTED_EDGE('',*,*,#2744,.T.);
#3787=ORIENTED_EDGE('',*,*,#2745,.T.);
#3788=ORIENTED_EDGE('',*,*,#2746,.T.);
#3789=ORIENTED_EDGE('',*,*,#2747,.T.);
#3790=ORIENTED_EDGE('',*,*,#2748,.T.);
#3791=ORIENTED_EDGE('',*,*,#2749,.T.);
#3792=ORIENTED_EDGE('',*,*,#2750,.T.);
#3793=ORIENTED_EDGE('',*,*,#2751,.T.);
#3794=ORIENTED_EDGE('',*,*,#2752,.T.);
#3795=ORIENTED_EDGE('',*,*,#2753,.T.);
#3796=ORIENTED_EDGE('',*,*,#2754,.T.);
#3797=ORIENTED_EDGE('',*,*,#2755,.T.);
#3798=ORIENTED_EDGE('',*,*,#2756,.T.);
#3799=ORIENTED_EDGE('',*,*,#2757,.T.);
#3800=ORIENTED_EDGE('',*,*,#2758,.T.);
#3801=ORIENTED_EDGE('',*,*,#2759,.T.);
#3802=ORIENTED_EDGE('',*,*,#2760,.T.);
#3803=ORIENTED_EDGE('',*,*,#2761,.T.);
#3804=ORIENTED_EDGE('',*,*,#2585,.T.);
#3805=ORIENTED_EDGE('',*,*,#2762,.T.);
#3806=ORIENTED_EDGE('',*,*,#2763,.F.);
#3807=ORIENTED_EDGE('',*,*,#2764,.F.);
#3808=ORIENTED_EDGE('',*,*,#2765,.F.);
#3809=ORIENTED_EDGE('',*,*,#2766,.F.);
#3810=ORIENTED_EDGE('',*,*,#2676,.F.);
#3811=ORIENTED_EDGE('',*,*,#2675,.F.);
#3812=ORIENTED_EDGE('',*,*,#2674,.F.);
#3813=ORIENTED_EDGE('',*,*,#2673,.F.);
#3814=ORIENTED_EDGE('',*,*,#2672,.F.);
#3815=ORIENTED_EDGE('',*,*,#2671,.F.);
#3816=ORIENTED_EDGE('',*,*,#2670,.F.);
#3817=ORIENTED_EDGE('',*,*,#2669,.F.);
#3818=ORIENTED_EDGE('',*,*,#2668,.F.);
#3819=ORIENTED_EDGE('',*,*,#2667,.F.);
#3820=ORIENTED_EDGE('',*,*,#2666,.F.);
#3821=ORIENTED_EDGE('',*,*,#2665,.F.);
#3822=ORIENTED_EDGE('',*,*,#2664,.F.);
#3823=ORIENTED_EDGE('',*,*,#2663,.F.);
#3824=ORIENTED_EDGE('',*,*,#2662,.F.);
#3825=ORIENTED_EDGE('',*,*,#2661,.F.);
#3826=ORIENTED_EDGE('',*,*,#2660,.F.);
#3827=ORIENTED_EDGE('',*,*,#2659,.F.);
#3828=ORIENTED_EDGE('',*,*,#2658,.F.);
#3829=ORIENTED_EDGE('',*,*,#2657,.F.);
#3830=ORIENTED_EDGE('',*,*,#2656,.F.);
#3831=ORIENTED_EDGE('',*,*,#2655,.F.);
#3832=ORIENTED_EDGE('',*,*,#2654,.F.);
#3833=ORIENTED_EDGE('',*,*,#2653,.F.);
#3834=ORIENTED_EDGE('',*,*,#2652,.F.);
#3835=ORIENTED_EDGE('',*,*,#2651,.F.);
#3836=ORIENTED_EDGE('',*,*,#2650,.F.);
#3837=ORIENTED_EDGE('',*,*,#2649,.F.);
#3838=ORIENTED_EDGE('',*,*,#2648,.F.);
#3839=ORIENTED_EDGE('',*,*,#2647,.F.);
#3840=ORIENTED_EDGE('',*,*,#2646,.F.);
#3841=ORIENTED_EDGE('',*,*,#2645,.F.);
#3842=ORIENTED_EDGE('',*,*,#2644,.F.);
#3843=ORIENTED_EDGE('',*,*,#2643,.F.);
#3844=ORIENTED_EDGE('',*,*,#2642,.F.);
#3845=ORIENTED_EDGE('',*,*,#2641,.F.);
#3846=ORIENTED_EDGE('',*,*,#2640,.F.);
#3847=ORIENTED_EDGE('',*,*,#2639,.F.);
#3848=ORIENTED_EDGE('',*,*,#2638,.F.);
#3849=ORIENTED_EDGE('',*,*,#2637,.F.);
#3850=ORIENTED_EDGE('',*,*,#2636,.F.);
#3851=ORIENTED_EDGE('',*,*,#2635,.F.);
#3852=ORIENTED_EDGE('',*,*,#2634,.F.);
#3853=ORIENTED_EDGE('',*,*,#2633,.F.);
#3854=ORIENTED_EDGE('',*,*,#2632,.F.);
#3855=ORIENTED_EDGE('',*,*,#2631,.F.);
#3856=ORIENTED_EDGE('',*,*,#2630,.F.);
#3857=ORIENTED_EDGE('',*,*,#2629,.F.);
#3858=ORIENTED_EDGE('',*,*,#2628,.F.);
#3859=ORIENTED_EDGE('',*,*,#2627,.F.);
#3860=ORIENTED_EDGE('',*,*,#2626,.F.);
#3861=ORIENTED_EDGE('',*,*,#2625,.F.);
#3862=ORIENTED_EDGE('',*,*,#2624,.F.);
#3863=ORIENTED_EDGE('',*,*,#2623,.F.);
#3864=ORIENTED_EDGE('',*,*,#2622,.F.);
#3865=ORIENTED_EDGE('',*,*,#2621,.F.);
#3866=ORIENTED_EDGE('',*,*,#2620,.F.);
#3867=ORIENTED_EDGE('',*,*,#2619,.F.);
#3868=ORIENTED_EDGE('',*,*,#2618,.F.);
#3869=ORIENTED_EDGE('',*,*,#2617,.F.);
#3870=ORIENTED_EDGE('',*,*,#2616,.F.);
#3871=ORIENTED_EDGE('',*,*,#2615,.F.);
#3872=ORIENTED_EDGE('',*,*,#2614,.F.);
#3873=ORIENTED_EDGE('',*,*,#2613,.F.);
#3874=ORIENTED_EDGE('',*,*,#2612,.F.);
#3875=ORIENTED_EDGE('',*,*,#2611,.F.);
#3876=ORIENTED_EDGE('',*,*,#2610,.F.);
#3877=ORIENTED_EDGE('',*,*,#2609,.F.);
#3878=ORIENTED_EDGE('',*,*,#2608,.F.);
#3879=ORIENTED_EDGE('',*,*,#2607,.F.);
#3880=ORIENTED_EDGE('',*,*,#2606,.F.);
#3881=ORIENTED_EDGE('',*,*,#2605,.F.);
#3882=ORIENTED_EDGE('',*,*,#2604,.F.);
#3883=ORIENTED_EDGE('',*,*,#2603,.F.);
#3884=ORIENTED_EDGE('',*,*,#2602,.F.);
#3885=ORIENTED_EDGE('',*,*,#2601,.F.);
#3886=ORIENTED_EDGE('',*,*,#2600,.F.);
#3887=ORIENTED_EDGE('',*,*,#2599,.F.);
#3888=ORIENTED_EDGE('',*,*,#2598,.F.);
#3889=ORIENTED_EDGE('',*,*,#2597,.F.);
#3890=ORIENTED_EDGE('',*,*,#2596,.F.);
#3891=ORIENTED_EDGE('',*,*,#2595,.F.);
#3892=ORIENTED_EDGE('',*,*,#2594,.F.);
#3893=ORIENTED_EDGE('',*,*,#2593,.F.);
#3894=ORIENTED_EDGE('',*,*,#2592,.F.);
#3895=ORIENTED_EDGE('',*,*,#2767,.F.);
#3896=ORIENTED_EDGE('',*,*,#2247,.T.);
#3897=ORIENTED_EDGE('',*,*,#2252,.T.);
#3898=ORIENTED_EDGE('',*,*,#2251,.T.);
#3899=ORIENTED_EDGE('',*,*,#2256,.T.);
#3900=ORIENTED_EDGE('',*,*,#2260,.T.);
#3901=ORIENTED_EDGE('',*,*,#2259,.T.);
#3902=ORIENTED_EDGE('',*,*,#2264,.T.);
#3903=ORIENTED_EDGE('',*,*,#2268,.T.);
#3904=ORIENTED_EDGE('',*,*,#2267,.T.);
#3905=ORIENTED_EDGE('',*,*,#2272,.T.);
#3906=ORIENTED_EDGE('',*,*,#2276,.T.);
#3907=ORIENTED_EDGE('',*,*,#2275,.T.);
#3908=ORIENTED_EDGE('',*,*,#2280,.T.);
#3909=ORIENTED_EDGE('',*,*,#2284,.T.);
#3910=ORIENTED_EDGE('',*,*,#2283,.T.);
#3911=ORIENTED_EDGE('',*,*,#2288,.T.);
#3912=ORIENTED_EDGE('',*,*,#2292,.T.);
#3913=ORIENTED_EDGE('',*,*,#2291,.T.);
#3914=ORIENTED_EDGE('',*,*,#2296,.T.);
#3915=ORIENTED_EDGE('',*,*,#2300,.T.);
#3916=ORIENTED_EDGE('',*,*,#2299,.T.);
#3917=ORIENTED_EDGE('',*,*,#2304,.T.);
#3918=ORIENTED_EDGE('',*,*,#2308,.T.);
#3919=ORIENTED_EDGE('',*,*,#2307,.T.);
#3920=ORIENTED_EDGE('',*,*,#2312,.T.);
#3921=ORIENTED_EDGE('',*,*,#2317,.T.);
#3922=ORIENTED_EDGE('',*,*,#2316,.T.);
#3923=ORIENTED_EDGE('',*,*,#2320,.T.);
#3924=ORIENTED_EDGE('',*,*,#2325,.T.);
#3925=ORIENTED_EDGE('',*,*,#2324,.T.);
#3926=ORIENTED_EDGE('',*,*,#2328,.T.);
#3927=ORIENTED_EDGE('',*,*,#2333,.T.);
#3928=ORIENTED_EDGE('',*,*,#2332,.T.);
#3929=ORIENTED_EDGE('',*,*,#2336,.T.);
#3930=ORIENTED_EDGE('',*,*,#2341,.T.);
#3931=ORIENTED_EDGE('',*,*,#2340,.T.);
#3932=ORIENTED_EDGE('',*,*,#2344,.T.);
#3933=ORIENTED_EDGE('',*,*,#2349,.T.);
#3934=ORIENTED_EDGE('',*,*,#2348,.T.);
#3935=ORIENTED_EDGE('',*,*,#2352,.T.);
#3936=ORIENTED_EDGE('',*,*,#2357,.T.);
#3937=ORIENTED_EDGE('',*,*,#2356,.T.);
#3938=ORIENTED_EDGE('',*,*,#2360,.T.);
#3939=ORIENTED_EDGE('',*,*,#2365,.T.);
#3940=ORIENTED_EDGE('',*,*,#2364,.T.);
#3941=ORIENTED_EDGE('',*,*,#2368,.T.);
#3942=ORIENTED_EDGE('',*,*,#2373,.T.);
#3943=ORIENTED_EDGE('',*,*,#2372,.T.);
#3944=ORIENTED_EDGE('',*,*,#2376,.T.);
#3945=ORIENTED_EDGE('',*,*,#2381,.T.);
#3946=ORIENTED_EDGE('',*,*,#2380,.T.);
#3947=ORIENTED_EDGE('',*,*,#2384,.T.);
#3948=ORIENTED_EDGE('',*,*,#2389,.T.);
#3949=ORIENTED_EDGE('',*,*,#2388,.T.);
#3950=ORIENTED_EDGE('',*,*,#2392,.T.);
#3951=ORIENTED_EDGE('',*,*,#2397,.T.);
#3952=ORIENTED_EDGE('',*,*,#2396,.T.);
#3953=ORIENTED_EDGE('',*,*,#2401,.T.);
#3954=ORIENTED_EDGE('',*,*,#2405,.T.);
#3955=ORIENTED_EDGE('',*,*,#2404,.T.);
#3956=ORIENTED_EDGE('',*,*,#2409,.T.);
#3957=ORIENTED_EDGE('',*,*,#2414,.T.);
#3958=ORIENTED_EDGE('',*,*,#2413,.T.);
#3959=ORIENTED_EDGE('',*,*,#2417,.T.);
#3960=ORIENTED_EDGE('',*,*,#2422,.T.);
#3961=ORIENTED_EDGE('',*,*,#2421,.T.);
#3962=ORIENTED_EDGE('',*,*,#2426,.T.);
#3963=ORIENTED_EDGE('',*,*,#2425,.T.);
#3964=ORIENTED_EDGE('',*,*,#2430,.T.);
#3965=ORIENTED_EDGE('',*,*,#2435,.T.);
#3966=ORIENTED_EDGE('',*,*,#2434,.T.);
#3967=ORIENTED_EDGE('',*,*,#2438,.T.);
#3968=ORIENTED_EDGE('',*,*,#2443,.T.);
#3969=ORIENTED_EDGE('',*,*,#2442,.T.);
#3970=ORIENTED_EDGE('',*,*,#2446,.T.);
#3971=ORIENTED_EDGE('',*,*,#2451,.T.);
#3972=ORIENTED_EDGE('',*,*,#2450,.T.);
#3973=ORIENTED_EDGE('',*,*,#2456,.T.);
#3974=ORIENTED_EDGE('',*,*,#2455,.T.);
#3975=ORIENTED_EDGE('',*,*,#2459,.T.);
#3976=ORIENTED_EDGE('',*,*,#2464,.T.);
#3977=ORIENTED_EDGE('',*,*,#2463,.T.);
#3978=ORIENTED_EDGE('',*,*,#2468,.T.);
#3979=ORIENTED_EDGE('',*,*,#2472,.T.);
#3980=ORIENTED_EDGE('',*,*,#2471,.T.);
#3981=ORIENTED_EDGE('',*,*,#2476,.T.);
#3982=ORIENTED_EDGE('',*,*,#2481,.T.);
#3983=ORIENTED_EDGE('',*,*,#2480,.T.);
#3984=ORIENTED_EDGE('',*,*,#2484,.T.);
#3985=ORIENTED_EDGE('',*,*,#2489,.T.);
#3986=ORIENTED_EDGE('',*,*,#2488,.T.);
#3987=ORIENTED_EDGE('',*,*,#2492,.T.);
#3988=ORIENTED_EDGE('',*,*,#2497,.T.);
#3989=ORIENTED_EDGE('',*,*,#2496,.T.);
#3990=ORIENTED_EDGE('',*,*,#2500,.T.);
#3991=ORIENTED_EDGE('',*,*,#2505,.T.);
#3992=ORIENTED_EDGE('',*,*,#2504,.T.);
#3993=ORIENTED_EDGE('',*,*,#2508,.T.);
#3994=ORIENTED_EDGE('',*,*,#2513,.T.);
#3995=ORIENTED_EDGE('',*,*,#2512,.T.);
#3996=ORIENTED_EDGE('',*,*,#2516,.T.);
#3997=ORIENTED_EDGE('',*,*,#2521,.T.);
#3998=ORIENTED_EDGE('',*,*,#2520,.T.);
#3999=ORIENTED_EDGE('',*,*,#2524,.T.);
#4000=ORIENTED_EDGE('',*,*,#2529,.T.);
#4001=ORIENTED_EDGE('',*,*,#2528,.T.);
#4002=ORIENTED_EDGE('',*,*,#2533,.T.);
#4003=ORIENTED_EDGE('',*,*,#2532,.T.);
#4004=ORIENTED_EDGE('',*,*,#2538,.T.);
#4005=ORIENTED_EDGE('',*,*,#2537,.T.);
#4006=ORIENTED_EDGE('',*,*,#2541,.T.);
#4007=ORIENTED_EDGE('',*,*,#2546,.T.);
#4008=ORIENTED_EDGE('',*,*,#2545,.T.);
#4009=ORIENTED_EDGE('',*,*,#2551,.T.);
#4010=ORIENTED_EDGE('',*,*,#2550,.T.);
#4011=ORIENTED_EDGE('',*,*,#2554,.T.);
#4012=ORIENTED_EDGE('',*,*,#2559,.T.);
#4013=ORIENTED_EDGE('',*,*,#2558,.T.);
#4014=ORIENTED_EDGE('',*,*,#2562,.T.);
#4015=ORIENTED_EDGE('',*,*,#2567,.T.);
#4016=ORIENTED_EDGE('',*,*,#2566,.T.);
#4017=ORIENTED_EDGE('',*,*,#2570,.T.);
#4018=ORIENTED_EDGE('',*,*,#2575,.T.);
#4019=ORIENTED_EDGE('',*,*,#2574,.T.);
#4020=ORIENTED_EDGE('',*,*,#2579,.T.);
#4021=ORIENTED_EDGE('',*,*,#2578,.T.);
#4022=ORIENTED_EDGE('',*,*,#2583,.T.);
#4023=ORIENTED_EDGE('',*,*,#2587,.T.);
#4024=ORIENTED_EDGE('',*,*,#2586,.T.);
#4025=ORIENTED_EDGE('',*,*,#2765,.T.);
#4026=ORIENTED_EDGE('',*,*,#2764,.T.);
#4027=ORIENTED_EDGE('',*,*,#2768,.F.);
#4028=ORIENTED_EDGE('',*,*,#2769,.F.);
#4029=ORIENTED_EDGE('',*,*,#2762,.F.);
#4030=ORIENTED_EDGE('',*,*,#2589,.F.);
#4031=ORIENTED_EDGE('',*,*,#2588,.F.);
#4032=ORIENTED_EDGE('',*,*,#2584,.F.);
#4033=ORIENTED_EDGE('',*,*,#2581,.F.);
#4034=ORIENTED_EDGE('',*,*,#2580,.F.);
#4035=ORIENTED_EDGE('',*,*,#2576,.F.);
#4036=ORIENTED_EDGE('',*,*,#2572,.F.);
#4037=ORIENTED_EDGE('',*,*,#2571,.F.);
#4038=ORIENTED_EDGE('',*,*,#2568,.F.);
#4039=ORIENTED_EDGE('',*,*,#2564,.F.);
#4040=ORIENTED_EDGE('',*,*,#2563,.F.);
#4041=ORIENTED_EDGE('',*,*,#2560,.F.);
#4042=ORIENTED_EDGE('',*,*,#2556,.F.);
#4043=ORIENTED_EDGE('',*,*,#2555,.F.);
#4044=ORIENTED_EDGE('',*,*,#2552,.F.);
#4045=ORIENTED_EDGE('',*,*,#2548,.F.);
#4046=ORIENTED_EDGE('',*,*,#2547,.F.);
#4047=ORIENTED_EDGE('',*,*,#2543,.F.);
#4048=ORIENTED_EDGE('',*,*,#2542,.F.);
#4049=ORIENTED_EDGE('',*,*,#2539,.F.);
#4050=ORIENTED_EDGE('',*,*,#2535,.F.);
#4051=ORIENTED_EDGE('',*,*,#2534,.F.);
#4052=ORIENTED_EDGE('',*,*,#2530,.F.);
#4053=ORIENTED_EDGE('',*,*,#2526,.F.);
#4054=ORIENTED_EDGE('',*,*,#2525,.F.);
#4055=ORIENTED_EDGE('',*,*,#2522,.F.);
#4056=ORIENTED_EDGE('',*,*,#2518,.F.);
#4057=ORIENTED_EDGE('',*,*,#2517,.F.);
#4058=ORIENTED_EDGE('',*,*,#2514,.F.);
#4059=ORIENTED_EDGE('',*,*,#2510,.F.);
#4060=ORIENTED_EDGE('',*,*,#2509,.F.);
#4061=ORIENTED_EDGE('',*,*,#2506,.F.);
#4062=ORIENTED_EDGE('',*,*,#2502,.F.);
#4063=ORIENTED_EDGE('',*,*,#2501,.F.);
#4064=ORIENTED_EDGE('',*,*,#2498,.F.);
#4065=ORIENTED_EDGE('',*,*,#2494,.F.);
#4066=ORIENTED_EDGE('',*,*,#2493,.F.);
#4067=ORIENTED_EDGE('',*,*,#2490,.F.);
#4068=ORIENTED_EDGE('',*,*,#2486,.F.);
#4069=ORIENTED_EDGE('',*,*,#2485,.F.);
#4070=ORIENTED_EDGE('',*,*,#2482,.F.);
#4071=ORIENTED_EDGE('',*,*,#2478,.F.);
#4072=ORIENTED_EDGE('',*,*,#2477,.F.);
#4073=ORIENTED_EDGE('',*,*,#2474,.F.);
#4074=ORIENTED_EDGE('',*,*,#2473,.F.);
#4075=ORIENTED_EDGE('',*,*,#2469,.F.);
#4076=ORIENTED_EDGE('',*,*,#2466,.F.);
#4077=ORIENTED_EDGE('',*,*,#2465,.F.);
#4078=ORIENTED_EDGE('',*,*,#2461,.F.);
#4079=ORIENTED_EDGE('',*,*,#2460,.F.);
#4080=ORIENTED_EDGE('',*,*,#2457,.F.);
#4081=ORIENTED_EDGE('',*,*,#2453,.F.);
#4082=ORIENTED_EDGE('',*,*,#2452,.F.);
#4083=ORIENTED_EDGE('',*,*,#2448,.F.);
#4084=ORIENTED_EDGE('',*,*,#2447,.F.);
#4085=ORIENTED_EDGE('',*,*,#2444,.F.);
#4086=ORIENTED_EDGE('',*,*,#2440,.F.);
#4087=ORIENTED_EDGE('',*,*,#2439,.F.);
#4088=ORIENTED_EDGE('',*,*,#2436,.F.);
#4089=ORIENTED_EDGE('',*,*,#2432,.F.);
#4090=ORIENTED_EDGE('',*,*,#2431,.F.);
#4091=ORIENTED_EDGE('',*,*,#2428,.F.);
#4092=ORIENTED_EDGE('',*,*,#2427,.F.);
#4093=ORIENTED_EDGE('',*,*,#2423,.F.);
#4094=ORIENTED_EDGE('',*,*,#2419,.F.);
#4095=ORIENTED_EDGE('',*,*,#2418,.F.);
#4096=ORIENTED_EDGE('',*,*,#2415,.F.);
#4097=ORIENTED_EDGE('',*,*,#2411,.F.);
#4098=ORIENTED_EDGE('',*,*,#2410,.F.);
#4099=ORIENTED_EDGE('',*,*,#2407,.F.);
#4100=ORIENTED_EDGE('',*,*,#2406,.F.);
#4101=ORIENTED_EDGE('',*,*,#2402,.F.);
#4102=ORIENTED_EDGE('',*,*,#2399,.F.);
#4103=ORIENTED_EDGE('',*,*,#2398,.F.);
#4104=ORIENTED_EDGE('',*,*,#2394,.F.);
#4105=ORIENTED_EDGE('',*,*,#2393,.F.);
#4106=ORIENTED_EDGE('',*,*,#2390,.F.);
#4107=ORIENTED_EDGE('',*,*,#2386,.F.);
#4108=ORIENTED_EDGE('',*,*,#2385,.F.);
#4109=ORIENTED_EDGE('',*,*,#2382,.F.);
#4110=ORIENTED_EDGE('',*,*,#2378,.F.);
#4111=ORIENTED_EDGE('',*,*,#2377,.F.);
#4112=ORIENTED_EDGE('',*,*,#2374,.F.);
#4113=ORIENTED_EDGE('',*,*,#2370,.F.);
#4114=ORIENTED_EDGE('',*,*,#2369,.F.);
#4115=ORIENTED_EDGE('',*,*,#2366,.F.);
#4116=ORIENTED_EDGE('',*,*,#2362,.F.);
#4117=ORIENTED_EDGE('',*,*,#2361,.F.);
#4118=ORIENTED_EDGE('',*,*,#2358,.F.);
#4119=ORIENTED_EDGE('',*,*,#2354,.F.);
#4120=ORIENTED_EDGE('',*,*,#2353,.F.);
#4121=ORIENTED_EDGE('',*,*,#2350,.F.);
#4122=ORIENTED_EDGE('',*,*,#2346,.F.);
#4123=ORIENTED_EDGE('',*,*,#2345,.F.);
#4124=ORIENTED_EDGE('',*,*,#2342,.F.);
#4125=ORIENTED_EDGE('',*,*,#2338,.F.);
#4126=ORIENTED_EDGE('',*,*,#2337,.F.);
#4127=ORIENTED_EDGE('',*,*,#2334,.F.);
#4128=ORIENTED_EDGE('',*,*,#2330,.F.);
#4129=ORIENTED_EDGE('',*,*,#2329,.F.);
#4130=ORIENTED_EDGE('',*,*,#2326,.F.);
#4131=ORIENTED_EDGE('',*,*,#2322,.F.);
#4132=ORIENTED_EDGE('',*,*,#2321,.F.);
#4133=ORIENTED_EDGE('',*,*,#2318,.F.);
#4134=ORIENTED_EDGE('',*,*,#2314,.F.);
#4135=ORIENTED_EDGE('',*,*,#2313,.F.);
#4136=ORIENTED_EDGE('',*,*,#2310,.F.);
#4137=ORIENTED_EDGE('',*,*,#2309,.F.);
#4138=ORIENTED_EDGE('',*,*,#2305,.F.);
#4139=ORIENTED_EDGE('',*,*,#2302,.F.);
#4140=ORIENTED_EDGE('',*,*,#2301,.F.);
#4141=ORIENTED_EDGE('',*,*,#2297,.F.);
#4142=ORIENTED_EDGE('',*,*,#2294,.F.);
#4143=ORIENTED_EDGE('',*,*,#2293,.F.);
#4144=ORIENTED_EDGE('',*,*,#2289,.F.);
#4145=ORIENTED_EDGE('',*,*,#2286,.F.);
#4146=ORIENTED_EDGE('',*,*,#2285,.F.);
#4147=ORIENTED_EDGE('',*,*,#2281,.F.);
#4148=ORIENTED_EDGE('',*,*,#2278,.F.);
#4149=ORIENTED_EDGE('',*,*,#2277,.F.);
#4150=ORIENTED_EDGE('',*,*,#2273,.F.);
#4151=ORIENTED_EDGE('',*,*,#2270,.F.);
#4152=ORIENTED_EDGE('',*,*,#2269,.F.);
#4153=ORIENTED_EDGE('',*,*,#2265,.F.);
#4154=ORIENTED_EDGE('',*,*,#2262,.F.);
#4155=ORIENTED_EDGE('',*,*,#2261,.F.);
#4156=ORIENTED_EDGE('',*,*,#2257,.F.);
#4157=ORIENTED_EDGE('',*,*,#2254,.F.);
#4158=ORIENTED_EDGE('',*,*,#2253,.F.);
#4159=ORIENTED_EDGE('',*,*,#2249,.F.);
#4160=ORIENTED_EDGE('',*,*,#2770,.F.);
#4161=ORIENTED_EDGE('',*,*,#2590,.F.);
#4162=ORIENTED_EDGE('',*,*,#2761,.F.);
#4163=ORIENTED_EDGE('',*,*,#2760,.F.);
#4164=ORIENTED_EDGE('',*,*,#2759,.F.);
#4165=ORIENTED_EDGE('',*,*,#2758,.F.);
#4166=ORIENTED_EDGE('',*,*,#2757,.F.);
#4167=ORIENTED_EDGE('',*,*,#2756,.F.);
#4168=ORIENTED_EDGE('',*,*,#2755,.F.);
#4169=ORIENTED_EDGE('',*,*,#2754,.F.);
#4170=ORIENTED_EDGE('',*,*,#2753,.F.);
#4171=ORIENTED_EDGE('',*,*,#2752,.F.);
#4172=ORIENTED_EDGE('',*,*,#2751,.F.);
#4173=ORIENTED_EDGE('',*,*,#2750,.F.);
#4174=ORIENTED_EDGE('',*,*,#2749,.F.);
#4175=ORIENTED_EDGE('',*,*,#2748,.F.);
#4176=ORIENTED_EDGE('',*,*,#2747,.F.);
#4177=ORIENTED_EDGE('',*,*,#2746,.F.);
#4178=ORIENTED_EDGE('',*,*,#2745,.F.);
#4179=ORIENTED_EDGE('',*,*,#2744,.F.);
#4180=ORIENTED_EDGE('',*,*,#2743,.F.);
#4181=ORIENTED_EDGE('',*,*,#2742,.F.);
#4182=ORIENTED_EDGE('',*,*,#2741,.F.);
#4183=ORIENTED_EDGE('',*,*,#2740,.F.);
#4184=ORIENTED_EDGE('',*,*,#2739,.F.);
#4185=ORIENTED_EDGE('',*,*,#2738,.F.);
#4186=ORIENTED_EDGE('',*,*,#2737,.F.);
#4187=ORIENTED_EDGE('',*,*,#2736,.F.);
#4188=ORIENTED_EDGE('',*,*,#2735,.F.);
#4189=ORIENTED_EDGE('',*,*,#2734,.F.);
#4190=ORIENTED_EDGE('',*,*,#2733,.F.);
#4191=ORIENTED_EDGE('',*,*,#2732,.F.);
#4192=ORIENTED_EDGE('',*,*,#2731,.F.);
#4193=ORIENTED_EDGE('',*,*,#2730,.F.);
#4194=ORIENTED_EDGE('',*,*,#2729,.F.);
#4195=ORIENTED_EDGE('',*,*,#2728,.F.);
#4196=ORIENTED_EDGE('',*,*,#2727,.F.);
#4197=ORIENTED_EDGE('',*,*,#2726,.F.);
#4198=ORIENTED_EDGE('',*,*,#2725,.F.);
#4199=ORIENTED_EDGE('',*,*,#2724,.F.);
#4200=ORIENTED_EDGE('',*,*,#2723,.F.);
#4201=ORIENTED_EDGE('',*,*,#2722,.F.);
#4202=ORIENTED_EDGE('',*,*,#2721,.F.);
#4203=ORIENTED_EDGE('',*,*,#2720,.F.);
#4204=ORIENTED_EDGE('',*,*,#2719,.F.);
#4205=ORIENTED_EDGE('',*,*,#2718,.F.);
#4206=ORIENTED_EDGE('',*,*,#2717,.F.);
#4207=ORIENTED_EDGE('',*,*,#2716,.F.);
#4208=ORIENTED_EDGE('',*,*,#2715,.F.);
#4209=ORIENTED_EDGE('',*,*,#2714,.F.);
#4210=ORIENTED_EDGE('',*,*,#2713,.F.);
#4211=ORIENTED_EDGE('',*,*,#2712,.F.);
#4212=ORIENTED_EDGE('',*,*,#2711,.F.);
#4213=ORIENTED_EDGE('',*,*,#2710,.F.);
#4214=ORIENTED_EDGE('',*,*,#2709,.F.);
#4215=ORIENTED_EDGE('',*,*,#2708,.F.);
#4216=ORIENTED_EDGE('',*,*,#2707,.F.);
#4217=ORIENTED_EDGE('',*,*,#2706,.F.);
#4218=ORIENTED_EDGE('',*,*,#2705,.F.);
#4219=ORIENTED_EDGE('',*,*,#2704,.F.);
#4220=ORIENTED_EDGE('',*,*,#2703,.F.);
#4221=ORIENTED_EDGE('',*,*,#2702,.F.);
#4222=ORIENTED_EDGE('',*,*,#2701,.F.);
#4223=ORIENTED_EDGE('',*,*,#2700,.F.);
#4224=ORIENTED_EDGE('',*,*,#2699,.F.);
#4225=ORIENTED_EDGE('',*,*,#2698,.F.);
#4226=ORIENTED_EDGE('',*,*,#2697,.F.);
#4227=ORIENTED_EDGE('',*,*,#2696,.F.);
#4228=ORIENTED_EDGE('',*,*,#2695,.F.);
#4229=ORIENTED_EDGE('',*,*,#2694,.F.);
#4230=ORIENTED_EDGE('',*,*,#2693,.F.);
#4231=ORIENTED_EDGE('',*,*,#2692,.F.);
#4232=ORIENTED_EDGE('',*,*,#2691,.F.);
#4233=ORIENTED_EDGE('',*,*,#2690,.F.);
#4234=ORIENTED_EDGE('',*,*,#2689,.F.);
#4235=ORIENTED_EDGE('',*,*,#2688,.F.);
#4236=ORIENTED_EDGE('',*,*,#2687,.F.);
#4237=ORIENTED_EDGE('',*,*,#2686,.F.);
#4238=ORIENTED_EDGE('',*,*,#2685,.F.);
#4239=ORIENTED_EDGE('',*,*,#2684,.F.);
#4240=ORIENTED_EDGE('',*,*,#2683,.F.);
#4241=ORIENTED_EDGE('',*,*,#2682,.F.);
#4242=ORIENTED_EDGE('',*,*,#2681,.F.);
#4243=ORIENTED_EDGE('',*,*,#2680,.F.);
#4244=ORIENTED_EDGE('',*,*,#2679,.F.);
#4245=ORIENTED_EDGE('',*,*,#2678,.F.);
#4246=ORIENTED_EDGE('',*,*,#2766,.T.);
#4247=ORIENTED_EDGE('',*,*,#2763,.T.);
#4248=ORIENTED_EDGE('',*,*,#2769,.T.);
#4249=ORIENTED_EDGE('',*,*,#2768,.T.);
#4250=ORIENTED_EDGE('',*,*,#2677,.T.);
#4251=ORIENTED_EDGE('',*,*,#2767,.T.);
#4252=ORIENTED_EDGE('',*,*,#2591,.T.);
#4253=ORIENTED_EDGE('',*,*,#2770,.T.);
#4254=ORIENTED_EDGE('',*,*,#2248,.T.);
#4255=CYLINDRICAL_SURFACE('',#4624,20.5);
#4256=CYLINDRICAL_SURFACE('',#4631,20.);
#4257=CYLINDRICAL_SURFACE('',#4634,0.5);
#4258=CYLINDRICAL_SURFACE('',#4637,0.5);
#4259=CYLINDRICAL_SURFACE('',#4639,0.5);
#4260=CYLINDRICAL_SURFACE('',#4641,0.5);
#4261=CYLINDRICAL_SURFACE('',#4644,0.5);
#4262=CYLINDRICAL_SURFACE('',#4646,0.5);
#4263=CYLINDRICAL_SURFACE('',#4647,0.5);
#4264=CYLINDRICAL_SURFACE('',#4649,0.5);
#4265=CYLINDRICAL_SURFACE('',#4664,4.);
#4266=CYLINDRICAL_SURFACE('',#4671,4.);
#4267=CYLINDRICAL_SURFACE('',#4678,4.);
#4268=CYLINDRICAL_SURFACE('',#4683,20.);
#4269=CYLINDRICAL_SURFACE('',#4690,4.);
#4270=CYLINDRICAL_SURFACE('',#4693,0.5);
#4271=CYLINDRICAL_SURFACE('',#4696,0.5);
#4272=CYLINDRICAL_SURFACE('',#4698,0.5);
#4273=CYLINDRICAL_SURFACE('',#4700,0.5);
#4274=CYLINDRICAL_SURFACE('',#4702,0.5);
#4275=CYLINDRICAL_SURFACE('',#4704,0.5);
#4276=CYLINDRICAL_SURFACE('',#4706,0.5);
#4277=CYLINDRICAL_SURFACE('',#4708,0.5);
#4278=CYLINDRICAL_SURFACE('',#4745,4.);
#4279=CYLINDRICAL_SURFACE('',#4750,4.);
#4280=CYLINDRICAL_SURFACE('',#4756,4.);
#4281=CYLINDRICAL_SURFACE('',#4764,4.);
#4282=CYLINDRICAL_SURFACE('',#4767,0.5);
#4283=CYLINDRICAL_SURFACE('',#4770,0.5);
#4284=CYLINDRICAL_SURFACE('',#4772,0.5);
#4285=CYLINDRICAL_SURFACE('',#4774,0.5);
#4286=CYLINDRICAL_SURFACE('',#4777,0.5);
#4287=CYLINDRICAL_SURFACE('',#4779,0.5);
#4288=CYLINDRICAL_SURFACE('',#4780,0.5);
#4289=CYLINDRICAL_SURFACE('',#4782,0.5);
#4290=CYLINDRICAL_SURFACE('',#4805,0.5);
#4291=CYLINDRICAL_SURFACE('',#4808,0.5);
#4292=CYLINDRICAL_SURFACE('',#4810,0.5);
#4293=CYLINDRICAL_SURFACE('',#4812,0.5);
#4294=CYLINDRICAL_SURFACE('',#4815,0.5);
#4295=CYLINDRICAL_SURFACE('',#4817,0.5);
#4296=CYLINDRICAL_SURFACE('',#4818,0.5);
#4297=CYLINDRICAL_SURFACE('',#4820,0.5);
#4298=CYLINDRICAL_SURFACE('',#4823,20.5);
#4299=CYLINDRICAL_SURFACE('',#4825,19.5);
#4300=CYLINDRICAL_SURFACE('',#4836,20.5);
#4301=CYLINDRICAL_SURFACE('',#4846,3.22275);
#4302=CYLINDRICAL_SURFACE('',#4848,3.22275);
#4303=CYLINDRICAL_SURFACE('',#4849,3.22275);
#4304=CYLINDRICAL_SURFACE('',#4850,3.22275);
#4305=CYLINDRICAL_SURFACE('',#4851,3.22275);
#4306=CYLINDRICAL_SURFACE('',#4852,3.22275);
#4307=CYLINDRICAL_SURFACE('',#4853,3.22275);
#4308=CYLINDRICAL_SURFACE('',#4854,3.22275);
#4309=CYLINDRICAL_SURFACE('',#4855,3.22275);
#4310=CYLINDRICAL_SURFACE('',#4856,3.22275);
#4311=CYLINDRICAL_SURFACE('',#4857,3.22275);
#4312=CYLINDRICAL_SURFACE('',#4858,3.22275);
#4313=CYLINDRICAL_SURFACE('',#4859,3.22275);
#4314=CYLINDRICAL_SURFACE('',#4860,3.22275);
#4315=CYLINDRICAL_SURFACE('',#4861,3.22275);
#4316=CYLINDRICAL_SURFACE('',#4862,3.22275);
#4317=CYLINDRICAL_SURFACE('',#4863,3.22275);
#4318=CYLINDRICAL_SURFACE('',#4864,3.22275);
#4319=CYLINDRICAL_SURFACE('',#4865,3.22275);
#4320=CYLINDRICAL_SURFACE('',#4866,3.22275);
#4321=CYLINDRICAL_SURFACE('',#4867,3.22275);
#4322=CYLINDRICAL_SURFACE('',#4868,3.22275);
#4323=CYLINDRICAL_SURFACE('',#4869,3.22275);
#4324=CYLINDRICAL_SURFACE('',#4870,3.22275);
#4325=CYLINDRICAL_SURFACE('',#4871,3.22275);
#4326=CYLINDRICAL_SURFACE('',#4872,3.22275);
#4327=CYLINDRICAL_SURFACE('',#4873,3.22275);
#4328=CYLINDRICAL_SURFACE('',#4874,3.22275);
#4329=CYLINDRICAL_SURFACE('',#4875,3.22275);
#4330=CYLINDRICAL_SURFACE('',#4876,3.22275);
#4331=CYLINDRICAL_SURFACE('',#4877,3.22275);
#4332=CYLINDRICAL_SURFACE('',#4878,3.22275);
#4333=CYLINDRICAL_SURFACE('',#4879,3.22275);
#4334=CYLINDRICAL_SURFACE('',#4880,3.22275);
#4335=CYLINDRICAL_SURFACE('',#4881,3.22275);
#4336=CYLINDRICAL_SURFACE('',#4882,3.22275);
#4337=CYLINDRICAL_SURFACE('',#4883,3.22275);
#4338=CYLINDRICAL_SURFACE('',#4884,3.22275);
#4339=CYLINDRICAL_SURFACE('',#4885,3.22275);
#4340=CYLINDRICAL_SURFACE('',#4886,3.22275);
#4341=CYLINDRICAL_SURFACE('',#4887,3.22275);
#4342=CYLINDRICAL_SURFACE('',#4888,3.22275);
#4343=CYLINDRICAL_SURFACE('',#4889,3.22275);
#4344=CYLINDRICAL_SURFACE('',#4890,3.22275);
#4345=CYLINDRICAL_SURFACE('',#4891,3.22275);
#4346=CYLINDRICAL_SURFACE('',#4892,3.22275);
#4347=CYLINDRICAL_SURFACE('',#4893,3.22275);
#4348=CYLINDRICAL_SURFACE('',#4894,3.22275);
#4349=CYLINDRICAL_SURFACE('',#4895,3.22275);
#4350=CYLINDRICAL_SURFACE('',#4896,3.22275);
#4351=CYLINDRICAL_SURFACE('',#4897,3.22275);
#4352=CYLINDRICAL_SURFACE('',#4898,3.22275);
#4353=CYLINDRICAL_SURFACE('',#4899,3.22275);
#4354=CYLINDRICAL_SURFACE('',#4900,3.22275);
#4355=CYLINDRICAL_SURFACE('',#4901,3.22275);
#4356=CYLINDRICAL_SURFACE('',#4902,3.22275);
#4357=CYLINDRICAL_SURFACE('',#4903,3.22275);
#4358=CYLINDRICAL_SURFACE('',#4904,3.22275);
#4359=CYLINDRICAL_SURFACE('',#4905,3.22275);
#4360=CYLINDRICAL_SURFACE('',#4906,3.22275);
#4361=CYLINDRICAL_SURFACE('',#4907,3.22275);
#4362=CYLINDRICAL_SURFACE('',#4908,3.22275);
#4363=CYLINDRICAL_SURFACE('',#4909,3.22275);
#4364=CYLINDRICAL_SURFACE('',#4910,3.22275);
#4365=CYLINDRICAL_SURFACE('',#4911,3.22275);
#4366=CYLINDRICAL_SURFACE('',#4912,3.22275);
#4367=CYLINDRICAL_SURFACE('',#4913,3.22275);
#4368=CYLINDRICAL_SURFACE('',#4914,3.22275);
#4369=CYLINDRICAL_SURFACE('',#4915,3.22275);
#4370=CYLINDRICAL_SURFACE('',#4916,3.22275);
#4371=CYLINDRICAL_SURFACE('',#4917,3.22275);
#4372=CYLINDRICAL_SURFACE('',#4918,3.22275);
#4373=CYLINDRICAL_SURFACE('',#4919,3.22275);
#4374=CYLINDRICAL_SURFACE('',#4920,3.22275);
#4375=CYLINDRICAL_SURFACE('',#4921,3.22275);
#4376=CYLINDRICAL_SURFACE('',#4922,3.22275);
#4377=CYLINDRICAL_SURFACE('',#4923,3.22275);
#4378=CYLINDRICAL_SURFACE('',#4924,3.22275);
#4379=CYLINDRICAL_SURFACE('',#4925,3.22275);
#4380=CYLINDRICAL_SURFACE('',#4926,3.22275);
#4381=CYLINDRICAL_SURFACE('',#4927,3.22275);
#4382=CYLINDRICAL_SURFACE('',#4928,3.22275);
#4383=CYLINDRICAL_SURFACE('',#4929,3.22275);
#4384=CYLINDRICAL_SURFACE('',#4930,3.22275);
#4385=CYLINDRICAL_SURFACE('',#4931,3.933);
#4386=CYLINDRICAL_SURFACE('',#4934,3.22275);
#4387=ADVANCED_FACE('',(#612),#4255,.F.);
#4388=ADVANCED_FACE('',(#613,#558),#584,.F.);
#4389=ADVANCED_FACE('',(#614,#559),#585,.F.);
#4390=ADVANCED_FACE('',(#615),#4256,.F.);
#4391=ADVANCED_FACE('',(#616),#4257,.T.);
#4392=ADVANCED_FACE('',(#617),#4258,.T.);
#4393=ADVANCED_FACE('',(#618),#4259,.T.);
#4394=ADVANCED_FACE('',(#619),#4260,.T.);
#4395=ADVANCED_FACE('',(#620),#4261,.T.);
#4396=ADVANCED_FACE('',(#621),#4262,.T.);
#4397=ADVANCED_FACE('',(#622),#4263,.T.);
#4398=ADVANCED_FACE('',(#623),#4264,.T.);
#4399=ADVANCED_FACE('',(#624),#586,.T.);
#4400=ADVANCED_FACE('',(#625),#587,.T.);
#4401=ADVANCED_FACE('',(#626),#588,.T.);
#4402=ADVANCED_FACE('',(#627),#589,.T.);
#4403=ADVANCED_FACE('',(#628,#560,#561,#562,#563,#564),#590,.F.);
#4404=ADVANCED_FACE('',(#629),#502,.T.);
#4405=ADVANCED_FACE('',(#630),#4265,.F.);
#4406=ADVANCED_FACE('',(#631),#503,.T.);
#4407=ADVANCED_FACE('',(#632),#4266,.F.);
#4408=ADVANCED_FACE('',(#633),#504,.T.);
#4409=ADVANCED_FACE('',(#634),#4267,.F.);
#4410=ADVANCED_FACE('',(#635),#505,.T.);
#4411=ADVANCED_FACE('',(#636),#4268,.F.);
#4412=ADVANCED_FACE('',(#637),#506,.T.);
#4413=ADVANCED_FACE('',(#638),#4269,.F.);
#4414=ADVANCED_FACE('',(#639),#4270,.T.);
#4415=ADVANCED_FACE('',(#640),#4271,.T.);
#4416=ADVANCED_FACE('',(#641),#4272,.T.);
#4417=ADVANCED_FACE('',(#642),#4273,.T.);
#4418=ADVANCED_FACE('',(#643),#4274,.T.);
#4419=ADVANCED_FACE('',(#644),#4275,.T.);
#4420=ADVANCED_FACE('',(#645),#4276,.T.);
#4421=ADVANCED_FACE('',(#646),#4277,.T.);
#4422=ADVANCED_FACE('',(#647),#591,.T.);
#4423=ADVANCED_FACE('',(#648,#565,#566,#567,#568,#569),#592,.T.);
#4424=ADVANCED_FACE('',(#649),#507,.T.);
#4425=ADVANCED_FACE('',(#650),#508,.T.);
#4426=ADVANCED_FACE('',(#651),#509,.T.);
#4427=ADVANCED_FACE('',(#652),#510,.T.);
#4428=ADVANCED_FACE('',(#653),#511,.T.);
#4429=ADVANCED_FACE('',(#654),#593,.T.);
#4430=ADVANCED_FACE('',(#655),#594,.T.);
#4431=ADVANCED_FACE('',(#656),#595,.T.);
#4432=ADVANCED_FACE('',(#657,#570),#596,.F.);
#4433=ADVANCED_FACE('',(#658,#571),#597,.F.);
#4434=ADVANCED_FACE('',(#659),#512,.T.);
#4435=ADVANCED_FACE('',(#660,#572,#573,#574,#575,#576),#598,.F.);
#4436=ADVANCED_FACE('',(#661),#4278,.F.);
#4437=ADVANCED_FACE('',(#662),#513,.T.);
#4438=ADVANCED_FACE('',(#663),#4279,.F.);
#4439=ADVANCED_FACE('',(#664),#514,.T.);
#4440=ADVANCED_FACE('',(#665),#4280,.F.);
#4441=ADVANCED_FACE('',(#666),#515,.T.);
#4442=ADVANCED_FACE('',(#667),#516,.T.);
#4443=ADVANCED_FACE('',(#668),#4281,.F.);
#4444=ADVANCED_FACE('',(#669),#4282,.T.);
#4445=ADVANCED_FACE('',(#670),#4283,.T.);
#4446=ADVANCED_FACE('',(#671),#4284,.T.);
#4447=ADVANCED_FACE('',(#672),#4285,.T.);
#4448=ADVANCED_FACE('',(#673),#4286,.T.);
#4449=ADVANCED_FACE('',(#674),#4287,.T.);
#4450=ADVANCED_FACE('',(#675),#4288,.T.);
#4451=ADVANCED_FACE('',(#676),#4289,.T.);
#4452=ADVANCED_FACE('',(#677),#599,.T.);
#4453=ADVANCED_FACE('',(#678),#600,.T.);
#4454=ADVANCED_FACE('',(#679),#601,.T.);
#4455=ADVANCED_FACE('',(#680),#602,.T.);
#4456=ADVANCED_FACE('',(#681),#603,.T.);
#4457=ADVANCED_FACE('',(#682),#604,.T.);
#4458=ADVANCED_FACE('',(#683),#605,.T.);
#4459=ADVANCED_FACE('',(#684),#606,.T.);
#4460=ADVANCED_FACE('',(#685),#517,.T.);
#4461=ADVANCED_FACE('',(#686,#577,#578,#579,#580,#581),#607,.T.);
#4462=ADVANCED_FACE('',(#687),#518,.T.);
#4463=ADVANCED_FACE('',(#688),#519,.T.);
#4464=ADVANCED_FACE('',(#689),#520,.T.);
#4465=ADVANCED_FACE('',(#690),#4290,.T.);
#4466=ADVANCED_FACE('',(#691),#4291,.T.);
#4467=ADVANCED_FACE('',(#692),#4292,.T.);
#4468=ADVANCED_FACE('',(#693),#4293,.T.);
#4469=ADVANCED_FACE('',(#694),#4294,.T.);
#4470=ADVANCED_FACE('',(#695),#4295,.T.);
#4471=ADVANCED_FACE('',(#696),#4296,.T.);
#4472=ADVANCED_FACE('',(#697),#4297,.T.);
#4473=ADVANCED_FACE('',(#698),#521,.T.);
#4474=ADVANCED_FACE('',(#699),#4298,.F.);
#4475=ADVANCED_FACE('',(#700),#4299,.F.);
#4476=ADVANCED_FACE('',(#701),#522,.T.);
#4477=ADVANCED_FACE('',(#702,#582),#608,.T.);
#4478=ADVANCED_FACE('',(#703),#523,.T.);
#4479=ADVANCED_FACE('',(#704),#4300,.T.);
#4480=ADVANCED_FACE('',(#705),#524,.T.);
#4481=ADVANCED_FACE('',(#706,#583),#609,.T.);
#4482=ADVANCED_FACE('',(#707),#525,.T.);
#4483=ADVANCED_FACE('',(#708),#4301,.T.);
#4484=ADVANCED_FACE('',(#709),#4302,.T.);
#4485=ADVANCED_FACE('',(#710),#4303,.T.);
#4486=ADVANCED_FACE('',(#711),#4304,.T.);
#4487=ADVANCED_FACE('',(#712),#4305,.T.);
#4488=ADVANCED_FACE('',(#713),#4306,.T.);
#4489=ADVANCED_FACE('',(#714),#4307,.T.);
#4490=ADVANCED_FACE('',(#715),#4308,.T.);
#4491=ADVANCED_FACE('',(#716),#4309,.T.);
#4492=ADVANCED_FACE('',(#717),#4310,.T.);
#4493=ADVANCED_FACE('',(#718),#4311,.T.);
#4494=ADVANCED_FACE('',(#719),#4312,.T.);
#4495=ADVANCED_FACE('',(#720),#4313,.T.);
#4496=ADVANCED_FACE('',(#721),#4314,.T.);
#4497=ADVANCED_FACE('',(#722),#4315,.T.);
#4498=ADVANCED_FACE('',(#723),#4316,.T.);
#4499=ADVANCED_FACE('',(#724),#4317,.T.);
#4500=ADVANCED_FACE('',(#725),#4318,.T.);
#4501=ADVANCED_FACE('',(#726),#4319,.T.);
#4502=ADVANCED_FACE('',(#727),#4320,.T.);
#4503=ADVANCED_FACE('',(#728),#4321,.T.);
#4504=ADVANCED_FACE('',(#729),#4322,.T.);
#4505=ADVANCED_FACE('',(#730),#4323,.T.);
#4506=ADVANCED_FACE('',(#731),#4324,.T.);
#4507=ADVANCED_FACE('',(#732),#4325,.T.);
#4508=ADVANCED_FACE('',(#733),#4326,.T.);
#4509=ADVANCED_FACE('',(#734),#4327,.T.);
#4510=ADVANCED_FACE('',(#735),#4328,.T.);
#4511=ADVANCED_FACE('',(#736),#4329,.T.);
#4512=ADVANCED_FACE('',(#737),#4330,.T.);
#4513=ADVANCED_FACE('',(#738),#4331,.T.);
#4514=ADVANCED_FACE('',(#739),#4332,.T.);
#4515=ADVANCED_FACE('',(#740),#4333,.T.);
#4516=ADVANCED_FACE('',(#741),#4334,.T.);
#4517=ADVANCED_FACE('',(#742),#4335,.T.);
#4518=ADVANCED_FACE('',(#743),#4336,.T.);
#4519=ADVANCED_FACE('',(#744),#4337,.T.);
#4520=ADVANCED_FACE('',(#745),#4338,.T.);
#4521=ADVANCED_FACE('',(#746),#4339,.T.);
#4522=ADVANCED_FACE('',(#747),#4340,.T.);
#4523=ADVANCED_FACE('',(#748),#4341,.T.);
#4524=ADVANCED_FACE('',(#749),#4342,.T.);
#4525=ADVANCED_FACE('',(#750),#4343,.T.);
#4526=ADVANCED_FACE('',(#751),#4344,.T.);
#4527=ADVANCED_FACE('',(#752),#4345,.T.);
#4528=ADVANCED_FACE('',(#753),#4346,.T.);
#4529=ADVANCED_FACE('',(#754),#4347,.T.);
#4530=ADVANCED_FACE('',(#755),#4348,.T.);
#4531=ADVANCED_FACE('',(#756),#4349,.T.);
#4532=ADVANCED_FACE('',(#757),#4350,.T.);
#4533=ADVANCED_FACE('',(#758),#4351,.T.);
#4534=ADVANCED_FACE('',(#759),#4352,.T.);
#4535=ADVANCED_FACE('',(#760),#4353,.T.);
#4536=ADVANCED_FACE('',(#761),#4354,.T.);
#4537=ADVANCED_FACE('',(#762),#4355,.T.);
#4538=ADVANCED_FACE('',(#763),#4356,.T.);
#4539=ADVANCED_FACE('',(#764),#4357,.T.);
#4540=ADVANCED_FACE('',(#765),#4358,.T.);
#4541=ADVANCED_FACE('',(#766),#4359,.T.);
#4542=ADVANCED_FACE('',(#767),#4360,.T.);
#4543=ADVANCED_FACE('',(#768),#4361,.T.);
#4544=ADVANCED_FACE('',(#769),#4362,.T.);
#4545=ADVANCED_FACE('',(#770),#4363,.T.);
#4546=ADVANCED_FACE('',(#771),#4364,.T.);
#4547=ADVANCED_FACE('',(#772),#4365,.T.);
#4548=ADVANCED_FACE('',(#773),#4366,.T.);
#4549=ADVANCED_FACE('',(#774),#4367,.T.);
#4550=ADVANCED_FACE('',(#775),#4368,.T.);
#4551=ADVANCED_FACE('',(#776),#4369,.T.);
#4552=ADVANCED_FACE('',(#777),#4370,.T.);
#4553=ADVANCED_FACE('',(#778),#4371,.T.);
#4554=ADVANCED_FACE('',(#779),#4372,.T.);
#4555=ADVANCED_FACE('',(#780),#4373,.T.);
#4556=ADVANCED_FACE('',(#781),#4374,.T.);
#4557=ADVANCED_FACE('',(#782),#4375,.T.);
#4558=ADVANCED_FACE('',(#783),#4376,.T.);
#4559=ADVANCED_FACE('',(#784),#4377,.T.);
#4560=ADVANCED_FACE('',(#785),#4378,.T.);
#4561=ADVANCED_FACE('',(#786),#4379,.T.);
#4562=ADVANCED_FACE('',(#787),#4380,.T.);
#4563=ADVANCED_FACE('',(#788),#4381,.T.);
#4564=ADVANCED_FACE('',(#789),#4382,.T.);
#4565=ADVANCED_FACE('',(#790),#4383,.T.);
#4566=ADVANCED_FACE('',(#791),#4384,.T.);
#4567=ADVANCED_FACE('',(#792),#4385,.T.);
#4568=ADVANCED_FACE('',(#793),#4386,.T.);
#4569=ADVANCED_FACE('',(#794),#47,.F.);
#4570=ADVANCED_FACE('',(#795),#48,.F.);
#4571=ADVANCED_FACE('',(#796),#610,.T.);
#4572=ADVANCED_FACE('',(#797),#611,.F.);
#4573=CLOSED_SHELL('',(#4387,#4388,#4389,#4390,#4391,#4392,#4393,#4394,
#4395,#4396,#4397,#4398,#4399,#4400,#4401,#4402,#4403,#4404,#4405,#4406,
#4407,#4408,#4409,#4410,#4411,#4412,#4413,#4414,#4415,#4416,#4417,#4418,
#4419,#4420,#4421,#4422,#4423,#4424,#4425,#4426,#4427,#4428,#4429,#4430,
#4431));
#4574=CLOSED_SHELL('',(#4432,#4433,#4434,#4435,#4436,#4437,#4438,#4439,
#4440,#4441,#4442,#4443,#4444,#4445,#4446,#4447,#4448,#4449,#4450,#4451,
#4452,#4453,#4454,#4455,#4456,#4457,#4458,#4459,#4460,#4461,#4462,#4463,
#4464,#4465,#4466,#4467,#4468,#4469,#4470,#4471,#4472,#4473,#4474));
#4575=CLOSED_SHELL('',(#4475,#4476,#4477,#4478,#4479,#4480,#4481,#4482));
#4576=CLOSED_SHELL('',(#4483,#4484,#4485,#4486,#4487,#4488,#4489,#4490,
#4491,#4492,#4493,#4494,#4495,#4496,#4497,#4498,#4499,#4500,#4501,#4502,
#4503,#4504,#4505,#4506,#4507,#4508,#4509,#4510,#4511,#4512,#4513,#4514,
#4515,#4516,#4517,#4518,#4519,#4520,#4521,#4522,#4523,#4524,#4525,#4526,
#4527,#4528,#4529,#4530,#4531,#4532,#4533,#4534,#4535,#4536,#4537,#4538,
#4539,#4540,#4541,#4542,#4543,#4544,#4545,#4546,#4547,#4548,#4549,#4550,
#4551,#4552,#4553,#4554,#4555,#4556,#4557,#4558,#4559,#4560,#4561,#4562,
#4563,#4564,#4565,#4566,#4567,#4568,#4569,#4570,#4571,#4572));
#4577=DERIVED_UNIT_ELEMENT(#4585,1.);
#4578=DERIVED_UNIT_ELEMENT(#74105,-3.);
#4579=DERIVED_UNIT_ELEMENT(#4585,1.);
#4580=DERIVED_UNIT_ELEMENT(#74105,-3.);
#4581=DERIVED_UNIT_ELEMENT(#4585,1.);
#4582=DERIVED_UNIT_ELEMENT(#74105,-3.);
#4583=DERIVED_UNIT_ELEMENT(#4585,1.);
#4584=DERIVED_UNIT_ELEMENT(#74105,-3.);
#4585=(
MASS_UNIT()
NAMED_UNIT(*)
SI_UNIT(.KILO.,.GRAM.)
);
#4586=DERIVED_UNIT((#4577,#4578));
#4587=DERIVED_UNIT((#4579,#4580));
#4588=DERIVED_UNIT((#4581,#4582));
#4589=DERIVED_UNIT((#4583,#4584));
#4590=MEASURE_REPRESENTATION_ITEM('density measure',
POSITIVE_RATIO_MEASURE(7850.),#4586);
#4591=MEASURE_REPRESENTATION_ITEM('density measure',
POSITIVE_RATIO_MEASURE(7850.),#4587);
#4592=MEASURE_REPRESENTATION_ITEM('density measure',
POSITIVE_RATIO_MEASURE(7850.),#4588);
#4593=MEASURE_REPRESENTATION_ITEM('density measure',
POSITIVE_RATIO_MEASURE(7850.),#4589);
#4594=PROPERTY_DEFINITION_REPRESENTATION(#4614,#4602);
#4595=PROPERTY_DEFINITION_REPRESENTATION(#4615,#4603);
#4596=PROPERTY_DEFINITION_REPRESENTATION(#4616,#4604);
#4597=PROPERTY_DEFINITION_REPRESENTATION(#4617,#4605);
#4598=PROPERTY_DEFINITION_REPRESENTATION(#4618,#4606);
#4599=PROPERTY_DEFINITION_REPRESENTATION(#4619,#4607);
#4600=PROPERTY_DEFINITION_REPRESENTATION(#4620,#4608);
#4601=PROPERTY_DEFINITION_REPRESENTATION(#4621,#4609);
#4602=REPRESENTATION('material name',(#4610),#74099);
#4603=REPRESENTATION('density',(#4590),#74099);
#4604=REPRESENTATION('material name',(#4611),#74100);
#4605=REPRESENTATION('density',(#4591),#74100);
#4606=REPRESENTATION('material name',(#4612),#74101);
#4607=REPRESENTATION('density',(#4592),#74101);
#4608=REPRESENTATION('material name',(#4613),#74102);
#4609=REPRESENTATION('density',(#4593),#74102);
#4610=DESCRIPTIVE_REPRESENTATION_ITEM('Steel','Steel');
#4611=DESCRIPTIVE_REPRESENTATION_ITEM('Steel','Steel');
#4612=DESCRIPTIVE_REPRESENTATION_ITEM('Steel','Steel');
#4613=DESCRIPTIVE_REPRESENTATION_ITEM('Steel','Steel');
#4614=PROPERTY_DEFINITION('material property','material name',#74134);
#4615=PROPERTY_DEFINITION('material property','density of part',#74134);
#4616=PROPERTY_DEFINITION('material property','material name',#74135);
#4617=PROPERTY_DEFINITION('material property','density of part',#74135);
#4618=PROPERTY_DEFINITION('material property','material name',#74136);
#4619=PROPERTY_DEFINITION('material property','density of part',#74136);
#4620=PROPERTY_DEFINITION('material property','material name',#74137);
#4621=PROPERTY_DEFINITION('material property','density of part',#74137);
#4622=AXIS2_PLACEMENT_3D('',#5775,#4947,#4948);
#4623=AXIS2_PLACEMENT_3D('',#5776,#4949,#4950);
#4624=AXIS2_PLACEMENT_3D('',#5777,#4951,#4952);
#4625=AXIS2_PLACEMENT_3D('',#5779,#4953,#4954);
#4626=AXIS2_PLACEMENT_3D('',#5782,#4956,#4957);
#4627=AXIS2_PLACEMENT_3D('',#5783,#4958,#4959);
#4628=AXIS2_PLACEMENT_3D('',#5785,#4960,#4961);
#4629=AXIS2_PLACEMENT_3D('',#5786,#4962,#4963);
#4630=AXIS2_PLACEMENT_3D('',#5788,#4964,#4965);
#4631=AXIS2_PLACEMENT_3D('',#5789,#4966,#4967);
#4632=AXIS2_PLACEMENT_3D('',#5792,#4968,#4969);
#4633=AXIS2_PLACEMENT_3D('',#5793,#4970,#4971);
#4634=AXIS2_PLACEMENT_3D('',#5795,#4973,#4974);
#4635=AXIS2_PLACEMENT_3D('',#5800,#4976,#4977);
#4636=AXIS2_PLACEMENT_3D('',#5803,#4979,#4980);
#4637=AXIS2_PLACEMENT_3D('',#5804,#4981,#4982);
#4638=AXIS2_PLACEMENT_3D('',#5808,#4984,#4985);
#4639=AXIS2_PLACEMENT_3D('',#5810,#4987,#4988);
#4640=AXIS2_PLACEMENT_3D('',#5814,#4990,#4991);
#4641=AXIS2_PLACEMENT_3D('',#5816,#4993,#4994);
#4642=AXIS2_PLACEMENT_3D('',#5821,#4996,#4997);
#4643=AXIS2_PLACEMENT_3D('',#5824,#4999,#5000);
#4644=AXIS2_PLACEMENT_3D('',#5825,#5001,#5002);
#4645=AXIS2_PLACEMENT_3D('',#5830,#5005,#5006);
#4646=AXIS2_PLACEMENT_3D('',#5831,#5007,#5008);
#4647=AXIS2_PLACEMENT_3D('',#5834,#5011,#5012);
#4648=AXIS2_PLACEMENT_3D('',#5839,#5015,#5016);
#4649=AXIS2_PLACEMENT_3D('',#5840,#5017,#5018);
#4650=AXIS2_PLACEMENT_3D('',#5843,#5021,#5022);
#4651=AXIS2_PLACEMENT_3D('',#5849,#5026,#5027);
#4652=AXIS2_PLACEMENT_3D('',#5853,#5030,#5031);
#4653=AXIS2_PLACEMENT_3D('',#5857,#5034,#5035);
#4654=AXIS2_PLACEMENT_3D('',#5861,#5038,#5039);
#4655=AXIS2_PLACEMENT_3D('',#5863,#5040,#5041);
#4656=AXIS2_PLACEMENT_3D('',#5865,#5042,#5043);
#4657=AXIS2_PLACEMENT_3D('',#5867,#5044,#5045);
#4658=AXIS2_PLACEMENT_3D('',#5869,#5046,#5047);
#4659=AXIS2_PLACEMENT_3D('',#5871,#5048,#5049);
#4660=AXIS2_PLACEMENT_3D('',#5872,#5050,#5051);
#4661=AXIS2_PLACEMENT_3D('',#5875,#5052,#5053);
#4662=AXIS2_PLACEMENT_3D('',#5876,#5054,#5055);
#4663=AXIS2_PLACEMENT_3D('',#5877,#5056,#5057);
#4664=AXIS2_PLACEMENT_3D('',#5878,#5058,#5059);
#4665=AXIS2_PLACEMENT_3D('',#5882,#5061,#5062);
#4666=AXIS2_PLACEMENT_3D('',#5883,#5063,#5064);
#4667=AXIS2_PLACEMENT_3D('',#5884,#5065,#5066);
#4668=AXIS2_PLACEMENT_3D('',#5887,#5067,#5068);
#4669=AXIS2_PLACEMENT_3D('',#5888,#5069,#5070);
#4670=AXIS2_PLACEMENT_3D('',#5889,#5071,#5072);
#4671=AXIS2_PLACEMENT_3D('',#5890,#5073,#5074);
#4672=AXIS2_PLACEMENT_3D('',#5894,#5076,#5077);
#4673=AXIS2_PLACEMENT_3D('',#5895,#5078,#5079);
#4674=AXIS2_PLACEMENT_3D('',#5896,#5080,#5081);
#4675=AXIS2_PLACEMENT_3D('',#5899,#5082,#5083);
#4676=AXIS2_PLACEMENT_3D('',#5900,#5084,#5085);
#4677=AXIS2_PLACEMENT_3D('',#5901,#5086,#5087);
#4678=AXIS2_PLACEMENT_3D('',#5902,#5088,#5089);
#4679=AXIS2_PLACEMENT_3D('',#5906,#5091,#5092);
#4680=AXIS2_PLACEMENT_3D('',#5907,#5093,#5094);
#4681=AXIS2_PLACEMENT_3D('',#5908,#5095,#5096);
#4682=AXIS2_PLACEMENT_3D('',#5909,#5097,#5098);
#4683=AXIS2_PLACEMENT_3D('',#5910,#5099,#5100);
#4684=AXIS2_PLACEMENT_3D('',#5914,#5102,#5103);
#4685=AXIS2_PLACEMENT_3D('',#5915,#5104,#5105);
#4686=AXIS2_PLACEMENT_3D('',#5916,#5106,#5107);
#4687=AXIS2_PLACEMENT_3D('',#5919,#5108,#5109);
#4688=AXIS2_PLACEMENT_3D('',#5920,#5110,#5111);
#4689=AXIS2_PLACEMENT_3D('',#5921,#5112,#5113);
#4690=AXIS2_PLACEMENT_3D('',#5922,#5114,#5115);
#4691=AXIS2_PLACEMENT_3D('',#5926,#5117,#5118);
#4692=AXIS2_PLACEMENT_3D('',#5927,#5119,#5120);
#4693=AXIS2_PLACEMENT_3D('',#5928,#5121,#5122);
#4694=AXIS2_PLACEMENT_3D('',#5933,#5124,#5125);
#4695=AXIS2_PLACEMENT_3D('',#5935,#5127,#5128);
#4696=AXIS2_PLACEMENT_3D('',#5936,#5129,#5130);
#4697=AXIS2_PLACEMENT_3D('',#5940,#5132,#5133);
#4698=AXIS2_PLACEMENT_3D('',#5942,#5135,#5136);
#4699=AXIS2_PLACEMENT_3D('',#5946,#5138,#5139);
#4700=AXIS2_PLACEMENT_3D('',#5948,#5141,#5142);
#4701=AXIS2_PLACEMENT_3D('',#5951,#5144,#5145);
#4702=AXIS2_PLACEMENT_3D('',#5953,#5147,#5148);
#4703=AXIS2_PLACEMENT_3D('',#5956,#5150,#5151);
#4704=AXIS2_PLACEMENT_3D('',#5957,#5152,#5153);
#4705=AXIS2_PLACEMENT_3D('',#5960,#5155,#5156);
#4706=AXIS2_PLACEMENT_3D('',#5961,#5157,#5158);
#4707=AXIS2_PLACEMENT_3D('',#5964,#5160,#5161);
#4708=AXIS2_PLACEMENT_3D('',#5965,#5162,#5163);
#4709=AXIS2_PLACEMENT_3D('',#5967,#5165,#5166);
#4710=AXIS2_PLACEMENT_3D('',#5969,#5168,#5169);
#4711=AXIS2_PLACEMENT_3D('',#5971,#5170,#5171);
#4712=AXIS2_PLACEMENT_3D('',#5973,#5172,#5173);
#4713=AXIS2_PLACEMENT_3D('',#5975,#5174,#5175);
#4714=AXIS2_PLACEMENT_3D('',#5977,#5176,#5177);
#4715=AXIS2_PLACEMENT_3D('',#5979,#5178,#5179);
#4716=AXIS2_PLACEMENT_3D('',#5980,#5180,#5181);
#4717=AXIS2_PLACEMENT_3D('',#5981,#5182,#5183);
#4718=AXIS2_PLACEMENT_3D('',#5982,#5184,#5185);
#4719=AXIS2_PLACEMENT_3D('',#5983,#5186,#5187);
#4720=AXIS2_PLACEMENT_3D('',#5984,#5188,#5189);
#4721=AXIS2_PLACEMENT_3D('',#5985,#5190,#5191);
#4722=AXIS2_PLACEMENT_3D('',#5986,#5192,#5193);
#4723=AXIS2_PLACEMENT_3D('',#5987,#5194,#5195);
#4724=AXIS2_PLACEMENT_3D('',#5988,#5196,#5197);
#4725=AXIS2_PLACEMENT_3D('',#5989,#5198,#5199);
#4726=AXIS2_PLACEMENT_3D('',#5990,#5200,#5201);
#4727=AXIS2_PLACEMENT_3D('',#5992,#5203,#5204);
#4728=AXIS2_PLACEMENT_3D('',#5994,#5206,#5207);
#4729=AXIS2_PLACEMENT_3D('',#5995,#5208,#5209);
#4730=AXIS2_PLACEMENT_3D('',#5996,#5210,#5211);
#4731=AXIS2_PLACEMENT_3D('',#5998,#5212,#5213);
#4732=AXIS2_PLACEMENT_3D('',#6000,#5214,#5215);
#4733=AXIS2_PLACEMENT_3D('',#6001,#5216,#5217);
#4734=AXIS2_PLACEMENT_3D('',#6003,#5218,#5219);
#4735=AXIS2_PLACEMENT_3D('',#6005,#5220,#5221);
#4736=AXIS2_PLACEMENT_3D('',#6006,#5222,#5223);
#4737=AXIS2_PLACEMENT_3D('',#6008,#5224,#5225);
#4738=AXIS2_PLACEMENT_3D('',#6010,#5226,#5227);
#4739=AXIS2_PLACEMENT_3D('',#6011,#5228,#5229);
#4740=AXIS2_PLACEMENT_3D('',#6012,#5230,#5231);
#4741=AXIS2_PLACEMENT_3D('',#6030,#5240,#5241);
#4742=AXIS2_PLACEMENT_3D('',#6032,#5242,#5243);
#4743=AXIS2_PLACEMENT_3D('',#6034,#5244,#5245);
#4744=AXIS2_PLACEMENT_3D('',#6036,#5246,#5247);
#4745=AXIS2_PLACEMENT_3D('',#6037,#5248,#5249);
#4746=AXIS2_PLACEMENT_3D('',#6040,#5251,#5252);
#4747=AXIS2_PLACEMENT_3D('',#6041,#5253,#5254);
#4748=AXIS2_PLACEMENT_3D('',#6043,#5255,#5256);
#4749=AXIS2_PLACEMENT_3D('',#6044,#5257,#5258);
#4750=AXIS2_PLACEMENT_3D('',#6045,#5259,#5260);
#4751=AXIS2_PLACEMENT_3D('',#6049,#5262,#5263);
#4752=AXIS2_PLACEMENT_3D('',#6050,#5264,#5265);
#4753=AXIS2_PLACEMENT_3D('',#6051,#5266,#5267);
#4754=AXIS2_PLACEMENT_3D('',#6053,#5268,#5269);
#4755=AXIS2_PLACEMENT_3D('',#6054,#5270,#5271);
#4756=AXIS2_PLACEMENT_3D('',#6055,#5272,#5273);
#4757=AXIS2_PLACEMENT_3D('',#6059,#5275,#5276);
#4758=AXIS2_PLACEMENT_3D('',#6060,#5277,#5278);
#4759=AXIS2_PLACEMENT_3D('',#6061,#5279,#5280);
#4760=AXIS2_PLACEMENT_3D('',#6062,#5281,#5282);
#4761=AXIS2_PLACEMENT_3D('',#6063,#5283,#5284);
#4762=AXIS2_PLACEMENT_3D('',#6065,#5285,#5286);
#4763=AXIS2_PLACEMENT_3D('',#6066,#5287,#5288);
#4764=AXIS2_PLACEMENT_3D('',#6067,#5289,#5290);
#4765=AXIS2_PLACEMENT_3D('',#6071,#5292,#5293);
#4766=AXIS2_PLACEMENT_3D('',#6072,#5294,#5295);
#4767=AXIS2_PLACEMENT_3D('',#6073,#5296,#5297);
#4768=AXIS2_PLACEMENT_3D('',#6075,#5298,#5299);
#4769=AXIS2_PLACEMENT_3D('',#6078,#5301,#5302);
#4770=AXIS2_PLACEMENT_3D('',#6079,#5303,#5304);
#4771=AXIS2_PLACEMENT_3D('',#6081,#5305,#5306);
#4772=AXIS2_PLACEMENT_3D('',#6083,#5308,#5309);
#4773=AXIS2_PLACEMENT_3D('',#6085,#5310,#5311);
#4774=AXIS2_PLACEMENT_3D('',#6087,#5313,#5314);
#4775=AXIS2_PLACEMENT_3D('',#6089,#5315,#5316);
#4776=AXIS2_PLACEMENT_3D('',#6092,#5318,#5319);
#4777=AXIS2_PLACEMENT_3D('',#6093,#5320,#5321);
#4778=AXIS2_PLACEMENT_3D('',#6096,#5323,#5324);
#4779=AXIS2_PLACEMENT_3D('',#6097,#5325,#5326);
#4780=AXIS2_PLACEMENT_3D('',#6099,#5328,#5329);
#4781=AXIS2_PLACEMENT_3D('',#6102,#5331,#5332);
#4782=AXIS2_PLACEMENT_3D('',#6103,#5333,#5334);
#4783=AXIS2_PLACEMENT_3D('',#6105,#5336,#5337);
#4784=AXIS2_PLACEMENT_3D('',#6111,#5341,#5342);
#4785=AXIS2_PLACEMENT_3D('',#6115,#5345,#5346);
#4786=AXIS2_PLACEMENT_3D('',#6119,#5349,#5350);
#4787=AXIS2_PLACEMENT_3D('',#6123,#5353,#5354);
#4788=AXIS2_PLACEMENT_3D('',#6129,#5358,#5359);
#4789=AXIS2_PLACEMENT_3D('',#6131,#5361,#5362);
#4790=AXIS2_PLACEMENT_3D('',#6135,#5365,#5366);
#4791=AXIS2_PLACEMENT_3D('',#6137,#5368,#5369);
#4792=AXIS2_PLACEMENT_3D('',#6139,#5370,#5371);
#4793=AXIS2_PLACEMENT_3D('',#6140,#5372,#5373);
#4794=AXIS2_PLACEMENT_3D('',#6141,#5374,#5375);
#4795=AXIS2_PLACEMENT_3D('',#6159,#5384,#5385);
#4796=AXIS2_PLACEMENT_3D('',#6161,#5386,#5387);
#4797=AXIS2_PLACEMENT_3D('',#6163,#5388,#5389);
#4798=AXIS2_PLACEMENT_3D('',#6165,#5390,#5391);
#4799=AXIS2_PLACEMENT_3D('',#6166,#5392,#5393);
#4800=AXIS2_PLACEMENT_3D('',#6167,#5394,#5395);
#4801=AXIS2_PLACEMENT_3D('',#6168,#5396,#5397);
#4802=AXIS2_PLACEMENT_3D('',#6169,#5398,#5399);
#4803=AXIS2_PLACEMENT_3D('',#6170,#5400,#5401);
#4804=AXIS2_PLACEMENT_3D('',#6171,#5402,#5403);
#4805=AXIS2_PLACEMENT_3D('',#6172,#5404,#5405);
#4806=AXIS2_PLACEMENT_3D('',#6173,#5406,#5407);
#4807=AXIS2_PLACEMENT_3D('',#6174,#5408,#5409);
#4808=AXIS2_PLACEMENT_3D('',#6175,#5410,#5411);
#4809=AXIS2_PLACEMENT_3D('',#6176,#5412,#5413);
#4810=AXIS2_PLACEMENT_3D('',#6177,#5414,#5415);
#4811=AXIS2_PLACEMENT_3D('',#6178,#5416,#5417);
#4812=AXIS2_PLACEMENT_3D('',#6179,#5418,#5419);
#4813=AXIS2_PLACEMENT_3D('',#6180,#5420,#5421);
#4814=AXIS2_PLACEMENT_3D('',#6181,#5422,#5423);
#4815=AXIS2_PLACEMENT_3D('',#6182,#5424,#5425);
#4816=AXIS2_PLACEMENT_3D('',#6183,#5426,#5427);
#4817=AXIS2_PLACEMENT_3D('',#6184,#5428,#5429);
#4818=AXIS2_PLACEMENT_3D('',#6185,#5430,#5431);
#4819=AXIS2_PLACEMENT_3D('',#6186,#5432,#5433);
#4820=AXIS2_PLACEMENT_3D('',#6187,#5434,#5435);
#4821=AXIS2_PLACEMENT_3D('',#6188,#5436,#5437);
#4822=AXIS2_PLACEMENT_3D('',#6189,#5438,#5439);
#4823=AXIS2_PLACEMENT_3D('',#6190,#5440,#5441);
#4824=AXIS2_PLACEMENT_3D('',#6192,#5443,#5444);
#4825=AXIS2_PLACEMENT_3D('',#6193,#5445,#5446);
#4826=AXIS2_PLACEMENT_3D('',#6195,#5447,#5448);
#4827=AXIS2_PLACEMENT_3D('',#6198,#5450,#5451);
#4828=AXIS2_PLACEMENT_3D('',#6199,#5452,#5453);
#4829=AXIS2_PLACEMENT_3D('',#6201,#5454,#5455);
#4830=AXIS2_PLACEMENT_3D('',#6202,#5456,#5457);
#4831=AXIS2_PLACEMENT_3D('',#6203,#5458,#5459);
#4832=AXIS2_PLACEMENT_3D('',#6205,#5460,#5461);
#4833=AXIS2_PLACEMENT_3D('',#6206,#5462,#5463);
#4834=AXIS2_PLACEMENT_3D('',#6208,#5464,#5465);
#4835=AXIS2_PLACEMENT_3D('',#6209,#5466,#5467);
#4836=AXIS2_PLACEMENT_3D('',#6210,#5468,#5469);
#4837=AXIS2_PLACEMENT_3D('',#6212,#5470,#5471);
#4838=AXIS2_PLACEMENT_3D('',#6214,#5473,#5474);
#4839=AXIS2_PLACEMENT_3D('',#6216,#5475,#5476);
#4840=AXIS2_PLACEMENT_3D('',#6217,#5477,#5478);
#4841=AXIS2_PLACEMENT_3D('',#6218,#5479,#5480);
#4842=AXIS2_PLACEMENT_3D('',#6220,#5481,#5482);
#4843=AXIS2_PLACEMENT_3D('',#6221,#5483,#5484);
#4844=AXIS2_PLACEMENT_3D('',#6222,#5485,#5486);
#4845=AXIS2_PLACEMENT_3D('',#6223,#5487,#5488);
#4846=AXIS2_PLACEMENT_3D('',#6224,#5489,#5490);
#4847=AXIS2_PLACEMENT_3D('',#6342,#5492,#5493);
#4848=AXIS2_PLACEMENT_3D('',#6413,#5494,#5495);
#4849=AXIS2_PLACEMENT_3D('',#6986,#5497,#5498);
#4850=AXIS2_PLACEMENT_3D('',#7564,#5500,#5501);
#4851=AXIS2_PLACEMENT_3D('',#8156,#5503,#5504);
#4852=AXIS2_PLACEMENT_3D('',#8708,#5506,#5507);
#4853=AXIS2_PLACEMENT_3D('',#9316,#5509,#5510);
#4854=AXIS2_PLACEMENT_3D('',#9898,#5512,#5513);
#4855=AXIS2_PLACEMENT_3D('',#10514,#5515,#5516);
#4856=AXIS2_PLACEMENT_3D('',#11060,#5518,#5519);
#4857=AXIS2_PLACEMENT_3D('',#11694,#5521,#5522);
#4858=AXIS2_PLACEMENT_3D('',#12258,#5524,#5525);
#4859=AXIS2_PLACEMENT_3D('',#12872,#5527,#5528);
#4860=AXIS2_PLACEMENT_3D('',#13436,#5530,#5531);
#4861=AXIS2_PLACEMENT_3D('',#14044,#5533,#5534);
#4862=AXIS2_PLACEMENT_3D('',#14612,#5536,#5537);
#4863=AXIS2_PLACEMENT_3D('',#15204,#5539,#5540);
#4864=AXIS2_PLACEMENT_3D('',#15795,#5542,#5543);
#4865=AXIS2_PLACEMENT_3D('',#16426,#5545,#5546);
#4866=AXIS2_PLACEMENT_3D('',#17067,#5548,#5549);
#4867=AXIS2_PLACEMENT_3D('',#17610,#5551,#5552);
#4868=AXIS2_PLACEMENT_3D('',#18321,#5554,#5555);
#4869=AXIS2_PLACEMENT_3D('',#18926,#5557,#5558);
#4870=AXIS2_PLACEMENT_3D('',#19649,#5560,#5561);
#4871=AXIS2_PLACEMENT_3D('',#20216,#5563,#5564);
#4872=AXIS2_PLACEMENT_3D('',#20833,#5566,#5567);
#4873=AXIS2_PLACEMENT_3D('',#21420,#5569,#5570);
#4874=AXIS2_PLACEMENT_3D('',#22023,#5572,#5573);
#4875=AXIS2_PLACEMENT_3D('',#22616,#5575,#5576);
#4876=AXIS2_PLACEMENT_3D('',#23219,#5578,#5579);
#4877=AXIS2_PLACEMENT_3D('',#23824,#5581,#5582);
#4878=AXIS2_PLACEMENT_3D('',#24389,#5584,#5585);
#4879=AXIS2_PLACEMENT_3D('',#24964,#5587,#5588);
#4880=AXIS2_PLACEMENT_3D('',#25557,#5590,#5591);
#4881=AXIS2_PLACEMENT_3D('',#26108,#5593,#5594);
#4882=AXIS2_PLACEMENT_3D('',#26697,#5596,#5597);
#4883=AXIS2_PLACEMENT_3D('',#27308,#5599,#5600);
#4884=AXIS2_PLACEMENT_3D('',#27899,#5602,#5603);
#4885=AXIS2_PLACEMENT_3D('',#28485,#5605,#5606);
#4886=AXIS2_PLACEMENT_3D('',#29133,#5608,#5609);
#4887=AXIS2_PLACEMENT_3D('',#29641,#5611,#5612);
#4888=AXIS2_PLACEMENT_3D('',#30199,#5614,#5615);
#4889=AXIS2_PLACEMENT_3D('',#30810,#5617,#5618);
#4890=AXIS2_PLACEMENT_3D('',#31389,#5620,#5621);
#4891=AXIS2_PLACEMENT_3D('',#31942,#5623,#5624);
#4892=AXIS2_PLACEMENT_3D('',#32460,#5626,#5627);
#4893=AXIS2_PLACEMENT_3D('',#32987,#5629,#5630);
#4894=AXIS2_PLACEMENT_3D('',#33612,#5632,#5633);
#4895=AXIS2_PLACEMENT_3D('',#34193,#5635,#5636);
#4896=AXIS2_PLACEMENT_3D('',#34860,#5638,#5639);
#4897=AXIS2_PLACEMENT_3D('',#35393,#5641,#5642);
#4898=AXIS2_PLACEMENT_3D('',#35883,#5644,#5645);
#4899=AXIS2_PLACEMENT_3D('',#36442,#5647,#5648);
#4900=AXIS2_PLACEMENT_3D('',#37029,#5650,#5651);
#4901=AXIS2_PLACEMENT_3D('',#37619,#5653,#5654);
#4902=AXIS2_PLACEMENT_3D('',#38169,#5656,#5657);
#4903=AXIS2_PLACEMENT_3D('',#38697,#5659,#5660);
#4904=AXIS2_PLACEMENT_3D('',#39226,#5662,#5663);
#4905=AXIS2_PLACEMENT_3D('',#39813,#5665,#5666);
#4906=AXIS2_PLACEMENT_3D('',#40422,#5668,#5669);
#4907=AXIS2_PLACEMENT_3D('',#41059,#5671,#5672);
#4908=AXIS2_PLACEMENT_3D('',#41666,#5674,#5675);
#4909=AXIS2_PLACEMENT_3D('',#42259,#5677,#5678);
#4910=AXIS2_PLACEMENT_3D('',#42850,#5680,#5681);
#4911=AXIS2_PLACEMENT_3D('',#43453,#5683,#5684);
#4912=AXIS2_PLACEMENT_3D('',#44108,#5686,#5687);
#4913=AXIS2_PLACEMENT_3D('',#44753,#5689,#5690);
#4914=AXIS2_PLACEMENT_3D('',#45366,#5692,#5693);
#4915=AXIS2_PLACEMENT_3D('',#45949,#5695,#5696);
#4916=AXIS2_PLACEMENT_3D('',#46574,#5698,#5699);
#4917=AXIS2_PLACEMENT_3D('',#47129,#5701,#5702);
#4918=AXIS2_PLACEMENT_3D('',#47507,#5704,#5705);
#4919=AXIS2_PLACEMENT_3D('',#48014,#5707,#5708);
#4920=AXIS2_PLACEMENT_3D('',#48577,#5710,#5711);
#4921=AXIS2_PLACEMENT_3D('',#48938,#5713,#5714);
#4922=AXIS2_PLACEMENT_3D('',#49467,#5716,#5717);
#4923=AXIS2_PLACEMENT_3D('',#50060,#5719,#5720);
#4924=AXIS2_PLACEMENT_3D('',#50639,#5722,#5723);
#4925=AXIS2_PLACEMENT_3D('',#51208,#5725,#5726);
#4926=AXIS2_PLACEMENT_3D('',#51831,#5728,#5729);
#4927=AXIS2_PLACEMENT_3D('',#52430,#5731,#5732);
#4928=AXIS2_PLACEMENT_3D('',#52949,#5734,#5735);
#4929=AXIS2_PLACEMENT_3D('',#53535,#5737,#5738);
#4930=AXIS2_PLACEMENT_3D('',#54123,#5740,#5741);
#4931=AXIS2_PLACEMENT_3D('',#54675,#5743,#5744);
#4932=AXIS2_PLACEMENT_3D('',#54752,#5745,#5746);
#4933=AXIS2_PLACEMENT_3D('',#61716,#5747,#5748);
#4934=AXIS2_PLACEMENT_3D('',#69150,#5749,#5750);
#4935=AXIS2_PLACEMENT_3D('',#69327,#5751,#5752);
#4936=AXIS2_PLACEMENT_3D('',#74081,#5753,#5754);
#4937=AXIS2_PLACEMENT_3D('',#74082,#5755,#5756);
#4938=AXIS2_PLACEMENT_3D('',#74083,#5757,#5758);
#4939=AXIS2_PLACEMENT_3D('',#74084,#5759,#5760);
#4940=AXIS2_PLACEMENT_3D('',#74085,#5761,#5762);
#4941=AXIS2_PLACEMENT_3D('',#74086,#5763,#5764);
#4942=AXIS2_PLACEMENT_3D('',#74087,#5765,#5766);
#4943=AXIS2_PLACEMENT_3D('',#74088,#5767,#5768);
#4944=AXIS2_PLACEMENT_3D('',#74089,#5769,#5770);
#4945=AXIS2_PLACEMENT_3D('',#74090,#5771,#5772);
#4946=AXIS2_PLACEMENT_3D('',#74091,#5773,#5774);
#4947=DIRECTION('axis',(0.,0.,1.));
#4948=DIRECTION('refdir',(1.,0.,0.));
#4949=DIRECTION('axis',(0.,0.,1.));
#4950=DIRECTION('refdir',(1.,0.,0.));
#4951=DIRECTION('center_axis',(0.,0.,1.));
#4952=DIRECTION('ref_axis',(1.,0.,0.));
#4953=DIRECTION('center_axis',(0.,0.,1.));
#4954=DIRECTION('ref_axis',(1.,0.,0.));
#4955=DIRECTION('',(0.,0.,1.));
#4956=DIRECTION('center_axis',(0.,0.,1.));
#4957=DIRECTION('ref_axis',(1.,0.,0.));
#4958=DIRECTION('center_axis',(0.,0.,1.));
#4959=DIRECTION('ref_axis',(1.,0.,0.));
#4960=DIRECTION('center_axis',(0.,0.,-1.));
#4961=DIRECTION('ref_axis',(1.,0.,0.));
#4962=DIRECTION('center_axis',(0.,0.,-1.));
#4963=DIRECTION('ref_axis',(-1.,0.,0.));
#4964=DIRECTION('center_axis',(0.,0.,1.));
#4965=DIRECTION('ref_axis',(1.,0.,0.));
#4966=DIRECTION('center_axis',(0.,0.,1.));
#4967=DIRECTION('ref_axis',(1.,0.,0.));
#4968=DIRECTION('center_axis',(0.,0.,1.));
#4969=DIRECTION('ref_axis',(1.,0.,0.));
#4970=DIRECTION('center_axis',(0.,0.,1.));
#4971=DIRECTION('ref_axis',(1.,0.,0.));
#4972=DIRECTION('',(0.,0.,1.));
#4973=DIRECTION('center_axis',(1.,0.,0.));
#4974=DIRECTION('ref_axis',(0.,0.707106781186546,-0.707106781186549));
#4975=DIRECTION('',(-1.,0.,0.));
#4976=DIRECTION('center_axis',(0.923879532511283,0.382683432365099,3.39891166203453E-15));
#4977=DIRECTION('ref_axis',(-0.382683432365099,0.923879532511283,8.20569863179162E-15));
#4978=DIRECTION('',(1.,0.,0.));
#4979=DIRECTION('center_axis',(0.923879532511286,-0.382683432365092,0.));
#4980=DIRECTION('ref_axis',(0.382683432365092,0.923879532511286,0.));
#4981=DIRECTION('center_axis',(0.707106781186548,0.707106781186548,0.));
#4982=DIRECTION('ref_axis',(-0.5,0.5,-0.707106781186548));
#4983=DIRECTION('',(-0.707106781186547,-0.707106781186547,0.));
#4984=DIRECTION('center_axis',(0.382683432365092,0.923879532511286,0.));
#4985=DIRECTION('ref_axis',(-0.923879532511286,0.382683432365092,0.));
#4986=DIRECTION('',(0.707106781186547,0.707106781186547,0.));
#4987=DIRECTION('center_axis',(0.,1.,0.));
#4988=DIRECTION('ref_axis',(-0.707106781186546,0.,-0.707106781186549));
#4989=DIRECTION('',(0.,-1.,0.));
#4990=DIRECTION('center_axis',(-0.382683432365099,0.923879532511283,3.39891166203453E-15));
#4991=DIRECTION('ref_axis',(-0.923879532511283,-0.382683432365099,8.20569863179162E-15));
#4992=DIRECTION('',(0.,1.,0.));
#4993=DIRECTION('center_axis',(-1.,0.,0.));
#4994=DIRECTION('ref_axis',(0.,-0.707106781186546,-0.707106781186549));
#4995=DIRECTION('',(1.,0.,0.));
#4996=DIRECTION('center_axis',(-0.923879532511283,-0.382683432365099,3.39891166203453E-15));
#4997=DIRECTION('ref_axis',(0.382683432365099,-0.923879532511283,8.20569863179162E-15));
#4998=DIRECTION('',(-1.,0.,0.));
#4999=DIRECTION('center_axis',(0.923879532511286,-0.382683432365092,0.));
#5000=DIRECTION('ref_axis',(0.382683432365092,0.923879532511286,0.));
#5001=DIRECTION('center_axis',(-0.707106781186548,-0.707106781186548,0.));
#5002=DIRECTION('ref_axis',(0.5,-0.5,-0.707106781186548));
#5003=DIRECTION('',(-0.707106781186547,-0.707106781186547,0.));
#5004=DIRECTION('',(0.707106781186547,0.707106781186547,0.));
#5005=DIRECTION('center_axis',(-0.382683432365092,-0.923879532511286,0.));
#5006=DIRECTION('ref_axis',(0.923879532511286,-0.382683432365092,0.));
#5007=DIRECTION('center_axis',(-0.707106781186548,0.707106781186548,0.));
#5008=DIRECTION('ref_axis',(-0.5,-0.5,-0.707106781186548));
#5009=DIRECTION('',(0.707106781186547,-0.707106781186547,0.));
#5010=DIRECTION('',(-0.707106781186547,0.707106781186547,0.));
#5011=DIRECTION('center_axis',(0.,-1.,0.));
#5012=DIRECTION('ref_axis',(0.707106781186546,0.,-0.707106781186549));
#5013=DIRECTION('',(0.,-1.,0.));
#5014=DIRECTION('',(0.,1.,0.));
#5015=DIRECTION('center_axis',(0.382683432365099,-0.923879532511283,3.39891166203453E-15));
#5016=DIRECTION('ref_axis',(0.923879532511283,0.382683432365099,8.20569863179162E-15));
#5017=DIRECTION('center_axis',(0.707106781186548,-0.707106781186548,0.));
#5018=DIRECTION('ref_axis',(0.5,0.5,-0.707106781186548));
#5019=DIRECTION('',(0.707106781186547,-0.707106781186547,0.));
#5020=DIRECTION('',(-0.707106781186547,0.707106781186547,0.));
#5021=DIRECTION('center_axis',(-0.707106781186548,0.707106781186548,0.));
#5022=DIRECTION('ref_axis',(-0.707106781186548,-0.707106781186548,0.));
#5023=DIRECTION('',(0.,0.,1.));
#5024=DIRECTION('',(-0.707106781186547,-0.707106781186547,0.));
#5025=DIRECTION('',(0.,0.,1.));
#5026=DIRECTION('center_axis',(-1.,0.,0.));
#5027=DIRECTION('ref_axis',(0.,-1.,0.));
#5028=DIRECTION('',(0.,0.,1.));
#5029=DIRECTION('',(0.,-1.,0.));
#5030=DIRECTION('center_axis',(-0.707106781186548,-0.707106781186548,0.));
#5031=DIRECTION('ref_axis',(0.707106781186548,-0.707106781186548,0.));
#5032=DIRECTION('',(0.,0.,1.));
#5033=DIRECTION('',(0.707106781186547,-0.707106781186547,0.));
#5034=DIRECTION('center_axis',(0.,-1.,0.));
#5035=DIRECTION('ref_axis',(1.,0.,0.));
#5036=DIRECTION('',(0.,0.,1.));
#5037=DIRECTION('',(1.,0.,0.));
#5038=DIRECTION('center_axis',(0.,0.,1.));
#5039=DIRECTION('ref_axis',(1.,0.,0.));
#5040=DIRECTION('center_axis',(0.,0.,-1.));
#5041=DIRECTION('ref_axis',(1.,0.,0.));
#5042=DIRECTION('center_axis',(0.,0.,-1.));
#5043=DIRECTION('ref_axis',(1.,0.,0.));
#5044=DIRECTION('center_axis',(0.,0.,-1.));
#5045=DIRECTION('ref_axis',(1.,0.,0.));
#5046=DIRECTION('center_axis',(0.,0.,-1.));
#5047=DIRECTION('ref_axis',(1.,0.,0.));
#5048=DIRECTION('center_axis',(0.,0.,-1.));
#5049=DIRECTION('ref_axis',(1.,0.,0.));
#5050=DIRECTION('center_axis',(0.,0.,-1.));
#5051=DIRECTION('ref_axis',(-1.,0.,0.));
#5052=DIRECTION('center_axis',(0.,0.,1.));
#5053=DIRECTION('ref_axis',(1.,0.,0.));
#5054=DIRECTION('center_axis',(0.,-1.,0.));
#5055=DIRECTION('ref_axis',(1.,0.,0.));
#5056=DIRECTION('center_axis',(0.,0.,1.));
#5057=DIRECTION('ref_axis',(1.,0.,0.));
#5058=DIRECTION('center_axis',(0.,0.,1.));
#5059=DIRECTION('ref_axis',(1.,0.,0.));
#5060=DIRECTION('',(0.,0.,1.));
#5061=DIRECTION('center_axis',(0.,0.,-1.));
#5062=DIRECTION('ref_axis',(1.,0.,0.));
#5063=DIRECTION('center_axis',(0.,0.,-1.));
#5064=DIRECTION('ref_axis',(1.,0.,0.));
#5065=DIRECTION('center_axis',(0.,0.,-1.));
#5066=DIRECTION('ref_axis',(-1.,0.,0.));
#5067=DIRECTION('center_axis',(0.,0.,1.));
#5068=DIRECTION('ref_axis',(1.,0.,0.));
#5069=DIRECTION('center_axis',(0.,-1.,0.));
#5070=DIRECTION('ref_axis',(1.,0.,0.));
#5071=DIRECTION('center_axis',(0.,0.,1.));
#5072=DIRECTION('ref_axis',(1.,0.,0.));
#5073=DIRECTION('center_axis',(0.,0.,1.));
#5074=DIRECTION('ref_axis',(1.,0.,0.));
#5075=DIRECTION('',(0.,0.,1.));
#5076=DIRECTION('center_axis',(0.,0.,-1.));
#5077=DIRECTION('ref_axis',(1.,0.,0.));
#5078=DIRECTION('center_axis',(0.,0.,-1.));
#5079=DIRECTION('ref_axis',(1.,0.,0.));
#5080=DIRECTION('center_axis',(0.,0.,-1.));
#5081=DIRECTION('ref_axis',(-1.,0.,0.));
#5082=DIRECTION('center_axis',(0.,0.,1.));
#5083=DIRECTION('ref_axis',(1.,0.,0.));
#5084=DIRECTION('center_axis',(0.,-1.,0.));
#5085=DIRECTION('ref_axis',(1.,0.,0.));
#5086=DIRECTION('center_axis',(0.,0.,1.));
#5087=DIRECTION('ref_axis',(1.,0.,0.));
#5088=DIRECTION('center_axis',(0.,0.,1.));
#5089=DIRECTION('ref_axis',(1.,0.,0.));
#5090=DIRECTION('',(0.,0.,1.));
#5091=DIRECTION('center_axis',(0.,0.,-1.));
#5092=DIRECTION('ref_axis',(1.,0.,0.));
#5093=DIRECTION('center_axis',(0.,0.,-1.));
#5094=DIRECTION('ref_axis',(1.,0.,0.));
#5095=DIRECTION('center_axis',(0.,0.,-1.));
#5096=DIRECTION('ref_axis',(-1.,0.,0.));
#5097=DIRECTION('center_axis',(-1.22464679914735E-16,-1.,0.));
#5098=DIRECTION('ref_axis',(1.,-1.22464679914735E-16,0.));
#5099=DIRECTION('center_axis',(0.,0.,1.));
#5100=DIRECTION('ref_axis',(1.,0.,0.));
#5101=DIRECTION('',(0.,0.,1.));
#5102=DIRECTION('center_axis',(0.,0.,-1.));
#5103=DIRECTION('ref_axis',(1.,0.,0.));
#5104=DIRECTION('center_axis',(0.,0.,-1.));
#5105=DIRECTION('ref_axis',(1.,0.,0.));
#5106=DIRECTION('center_axis',(0.,0.,-1.));
#5107=DIRECTION('ref_axis',(-1.,0.,0.));
#5108=DIRECTION('center_axis',(0.,0.,1.));
#5109=DIRECTION('ref_axis',(1.,0.,0.));
#5110=DIRECTION('center_axis',(0.,-1.,0.));
#5111=DIRECTION('ref_axis',(1.,0.,0.));
#5112=DIRECTION('center_axis',(0.,0.,1.));
#5113=DIRECTION('ref_axis',(1.,0.,0.));
#5114=DIRECTION('center_axis',(0.,0.,1.));
#5115=DIRECTION('ref_axis',(1.,0.,0.));
#5116=DIRECTION('',(0.,0.,1.));
#5117=DIRECTION('center_axis',(0.,0.,-1.));
#5118=DIRECTION('ref_axis',(1.,0.,0.));
#5119=DIRECTION('center_axis',(0.,0.,-1.));
#5120=DIRECTION('ref_axis',(1.,0.,0.));
#5121=DIRECTION('center_axis',(-1.,0.,0.));
#5122=DIRECTION('ref_axis',(0.,0.707106781186546,0.707106781186549));
#5123=DIRECTION('',(1.,0.,0.));
#5124=DIRECTION('center_axis',(-0.923879532511286,0.382683432365092,0.));
#5125=DIRECTION('ref_axis',(0.382683432365092,0.923879532511286,0.));
#5126=DIRECTION('',(-1.,0.,0.));
#5127=DIRECTION('center_axis',(-0.923879532511286,-0.382683432365092,8.20569863179164E-15));
#5128=DIRECTION('ref_axis',(-0.382683432365092,0.923879532511286,1.98103089256178E-14));
#5129=DIRECTION('center_axis',(-0.707106781186548,0.707106781186548,0.));
#5130=DIRECTION('ref_axis',(0.499999999999999,0.499999999999999,0.707106781186549));
#5131=DIRECTION('',(0.707106781186547,-0.707106781186547,0.));
#5132=DIRECTION('center_axis',(-0.382683432365092,0.923879532511286,8.20569863179164E-15));
#5133=DIRECTION('ref_axis',(0.923879532511286,0.382683432365092,1.98103089256178E-14));
#5134=DIRECTION('',(-0.707106781186547,0.707106781186547,0.));
#5135=DIRECTION('center_axis',(0.,1.,0.));
#5136=DIRECTION('ref_axis',(0.707106781186546,0.,0.707106781186549));
#5137=DIRECTION('',(0.,-1.,0.));
#5138=DIRECTION('center_axis',(0.382683432365092,0.923879532511286,0.));
#5139=DIRECTION('ref_axis',(0.923879532511286,-0.382683432365092,0.));
#5140=DIRECTION('',(0.,1.,0.));
#5141=DIRECTION('center_axis',(0.707106781186548,0.707106781186548,0.));
#5142=DIRECTION('ref_axis',(0.499999999999999,-0.499999999999999,0.707106781186549));
#5143=DIRECTION('',(-0.707106781186547,-0.707106781186547,0.));
#5144=DIRECTION('center_axis',(0.923879532511286,0.382683432365092,8.20569863179164E-15));
#5145=DIRECTION('ref_axis',(0.382683432365092,-0.923879532511286,1.98103089256178E-14));
#5146=DIRECTION('',(0.707106781186547,0.707106781186547,0.));
#5147=DIRECTION('center_axis',(1.,0.,0.));
#5148=DIRECTION('ref_axis',(0.,-0.707106781186546,0.707106781186549));
#5149=DIRECTION('',(-1.,0.,0.));
#5150=DIRECTION('center_axis',(0.923879532511286,-0.382683432365092,0.));
#5151=DIRECTION('ref_axis',(-0.382683432365092,-0.923879532511286,0.));
#5152=DIRECTION('center_axis',(0.707106781186548,-0.707106781186548,0.));
#5153=DIRECTION('ref_axis',(-0.499999999999999,-0.499999999999999,0.707106781186549));
#5154=DIRECTION('',(-0.707106781186547,0.707106781186547,0.));
#5155=DIRECTION('center_axis',(0.382683432365092,-0.923879532511286,8.20569863179164E-15));
#5156=DIRECTION('ref_axis',(-0.923879532511286,-0.382683432365092,1.98103089256178E-14));
#5157=DIRECTION('center_axis',(0.,-1.,0.));
#5158=DIRECTION('ref_axis',(-0.707106781186546,0.,0.707106781186549));
#5159=DIRECTION('',(0.,1.,0.));
#5160=DIRECTION('center_axis',(-0.382683432365092,-0.923879532511286,0.));
#5161=DIRECTION('ref_axis',(-0.923879532511286,0.382683432365092,0.));
#5162=DIRECTION('center_axis',(-0.707106781186548,-0.707106781186548,0.));
#5163=DIRECTION('ref_axis',(-0.499999999999999,0.499999999999999,0.707106781186549));
#5164=DIRECTION('',(0.707106781186547,0.707106781186547,0.));
#5165=DIRECTION('center_axis',(0.,1.,0.));
#5166=DIRECTION('ref_axis',(-1.,0.,0.));
#5167=DIRECTION('',(0.,0.,1.));
#5168=DIRECTION('center_axis',(0.,0.,1.));
#5169=DIRECTION('ref_axis',(1.,0.,0.));
#5170=DIRECTION('center_axis',(0.,0.,1.));
#5171=DIRECTION('ref_axis',(1.,0.,0.));
#5172=DIRECTION('center_axis',(0.,0.,1.));
#5173=DIRECTION('ref_axis',(1.,0.,0.));
#5174=DIRECTION('center_axis',(0.,0.,1.));
#5175=DIRECTION('ref_axis',(1.,0.,0.));
#5176=DIRECTION('center_axis',(0.,0.,1.));
#5177=DIRECTION('ref_axis',(1.,0.,0.));
#5178=DIRECTION('center_axis',(0.,0.,1.));
#5179=DIRECTION('ref_axis',(1.,0.,0.));
#5180=DIRECTION('center_axis',(0.,0.,-1.));
#5181=DIRECTION('ref_axis',(-1.,0.,0.));
#5182=DIRECTION('center_axis',(0.,-1.,0.));
#5183=DIRECTION('ref_axis',(1.,0.,0.));
#5184=DIRECTION('center_axis',(0.,0.,-1.));
#5185=DIRECTION('ref_axis',(-1.,0.,0.));
#5186=DIRECTION('center_axis',(0.,-1.,0.));
#5187=DIRECTION('ref_axis',(1.,0.,0.));
#5188=DIRECTION('center_axis',(0.,0.,-1.));
#5189=DIRECTION('ref_axis',(-1.,0.,0.));
#5190=DIRECTION('center_axis',(0.,-1.,0.));
#5191=DIRECTION('ref_axis',(1.,0.,0.));
#5192=DIRECTION('center_axis',(0.,0.,-1.));
#5193=DIRECTION('ref_axis',(-1.,0.,0.));
#5194=DIRECTION('center_axis',(-1.22464679914735E-16,-1.,0.));
#5195=DIRECTION('ref_axis',(1.,-1.22464679914735E-16,0.));
#5196=DIRECTION('center_axis',(0.,0.,-1.));
#5197=DIRECTION('ref_axis',(-1.,0.,0.));
#5198=DIRECTION('center_axis',(0.,-1.,0.));
#5199=DIRECTION('ref_axis',(1.,0.,0.));
#5200=DIRECTION('center_axis',(0.707106781186548,0.707106781186548,0.));
#5201=DIRECTION('ref_axis',(-0.707106781186548,0.707106781186548,0.));
#5202=DIRECTION('',(0.,0.,1.));
#5203=DIRECTION('center_axis',(1.,0.,0.));
#5204=DIRECTION('ref_axis',(0.,1.,0.));
#5205=DIRECTION('',(0.,0.,1.));
#5206=DIRECTION('center_axis',(0.707106781186548,-0.707106781186548,0.));
#5207=DIRECTION('ref_axis',(0.707106781186548,0.707106781186548,0.));
#5208=DIRECTION('axis',(0.,0.,1.));
#5209=DIRECTION('refdir',(1.,0.,0.));
#5210=DIRECTION('center_axis',(0.,0.,-1.));
#5211=DIRECTION('ref_axis',(-1.,0.,0.));
#5212=DIRECTION('center_axis',(0.,0.,1.));
#5213=DIRECTION('ref_axis',(1.,0.,0.));
#5214=DIRECTION('center_axis',(0.,0.,1.));
#5215=DIRECTION('ref_axis',(1.,0.,0.));
#5216=DIRECTION('center_axis',(0.,0.,1.));
#5217=DIRECTION('ref_axis',(1.,0.,0.));
#5218=DIRECTION('center_axis',(0.,0.,1.));
#5219=DIRECTION('ref_axis',(1.,0.,0.));
#5220=DIRECTION('center_axis',(0.,0.,-1.));
#5221=DIRECTION('ref_axis',(1.,0.,0.));
#5222=DIRECTION('center_axis',(0.,0.,1.));
#5223=DIRECTION('ref_axis',(1.,0.,0.));
#5224=DIRECTION('center_axis',(0.,0.,-1.));
#5225=DIRECTION('ref_axis',(1.,0.,0.));
#5226=DIRECTION('center_axis',(0.,-1.,0.));
#5227=DIRECTION('ref_axis',(-1.,0.,0.));
#5228=DIRECTION('center_axis',(0.,0.,1.));
#5229=DIRECTION('ref_axis',(1.,0.,0.));
#5230=DIRECTION('center_axis',(0.,0.,1.));
#5231=DIRECTION('ref_axis',(1.,0.,0.));
#5232=DIRECTION('',(0.707106781186547,0.707106781186547,0.));
#5233=DIRECTION('',(1.,0.,0.));
#5234=DIRECTION('',(0.707106781186547,-0.707106781186547,0.));
#5235=DIRECTION('',(0.,-1.,0.));
#5236=DIRECTION('',(-0.707106781186547,-0.707106781186547,0.));
#5237=DIRECTION('',(-1.,0.,0.));
#5238=DIRECTION('',(-0.707106781186547,0.707106781186547,0.));
#5239=DIRECTION('',(0.,1.,0.));
#5240=DIRECTION('center_axis',(0.,0.,-1.));
#5241=DIRECTION('ref_axis',(1.,0.,0.));
#5242=DIRECTION('center_axis',(0.,0.,-1.));
#5243=DIRECTION('ref_axis',(1.,0.,0.));
#5244=DIRECTION('center_axis',(0.,0.,-1.));
#5245=DIRECTION('ref_axis',(1.,0.,0.));
#5246=DIRECTION('center_axis',(0.,0.,-1.));
#5247=DIRECTION('ref_axis',(1.,0.,0.));
#5248=DIRECTION('center_axis',(0.,0.,1.));
#5249=DIRECTION('ref_axis',(1.,0.,0.));
#5250=DIRECTION('',(0.,0.,1.));
#5251=DIRECTION('center_axis',(0.,0.,-1.));
#5252=DIRECTION('ref_axis',(1.,0.,0.));
#5253=DIRECTION('center_axis',(0.,0.,1.));
#5254=DIRECTION('ref_axis',(1.,0.,0.));
#5255=DIRECTION('center_axis',(0.,-1.,0.));
#5256=DIRECTION('ref_axis',(-1.,0.,0.));
#5257=DIRECTION('center_axis',(0.,0.,1.));
#5258=DIRECTION('ref_axis',(1.,0.,0.));
#5259=DIRECTION('center_axis',(0.,0.,1.));
#5260=DIRECTION('ref_axis',(1.,0.,0.));
#5261=DIRECTION('',(0.,0.,1.));
#5262=DIRECTION('center_axis',(0.,0.,-1.));
#5263=DIRECTION('ref_axis',(1.,0.,0.));
#5264=DIRECTION('center_axis',(0.,0.,-1.));
#5265=DIRECTION('ref_axis',(1.,0.,0.));
#5266=DIRECTION('center_axis',(0.,0.,1.));
#5267=DIRECTION('ref_axis',(1.,0.,0.));
#5268=DIRECTION('center_axis',(0.,-1.,0.));
#5269=DIRECTION('ref_axis',(-1.,0.,0.));
#5270=DIRECTION('center_axis',(0.,0.,1.));
#5271=DIRECTION('ref_axis',(1.,0.,0.));
#5272=DIRECTION('center_axis',(0.,0.,1.));
#5273=DIRECTION('ref_axis',(1.,0.,0.));
#5274=DIRECTION('',(0.,0.,1.));
#5275=DIRECTION('center_axis',(0.,0.,-1.));
#5276=DIRECTION('ref_axis',(1.,0.,0.));
#5277=DIRECTION('center_axis',(0.,0.,-1.));
#5278=DIRECTION('ref_axis',(1.,0.,0.));
#5279=DIRECTION('center_axis',(0.,0.,1.));
#5280=DIRECTION('ref_axis',(1.,0.,0.));
#5281=DIRECTION('center_axis',(1.22464679914735E-16,-1.,0.));
#5282=DIRECTION('ref_axis',(-1.,-1.22464679914735E-16,0.));
#5283=DIRECTION('center_axis',(0.,0.,1.));
#5284=DIRECTION('ref_axis',(1.,0.,0.));
#5285=DIRECTION('center_axis',(0.,-1.,0.));
#5286=DIRECTION('ref_axis',(-1.,0.,0.));
#5287=DIRECTION('center_axis',(0.,0.,1.));
#5288=DIRECTION('ref_axis',(1.,0.,0.));
#5289=DIRECTION('center_axis',(0.,0.,1.));
#5290=DIRECTION('ref_axis',(1.,0.,0.));
#5291=DIRECTION('',(0.,0.,1.));
#5292=DIRECTION('center_axis',(0.,0.,-1.));
#5293=DIRECTION('ref_axis',(1.,0.,0.));
#5294=DIRECTION('center_axis',(0.,0.,-1.));
#5295=DIRECTION('ref_axis',(1.,0.,0.));
#5296=DIRECTION('center_axis',(0.707106781186548,0.707106781186548,0.));
#5297=DIRECTION('ref_axis',(-0.499999999999996,0.499999999999996,-0.707106781186553));
#5298=DIRECTION('center_axis',(0.382683432365092,0.923879532511286,0.));
#5299=DIRECTION('ref_axis',(-0.923879532511286,0.382683432365092,0.));
#5300=DIRECTION('',(0.707106781186547,0.707106781186547,0.));
#5301=DIRECTION('center_axis',(0.923879532511283,0.382683432365099,3.39891166203448E-15));
#5302=DIRECTION('ref_axis',(-0.382683432365099,0.923879532511283,8.2056986317915E-15));
#5303=DIRECTION('center_axis',(0.,1.,0.));
#5304=DIRECTION('ref_axis',(-0.707106781186541,0.,-0.707106781186554));
#5305=DIRECTION('center_axis',(-0.382683432365099,0.923879532511283,3.39891166203448E-15));
#5306=DIRECTION('ref_axis',(-0.923879532511283,-0.382683432365099,8.2056986317915E-15));
#5307=DIRECTION('',(0.,1.,0.));
#5308=DIRECTION('center_axis',(-0.707106781186548,0.707106781186548,0.));
#5309=DIRECTION('ref_axis',(-0.499999999999996,-0.499999999999996,-0.707106781186553));
#5310=DIRECTION('center_axis',(-0.923879532511286,0.382683432365092,0.));
#5311=DIRECTION('ref_axis',(-0.382683432365092,-0.923879532511286,0.));
#5312=DIRECTION('',(-0.707106781186547,0.707106781186547,0.));
#5313=DIRECTION('center_axis',(-0.707106781186548,-0.707106781186548,0.));
#5314=DIRECTION('ref_axis',(0.499999999999996,-0.499999999999996,-0.707106781186553));
#5315=DIRECTION('center_axis',(-0.382683432365092,-0.923879532511286,0.));
#5316=DIRECTION('ref_axis',(0.923879532511286,-0.382683432365092,0.));
#5317=DIRECTION('',(-0.707106781186547,-0.707106781186547,0.));
#5318=DIRECTION('center_axis',(0.923879532511286,0.382683432365092,-8.20569863179153E-15));
#5319=DIRECTION('ref_axis',(-0.382683432365092,0.923879532511286,1.98103089256176E-14));
#5320=DIRECTION('center_axis',(0.,-1.,0.));
#5321=DIRECTION('ref_axis',(0.707106781186541,0.,-0.707106781186554));
#5322=DIRECTION('',(0.,-1.,0.));
#5323=DIRECTION('center_axis',(0.382683432365099,-0.923879532511283,3.39891166203448E-15));
#5324=DIRECTION('ref_axis',(0.923879532511283,0.382683432365099,8.2056986317915E-15));
#5325=DIRECTION('center_axis',(-1.,0.,0.));
#5326=DIRECTION('ref_axis',(0.,-0.707106781186541,-0.707106781186554));
#5327=DIRECTION('',(-1.,0.,0.));
#5328=DIRECTION('center_axis',(0.707106781186548,-0.707106781186548,0.));
#5329=DIRECTION('ref_axis',(0.499999999999996,0.499999999999996,-0.707106781186553));
#5330=DIRECTION('',(0.707106781186547,-0.707106781186547,0.));
#5331=DIRECTION('center_axis',(0.923879532511286,-0.382683432365092,0.));
#5332=DIRECTION('ref_axis',(0.382683432365092,0.923879532511286,0.));
#5333=DIRECTION('center_axis',(1.,0.,0.));
#5334=DIRECTION('ref_axis',(0.,0.707106781186541,-0.707106781186554));
#5335=DIRECTION('',(1.,0.,0.));
#5336=DIRECTION('center_axis',(-1.,0.,0.));
#5337=DIRECTION('ref_axis',(0.,-1.,0.));
#5338=DIRECTION('',(0.,0.,1.));
#5339=DIRECTION('',(0.,-1.,0.));
#5340=DIRECTION('',(0.,0.,1.));
#5341=DIRECTION('center_axis',(-0.707106781186548,-0.707106781186548,0.));
#5342=DIRECTION('ref_axis',(0.707106781186548,-0.707106781186548,0.));
#5343=DIRECTION('',(0.,0.,1.));
#5344=DIRECTION('',(0.707106781186547,-0.707106781186547,0.));
#5345=DIRECTION('center_axis',(0.,-1.,0.));
#5346=DIRECTION('ref_axis',(1.,0.,0.));
#5347=DIRECTION('',(0.,0.,1.));
#5348=DIRECTION('',(1.,0.,0.));
#5349=DIRECTION('center_axis',(0.707106781186548,-0.707106781186548,0.));
#5350=DIRECTION('ref_axis',(0.707106781186548,0.707106781186548,0.));
#5351=DIRECTION('',(0.,0.,1.));
#5352=DIRECTION('',(0.707106781186547,0.707106781186547,0.));
#5353=DIRECTION('center_axis',(0.707106781186548,0.707106781186548,0.));
#5354=DIRECTION('ref_axis',(-0.707106781186548,0.707106781186548,0.));
#5355=DIRECTION('',(0.,0.,1.));
#5356=DIRECTION('',(-0.707106781186547,0.707106781186547,0.));
#5357=DIRECTION('',(0.,0.,1.));
#5358=DIRECTION('center_axis',(1.,0.,0.));
#5359=DIRECTION('ref_axis',(0.,1.,0.));
#5360=DIRECTION('',(0.,1.,0.));
#5361=DIRECTION('center_axis',(0.,1.,0.));
#5362=DIRECTION('ref_axis',(-1.,0.,0.));
#5363=DIRECTION('',(0.,0.,1.));
#5364=DIRECTION('',(-1.,0.,0.));
#5365=DIRECTION('center_axis',(-0.707106781186548,0.707106781186548,0.));
#5366=DIRECTION('ref_axis',(-0.707106781186548,-0.707106781186548,0.));
#5367=DIRECTION('',(-0.707106781186547,-0.707106781186547,0.));
#5368=DIRECTION('center_axis',(0.,0.,-1.));
#5369=DIRECTION('ref_axis',(-1.,0.,0.));
#5370=DIRECTION('center_axis',(0.,0.,1.));
#5371=DIRECTION('ref_axis',(1.,0.,0.));
#5372=DIRECTION('center_axis',(0.,-1.,0.));
#5373=DIRECTION('ref_axis',(1.,0.,0.));
#5374=DIRECTION('center_axis',(0.,0.,1.));
#5375=DIRECTION('ref_axis',(1.,0.,0.));
#5376=DIRECTION('',(0.707106781186547,-0.707106781186547,0.));
#5377=DIRECTION('',(1.,0.,0.));
#5378=DIRECTION('',(0.707106781186547,0.707106781186547,0.));
#5379=DIRECTION('',(0.,1.,0.));
#5380=DIRECTION('',(-0.707106781186547,0.707106781186547,0.));
#5381=DIRECTION('',(-1.,0.,0.));
#5382=DIRECTION('',(-0.707106781186547,-0.707106781186547,0.));
#5383=DIRECTION('',(0.,-1.,0.));
#5384=DIRECTION('center_axis',(0.,0.,1.));
#5385=DIRECTION('ref_axis',(1.,0.,0.));
#5386=DIRECTION('center_axis',(0.,0.,1.));
#5387=DIRECTION('ref_axis',(1.,0.,0.));
#5388=DIRECTION('center_axis',(0.,0.,1.));
#5389=DIRECTION('ref_axis',(1.,0.,0.));
#5390=DIRECTION('center_axis',(0.,0.,1.));
#5391=DIRECTION('ref_axis',(1.,0.,0.));
#5392=DIRECTION('center_axis',(0.,0.,-1.));
#5393=DIRECTION('ref_axis',(-1.,0.,0.));
#5394=DIRECTION('center_axis',(0.,-1.,0.));
#5395=DIRECTION('ref_axis',(1.,0.,0.));
#5396=DIRECTION('center_axis',(0.,0.,-1.));
#5397=DIRECTION('ref_axis',(-1.,0.,0.));
#5398=DIRECTION('center_axis',(-1.22464679914735E-16,-1.,0.));
#5399=DIRECTION('ref_axis',(1.,-1.22464679914735E-16,0.));
#5400=DIRECTION('center_axis',(0.,0.,-1.));
#5401=DIRECTION('ref_axis',(-1.,0.,0.));
#5402=DIRECTION('center_axis',(0.,-1.,0.));
#5403=DIRECTION('ref_axis',(1.,0.,0.));
#5404=DIRECTION('center_axis',(0.707106781186548,-0.707106781186548,0.));
#5405=DIRECTION('ref_axis',(-0.5,-0.5,0.707106781186547));
#5406=DIRECTION('center_axis',(0.382683432365092,-0.923879532511286,8.20569863179167E-15));
#5407=DIRECTION('ref_axis',(-0.923879532511286,-0.382683432365092,1.98103089256179E-14));
#5408=DIRECTION('center_axis',(0.923879532511286,-0.382683432365092,0.));
#5409=DIRECTION('ref_axis',(-0.382683432365092,-0.923879532511286,0.));
#5410=DIRECTION('center_axis',(0.,-1.,0.));
#5411=DIRECTION('ref_axis',(-0.707106781186548,0.,0.707106781186548));
#5412=DIRECTION('center_axis',(-0.382683432365092,-0.923879532511286,0.));
#5413=DIRECTION('ref_axis',(-0.923879532511286,0.382683432365092,0.));
#5414=DIRECTION('center_axis',(-0.707106781186548,-0.707106781186548,0.));
#5415=DIRECTION('ref_axis',(-0.5,0.5,0.707106781186547));
#5416=DIRECTION('center_axis',(-0.923879532511286,-0.382683432365092,8.20569863179167E-15));
#5417=DIRECTION('ref_axis',(-0.382683432365092,0.923879532511286,1.98103089256179E-14));
#5418=DIRECTION('center_axis',(-0.707106781186548,0.707106781186548,0.));
#5419=DIRECTION('ref_axis',(0.5,0.5,0.707106781186547));
#5420=DIRECTION('center_axis',(-0.382683432365092,0.923879532511286,8.20569863179167E-15));
#5421=DIRECTION('ref_axis',(0.923879532511286,0.382683432365092,1.98103089256179E-14));
#5422=DIRECTION('center_axis',(0.923879532511286,-0.382683432365092,0.));
#5423=DIRECTION('ref_axis',(-0.382683432365092,-0.923879532511286,0.));
#5424=DIRECTION('center_axis',(0.,1.,0.));
#5425=DIRECTION('ref_axis',(0.707106781186548,0.,0.707106781186548));
#5426=DIRECTION('center_axis',(0.382683432365092,0.923879532511286,0.));
#5427=DIRECTION('ref_axis',(0.923879532511286,-0.382683432365092,0.));
#5428=DIRECTION('center_axis',(-1.,0.,0.));
#5429=DIRECTION('ref_axis',(0.,0.707106781186548,0.707106781186548));
#5430=DIRECTION('center_axis',(0.707106781186548,0.707106781186548,0.));
#5431=DIRECTION('ref_axis',(0.5,-0.5,0.707106781186547));
#5432=DIRECTION('center_axis',(0.923879532511286,0.382683432365092,8.20569863179167E-15));
#5433=DIRECTION('ref_axis',(0.382683432365092,-0.923879532511286,1.98103089256179E-14));
#5434=DIRECTION('center_axis',(1.,0.,0.));
#5435=DIRECTION('ref_axis',(0.,-0.707106781186548,0.707106781186548));
#5436=DIRECTION('center_axis',(0.,0.,1.));
#5437=DIRECTION('ref_axis',(1.,0.,0.));
#5438=DIRECTION('center_axis',(0.,-1.,0.));
#5439=DIRECTION('ref_axis',(-1.,0.,0.));
#5440=DIRECTION('center_axis',(0.,0.,1.));
#5441=DIRECTION('ref_axis',(1.,0.,0.));
#5442=DIRECTION('',(0.,0.,1.));
#5443=DIRECTION('axis',(0.,0.,1.));
#5444=DIRECTION('refdir',(1.,0.,0.));
#5445=DIRECTION('center_axis',(0.,0.,1.));
#5446=DIRECTION('ref_axis',(1.,0.,0.));
#5447=DIRECTION('center_axis',(0.,0.,1.));
#5448=DIRECTION('ref_axis',(1.,0.,0.));
#5449=DIRECTION('',(0.,0.,1.));
#5450=DIRECTION('center_axis',(0.,0.,1.));
#5451=DIRECTION('ref_axis',(1.,0.,0.));
#5452=DIRECTION('center_axis',(0.,0.,1.));
#5453=DIRECTION('ref_axis',(1.,0.,0.));
#5454=DIRECTION('center_axis',(0.,0.,1.));
#5455=DIRECTION('ref_axis',(1.,0.,0.));
#5456=DIRECTION('center_axis',(1.22464679914735E-16,-1.,0.));
#5457=DIRECTION('ref_axis',(-1.,-1.22464679914735E-16,0.));
#5458=DIRECTION('center_axis',(0.,0.,-1.));
#5459=DIRECTION('ref_axis',(-1.,0.,0.));
#5460=DIRECTION('center_axis',(0.,0.,1.));
#5461=DIRECTION('ref_axis',(1.,0.,0.));
#5462=DIRECTION('center_axis',(0.,0.,1.));
#5463=DIRECTION('ref_axis',(1.,0.,0.));
#5464=DIRECTION('center_axis',(0.,0.,1.));
#5465=DIRECTION('ref_axis',(1.,0.,0.));
#5466=DIRECTION('center_axis',(1.22464679914735E-16,-1.,0.));
#5467=DIRECTION('ref_axis',(-1.,-1.22464679914735E-16,0.));
#5468=DIRECTION('center_axis',(0.,0.,1.));
#5469=DIRECTION('ref_axis',(1.,0.,0.));
#5470=DIRECTION('center_axis',(0.,0.,1.));
#5471=DIRECTION('ref_axis',(1.,0.,0.));
#5472=DIRECTION('',(0.,0.,-1.));
#5473=DIRECTION('center_axis',(0.,0.,1.));
#5474=DIRECTION('ref_axis',(1.,0.,0.));
#5475=DIRECTION('center_axis',(0.,0.,1.));
#5476=DIRECTION('ref_axis',(1.,0.,0.));
#5477=DIRECTION('center_axis',(1.22464679914735E-16,-1.,0.));
#5478=DIRECTION('ref_axis',(-1.,-1.22464679914735E-16,0.));
#5479=DIRECTION('center_axis',(0.,0.,1.));
#5480=DIRECTION('ref_axis',(1.,0.,0.));
#5481=DIRECTION('center_axis',(0.,0.,1.));
#5482=DIRECTION('ref_axis',(1.,0.,0.));
#5483=DIRECTION('center_axis',(0.,0.,1.));
#5484=DIRECTION('ref_axis',(1.,0.,0.));
#5485=DIRECTION('center_axis',(1.22464679914735E-16,-1.,0.));
#5486=DIRECTION('ref_axis',(-1.,-1.22464679914735E-16,0.));
#5487=DIRECTION('axis',(0.,0.,1.));
#5488=DIRECTION('refdir',(1.,0.,0.));
#5489=DIRECTION('center_axis',(0.,0.,1.));
#5490=DIRECTION('ref_axis',(-0.45775083898785,-0.889080519079076,0.));
#5491=DIRECTION('',(0.,0.,-1.));
#5492=DIRECTION('center_axis',(0.,0.,-1.));
#5493=DIRECTION('ref_axis',(1.,-1.55574189099595E-12,0.));
#5494=DIRECTION('center_axis',(0.,0.,1.));
#5495=DIRECTION('ref_axis',(-0.45775083898785,-0.889080519079076,0.));
#5496=DIRECTION('',(0.,0.,-1.));
#5497=DIRECTION('center_axis',(0.,0.,1.));
#5498=DIRECTION('ref_axis',(-0.45775083898785,-0.889080519079076,0.));
#5499=DIRECTION('',(0.,0.,-1.));
#5500=DIRECTION('center_axis',(0.,0.,1.));
#5501=DIRECTION('ref_axis',(-0.45775083898785,-0.889080519079076,0.));
#5502=DIRECTION('',(0.,0.,-1.));
#5503=DIRECTION('center_axis',(0.,0.,1.));
#5504=DIRECTION('ref_axis',(-0.45775083898785,-0.889080519079076,0.));
#5505=DIRECTION('',(0.,0.,-1.));
#5506=DIRECTION('center_axis',(0.,0.,1.));
#5507=DIRECTION('ref_axis',(-0.45775083898785,-0.889080519079076,0.));
#5508=DIRECTION('',(0.,0.,-1.));
#5509=DIRECTION('center_axis',(0.,0.,1.));
#5510=DIRECTION('ref_axis',(-0.45775083898785,-0.889080519079076,0.));
#5511=DIRECTION('',(0.,0.,-1.));
#5512=DIRECTION('center_axis',(0.,0.,1.));
#5513=DIRECTION('ref_axis',(-0.45775083898785,-0.889080519079076,0.));
#5514=DIRECTION('',(0.,0.,-1.));
#5515=DIRECTION('center_axis',(0.,0.,1.));
#5516=DIRECTION('ref_axis',(-0.45775083898785,-0.889080519079076,0.));
#5517=DIRECTION('',(0.,0.,-1.));
#5518=DIRECTION('center_axis',(0.,0.,1.));
#5519=DIRECTION('ref_axis',(-0.45775083898785,-0.889080519079076,0.));
#5520=DIRECTION('',(0.,0.,-1.));
#5521=DIRECTION('center_axis',(0.,0.,1.));
#5522=DIRECTION('ref_axis',(-0.45775083898785,-0.889080519079076,0.));
#5523=DIRECTION('',(0.,0.,-1.));
#5524=DIRECTION('center_axis',(0.,0.,1.));
#5525=DIRECTION('ref_axis',(-0.45775083898785,-0.889080519079076,0.));
#5526=DIRECTION('',(0.,0.,-1.));
#5527=DIRECTION('center_axis',(0.,0.,1.));
#5528=DIRECTION('ref_axis',(-0.45775083898785,-0.889080519079076,0.));
#5529=DIRECTION('',(0.,0.,-1.));
#5530=DIRECTION('center_axis',(0.,0.,1.));
#5531=DIRECTION('ref_axis',(-0.45775083898785,-0.889080519079076,0.));
#5532=DIRECTION('',(0.,0.,-1.));
#5533=DIRECTION('center_axis',(0.,0.,1.));
#5534=DIRECTION('ref_axis',(-0.45775083898785,-0.889080519079076,0.));
#5535=DIRECTION('',(0.,0.,-1.));
#5536=DIRECTION('center_axis',(0.,0.,1.));
#5537=DIRECTION('ref_axis',(-0.45775083898785,-0.889080519079076,0.));
#5538=DIRECTION('',(0.,0.,-1.));
#5539=DIRECTION('center_axis',(0.,0.,1.));
#5540=DIRECTION('ref_axis',(-0.45775083898785,-0.889080519079076,0.));
#5541=DIRECTION('',(0.,0.,-1.));
#5542=DIRECTION('center_axis',(0.,0.,1.));
#5543=DIRECTION('ref_axis',(-0.45775083898785,-0.889080519079076,0.));
#5544=DIRECTION('',(0.,0.,-1.));
#5545=DIRECTION('center_axis',(0.,0.,1.));
#5546=DIRECTION('ref_axis',(-0.45775083898785,-0.889080519079076,0.));
#5547=DIRECTION('',(0.,0.,-1.));
#5548=DIRECTION('center_axis',(0.,0.,1.));
#5549=DIRECTION('ref_axis',(-0.45775083898785,-0.889080519079076,0.));
#5550=DIRECTION('',(0.,0.,-1.));
#5551=DIRECTION('center_axis',(0.,0.,1.));
#5552=DIRECTION('ref_axis',(-0.45775083898785,-0.889080519079076,0.));
#5553=DIRECTION('',(0.,0.,-1.));
#5554=DIRECTION('center_axis',(0.,0.,1.));
#5555=DIRECTION('ref_axis',(-0.45775083898785,-0.889080519079076,0.));
#5556=DIRECTION('',(0.,0.,-1.));
#5557=DIRECTION('center_axis',(0.,0.,1.));
#5558=DIRECTION('ref_axis',(-0.45775083898785,-0.889080519079076,0.));
#5559=DIRECTION('',(0.,0.,-1.));
#5560=DIRECTION('center_axis',(0.,0.,1.));
#5561=DIRECTION('ref_axis',(-0.45775083898785,-0.889080519079076,0.));
#5562=DIRECTION('',(0.,0.,-1.));
#5563=DIRECTION('center_axis',(0.,0.,1.));
#5564=DIRECTION('ref_axis',(-0.45775083898785,-0.889080519079076,0.));
#5565=DIRECTION('',(0.,0.,-1.));
#5566=DIRECTION('center_axis',(0.,0.,1.));
#5567=DIRECTION('ref_axis',(-0.45775083898785,-0.889080519079076,0.));
#5568=DIRECTION('',(0.,0.,-1.));
#5569=DIRECTION('center_axis',(0.,0.,1.));
#5570=DIRECTION('ref_axis',(-0.45775083898785,-0.889080519079076,0.));
#5571=DIRECTION('',(0.,0.,-1.));
#5572=DIRECTION('center_axis',(0.,0.,1.));
#5573=DIRECTION('ref_axis',(-0.45775083898785,-0.889080519079076,0.));
#5574=DIRECTION('',(0.,0.,-1.));
#5575=DIRECTION('center_axis',(0.,0.,1.));
#5576=DIRECTION('ref_axis',(-0.45775083898785,-0.889080519079076,0.));
#5577=DIRECTION('',(0.,0.,-1.));
#5578=DIRECTION('center_axis',(0.,0.,1.));
#5579=DIRECTION('ref_axis',(-0.45775083898785,-0.889080519079076,0.));
#5580=DIRECTION('',(0.,0.,-1.));
#5581=DIRECTION('center_axis',(0.,0.,1.));
#5582=DIRECTION('ref_axis',(-0.45775083898785,-0.889080519079076,0.));
#5583=DIRECTION('',(0.,0.,-1.));
#5584=DIRECTION('center_axis',(0.,0.,1.));
#5585=DIRECTION('ref_axis',(-0.45775083898785,-0.889080519079076,0.));
#5586=DIRECTION('',(0.,0.,-1.));
#5587=DIRECTION('center_axis',(0.,0.,1.));
#5588=DIRECTION('ref_axis',(-0.45775083898785,-0.889080519079076,0.));
#5589=DIRECTION('',(0.,0.,-1.));
#5590=DIRECTION('center_axis',(0.,0.,1.));
#5591=DIRECTION('ref_axis',(-0.45775083898785,-0.889080519079076,0.));
#5592=DIRECTION('',(0.,0.,-1.));
#5593=DIRECTION('center_axis',(0.,0.,1.));
#5594=DIRECTION('ref_axis',(-0.45775083898785,-0.889080519079076,0.));
#5595=DIRECTION('',(0.,0.,-1.));
#5596=DIRECTION('center_axis',(0.,0.,1.));
#5597=DIRECTION('ref_axis',(-0.45775083898785,-0.889080519079076,0.));
#5598=DIRECTION('',(0.,0.,-1.));
#5599=DIRECTION('center_axis',(0.,0.,1.));
#5600=DIRECTION('ref_axis',(-0.45775083898785,-0.889080519079076,0.));
#5601=DIRECTION('',(0.,0.,-1.));
#5602=DIRECTION('center_axis',(0.,0.,1.));
#5603=DIRECTION('ref_axis',(-0.45775083898785,-0.889080519079076,0.));
#5604=DIRECTION('',(0.,0.,-1.));
#5605=DIRECTION('center_axis',(0.,0.,1.));
#5606=DIRECTION('ref_axis',(-0.45775083898785,-0.889080519079076,0.));
#5607=DIRECTION('',(0.,0.,-1.));
#5608=DIRECTION('center_axis',(0.,0.,1.));
#5609=DIRECTION('ref_axis',(-0.45775083898785,-0.889080519079076,0.));
#5610=DIRECTION('',(0.,0.,-1.));
#5611=DIRECTION('center_axis',(0.,0.,1.));
#5612=DIRECTION('ref_axis',(-0.45775083898785,-0.889080519079076,0.));
#5613=DIRECTION('',(0.,0.,-1.));
#5614=DIRECTION('center_axis',(0.,0.,1.));
#5615=DIRECTION('ref_axis',(-0.45775083898785,-0.889080519079076,0.));
#5616=DIRECTION('',(0.,0.,-1.));
#5617=DIRECTION('center_axis',(0.,0.,1.));
#5618=DIRECTION('ref_axis',(-0.45775083898785,-0.889080519079076,0.));
#5619=DIRECTION('',(0.,0.,-1.));
#5620=DIRECTION('center_axis',(0.,0.,1.));
#5621=DIRECTION('ref_axis',(-0.45775083898785,-0.889080519079076,0.));
#5622=DIRECTION('',(0.,0.,-1.));
#5623=DIRECTION('center_axis',(0.,0.,1.));
#5624=DIRECTION('ref_axis',(-0.45775083898785,-0.889080519079076,0.));
#5625=DIRECTION('',(0.,0.,-1.));
#5626=DIRECTION('center_axis',(0.,0.,1.));
#5627=DIRECTION('ref_axis',(-0.45775083898785,-0.889080519079076,0.));
#5628=DIRECTION('',(0.,0.,-1.));
#5629=DIRECTION('center_axis',(0.,0.,1.));
#5630=DIRECTION('ref_axis',(-0.45775083898785,-0.889080519079076,0.));
#5631=DIRECTION('',(0.,0.,-1.));
#5632=DIRECTION('center_axis',(0.,0.,1.));
#5633=DIRECTION('ref_axis',(-0.45775083898785,-0.889080519079076,0.));
#5634=DIRECTION('',(0.,0.,-1.));
#5635=DIRECTION('center_axis',(0.,0.,1.));
#5636=DIRECTION('ref_axis',(-0.45775083898785,-0.889080519079076,0.));
#5637=DIRECTION('',(0.,0.,-1.));
#5638=DIRECTION('center_axis',(0.,0.,1.));
#5639=DIRECTION('ref_axis',(-0.45775083898785,-0.889080519079076,0.));
#5640=DIRECTION('',(0.,0.,-1.));
#5641=DIRECTION('center_axis',(0.,0.,1.));
#5642=DIRECTION('ref_axis',(-0.45775083898785,-0.889080519079076,0.));
#5643=DIRECTION('',(0.,0.,-1.));
#5644=DIRECTION('center_axis',(0.,0.,1.));
#5645=DIRECTION('ref_axis',(-0.45775083898785,-0.889080519079076,0.));
#5646=DIRECTION('',(0.,0.,-1.));
#5647=DIRECTION('center_axis',(0.,0.,1.));
#5648=DIRECTION('ref_axis',(-0.45775083898785,-0.889080519079076,0.));
#5649=DIRECTION('',(0.,0.,-1.));
#5650=DIRECTION('center_axis',(0.,0.,1.));
#5651=DIRECTION('ref_axis',(-0.45775083898785,-0.889080519079076,0.));
#5652=DIRECTION('',(0.,0.,-1.));
#5653=DIRECTION('center_axis',(0.,0.,1.));
#5654=DIRECTION('ref_axis',(-0.45775083898785,-0.889080519079076,0.));
#5655=DIRECTION('',(0.,0.,-1.));
#5656=DIRECTION('center_axis',(0.,0.,1.));
#5657=DIRECTION('ref_axis',(-0.45775083898785,-0.889080519079076,0.));
#5658=DIRECTION('',(0.,0.,-1.));
#5659=DIRECTION('center_axis',(0.,0.,1.));
#5660=DIRECTION('ref_axis',(-0.45775083898785,-0.889080519079076,0.));
#5661=DIRECTION('',(0.,0.,-1.));
#5662=DIRECTION('center_axis',(0.,0.,1.));
#5663=DIRECTION('ref_axis',(-0.45775083898785,-0.889080519079076,0.));
#5664=DIRECTION('',(0.,0.,-1.));
#5665=DIRECTION('center_axis',(0.,0.,1.));
#5666=DIRECTION('ref_axis',(-0.45775083898785,-0.889080519079076,0.));
#5667=DIRECTION('',(0.,0.,-1.));
#5668=DIRECTION('center_axis',(0.,0.,1.));
#5669=DIRECTION('ref_axis',(-0.45775083898785,-0.889080519079076,0.));
#5670=DIRECTION('',(0.,0.,-1.));
#5671=DIRECTION('center_axis',(0.,0.,1.));
#5672=DIRECTION('ref_axis',(-0.45775083898785,-0.889080519079076,0.));
#5673=DIRECTION('',(0.,0.,-1.));
#5674=DIRECTION('center_axis',(0.,0.,1.));
#5675=DIRECTION('ref_axis',(-0.45775083898785,-0.889080519079076,0.));
#5676=DIRECTION('',(0.,0.,-1.));
#5677=DIRECTION('center_axis',(0.,0.,1.));
#5678=DIRECTION('ref_axis',(-0.45775083898785,-0.889080519079076,0.));
#5679=DIRECTION('',(0.,0.,-1.));
#5680=DIRECTION('center_axis',(0.,0.,1.));
#5681=DIRECTION('ref_axis',(-0.45775083898785,-0.889080519079076,0.));
#5682=DIRECTION('',(0.,0.,-1.));
#5683=DIRECTION('center_axis',(0.,0.,1.));
#5684=DIRECTION('ref_axis',(-0.45775083898785,-0.889080519079076,0.));
#5685=DIRECTION('',(0.,0.,-1.));
#5686=DIRECTION('center_axis',(0.,0.,1.));
#5687=DIRECTION('ref_axis',(-0.45775083898785,-0.889080519079076,0.));
#5688=DIRECTION('',(0.,0.,-1.));
#5689=DIRECTION('center_axis',(0.,0.,1.));
#5690=DIRECTION('ref_axis',(-0.45775083898785,-0.889080519079076,0.));
#5691=DIRECTION('',(0.,0.,-1.));
#5692=DIRECTION('center_axis',(0.,0.,1.));
#5693=DIRECTION('ref_axis',(-0.45775083898785,-0.889080519079076,0.));
#5694=DIRECTION('',(0.,0.,-1.));
#5695=DIRECTION('center_axis',(0.,0.,1.));
#5696=DIRECTION('ref_axis',(-0.45775083898785,-0.889080519079076,0.));
#5697=DIRECTION('',(0.,0.,-1.));
#5698=DIRECTION('center_axis',(0.,0.,1.));
#5699=DIRECTION('ref_axis',(-0.45775083898785,-0.889080519079076,0.));
#5700=DIRECTION('',(0.,0.,-1.));
#5701=DIRECTION('center_axis',(0.,0.,1.));
#5702=DIRECTION('ref_axis',(-0.45775083898785,-0.889080519079076,0.));
#5703=DIRECTION('',(0.,0.,-1.));
#5704=DIRECTION('center_axis',(0.,0.,1.));
#5705=DIRECTION('ref_axis',(-0.45775083898785,-0.889080519079076,0.));
#5706=DIRECTION('',(0.,0.,-1.));
#5707=DIRECTION('center_axis',(0.,0.,1.));
#5708=DIRECTION('ref_axis',(-0.45775083898785,-0.889080519079076,0.));
#5709=DIRECTION('',(0.,0.,-1.));
#5710=DIRECTION('center_axis',(0.,0.,1.));
#5711=DIRECTION('ref_axis',(-0.45775083898785,-0.889080519079076,0.));
#5712=DIRECTION('',(0.,0.,-1.));
#5713=DIRECTION('center_axis',(0.,0.,1.));
#5714=DIRECTION('ref_axis',(-0.45775083898785,-0.889080519079076,0.));
#5715=DIRECTION('',(0.,0.,-1.));
#5716=DIRECTION('center_axis',(0.,0.,1.));
#5717=DIRECTION('ref_axis',(-0.45775083898785,-0.889080519079076,0.));
#5718=DIRECTION('',(0.,0.,-1.));
#5719=DIRECTION('center_axis',(0.,0.,1.));
#5720=DIRECTION('ref_axis',(-0.45775083898785,-0.889080519079076,0.));
#5721=DIRECTION('',(0.,0.,-1.));
#5722=DIRECTION('center_axis',(0.,0.,1.));
#5723=DIRECTION('ref_axis',(-0.45775083898785,-0.889080519079076,0.));
#5724=DIRECTION('',(0.,0.,-1.));
#5725=DIRECTION('center_axis',(0.,0.,1.));
#5726=DIRECTION('ref_axis',(-0.45775083898785,-0.889080519079076,0.));
#5727=DIRECTION('',(0.,0.,-1.));
#5728=DIRECTION('center_axis',(0.,0.,1.));
#5729=DIRECTION('ref_axis',(-0.45775083898785,-0.889080519079076,0.));
#5730=DIRECTION('',(0.,0.,-1.));
#5731=DIRECTION('center_axis',(0.,0.,1.));
#5732=DIRECTION('ref_axis',(-0.45775083898785,-0.889080519079076,0.));
#5733=DIRECTION('',(0.,0.,-1.));
#5734=DIRECTION('center_axis',(0.,0.,1.));
#5735=DIRECTION('ref_axis',(-0.45775083898785,-0.889080519079076,0.));
#5736=DIRECTION('',(0.,0.,-1.));
#5737=DIRECTION('center_axis',(0.,0.,1.));
#5738=DIRECTION('ref_axis',(-0.45775083898785,-0.889080519079076,0.));
#5739=DIRECTION('',(0.,0.,-1.));
#5740=DIRECTION('center_axis',(0.,0.,1.));
#5741=DIRECTION('ref_axis',(-0.45775083898785,-0.889080519079076,0.));
#5742=DIRECTION('',(0.,0.,-1.));
#5743=DIRECTION('center_axis',(0.,0.,1.));
#5744=DIRECTION('ref_axis',(1.,0.,0.));
#5745=DIRECTION('center_axis',(0.,0.,-1.));
#5746=DIRECTION('ref_axis',(1.,0.,0.));
#5747=DIRECTION('center_axis',(0.,0.,-1.));
#5748=DIRECTION('ref_axis',(1.,0.,0.));
#5749=DIRECTION('center_axis',(0.,0.,1.));
#5750=DIRECTION('ref_axis',(-0.45775083898785,-0.889080519079076,0.));
#5751=DIRECTION('center_axis',(0.,0.,1.));
#5752=DIRECTION('ref_axis',(1.,-1.55574189099595E-12,0.));
#5753=DIRECTION('center_axis',(0.,0.,1.));
#5754=DIRECTION('ref_axis',(1.,0.,0.));
#5755=DIRECTION('center_axis',(0.,0.,1.));
#5756=DIRECTION('ref_axis',(1.,0.,0.));
#5757=DIRECTION('',(0.,0.,1.));
#5758=DIRECTION('',(1.,0.,0.));
#5759=DIRECTION('',(-1.63349071185604E-16,-7.87117878343273E-17,1.));
#5760=DIRECTION('',(1.,1.04473373618377E-15,1.63349071185604E-16));
#5761=DIRECTION('',(-1.20939906596758E-17,-1.3997410048713E-33,1.));
#5762=DIRECTION('',(1.,2.20374371076739E-17,1.20939906596758E-17));
#5763=DIRECTION('',(1.98206610355338E-16,-2.21889488581915E-19,0.999999999999999));
#5764=DIRECTION('',(1.,-6.93889390390723E-17,5.55111512312578E-17));
#5765=DIRECTION('',(2.06013535156719E-16,-4.71344509643335E-33,0.999999999999998));
#5766=DIRECTION('',(0.952263949897106,0.305275891164635,5.75384988659927E-17));
#5767=DIRECTION('',(1.59781860987693E-16,1.155334602982E-33,0.999999999999998));
#5768=DIRECTION('',(0.952263949897106,0.305275891164635,7.20959914802382E-17));
#5769=DIRECTION('',(-2.10352082696537E-16,-5.98273021488495E-18,1.));
#5770=DIRECTION('',(0.977686539610761,-0.210069108304712,2.04401613030025E-16));
#5771=DIRECTION('',(-4.6711005257732E-18,-1.74794478769621E-17,1.));
#5772=DIRECTION('',(1.,-1.2205539374958E-15,4.67110052577318E-18));
#5773=DIRECTION('',(6.12323399573677E-17,-6.12323399573677E-17,1.));
#5774=DIRECTION('',(1.,-1.24370658107054E-17,-6.12323399573677E-17));
#5775=CARTESIAN_POINT('',(0.,0.,0.));
#5776=CARTESIAN_POINT('',(0.,0.,0.));
#5777=CARTESIAN_POINT('Origin',(0.,0.,4.));
#5778=CARTESIAN_POINT('',(-20.5,-2.51052593825207E-15,2.06740544556191));
#5779=CARTESIAN_POINT('Origin',(0.,0.,2.06740544556191));
#5780=CARTESIAN_POINT('',(-20.5,-2.51052593825207E-15,5.93259455443809));
#5781=CARTESIAN_POINT('',(-20.5,-2.51052593825207E-15,4.));
#5782=CARTESIAN_POINT('Origin',(0.,0.,5.93259455443809));
#5783=CARTESIAN_POINT('Origin',(19.5,0.,5.93259455443809));
#5784=CARTESIAN_POINT('',(-20.,2.44929359829471E-15,5.93259455443809));
#5785=CARTESIAN_POINT('Origin',(0.,0.,5.93259455443809));
#5786=CARTESIAN_POINT('Origin',(20.5,0.,2.06740544556191));
#5787=CARTESIAN_POINT('',(-20.,-2.44929359829471E-15,2.06740544556191));
#5788=CARTESIAN_POINT('Origin',(0.,0.,2.06740544556191));
#5789=CARTESIAN_POINT('Origin',(0.,0.,0.));
#5790=CARTESIAN_POINT('',(20.,-2.44929359829471E-15,0.5));
#5791=CARTESIAN_POINT('',(-20.,-2.44929359829471E-15,0.5));
#5792=CARTESIAN_POINT('Origin',(0.,0.,0.5));
#5793=CARTESIAN_POINT('Origin',(0.,0.,0.5));
#5794=CARTESIAN_POINT('',(-20.,-2.44929359829471E-15,0.));
#5795=CARTESIAN_POINT('Origin',(13.5,29.5,0.5));
#5796=CARTESIAN_POINT('',(26.7928932188135,29.5,0.));
#5797=CARTESIAN_POINT('',(-26.7928932188135,29.5,0.));
#5798=CARTESIAN_POINT('',(13.5,29.5,0.));
#5799=CARTESIAN_POINT('',(-27.,30.,0.5));
#5800=CARTESIAN_POINT('Origin',(-26.7928932188135,29.5,0.5));
#5801=CARTESIAN_POINT('',(27.,30.,0.5));
#5802=CARTESIAN_POINT('',(13.5,30.,0.5));
#5803=CARTESIAN_POINT('Origin',(26.7928932188135,29.5,0.5));
#5804=CARTESIAN_POINT('Origin',(-27.3964466094067,28.8964466094067,0.5));
#5805=CARTESIAN_POINT('',(-29.5,26.7928932188135,0.));
#5806=CARTESIAN_POINT('',(-27.3964466094067,28.8964466094067,0.));
#5807=CARTESIAN_POINT('',(-30.,27.,0.5));
#5808=CARTESIAN_POINT('Origin',(-29.5,26.7928932188135,0.5));
#5809=CARTESIAN_POINT('',(-27.75,29.25,0.5));
#5810=CARTESIAN_POINT('Origin',(-29.5,13.5,0.5));
#5811=CARTESIAN_POINT('',(-29.5,-26.7928932188135,0.));
#5812=CARTESIAN_POINT('',(-29.5,13.5,0.));
#5813=CARTESIAN_POINT('',(-30.,-27.,0.5));
#5814=CARTESIAN_POINT('Origin',(-29.5,-26.7928932188135,0.5));
#5815=CARTESIAN_POINT('',(-30.,13.5,0.5));
#5816=CARTESIAN_POINT('Origin',(-13.5,-29.5,0.5));
#5817=CARTESIAN_POINT('',(-26.7928932188135,-29.5,0.));
#5818=CARTESIAN_POINT('',(26.7928932188135,-29.5,0.));
#5819=CARTESIAN_POINT('',(-13.5,-29.5,0.));
#5820=CARTESIAN_POINT('',(27.,-30.,0.5));
#5821=CARTESIAN_POINT('Origin',(26.7928932188135,-29.5,0.5));
#5822=CARTESIAN_POINT('',(-27.,-30.,0.5));
#5823=CARTESIAN_POINT('',(-13.5,-30.,0.5));
#5824=CARTESIAN_POINT('Origin',(-26.7928932188135,-29.5,0.5));
#5825=CARTESIAN_POINT('Origin',(27.3964466094067,-28.8964466094067,0.5));
#5826=CARTESIAN_POINT('',(30.,-27.,0.5));
#5827=CARTESIAN_POINT('',(27.75,-29.25,0.5));
#5828=CARTESIAN_POINT('',(29.5,-26.7928932188135,0.));
#5829=CARTESIAN_POINT('',(27.3964466094067,-28.8964466094067,0.));
#5830=CARTESIAN_POINT('Origin',(29.5,-26.7928932188135,0.5));
#5831=CARTESIAN_POINT('Origin',(-28.8964466094067,-27.3964466094067,0.5));
#5832=CARTESIAN_POINT('',(-28.8964466094067,-27.3964466094067,0.));
#5833=CARTESIAN_POINT('',(-29.25,-27.75,0.5));
#5834=CARTESIAN_POINT('Origin',(29.5,-13.5,0.5));
#5835=CARTESIAN_POINT('',(30.,27.,0.5));
#5836=CARTESIAN_POINT('',(30.,-13.5,0.5));
#5837=CARTESIAN_POINT('',(29.5,26.7928932188135,0.));
#5838=CARTESIAN_POINT('',(29.5,-13.5,0.));
#5839=CARTESIAN_POINT('Origin',(29.5,26.7928932188135,0.5));
#5840=CARTESIAN_POINT('Origin',(28.8964466094067,27.3964466094067,0.5));
#5841=CARTESIAN_POINT('',(29.25,27.75,0.5));
#5842=CARTESIAN_POINT('',(28.8964466094067,27.3964466094067,0.));
#5843=CARTESIAN_POINT('Origin',(-27.,30.,0.));
#5844=CARTESIAN_POINT('',(-30.,27.,7.5));
#5845=CARTESIAN_POINT('',(-30.,27.,0.));
#5846=CARTESIAN_POINT('',(-27.,30.,7.5));
#5847=CARTESIAN_POINT('',(-27.75,29.25,7.5));
#5848=CARTESIAN_POINT('',(-27.,30.,0.));
#5849=CARTESIAN_POINT('Origin',(-30.,27.,0.));
#5850=CARTESIAN_POINT('',(-30.,-27.,7.5));
#5851=CARTESIAN_POINT('',(-30.,-27.,0.));
#5852=CARTESIAN_POINT('',(-30.,13.5,7.5));
#5853=CARTESIAN_POINT('Origin',(-30.,-27.,0.));
#5854=CARTESIAN_POINT('',(-27.,-30.,7.5));
#5855=CARTESIAN_POINT('',(-27.,-30.,0.));
#5856=CARTESIAN_POINT('',(-29.25,-27.75,7.5));
#5857=CARTESIAN_POINT('Origin',(-27.,-30.,0.));
#5858=CARTESIAN_POINT('',(27.,-30.,7.5));
#5859=CARTESIAN_POINT('',(27.,-30.,0.));
#5860=CARTESIAN_POINT('',(-13.5,-30.,7.5));
#5861=CARTESIAN_POINT('Origin',(0.,0.,0.));
#5862=CARTESIAN_POINT('',(28.0502525316942,-23.5502525316942,0.));
#5863=CARTESIAN_POINT('Origin',(23.5502525316942,-23.5502525316942,0.));
#5864=CARTESIAN_POINT('',(-19.0502525316942,23.5502525316942,0.));
#5865=CARTESIAN_POINT('Origin',(-23.5502525316942,23.5502525316942,0.));
#5866=CARTESIAN_POINT('',(-19.0502525316942,-23.5502525316942,0.));
#5867=CARTESIAN_POINT('Origin',(-23.5502525316942,-23.5502525316942,0.));
#5868=CARTESIAN_POINT('',(20.5,-2.51052593825207E-15,0.));
#5869=CARTESIAN_POINT('Origin',(0.,0.,0.));
#5870=CARTESIAN_POINT('',(28.0502525316942,23.5502525316942,0.));
#5871=CARTESIAN_POINT('Origin',(23.5502525316942,23.5502525316942,0.));
#5872=CARTESIAN_POINT('Origin',(23.5502525316942,-23.5502525316942,0.5));
#5873=CARTESIAN_POINT('',(19.5502525316942,-23.5502525316942,0.5));
#5874=CARTESIAN_POINT('',(27.5502525316942,-23.5502525316942,0.5));
#5875=CARTESIAN_POINT('Origin',(23.5502525316942,-23.5502525316942,0.5));
#5876=CARTESIAN_POINT('Origin',(28.0502525316942,-23.5502525316942,0.5));
#5877=CARTESIAN_POINT('Origin',(23.5502525316942,-23.5502525316942,0.5));
#5878=CARTESIAN_POINT('Origin',(23.5502525316942,-23.5502525316942,0.));
#5879=CARTESIAN_POINT('',(19.5502525316942,-23.5502525316942,7.5));
#5880=CARTESIAN_POINT('',(19.5502525316942,-23.5502525316942,0.));
#5881=CARTESIAN_POINT('',(27.5502525316942,-23.5502525316942,7.5));
#5882=CARTESIAN_POINT('Origin',(23.5502525316942,-23.5502525316942,7.5));
#5883=CARTESIAN_POINT('Origin',(23.5502525316942,-23.5502525316942,7.5));
#5884=CARTESIAN_POINT('Origin',(23.5502525316942,23.5502525316942,0.5));
#5885=CARTESIAN_POINT('',(19.5502525316942,23.5502525316942,0.5));
#5886=CARTESIAN_POINT('',(27.5502525316942,23.5502525316942,0.5));
#5887=CARTESIAN_POINT('Origin',(23.5502525316942,23.5502525316942,0.5));
#5888=CARTESIAN_POINT('Origin',(28.0502525316942,23.5502525316942,0.5));
#5889=CARTESIAN_POINT('Origin',(23.5502525316942,23.5502525316942,0.5));
#5890=CARTESIAN_POINT('Origin',(23.5502525316942,23.5502525316942,0.));
#5891=CARTESIAN_POINT('',(19.5502525316942,23.5502525316942,7.5));
#5892=CARTESIAN_POINT('',(19.5502525316942,23.5502525316942,0.));
#5893=CARTESIAN_POINT('',(27.5502525316942,23.5502525316942,7.5));
#5894=CARTESIAN_POINT('Origin',(23.5502525316942,23.5502525316942,7.5));
#5895=CARTESIAN_POINT('Origin',(23.5502525316942,23.5502525316942,7.5));
#5896=CARTESIAN_POINT('Origin',(-23.5502525316942,23.5502525316942,0.5));
#5897=CARTESIAN_POINT('',(-27.5502525316942,23.5502525316942,0.5));
#5898=CARTESIAN_POINT('',(-19.5502525316942,23.5502525316942,0.5));
#5899=CARTESIAN_POINT('Origin',(-23.5502525316942,23.5502525316942,0.5));
#5900=CARTESIAN_POINT('Origin',(-19.0502525316942,23.5502525316942,0.5));
#5901=CARTESIAN_POINT('Origin',(-23.5502525316942,23.5502525316942,0.5));
#5902=CARTESIAN_POINT('Origin',(-23.5502525316942,23.5502525316942,0.));
#5903=CARTESIAN_POINT('',(-27.5502525316942,23.5502525316942,7.5));
#5904=CARTESIAN_POINT('',(-27.5502525316942,23.5502525316942,0.));
#5905=CARTESIAN_POINT('',(-19.5502525316942,23.5502525316942,7.5));
#5906=CARTESIAN_POINT('Origin',(-23.5502525316942,23.5502525316942,7.5));
#5907=CARTESIAN_POINT('Origin',(-23.5502525316942,23.5502525316942,7.5));
#5908=CARTESIAN_POINT('Origin',(0.,0.,0.5));
#5909=CARTESIAN_POINT('Origin',(20.5,-2.51052593825207E-15,0.5));
#5910=CARTESIAN_POINT('Origin',(0.,0.,0.));
#5911=CARTESIAN_POINT('',(-20.,-2.44929359829471E-15,7.5));
#5912=CARTESIAN_POINT('',(-20.,-2.44929359829471E-15,0.));
#5913=CARTESIAN_POINT('',(20.,-2.44929359829471E-15,7.5));
#5914=CARTESIAN_POINT('Origin',(0.,0.,7.5));
#5915=CARTESIAN_POINT('Origin',(0.,0.,7.5));
#5916=CARTESIAN_POINT('Origin',(-23.5502525316942,-23.5502525316942,0.5));
#5917=CARTESIAN_POINT('',(-27.5502525316942,-23.5502525316942,0.5));
#5918=CARTESIAN_POINT('',(-19.5502525316942,-23.5502525316942,0.5));
#5919=CARTESIAN_POINT('Origin',(-23.5502525316942,-23.5502525316942,0.5));
#5920=CARTESIAN_POINT('Origin',(-19.0502525316942,-23.5502525316942,0.5));
#5921=CARTESIAN_POINT('Origin',(-23.5502525316942,-23.5502525316942,0.5));
#5922=CARTESIAN_POINT('Origin',(-23.5502525316942,-23.5502525316942,0.));
#5923=CARTESIAN_POINT('',(-27.5502525316942,-23.5502525316942,7.5));
#5924=CARTESIAN_POINT('',(-27.5502525316942,-23.5502525316942,0.));
#5925=CARTESIAN_POINT('',(-19.5502525316942,-23.5502525316942,7.5));
#5926=CARTESIAN_POINT('Origin',(-23.5502525316942,-23.5502525316942,7.5));
#5927=CARTESIAN_POINT('Origin',(-23.5502525316942,-23.5502525316942,7.5));
#5928=CARTESIAN_POINT('Origin',(13.5,29.5,7.5));
#5929=CARTESIAN_POINT('',(-26.7928932188135,29.5,8.));
#5930=CARTESIAN_POINT('',(26.7928932188135,29.5,8.));
#5931=CARTESIAN_POINT('',(13.5,29.5,8.));
#5932=CARTESIAN_POINT('',(27.,30.,7.5));
#5933=CARTESIAN_POINT('Origin',(26.7928932188135,29.5,7.5));
#5934=CARTESIAN_POINT('',(13.5,30.,7.5));
#5935=CARTESIAN_POINT('Origin',(-26.7928932188135,29.5,7.5));
#5936=CARTESIAN_POINT('Origin',(28.8964466094067,27.3964466094067,7.5));
#5937=CARTESIAN_POINT('',(29.5,26.7928932188135,8.));
#5938=CARTESIAN_POINT('',(28.8964466094067,27.3964466094067,8.));
#5939=CARTESIAN_POINT('',(30.,27.,7.5));
#5940=CARTESIAN_POINT('Origin',(29.5,26.7928932188135,7.5));
#5941=CARTESIAN_POINT('',(29.25,27.75,7.5));
#5942=CARTESIAN_POINT('Origin',(29.5,-13.5,7.5));
#5943=CARTESIAN_POINT('',(29.5,-26.7928932188135,8.));
#5944=CARTESIAN_POINT('',(29.5,-13.5,8.));
#5945=CARTESIAN_POINT('',(30.,-27.,7.5));
#5946=CARTESIAN_POINT('Origin',(29.5,-26.7928932188135,7.5));
#5947=CARTESIAN_POINT('',(30.,-13.5,7.5));
#5948=CARTESIAN_POINT('Origin',(27.3964466094067,-28.8964466094067,7.5));
#5949=CARTESIAN_POINT('',(26.7928932188135,-29.5,8.));
#5950=CARTESIAN_POINT('',(27.3964466094067,-28.8964466094067,8.));
#5951=CARTESIAN_POINT('Origin',(26.7928932188135,-29.5,7.5));
#5952=CARTESIAN_POINT('',(27.75,-29.25,7.5));
#5953=CARTESIAN_POINT('Origin',(-13.5,-29.5,7.5));
#5954=CARTESIAN_POINT('',(-26.7928932188135,-29.5,8.));
#5955=CARTESIAN_POINT('',(-13.5,-29.5,8.));
#5956=CARTESIAN_POINT('Origin',(-26.7928932188135,-29.5,7.5));
#5957=CARTESIAN_POINT('Origin',(-28.8964466094067,-27.3964466094067,7.5));
#5958=CARTESIAN_POINT('',(-29.5,-26.7928932188135,8.));
#5959=CARTESIAN_POINT('',(-28.8964466094067,-27.3964466094067,8.));
#5960=CARTESIAN_POINT('Origin',(-29.5,-26.7928932188135,7.5));
#5961=CARTESIAN_POINT('Origin',(-29.5,13.5,7.5));
#5962=CARTESIAN_POINT('',(-29.5,26.7928932188135,8.));
#5963=CARTESIAN_POINT('',(-29.5,13.5,8.));
#5964=CARTESIAN_POINT('Origin',(-29.5,26.7928932188135,7.5));
#5965=CARTESIAN_POINT('Origin',(-27.3964466094067,28.8964466094067,7.5));
#5966=CARTESIAN_POINT('',(-27.3964466094067,28.8964466094067,8.));
#5967=CARTESIAN_POINT('Origin',(27.,30.,0.));
#5968=CARTESIAN_POINT('',(27.,30.,0.));
#5969=CARTESIAN_POINT('Origin',(0.,0.,8.));
#5970=CARTESIAN_POINT('',(28.0502525316942,-23.5502525316942,8.));
#5971=CARTESIAN_POINT('Origin',(23.5502525316942,-23.5502525316942,8.));
#5972=CARTESIAN_POINT('',(-19.0502525316942,23.5502525316942,8.));
#5973=CARTESIAN_POINT('Origin',(-23.5502525316942,23.5502525316942,8.));
#5974=CARTESIAN_POINT('',(-19.0502525316942,-23.5502525316942,8.));
#5975=CARTESIAN_POINT('Origin',(-23.5502525316942,-23.5502525316942,8.));
#5976=CARTESIAN_POINT('',(20.5,-2.51052593825207E-15,8.));
#5977=CARTESIAN_POINT('Origin',(0.,0.,8.));
#5978=CARTESIAN_POINT('',(28.0502525316942,23.5502525316942,8.));
#5979=CARTESIAN_POINT('Origin',(23.5502525316942,23.5502525316942,8.));
#5980=CARTESIAN_POINT('Origin',(23.5502525316942,-23.5502525316942,7.5));
#5981=CARTESIAN_POINT('Origin',(28.0502525316942,-23.5502525316942,7.5));
#5982=CARTESIAN_POINT('Origin',(23.5502525316942,23.5502525316942,7.5));
#5983=CARTESIAN_POINT('Origin',(28.0502525316942,23.5502525316942,7.5));
#5984=CARTESIAN_POINT('Origin',(-23.5502525316942,23.5502525316942,7.5));
#5985=CARTESIAN_POINT('Origin',(-19.0502525316942,23.5502525316942,7.5));
#5986=CARTESIAN_POINT('Origin',(0.,0.,7.5));
#5987=CARTESIAN_POINT('Origin',(20.5,-2.51052593825207E-15,7.5));
#5988=CARTESIAN_POINT('Origin',(-23.5502525316942,-23.5502525316942,7.5));
#5989=CARTESIAN_POINT('Origin',(-19.0502525316942,-23.5502525316942,7.5));
#5990=CARTESIAN_POINT('Origin',(30.,27.,0.));
#5991=CARTESIAN_POINT('',(30.,27.,0.));
#5992=CARTESIAN_POINT('Origin',(30.,-27.,0.));
#5993=CARTESIAN_POINT('',(30.,-27.,0.));
#5994=CARTESIAN_POINT('Origin',(27.,-30.,0.));
#5995=CARTESIAN_POINT('',(0.,0.,0.));
#5996=CARTESIAN_POINT('Origin',(20.5,0.,-54.5));
#5997=CARTESIAN_POINT('',(-20.5,-2.51052593825207E-15,-54.5));
#5998=CARTESIAN_POINT('Origin',(0.,0.,-54.5));
#5999=CARTESIAN_POINT('',(-20.,-2.44929359829471E-15,-54.5));
#6000=CARTESIAN_POINT('Origin',(0.,0.,-54.5));
#6001=CARTESIAN_POINT('Origin',(20.,0.,-37.5));
#6002=CARTESIAN_POINT('',(-20.5,-2.51052593825207E-15,-37.5));
#6003=CARTESIAN_POINT('Origin',(0.,0.,-37.5));
#6004=CARTESIAN_POINT('',(20.,-2.44929359829471E-15,-37.5));
#6005=CARTESIAN_POINT('Origin',(0.,0.,-37.5));
#6006=CARTESIAN_POINT('Origin',(23.5502525316942,-23.5502525316942,-54.5));
#6007=CARTESIAN_POINT('',(19.0502525316942,-23.5502525316942,-55.));
#6008=CARTESIAN_POINT('Origin',(23.5502525316942,-23.5502525316942,-55.));
#6009=CARTESIAN_POINT('',(19.5502525316942,-23.5502525316942,-54.5));
#6010=CARTESIAN_POINT('Origin',(19.0502525316942,-23.5502525316942,-54.5));
#6011=CARTESIAN_POINT('Origin',(23.5502525316942,-23.5502525316942,-54.5));
#6012=CARTESIAN_POINT('Origin',(0.,0.,-55.));
#6013=CARTESIAN_POINT('',(26.7928932188135,-29.5,-55.));
#6014=CARTESIAN_POINT('',(29.5,-26.7928932188135,-55.));
#6015=CARTESIAN_POINT('',(27.3964466094067,-28.8964466094067,-55.));
#6016=CARTESIAN_POINT('',(-26.7928932188135,-29.5,-55.));
#6017=CARTESIAN_POINT('',(-13.5,-29.5,-55.));
#6018=CARTESIAN_POINT('',(-29.5,-26.7928932188135,-55.));
#6019=CARTESIAN_POINT('',(-28.8964466094067,-27.3964466094067,-55.));
#6020=CARTESIAN_POINT('',(-29.5,26.7928932188135,-55.));
#6021=CARTESIAN_POINT('',(-29.5,13.5,-55.));
#6022=CARTESIAN_POINT('',(-26.7928932188135,29.5,-55.));
#6023=CARTESIAN_POINT('',(-27.3964466094067,28.8964466094067,-55.));
#6024=CARTESIAN_POINT('',(26.7928932188135,29.5,-55.));
#6025=CARTESIAN_POINT('',(13.5,29.5,-55.));
#6026=CARTESIAN_POINT('',(29.5,26.7928932188135,-55.));
#6027=CARTESIAN_POINT('',(28.8964466094067,27.3964466094067,-55.));
#6028=CARTESIAN_POINT('',(29.5,-13.5,-55.));
#6029=CARTESIAN_POINT('',(-28.0502525316942,23.5502525316942,-55.));
#6030=CARTESIAN_POINT('Origin',(-23.5502525316942,23.5502525316942,-55.));
#6031=CARTESIAN_POINT('',(-20.5,2.51052593825207E-15,-55.));
#6032=CARTESIAN_POINT('Origin',(0.,0.,-55.));
#6033=CARTESIAN_POINT('',(19.0502525316942,23.5502525316942,-55.));
#6034=CARTESIAN_POINT('Origin',(23.5502525316942,23.5502525316942,-55.));
#6035=CARTESIAN_POINT('',(-28.0502525316942,-23.5502525316942,-55.));
#6036=CARTESIAN_POINT('Origin',(-23.5502525316942,-23.5502525316942,-55.));
#6037=CARTESIAN_POINT('Origin',(23.5502525316942,-23.5502525316942,-50.));
#6038=CARTESIAN_POINT('',(19.5502525316942,-23.5502525316942,-37.5));
#6039=CARTESIAN_POINT('',(19.5502525316942,-23.5502525316942,-50.));
#6040=CARTESIAN_POINT('Origin',(23.5502525316942,-23.5502525316942,-37.5));
#6041=CARTESIAN_POINT('Origin',(-23.5502525316942,23.5502525316942,-54.5));
#6042=CARTESIAN_POINT('',(-27.5502525316942,23.5502525316942,-54.5));
#6043=CARTESIAN_POINT('Origin',(-28.0502525316942,23.5502525316942,-54.5));
#6044=CARTESIAN_POINT('Origin',(-23.5502525316942,23.5502525316942,-54.5));
#6045=CARTESIAN_POINT('Origin',(-23.5502525316942,23.5502525316942,-50.));
#6046=CARTESIAN_POINT('',(-27.5502525316942,23.5502525316942,-37.5));
#6047=CARTESIAN_POINT('',(-27.5502525316942,23.5502525316942,-50.));
#6048=CARTESIAN_POINT('',(-19.5502525316942,23.5502525316942,-37.5));
#6049=CARTESIAN_POINT('Origin',(-23.5502525316942,23.5502525316942,-37.5));
#6050=CARTESIAN_POINT('Origin',(-23.5502525316942,23.5502525316942,-37.5));
#6051=CARTESIAN_POINT('Origin',(-23.5502525316942,-23.5502525316942,-54.5));
#6052=CARTESIAN_POINT('',(-27.5502525316942,-23.5502525316942,-54.5));
#6053=CARTESIAN_POINT('Origin',(-28.0502525316942,-23.5502525316942,-54.5));
#6054=CARTESIAN_POINT('Origin',(-23.5502525316942,-23.5502525316942,-54.5));
#6055=CARTESIAN_POINT('Origin',(-23.5502525316942,-23.5502525316942,-50.));
#6056=CARTESIAN_POINT('',(-27.5502525316942,-23.5502525316942,-37.5));
#6057=CARTESIAN_POINT('',(-27.5502525316942,-23.5502525316942,-50.));
#6058=CARTESIAN_POINT('',(-19.5502525316942,-23.5502525316942,-37.5));
#6059=CARTESIAN_POINT('Origin',(-23.5502525316942,-23.5502525316942,-37.5));
#6060=CARTESIAN_POINT('Origin',(-23.5502525316942,-23.5502525316942,-37.5));
#6061=CARTESIAN_POINT('Origin',(0.,0.,-54.5));
#6062=CARTESIAN_POINT('Origin',(-20.5,-2.51052593825207E-15,-54.5));
#6063=CARTESIAN_POINT('Origin',(23.5502525316942,23.5502525316942,-54.5));
#6064=CARTESIAN_POINT('',(19.5502525316942,23.5502525316942,-54.5));
#6065=CARTESIAN_POINT('Origin',(19.0502525316942,23.5502525316942,-54.5));
#6066=CARTESIAN_POINT('Origin',(23.5502525316942,23.5502525316942,-54.5));
#6067=CARTESIAN_POINT('Origin',(23.5502525316942,23.5502525316942,-50.));
#6068=CARTESIAN_POINT('',(19.5502525316942,23.5502525316942,-37.5));
#6069=CARTESIAN_POINT('',(19.5502525316942,23.5502525316942,-50.));
#6070=CARTESIAN_POINT('',(27.5502525316942,23.5502525316942,-37.5));
#6071=CARTESIAN_POINT('Origin',(23.5502525316942,23.5502525316942,-37.5));
#6072=CARTESIAN_POINT('Origin',(23.5502525316942,23.5502525316942,-37.5));
#6073=CARTESIAN_POINT('Origin',(-27.3964466094067,28.8964466094067,-54.5));
#6074=CARTESIAN_POINT('',(-30.,27.,-54.5));
#6075=CARTESIAN_POINT('Origin',(-29.5,26.7928932188135,-54.5));
#6076=CARTESIAN_POINT('',(-27.,30.,-54.5));
#6077=CARTESIAN_POINT('',(-27.75,29.25,-54.5));
#6078=CARTESIAN_POINT('Origin',(-26.7928932188135,29.5,-54.5));
#6079=CARTESIAN_POINT('Origin',(-29.5,13.5,-54.5));
#6080=CARTESIAN_POINT('',(-30.,-27.,-54.5));
#6081=CARTESIAN_POINT('Origin',(-29.5,-26.7928932188135,-54.5));
#6082=CARTESIAN_POINT('',(-30.,13.5,-54.5));
#6083=CARTESIAN_POINT('Origin',(-28.8964466094067,-27.3964466094067,-54.5));
#6084=CARTESIAN_POINT('',(-27.,-30.,-54.5));
#6085=CARTESIAN_POINT('Origin',(-26.7928932188135,-29.5,-54.5));
#6086=CARTESIAN_POINT('',(-29.25,-27.75,-54.5));
#6087=CARTESIAN_POINT('Origin',(27.3964466094067,-28.8964466094067,-54.5));
#6088=CARTESIAN_POINT('',(30.,-27.,-54.5));
#6089=CARTESIAN_POINT('Origin',(29.5,-26.7928932188135,-54.5));
#6090=CARTESIAN_POINT('',(27.,-30.,-54.5));
#6091=CARTESIAN_POINT('',(27.75,-29.25,-54.5));
#6092=CARTESIAN_POINT('Origin',(26.7928932188135,-29.5,-54.5));
#6093=CARTESIAN_POINT('Origin',(29.5,-13.5,-54.5));
#6094=CARTESIAN_POINT('',(30.,27.,-54.5));
#6095=CARTESIAN_POINT('',(30.,-13.5,-54.5));
#6096=CARTESIAN_POINT('Origin',(29.5,26.7928932188135,-54.5));
#6097=CARTESIAN_POINT('Origin',(-13.5,-29.5,-54.5));
#6098=CARTESIAN_POINT('',(-13.5,-30.,-54.5));
#6099=CARTESIAN_POINT('Origin',(28.8964466094067,27.3964466094067,-54.5));
#6100=CARTESIAN_POINT('',(27.,30.,-54.5));
#6101=CARTESIAN_POINT('',(29.25,27.75,-54.5));
#6102=CARTESIAN_POINT('Origin',(26.7928932188135,29.5,-54.5));
#6103=CARTESIAN_POINT('Origin',(13.5,29.5,-54.5));
#6104=CARTESIAN_POINT('',(13.5,30.,-54.5));
#6105=CARTESIAN_POINT('Origin',(-30.,27.,-50.));
#6106=CARTESIAN_POINT('',(-30.,-27.,-37.5));
#6107=CARTESIAN_POINT('',(-30.,-27.,-50.));
#6108=CARTESIAN_POINT('',(-30.,27.,-37.5));
#6109=CARTESIAN_POINT('',(-30.,13.5,-37.5));
#6110=CARTESIAN_POINT('',(-30.,27.,-50.));
#6111=CARTESIAN_POINT('Origin',(-30.,-27.,-50.));
#6112=CARTESIAN_POINT('',(-27.,-30.,-37.5));
#6113=CARTESIAN_POINT('',(-27.,-30.,-50.));
#6114=CARTESIAN_POINT('',(-29.25,-27.75,-37.5));
#6115=CARTESIAN_POINT('Origin',(-27.,-30.,-50.));
#6116=CARTESIAN_POINT('',(27.,-30.,-37.5));
#6117=CARTESIAN_POINT('',(27.,-30.,-50.));
#6118=CARTESIAN_POINT('',(-13.5,-30.,-37.5));
#6119=CARTESIAN_POINT('Origin',(27.,-30.,-50.));
#6120=CARTESIAN_POINT('',(30.,-27.,-37.5));
#6121=CARTESIAN_POINT('',(30.,-27.,-50.));
#6122=CARTESIAN_POINT('',(27.75,-29.25,-37.5));
#6123=CARTESIAN_POINT('Origin',(30.,27.,-50.));
#6124=CARTESIAN_POINT('',(27.,30.,-37.5));
#6125=CARTESIAN_POINT('',(27.,30.,-50.));
#6126=CARTESIAN_POINT('',(30.,27.,-37.5));
#6127=CARTESIAN_POINT('',(29.25,27.75,-37.5));
#6128=CARTESIAN_POINT('',(30.,27.,-50.));
#6129=CARTESIAN_POINT('Origin',(30.,-27.,-50.));
#6130=CARTESIAN_POINT('',(30.,-13.5,-37.5));
#6131=CARTESIAN_POINT('Origin',(27.,30.,-50.));
#6132=CARTESIAN_POINT('',(-27.,30.,-37.5));
#6133=CARTESIAN_POINT('',(-27.,30.,-50.));
#6134=CARTESIAN_POINT('',(13.5,30.,-37.5));
#6135=CARTESIAN_POINT('Origin',(-27.,30.,-50.));
#6136=CARTESIAN_POINT('',(-27.75,29.25,-37.5));
#6137=CARTESIAN_POINT('Origin',(-23.5502525316942,23.5502525316942,-37.5));
#6138=CARTESIAN_POINT('',(-19.0502525316942,23.5502525316942,-37.));
#6139=CARTESIAN_POINT('Origin',(-23.5502525316942,23.5502525316942,-37.));
#6140=CARTESIAN_POINT('Origin',(-19.0502525316942,23.5502525316942,-37.5));
#6141=CARTESIAN_POINT('Origin',(0.,0.,-37.));
#6142=CARTESIAN_POINT('',(26.7928932188135,29.5,-37.));
#6143=CARTESIAN_POINT('',(29.5,26.7928932188135,-37.));
#6144=CARTESIAN_POINT('',(28.8964466094067,27.3964466094067,-37.));
#6145=CARTESIAN_POINT('',(-26.7928932188135,29.5,-37.));
#6146=CARTESIAN_POINT('',(13.5,29.5,-37.));
#6147=CARTESIAN_POINT('',(-29.5,26.7928932188135,-37.));
#6148=CARTESIAN_POINT('',(-27.3964466094067,28.8964466094067,-37.));
#6149=CARTESIAN_POINT('',(-29.5,-26.7928932188135,-37.));
#6150=CARTESIAN_POINT('',(-29.5,13.5,-37.));
#6151=CARTESIAN_POINT('',(-26.7928932188135,-29.5,-37.));
#6152=CARTESIAN_POINT('',(-28.8964466094067,-27.3964466094067,-37.));
#6153=CARTESIAN_POINT('',(26.7928932188135,-29.5,-37.));
#6154=CARTESIAN_POINT('',(-13.5,-29.5,-37.));
#6155=CARTESIAN_POINT('',(29.5,-26.7928932188135,-37.));
#6156=CARTESIAN_POINT('',(27.3964466094067,-28.8964466094067,-37.));
#6157=CARTESIAN_POINT('',(29.5,-13.5,-37.));
#6158=CARTESIAN_POINT('',(-19.0502525316942,-23.5502525316942,-37.));
#6159=CARTESIAN_POINT('Origin',(-23.5502525316942,-23.5502525316942,-37.));
#6160=CARTESIAN_POINT('',(28.0502525316942,23.5502525316942,-37.));
#6161=CARTESIAN_POINT('Origin',(23.5502525316942,23.5502525316942,-37.));
#6162=CARTESIAN_POINT('',(19.0502525316942,-23.5502525316942,-37.));
#6163=CARTESIAN_POINT('Origin',(23.5502525316942,-23.5502525316942,-37.));
#6164=CARTESIAN_POINT('',(20.5,-2.51052593825207E-15,-37.));
#6165=CARTESIAN_POINT('Origin',(0.,0.,-37.));
#6166=CARTESIAN_POINT('Origin',(-23.5502525316942,-23.5502525316942,-37.5));
#6167=CARTESIAN_POINT('Origin',(-19.0502525316942,-23.5502525316942,-37.5));
#6168=CARTESIAN_POINT('Origin',(0.,0.,-37.5));
#6169=CARTESIAN_POINT('Origin',(20.5,-2.51052593825207E-15,-37.5));
#6170=CARTESIAN_POINT('Origin',(23.5502525316942,23.5502525316942,-37.5));
#6171=CARTESIAN_POINT('Origin',(28.0502525316942,23.5502525316942,-37.5));
#6172=CARTESIAN_POINT('Origin',(-28.8964466094067,-27.3964466094067,-37.5));
#6173=CARTESIAN_POINT('Origin',(-29.5,-26.7928932188135,-37.5));
#6174=CARTESIAN_POINT('Origin',(-26.7928932188135,-29.5,-37.5));
#6175=CARTESIAN_POINT('Origin',(-29.5,13.5,-37.5));
#6176=CARTESIAN_POINT('Origin',(-29.5,26.7928932188135,-37.5));
#6177=CARTESIAN_POINT('Origin',(-27.3964466094067,28.8964466094067,-37.5));
#6178=CARTESIAN_POINT('Origin',(-26.7928932188135,29.5,-37.5));
#6179=CARTESIAN_POINT('Origin',(28.8964466094067,27.3964466094067,-37.5));
#6180=CARTESIAN_POINT('Origin',(29.5,26.7928932188135,-37.5));
#6181=CARTESIAN_POINT('Origin',(26.7928932188135,29.5,-37.5));
#6182=CARTESIAN_POINT('Origin',(29.5,-13.5,-37.5));
#6183=CARTESIAN_POINT('Origin',(29.5,-26.7928932188135,-37.5));
#6184=CARTESIAN_POINT('Origin',(13.5,29.5,-37.5));
#6185=CARTESIAN_POINT('Origin',(27.3964466094067,-28.8964466094067,-37.5));
#6186=CARTESIAN_POINT('Origin',(26.7928932188135,-29.5,-37.5));
#6187=CARTESIAN_POINT('Origin',(-13.5,-29.5,-37.5));
#6188=CARTESIAN_POINT('Origin',(23.5502525316942,-23.5502525316942,-37.5));
#6189=CARTESIAN_POINT('Origin',(19.0502525316942,-23.5502525316942,-37.5));
#6190=CARTESIAN_POINT('Origin',(0.,0.,-46.));
#6191=CARTESIAN_POINT('',(-20.5,-2.51052593825207E-15,-46.));
#6192=CARTESIAN_POINT('',(0.,0.,0.));
#6193=CARTESIAN_POINT('Origin',(0.,0.,4.));
#6194=CARTESIAN_POINT('',(-19.5,-2.38806125833734E-15,2.9));
#6195=CARTESIAN_POINT('Origin',(0.,0.,2.9));
#6196=CARTESIAN_POINT('',(-19.5,-2.38806125833734E-15,5.1));
#6197=CARTESIAN_POINT('',(-19.5,-2.38806125833734E-15,4.));
#6198=CARTESIAN_POINT('Origin',(0.,0.,5.1));
#6199=CARTESIAN_POINT('Origin',(0.,0.,2.9));
#6200=CARTESIAN_POINT('',(-19.9,-2.43704713030323E-15,2.5));
#6201=CARTESIAN_POINT('Origin',(0.,0.,2.5));
#6202=CARTESIAN_POINT('Origin',(-19.9,-2.43704713030323E-15,2.9));
#6203=CARTESIAN_POINT('Origin',(20.1,0.,2.5));
#6204=CARTESIAN_POINT('',(-20.1,-2.46154006628618E-15,2.5));
#6205=CARTESIAN_POINT('Origin',(0.,0.,2.5));
#6206=CARTESIAN_POINT('Origin',(0.,0.,2.9));
#6207=CARTESIAN_POINT('',(-20.5,-2.51052593825207E-15,2.9));
#6208=CARTESIAN_POINT('Origin',(0.,0.,2.9));
#6209=CARTESIAN_POINT('Origin',(-20.1,-2.46154006628618E-15,2.9));
#6210=CARTESIAN_POINT('Origin',(0.,0.,4.));
#6211=CARTESIAN_POINT('',(-20.5,-2.51052593825207E-15,5.1));
#6212=CARTESIAN_POINT('Origin',(0.,0.,5.1));
#6213=CARTESIAN_POINT('',(-20.5,-2.51052593825207E-15,4.));
#6214=CARTESIAN_POINT('Origin',(0.,0.,5.1));
#6215=CARTESIAN_POINT('',(-20.1,-2.46154006628618E-15,5.5));
#6216=CARTESIAN_POINT('Origin',(0.,0.,5.5));
#6217=CARTESIAN_POINT('Origin',(-20.1,-2.46154006628618E-15,5.1));
#6218=CARTESIAN_POINT('Origin',(19.9,0.,5.5));
#6219=CARTESIAN_POINT('',(-19.9,-2.43704713030323E-15,5.5));
#6220=CARTESIAN_POINT('Origin',(0.,0.,5.5));
#6221=CARTESIAN_POINT('Origin',(0.,0.,5.1));
#6222=CARTESIAN_POINT('Origin',(-19.9,-2.43704713030323E-15,5.1));
#6223=CARTESIAN_POINT('',(0.,0.,0.));
#6224=CARTESIAN_POINT('Origin',(-23.5502525316942,23.5502525316942,-77.3107734492734));
#6225=CARTESIAN_POINT('',(-22.0750360153461,26.4155367745563,-74.34623438385));
#6226=CARTESIAN_POINT('',(-22.0750360153461,26.4155367745563,-74.5928284611549));
#6227=CARTESIAN_POINT('',(-22.0750360153461,26.4155367745563,-77.3107734492734));
#6228=CARTESIAN_POINT('',(-25.4217763663954,20.9266069575655,-74.9999352075484));
#6229=CARTESIAN_POINT('Ctrl Pts',(-25.4217763663954,20.9266069575655,-74.9999352075484));
#6230=CARTESIAN_POINT('Ctrl Pts',(-25.3415113023851,20.8693515180845,-74.9938139384461));
#6231=CARTESIAN_POINT('Ctrl Pts',(-25.258468139995,20.8156772001763,-74.9876926693437));
#6232=CARTESIAN_POINT('Ctrl Pts',(-25.1730031022917,20.7658678333945,-74.9815714002414));
#6233=CARTESIAN_POINT('Ctrl Pts',(-25.087650312619,20.7161238852152,-74.9754581706886));
#6234=CARTESIAN_POINT('Ctrl Pts',(-24.9998823463237,20.6702350229595,-74.9693449411357));
#6235=CARTESIAN_POINT('Ctrl Pts',(-24.910086288991,20.6284432095419,-74.9632317115829));
#6236=CARTESIAN_POINT('Ctrl Pts',(-24.8183856393031,20.5857649833941,-74.9569888192073));
#6237=CARTESIAN_POINT('Ctrl Pts',(-24.7245702542372,20.5473598737791,-74.9507459268316));
#6238=CARTESIAN_POINT('Ctrl Pts',(-24.629081335484,20.5134374279031,-74.944503034456));
#6239=CARTESIAN_POINT('Ctrl Pts',(-24.5357311202979,20.4802747566371,-74.9383999666418));
#6240=CARTESIAN_POINT('Ctrl Pts',(-24.4407819924413,20.4513962064306,-74.9322968988277));
#6241=CARTESIAN_POINT('Ctrl Pts',(-24.3446673004952,20.4269493543496,-74.9261938310135));
#6242=CARTESIAN_POINT('Ctrl Pts',(-24.248581729055,20.4025099090935,-74.9200926122863));
#6243=CARTESIAN_POINT('Ctrl Pts',(-24.1513317232489,20.3824996035349,-74.9139913935591));
#6244=CARTESIAN_POINT('Ctrl Pts',(-24.0533648896118,20.3670158898765,-74.9078901748319));
#6245=CARTESIAN_POINT('Ctrl Pts',(-23.9554004768615,20.3515325588407,-74.9017891068737));
#6246=CARTESIAN_POINT('Ctrl Pts',(-23.8567197084106,20.34057566546,-74.8956880389155));
#6247=CARTESIAN_POINT('Ctrl Pts',(-23.7577783523882,20.3341911833606,-74.8895869709572));
#6248=CARTESIAN_POINT('Ctrl Pts',(-23.654820760349,20.3275475418157,-74.8832382479248));
#6249=CARTESIAN_POINT('Ctrl Pts',(-23.5515814925213,20.3258554514295,-74.8768895248922));
#6250=CARTESIAN_POINT('Ctrl Pts',(-23.4485758461978,20.3291068637483,-74.8705408018598));
#6251=CARTESIAN_POINT('Ctrl Pts',(-23.3494534047172,20.3322357012326,-74.8644314190276));
#6252=CARTESIAN_POINT('Ctrl Pts',(-23.2505477343847,20.3399419342038,-74.8583220361954));
#6253=CARTESIAN_POINT('Ctrl Pts',(-23.1523126956406,20.3521653769435,-74.8522126533633));
#6254=CARTESIAN_POINT('Ctrl Pts',(-23.0540112475345,20.3643970830385,-74.8460991404343));
#6255=CARTESIAN_POINT('Ctrl Pts',(-22.9563817675357,20.3811519995275,-74.8399856275054));
#6256=CARTESIAN_POINT('Ctrl Pts',(-22.8598671888174,20.4023189808007,-74.8338721145765));
#6257=CARTESIAN_POINT('Ctrl Pts',(-22.7632121778204,20.4235167608139,-74.8277497062603));
#6258=CARTESIAN_POINT('Ctrl Pts',(-22.6676757279364,20.4491392935652,-74.8216272979441));
#6259=CARTESIAN_POINT('Ctrl Pts',(-22.5736844908171,20.479025997549,-74.8155048896279));
#6260=CARTESIAN_POINT('Ctrl Pts',(-22.5629248082052,20.4824472893528,-74.8148040246077));
#6261=CARTESIAN_POINT('Ctrl Pts',(-22.5521853514869,20.4859244104502,-74.8141031595875));
#6262=CARTESIAN_POINT('Ctrl Pts',(-22.5414667417776,20.4894570807432,-74.8134022945673));
#6263=CARTESIAN_POINT('Ctrl Pts',(-22.4469052689154,20.5206229236182,-74.8072191392529));
#6264=CARTESIAN_POINT('Ctrl Pts',(-22.3536296772483,20.5562276387414,-74.8010359839384));
#6265=CARTESIAN_POINT('Ctrl Pts',(-22.2620859036837,20.5961461861169,-74.794852828624));
#6266=CARTESIAN_POINT('Ctrl Pts',(-22.1706627851161,20.6360121207146,-74.7886778227287));
#6267=CARTESIAN_POINT('Ctrl Pts',(-22.0809673405844,20.6801804139711,-74.7825028168334));
#6268=CARTESIAN_POINT('Ctrl Pts',(-21.9934295894148,20.7284765149111,-74.7763278109382));
#6269=CARTESIAN_POINT('Ctrl Pts',(-21.9059816187024,20.7767230824101,-74.7701591382517));
#6270=CARTESIAN_POINT('Ctrl Pts',(-21.820687318068,20.8290888320475,-74.7639904655652));
#6271=CARTESIAN_POINT('Ctrl Pts',(-21.7379551100751,20.8853518547284,-74.7578217928787));
#6272=CARTESIAN_POINT('Ctrl Pts',(-21.6552799289935,20.9415760955795,-74.7516573722285));
#6273=CARTESIAN_POINT('Ctrl Pts',(-21.5751636860409,21.0016920258799,-74.7454929515783));
#6274=CARTESIAN_POINT('Ctrl Pts',(-21.4979878736985,21.0654331547491,-74.7393285309281));
#6275=CARTESIAN_POINT('Ctrl Pts',(-21.4208394097242,21.129151696025,-74.7331662947297));
#6276=CARTESIAN_POINT('Ctrl Pts',(-21.3466296389297,21.196492607828,-74.7270040585313));
#6277=CARTESIAN_POINT('Ctrl Pts',(-21.2757081471388,21.2671481965427,-74.720841822333));
#6278=CARTESIAN_POINT('Ctrl Pts',(-21.2047930105908,21.337797453842,-74.7146801383298));
#6279=CARTESIAN_POINT('Ctrl Pts',(-21.1371658735867,21.4117604921122,-74.7085184543267));
#6280=CARTESIAN_POINT('Ctrl Pts',(-21.073139799602,21.4886924246377,-74.7023567703235));
#6281=CARTESIAN_POINT('Ctrl Pts',(-21.0091025120195,21.5656378311075,-74.6961940071561));
#6282=CARTESIAN_POINT('Ctrl Pts',(-20.9486678171902,21.6455528323533,-74.6900312439888));
#6283=CARTESIAN_POINT('Ctrl Pts',(-20.8921081564378,21.728059884691,-74.6838684808214));
#6284=CARTESIAN_POINT('Ctrl Pts',(-20.8354870738039,21.8106565369009,-74.6776990251014));
#6285=CARTESIAN_POINT('Ctrl Pts',(-20.7827496734932,21.895850503713,-74.6715295693814));
#6286=CARTESIAN_POINT('Ctrl Pts',(-20.7341246787443,21.9832357869402,-74.6653601136613));
#6287=CARTESIAN_POINT('Ctrl Pts',(-20.6854719686393,22.0706708781775,-74.6591871414646));
#6288=CARTESIAN_POINT('Ctrl Pts',(-20.640936524947,22.1602993860099,-74.6530141692678));
#6289=CARTESIAN_POINT('Ctrl Pts',(-20.6006998362459,22.2516931532777,-74.6468411970711));
#6290=CARTESIAN_POINT('Ctrl Pts',(-20.5603959140281,22.3432396350101,-74.6406579101432));
#6291=CARTESIAN_POINT('Ctrl Pts',(-20.5244052504831,22.4365568643179,-74.6344746232152));
#6292=CARTESIAN_POINT('Ctrl Pts',(-20.4928602248663,22.5311991255129,-74.6282913362873));
#6293=CARTESIAN_POINT('Ctrl Pts',(-20.4694334833756,22.6014846853995,-74.6236993519223));
#6294=CARTESIAN_POINT('Ctrl Pts',(-20.448457569277,22.6725006748828,-74.6191073675574));
#6295=CARTESIAN_POINT('Ctrl Pts',(-20.4299684107723,22.7440611355466,-74.6145153831924));
#6296=CARTESIAN_POINT('Ctrl Pts',(-20.4051527281407,22.8401077825774,-74.6083521374925));
#6297=CARTESIAN_POINT('Ctrl Pts',(-20.3847309724908,22.9374751239296,-74.6021888917926));
#6298=CARTESIAN_POINT('Ctrl Pts',(-20.3688412132802,23.0357240236724,-74.5960256460927));
#6299=CARTESIAN_POINT('Ctrl Pts',(-20.3529733103834,23.1338377823624,-74.5898708779178));
#6300=CARTESIAN_POINT('Ctrl Pts',(-20.3416250837045,23.2328302632332,-74.583716109743));
#6301=CARTESIAN_POINT('Ctrl Pts',(-20.3348844607828,23.3322485614009,-74.5775613415682));
#6302=CARTESIAN_POINT('Ctrl Pts',(-20.328151101818,23.4315597225525,-74.5714132060103));
#6303=CARTESIAN_POINT('Ctrl Pts',(-20.3260155052307,23.5312953564624,-74.5652650704526));
#6304=CARTESIAN_POINT('Ctrl Pts',(-20.3285141415369,23.6309947628186,-74.5591169348947));
#6305=CARTESIAN_POINT('Ctrl Pts',(-20.33101090078,23.7306192714827,-74.5529734180321));
#6306=CARTESIAN_POINT('Ctrl Pts',(-20.3381349607413,23.8302071723837,-74.5468299011694));
#6307=CARTESIAN_POINT('Ctrl Pts',(-20.3498707423274,23.9292960183673,-74.5406863843068));
#6308=CARTESIAN_POINT('Ctrl Pts',(-20.3616019334391,24.0283461055516,-74.534545270493));
#6309=CARTESIAN_POINT('Ctrl Pts',(-20.3779412109984,24.126897093364,-74.5284041566791));
#6310=CARTESIAN_POINT('Ctrl Pts',(-20.3988210640403,24.2244908183412,-74.5222630428653));
#6311=CARTESIAN_POINT('Ctrl Pts',(-20.4196983797654,24.3220726837427,-74.5161226753188));
#6312=CARTESIAN_POINT('Ctrl Pts',(-20.4451150829239,24.4186970913747,-74.5099823077723));
#6313=CARTESIAN_POINT('Ctrl Pts',(-20.4749525820067,24.513916260363,-74.5038419402258));
#6314=CARTESIAN_POINT('Ctrl Pts',(-20.5047945003841,24.6091495324626,-74.4977006632165));
#6315=CARTESIAN_POINT('Ctrl Pts',(-20.5390583847173,24.7029767366334,-74.4915593862072));
#6316=CARTESIAN_POINT('Ctrl Pts',(-20.5775761475754,24.7949664256483,-74.4854181091979));
#6317=CARTESIAN_POINT('Ctrl Pts',(-20.6161350597049,24.8870543890281,-74.4792702713436));
#6318=CARTESIAN_POINT('Ctrl Pts',(-20.6589567566051,24.9773005144231,-74.4731224334892));
#6319=CARTESIAN_POINT('Ctrl Pts',(-20.7058255140535,25.0652946115769,-74.4669745956349));
#6320=CARTESIAN_POINT('Ctrl Pts',(-20.7527202648339,25.1533375101054,-74.4608233482003));
#6321=CARTESIAN_POINT('Ctrl Pts',(-20.8036663231178,25.2391255185451,-74.4546721007656));
#6322=CARTESIAN_POINT('Ctrl Pts',(-20.8584037256175,25.3222761115947,-74.448520853331));
#6323=CARTESIAN_POINT('Ctrl Pts',(-20.9132333607873,25.4055668136167,-74.4423592410279));
#6324=CARTESIAN_POINT('Ctrl Pts',(-20.9718668443349,25.4862108707842,-74.4361976287249));
#6325=CARTESIAN_POINT('Ctrl Pts',(-21.0340028298801,25.5638575080042,-74.4300360164218));
#6326=CARTESIAN_POINT('Ctrl Pts',(-21.0824331724179,25.624377240724,-74.4252335015537));
#6327=CARTESIAN_POINT('Ctrl Pts',(-21.1329904450727,25.6830766640724,-74.4204309866857));
#6328=CARTESIAN_POINT('Ctrl Pts',(-21.1855169164876,25.7398056899147,-74.4156284718176));
#6329=CARTESIAN_POINT('Ctrl Pts',(-21.2530294424229,25.8127197792358,-74.4094557763966));
#6330=CARTESIAN_POINT('Ctrl Pts',(-21.3240358231561,25.8826362572171,-74.4032830809755));
#6331=CARTESIAN_POINT('Ctrl Pts',(-21.3982393509863,25.9492016417337,-74.3971103855545));
#6332=CARTESIAN_POINT('Ctrl Pts',(-21.4723549916283,26.0156881857337,-74.390945001118));
#6333=CARTESIAN_POINT('Ctrl Pts',(-21.5496599390032,26.0788312316746,-74.3847796166815));
#6334=CARTESIAN_POINT('Ctrl Pts',(-21.629818783366,26.1383119940679,-74.378614232245));
#6335=CARTESIAN_POINT('Ctrl Pts',(-21.709889671605,26.1977274898354,-74.3724556129175));
#6336=CARTESIAN_POINT('Ctrl Pts',(-21.7928078831468,26.2534884358914,-74.3662969935899));
#6337=CARTESIAN_POINT('Ctrl Pts',(-21.878203809864,26.3053152595329,-74.3601383742624));
#6338=CARTESIAN_POINT('Ctrl Pts',(-21.9424684381944,26.3443174893453,-74.3555037107916));
#6339=CARTESIAN_POINT('Ctrl Pts',(-22.008135510676,26.3810924677873,-74.3508690473208));
#6340=CARTESIAN_POINT('Ctrl Pts',(-22.0750360153461,26.4155367745563,-74.34623438385));
#6341=CARTESIAN_POINT('',(-21.6786659999551,20.9266516823436,-75.));
#6342=CARTESIAN_POINT('Origin',(-23.5502525316942,23.5502525316942,-75.));
#6343=CARTESIAN_POINT('Ctrl Pts',(-21.6786659999559,20.9266516823431,-75.));
#6344=CARTESIAN_POINT('Ctrl Pts',(-21.5953389643838,20.9860943210909,-74.9936814370945));
#6345=CARTESIAN_POINT('Ctrl Pts',(-21.5147913918717,21.049549467126,-74.9873628741889));
#6346=CARTESIAN_POINT('Ctrl Pts',(-21.4374147601277,21.1167295477177,-74.9810443112834));
#6347=CARTESIAN_POINT('Ctrl Pts',(-21.360082230324,21.1838713380423,-74.974729349735));
#6348=CARTESIAN_POINT('Ctrl Pts',(-21.2859173479357,21.2547335710304,-74.9684143881866));
#6349=CARTESIAN_POINT('Ctrl Pts',(-21.2152787784318,21.3289882218752,-74.9620994266382));
#6350=CARTESIAN_POINT('Ctrl Pts',(-21.1446641252583,21.4032177320811,-74.9557866031669));
#6351=CARTESIAN_POINT('Ctrl Pts',(-21.0775736858381,21.4808370797315,-74.9494737796956));
#6352=CARTESIAN_POINT('Ctrl Pts',(-21.0143290622971,21.5614816248623,-74.9431609562242));
#6353=CARTESIAN_POINT('Ctrl Pts',(-20.951073264801,21.6421404181374,-74.9368470174137));
#6354=CARTESIAN_POINT('Ctrl Pts',(-20.891664896588,21.7258251629485,-74.9305330786033));
#6355=CARTESIAN_POINT('Ctrl Pts',(-20.836384932994,21.812138548313,-74.9242191397928));
#6356=CARTESIAN_POINT('Ctrl Pts',(-20.7810964622985,21.8984652165505,-74.9179042293225));
#6357=CARTESIAN_POINT('Ctrl Pts',(-20.7299378798827,21.987420989795,-74.9115893188522));
#6358=CARTESIAN_POINT('Ctrl Pts',(-20.6831459758555,22.0785808427749,-74.9052744083819));
#6359=CARTESIAN_POINT('Ctrl Pts',(-20.6363370244541,22.1697739074002,-74.8989571972435));
#6360=CARTESIAN_POINT('Ctrl Pts',(-20.5938981036181,22.2631722901541,-74.8926399861051));
#6361=CARTESIAN_POINT('Ctrl Pts',(-20.5560190413555,22.3583283026284,-74.8863227749666));
#6362=CARTESIAN_POINT('Ctrl Pts',(-20.5181182037228,22.4535390170214,-74.8800019322808));
#6363=CARTESIAN_POINT('Ctrl Pts',(-20.4847825930215,22.5505089967735,-74.873681089595));
#6364=CARTESIAN_POINT('Ctrl Pts',(-20.4561528862024,22.6487732217445,-74.8673602469092));
#6365=CARTESIAN_POINT('Ctrl Pts',(-20.4274806993935,22.7471832485325,-74.8610300255268));
#6366=CARTESIAN_POINT('Ctrl Pts',(-20.4035284747333,22.8468909664517,-74.8546998041444));
#6367=CARTESIAN_POINT('Ctrl Pts',(-20.3843863356202,22.9474185652856,-74.848369582762));
#6368=CARTESIAN_POINT('Ctrl Pts',(-20.3652284999638,23.0480285966944,-74.8420341706017));
#6369=CARTESIAN_POINT('Ctrl Pts',(-20.3508886683515,23.1494594485779,-74.8356987584413));
#6370=CARTESIAN_POINT('Ctrl Pts',(-20.3414051432903,23.2512274484091,-74.8293633462809));
#6371=CARTESIAN_POINT('Ctrl Pts',(-20.3319048778812,23.3531750894307,-74.8230167508313));
#6372=CARTESIAN_POINT('Ctrl Pts',(-20.3272780627577,23.455460663043,-74.8166701553816));
#6373=CARTESIAN_POINT('Ctrl Pts',(-20.3275109058534,23.5575993386909,-74.8103235599319));
#6374=CARTESIAN_POINT('Ctrl Pts',(-20.3276235433911,23.6070087871021,-74.8072534028297));
#6375=CARTESIAN_POINT('Ctrl Pts',(-20.3288726238348,23.6563839188311,-74.8041832457274));
#6376=CARTESIAN_POINT('Ctrl Pts',(-20.3312522444282,23.7056703977242,-74.8011130886251));
#6377=CARTESIAN_POINT('Ctrl Pts',(-20.3359855990695,23.803707195804,-74.7950061729219));
#6378=CARTESIAN_POINT('Ctrl Pts',(-20.3452120687348,23.9017381762126,-74.7888992572187));
#6379=CARTESIAN_POINT('Ctrl Pts',(-20.3589418227391,23.9993110149775,-74.7827923415155));
#6380=CARTESIAN_POINT('Ctrl Pts',(-20.3726508265874,24.0967363892186,-74.7766946553625));
#6381=CARTESIAN_POINT('Ctrl Pts',(-20.390849534989,24.1937045619621,-74.7705969692095));
#6382=CARTESIAN_POINT('Ctrl Pts',(-20.4134961449647,24.2897638113998,-74.7644992830566));
#6383=CARTESIAN_POINT('Ctrl Pts',(-20.4361155854473,24.3857078170495,-74.7584089123933));
#6384=CARTESIAN_POINT('Ctrl Pts',(-20.4631722242813,24.480744636249,-74.75231854173));
#6385=CARTESIAN_POINT('Ctrl Pts',(-20.4945726794429,24.5744293733799,-74.7462281710667));
#6386=CARTESIAN_POINT('Ctrl Pts',(-20.5259451041581,24.6680304803537,-74.7401432371338));
#6387=CARTESIAN_POINT('Ctrl Pts',(-20.5616534978379,24.7602814841342,-74.7340583032009));
#6388=CARTESIAN_POINT('Ctrl Pts',(-20.6015540524192,24.850750452039,-74.727973369268));
#6389=CARTESIAN_POINT('Ctrl Pts',(-20.6414356065688,24.941176339103,-74.7218913329482));
#6390=CARTESIAN_POINT('Ctrl Pts',(-20.6855051785528,25.0298214690489,-74.7158092966284));
#6391=CARTESIAN_POINT('Ctrl Pts',(-20.7335703639388,25.1162726874868,-74.7097272603086));
#6392=CARTESIAN_POINT('Ctrl Pts',(-20.7816261967079,25.2027070840792,-74.7036464074432));
#6393=CARTESIAN_POINT('Ctrl Pts',(-20.8336758822721,25.2869480285228,-74.6975655545778));
#6394=CARTESIAN_POINT('Ctrl Pts',(-20.8894810127551,25.3686068663888,-74.6914847017125));
#6395=CARTESIAN_POINT('Ctrl Pts',(-20.9452910002887,25.4502728115065,-74.6854033195945));
#6396=CARTESIAN_POINT('Ctrl Pts',(-21.0048568299811,25.5293558370004,-74.6793219374765));
#6397=CARTESIAN_POINT('Ctrl Pts',(-21.0678973721169,25.6054971458995,-74.6732405553586));
#6398=CARTESIAN_POINT('Ctrl Pts',(-21.1310034071258,25.6817175580694,-74.6671528552875));
#6399=CARTESIAN_POINT('Ctrl Pts',(-21.1975910790742,25.7549898072669,-74.6610651552165));
#6400=CARTESIAN_POINT('Ctrl Pts',(-21.2673397998154,25.8249892243964,-74.6549774551454));
#6401=CARTESIAN_POINT('Ctrl Pts',(-21.3371248324939,25.8950250839785,-74.648886585752));
#6402=CARTESIAN_POINT('Ctrl Pts',(-21.4100738611773,25.961784419933,-74.6427957163585));
#6403=CARTESIAN_POINT('Ctrl Pts',(-21.4858320410197,26.0249819310797,-74.6367048469651));
#6404=CARTESIAN_POINT('Ctrl Pts',(-21.5617220540533,26.0882894175399,-74.6306033783366));
#6405=CARTESIAN_POINT('Ctrl Pts',(-21.6404306276229,26.148022430094,-74.6245019097082));
#6406=CARTESIAN_POINT('Ctrl Pts',(-21.721572609624,26.2039381395079,-74.6184004410798));
#6407=CARTESIAN_POINT('Ctrl Pts',(-21.7932718405507,26.2533467595936,-74.6130090198033));
#6408=CARTESIAN_POINT('Ctrl Pts',(-21.8668704763583,26.2997753984595,-74.6076175985267));
#6409=CARTESIAN_POINT('Ctrl Pts',(-21.9420880268178,26.3430870215549,-74.6022261772502));
#6410=CARTESIAN_POINT('Ctrl Pts',(-21.9857916038119,26.3682523299587,-74.5990936052184));
#6411=CARTESIAN_POINT('Ctrl Pts',(-22.0301241723035,26.3924135214964,-74.5959610331866));
#6412=CARTESIAN_POINT('Ctrl Pts',(-22.0750360153461,26.4155367745563,-74.5928284611549));
#6413=CARTESIAN_POINT('Origin',(-23.5502525316942,23.5502525316942,-77.3107734492734));
#6414=CARTESIAN_POINT('',(-22.0750359288953,26.4155367300463,-73.0942273918946));
#6415=CARTESIAN_POINT('',(-22.0750360358082,26.4155367850914,-73.3444460357026));
#6416=CARTESIAN_POINT('',(-22.0750360153461,26.4155367745563,-77.3107734492734));
#6417=CARTESIAN_POINT('',(-26.7730020387288,23.5520350602361,-73.9392265507638));
#6418=CARTESIAN_POINT('Ctrl Pts',(-22.0750359288982,26.4155367300479,-73.0942273918944));
#6419=CARTESIAN_POINT('Ctrl Pts',(-21.9758156807267,26.3644523184142,-73.1006565431777));
#6420=CARTESIAN_POINT('Ctrl Pts',(-21.8791677413006,26.3081726902462,-73.107227114123));
#6421=CARTESIAN_POINT('Ctrl Pts',(-21.7683929477152,26.2356784042351,-73.1152329722461));
#6422=CARTESIAN_POINT('Ctrl Pts',(-21.7513902192451,26.2243187322248,-73.1164754871717));
#6423=CARTESIAN_POINT('Ctrl Pts',(-21.7293242957989,26.2092706067793,-73.1181064454393));
#6424=CARTESIAN_POINT('Ctrl Pts',(-21.7241618682612,26.2057279414766,-73.1184893475809));
#6425=CARTESIAN_POINT('Ctrl Pts',(-21.7162255886803,26.200247660599,-73.1190800573103));
#6426=CARTESIAN_POINT('Ctrl Pts',(-21.7134443895898,26.1983206690126,-73.11928745924));
#6427=CARTESIAN_POINT('Ctrl Pts',(-21.7079761780451,26.1945191848645,-73.119696016041));
#6428=CARTESIAN_POINT('Ctrl Pts',(-21.7052889786307,26.1926449673525,-73.1198971602259));
#6429=CARTESIAN_POINT('Ctrl Pts',(-21.6993781652064,26.1885089917925,-73.1203404195727));
#6430=CARTESIAN_POINT('Ctrl Pts',(-21.6961558329221,26.1862454188536,-73.1205826041859));
#6431=CARTESIAN_POINT('Ctrl Pts',(-21.6894883047369,26.181543444799,-73.1210848430545));
#6432=CARTESIAN_POINT('Ctrl Pts',(-21.6860437358896,26.1791041713051,-73.1213449306176));
#6433=CARTESIAN_POINT('Ctrl Pts',(-21.6772515691842,26.1728520230083,-73.122010393652));
#6434=CARTESIAN_POINT('Ctrl Pts',(-21.6719108358474,26.1690295687906,-73.1224161386826));
#6435=CARTESIAN_POINT('Ctrl Pts',(-21.6565573532798,26.1579696884056,-73.1235869659269));
#6436=CARTESIAN_POINT('Ctrl Pts',(-21.6465745721204,26.1506910365506,-73.124353645096));
#6437=CARTESIAN_POINT('Ctrl Pts',(-21.5498283666167,26.0792957421229,-73.1318371002061));
#6438=CARTESIAN_POINT('Ctrl Pts',(-21.4663035116653,26.0109248873183,-73.1387210661691));
#6439=CARTESIAN_POINT('Ctrl Pts',(-21.1718756290592,25.744157415911,-73.1646304836934));
#6440=CARTESIAN_POINT('Ctrl Pts',(-20.984549395833,25.5218057605228,-73.1846172929653));
#6441=CARTESIAN_POINT('Ctrl Pts',(-20.7758346866239,25.193034785017,-73.2104771321748));
#6442=CARTESIAN_POINT('Ctrl Pts',(-20.7261675010089,25.1061048092495,-73.216998319401));
#6443=CARTESIAN_POINT('Ctrl Pts',(-20.6776338495075,25.0111503905604,-73.2236846544647));
#6444=CARTESIAN_POINT('Ctrl Pts',(-20.6746643105732,25.0052965281475,-73.224095135855));
#6445=CARTESIAN_POINT('Ctrl Pts',(-20.6705875463504,24.9971987625241,-73.2246605404268));
#6446=CARTESIAN_POINT('Ctrl Pts',(-20.6694650446622,24.9949626331997,-73.224816417652));
#6447=CARTESIAN_POINT('Ctrl Pts',(-20.6675455286312,24.991127643746,-73.2250833101893));
#6448=CARTESIAN_POINT('Ctrl Pts',(-20.6667472398382,24.9895294285814,-73.2251944060458));
#6449=CARTESIAN_POINT('Ctrl Pts',(-20.6651907683962,24.9864068002571,-73.2254112117154));
#6450=CARTESIAN_POINT('Ctrl Pts',(-20.6644324668646,24.9848824542151,-73.2255169287173));
#6451=CARTESIAN_POINT('Ctrl Pts',(-20.6625988114931,24.9811890836554,-73.2257727856187));
#6452=CARTESIAN_POINT('Ctrl Pts',(-20.6615246907353,24.9790194421771,-73.2259228472739));
#6453=CARTESIAN_POINT('Ctrl Pts',(-20.658224207919,24.9723337839319,-73.226384525098));
#6454=CARTESIAN_POINT('Ctrl Pts',(-20.6560059697659,24.967813730749,-73.2266956313704));
#6455=CARTESIAN_POINT('Ctrl Pts',(-20.6316796087033,24.9179493291584,-73.2301166109482));
#6456=CARTESIAN_POINT('Ctrl Pts',(-20.6106269767844,24.8720939499548,-73.2331616659311));
#6457=CARTESIAN_POINT('Ctrl Pts',(-20.5516013833588,24.7351352889643,-73.2420160836417));
#6458=CARTESIAN_POINT('Ctrl Pts',(-20.5167242707689,24.6427566831872,-73.2476812271916));
#6459=CARTESIAN_POINT('Ctrl Pts',(-20.378219893922,24.2177957195679,-73.2729773013602));
#6460=CARTESIAN_POINT('Ctrl Pts',(-20.3246889110931,23.8714097868669,-73.2918229258487));
#6461=CARTESIAN_POINT('Ctrl Pts',(-20.3277884887598,23.5026901382269,-73.31412075425));
#6462=CARTESIAN_POINT('Ctrl Pts',(-20.3281556465789,23.4822207587216,-73.315364728141));
#6463=CARTESIAN_POINT('Ctrl Pts',(-20.3288897824493,23.4554958587125,-73.3169972821561));
#6464=CARTESIAN_POINT('Ctrl Pts',(-20.329080015965,23.4492356403689,-73.3173803054869));
#6465=CARTESIAN_POINT('Ctrl Pts',(-20.3294011220676,23.4395944664419,-73.3179711299722));
#6466=CARTESIAN_POINT('Ctrl Pts',(-20.3295190730395,23.4362130715831,-73.3181785249884));
#6467=CARTESIAN_POINT('Ctrl Pts',(-20.3297524439943,23.4298121799517,-73.3185714585507));
#6468=CARTESIAN_POINT('Ctrl Pts',(-20.3298667862271,23.4267926455105,-73.3187569630298));
#6469=CARTESIAN_POINT('Ctrl Pts',(-20.3301359665332,23.4199390903355,-73.3191783371943));
#6470=CARTESIAN_POINT('Ctrl Pts',(-20.3302934054858,23.4161051814898,-73.3194142883652));
#6471=CARTESIAN_POINT('Ctrl Pts',(-20.3307455197778,23.4055550641991,-73.3200642217056));
#6472=CARTESIAN_POINT('Ctrl Pts',(-20.3310543624622,23.3988395104742,-73.3204786486199));
#6473=CARTESIAN_POINT('Ctrl Pts',(-20.3317860880408,23.3839443910274,-73.3213994644717));
#6474=CARTESIAN_POINT('Ctrl Pts',(-20.3322191442286,23.3757653925121,-73.3219061712179));
#6475=CARTESIAN_POINT('Ctrl Pts',(-20.3336299016449,23.3509153883375,-73.3234490138133));
#6476=CARTESIAN_POINT('Ctrl Pts',(-20.3347059957013,23.3342504511807,-73.3244882357131));
#6477=CARTESIAN_POINT('Ctrl Pts',(-20.3390560025035,23.2741518255148,-73.3282528091653));
#6478=CARTESIAN_POINT('Ctrl Pts',(-20.3430807268434,23.2307788011838,-73.3310015357318));
#6479=CARTESIAN_POINT('Ctrl Pts',(-20.3596187397975,23.0847853037168,-73.3403649154961));
#6480=CARTESIAN_POINT('Ctrl Pts',(-20.3761887061833,22.9826972682358,-73.3471009546443));
#6481=CARTESIAN_POINT('Ctrl Pts',(-20.4627888810171,22.5743936805856,-73.3747603954331));
#6482=CARTESIAN_POINT('Ctrl Pts',(-20.5724844447409,22.2783979489563,-73.3966607477543));
#6483=CARTESIAN_POINT('Ctrl Pts',(-20.72525270061,21.9992815394004,-73.4170312838822));
#6484=CARTESIAN_POINT('Ctrl Pts',(-20.7272684533362,21.9956156099976,-73.4172987440077));
#6485=CARTESIAN_POINT('Ctrl Pts',(-20.7320314021978,21.9869933273712,-73.4179275868077));
#6486=CARTESIAN_POINT('Ctrl Pts',(-20.7347845547474,21.982040254456,-73.4182886505243));
#6487=CARTESIAN_POINT('Ctrl Pts',(-20.7388096735962,21.9748436104409,-73.4188129800835));
#6488=CARTESIAN_POINT('Ctrl Pts',(-20.740071274099,21.9725942945982,-73.4189768192117));
#6489=CARTESIAN_POINT('Ctrl Pts',(-20.7488576502879,21.9569729852645,-73.4201143743069));
#6490=CARTESIAN_POINT('Ctrl Pts',(-20.7564753106704,21.9436530620976,-73.4210828434701));
#6491=CARTESIAN_POINT('Ctrl Pts',(-20.7677149967475,21.9243215159098,-73.4224856474612));
#6492=CARTESIAN_POINT('Ctrl Pts',(-20.7712618489792,21.9182667507948,-73.4229246169314));
#6493=CARTESIAN_POINT('Ctrl Pts',(-20.7761357471222,21.9100085732814,-73.4235227371944));
#6494=CARTESIAN_POINT('Ctrl Pts',(-20.7774456628334,21.9077951515272,-73.4236829913666));
#6495=CARTESIAN_POINT('Ctrl Pts',(-20.7796795221479,21.9040307907654,-73.4239554320307));
#6496=CARTESIAN_POINT('Ctrl Pts',(-20.7806021188893,21.9024790604854,-73.4240677065757));
#6497=CARTESIAN_POINT('Ctrl Pts',(-20.7823932632958,21.8994722603002,-73.4242852026202));
#6498=CARTESIAN_POINT('Ctrl Pts',(-20.7832616488853,21.8980171100471,-73.4243904333888));
#6499=CARTESIAN_POINT('Ctrl Pts',(-20.7853466389252,21.8945295544505,-73.4246425758502));
#6500=CARTESIAN_POINT('Ctrl Pts',(-20.7865643360358,21.8924978060167,-73.4247894147454));
#6501=CARTESIAN_POINT('Ctrl Pts',(-20.7902424450221,21.8863761345528,-73.4252316902909));
#6502=CARTESIAN_POINT('Ctrl Pts',(-20.792709717846,21.8822903097043,-73.425526677476));
#6503=CARTESIAN_POINT('Ctrl Pts',(-20.8151569675511,21.8453034139559,-73.4281953413313));
#6504=CARTESIAN_POINT('Ctrl Pts',(-20.8357169037455,21.8127555138264,-73.4305314757884));
#6505=CARTESIAN_POINT('Ctrl Pts',(-20.9049149837808,21.7074376823409,-73.4380770142831));
#6506=CARTESIAN_POINT('Ctrl Pts',(-20.9559375463648,21.6362751017372,-73.4431540398035));
#6507=CARTESIAN_POINT('Ctrl Pts',(-21.0324575601329,21.5382430338127,-73.4502499940243));
#6508=CARTESIAN_POINT('Ctrl Pts',(-21.0556133893881,21.5096032743064,-73.4523360885993));
#6509=CARTESIAN_POINT('Ctrl Pts',(-21.278756091482,21.2430903410978,-73.4719356771536));
#6510=CARTESIAN_POINT('Ctrl Pts',(-21.5116475424034,21.0349442817447,-73.488867576768));
#6511=CARTESIAN_POINT('Ctrl Pts',(-21.7762957243048,20.8596690756067,-73.507847290662));
#6512=CARTESIAN_POINT('Ctrl Pts',(-21.7818704208894,20.8560018384863,-73.5082468871696));
#6513=CARTESIAN_POINT('Ctrl Pts',(-21.7980654700034,20.8454200662502,-73.5094072096528));
#6514=CARTESIAN_POINT('Ctrl Pts',(-21.8087151834232,20.838550884582,-73.5101695504745));
#6515=CARTESIAN_POINT('Ctrl Pts',(-21.8225413072594,20.8297479257202,-73.5111585160949));
#6516=CARTESIAN_POINT('Ctrl Pts',(-21.8256810355493,20.8277565187179,-73.5113830470236));
#6517=CARTESIAN_POINT('Ctrl Pts',(-21.8468217371978,20.8143990426028,-73.5128945578803));
#6518=CARTESIAN_POINT('Ctrl Pts',(-21.8649311713159,20.803206361008,-73.5141877821618));
#6519=CARTESIAN_POINT('Ctrl Pts',(-21.888592963779,20.7889040395359,-73.5158759820131));
#6520=CARTESIAN_POINT('Ctrl Pts',(-21.8940457864662,20.7856300925655,-73.5162649202174));
#6521=CARTESIAN_POINT('Ctrl Pts',(-21.9027560427582,20.7804353569413,-73.5168860514657));
#6522=CARTESIAN_POINT('Ctrl Pts',(-21.9060072468433,20.7785041113529,-73.5171178620881));
#6523=CARTESIAN_POINT('Ctrl Pts',(-21.9120990431188,20.7749000175487,-73.5175521468133));
#6524=CARTESIAN_POINT('Ctrl Pts',(-21.9149388201346,20.7732257953155,-73.5177545704775));
#6525=CARTESIAN_POINT('Ctrl Pts',(-21.92130682989,20.7694846190779,-73.5182084401133));
#6526=CARTESIAN_POINT('Ctrl Pts',(-21.9248364331385,20.767420019743,-73.5184599713082));
#6527=CARTESIAN_POINT('Ctrl Pts',(-21.935169392448,20.7614022436365,-73.5191962342525));
#6528=CARTESIAN_POINT('Ctrl Pts',(-21.9419832724265,20.7574672796902,-73.5196816255655));
#6529=CARTESIAN_POINT('Ctrl Pts',(-21.957425478504,20.7486247775465,-73.5207814135541));
#6530=CARTESIAN_POINT('Ctrl Pts',(-21.9660621746895,20.7437320875481,-73.5213963417332));
#6531=CARTESIAN_POINT('Ctrl Pts',(-21.993605107078,20.7282966581067,-73.5233569115272));
#6532=CARTESIAN_POINT('Ctrl Pts',(-22.0125947170841,20.7179046425228,-73.5247079361831));
#6533=CARTESIAN_POINT('Ctrl Pts',(-22.0861374788476,20.6786161228805,-73.5299382934159));
#6534=CARTESIAN_POINT('Ctrl Pts',(-22.1414090614959,20.6510995881107,-73.5338656045585));
#6535=CARTESIAN_POINT('Ctrl Pts',(-22.3070265689111,20.5745028126027,-73.5456280499296));
#6536=CARTESIAN_POINT('Ctrl Pts',(-22.4193705535818,20.5300210816243,-73.5536040486037));
#6537=CARTESIAN_POINT('Ctrl Pts',(-22.8057419635218,20.401624396989,-73.5808957826998));
#6538=CARTESIAN_POINT('Ctrl Pts',(-23.0883788894103,20.3479346347013,-73.6007436413631));
#6539=CARTESIAN_POINT('Ctrl Pts',(-23.3747803484998,20.3322831060708,-73.6188898450561));
#6540=CARTESIAN_POINT('Ctrl Pts',(-23.3751655524019,20.3322621244672,-73.6189142475701));
#6541=CARTESIAN_POINT('Ctrl Pts',(-23.3910216990411,20.3314013142865,-73.6199185737069));
#6542=CARTESIAN_POINT('Ctrl Pts',(-23.4064988663177,20.3306729745878,-73.6208928436122));
#6543=CARTESIAN_POINT('Ctrl Pts',(-23.4255073462744,20.32991580152,-73.6220814816862));
#6544=CARTESIAN_POINT('Ctrl Pts',(-23.4290338915378,20.3297811285349,-73.6223016688528));
#6545=CARTESIAN_POINT('Ctrl Pts',(-23.4348667689977,20.3295679750413,-73.6226652951191));
#6546=CARTESIAN_POINT('Ctrl Pts',(-23.4371729645218,20.3294861789059,-73.6228089200425));
#6547=CARTESIAN_POINT('Ctrl Pts',(-23.4411581608415,20.3293491176179,-73.6230568563884));
#6548=CARTESIAN_POINT('Ctrl Pts',(-23.442837112724,20.32929268836,-73.6231612335248));
#6549=CARTESIAN_POINT('Ctrl Pts',(-23.446611706597,20.3291687795872,-73.6233957175267));
#6550=CARTESIAN_POINT('Ctrl Pts',(-23.4487073667277,20.329102032533,-73.6235257823563));
#6551=CARTESIAN_POINT('Ctrl Pts',(-23.4543029990669,20.3289292770869,-73.6238727494713));
#6552=CARTESIAN_POINT('Ctrl Pts',(-23.4578030939631,20.3288269272102,-73.6240894452205));
#6553=CARTESIAN_POINT('Ctrl Pts',(-23.4742454541612,20.3283729386707,-73.6251058754951));
#6554=CARTESIAN_POINT('Ctrl Pts',(-23.4871898339757,20.3280935819665,-73.6259015891815));
#6555=CARTESIAN_POINT('Ctrl Pts',(-23.5900685676046,20.3264935294867,-73.6321926174568));
#6556=CARTESIAN_POINT('Ctrl Pts',(-23.6800299149093,20.3288601996525,-73.6374930202744));
#6557=CARTESIAN_POINT('Ctrl Pts',(-23.852083778636,20.3406076196147,-73.6474434596173));
#6558=CARTESIAN_POINT('Ctrl Pts',(-23.934142371661,20.3493850890063,-73.6521073160595));
#6559=CARTESIAN_POINT('Ctrl Pts',(-24.041179294247,20.3650103897594,-73.6581805730917));
#6560=CARTESIAN_POINT('Ctrl Pts',(-24.0665364940799,20.3690220349133,-73.6596185219087));
#6561=CARTESIAN_POINT('Ctrl Pts',(-24.1137511356775,20.3770710378569,-73.6622983138799));
#6562=CARTESIAN_POINT('Ctrl Pts',(-24.135619908862,20.3810323583784,-73.6635404818334));
#6563=CARTESIAN_POINT('Ctrl Pts',(-24.176679781833,20.3889094600406,-73.6658769452275));
#6564=CARTESIAN_POINT('Ctrl Pts',(-24.1958795269183,20.3927745984768,-73.6669712295623));
#6565=CARTESIAN_POINT('Ctrl Pts',(-24.2809569264454,20.410710143665,-73.6718317355551));
#6566=CARTESIAN_POINT('Ctrl Pts',(-24.3464181684235,20.4266687986296,-73.67560277403));
#6567=CARTESIAN_POINT('Ctrl Pts',(-24.5486780689916,20.4827488726202,-73.6874501815381));
#6568=CARTESIAN_POINT('Ctrl Pts',(-24.6833342008178,20.5298963212732,-73.6956293085145));
#6569=CARTESIAN_POINT('Ctrl Pts',(-24.8215061499554,20.5888185621005,-73.7045608070273));
#6570=CARTESIAN_POINT('Ctrl Pts',(-24.8285820367175,20.5918660469175,-73.7050197010606));
#6571=CARTESIAN_POINT('Ctrl Pts',(-24.8469398306658,20.5998506493155,-73.7062142422856));
#6572=CARTESIAN_POINT('Ctrl Pts',(-24.8582044135229,20.6048270806791,-73.7069511476958));
#6573=CARTESIAN_POINT('Ctrl Pts',(-24.8762213105506,20.6129102634189,-73.7081362211176));
#6574=CARTESIAN_POINT('Ctrl Pts',(-24.8829919496606,20.6159760542795,-73.7085830322922));
#6575=CARTESIAN_POINT('Ctrl Pts',(-24.915060668055,20.6306308759748,-73.7107063889694));
#6576=CARTESIAN_POINT('Ctrl Pts',(-24.9402179642565,20.6425235410514,-73.7123930381376));
#6577=CARTESIAN_POINT('Ctrl Pts',(-24.970908673687,20.6575213287143,-73.7144775583137));
#6578=CARTESIAN_POINT('Ctrl Pts',(-24.9765915892829,20.6603192144065,-73.7148646847351));
#6579=CARTESIAN_POINT('Ctrl Pts',(-24.9859807654453,20.6649762548078,-73.7155061915969));
#6580=CARTESIAN_POINT('Ctrl Pts',(-24.9896917704035,20.6668258492618,-73.7157602369089));
#6581=CARTESIAN_POINT('Ctrl Pts',(-24.9962194126344,20.6700950203113,-73.7162079768247));
#6582=CARTESIAN_POINT('Ctrl Pts',(-24.9990375603495,20.6715115826363,-73.7164015653749));
#6583=CARTESIAN_POINT('Ctrl Pts',(-25.0046583750909,20.6743472700287,-73.7167882561897));
#6584=CARTESIAN_POINT('Ctrl Pts',(-25.0074610557714,20.6757663604581,-73.7169813570767));
#6585=CARTESIAN_POINT('Ctrl Pts',(-25.015173889584,20.6796858038294,-73.7175135545716));
#6586=CARTESIAN_POINT('Ctrl Pts',(-25.0200796953421,20.6821946465869,-73.7178529501426));
#6587=CARTESIAN_POINT('Ctrl Pts',(-25.0395440322177,20.6922118190374,-73.7192030898002));
#6588=CARTESIAN_POINT('Ctrl Pts',(-25.0540514631789,20.6998184162532,-73.7202173029757));
#6589=CARTESIAN_POINT('Ctrl Pts',(-25.0903016001945,20.7191790047341,-73.7227717516774));
#6590=CARTESIAN_POINT('Ctrl Pts',(-25.1119679597188,20.7310729851955,-73.724316937074));
#6591=CARTESIAN_POINT('Ctrl Pts',(-25.1974933075352,20.779311506939,-73.7304911496828));
#6592=CARTESIAN_POINT('Ctrl Pts',(-25.2602339928692,20.8175838100533,-73.7351886257889));
#6593=CARTESIAN_POINT('Ctrl Pts',(-25.4432632974591,20.9380055362176,-73.7494078992253));
#6594=CARTESIAN_POINT('Ctrl Pts',(-25.5593410104589,21.0261923772822,-73.7591289353105));
#6595=CARTESIAN_POINT('Ctrl Pts',(-25.8547327084271,21.2839303624163,-73.7855927189618));
#6596=CARTESIAN_POINT('Ctrl Pts',(-26.0212363053244,21.466720601368,-73.8024933888385));
#6597=CARTESIAN_POINT('Ctrl Pts',(-26.1736443642566,21.6783184171562,-73.8189690473407));
#6598=CARTESIAN_POINT('Ctrl Pts',(-26.1819245423139,21.6899771534297,-73.8198676343764));
#6599=CARTESIAN_POINT('Ctrl Pts',(-26.1922831929323,21.7047700262716,-73.8209958191519));
#6600=CARTESIAN_POINT('Ctrl Pts',(-26.1944339828318,21.7078529695617,-73.8212302896136));
#6601=CARTESIAN_POINT('Ctrl Pts',(-26.1978211373298,21.7127262666405,-73.8215998872281));
#6602=CARTESIAN_POINT('Ctrl Pts',(-26.1990610827548,21.7145141090956,-73.8217352599974));
#6603=CARTESIAN_POINT('Ctrl Pts',(-26.2013596783686,21.7178355671272,-73.8219863461941));
#6604=CARTESIAN_POINT('Ctrl Pts',(-26.2024188039935,21.7193688381454,-73.82210209212));
#6605=CARTESIAN_POINT('Ctrl Pts',(-26.2047740677519,21.7227848297524,-73.8223596035649));
#6606=CARTESIAN_POINT('Ctrl Pts',(-26.2060695299175,21.7246680063816,-73.8225013222168));
#6607=CARTESIAN_POINT('Ctrl Pts',(-26.2098408952567,21.7301628435182,-73.8229141339957));
#6608=CARTESIAN_POINT('Ctrl Pts',(-26.2123114549546,21.7337781921479,-73.8231848611488));
#6609=CARTESIAN_POINT('Ctrl Pts',(-26.2299039826636,21.7596355865177,-73.8251149153877));
#6610=CARTESIAN_POINT('Ctrl Pts',(-26.2447549459512,21.7820619884561,-73.8267560748414));
#6611=CARTESIAN_POINT('Ctrl Pts',(-26.2853806495699,21.8451114826825,-73.8312871398988));
#6612=CARTESIAN_POINT('Ctrl Pts',(-26.3105300767433,21.8861310771874,-73.8341407406226));
#6613=CARTESIAN_POINT('Ctrl Pts',(-26.5046048529728,22.2191874854402,-73.8566928070685));
#6614=CARTESIAN_POINT('Ctrl Pts',(-26.6276479308132,22.5355504961937,-73.8745957281164));
#6615=CARTESIAN_POINT('Ctrl Pts',(-26.7033217867866,22.8834558309663,-73.8953095069888));
#6616=CARTESIAN_POINT('Ctrl Pts',(-26.7071178503884,22.9016656764101,-73.8963957567001));
#6617=CARTESIAN_POINT('Ctrl Pts',(-26.7143921840814,22.9381386272106,-73.8985763867742));
#6618=CARTESIAN_POINT('Ctrl Pts',(-26.7178704842886,22.9564009855831,-73.8996707198113));
#6619=CARTESIAN_POINT('Ctrl Pts',(-26.7223738108325,22.9812111880614,-73.9011612828438));
#6620=CARTESIAN_POINT('Ctrl Pts',(-26.7235369736599,22.9877338121914,-73.9015535141595));
#6621=CARTESIAN_POINT('Ctrl Pts',(-26.7271998051643,23.0086466682404,-73.9028122953579));
#6622=CARTESIAN_POINT('Ctrl Pts',(-26.7296217401929,23.0230501836991,-73.9036811000038));
#6623=CARTESIAN_POINT('Ctrl Pts',(-26.7390577233955,23.0815981481341,-73.907220744086));
#6624=CARTESIAN_POINT('Ctrl Pts',(-26.7452506696875,23.1258681834554,-73.9099159264471));
#6625=CARTESIAN_POINT('Ctrl Pts',(-26.7513987888541,23.1776459588676,-73.9130944818731));
#6626=CARTESIAN_POINT('Ctrl Pts',(-26.752251221644,23.1850438161157,-73.9135492459722));
#6627=CARTESIAN_POINT('Ctrl Pts',(-26.7535703423128,23.1968515818765,-73.9142761118865));
#6628=CARTESIAN_POINT('Ctrl Pts',(-26.7540535854108,23.2012596448741,-73.914547690016));
#6629=CARTESIAN_POINT('Ctrl Pts',(-26.7548902851022,23.2090400907829,-73.9150274412236));
#6630=CARTESIAN_POINT('Ctrl Pts',(-26.7552475209327,23.2124120675446,-73.9152354945338));
#6631=CARTESIAN_POINT('Ctrl Pts',(-26.7559241559984,23.2188965458795,-73.9156358501233));
#6632=CARTESIAN_POINT('Ctrl Pts',(-26.7562443456957,23.2220089626036,-73.9158281271736));
#6633=CARTESIAN_POINT('Ctrl Pts',(-26.7569178894717,23.2286511789244,-73.9162387125626));
#6634=CARTESIAN_POINT('Ctrl Pts',(-26.7572699487036,23.2321811030639,-73.9164570615696));
#6635=CARTESIAN_POINT('Ctrl Pts',(-26.7580997164055,23.240642217053,-73.9169807959942));
#6636=CARTESIAN_POINT('Ctrl Pts',(-26.7585718825053,23.2455739302734,-73.9172863561342));
#6637=CARTESIAN_POINT('Ctrl Pts',(-26.7598069076893,23.2587948786291,-73.9181062943876));
#6638=CARTESIAN_POINT('Ctrl Pts',(-26.7605490216312,23.2670859718664,-73.9186213263913));
#6639=CARTESIAN_POINT('Ctrl Pts',(-26.7691406263219,23.367451317547,-73.9248661657328));
#6640=CARTESIAN_POINT('Ctrl Pts',(-26.7730577462239,23.4598091419467,-73.9307192919354));
#6641=CARTESIAN_POINT('Ctrl Pts',(-26.7730019438629,23.5521990328162,-73.9366887153694));
#6642=CARTESIAN_POINT('Ctrl Pts',(-22.0750360153461,26.4155367745563,-74.34623438385));
#6643=CARTESIAN_POINT('Ctrl Pts',(-22.1638502850276,26.46126357386,-74.3400816013948));
#6644=CARTESIAN_POINT('Ctrl Pts',(-22.2548390451486,26.5028809965016,-74.3339288189396));
#6645=CARTESIAN_POINT('Ctrl Pts',(-22.3475842422765,26.540186736343,-74.3277760364844));
#6646=CARTESIAN_POINT('Ctrl Pts',(-22.4403129201626,26.5774858315003,-74.3216243499274));
#6647=CARTESIAN_POINT('Ctrl Pts',(-22.5347970105746,26.6104746083562,-74.3154726633705));
#6648=CARTESIAN_POINT('Ctrl Pts',(-22.6305982685655,26.6389988143806,-74.3093209768136));
#6649=CARTESIAN_POINT('Ctrl Pts',(-22.726408047016,26.6675255573168,-74.3031687431323));
#6650=CARTESIAN_POINT('Ctrl Pts',(-22.8235348095442,26.691586817123,-74.2970165094511));
#6651=CARTESIAN_POINT('Ctrl Pts',(-22.9215259051911,26.7110784350976,-74.2908642757698));
#6652=CARTESIAN_POINT('Ctrl Pts',(-23.0199097668309,26.7306481789941,-74.2846873828259));
#6653=CARTESIAN_POINT('Ctrl Pts',(-23.1191644739776,26.7456114804933,-74.278510489882));
#6654=CARTESIAN_POINT('Ctrl Pts',(-23.2188238826832,26.7559151173564,-74.272333596938));
#6655=CARTESIAN_POINT('Ctrl Pts',(-23.3182371317515,26.7661933041437,-74.2661719609753));
#6656=CARTESIAN_POINT('Ctrl Pts',(-23.4180526475076,26.7718348372567,-74.2600103250126));
#6657=CARTESIAN_POINT('Ctrl Pts',(-23.5178062923391,26.7728391952382,-74.2538486890499));
#6658=CARTESIAN_POINT('Ctrl Pts',(-23.61793044092,26.7738472835937,-74.2476641676153));
#6659=CARTESIAN_POINT('Ctrl Pts',(-23.717991819053,26.7701837123499,-74.2414796461808));
#6660=CARTESIAN_POINT('Ctrl Pts',(-23.8175262436563,26.761900445989,-74.2352951247462));
#6661=CARTESIAN_POINT('Ctrl Pts',(-23.9170606682595,26.753617179628,-74.2291106033117));
#6662=CARTESIAN_POINT('Ctrl Pts',(-24.0160677153349,26.7407143351953,-74.2229260818772));
#6663=CARTESIAN_POINT('Ctrl Pts',(-24.1140948251003,26.7232951457583,-74.2167415604426));
#6664=CARTESIAN_POINT('Ctrl Pts',(-24.2119463802174,26.705907151974,-74.2105681147349));
#6665=CARTESIAN_POINT('Ctrl Pts',(-24.3091642918956,26.6839580768627,-74.2043946690271));
#6666=CARTESIAN_POINT('Ctrl Pts',(-24.40529055219,26.6575065518874,-74.1982212233194));
#6667=CARTESIAN_POINT('Ctrl Pts',(-24.5012870325805,26.6310907390719,-74.1920561123704));
#6668=CARTESIAN_POINT('Ctrl Pts',(-24.5961943760753,26.6001846729129,-74.1858910014214));
#6669=CARTESIAN_POINT('Ctrl Pts',(-24.6895630872402,26.5648982854307,-74.1797258904724));
#6670=CARTESIAN_POINT('Ctrl Pts',(-24.7828332965206,26.5296491242915,-74.1735672835764));
#6671=CARTESIAN_POINT('Ctrl Pts',(-24.874567696709,26.4900289818559,-74.1674086766804));
#6672=CARTESIAN_POINT('Ctrl Pts',(-24.9643312583758,26.4461977862262,-74.1612500697845));
#6673=CARTESIAN_POINT('Ctrl Pts',(-25.0540297073452,26.4023983848717,-74.1550959302191));
#6674=CARTESIAN_POINT('Ctrl Pts',(-25.1417597711075,26.3543941933535,-74.1489417906537));
#6675=CARTESIAN_POINT('Ctrl Pts',(-25.2271065991256,26.3023931529268,-74.1427876510884));
#6676=CARTESIAN_POINT('Ctrl Pts',(-25.3124213477109,26.2504116582047,-74.1366358246881));
#6677=CARTESIAN_POINT('Ctrl Pts',(-25.3953542701286,26.1944365253345,-74.1304839982879));
#6678=CARTESIAN_POINT('Ctrl Pts',(-25.4755161133061,26.1347210851533,-74.1243321718877));
#6679=CARTESIAN_POINT('Ctrl Pts',(-25.5556692449119,26.0750121345351,-74.1181810140359));
#6680=CARTESIAN_POINT('Ctrl Pts',(-25.6330515478184,26.0115639441327,-74.1120298561841));
#6681=CARTESIAN_POINT('Ctrl Pts',(-25.7073045326274,25.9446719243174,-74.1058786983323));
#6682=CARTESIAN_POINT('Ctrl Pts',(-25.7815692879801,25.8777693008147,-74.0997265654023));
#6683=CARTESIAN_POINT('Ctrl Pts',(-25.852703417293,25.8074220541724,-74.0935744324723));
#6684=CARTESIAN_POINT('Ctrl Pts',(-25.92038392367,25.7339637642684,-74.0874222995422));
#6685=CARTESIAN_POINT('Ctrl Pts',(-25.9881370002476,25.6604267089544,-74.0812635700078));
#6686=CARTESIAN_POINT('Ctrl Pts',(-26.052428764335,25.5837722690493,-74.0751048404735));
#6687=CARTESIAN_POINT('Ctrl Pts',(-26.1129753969161,25.5043684644293,-74.0689461109391));
#6688=CARTESIAN_POINT('Ctrl Pts',(-26.1735559143592,25.4249202215499,-74.062783934678));
#6689=CARTESIAN_POINT('Ctrl Pts',(-26.2303868792733,25.3427199068222,-74.0566217584168));
#6690=CARTESIAN_POINT('Ctrl Pts',(-26.2832280450616,25.258164240722,-74.0504595821557));
#6691=CARTESIAN_POINT('Ctrl Pts',(-26.3361576398668,25.1734670717931,-74.0442870935711));
#6692=CARTESIAN_POINT('Ctrl Pts',(-26.3850838858273,25.0864070568192,-74.0381146049866));
#6693=CARTESIAN_POINT('Ctrl Pts',(-26.4298126296483,24.99740532417,-74.0319421164021));
#6694=CARTESIAN_POINT('Ctrl Pts',(-26.463840758868,24.9296957888544,-74.0272462939573));
#6695=CARTESIAN_POINT('Ctrl Pts',(-26.4954404739716,24.8608629589719,-74.0225504715125));
#6696=CARTESIAN_POINT('Ctrl Pts',(-26.524545431243,24.7910987390034,-74.0178546490678));
#6697=CARTESIAN_POINT('Ctrl Pts',(-26.5671860774408,24.6888896413158,-74.0109749652528));
#6698=CARTESIAN_POINT('Ctrl Pts',(-26.604598155147,24.5843757468685,-74.0040952814378));
#6699=CARTESIAN_POINT('Ctrl Pts',(-26.6365541860418,24.4780777635515,-73.9972155976228));
#6700=CARTESIAN_POINT('Ctrl Pts',(-26.6684132457932,24.3721023433531,-73.9903567903306));
#6701=CARTESIAN_POINT('Ctrl Pts',(-26.694849181671,24.2643538679654,-73.9834979830383));
#6702=CARTESIAN_POINT('Ctrl Pts',(-26.7156828145406,24.1553712695786,-73.9766391757461));
#6703=CARTESIAN_POINT('Ctrl Pts',(-26.7364026540635,24.0469839343746,-73.9698178312738));
#6704=CARTESIAN_POINT('Ctrl Pts',(-26.7515811121171,23.937376159783,-73.9629964868015));
#6705=CARTESIAN_POINT('Ctrl Pts',(-26.7610895711912,23.8270973768584,-73.9561751423292));
#6706=CARTESIAN_POINT('Ctrl Pts',(-26.7689646066732,23.7357629848532,-73.9505256118074));
#6707=CARTESIAN_POINT('Ctrl Pts',(-26.7729511894786,23.6439687332407,-73.9448760812856));
#6708=CARTESIAN_POINT('Ctrl Pts',(-26.7730020387288,23.5520350602361,-73.9392265507638));
#6709=CARTESIAN_POINT('',(-26.7730019206732,23.5522370557033,-74.1857734492731));
#6710=CARTESIAN_POINT('Ctrl Pts',(-22.0750360153461,26.4155367745563,-74.5928284611549));
#6711=CARTESIAN_POINT('Ctrl Pts',(-22.1636076089027,26.4611386299462,-74.5866506497362));
#6712=CARTESIAN_POINT('Ctrl Pts',(-22.2544338538382,26.5027009229343,-74.5804728383175));
#6713=CARTESIAN_POINT('Ctrl Pts',(-22.3471109305284,26.5399963083487,-74.5742950268988));
#6714=CARTESIAN_POINT('Ctrl Pts',(-22.4396766330714,26.5772468742468,-74.5681246396297));
#6715=CARTESIAN_POINT('Ctrl Pts',(-22.5340883468709,26.6102405661368,-74.5619542523606));
#6716=CARTESIAN_POINT('Ctrl Pts',(-22.6299185416649,26.6387963486566,-74.5557838650914));
#6717=CARTESIAN_POINT('Ctrl Pts',(-22.7285671015863,26.6681919564717,-74.5494320067907));
#6718=CARTESIAN_POINT('Ctrl Pts',(-22.8287184657271,26.6928843316223,-74.5430801484901));
#6719=CARTESIAN_POINT('Ctrl Pts',(-22.9298848592266,26.7127296483635,-74.5367282901894));
#6720=CARTESIAN_POINT('Ctrl Pts',(-23.0280174924835,26.7319798471921,-74.5305669103126));
#6721=CARTESIAN_POINT('Ctrl Pts',(-23.1271046867706,26.7466694756759,-74.5244055304357));
#6722=CARTESIAN_POINT('Ctrl Pts',(-23.2266879909635,26.7567184289839,-74.5182441505589));
#6723=CARTESIAN_POINT('Ctrl Pts',(-23.3262472978702,26.7667649607253,-74.5120842554329));
#6724=CARTESIAN_POINT('Ctrl Pts',(-23.4263020466877,26.7721729965736,-74.5059243603069));
#6725=CARTESIAN_POINT('Ctrl Pts',(-23.5263874747349,26.772914167913,-74.499764465181));
#6726=CARTESIAN_POINT('Ctrl Pts',(-23.626475309744,26.7736553570768,-74.4936044219152));
#6727=CARTESIAN_POINT('Ctrl Pts',(-23.726593392647,26.7697294562033,-74.4874443786495));
#6728=CARTESIAN_POINT('Ctrl Pts',(-23.8262767533552,26.7611602213602,-74.4812843353837));
#6729=CARTESIAN_POINT('Ctrl Pts',(-23.9259889296083,26.752588509402,-74.4751225114296));
#6730=CARTESIAN_POINT('Ctrl Pts',(-24.0252657029357,26.7393708335459,-74.4689606874755));
#6731=CARTESIAN_POINT('Ctrl Pts',(-24.1236480019802,26.7215827253441,-74.4627988635213));
#6732=CARTESIAN_POINT('Ctrl Pts',(-24.222140422206,26.7037747065739,-74.4566301425203));
#6733=CARTESIAN_POINT('Ctrl Pts',(-24.3197359439699,26.6813861237143,-74.4504614215192));
#6734=CARTESIAN_POINT('Ctrl Pts',(-24.415986659057,26.6545434303085,-74.4442927005181));
#6735=CARTESIAN_POINT('Ctrl Pts',(-24.5123022205314,26.6276826523441,-74.4381198235036));
#6736=CARTESIAN_POINT('Ctrl Pts',(-24.6072707614017,26.5963619250118,-74.431946946489));
#6737=CARTESIAN_POINT('Ctrl Pts',(-24.7004623612232,26.5607566274488,-74.4257740694744));
#6738=CARTESIAN_POINT('Ctrl Pts',(-24.7937922583881,26.5250984912385,-74.4195920318435));
#6739=CARTESIAN_POINT('Ctrl Pts',(-24.8853395574873,26.4851432701484,-74.4134099942126));
#6740=CARTESIAN_POINT('Ctrl Pts',(-24.9746972375318,26.4411131029621,-74.4072279565817));
#6741=CARTESIAN_POINT('Ctrl Pts',(-24.9934334752511,26.4318809957855,-74.4059317263462));
#6742=CARTESIAN_POINT('Ctrl Pts',(-25.0120735458385,26.422469890201,-74.4046354961108));
#6743=CARTESIAN_POINT('Ctrl Pts',(-25.0306138588376,26.412882075243,-74.4033392658753));
#6744=CARTESIAN_POINT('Ctrl Pts',(-25.1190531126965,26.3671471838704,-74.3971561105609));
#6745=CARTESIAN_POINT('Ctrl Pts',(-25.2055203593367,26.3172327871667,-74.3909729552464));
#6746=CARTESIAN_POINT('Ctrl Pts',(-25.289595062973,26.2633329067264,-74.384789799932));
#6747=CARTESIAN_POINT('Ctrl Pts',(-25.3735589558713,26.2095040665071,-74.3786147940367));
#6748=CARTESIAN_POINT('Ctrl Pts',(-25.4551362129971,26.1517004159409,-74.3724397881414));
#6749=CARTESIAN_POINT('Ctrl Pts',(-25.5339298493267,26.0901623454494,-74.3662647822462));
#6750=CARTESIAN_POINT('Ctrl Pts',(-25.6126426733369,26.0286873896261,-74.3600961095597));
#6751=CARTESIAN_POINT('Ctrl Pts',(-25.6885772138999,25.963485894204,-74.3539274368732));
#6752=CARTESIAN_POINT('Ctrl Pts',(-25.7613653037703,25.8948415941232,-74.3477587641867));
#6753=CARTESIAN_POINT('Ctrl Pts',(-25.834103221162,25.8262446102269,-74.3415943435365));
#6754=CARTESIAN_POINT('Ctrl Pts',(-25.903698686081,25.7542098358229,-74.3354299228863));
#6755=CARTESIAN_POINT('Ctrl Pts',(-25.9698171759252,25.6790607651636,-74.3292655022361));
#6756=CARTESIAN_POINT('Ctrl Pts',(-26.0359122357238,25.6039383246672,-74.3231032660377));
#6757=CARTESIAN_POINT('Ctrl Pts',(-26.0985324834489,25.5257041054362,-74.3169410298394));
#6758=CARTESIAN_POINT('Ctrl Pts',(-26.1573814203929,25.4447172371486,-74.310778793641));
#6759=CARTESIAN_POINT('Ctrl Pts',(-26.2162250839103,25.3637376260579,-74.3046171096378));
#6760=CARTESIAN_POINT('Ctrl Pts',(-26.2712978543429,25.2800062063495,-74.2984554256346));
#6761=CARTESIAN_POINT('Ctrl Pts',(-26.3223451800199,25.1939130536994,-74.2922937416315));
#6762=CARTESIAN_POINT('Ctrl Pts',(-26.3734014461824,25.1078048225987,-74.2861309784641));
#6763=CARTESIAN_POINT('Ctrl Pts',(-26.420430646287,25.0193344088958,-74.2799682152967));
#6764=CARTESIAN_POINT('Ctrl Pts',(-26.4632235061485,24.928917706596,-74.2738054521294));
#6765=CARTESIAN_POINT('Ctrl Pts',(-26.5060628376104,24.8384028148112,-74.2676359964094));
#6766=CARTESIAN_POINT('Ctrl Pts',(-26.5446564567202,24.7459378055551,-74.2614665406893));
#6767=CARTESIAN_POINT('Ctrl Pts',(-26.5788427587947,24.6519597517899,-74.2552970849693));
#6768=CARTESIAN_POINT('Ctrl Pts',(-26.613048546435,24.5579281322562,-74.2491241127726));
#6769=CARTESIAN_POINT('Ctrl Pts',(-26.6428418851251,24.4623821635771,-74.2429511405758));
#6770=CARTESIAN_POINT('Ctrl Pts',(-26.668111315878,24.3657733250454,-74.2367781683791));
#6771=CARTESIAN_POINT('Ctrl Pts',(-26.6934229705998,24.2690030579229,-74.2305948814511));
#6772=CARTESIAN_POINT('Ctrl Pts',(-26.7141955280556,24.1711667967266,-74.2244115945232));
#6773=CARTESIAN_POINT('Ctrl Pts',(-26.7303687981163,24.0727255879733,-74.2182283075952));
#6774=CARTESIAN_POINT('Ctrl Pts',(-26.7423797890527,23.9996187603704,-74.2136363232303));
#6775=CARTESIAN_POINT('Ctrl Pts',(-26.7518552545503,23.9261784765462,-74.2090443388653));
#6776=CARTESIAN_POINT('Ctrl Pts',(-26.7587891415197,23.8525940371305,-74.2044523545004));
#6777=CARTESIAN_POINT('Ctrl Pts',(-26.7681908443758,23.752820412715,-74.1982260527579));
#6778=CARTESIAN_POINT('Ctrl Pts',(-26.7729401209426,23.6525961559481,-74.1919997510155));
#6779=CARTESIAN_POINT('Ctrl Pts',(-26.7730019206732,23.5522370557033,-74.1857734492731));
#6780=CARTESIAN_POINT('Ctrl Pts',(-26.7730018334319,23.552374005015,-74.1834084018853));
#6781=CARTESIAN_POINT('Ctrl Pts',(-26.7731731936204,23.2920591934439,-74.1683346339349));
#6782=CARTESIAN_POINT('Ctrl Pts',(-26.7418053767837,23.0326559172775,-74.1542544132757));
#6783=CARTESIAN_POINT('Ctrl Pts',(-26.6527383336224,22.6708854196747,-74.1330410158101));
#6784=CARTESIAN_POINT('Ctrl Pts',(-26.6202498266327,22.5634305571839,-74.126542358643));
#6785=CARTESIAN_POINT('Ctrl Pts',(-26.5653829434107,22.4111406508839,-74.1169029855998));
#6786=CARTESIAN_POINT('Ctrl Pts',(-26.5474598812864,22.3647842864118,-74.1139099833266));
#6787=CARTESIAN_POINT('Ctrl Pts',(-26.5254646687034,22.3115870046156,-74.110400313905));
#6788=CARTESIAN_POINT('Ctrl Pts',(-26.5224297838194,22.304322385826,-74.1099193972657));
#6789=CARTESIAN_POINT('Ctrl Pts',(-26.5177769187787,22.293298545438,-74.1091871040994));
#6790=CARTESIAN_POINT('Ctrl Pts',(-26.5161783321312,22.2895311280677,-74.1089363934697));
#6791=CARTESIAN_POINT('Ctrl Pts',(-26.5132694580615,22.2827118865635,-74.1084817763106));
#6792=CARTESIAN_POINT('Ctrl Pts',(-26.5119616190123,22.2796590188185,-74.108277954225));
#6793=CARTESIAN_POINT('Ctrl Pts',(-26.5093390270982,22.2735631946185,-74.1078703754233));
#6794=CARTESIAN_POINT('Ctrl Pts',(-26.5080242938307,22.2705202340388,-74.1076666195734));
#6795=CARTESIAN_POINT('Ctrl Pts',(-26.5043159139954,22.2619734011992,-74.107093485947));
#6796=CARTESIAN_POINT('Ctrl Pts',(-26.5019115929895,22.256474200677,-74.1067237401197));
#6797=CARTESIAN_POINT('Ctrl Pts',(-26.4919945701673,22.2339633618703,-74.1052061459204));
#6798=CARTESIAN_POINT('Ctrl Pts',(-26.4843501687463,22.2170104560567,-74.1040537468586));
#6799=CARTESIAN_POINT('Ctrl Pts',(-26.4697159119018,22.1852917284274,-74.1018793990026));
#6800=CARTESIAN_POINT('Ctrl Pts',(-26.4627596453122,22.1705109906939,-74.1008586515998));
#6801=CARTESIAN_POINT('Ctrl Pts',(-26.4500719660861,22.1440756316,-74.0990193529368));
#6802=CARTESIAN_POINT('Ctrl Pts',(-26.444381869436,22.1324014835075,-74.0982022600768));
#6803=CARTESIAN_POINT('Ctrl Pts',(-26.4348968024971,22.1132363506917,-74.0968528165984));
#6804=CARTESIAN_POINT('Ctrl Pts',(-26.4311428017041,22.105725161394,-74.0963218949798));
#6805=CARTESIAN_POINT('Ctrl Pts',(-26.4255063987995,22.0945569320732,-74.0955294108137));
#6806=CARTESIAN_POINT('Ctrl Pts',(-26.4236462600132,22.0908886425752,-74.0952686183662));
#6807=CARTESIAN_POINT('Ctrl Pts',(-26.4176360100783,22.0790921592347,-74.094428365001));
#6808=CARTESIAN_POINT('Ctrl Pts',(-26.4134584202331,22.0709780843051,-74.093847960863));
#6809=CARTESIAN_POINT('Ctrl Pts',(-26.3982162032591,22.0416798007035,-74.0917433489619));
#6810=CARTESIAN_POINT('Ctrl Pts',(-26.3869506828606,22.0206014897318,-74.0902123179817));
#6811=CARTESIAN_POINT('Ctrl Pts',(-26.2296131837086,21.7339322389166,-74.0691570833579));
#6812=CARTESIAN_POINT('Ctrl Pts',(-26.0470256099903,21.490142246053,-74.048285803409));
#6813=CARTESIAN_POINT('Ctrl Pts',(-25.7919426967307,21.2341456103311,-74.0241051369264));
#6814=CARTESIAN_POINT('Ctrl Pts',(-25.7496156218093,21.1939145352312,-74.020232262364));
#6815=CARTESIAN_POINT('Ctrl Pts',(-25.6729775439087,21.1249368906135,-74.01349354921));
#6816=CARTESIAN_POINT('Ctrl Pts',(-25.6391171446194,21.0957133648934,-74.0106049306079));
#6817=CARTESIAN_POINT('Ctrl Pts',(-25.5878132502417,21.0532659800151,-74.0063718181071));
#6818=CARTESIAN_POINT('Ctrl Pts',(-25.5708269651545,21.0395007431033,-74.0049929260526));
#6819=CARTESIAN_POINT('Ctrl Pts',(-25.5504859041213,21.0233570313041,-74.0033697458957));
#6820=CARTESIAN_POINT('Ctrl Pts',(-25.5472655582968,21.0208112127281,-74.0031135936597));
#6821=CARTESIAN_POINT('Ctrl Pts',(-25.5426073722957,21.0171431621158,-74.0027442746002));
#6822=CARTESIAN_POINT('Ctrl Pts',(-25.5411734471658,21.0160160002134,-74.002630751439));
#6823=CARTESIAN_POINT('Ctrl Pts',(-25.5383238722555,21.0137799532882,-74.0024054787508));
#6824=CARTESIAN_POINT('Ctrl Pts',(-25.5369082550465,21.0126710388054,-74.0022937274034));
#6825=CARTESIAN_POINT('Ctrl Pts',(-25.5340799319032,21.0104593077088,-74.002070772594));
#6826=CARTESIAN_POINT('Ctrl Pts',(-25.5326672323665,21.0093564832459,-74.0019595685063));
#6827=CARTESIAN_POINT('Ctrl Pts',(-25.5292647387224,21.0067048901377,-74.0016921111418));
#6828=CARTESIAN_POINT('Ctrl Pts',(-25.5272740416981,21.0051572742396,-74.001535940698));
#6829=CARTESIAN_POINT('Ctrl Pts',(-25.5211600438974,21.0004156066549,-74.0010572426436));
#6830=CARTESIAN_POINT('Ctrl Pts',(-25.5170307777783,20.9972292067746,-74.0007352576979));
#6831=CARTESIAN_POINT('Ctrl Pts',(-25.4697915624277,20.9609591019028,-73.9970665033251));
#6832=CARTESIAN_POINT('Ctrl Pts',(-25.4258560569786,20.9289584175873,-73.9937945995209));
#6833=CARTESIAN_POINT('Ctrl Pts',(-25.3705114997343,20.8907523325541,-73.9898149133693));
#6834=CARTESIAN_POINT('Ctrl Pts',(-25.359849831816,20.8834863926253,-73.989054607345));
#6835=CARTESIAN_POINT('Ctrl Pts',(-25.2689269212389,20.8223186778309,-73.9826218083097));
#6836=CARTESIAN_POINT('Ctrl Pts',(-25.1863155876713,20.7719859818886,-73.9771126591773));
#6837=CARTESIAN_POINT('Ctrl Pts',(-25.0401320728113,20.6917060354189,-73.9677147371931));
#6838=CARTESIAN_POINT('Ctrl Pts',(-24.9776182704327,20.6599832627997,-73.9638000600999));
#6839=CARTESIAN_POINT('Ctrl Pts',(-24.7735165411243,20.564649596152,-73.9512135054993));
#6840=CARTESIAN_POINT('Ctrl Pts',(-24.6283596435621,20.5092196871638,-73.9425435688092));
#6841=CARTESIAN_POINT('Ctrl Pts',(-24.4006048966428,20.4406132568563,-73.9288150233273));
#6842=CARTESIAN_POINT('Ctrl Pts',(-24.3205437188905,20.4198203859502,-73.9239689592116));
#6843=CARTESIAN_POINT('Ctrl Pts',(-24.1983389395987,20.3930542528631,-73.9164892662991));
#6844=CARTESIAN_POINT('Ctrl Pts',(-24.1567283199703,20.3847977742896,-73.9139284032327));
#6845=CARTESIAN_POINT('Ctrl Pts',(-24.1074783869251,20.3760321888643,-73.9108771049625));
#6846=CARTESIAN_POINT('Ctrl Pts',(-24.0999838147574,20.3747256536103,-73.9104122272031));
#6847=CARTESIAN_POINT('Ctrl Pts',(-24.0884803473159,20.3727621881554,-73.9096978189052));
#6848=CARTESIAN_POINT('Ctrl Pts',(-24.0844746836128,20.3720862747228,-73.9094488916634));
#6849=CARTESIAN_POINT('Ctrl Pts',(-24.07716074237,20.370866342397,-73.9089940784488));
#6850=CARTESIAN_POINT('Ctrl Pts',(-24.0738528688596,20.3703199082009,-73.9087882694578));
#6851=CARTESIAN_POINT('Ctrl Pts',(-24.0671947451766,20.3692307101382,-73.9083737896306));
#6852=CARTESIAN_POINT('Ctrl Pts',(-24.0638444785661,20.3686880748171,-73.9081651150007));
#6853=CARTESIAN_POINT('Ctrl Pts',(-24.0542903969377,20.3671561054015,-73.9075696994322));
#6854=CARTESIAN_POINT('Ctrl Pts',(-24.048084563035,20.3661796216691,-73.9071825516606));
#6855=CARTESIAN_POINT('Ctrl Pts',(-24.0215830601376,20.3620889994941,-73.9055275454476));
#6856=CARTESIAN_POINT('Ctrl Pts',(-24.0012610883809,20.3591507743765,-73.9042541320727));
#6857=CARTESIAN_POINT('Ctrl Pts',(-23.6414538441664,20.3106341251809,-73.8816279678724));
#6858=CARTESIAN_POINT('Ctrl Pts',(-23.2969308663212,20.3192851419755,-73.8583524628253));
#6859=CARTESIAN_POINT('Ctrl Pts',(-22.8594984343816,20.4007283300809,-73.8284146377176));
#6860=CARTESIAN_POINT('Ctrl Pts',(-22.7595796870382,20.4243152825993,-73.821577723196));
#6861=CARTESIAN_POINT('Ctrl Pts',(-22.6282540538186,20.4620178446651,-73.8127274999079));
#6862=CARTESIAN_POINT('Ctrl Pts',(-22.5957075908082,20.4719220035411,-73.8105456776735));
#6863=CARTESIAN_POINT('Ctrl Pts',(-22.5520730251936,20.4859589939648,-73.8076417242578));
#6864=CARTESIAN_POINT('Ctrl Pts',(-22.5408432183487,20.4896398380281,-73.8068962700496));
#6865=CARTESIAN_POINT('Ctrl Pts',(-22.5244855442217,20.49510129026,-73.8058134688052));
#6866=CARTESIAN_POINT('Ctrl Pts',(-22.5193416802277,20.4968331635176,-73.805473410805));
#6867=CARTESIAN_POINT('Ctrl Pts',(-22.5101273883393,20.4999614363531,-73.8048650827754));
#6868=CARTESIAN_POINT('Ctrl Pts',(-22.506055351018,20.501353004236,-73.8045965357065));
#6869=CARTESIAN_POINT('Ctrl Pts',(-22.4998441667246,20.5034895018634,-73.8041873686863));
#6870=CARTESIAN_POINT('Ctrl Pts',(-22.4977030177515,20.5042285308176,-73.8040464012964));
#6871=CARTESIAN_POINT('Ctrl Pts',(-22.4937986512272,20.5055807520359,-73.8037895015613));
#6872=CARTESIAN_POINT('Ctrl Pts',(-22.4920351857257,20.5061932194986,-73.803673526039));
#6873=CARTESIAN_POINT('Ctrl Pts',(-22.4882251015333,20.5075202070863,-73.8034230777163));
#6874=CARTESIAN_POINT('Ctrl Pts',(-22.4861786743836,20.5082352589158,-73.8032886372789));
#6875=CARTESIAN_POINT('Ctrl Pts',(-22.4806259882158,20.51018173808,-73.80292405862));
#6876=CARTESIAN_POINT('Ctrl Pts',(-22.4771211214997,20.5114171709872,-73.8026941591273));
#6877=CARTESIAN_POINT('Ctrl Pts',(-22.4605794734741,20.5172801349079,-73.8016101405867));
#6878=CARTESIAN_POINT('Ctrl Pts',(-22.4475701836713,20.5219856033909,-73.8007606025528));
#6879=CARTESIAN_POINT('Ctrl Pts',(-22.244104145818,20.5970644316854,-73.7875148789264));
#6880=CARTESIAN_POINT('Ctrl Pts',(-22.0606530356323,20.6852108778867,-73.7761229725251));
#6881=CARTESIAN_POINT('Ctrl Pts',(-21.7638912434107,20.8640674739802,-73.756744722397));
#6882=CARTESIAN_POINT('Ctrl Pts',(-21.646164762407,20.9461932788097,-73.7487658703992));
#6883=CARTESIAN_POINT('Ctrl Pts',(-21.4270915312859,21.1218399115396,-73.7327358188833));
#6884=CARTESIAN_POINT('Ctrl Pts',(-21.3255009291452,21.2145569770672,-73.7247179945337));
#6885=CARTESIAN_POINT('Ctrl Pts',(-21.2151169684542,21.3290528024566,-73.7151043032376));
#6886=CARTESIAN_POINT('Ctrl Pts',(-21.2002474724256,21.3447905570142,-73.7137888743219));
#6887=CARTESIAN_POINT('Ctrl Pts',(-21.1813736392967,21.3651740608185,-73.7120922530703));
#6888=CARTESIAN_POINT('Ctrl Pts',(-21.1772221842605,21.3696833170005,-73.711717366033));
#6889=CARTESIAN_POINT('Ctrl Pts',(-21.1705643161092,21.3769565369993,-73.7111133855583));
#6890=CARTESIAN_POINT('Ctrl Pts',(-21.1680497812854,21.3797130734696,-73.7108846377599));
#6891=CARTESIAN_POINT('Ctrl Pts',(-21.1632768923156,21.384963594933,-73.7104492295681));
#6892=CARTESIAN_POINT('Ctrl Pts',(-21.1610176441365,21.3874567635766,-73.710242607455));
#6893=CARTESIAN_POINT('Ctrl Pts',(-21.1558859809618,21.3931376077002,-73.7097720939159));
#6894=CARTESIAN_POINT('Ctrl Pts',(-21.1530160241333,21.3963274863137,-73.7095080992428));
#6895=CARTESIAN_POINT('Ctrl Pts',(-21.1443201213155,21.4060316529311,-73.7087055976501));
#6896=CARTESIAN_POINT('Ctrl Pts',(-21.1385143307542,21.4125638761718,-73.7081662451342));
#6897=CARTESIAN_POINT('Ctrl Pts',(-21.0976820853821,21.4588832105907,-73.7043475318647));
#6898=CARTESIAN_POINT('Ctrl Pts',(-21.063617146124,21.4995035587788,-73.7010284498143));
#6899=CARTESIAN_POINT('Ctrl Pts',(-21.0278066659131,21.5444100467975,-73.6973877640093));
#6900=CARTESIAN_POINT('Ctrl Pts',(-21.0250495383985,21.5478821707593,-73.6971064524718));
#6901=CARTESIAN_POINT('Ctrl Pts',(-21.018266294329,21.5564607817363,-73.6964118609188));
#6902=CARTESIAN_POINT('Ctrl Pts',(-21.0142484643566,21.5615737698344,-73.695998263067));
#6903=CARTESIAN_POINT('Ctrl Pts',(-21.0039040382932,21.574820151016,-73.6949277414588));
#6904=CARTESIAN_POINT('Ctrl Pts',(-20.9976009617988,21.5829717435713,-73.6942699296701));
#6905=CARTESIAN_POINT('Ctrl Pts',(-20.9872567245945,21.5964830695988,-73.6931811865302));
#6906=CARTESIAN_POINT('Ctrl Pts',(-20.9831929904259,21.6018254920664,-73.6927510997639));
#6907=CARTESIAN_POINT('Ctrl Pts',(-20.8772262041948,21.7420425799459,-73.6814736374));
#6908=CARTESIAN_POINT('Ctrl Pts',(-20.786088388299,21.8846967975081,-73.67023454867));
#6909=CARTESIAN_POINT('Ctrl Pts',(-20.6294657304119,22.1784032059693,-73.6477753594769));
#6910=CARTESIAN_POINT('Ctrl Pts',(-20.5635030056395,22.3286570098561,-73.6366003936102));
#6911=CARTESIAN_POINT('Ctrl Pts',(-20.4857445451581,22.5502775715763,-73.6210187343627));
#6912=CARTESIAN_POINT('Ctrl Pts',(-20.4644556141968,22.6180411500755,-73.6163715925069));
#6913=CARTESIAN_POINT('Ctrl Pts',(-20.4401615155956,22.7053640457343,-73.610576864214));
#6914=CARTESIAN_POINT('Ctrl Pts',(-20.435074213302,22.7243186538684,-73.6093305482742));
#6915=CARTESIAN_POINT('Ctrl Pts',(-20.428186704274,22.7509499254413,-73.607596696327));
#6916=CARTESIAN_POINT('Ctrl Pts',(-20.4262411546113,22.7585880787836,-73.6071013853896));
#6917=CARTESIAN_POINT('Ctrl Pts',(-20.423344100896,22.7701387966519,-73.6063554221177));
#6918=CARTESIAN_POINT('Ctrl Pts',(-20.422371892099,22.7740460649213,-73.6061036136483));
#6919=CARTESIAN_POINT('Ctrl Pts',(-20.4206000450068,22.7812244344559,-73.6056419792606));
#6920=CARTESIAN_POINT('Ctrl Pts',(-20.4197982078921,22.7844949795886,-73.605432028118));
#6921=CARTESIAN_POINT('Ctrl Pts',(-20.418516376307,22.7897589947419,-73.6050947163301));
#6922=CARTESIAN_POINT('Ctrl Pts',(-20.4180331583697,22.7917516654239,-73.6049671687204));
#6923=CARTESIAN_POINT('Ctrl Pts',(-20.4171119860626,22.7955662426078,-73.6047232741843));
#6924=CARTESIAN_POINT('Ctrl Pts',(-20.4166737220293,22.7973880569998,-73.6046069101104));
#6925=CARTESIAN_POINT('Ctrl Pts',(-20.4156760752098,22.8015511257531,-73.604341272812));
#6926=CARTESIAN_POINT('Ctrl Pts',(-20.4151177274076,22.8038926212885,-73.6041920604894));
#6927=CARTESIAN_POINT('Ctrl Pts',(-20.4136717905408,22.8099865758389,-73.6038042211352));
#6928=CARTESIAN_POINT('Ctrl Pts',(-20.4127883088303,22.8137400187149,-73.6035658319005));
#6929=CARTESIAN_POINT('Ctrl Pts',(-20.4073772073704,22.8369153285242,-73.6020969038803));
#6930=CARTESIAN_POINT('Ctrl Pts',(-20.4030230767316,22.8563778490695,-73.6008762390203));
#6931=CARTESIAN_POINT('Ctrl Pts',(-20.3972964150641,22.8831390524395,-73.5992139530539));
#6932=CARTESIAN_POINT('Ctrl Pts',(-20.3957681350738,22.8904034115707,-73.5987643501517));
#6933=CARTESIAN_POINT('Ctrl Pts',(-20.3929826225252,22.9038746336809,-73.5979334973003));
#6934=CARTESIAN_POINT('Ctrl Pts',(-20.3917185631697,22.9100800257116,-73.5975519118949));
#6935=CARTESIAN_POINT('Ctrl Pts',(-20.3556743053576,23.0897306488406,-73.5865366203628));
#6936=CARTESIAN_POINT('Ctrl Pts',(-20.3352106074342,23.2657667413021,-73.5765925619934));
#6937=CARTESIAN_POINT('Ctrl Pts',(-20.3240454113311,23.5998654555163,-73.5578950111063));
#6938=CARTESIAN_POINT('Ctrl Pts',(-20.3303135582794,23.7572895311376,-73.5491548076088));
#6939=CARTESIAN_POINT('Ctrl Pts',(-20.362713992734,24.0428208619325,-73.5327085040281));
#6940=CARTESIAN_POINT('Ctrl Pts',(-20.3851791635773,24.1710020138349,-73.5251037329687));
#6941=CARTESIAN_POINT('Ctrl Pts',(-20.4185226257497,24.3108943111876,-73.5164077662797));
#6942=CARTESIAN_POINT('Ctrl Pts',(-20.4218094327274,24.3243015532919,-73.5155703324412));
#6943=CARTESIAN_POINT('Ctrl Pts',(-20.427712554048,24.3477291112185,-73.5140997978857));
#6944=CARTESIAN_POINT('Ctrl Pts',(-20.4302912370297,24.3577587686641,-73.5134679171008));
#6945=CARTESIAN_POINT('Ctrl Pts',(-20.434083898284,24.3722207351997,-73.5125533776723));
#6946=CARTESIAN_POINT('Ctrl Pts',(-20.4352591046716,24.3766632217766,-73.5122719789936));
#6947=CARTESIAN_POINT('Ctrl Pts',(-20.4373215804574,24.38439283631,-73.5117815465301));
#6948=CARTESIAN_POINT('Ctrl Pts',(-20.4382045670207,24.38768110798,-73.5115726523618));
#6949=CARTESIAN_POINT('Ctrl Pts',(-20.4399169954336,24.394018137354,-73.5111695790786));
#6950=CARTESIAN_POINT('Ctrl Pts',(-20.4407457135376,24.3970670882169,-73.5109754237381));
#6951=CARTESIAN_POINT('Ctrl Pts',(-20.4427156825568,24.4042729507486,-73.5105160274139));
#6952=CARTESIAN_POINT('Ctrl Pts',(-20.4438607908298,24.4084287938441,-73.5102506608692));
#6953=CARTESIAN_POINT('Ctrl Pts',(-20.4472887751136,24.4207729205915,-73.5094611893633));
#6954=CARTESIAN_POINT('Ctrl Pts',(-20.4495957003912,24.4289544347353,-73.50893630005));
#6955=CARTESIAN_POINT('Ctrl Pts',(-20.4710094267654,24.5037638383739,-73.5041216907847));
#6956=CARTESIAN_POINT('Ctrl Pts',(-20.492227406454,24.5697637077898,-73.4997631113147));
#6957=CARTESIAN_POINT('Ctrl Pts',(-20.5188236003766,24.6441677387285,-73.4947160399268));
#6958=CARTESIAN_POINT('Ctrl Pts',(-20.5221332328792,24.6532962093144,-73.4940945131101));
#6959=CARTESIAN_POINT('Ctrl Pts',(-20.5841168297762,24.8218749577686,-73.4825736640319));
#6960=CARTESIAN_POINT('Ctrl Pts',(-20.6552603631311,24.9764331059884,-73.4712780980678));
#6961=CARTESIAN_POINT('Ctrl Pts',(-20.8295286715011,25.2876921481589,-73.4472084338869));
#6962=CARTESIAN_POINT('Ctrl Pts',(-20.9348248520234,25.4424939465576,-73.4344429208427));
#6963=CARTESIAN_POINT('Ctrl Pts',(-21.0961741495497,25.6402989949978,-73.4176740415605));
#6964=CARTESIAN_POINT('Ctrl Pts',(-21.1410830942451,25.6919105714252,-73.4132537704316));
#6965=CARTESIAN_POINT('Ctrl Pts',(-21.1925584229928,25.7473982061385,-73.4084872928207));
#6966=CARTESIAN_POINT('Ctrl Pts',(-21.1975307190187,25.7527217595166,-73.4080298436341));
#6967=CARTESIAN_POINT('Ctrl Pts',(-21.2051249552495,25.7607974102057,-73.4073357477571));
#6968=CARTESIAN_POINT('Ctrl Pts',(-21.2077337444805,25.7635617603417,-73.4070981251452));
#6969=CARTESIAN_POINT('Ctrl Pts',(-21.2120029816633,25.7680695667169,-73.4067105981867));
#6970=CARTESIAN_POINT('Ctrl Pts',(-21.2136604941682,25.7698157791186,-73.4065604706438));
#6971=CARTESIAN_POINT('Ctrl Pts',(-21.2168570882644,25.7731758863011,-73.4062715765223));
#6972=CARTESIAN_POINT('Ctrl Pts',(-21.2183958904462,25.7747900433169,-73.4061327884906));
#6973=CARTESIAN_POINT('Ctrl Pts',(-21.2211986716251,25.7777239723194,-73.4058805143548));
#6974=CARTESIAN_POINT('Ctrl Pts',(-21.2224620912472,25.7790442598073,-73.4057669858953));
#6975=CARTESIAN_POINT('Ctrl Pts',(-21.2250322014036,25.78172548417,-73.405536426412));
#6976=CARTESIAN_POINT('Ctrl Pts',(-21.2263389589364,25.7830863428913,-73.4054194016712));
#6977=CARTESIAN_POINT('Ctrl Pts',(-21.2300743839009,25.7869695870701,-73.4050854544928));
#6978=CARTESIAN_POINT('Ctrl Pts',(-21.2325059777905,25.7894891729297,-73.404868760672));
#6979=CARTESIAN_POINT('Ctrl Pts',(-21.2429536235344,25.8002796370593,-73.4039406403197));
#6980=CARTESIAN_POINT('Ctrl Pts',(-21.251010006268,25.8085116056728,-73.4032323311843));
#6981=CARTESIAN_POINT('Ctrl Pts',(-21.3922155024301,25.9512556148662,-73.3909418399778));
#6982=CARTESIAN_POINT('Ctrl Pts',(-21.536938042602,26.0738466826071,-73.3802472402356));
#6983=CARTESIAN_POINT('Ctrl Pts',(-21.8138821578065,26.2693586443004,-73.3612607451901));
#6984=CARTESIAN_POINT('Ctrl Pts',(-21.9420042342511,26.3470442060735,-73.3529587830562));
#6985=CARTESIAN_POINT('Ctrl Pts',(-22.0750360358082,26.4155367850914,-73.3444460357026));
#6986=CARTESIAN_POINT('Origin',(-23.5502525316942,23.5502525316942,-77.3107734492734));
#6987=CARTESIAN_POINT('',(-22.0750359824043,26.4155367575959,-71.8489552970435));
#6988=CARTESIAN_POINT('',(-22.0750360205127,26.4155367772164,-72.0953994964366));
#6989=CARTESIAN_POINT('',(-22.0750360153461,26.4155367745563,-77.3107734492734));
#6990=CARTESIAN_POINT('Ctrl Pts',(-22.0750359824043,26.4155367575959,-71.8489552970435));
#6991=CARTESIAN_POINT('Ctrl Pts',(-21.9777291534232,26.3654374888483,-71.8553412661841));
#6992=CARTESIAN_POINT('Ctrl Pts',(-21.8830050340865,26.3103970587655,-71.8615301479144));
#6993=CARTESIAN_POINT('Ctrl Pts',(-21.6716115338078,26.1726957195411,-71.8756798750198));
#6994=CARTESIAN_POINT('Ctrl Pts',(-21.5572972618043,26.0869095881927,-71.8835940046763));
#6995=CARTESIAN_POINT('Ctrl Pts',(-21.3160947428769,25.8795020721675,-71.9016071275874));
#6996=CARTESIAN_POINT('Ctrl Pts',(-21.1927128203315,25.7545341372085,-71.9117715040743));
#6997=CARTESIAN_POINT('Ctrl Pts',(-21.0715695807337,25.6099674165137,-71.9232295631562));
#6998=CARTESIAN_POINT('Ctrl Pts',(-21.0630875385045,25.599717063337,-71.9240403537687));
#6999=CARTESIAN_POINT('Ctrl Pts',(-21.0514487236261,25.5854731581692,-71.9251649049877));
#7000=CARTESIAN_POINT('Ctrl Pts',(-21.0482374943415,25.5815241093113,-71.9254764571077));
#7001=CARTESIAN_POINT('Ctrl Pts',(-21.0428325947734,25.5748451048418,-71.9260030137902));
#7002=CARTESIAN_POINT('Ctrl Pts',(-21.0406339871695,25.5721191415714,-71.926217818704));
#7003=CARTESIAN_POINT('Ctrl Pts',(-21.0362924530504,25.5667182598519,-71.9266432044628));
#7004=CARTESIAN_POINT('Ctrl Pts',(-21.0341493414999,25.5640434955213,-71.9268537774642));
#7005=CARTESIAN_POINT('Ctrl Pts',(-21.0294356578141,25.5581411928867,-71.9273182291355));
#7006=CARTESIAN_POINT('Ctrl Pts',(-21.0268670116346,25.5549121298034,-71.9275721846476));
#7007=CARTESIAN_POINT('Ctrl Pts',(-21.0179197566787,25.5436200287897,-71.9284597945172));
#7008=CARTESIAN_POINT('Ctrl Pts',(-21.0115735870028,25.5355314727357,-71.929094743219));
#7009=CARTESIAN_POINT('Ctrl Pts',(-20.947076924091,25.4525118381883,-71.9356034220269));
#7010=CARTESIAN_POINT('Ctrl Pts',(-20.8922280604317,25.3750858285623,-71.9416066058685));
#7011=CARTESIAN_POINT('Ctrl Pts',(-20.6944986942914,25.0681001448142,-71.9651949418541));
#7012=CARTESIAN_POINT('Ctrl Pts',(-20.5773115792254,24.823347305175,-71.9836804191454));
#7013=CARTESIAN_POINT('Ctrl Pts',(-20.4666212653899,24.4903796442771,-72.0072705451087));
#7014=CARTESIAN_POINT('Ctrl Pts',(-20.4440613567244,24.4129220786975,-72.0126455682629));
#7015=CARTESIAN_POINT('Ctrl Pts',(-20.4147584566119,24.2961568345057,-72.020509570936));
#7016=CARTESIAN_POINT('Ctrl Pts',(-20.4058000343932,24.2574407161664,-72.0230784833591));
#7017=CARTESIAN_POINT('Ctrl Pts',(-20.3939415007324,24.2014995100962,-72.0267257059563));
#7018=CARTESIAN_POINT('Ctrl Pts',(-20.3904620636705,24.1844024984702,-72.0278317614911));
#7019=CARTESIAN_POINT('Ctrl Pts',(-20.3857378469712,24.160184171031,-72.0293855297584));
#7020=CARTESIAN_POINT('Ctrl Pts',(-20.3843779882386,24.1530859845995,-72.0298393529876));
#7021=CARTESIAN_POINT('Ctrl Pts',(-20.3823431850721,24.14226792485,-72.0305285496676));
#7022=CARTESIAN_POINT('Ctrl Pts',(-20.381650899973,24.1385513961735,-72.0307648810856));
#7023=CARTESIAN_POINT('Ctrl Pts',(-20.3805298232945,24.1324735155421,-72.0311506386431));
#7024=CARTESIAN_POINT('Ctrl Pts',(-20.3800971294116,24.130112900788,-72.0313002846857));
#7025=CARTESIAN_POINT('Ctrl Pts',(-20.3792683836582,24.125562922286,-72.031588370905));
#7026=CARTESIAN_POINT('Ctrl Pts',(-20.3788719615023,24.1233736285842,-72.0317268321561));
#7027=CARTESIAN_POINT('Ctrl Pts',(-20.3781687280862,24.119466857948,-72.0319736343711));
#7028=CARTESIAN_POINT('Ctrl Pts',(-20.3778610452337,24.1177495475479,-72.0320820251874));
#7029=CARTESIAN_POINT('Ctrl Pts',(-20.3772268812357,24.1141933725559,-72.0323062784514));
#7030=CARTESIAN_POINT('Ctrl Pts',(-20.3769006050758,24.1123544800355,-72.0324221287565));
#7031=CARTESIAN_POINT('Ctrl Pts',(-20.3759834211874,24.1071589803208,-72.0327491354142));
#7032=CARTESIAN_POINT('Ctrl Pts',(-20.3753962371025,24.1038017051077,-72.0329600781));
#7033=CARTESIAN_POINT('Ctrl Pts',(-20.3729775816292,24.0898423864206,-72.0338356682477));
#7034=CARTESIAN_POINT('Ctrl Pts',(-20.3711938545097,24.0792319777876,-72.0344976169819));
#7035=CARTESIAN_POINT('Ctrl Pts',(-20.3401319842542,23.888628460456,-72.0463277098167));
#7036=CARTESIAN_POINT('Ctrl Pts',(-20.3261253554334,23.7064489255816,-72.0566676403883));
#7037=CARTESIAN_POINT('Ctrl Pts',(-20.3289657225009,23.3572673473885,-72.0762462254496));
#7038=CARTESIAN_POINT('Ctrl Pts',(-20.3432654359956,23.1908583874367,-72.0854778049068));
#7039=CARTESIAN_POINT('Ctrl Pts',(-20.3880039481781,22.9193370622962,-72.1011787405092));
#7040=CARTESIAN_POINT('Ctrl Pts',(-20.4110137617024,22.8133352814155,-72.1074702243302));
#7041=CARTESIAN_POINT('Ctrl Pts',(-20.4520811771191,22.6615228375527,-72.1168424069214));
#7042=CARTESIAN_POINT('Ctrl Pts',(-20.4659144919076,22.6146432805094,-72.1197873257624));
#7043=CARTESIAN_POINT('Ctrl Pts',(-20.4832105835241,22.5605892511582,-72.1232482174252));
#7044=CARTESIAN_POINT('Ctrl Pts',(-20.4856408279504,22.5530891427696,-72.1237298930721));
#7045=CARTESIAN_POINT('Ctrl Pts',(-20.4893809463424,22.5416893839822,-72.1244642792005));
#7046=CARTESIAN_POINT('Ctrl Pts',(-20.4906708185243,22.5377831617258,-72.1247163284514));
#7047=CARTESIAN_POINT('Ctrl Pts',(-20.4930234644322,22.5307040091725,-72.1251738516152));
#7048=CARTESIAN_POINT('Ctrl Pts',(-20.4940837091341,22.527530239298,-72.1253792415711));
#7049=CARTESIAN_POINT('Ctrl Pts',(-20.49621411608,22.52118590791,-72.1257903571472));
#7050=CARTESIAN_POINT('Ctrl Pts',(-20.4972842774074,22.5180153504142,-72.1259960825283));
#7051=CARTESIAN_POINT('Ctrl Pts',(-20.5003118511548,22.5090914779391,-72.1265758876328));
#7052=CARTESIAN_POINT('Ctrl Pts',(-20.5022805943097,22.5033420470909,-72.1269503429847));
#7053=CARTESIAN_POINT('Ctrl Pts',(-20.5104606266446,22.4796720993922,-72.1284956901964));
#7054=CARTESIAN_POINT('Ctrl Pts',(-20.5168136933384,22.4618013030087,-72.129671288589));
#7055=CARTESIAN_POINT('Ctrl Pts',(-20.5257780582922,22.4372732726301,-72.1312972975468));
#7056=CARTESIAN_POINT('Ctrl Pts',(-20.5282544118218,22.4305668465466,-72.1317431702275));
#7057=CARTESIAN_POINT('Ctrl Pts',(-20.5312044853172,22.4226585779567,-72.1322704820308));
#7058=CARTESIAN_POINT('Ctrl Pts',(-20.5316566540999,22.4214486698116,-72.1323511994399));
#7059=CARTESIAN_POINT('Ctrl Pts',(-20.5357117980481,22.4106178219614,-72.1330741460223));
#7060=CARTESIAN_POINT('Ctrl Pts',(-20.539359997375,22.4010139797499,-72.1337178842916));
#7061=CARTESIAN_POINT('Ctrl Pts',(-20.5469034077748,22.3814385145636,-72.1350355611625));
#7062=CARTESIAN_POINT('Ctrl Pts',(-20.5508025066026,22.3714685356557,-72.1357096229055));
#7063=CARTESIAN_POINT('Ctrl Pts',(-20.5572984607302,22.3550993268493,-72.1368212321806));
#7064=CARTESIAN_POINT('Ctrl Pts',(-20.5598663606759,22.3486886337079,-72.1372578152524));
#7065=CARTESIAN_POINT('Ctrl Pts',(-20.564660582047,22.3368305510708,-72.1380676888874));
#7066=CARTESIAN_POINT('Ctrl Pts',(-20.5668812614038,22.3313808995148,-72.1384407918372));
#7067=CARTESIAN_POINT('Ctrl Pts',(-20.5736315613165,22.3149443144508,-72.1395688480641));
#7068=CARTESIAN_POINT('Ctrl Pts',(-20.5782070027763,22.3039764142392,-72.1403253000523));
#7069=CARTESIAN_POINT('Ctrl Pts',(-20.5881904122782,22.280412595688,-72.1419585326713));
#7070=CARTESIAN_POINT('Ctrl Pts',(-20.5936182765269,22.267825405309,-72.1428359461744));
#7071=CARTESIAN_POINT('Ctrl Pts',(-20.7019342245609,22.0209843318913,-72.160140838154));
#7072=CARTESIAN_POINT('Ctrl Pts',(-20.8322636547231,21.7998030102599,-72.1775039521415));
#7073=CARTESIAN_POINT('Ctrl Pts',(-21.0914865460765,21.4597736467118,-72.2063861223673));
#7074=CARTESIAN_POINT('Ctrl Pts',(-21.2064159121376,21.3316767577781,-72.2178761529594));
#7075=CARTESIAN_POINT('Ctrl Pts',(-21.3346565448832,21.2098942156211,-72.2289734905258));
#7076=CARTESIAN_POINT('Ctrl Pts',(-21.338294733384,21.2064553297857,-72.2292870003297));
#7077=CARTESIAN_POINT('Ctrl Pts',(-21.3440586288385,21.2010325591233,-72.2297815798355));
#7078=CARTESIAN_POINT('Ctrl Pts',(-21.3461790139652,21.19904306737,-72.2299630740623));
#7079=CARTESIAN_POINT('Ctrl Pts',(-21.3501927173132,21.1952873345385,-72.2303057747627));
#7080=CARTESIAN_POINT('Ctrl Pts',(-21.3520854754084,21.1935205020732,-72.230467026579));
#7081=CARTESIAN_POINT('Ctrl Pts',(-21.3553544641469,21.1904763641217,-72.2307449067749));
#7082=CARTESIAN_POINT('Ctrl Pts',(-21.3567296835061,21.1891979786376,-72.2308616189321));
#7083=CARTESIAN_POINT('Ctrl Pts',(-21.3593900727635,21.1867292470412,-72.2310870359558));
#7084=CARTESIAN_POINT('Ctrl Pts',(-21.3606750942658,21.1855387484659,-72.2311957528207));
#7085=CARTESIAN_POINT('Ctrl Pts',(-21.3637004504339,21.1827405101829,-72.2314513235572));
#7086=CARTESIAN_POINT('Ctrl Pts',(-21.3654415915475,21.1811336381043,-72.2315981103094));
#7087=CARTESIAN_POINT('Ctrl Pts',(-21.3705773720386,21.1764043828781,-72.2320302093342));
#7088=CARTESIAN_POINT('Ctrl Pts',(-21.3739769624592,21.1732873483914,-72.2323151130392));
#7089=CARTESIAN_POINT('Ctrl Pts',(-21.4031846320796,21.1466224535026,-72.2347533989894));
#7090=CARTESIAN_POINT('Ctrl Pts',(-21.4293686193564,21.1234872376781,-72.2368760140068));
#7091=CARTESIAN_POINT('Ctrl Pts',(-21.460783207273,21.0966273846338,-72.2393561618848));
#7092=CARTESIAN_POINT('Ctrl Pts',(-21.4656538627591,21.0924879354044,-72.2397388401132));
#7093=CARTESIAN_POINT('Ctrl Pts',(-21.4716997283573,21.0873806057529,-72.2402116079772));
#7094=CARTESIAN_POINT('Ctrl Pts',(-21.4728633140779,21.0863990623501,-72.2403024942067));
#7095=CARTESIAN_POINT('Ctrl Pts',(-21.4771658183141,21.0827748970356,-72.2406381805694));
#7096=CARTESIAN_POINT('Ctrl Pts',(-21.4803091007653,21.0801374348168,-72.2408826826033));
#7097=CARTESIAN_POINT('Ctrl Pts',(-21.4850460500589,21.0761781517422,-72.2412500514004));
#7098=CARTESIAN_POINT('Ctrl Pts',(-21.4866359559471,21.0748518615668,-72.2413731693396));
#7099=CARTESIAN_POINT('Ctrl Pts',(-21.6612455209653,20.9294787201626,-72.254874260667));
#7100=CARTESIAN_POINT('Ctrl Pts',(-21.8489032789655,20.8039388854537,-72.2672431215133));
#7101=CARTESIAN_POINT('Ctrl Pts',(-22.1509140677271,20.64483267797,-72.2863604295186));
#7102=CARTESIAN_POINT('Ctrl Pts',(-22.2565396898978,20.5962861569875,-72.2929097634569));
#7103=CARTESIAN_POINT('Ctrl Pts',(-22.4411712549438,20.5232331816516,-72.304371504602));
#7104=CARTESIAN_POINT('Ctrl Pts',(-22.5189215182431,20.4958684455546,-72.309201141605));
#7105=CARTESIAN_POINT('Ctrl Pts',(-22.6378260914721,20.4590770404931,-72.3166436325809));
#7106=CARTESIAN_POINT('Ctrl Pts',(-22.6782597576692,20.4474286125936,-72.3191838685214));
#7107=CARTESIAN_POINT('Ctrl Pts',(-22.7262265413084,20.4346216001707,-72.3222121398206));
#7108=CARTESIAN_POINT('Ctrl Pts',(-22.7335514206105,20.4326935141443,-72.3226749799785));
#7109=CARTESIAN_POINT('Ctrl Pts',(-22.7448012344292,20.4297746585994,-72.3233864643725));
#7110=CARTESIAN_POINT('Ctrl Pts',(-22.7487213865226,20.4287654226674,-72.3236345094717));
#7111=CARTESIAN_POINT('Ctrl Pts',(-22.7555678130577,20.4270165702933,-72.3240679234259));
#7112=CARTESIAN_POINT('Ctrl Pts',(-22.75849325071,20.4262736723706,-72.3242531857306));
#7113=CARTESIAN_POINT('Ctrl Pts',(-22.7650832510381,20.4246100313381,-72.3246706706643));
#7114=CARTESIAN_POINT('Ctrl Pts',(-22.7687483932925,20.4236916221987,-72.3249029685249));
#7115=CARTESIAN_POINT('Ctrl Pts',(-22.7785742756673,20.4212478156044,-72.3255260255025));
#7116=CARTESIAN_POINT('Ctrl Pts',(-22.7847378976524,20.4197341739326,-72.3259171640728));
#7117=CARTESIAN_POINT('Ctrl Pts',(-22.8114845180007,20.4132495422801,-72.3276158359357));
#7118=CARTESIAN_POINT('Ctrl Pts',(-22.8321113843946,20.4084633612162,-72.3289293178218));
#7119=CARTESIAN_POINT('Ctrl Pts',(-22.8656332182331,20.4010324399458,-72.3310699286203));
#7120=CARTESIAN_POINT('Ctrl Pts',(-22.8785000792891,20.3982627752031,-72.3318929958256));
#7121=CARTESIAN_POINT('Ctrl Pts',(-22.8973149140474,20.3943332127647,-72.3330986856588));
#7122=CARTESIAN_POINT('Ctrl Pts',(-22.9032498844473,20.3931111262805,-72.3334793201486));
#7123=CARTESIAN_POINT('Ctrl Pts',(-22.9175212831654,20.3902143942384,-72.3343953590149));
#7124=CARTESIAN_POINT('Ctrl Pts',(-22.9258609289715,20.3885559954558,-72.3349312740036));
#7125=CARTESIAN_POINT('Ctrl Pts',(-22.9357176618942,20.3866364321928,-72.3355654177624));
#7126=CARTESIAN_POINT('Ctrl Pts',(-22.9372285557843,20.3863433142591,-72.3356626432658));
#7127=CARTESIAN_POINT('Ctrl Pts',(-22.9504859006057,20.3837812025614,-72.3365159289196));
#7128=CARTESIAN_POINT('Ctrl Pts',(-22.9622445651909,20.3815765755326,-72.3372739951741));
#7129=CARTESIAN_POINT('Ctrl Pts',(-22.9779258405216,20.3787267916119,-72.3382866209504));
#7130=CARTESIAN_POINT('Ctrl Pts',(-22.981837871107,20.3780233257826,-72.338539380669));
#7131=CARTESIAN_POINT('Ctrl Pts',(-22.9906961328552,20.3764473351559,-72.3391120351599));
#7132=CARTESIAN_POINT('Ctrl Pts',(-22.9956431141157,20.37557913392,-72.3394320612992));
#7133=CARTESIAN_POINT('Ctrl Pts',(-23.0216604490222,20.3710757282314,-72.3411163231002));
#7134=CARTESIAN_POINT('Ctrl Pts',(-23.0427641804424,20.3676387824754,-72.3424865316952));
#7135=CARTESIAN_POINT('Ctrl Pts',(-23.3621365272321,20.3188832018215,-72.3632836424348));
#7136=CARTESIAN_POINT('Ctrl Pts',(-23.6652637311821,20.3154655364759,-72.3840330942772));
#7137=CARTESIAN_POINT('Ctrl Pts',(-24.0313702638923,20.3629009939869,-72.408712319235));
#7138=CARTESIAN_POINT('Ctrl Pts',(-24.0981007429276,20.3736903122922,-72.4131852351952));
#7139=CARTESIAN_POINT('Ctrl Pts',(-24.2133381993442,20.3960623864423,-72.4208138778078));
#7140=CARTESIAN_POINT('Ctrl Pts',(-24.2620068863861,20.4066869632356,-72.4240055181291));
#7141=CARTESIAN_POINT('Ctrl Pts',(-24.3162994703718,20.4198649608222,-72.4275172992848));
#7142=CARTESIAN_POINT('Ctrl Pts',(-24.3221820927456,20.4213103765406,-72.4278971559662));
#7143=CARTESIAN_POINT('Ctrl Pts',(-24.3312906976889,20.4235756977035,-72.4284842835377));
#7144=CARTESIAN_POINT('Ctrl Pts',(-24.3345195058716,20.4243840196792,-72.4286922051947));
#7145=CARTESIAN_POINT('Ctrl Pts',(-24.3398902796061,20.425737421379,-72.4290377163125));
#7146=CARTESIAN_POINT('Ctrl Pts',(-24.3420329374471,20.4262797026431,-72.4291754659622));
#7147=CARTESIAN_POINT('Ctrl Pts',(-24.3462001499589,20.4273389373883,-72.4294431927061));
#7148=CARTESIAN_POINT('Ctrl Pts',(-24.348224762364,20.4278556562696,-72.4295731833326));
#7149=CARTESIAN_POINT('Ctrl Pts',(-24.3520168662245,20.428827401178,-72.4298164993709));
#7150=CARTESIAN_POINT('Ctrl Pts',(-24.3537844616703,20.4292819565245,-72.4299298510646));
#7151=CARTESIAN_POINT('Ctrl Pts',(-24.3578025827445,20.4303188975417,-72.430187378812));
#7152=CARTESIAN_POINT('Ctrl Pts',(-24.36005286077,20.4309022157488,-72.4303314995742));
#7153=CARTESIAN_POINT('Ctrl Pts',(-24.365771246557,20.4323911434937,-72.4306974803245));
#7154=CARTESIAN_POINT('Ctrl Pts',(-24.369238488558,20.4333001077603,-72.4309191452699));
#7155=CARTESIAN_POINT('Ctrl Pts',(-24.3883551037096,20.4383457760665,-72.4321400000635));
#7156=CARTESIAN_POINT('Ctrl Pts',(-24.4039750222881,20.442594649655,-72.4331327595173));
#7157=CARTESIAN_POINT('Ctrl Pts',(-24.7094583233584,20.5281682197159,-72.4524664718376));
#7158=CARTESIAN_POINT('Ctrl Pts',(-24.9865995929362,20.6496098320321,-72.4686576850556));
#7159=CARTESIAN_POINT('Ctrl Pts',(-25.3126511677611,20.8508470818915,-72.4902690497409));
#7160=CARTESIAN_POINT('Ctrl Pts',(-25.380744556037,20.8965501001412,-72.4949353947562));
#7161=CARTESIAN_POINT('Ctrl Pts',(-25.5102313377665,20.9908162278489,-72.5042050018888));
#7162=CARTESIAN_POINT('Ctrl Pts',(-25.571744180153,21.0391170872353,-72.5087979869266));
#7163=CARTESIAN_POINT('Ctrl Pts',(-25.6617446867427,21.1152383374561,-72.5158548421325));
#7164=CARTESIAN_POINT('Ctrl Pts',(-25.6915754173723,21.1414293062824,-72.5182530021999));
#7165=CARTESIAN_POINT('Ctrl Pts',(-25.7264215175184,21.1731825639828,-72.5211288614429));
#7166=CARTESIAN_POINT('Ctrl Pts',(-25.7319117638342,21.1782204746584,-72.5215842186927));
#7167=CARTESIAN_POINT('Ctrl Pts',(-25.740338177641,21.1860066478047,-72.5222865901318));
#7168=CARTESIAN_POINT('Ctrl Pts',(-25.7432867804627,21.1887414646936,-72.5225330290847));
#7169=CARTESIAN_POINT('Ctrl Pts',(-25.748653055057,21.1937373802264,-72.5229827464392));
#7170=CARTESIAN_POINT('Ctrl Pts',(-25.7510723802493,21.195996701438,-72.5231859483396));
#7171=CARTESIAN_POINT('Ctrl Pts',(-25.755964726714,21.2005796203704,-72.523597780786));
#7172=CARTESIAN_POINT('Ctrl Pts',(-25.7584375671663,21.2029034041796,-72.5238064192189));
#7173=CARTESIAN_POINT('Ctrl Pts',(-25.7654985778125,21.2095598263624,-72.5244035412513));
#7174=CARTESIAN_POINT('Ctrl Pts',(-25.7700776796803,21.2139020235089,-72.5247924380626));
#7175=CARTESIAN_POINT('Ctrl Pts',(-25.7897424767466,21.2326594427524,-72.526469742548));
#7176=CARTESIAN_POINT('Ctrl Pts',(-25.8047004632204,21.2472072800857,-72.527763916228));
#7177=CARTESIAN_POINT('Ctrl Pts',(-26.0705967407166,21.5108853698052,-72.5511055858821));
#7178=CARTESIAN_POINT('Ctrl Pts',(-26.2789393451483,21.7994567368782,-72.5752273288794));
#7179=CARTESIAN_POINT('Ctrl Pts',(-26.465544546221,22.1749239035985,-72.6034019168748));
#7180=CARTESIAN_POINT('Ctrl Pts',(-26.4930465590552,22.234798044973,-72.6077960018667));
#7181=CARTESIAN_POINT('Ctrl Pts',(-26.5436492890504,22.3545096144307,-72.6163377765977));
#7182=CARTESIAN_POINT('Ctrl Pts',(-26.5668387211603,22.4142796741457,-72.6204870855576));
#7183=CARTESIAN_POINT('Ctrl Pts',(-26.5934400647382,22.4894175976518,-72.6255275210407));
#7184=CARTESIAN_POINT('Ctrl Pts',(-26.5985416333777,22.5041671170987,-72.6265086575913));
#7185=CARTESIAN_POINT('Ctrl Pts',(-26.6047295868064,22.5224872886051,-72.6277165468396));
#7186=CARTESIAN_POINT('Ctrl Pts',(-26.6059170677132,22.5260232025104,-72.6279491822946));
#7187=CARTESIAN_POINT('Ctrl Pts',(-26.6077782979381,22.5315973596767,-72.6283151295849));
#7188=CARTESIAN_POINT('Ctrl Pts',(-26.6084561493253,22.5336342139877,-72.6284486847928));
#7189=CARTESIAN_POINT('Ctrl Pts',(-26.6097197214898,22.5374437824164,-72.6286981639813));
#7190=CARTESIAN_POINT('Ctrl Pts',(-26.6103059330636,22.5392163162974,-72.6288141165264));
#7191=CARTESIAN_POINT('Ctrl Pts',(-26.6116190286327,22.5431983404738,-72.62907432295));
#7192=CARTESIAN_POINT('Ctrl Pts',(-26.6123450595428,22.545408104124,-72.6292185254383));
#7193=CARTESIAN_POINT('Ctrl Pts',(-26.6141852146144,22.5510293551839,-72.6295848599222));
#7194=CARTESIAN_POINT('Ctrl Pts',(-26.6152960371554,22.5544419313,-72.6298067962042));
#7195=CARTESIAN_POINT('Ctrl Pts',(-26.6214029148697,22.5733099958477,-72.6310313746163));
#7196=CARTESIAN_POINT('Ctrl Pts',(-26.626287887589,22.588801591821,-72.6320275402137));
#7197=CARTESIAN_POINT('Ctrl Pts',(-26.7248916703118,22.9099471182035,-72.6524998026793));
#7198=CARTESIAN_POINT('Ctrl Pts',(-26.7727489747728,23.2278829040988,-72.6695650113928));
#7199=CARTESIAN_POINT('Ctrl Pts',(-26.7731395527062,23.7224995396896,-72.6975928801036));
#7200=CARTESIAN_POINT('Ctrl Pts',(-26.7590578347791,23.8969868809995,-72.7077368667361));
#7201=CARTESIAN_POINT('Ctrl Pts',(-26.7290519982083,24.0808028784832,-72.7190629401086));
#7202=CARTESIAN_POINT('Ctrl Pts',(-26.7271392598985,24.0921385248448,-72.7197639288064));
#7203=CARTESIAN_POINT('Ctrl Pts',(-26.7244033267836,24.1078402190251,-72.7207384940478));
#7204=CARTESIAN_POINT('Ctrl Pts',(-26.7236316758482,24.1122152583552,-72.7210104281687));
#7205=CARTESIAN_POINT('Ctrl Pts',(-26.7222893111018,24.1197351463267,-72.7214785023811));
#7206=CARTESIAN_POINT('Ctrl Pts',(-26.721722959129,24.1228807759146,-72.7216745031935));
#7207=CARTESIAN_POINT('Ctrl Pts',(-26.7205465398087,24.1293595569638,-72.7220786067355));
#7208=CARTESIAN_POINT('Ctrl Pts',(-26.7199358935016,24.1326925975788,-72.7222867276887));
#7209=CARTESIAN_POINT('Ctrl Pts',(-26.7185060201455,24.1404283106931,-72.7227702913915));
#7210=CARTESIAN_POINT('Ctrl Pts',(-26.7176828721995,24.1448302431195,-72.7230458590531));
#7211=CARTESIAN_POINT('Ctrl Pts',(-26.715045990241,24.1587705658784,-72.7239198220993));
#7212=CARTESIAN_POINT('Ctrl Pts',(-26.7131983376488,24.1683024151757,-72.724519300635));
#7213=CARTESIAN_POINT('Ctrl Pts',(-26.681546985842,24.3277287179517,-72.7345781686208));
#7214=CARTESIAN_POINT('Ctrl Pts',(-26.6411660145329,24.4753014730892,-72.7443807014553));
#7215=CARTESIAN_POINT('Ctrl Pts',(-26.5342127841754,24.7794231094666,-72.7656486709851));
#7216=CARTESIAN_POINT('Ctrl Pts',(-26.465411370887,24.9347090509299,-72.7771487632234));
#7217=CARTESIAN_POINT('Ctrl Pts',(-26.3269578320015,25.1906058697027,-72.7968275056138));
#7218=CARTESIAN_POINT('Ctrl Pts',(-26.2632064498773,25.2940232689196,-72.8050005531721));
#7219=CARTESIAN_POINT('Ctrl Pts',(-26.1850678330646,25.4060804532983,-72.8139364889437));
#7220=CARTESIAN_POINT('Ctrl Pts',(-26.1762788674388,25.418496264952,-72.8149276800251));
#7221=CARTESIAN_POINT('Ctrl Pts',(-26.1648304170246,25.4344286028968,-72.8162005712717));
#7222=CARTESIAN_POINT('Ctrl Pts',(-26.1622513064208,25.4380023527754,-72.8164861539765));
#7223=CARTESIAN_POINT('Ctrl Pts',(-26.1590290828877,25.4424479872635,-72.8168414777987));
#7224=CARTESIAN_POINT('Ctrl Pts',(-26.1583928633286,25.4433248352904,-72.8169115644473));
#7225=CARTESIAN_POINT('Ctrl Pts',(-26.1558068923294,25.4468850839916,-72.8171961487189));
#7226=CARTESIAN_POINT('Ctrl Pts',(-26.1538534335845,25.4495658045689,-72.8174104585923));
#7227=CARTESIAN_POINT('Ctrl Pts',(-26.1511454710819,25.4532698981009,-72.8177066177129));
#7228=CARTESIAN_POINT('Ctrl Pts',(-26.1503945020535,25.4542958381839,-72.8177886500965));
#7229=CARTESIAN_POINT('Ctrl Pts',(-26.1481278891553,25.4573885410731,-72.8180359480855));
#7230=CARTESIAN_POINT('Ctrl Pts',(-26.1466103830061,25.4594539456866,-72.8182011161122));
#7231=CARTESIAN_POINT('Ctrl Pts',(-26.1217003066156,25.4932732273269,-72.8209058162147));
#7232=CARTESIAN_POINT('Ctrl Pts',(-26.0977278818961,25.5245986956891,-72.8234141521142));
#7233=CARTESIAN_POINT('Ctrl Pts',(-26.070213032434,25.5592173033174,-72.8261823247367));
#7234=CARTESIAN_POINT('Ctrl Pts',(-26.0672326213908,25.5629501263868,-72.8264807571691));
#7235=CARTESIAN_POINT('Ctrl Pts',(-26.062735144519,25.5685573891051,-72.8269289520568));
#7236=CARTESIAN_POINT('Ctrl Pts',(-26.061224272843,25.570436754096,-72.8270791556201));
#7237=CARTESIAN_POINT('Ctrl Pts',(-26.0586054522387,25.5736868139997,-72.8273388777985));
#7238=CARTESIAN_POINT('Ctrl Pts',(-26.0574984884602,25.5750582954968,-72.8274484675571));
#7239=CARTESIAN_POINT('Ctrl Pts',(-26.0551912572214,25.5779120646658,-72.8276764801144));
#7240=CARTESIAN_POINT('Ctrl Pts',(-26.053990800291,25.5793941932541,-72.8277948882979));
#7241=CARTESIAN_POINT('Ctrl Pts',(-26.0511377967888,25.5829102306204,-72.8280757603484));
#7242=CARTESIAN_POINT('Ctrl Pts',(-26.0494840789561,25.5849431969942,-72.8282381391084));
#7243=CARTESIAN_POINT('Ctrl Pts',(-26.0439678112563,25.5917076433767,-72.8287783733276));
#7244=CARTESIAN_POINT('Ctrl Pts',(-26.0400942600907,25.5964301968834,-72.829155434366));
#7245=CARTESIAN_POINT('Ctrl Pts',(-26.0309136877108,25.6075582905587,-72.8300437715298));
#7246=CARTESIAN_POINT('Ctrl Pts',(-26.0255952164739,25.6139543882733,-72.8305542362187));
#7247=CARTESIAN_POINT('Ctrl Pts',(-25.830583953334,25.8466402374352,-72.8491230536153));
#7248=CARTESIAN_POINT('Ctrl Pts',(-25.6106763437511,26.045854643975,-72.8650564241307));
#7249=CARTESIAN_POINT('Ctrl Pts',(-25.2001645860434,26.325957729553,-72.8930255219344));
#7250=CARTESIAN_POINT('Ctrl Pts',(-25.023395032122,26.4236793804682,-72.9046130661058));
#7251=CARTESIAN_POINT('Ctrl Pts',(-24.8267094650557,26.5094662182072,-72.9176484156279));
#7252=CARTESIAN_POINT('Ctrl Pts',(-24.8147134749497,26.5146118992978,-72.9184438163855));
#7253=CARTESIAN_POINT('Ctrl Pts',(-24.7983664890463,26.5215066602354,-72.919528318545));
#7254=CARTESIAN_POINT('Ctrl Pts',(-24.7940423326493,26.5233193788359,-72.9198152518033));
#7255=CARTESIAN_POINT('Ctrl Pts',(-24.786702069711,26.5263776551955,-72.9203024245227));
#7256=CARTESIAN_POINT('Ctrl Pts',(-24.7836879896329,26.5276280843882,-72.9205024981912));
#7257=CARTESIAN_POINT('Ctrl Pts',(-24.7776263806347,26.5301320353331,-72.9209049271581));
#7258=CARTESIAN_POINT('Ctrl Pts',(-24.7745788186264,26.5313854647032,-72.9211072852558));
#7259=CARTESIAN_POINT('Ctrl Pts',(-24.7676763270436,26.5342120153748,-72.9215656835205));
#7260=CARTESIAN_POINT('Ctrl Pts',(-24.7638202662534,26.5357823424828,-72.9218218180042));
#7261=CARTESIAN_POINT('Ctrl Pts',(-24.7557591654865,26.5390469159325,-72.9223573792923));
#7262=CARTESIAN_POINT('Ctrl Pts',(-24.7515535745491,26.5407397694985,-72.9226368526282));
#7263=CARTESIAN_POINT('Ctrl Pts',(-24.740556617399,26.5451393735151,-72.9233678038495));
#7264=CARTESIAN_POINT('Ctrl Pts',(-24.7337596163371,26.5478318869312,-72.9238197619237));
#7265=CARTESIAN_POINT('Ctrl Pts',(-24.713632318278,26.5557258366114,-72.9251586394627));
#7266=CARTESIAN_POINT('Ctrl Pts',(-24.7002766079937,26.560861594273,-72.9260477646332));
#7267=CARTESIAN_POINT('Ctrl Pts',(-24.5575115091148,26.614671377569,-72.9355601647306));
#7268=CARTESIAN_POINT('Ctrl Pts',(-24.4251497914064,26.6550519062576,-72.9444602045012));
#7269=CARTESIAN_POINT('Ctrl Pts',(-24.1249901353173,26.7259029852119,-72.9648141469786));
#7270=CARTESIAN_POINT('Ctrl Pts',(-23.9565347422769,26.7518155470262,-72.9763578071717));
#7271=CARTESIAN_POINT('Ctrl Pts',(-23.6452405225055,26.7747296978135,-72.9974666016246));
#7272=CARTESIAN_POINT('Ctrl Pts',(-23.5030969908233,26.7757849281901,-73.0070146660093));
#7273=CARTESIAN_POINT('Ctrl Pts',(-23.3529920376228,26.7669706931905,-73.01672966143));
#7274=CARTESIAN_POINT('Ctrl Pts',(-23.3446494008634,26.7664482329231,-73.0172683770659));
#7275=CARTESIAN_POINT('Ctrl Pts',(-23.2996452972319,26.763454009875,-73.0201674894931));
#7276=CARTESIAN_POINT('Ctrl Pts',(-23.2630242042034,26.7603877158433,-73.0225016189072));
#7277=CARTESIAN_POINT('Ctrl Pts',(-23.2213547699675,26.7561798813537,-73.0251229710299));
#7278=CARTESIAN_POINT('Ctrl Pts',(-23.2162490586078,26.7556519747898,-73.025443569872));
#7279=CARTESIAN_POINT('Ctrl Pts',(-23.2087075992699,26.7548540087959,-73.0259162170039));
#7280=CARTESIAN_POINT('Ctrl Pts',(-23.2062708953098,26.7545933690325,-73.0260687944292));
#7281=CARTESIAN_POINT('Ctrl Pts',(-23.2019590315102,26.7541271794695,-73.0263385394056));
#7282=CARTESIAN_POINT('Ctrl Pts',(-23.2000837538161,26.7539227625389,-73.0264557713762));
#7283=CARTESIAN_POINT('Ctrl Pts',(-23.1961694684679,26.7534926031359,-73.0267002962069));
#7284=CARTESIAN_POINT('Ctrl Pts',(-23.1941305010251,26.7532665607428,-73.0268275715536));
#7285=CARTESIAN_POINT('Ctrl Pts',(-23.188808818646,26.7526714482595,-73.0271595045077));
#7286=CARTESIAN_POINT('Ctrl Pts',(-23.1855264422285,26.7522992763207,-73.0273639858034));
#7287=CARTESIAN_POINT('Ctrl Pts',(-23.1712915703238,26.7506630845301,-73.0282496982272));
#7288=CARTESIAN_POINT('Ctrl Pts',(-23.1603448593197,26.7493478932452,-73.0289280598057));
#7289=CARTESIAN_POINT('Ctrl Pts',(-23.0812273695827,26.7394301966803,-73.033812370134));
#7290=CARTESIAN_POINT('Ctrl Pts',(-23.0133346995317,26.7287049257098,-73.0379040780433));
#7291=CARTESIAN_POINT('Ctrl Pts',(-22.8852406234207,26.7042471113173,-73.0455220153909));
#7292=CARTESIAN_POINT('Ctrl Pts',(-22.8249915555888,26.6909403349312,-73.0490616380125));
#7293=CARTESIAN_POINT('Ctrl Pts',(-22.5255467966103,26.6157267111193,-73.0665963264064));
#7294=CARTESIAN_POINT('Ctrl Pts',(-22.2940244688461,26.5282848930883,-73.0800376425379));
#7295=CARTESIAN_POINT('Ctrl Pts',(-22.0750359288982,26.4155367300479,-73.0942273918944));
#7296=CARTESIAN_POINT('Ctrl Pts',(-22.0750360358082,26.4155367850914,-73.3444460357026));
#7297=CARTESIAN_POINT('Ctrl Pts',(-22.0900522043839,26.4232679899663,-73.3434851462927));
#7298=CARTESIAN_POINT('Ctrl Pts',(-22.105130934277,26.4308820708058,-73.3425217028701));
#7299=CARTESIAN_POINT('Ctrl Pts',(-22.2119811348726,26.4837862176688,-73.3357019430998));
#7300=CARTESIAN_POINT('Ctrl Pts',(-22.3057946946976,26.5247965351268,-73.3297496648075));
#7301=CARTESIAN_POINT('Ctrl Pts',(-22.4457726315562,26.5782052841756,-73.3208151658341));
#7302=CARTESIAN_POINT('Ctrl Pts',(-22.4905180480599,26.5941540051938,-73.3179519354376));
#7303=CARTESIAN_POINT('Ctrl Pts',(-22.5430287315366,26.6115723569861,-73.3145780437848));
#7304=CARTESIAN_POINT('Ctrl Pts',(-22.5504685232802,26.6140101577384,-73.3140997105509));
#7305=CARTESIAN_POINT('Ctrl Pts',(-22.5618211435582,26.6176843225716,-73.3133693009795));
#7306=CARTESIAN_POINT('Ctrl Pts',(-22.5657276096154,26.618940374779,-73.3131178741964));
#7307=CARTESIAN_POINT('Ctrl Pts',(-22.572824967011,26.6212074519544,-73.312660907058));
#7308=CARTESIAN_POINT('Ctrl Pts',(-22.5760150595697,26.622220974606,-73.3124554492909));
#7309=CARTESIAN_POINT('Ctrl Pts',(-22.5824059855557,26.6242404762025,-73.3120437156098));
#7310=CARTESIAN_POINT('Ctrl Pts',(-22.5856068224958,26.6252464301344,-73.3118374391682));
#7311=CARTESIAN_POINT('Ctrl Pts',(-22.5946462553478,26.6280718257314,-73.3112547150411));
#7312=CARTESIAN_POINT('Ctrl Pts',(-22.6004884445562,26.6298796422545,-73.3108778859467));
#7313=CARTESIAN_POINT('Ctrl Pts',(-22.6247430722789,26.6373094518428,-73.3093125141375));
#7314=CARTESIAN_POINT('Ctrl Pts',(-22.643200257472,26.6427829411889,-73.3081191152857));
#7315=CARTESIAN_POINT('Ctrl Pts',(-23.0385023733989,26.7561667540438,-73.2825093410385));
#7316=CARTESIAN_POINT('Ctrl Pts',(-23.4318113181324,26.7945645748825,-73.255453978345));
#7317=CARTESIAN_POINT('Ctrl Pts',(-23.9262068513738,26.7527011995316,-73.2224555356987));
#7318=CARTESIAN_POINT('Ctrl Pts',(-24.0297685483208,26.7388397901194,-73.2156390797172));
#7319=CARTESIAN_POINT('Ctrl Pts',(-24.1370323364614,26.7191369402607,-73.2088003734989));
#7320=CARTESIAN_POINT('Ctrl Pts',(-24.1415774437726,26.7182919542899,-73.2085110176226));
#7321=CARTESIAN_POINT('Ctrl Pts',(-24.1488246606203,26.7169284764174,-73.2080503272773));
#7322=CARTESIAN_POINT('Ctrl Pts',(-24.1515279303664,26.7164163031219,-73.2078786394513));
#7323=CARTESIAN_POINT('Ctrl Pts',(-24.156662885971,26.7154365984318,-73.2075528081832));
#7324=CARTESIAN_POINT('Ctrl Pts',(-24.1590946932532,26.714969725459,-73.207398627449));
#7325=CARTESIAN_POINT('Ctrl Pts',(-24.1633511314254,26.7141474612139,-73.2071289857693));
#7326=CARTESIAN_POINT('Ctrl Pts',(-24.1651759952896,26.7137932935657,-73.2070134543003));
#7327=CARTESIAN_POINT('Ctrl Pts',(-24.1687486937133,26.7130966998768,-73.2067874104048));
#7328=CARTESIAN_POINT('Ctrl Pts',(-24.1704965472834,26.7127544045479,-73.2066768906468));
#7329=CARTESIAN_POINT('Ctrl Pts',(-24.1746782486419,26.711931870389,-73.2064126319414));
#7330=CARTESIAN_POINT('Ctrl Pts',(-24.1771118319032,26.7114502690326,-73.2062589715544));
#7331=CARTESIAN_POINT('Ctrl Pts',(-24.1858496587277,26.7097105834375,-73.2057077016014));
#7332=CARTESIAN_POINT('Ctrl Pts',(-24.192150745365,26.7084364360284,-73.2053110083888));
#7333=CARTESIAN_POINT('Ctrl Pts',(-24.2874983246582,26.6888589863246,-73.199320463505));
#7334=CARTESIAN_POINT('Ctrl Pts',(-24.3757449828602,26.6668127564783,-73.193936865044));
#7335=CARTESIAN_POINT('Ctrl Pts',(-24.7480232203334,26.5568811999074,-73.1714616144944));
#7336=CARTESIAN_POINT('Ctrl Pts',(-25.0200897020776,26.4336665388322,-73.1555022266506));
#7337=CARTESIAN_POINT('Ctrl Pts',(-25.3411740531659,26.2308351628172,-73.1335811151271));
#7338=CARTESIAN_POINT('Ctrl Pts',(-25.4091972318549,26.1841177744388,-73.128746296913));
#7339=CARTESIAN_POINT('Ctrl Pts',(-25.5092059264325,26.1096277126221,-73.121290228028));
#7340=CARTESIAN_POINT('Ctrl Pts',(-25.5425620816965,26.0837485586612,-73.1187416376436));
#7341=CARTESIAN_POINT('Ctrl Pts',(-25.5812970548647,26.0524581971578,-73.1157043845115));
#7342=CARTESIAN_POINT('Ctrl Pts',(-25.5871781094714,26.0476730482326,-73.1152410885986));
#7343=CARTESIAN_POINT('Ctrl Pts',(-25.596174479669,26.040300191122,-73.1145290354615));
#7344=CARTESIAN_POINT('Ctrl Pts',(-25.5993019222952,26.0377272668554,-73.1142808787871));
#7345=CARTESIAN_POINT('Ctrl Pts',(-25.6047520678864,26.0332262188089,-73.1138473272955));
#7346=CARTESIAN_POINT('Ctrl Pts',(-25.6070769319805,26.0313007096638,-73.1136620392027));
#7347=CARTESIAN_POINT('Ctrl Pts',(-25.6119367962838,26.0272641260413,-73.1132739836985));
#7348=CARTESIAN_POINT('Ctrl Pts',(-25.6144712660578,26.0251524209749,-73.1130711906292));
#7349=CARTESIAN_POINT('Ctrl Pts',(-25.6214840800703,26.0192911200139,-73.1125089044615));
#7350=CARTESIAN_POINT('Ctrl Pts',(-25.6259554635248,26.0155332491118,-73.1121490722885));
#7351=CARTESIAN_POINT('Ctrl Pts',(-25.6435475854368,26.0006665661759,-73.1107281257167));
#7352=CARTESIAN_POINT('Ctrl Pts',(-25.6565893741395,25.9894651526301,-73.1096631985598));
#7353=CARTESIAN_POINT('Ctrl Pts',(-25.8717529929242,25.8016516950782,-73.0918991879337));
#7354=CARTESIAN_POINT('Ctrl Pts',(-26.0510773937628,25.600612391256,-73.0740793885299));
#7355=CARTESIAN_POINT('Ctrl Pts',(-26.283884961126,25.2629932991459,-73.0463324259503));
#7356=CARTESIAN_POINT('Ctrl Pts',(-26.3565963822766,25.141058819488,-73.0367027737387));
#7357=CARTESIAN_POINT('Ctrl Pts',(-26.4500821039092,24.9578000628833,-73.0231016822347));
#7358=CARTESIAN_POINT('Ctrl Pts',(-26.4774248028125,24.9000174275619,-73.0189323365691));
#7359=CARTESIAN_POINT('Ctrl Pts',(-26.5142904813043,24.8157113866528,-73.0130563135091));
#7360=CARTESIAN_POINT('Ctrl Pts',(-26.5252114700685,24.7898196043361,-73.0112791636726));
#7361=CARTESIAN_POINT('Ctrl Pts',(-26.5374619143955,24.759681038465,-73.0092449280717));
#7362=CARTESIAN_POINT('Ctrl Pts',(-26.5391225025742,24.7555713720106,-73.0089682771066));
#7363=CARTESIAN_POINT('Ctrl Pts',(-26.5416313662326,24.7493253044259,-73.008548940211));
#7364=CARTESIAN_POINT('Ctrl Pts',(-26.5424858348326,24.7471914214038,-73.0084058795575));
#7365=CARTESIAN_POINT('Ctrl Pts',(-26.5440294629696,24.7433245021043,-73.0081469965661));
#7366=CARTESIAN_POINT('Ctrl Pts',(-26.5447193990714,24.7415917869236,-73.0080311271481));
#7367=CARTESIAN_POINT('Ctrl Pts',(-26.5462077605569,24.7378444335398,-73.0077808224934));
#7368=CARTESIAN_POINT('Ctrl Pts',(-26.5470056559175,24.7358295942267,-73.0076464199407));
#7369=CARTESIAN_POINT('Ctrl Pts',(-26.549168832447,24.7303510212098,-73.0072814460406));
#7370=CARTESIAN_POINT('Ctrl Pts',(-26.5505301500167,24.7268857103878,-73.0070511153188));
#7371=CARTESIAN_POINT('Ctrl Pts',(-26.5569608695626,24.7104322264947,-73.0059599363398));
#7372=CARTESIAN_POINT('Ctrl Pts',(-26.5619520570333,24.6974133482053,-73.0051037548949));
#7373=CARTESIAN_POINT('Ctrl Pts',(-26.6498501318137,24.4636142018348,-72.9898500352905));
#7374=CARTESIAN_POINT('Ctrl Pts',(-26.7083752173632,24.2343830622935,-72.97680646124));
#7375=CARTESIAN_POINT('Ctrl Pts',(-26.7623425028029,23.8521346975943,-72.9552321719404));
#7376=CARTESIAN_POINT('Ctrl Pts',(-26.7729160826212,23.7022071080646,-72.9468182263386));
#7377=CARTESIAN_POINT('Ctrl Pts',(-26.7730250382214,23.5118544729735,-72.935799676369));
#7378=CARTESIAN_POINT('Ctrl Pts',(-26.7722943008018,23.471616057052,-72.9334522222895));
#7379=CARTESIAN_POINT('Ctrl Pts',(-26.7703932184515,23.4201009692817,-72.9304180254313));
#7380=CARTESIAN_POINT('Ctrl Pts',(-26.7699166489407,23.4088013408913,-72.9297507095289));
#7381=CARTESIAN_POINT('Ctrl Pts',(-26.7688945832923,23.3872615454365,-72.9284750969429));
#7382=CARTESIAN_POINT('Ctrl Pts',(-26.7683596696402,23.3770210010631,-72.9278671090946));
#7383=CARTESIAN_POINT('Ctrl Pts',(-26.7647325812258,23.3134122996492,-72.9240807407934));
#7384=CARTESIAN_POINT('Ctrl Pts',(-26.7603619505714,23.2601279246421,-72.9208655149557));
#7385=CARTESIAN_POINT('Ctrl Pts',(-26.7537355380331,23.1982711537277,-72.9170744378423));
#7386=CARTESIAN_POINT('Ctrl Pts',(-26.7527672054969,23.1895670398442,-72.9165396310103));
#7387=CARTESIAN_POINT('Ctrl Pts',(-26.7512713702169,23.1766024455635,-72.9157410009461));
#7388=CARTESIAN_POINT('Ctrl Pts',(-26.750770808147,23.1723388467725,-72.915478029505));
#7389=CARTESIAN_POINT('Ctrl Pts',(-26.7498629422377,23.1647371728677,-72.9150085778163));
#7390=CARTESIAN_POINT('Ctrl Pts',(-26.7494589289791,23.1613987049362,-72.914802201925));
#7391=CARTESIAN_POINT('Ctrl Pts',(-26.7485962681694,23.1543626627979,-72.9143668178403));
#7392=CARTESIAN_POINT('Ctrl Pts',(-26.7481364324005,23.1506652416534,-72.9141377723295));
#7393=CARTESIAN_POINT('Ctrl Pts',(-26.7469052161776,23.1409036008926,-72.9135323936546));
#7394=CARTESIAN_POINT('Ctrl Pts',(-26.7461229941646,23.1348407857749,-72.9131557177424));
#7395=CARTESIAN_POINT('Ctrl Pts',(-26.7425094066653,23.1074471241554,-72.9114506578144));
#7396=CARTESIAN_POINT('Ctrl Pts',(-26.7394817509966,23.0861431315339,-72.9101160685041));
#7397=CARTESIAN_POINT('Ctrl Pts',(-26.7157546167207,22.9304008043411,-72.9002949672586));
#7398=CARTESIAN_POINT('Ctrl Pts',(-26.6867783771639,22.7973803545223,-72.8915445695326));
#7399=CARTESIAN_POINT('Ctrl Pts',(-26.6031703685121,22.5041409558594,-72.8714366189131));
#7400=CARTESIAN_POINT('Ctrl Pts',(-26.5441501841638,22.3455843788541,-72.8599851009913));
#7401=CARTESIAN_POINT('Ctrl Pts',(-26.3960421518399,22.0267875348199,-72.8362061523148));
#7402=CARTESIAN_POINT('Ctrl Pts',(-26.3051547035346,21.867993464027,-72.8239266993623));
#7403=CARTESIAN_POINT('Ctrl Pts',(-26.1949148444702,21.708512975136,-72.8117122868386));
#7404=CARTESIAN_POINT('Ctrl Pts',(-26.1884894621204,21.6993205365675,-72.8110087580274));
#7405=CARTESIAN_POINT('Ctrl Pts',(-26.1800165286662,21.6873325428035,-72.8100921451008));
#7406=CARTESIAN_POINT('Ctrl Pts',(-26.1780123739787,21.6845066282215,-72.8098761367108));
#7407=CARTESIAN_POINT('Ctrl Pts',(-26.1749142960959,21.6801531452956,-72.8095434686959));
#7408=CARTESIAN_POINT('Ctrl Pts',(-26.1738235953142,21.6786233038024,-72.8094265871414));
#7409=CARTESIAN_POINT('Ctrl Pts',(-26.1717556176469,21.6757280714165,-72.8092054276933));
#7410=CARTESIAN_POINT('Ctrl Pts',(-26.1707786167294,21.6743624977332,-72.809101131805));
#7411=CARTESIAN_POINT('Ctrl Pts',(-26.168504920955,21.671189750448,-72.8088588514499));
#7412=CARTESIAN_POINT('Ctrl Pts',(-26.1672074242551,21.6693831582107,-72.808720923714));
#7413=CARTESIAN_POINT('Ctrl Pts',(-26.1635229311059,21.6642641829456,-72.8083301835227));
#7414=CARTESIAN_POINT('Ctrl Pts',(-26.1611314980298,21.6609549755531,-72.8080776784895));
#7415=CARTESIAN_POINT('Ctrl Pts',(-26.1464963408314,21.6407840530583,-72.8065390661557));
#7416=CARTESIAN_POINT('Ctrl Pts',(-26.1340952357037,21.6240363645369,-72.8052637331039));
#7417=CARTESIAN_POINT('Ctrl Pts',(-26.0963887803696,21.574133286754,-72.8014662382974));
#7418=CARTESIAN_POINT('Ctrl Pts',(-26.0706004658224,21.5413464313524,-72.7989747481181));
#7419=CARTESIAN_POINT('Ctrl Pts',(-25.9944692493683,21.4483289544368,-72.7918866132314));
#7420=CARTESIAN_POINT('Ctrl Pts',(-25.9425512445703,21.3894224752071,-72.7873729420552));
#7421=CARTESIAN_POINT('Ctrl Pts',(-25.6421681319233,21.0727194466117,-72.7625919586977));
#7422=CARTESIAN_POINT('Ctrl Pts',(-25.3542774843463,20.8558546232499,-72.7433036193204));
#7423=CARTESIAN_POINT('Ctrl Pts',(-25.0184855840522,20.6813107291108,-72.7204177764769));
#7424=CARTESIAN_POINT('Ctrl Pts',(-25.0002602872651,20.6720564227562,-72.7191757507835));
#7425=CARTESIAN_POINT('Ctrl Pts',(-24.9763398392287,20.6601951368106,-72.7175453324585));
#7426=CARTESIAN_POINT('Ctrl Pts',(-24.970723106729,20.6574303631158,-72.7171624764299));
#7427=CARTESIAN_POINT('Ctrl Pts',(-24.9620583666122,20.6531965613691,-72.7165718148272));
#7428=CARTESIAN_POINT('Ctrl Pts',(-24.9590160198947,20.651715927668,-72.7163644147822));
#7429=CARTESIAN_POINT('Ctrl Pts',(-24.9529628700499,20.6487817931211,-72.7159517464647));
#7430=CARTESIAN_POINT('Ctrl Pts',(-24.9499521254376,20.6473281807566,-72.7157464824022));
#7431=CARTESIAN_POINT('Ctrl Pts',(-24.943360791487,20.6441584684106,-72.7152970813501));
#7432=CARTESIAN_POINT('Ctrl Pts',(-24.9397792854021,20.6424442971884,-72.7150528776313));
#7433=CARTESIAN_POINT('Ctrl Pts',(-24.929588500293,20.637589936801,-72.7143579759328));
#7434=CARTESIAN_POINT('Ctrl Pts',(-24.9229717131273,20.6344656475974,-72.7139067266474));
#7435=CARTESIAN_POINT('Ctrl Pts',(-24.9081169012327,20.6275133310221,-72.7128935136403));
#7436=CARTESIAN_POINT('Ctrl Pts',(-24.8998732408845,20.6236975570161,-72.712331129337));
#7437=CARTESIAN_POINT('Ctrl Pts',(-24.7231750070766,20.5428139480183,-72.7002741219425));
#7438=CARTESIAN_POINT('Ctrl Pts',(-24.5484334814491,20.4803914420529,-72.6882686001742));
#7439=CARTESIAN_POINT('Ctrl Pts',(-24.0945479515876,20.3611183529609,-72.6569649847195));
#7440=CARTESIAN_POINT('Ctrl Pts',(-23.8114407566507,20.3255644331804,-72.6372603477567));
#7441=CARTESIAN_POINT('Ctrl Pts',(-23.4904908376253,20.3278459271695,-72.6166287440313));
#7442=CARTESIAN_POINT('Ctrl Pts',(-23.4536429016258,20.3287400524288,-72.6142875485335));
#7443=CARTESIAN_POINT('Ctrl Pts',(-23.4116830737946,20.330478864922,-72.6116590157396));
#7444=CARTESIAN_POINT('Ctrl Pts',(-23.406550113058,20.3307038714546,-72.6113381058583));
#7445=CARTESIAN_POINT('Ctrl Pts',(-23.3989684754661,20.331054384918,-72.6108650727259));
#7446=CARTESIAN_POINT('Ctrl Pts',(-23.396519400924,20.3311704112015,-72.6107124192313));
#7447=CARTESIAN_POINT('Ctrl Pts',(-23.3921859554331,20.3313806672587,-72.6104425774347));
#7448=CARTESIAN_POINT('Ctrl Pts',(-23.3903015334821,20.3314737569987,-72.6103253245714));
#7449=CARTESIAN_POINT('Ctrl Pts',(-23.3863687875621,20.3316714953625,-72.6100808079457));
#7450=CARTESIAN_POINT('Ctrl Pts',(-23.3843204856661,20.3317764442916,-72.6099535616029));
#7451=CARTESIAN_POINT('Ctrl Pts',(-23.3789752638601,20.332055433948,-72.6096217742592));
#7452=CARTESIAN_POINT('Ctrl Pts',(-23.3756784980491,20.3322325862265,-72.6094174093098));
#7453=CARTESIAN_POINT('Ctrl Pts',(-23.3613899987229,20.333022403269,-72.6085328248107));
#7454=CARTESIAN_POINT('Ctrl Pts',(-23.350401002179,20.3336863299739,-72.6078554660607));
#7455=CARTESIAN_POINT('Ctrl Pts',(-23.2710178075202,20.3388908461009,-72.6029822961744));
#7456=CARTESIAN_POINT('Ctrl Pts',(-23.2027747722018,20.3455564928959,-72.5989001860272));
#7457=CARTESIAN_POINT('Ctrl Pts',(-23.0641761347029,20.3635743242518,-72.5907348462318));
#7458=CARTESIAN_POINT('Ctrl Pts',(-22.9938813217755,20.3750926306353,-72.586659912837));
#7459=CARTESIAN_POINT('Ctrl Pts',(-22.581214509676,20.4568383043441,-72.5628405632533));
#7460=CARTESIAN_POINT('Ctrl Pts',(-22.2517685331347,20.5800363411628,-72.543940432377));
#7461=CARTESIAN_POINT('Ctrl Pts',(-21.9306618056225,20.7639526614434,-72.5215643892726));
#7462=CARTESIAN_POINT('Ctrl Pts',(-21.9129025614361,20.7743515732138,-72.520313947));
#7463=CARTESIAN_POINT('Ctrl Pts',(-21.8898585775834,20.7881430340005,-72.5186740322847));
#7464=CARTESIAN_POINT('Ctrl Pts',(-21.8844821688591,20.7913821002464,-72.5182901776504));
#7465=CARTESIAN_POINT('Ctrl Pts',(-21.8762195282964,20.7963929609402,-72.5176983243276));
#7466=CARTESIAN_POINT('Ctrl Pts',(-21.8733265485137,20.7981536456268,-72.5174907338923));
#7467=CARTESIAN_POINT('Ctrl Pts',(-21.8676108914869,20.8016445868501,-72.5170798703797));
#7468=CARTESIAN_POINT('Ctrl Pts',(-21.8647880942096,20.8033746396749,-72.5168766049774));
#7469=CARTESIAN_POINT('Ctrl Pts',(-21.8586028039712,20.8071786411742,-72.5164304366106));
#7470=CARTESIAN_POINT('Ctrl Pts',(-21.855241452156,20.8092544269559,-72.5161874660522));
#7471=CARTESIAN_POINT('Ctrl Pts',(-21.8457395687584,20.8151464292877,-72.5154992039024));
#7472=CARTESIAN_POINT('Ctrl Pts',(-21.8396080787796,20.8189771177922,-72.5150533772497));
#7473=CARTESIAN_POINT('Ctrl Pts',(-21.825914074999,20.8275967373245,-72.5140538436102));
#7474=CARTESIAN_POINT('Ctrl Pts',(-21.8183585410633,20.8323965953965,-72.513499732258));
#7475=CARTESIAN_POINT('Ctrl Pts',(-21.6645155785371,20.9310315127397,-72.5021629413938));
#7476=CARTESIAN_POINT('Ctrl Pts',(-21.5260610016184,21.0364997121222,-72.4909327575785));
#7477=CARTESIAN_POINT('Ctrl Pts',(-21.1598359467355,21.3654244957262,-72.4582007333772));
#7478=CARTESIAN_POINT('Ctrl Pts',(-20.9557444641652,21.612189705943,-72.4359696888479));
#7479=CARTESIAN_POINT('Ctrl Pts',(-20.7826992529491,21.8988790799341,-72.4147743795314));
#7480=CARTESIAN_POINT('Ctrl Pts',(-20.7743483134476,21.9129556050497,-72.4137447368886));
#7481=CARTESIAN_POINT('Ctrl Pts',(-20.7642922182614,21.9302044936042,-72.4124970517785));
#7482=CARTESIAN_POINT('Ctrl Pts',(-20.7624848677775,21.933316550873,-72.4122724960208));
#7483=CARTESIAN_POINT('Ctrl Pts',(-20.759516385288,21.9384477207615,-72.4119031654202));
#7484=CARTESIAN_POINT('Ctrl Pts',(-20.7583522291408,21.9404650649528,-72.411758194431));
#7485=CARTESIAN_POINT('Ctrl Pts',(-20.7562587112814,21.9441019843636,-72.4114972592962));
#7486=CARTESIAN_POINT('Ctrl Pts',(-20.7553285723107,21.9457211014882,-72.4113812444837));
#7487=CARTESIAN_POINT('Ctrl Pts',(-20.753333194273,21.9492015076725,-72.4111321864348));
#7488=CARTESIAN_POINT('Ctrl Pts',(-20.752268408661,21.9510630467112,-72.4109991730698));
#7489=CARTESIAN_POINT('Ctrl Pts',(-20.7493615998514,21.9561567408984,-72.4106357496681));
#7490=CARTESIAN_POINT('Ctrl Pts',(-20.74752330652,21.9593910377238,-72.410405582289));
#7491=CARTESIAN_POINT('Ctrl Pts',(-20.7380636555902,21.9761016548405,-72.4092193941321));
#7492=CARTESIAN_POINT('Ctrl Pts',(-20.7305337104048,21.989629883668,-72.4082692143598));
#7493=CARTESIAN_POINT('Ctrl Pts',(-20.6858243713992,22.0713343192976,-72.4025879111214));
#7494=CARTESIAN_POINT('Ctrl Pts',(-20.6510182979625,22.1407878131696,-72.3979972146846));
#7495=CARTESIAN_POINT('Ctrl Pts',(-20.5558119212181,22.3492537778529,-72.38471273206));
#7496=CARTESIAN_POINT('Ctrl Pts',(-20.5026636937856,22.491346944833,-72.3762784129801));
#7497=CARTESIAN_POINT('Ctrl Pts',(-20.4321144308882,22.7300044828328,-72.3623720505439));
#7498=CARTESIAN_POINT('Ctrl Pts',(-20.4087647976555,22.8245486955147,-72.3569283292848));
#7499=CARTESIAN_POINT('Ctrl Pts',(-20.3567085568718,23.0855956017489,-72.3418194569642));
#7500=CARTESIAN_POINT('Ctrl Pts',(-20.3367564655348,23.2535039972248,-72.3320017838661));
#7501=CARTESIAN_POINT('Ctrl Pts',(-20.3295937579461,23.4336106744,-72.3210400961515));
#7502=CARTESIAN_POINT('Ctrl Pts',(-20.3292002550901,23.4450361551618,-72.3203429676856));
#7503=CARTESIAN_POINT('Ctrl Pts',(-20.3287385702888,23.4608936861442,-72.3193729158071));
#7504=CARTESIAN_POINT('Ctrl Pts',(-20.3286187237968,23.4653242425301,-72.3191016148444));
#7505=CARTESIAN_POINT('Ctrl Pts',(-20.3284282492657,23.4729475866262,-72.3186343356407));
#7506=CARTESIAN_POINT('Ctrl Pts',(-20.3283532263996,23.4761402667875,-72.3184384955782));
#7507=CARTESIAN_POINT('Ctrl Pts',(-20.3282083454434,23.4827224073648,-72.3180344498135));
#7508=CARTESIAN_POINT('Ctrl Pts',(-20.3281390898806,23.4861118753894,-72.3178262254764));
#7509=CARTESIAN_POINT('Ctrl Pts',(-20.3279922754576,23.4938987655694,-72.3173474820785));
#7510=CARTESIAN_POINT('Ctrl Pts',(-20.3279183700067,23.4982962424339,-72.3170768486563));
#7511=CARTESIAN_POINT('Ctrl Pts',(-20.3277152302911,23.5120602295998,-72.3162289091511));
#7512=CARTESIAN_POINT('Ctrl Pts',(-20.3276178328424,23.5214270974915,-72.3156506046861));
#7513=CARTESIAN_POINT('Ctrl Pts',(-20.3274869753145,23.5430997129128,-72.3143096007185));
#7514=CARTESIAN_POINT('Ctrl Pts',(-20.3274831581506,23.5554054321558,-72.3135459771651));
#7515=CARTESIAN_POINT('Ctrl Pts',(-20.327706357012,23.5966068973697,-72.3109817248945));
#7516=CARTESIAN_POINT('Ctrl Pts',(-20.328251526394,23.6254988557357,-72.3091711751437));
#7517=CARTESIAN_POINT('Ctrl Pts',(-20.3313970666911,23.7228037324984,-72.3030302021037));
#7518=CARTESIAN_POINT('Ctrl Pts',(-20.3357886086877,23.7911362908748,-72.2986451292109));
#7519=CARTESIAN_POINT('Ctrl Pts',(-20.358224304757,24.0240380242361,-72.2834484585624));
#7520=CARTESIAN_POINT('Ctrl Pts',(-20.3867649108549,24.1873175893728,-72.2723483410731));
#7521=CARTESIAN_POINT('Ctrl Pts',(-20.4766193488191,24.5391728846557,-72.2477847368994));
#7522=CARTESIAN_POINT('Ctrl Pts',(-20.5430430290113,24.7257897630923,-72.2343271449293));
#7523=CARTESIAN_POINT('Ctrl Pts',(-20.6424340464649,24.9402916922294,-72.2191112340513));
#7524=CARTESIAN_POINT('Ctrl Pts',(-20.6593477803283,24.9751340227908,-72.2166491305541));
#7525=CARTESIAN_POINT('Ctrl Pts',(-20.6790383146339,25.0139017602392,-72.2139273461744));
#7526=CARTESIAN_POINT('Ctrl Pts',(-20.6811996501787,25.0181338989117,-72.2136304583473));
#7527=CARTESIAN_POINT('Ctrl Pts',(-20.6844690086226,25.0245008643299,-72.2131841901446));
#7528=CARTESIAN_POINT('Ctrl Pts',(-20.6855700614013,25.0266392330286,-72.2130343739313));
#7529=CARTESIAN_POINT('Ctrl Pts',(-20.6874813917749,25.0303410641366,-72.2127751346105));
#7530=CARTESIAN_POINT('Ctrl Pts',(-20.6882905567677,25.0319050947237,-72.2126656409976));
#7531=CARTESIAN_POINT('Ctrl Pts',(-20.6899794574327,25.0351630159769,-72.2124376378472));
#7532=CARTESIAN_POINT('Ctrl Pts',(-20.6908594151449,25.0368567866077,-72.2123191431937));
#7533=CARTESIAN_POINT('Ctrl Pts',(-20.6929544315746,25.0408805989838,-72.2120377400344));
#7534=CARTESIAN_POINT('Ctrl Pts',(-20.6941708399676,25.0432099450992,-72.2118749174835));
#7535=CARTESIAN_POINT('Ctrl Pts',(-20.69824274281,25.0509841956773,-72.211331748513));
#7536=CARTESIAN_POINT('Ctrl Pts',(-20.7011109919279,25.056422459367,-72.210952208355));
#7537=CARTESIAN_POINT('Ctrl Pts',(-20.7788648823567,25.2028286582762,-72.2007448251905));
#7538=CARTESIAN_POINT('Ctrl Pts',(-20.8641178122395,25.3380706058086,-72.19157214866));
#7539=CARTESIAN_POINT('Ctrl Pts',(-21.0969186923549,25.6528771362757,-72.1694878674436));
#7540=CARTESIAN_POINT('Ctrl Pts',(-21.2544891181059,25.8238722598998,-72.1567838214787));
#7541=CARTESIAN_POINT('Ctrl Pts',(-21.5169995937052,26.0533805382081,-72.1366356612996));
#7542=CARTESIAN_POINT('Ctrl Pts',(-21.6090632260881,26.1254314754588,-72.1297353287102));
#7543=CARTESIAN_POINT('Ctrl Pts',(-21.7135206279288,26.1983926178976,-72.1219822034176));
#7544=CARTESIAN_POINT('Ctrl Pts',(-21.7222436214134,26.2044215960496,-72.1213353499733));
#7545=CARTESIAN_POINT('Ctrl Pts',(-21.7345385552521,26.2128299927629,-72.1204243879174));
#7546=CARTESIAN_POINT('Ctrl Pts',(-21.7380858033918,26.2152455389987,-72.120161652897));
#7547=CARTESIAN_POINT('Ctrl Pts',(-21.7442508189623,26.2194256888055,-72.1197051772629));
#7548=CARTESIAN_POINT('Ctrl Pts',(-21.7468663804316,26.2211935490813,-72.1195115603052));
#7549=CARTESIAN_POINT('Ctrl Pts',(-21.7521346020615,26.2247430784347,-72.1191216721872));
#7550=CARTESIAN_POINT('Ctrl Pts',(-21.7547873223122,26.2265246507537,-72.118925397701));
#7551=CARTESIAN_POINT('Ctrl Pts',(-21.761100685248,26.2307511067096,-72.1184583814117));
#7552=CARTESIAN_POINT('Ctrl Pts',(-21.764763688993,26.2331924364598,-72.1181875059749));
#7553=CARTESIAN_POINT('Ctrl Pts',(-21.7762552512838,26.2408174107211,-72.1173379797739));
#7554=CARTESIAN_POINT('Ctrl Pts',(-21.7841014151399,26.2459743180915,-72.1167583252035));
#7555=CARTESIAN_POINT('Ctrl Pts',(-21.8023115259888,26.2578293225027,-72.1154138357312));
#7556=CARTESIAN_POINT('Ctrl Pts',(-21.8126915807703,26.2645022940685,-72.114648070505));
#7557=CARTESIAN_POINT('Ctrl Pts',(-21.8475969222775,26.2866594246915,-72.1120749071122));
#7558=CARTESIAN_POINT('Ctrl Pts',(-21.8722923072265,26.3018717285867,-72.1102575103772));
#7559=CARTESIAN_POINT('Ctrl Pts',(-21.9477822592086,26.3469792212305,-72.1047100262824));
#7560=CARTESIAN_POINT('Ctrl Pts',(-21.9991924265224,26.3758149498707,-72.1009426615874));
#7561=CARTESIAN_POINT('Ctrl Pts',(-22.0592366211213,26.4073609035813,-72.0965536886999));
#7562=CARTESIAN_POINT('Ctrl Pts',(-22.0671281311305,26.4114653315986,-72.095977076891));
#7563=CARTESIAN_POINT('Ctrl Pts',(-22.0750360205127,26.4155367772164,-72.0953994964366));
#7564=CARTESIAN_POINT('Origin',(-23.5502525316942,23.5502525316942,-77.3107734492734));
#7565=CARTESIAN_POINT('',(-22.0750359531635,26.415536742541,-70.5966750543042));
#7566=CARTESIAN_POINT('',(-22.0750360699906,26.4155368026905,-70.8406447795461));
#7567=CARTESIAN_POINT('',(-22.0750360153461,26.4155367745563,-77.3107734492734));
#7568=CARTESIAN_POINT('',(-26.7730024145035,23.5493834215643,-71.4421835438062));
#7569=CARTESIAN_POINT('Ctrl Pts',(-22.0750359531635,26.415536742541,-70.5966750543042));
#7570=CARTESIAN_POINT('Ctrl Pts',(-21.9892850292296,26.3713871310879,-70.6032038036302));
#7571=CARTESIAN_POINT('Ctrl Pts',(-21.9055397994592,26.3234003042188,-70.6097295152631));
#7572=CARTESIAN_POINT('Ctrl Pts',(-21.7599034326677,26.2310246085883,-70.6212244394833));
#7573=CARTESIAN_POINT('Ctrl Pts',(-21.6972050630861,26.1880746732894,-70.6262247757862));
#7574=CARTESIAN_POINT('Ctrl Pts',(-21.6063131854465,26.1209696179805,-70.633488007698));
#7575=CARTESIAN_POINT('Ctrl Pts',(-21.5769262927655,26.0984814004276,-70.6358385939486));
#7576=CARTESIAN_POINT('Ctrl Pts',(-21.5439017569547,26.0722954699336,-70.6384765743049));
#7577=CARTESIAN_POINT('Ctrl Pts',(-21.5398794458165,26.0690903728567,-70.6387978123834));
#7578=CARTESIAN_POINT('Ctrl Pts',(-21.5339503179122,26.0643426176988,-70.6392712232271));
#7579=CARTESIAN_POINT('Ctrl Pts',(-21.5320375873696,26.0628074099904,-70.6394239275884));
#7580=CARTESIAN_POINT('Ctrl Pts',(-21.528690250545,26.0601144610338,-70.6396911313837));
#7581=CARTESIAN_POINT('Ctrl Pts',(-21.5272548840587,26.058957671531,-70.6398056997738));
#7582=CARTESIAN_POINT('Ctrl Pts',(-21.5242671871098,26.0565455974481,-70.6400441486958));
#7583=CARTESIAN_POINT('Ctrl Pts',(-21.5227150332066,26.0552901043058,-70.6401680134129));
#7584=CARTESIAN_POINT('Ctrl Pts',(-21.5195499894223,26.0527251216449,-70.6404205652415));
#7585=CARTESIAN_POINT('Ctrl Pts',(-21.5179371967983,26.0514155128392,-70.6405492435975));
#7586=CARTESIAN_POINT('Ctrl Pts',(-21.5139912669188,26.048205029417,-70.6408640451094));
#7587=CARTESIAN_POINT('Ctrl Pts',(-21.5116595179733,26.0463024398264,-70.641050044644));
#7588=CARTESIAN_POINT('Ctrl Pts',(-21.5052616076968,26.0410671221099,-70.6415603379586));
#7589=CARTESIAN_POINT('Ctrl Pts',(-21.5012009089658,26.037727687623,-70.6418841535717));
#7590=CARTESIAN_POINT('Ctrl Pts',(-21.355169040619,25.9170338642853,-70.6535277656782));
#7591=CARTESIAN_POINT('Ctrl Pts',(-21.2234864664741,25.7877125674087,-70.6639839209856));
#7592=CARTESIAN_POINT('Ctrl Pts',(-20.9009941774329,25.4115451061679,-70.6917743222833));
#7593=CARTESIAN_POINT('Ctrl Pts',(-20.7337473722454,25.147205145449,-70.7089016170191));
#7594=CARTESIAN_POINT('Ctrl Pts',(-20.5993451455506,24.8458663179146,-70.7288746408929));
#7595=CARTESIAN_POINT('Ctrl Pts',(-20.5918535332808,24.8286674986169,-70.7300152341073));
#7596=CARTESIAN_POINT('Ctrl Pts',(-20.5821448560426,24.8058364587985,-70.7315305193548));
#7597=CARTESIAN_POINT('Ctrl Pts',(-20.5797927856637,24.8002617591353,-70.7319006012072));
#7598=CARTESIAN_POINT('Ctrl Pts',(-20.5761663714328,24.7915986702821,-70.7324758626447));
#7599=CARTESIAN_POINT('Ctrl Pts',(-20.5748810989189,24.7885148469309,-70.7326806702083));
#7600=CARTESIAN_POINT('Ctrl Pts',(-20.5723178842173,24.7823377557452,-70.7330909753885));
#7601=CARTESIAN_POINT('Ctrl Pts',(-20.5710399606582,24.7792444846443,-70.7332964733336));
#7602=CARTESIAN_POINT('Ctrl Pts',(-20.5681983627368,24.7723357933626,-70.7337555172112));
#7603=CARTESIAN_POINT('Ctrl Pts',(-20.5666371898208,24.768519356545,-70.7340091475854));
#7604=CARTESIAN_POINT('Ctrl Pts',(-20.5620949374191,24.7573542853407,-70.7347512997315));
#7605=CARTESIAN_POINT('Ctrl Pts',(-20.5591336687111,24.7499976702905,-70.7352404911954));
#7606=CARTESIAN_POINT('Ctrl Pts',(-20.537699307516,24.6961761246824,-70.7388209476672));
#7607=CARTESIAN_POINT('Ctrl Pts',(-20.5202835494736,24.6492999929661,-70.7419476507049));
#7608=CARTESIAN_POINT('Ctrl Pts',(-20.4671317143038,24.4953565749744,-70.7522504601279));
#7609=CARTESIAN_POINT('Ctrl Pts',(-20.4359308090597,24.3868235280148,-70.7595712548786));
#7610=CARTESIAN_POINT('Ctrl Pts',(-20.3340723534792,23.946696683913,-70.7894439984553));
#7611=CARTESIAN_POINT('Ctrl Pts',(-20.3102229057037,23.6065552108426,-70.8131971284455));
#7612=CARTESIAN_POINT('Ctrl Pts',(-20.3401054464487,23.2654976471702,-70.8348416262284));
#7613=CARTESIAN_POINT('Ctrl Pts',(-20.3404145506776,23.2620342306911,-70.8350611693359));
#7614=CARTESIAN_POINT('Ctrl Pts',(-20.3418240516454,23.2465247439172,-70.8360431389173));
#7615=CARTESIAN_POINT('Ctrl Pts',(-20.3429866771223,23.2344842150292,-70.8368023291684));
#7616=CARTESIAN_POINT('Ctrl Pts',(-20.3445800802736,23.2189001025309,-70.8377806275089));
#7617=CARTESIAN_POINT('Ctrl Pts',(-20.3449489694734,23.2153504976337,-70.8380031643972));
#7618=CARTESIAN_POINT('Ctrl Pts',(-20.3455232900249,23.2099120257479,-70.8383436674066));
#7619=CARTESIAN_POINT('Ctrl Pts',(-20.3457244953918,23.2080227302547,-70.8384618724142));
#7620=CARTESIAN_POINT('Ctrl Pts',(-20.3461224479411,23.2043171236231,-70.8386935500811));
#7621=CARTESIAN_POINT('Ctrl Pts',(-20.346319067803,23.2025008111201,-70.8388070290018));
#7622=CARTESIAN_POINT('Ctrl Pts',(-20.346756910027,23.1984880551759,-70.8390575635751));
#7623=CARTESIAN_POINT('Ctrl Pts',(-20.3469988462892,23.1962916977149,-70.8391945778825));
#7624=CARTESIAN_POINT('Ctrl Pts',(-20.3475060538636,23.1917302517588,-70.8394788982338));
#7625=CARTESIAN_POINT('Ctrl Pts',(-20.3477716866329,23.1893652036136,-70.8396261837204));
#7626=CARTESIAN_POINT('Ctrl Pts',(-20.3484606741315,23.1832915029774,-70.8400040979049));
#7627=CARTESIAN_POINT('Ctrl Pts',(-20.3488878542187,23.179583274952,-70.8402345120502));
#7628=CARTESIAN_POINT('Ctrl Pts',(-20.3501464650398,23.1688221195246,-70.8409022677099));
#7629=CARTESIAN_POINT('Ctrl Pts',(-20.3509947737307,23.161771132547,-70.8413386776453));
#7630=CARTESIAN_POINT('Ctrl Pts',(-20.3539574440431,23.1378139783144,-70.8428178327285));
#7631=CARTESIAN_POINT('Ctrl Pts',(-20.3561826035084,23.1209214589807,-70.8438546464765));
#7632=CARTESIAN_POINT('Ctrl Pts',(-20.3657315971399,23.0526174547791,-70.8480248737247));
#7633=CARTESIAN_POINT('Ctrl Pts',(-20.3741639689777,23.0013660699005,-70.8511032926738));
#7634=CARTESIAN_POINT('Ctrl Pts',(-20.3967037709155,22.8823983212118,-70.8581770549293));
#7635=CARTESIAN_POINT('Ctrl Pts',(-20.4117596443322,22.8148870398657,-70.8621363831965));
#7636=CARTESIAN_POINT('Ctrl Pts',(-20.4968242824211,22.4839685750669,-70.8814943166409));
#7637=CARTESIAN_POINT('Ctrl Pts',(-20.5978707671488,22.229711104634,-70.8963157456147));
#7638=CARTESIAN_POINT('Ctrl Pts',(-20.7745337107521,21.9101037587168,-70.9176288425984));
#7639=CARTESIAN_POINT('Ctrl Pts',(-20.8228307861055,21.8309878436158,-70.9231396822197));
#7640=CARTESIAN_POINT('Ctrl Pts',(-20.880161711729,21.7455816386368,-70.9294015139037));
#7641=CARTESIAN_POINT('Ctrl Pts',(-20.8858982885614,21.737123059641,-70.9300251861296));
#7642=CARTESIAN_POINT('Ctrl Pts',(-20.8940014723468,21.7252964185789,-70.9309021784169));
#7643=CARTESIAN_POINT('Ctrl Pts',(-20.8963344868586,21.7219053228409,-70.9311542198023));
#7644=CARTESIAN_POINT('Ctrl Pts',(-20.9006205713289,21.715700878964,-70.9316164267244));
#7645=CARTESIAN_POINT('Ctrl Pts',(-20.9025716443979,21.7128861526524,-70.9318265158399));
#7646=CARTESIAN_POINT('Ctrl Pts',(-20.9065286760029,21.7071969101552,-70.9322519756317));
#7647=CARTESIAN_POINT('Ctrl Pts',(-20.9085348443187,21.704322546757,-70.9324673541369));
#7648=CARTESIAN_POINT('Ctrl Pts',(-20.9134743060289,21.6972700135559,-70.9329968534213));
#7649=CARTESIAN_POINT('Ctrl Pts',(-20.9164128381189,21.6930955399629,-70.933311175083));
#7650=CARTESIAN_POINT('Ctrl Pts',(-20.9271028272931,21.677985761959,-70.9344521840119));
#7651=CARTESIAN_POINT('Ctrl Pts',(-20.9349124867696,21.6670919784106,-70.9352811123814));
#7652=CARTESIAN_POINT('Ctrl Pts',(-21.0489977158415,21.5100316970904,-70.9473245323954));
#7653=CARTESIAN_POINT('Ctrl Pts',(-21.1672965071065,21.3730347818828,-70.9590228718309));
#7654=CARTESIAN_POINT('Ctrl Pts',(-21.3227766837434,21.220911968814,-70.9735148075534));
#7655=CARTESIAN_POINT('Ctrl Pts',(-21.3495622263754,21.1955894585539,-70.9759823219047));
#7656=CARTESIAN_POINT('Ctrl Pts',(-21.579982798918,20.9851210645971,-70.9969502185605));
#7657=CARTESIAN_POINT('Ctrl Pts',(-21.8061342493775,20.8262977913076,-71.0159702208884));
#7658=CARTESIAN_POINT('Ctrl Pts',(-22.0635271434046,20.6908805017038,-71.034366750045));
#7659=CARTESIAN_POINT('Ctrl Pts',(-22.0773820235936,20.683719211485,-71.0353474863602));
#7660=CARTESIAN_POINT('Ctrl Pts',(-22.0944417081503,20.675057770836,-71.0365429535999));
#7661=CARTESIAN_POINT('Ctrl Pts',(-22.0975973939008,20.6734621121898,-71.0367635838509));
#7662=CARTESIAN_POINT('Ctrl Pts',(-22.1028185133072,20.6708328576766,-71.0371277749874));
#7663=CARTESIAN_POINT('Ctrl Pts',(-22.1048824319863,20.6697962880334,-71.0372715227895));
#7664=CARTESIAN_POINT('Ctrl Pts',(-22.108578404195,20.6679450186253,-71.0375285480613));
#7665=CARTESIAN_POINT('Ctrl Pts',(-22.1102100309623,20.6671294878519,-71.0376418780262));
#7666=CARTESIAN_POINT('Ctrl Pts',(-22.1137209660678,20.6653783523669,-71.0378854474643));
#7667=CARTESIAN_POINT('Ctrl Pts',(-22.1156004912948,20.6644432010854,-71.0380156579382));
#7668=CARTESIAN_POINT('Ctrl Pts',(-22.1194738573454,20.6625207405351,-71.0382836292246));
#7669=CARTESIAN_POINT('Ctrl Pts',(-22.1214678102611,20.661533657779,-71.0384213757156));
#7670=CARTESIAN_POINT('Ctrl Pts',(-22.1264786917714,20.6590595377337,-71.0387670367515));
#7671=CARTESIAN_POINT('Ctrl Pts',(-22.1294969379766,20.6575751527361,-71.0389747857966));
#7672=CARTESIAN_POINT('Ctrl Pts',(-22.1380375392721,20.6533914442138,-71.0395613718558));
#7673=CARTESIAN_POINT('Ctrl Pts',(-22.1435653374531,20.6507031729179,-71.0399395305982));
#7674=CARTESIAN_POINT('Ctrl Pts',(-22.1617184304461,20.641939116138,-71.0411765819042));
#7675=CARTESIAN_POINT('Ctrl Pts',(-22.174375866046,20.6359297474945,-71.0420315212618));
#7676=CARTESIAN_POINT('Ctrl Pts',(-22.2259836667265,20.6118390900819,-71.0454881222256));
#7677=CARTESIAN_POINT('Ctrl Pts',(-22.2652562310139,20.5944537428358,-71.0480512321415));
#7678=CARTESIAN_POINT('Ctrl Pts',(-22.3780010824317,20.5472154521471,-71.0552518989229));
#7679=CARTESIAN_POINT('Ctrl Pts',(-22.4522464012086,20.5192808563478,-71.0598069040343));
#7680=CARTESIAN_POINT('Ctrl Pts',(-22.863831542639,20.3815352502135,-71.0844264581023));
#7681=CARTESIAN_POINT('Ctrl Pts',(-23.2164546255123,20.3252680465064,-71.1035609964176));
#7682=CARTESIAN_POINT('Ctrl Pts',(-23.5921915047673,20.3277068608455,-71.1262757346744));
#7683=CARTESIAN_POINT('Ctrl Pts',(-23.6132106148638,20.3280489804896,-71.1275528394202));
#7684=CARTESIAN_POINT('Ctrl Pts',(-23.6405512317939,20.3287616094564,-71.1292228509764));
#7685=CARTESIAN_POINT('Ctrl Pts',(-23.6468774337668,20.3289451504129,-71.129609880202));
#7686=CARTESIAN_POINT('Ctrl Pts',(-23.6569755599138,20.3292678989532,-71.1302286651942));
#7687=CARTESIAN_POINT('Ctrl Pts',(-23.6607478736644,20.329395101084,-71.1304600435583));
#7688=CARTESIAN_POINT('Ctrl Pts',(-23.6675368968589,20.3296359674851,-71.1308768564353));
#7689=CARTESIAN_POINT('Ctrl Pts',(-23.670553691065,20.3297472441774,-71.1310622157031));
#7690=CARTESIAN_POINT('Ctrl Pts',(-23.6776209163499,20.3300178681161,-71.1314967801037));
#7691=CARTESIAN_POINT('Ctrl Pts',(-23.6816712054322,20.3301806185415,-71.1317460919112));
#7692=CARTESIAN_POINT('Ctrl Pts',(-23.693314937081,20.3306704969953,-71.1324635619173));
#7693=CARTESIAN_POINT('Ctrl Pts',(-23.7009075053963,20.3310168448729,-71.1329323233742));
#7694=CARTESIAN_POINT('Ctrl Pts',(-23.7510490196824,20.3334819094208,-71.1360341852083));
#7695=CARTESIAN_POINT('Ctrl Pts',(-23.7935519016257,20.3364171903181,-71.1386928443388));
#7696=CARTESIAN_POINT('Ctrl Pts',(-23.9181342268814,20.347506367367,-71.1465766656584));
#7697=CARTESIAN_POINT('Ctrl Pts',(-23.9999684168833,20.3579690844458,-71.1518724480335));
#7698=CARTESIAN_POINT('Ctrl Pts',(-24.1751966935086,20.3872438516674,-71.1634659980193));
#7699=CARTESIAN_POINT('Ctrl Pts',(-24.2683400513007,20.407081021823,-71.1697871080189));
#7700=CARTESIAN_POINT('Ctrl Pts',(-24.3886318233353,20.4383263230843,-71.1781280163419));
#7701=CARTESIAN_POINT('Ctrl Pts',(-24.4166996635281,20.4460241422021,-71.1800868722044));
#7702=CARTESIAN_POINT('Ctrl Pts',(-24.468334272944,20.4609401860885,-71.1837117834367));
#7703=CARTESIAN_POINT('Ctrl Pts',(-24.4919301007552,20.4680506898726,-71.1853765939769));
#7704=CARTESIAN_POINT('Ctrl Pts',(-24.5358229932785,20.4818287105749,-71.1884875015241));
#7705=CARTESIAN_POINT('Ctrl Pts',(-24.5561399142455,20.4884288185778,-71.1899331289735));
#7706=CARTESIAN_POINT('Ctrl Pts',(-24.6434728607559,20.5177626747209,-71.196169134661));
#7707=CARTESIAN_POINT('Ctrl Pts',(-24.7097965410869,20.542498657975,-71.2009614615115));
#7708=CARTESIAN_POINT('Ctrl Pts',(-24.8742539360703,20.6100834295595,-71.2129222777329));
#7709=CARTESIAN_POINT('Ctrl Pts',(-24.9711759180797,20.6556791904232,-71.2200440030226));
#7710=CARTESIAN_POINT('Ctrl Pts',(-25.1018714970696,20.7253135924841,-71.2295898559903));
#7711=CARTESIAN_POINT('Ctrl Pts',(-25.1377171200278,20.7453001257383,-71.2322014345765));
#7712=CARTESIAN_POINT('Ctrl Pts',(-25.1773470867849,20.7683998736378,-71.2350730827209));
#7713=CARTESIAN_POINT('Ctrl Pts',(-25.1815154862095,20.7708421488451,-71.235374934865));
#7714=CARTESIAN_POINT('Ctrl Pts',(-25.1877681537444,20.7745245133703,-71.2358274040225));
#7715=CARTESIAN_POINT('Ctrl Pts',(-25.1898565159266,20.7757575832124,-71.235978473886));
#7716=CARTESIAN_POINT('Ctrl Pts',(-25.1934632645777,20.7778926760953,-71.2362392882517));
#7717=CARTESIAN_POINT('Ctrl Pts',(-25.1949823011349,20.7787935897017,-71.2363491053102));
#7718=CARTESIAN_POINT('Ctrl Pts',(-25.1981051678671,20.7806491782135,-71.2365748088885));
#7719=CARTESIAN_POINT('Ctrl Pts',(-25.1997089070507,20.7816039964039,-71.236690685213));
#7720=CARTESIAN_POINT('Ctrl Pts',(-25.203482301078,20.7838550042931,-71.2369632514795));
#7721=CARTESIAN_POINT('Ctrl Pts',(-25.2056512683338,20.7851523575912,-71.237119864896));
#7722=CARTESIAN_POINT('Ctrl Pts',(-25.210239193625,20.7879039275634,-71.2374510223126));
#7723=CARTESIAN_POINT('Ctrl Pts',(-25.212657774047,20.7893587744348,-71.2376255249954));
#7724=CARTESIAN_POINT('Ctrl Pts',(-25.2191823694586,20.7932951913422,-71.238096097238));
#7725=CARTESIAN_POINT('Ctrl Pts',(-25.2232847793813,20.7957827680566,-71.2383917786249));
#7726=CARTESIAN_POINT('Ctrl Pts',(-25.2359309008559,20.803489667227,-71.2393026917029));
#7727=CARTESIAN_POINT('Ctrl Pts',(-25.2444559557694,20.8087397081276,-71.2399159736936));
#7728=CARTESIAN_POINT('Ctrl Pts',(-25.2760210822053,20.828382137102,-71.2421843383901));
#7729=CARTESIAN_POINT('Ctrl Pts',(-25.2989040850165,20.8430263888306,-71.2438240251639));
#7730=CARTESIAN_POINT('Ctrl Pts',(-25.3934156206076,20.9052085966818,-71.2505883138839));
#7731=CARTESIAN_POINT('Ctrl Pts',(-25.4633179034705,20.9553169157508,-71.2555723900795));
#7732=CARTESIAN_POINT('Ctrl Pts',(-25.7679162563114,21.1926707687169,-71.2776021714226));
#7733=CARTESIAN_POINT('Ctrl Pts',(-25.977750902946,21.4093445452344,-71.2938002440374));
#7734=CARTESIAN_POINT('Ctrl Pts',(-26.166841485475,21.668760224476,-71.312597940705));
#7735=CARTESIAN_POINT('Ctrl Pts',(-26.1789419793269,21.6857035739098,-71.313822471663));
#7736=CARTESIAN_POINT('Ctrl Pts',(-26.1938703911685,21.7070408139461,-71.3153612480714));
#7737=CARTESIAN_POINT('Ctrl Pts',(-26.196853106376,21.7113261544222,-71.3156701281165));
#7738=CARTESIAN_POINT('Ctrl Pts',(-26.2021170900613,21.7189283843995,-71.3162178053392));
#7739=CARTESIAN_POINT('Ctrl Pts',(-26.2044025869117,21.7222423422886,-71.3164564549917));
#7740=CARTESIAN_POINT('Ctrl Pts',(-26.2090961134865,21.7290752882695,-71.3169483346181));
#7741=CARTESIAN_POINT('Ctrl Pts',(-26.2115033795865,21.7325947892271,-71.3172015905934));
#7742=CARTESIAN_POINT('Ctrl Pts',(-26.2435751425151,21.7796850324163,-71.3205888217182));
#7743=CARTESIAN_POINT('Ctrl Pts',(-26.2721719186701,21.8239703092295,-71.3237598136174));
#7744=CARTESIAN_POINT('Ctrl Pts',(-26.3042183443168,21.8763750217552,-71.3275032315013));
#7745=CARTESIAN_POINT('Ctrl Pts',(-26.3087377715978,21.8838333784637,-71.328035790609));
#7746=CARTESIAN_POINT('Ctrl Pts',(-26.3154329563237,21.8949842304217,-71.3288317284853));
#7747=CARTESIAN_POINT('Ctrl Pts',(-26.3176317366415,21.8986629138726,-71.3290942641381));
#7748=CARTESIAN_POINT('Ctrl Pts',(-26.3215424129114,21.9052354309832,-71.3295632468334));
#7749=CARTESIAN_POINT('Ctrl Pts',(-26.3232571336195,21.9081275836668,-71.3297695903778));
#7750=CARTESIAN_POINT('Ctrl Pts',(-26.3268648073566,21.9142342708926,-71.3302052251803));
#7751=CARTESIAN_POINT('Ctrl Pts',(-26.3287567099964,21.9174494174132,-71.3304345543032));
#7752=CARTESIAN_POINT('Ctrl Pts',(-26.3337439007024,21.925958540991,-71.3310414135238));
#7753=CARTESIAN_POINT('Ctrl Pts',(-26.3368296569134,21.9312580616756,-71.3314192892863));
#7754=CARTESIAN_POINT('Ctrl Pts',(-26.3507682883173,21.9553543644333,-71.3331371193073));
#7755=CARTESIAN_POINT('Ctrl Pts',(-26.3614460234371,21.974251331858,-71.3344833921636));
#7756=CARTESIAN_POINT('Ctrl Pts',(-26.4386132310049,22.1140980681876,-71.3444417768299));
#7757=CARTESIAN_POINT('Ctrl Pts',(-26.4974536756728,22.2390837798798,-71.3533257501392));
#7758=CARTESIAN_POINT('Ctrl Pts',(-26.6675128583361,22.6701002962163,-71.3839028677412));
#7759=CARTESIAN_POINT('Ctrl Pts',(-26.7403957530622,22.989057686152,-71.406635760132));
#7760=CARTESIAN_POINT('Ctrl Pts',(-26.7651345498603,23.3249042087348,-71.4282245839749));
#7761=CARTESIAN_POINT('Ctrl Pts',(-26.7659137220449,23.3363100755452,-71.4289547380944));
#7762=CARTESIAN_POINT('Ctrl Pts',(-26.7670031026628,23.3536103190369,-71.4300573828326));
#7763=CARTESIAN_POINT('Ctrl Pts',(-26.7673578308445,23.3595016706257,-71.4304320220343));
#7764=CARTESIAN_POINT('Ctrl Pts',(-26.7686820702394,23.3825499236053,-71.4318942787692));
#7765=CARTESIAN_POINT('Ctrl Pts',(-26.7695305580163,23.3997138995711,-71.4329758216672));
#7766=CARTESIAN_POINT('Ctrl Pts',(-26.7703932948379,23.4205434702407,-71.4342787053149));
#7767=CARTESIAN_POINT('Ctrl Pts',(-26.7705386173413,23.4242029303488,-71.4345072428034));
#7768=CARTESIAN_POINT('Ctrl Pts',(-26.770766902714,23.4302097665429,-71.434881775814));
#7769=CARTESIAN_POINT('Ctrl Pts',(-26.7708535374045,23.4325569858945,-71.4350279770372));
#7770=CARTESIAN_POINT('Ctrl Pts',(-26.7710010603859,23.4366760355387,-71.4352842735568));
#7771=CARTESIAN_POINT('Ctrl Pts',(-26.7710630526366,23.4384478189484,-71.4353944312232));
#7772=CARTESIAN_POINT('Ctrl Pts',(-26.7711833829345,23.4419701154023,-71.4356132512964));
#7773=CARTESIAN_POINT('Ctrl Pts',(-26.7712417557756,23.4437206184636,-71.435721915374));
#7774=CARTESIAN_POINT('Ctrl Pts',(-26.7713657670809,23.4475328055368,-71.4359583777471));
#7775=CARTESIAN_POINT('Ctrl Pts',(-26.7714308533296,23.44959450862,-71.4360861447737));
#7776=CARTESIAN_POINT('Ctrl Pts',(-26.7715849287522,23.4546283118795,-71.4363978167068));
#7777=CARTESIAN_POINT('Ctrl Pts',(-26.7716717844036,23.4576004826506,-71.4365816019813));
#7778=CARTESIAN_POINT('Ctrl Pts',(-26.772036872106,23.4707152692677,-71.4373915216383));
#7779=CARTESIAN_POINT('Ctrl Pts',(-26.7722713216653,23.4808591907938,-71.4380152327469));
#7780=CARTESIAN_POINT('Ctrl Pts',(-26.7728156331387,23.5104614351481,-71.4398278091507));
#7781=CARTESIAN_POINT('Ctrl Pts',(-26.7729971661461,23.5299219717071,-71.4410098780681));
#7782=CARTESIAN_POINT('Ctrl Pts',(-26.7730024145035,23.5493834215643,-71.4421835438062));
#7783=CARTESIAN_POINT('Ctrl Pts',(-26.7730024138161,23.5493808760687,-71.4421833902944));
#7784=CARTESIAN_POINT('Ctrl Pts',(-26.7730886644055,23.8682729577653,-71.4614148940303));
#7785=CARTESIAN_POINT('Ctrl Pts',(-26.7258452154471,24.1854881446483,-71.4784165817878));
#7786=CARTESIAN_POINT('Ctrl Pts',(-26.5851120910655,24.6467884258757,-71.5058464668276));
#7787=CARTESIAN_POINT('Ctrl Pts',(-26.5256933700641,24.7990534522733,-71.5153592880398));
#7788=CARTESIAN_POINT('Ctrl Pts',(-26.4503352561812,24.9558676944753,-71.5259462116029));
#7789=CARTESIAN_POINT('Ctrl Pts',(-26.4456168559279,24.9655614097221,-71.5266039281923));
#7790=CARTESIAN_POINT('Ctrl Pts',(-26.4387830660695,24.979423887874,-71.5275492570845));
#7791=CARTESIAN_POINT('Ctrl Pts',(-26.4367070723881,24.9836120809651,-71.5278354900792));
#7792=CARTESIAN_POINT('Ctrl Pts',(-26.4330958662347,24.9908578129591,-71.5283317752795));
#7793=CARTESIAN_POINT('Ctrl Pts',(-26.4315648793972,24.9939174591413,-71.5285416789351));
#7794=CARTESIAN_POINT('Ctrl Pts',(-26.4286170420225,24.999785284529,-71.5289448861996));
#7795=CARTESIAN_POINT('Ctrl Pts',(-26.4272009460425,25.0025938403817,-71.5291381630989));
#7796=CARTESIAN_POINT('Ctrl Pts',(-26.42386338162,25.0091892259508,-71.5295927165369));
#7797=CARTESIAN_POINT('Ctrl Pts',(-26.4219385389692,25.0129743336827,-71.5298541117765));
#7798=CARTESIAN_POINT('Ctrl Pts',(-26.4152980251481,25.0259689460633,-71.5307533219502));
#7799=CARTESIAN_POINT('Ctrl Pts',(-26.4105455252151,25.0351594656148,-71.5313924362837));
#7800=CARTESIAN_POINT('Ctrl Pts',(-26.3568149188174,25.1378501743489,-71.5385692384689));
#7801=CARTESIAN_POINT('Ctrl Pts',(-26.3033212168519,25.228902978184,-71.5452678261338));
#7802=CARTESIAN_POINT('Ctrl Pts',(-26.0888247736793,25.5560921159573,-71.5706531916715));
#7803=CARTESIAN_POINT('Ctrl Pts',(-25.9011177900716,25.7731175462074,-71.5903136845913));
#7804=CARTESIAN_POINT('Ctrl Pts',(-25.6544581696233,25.9916383244703,-71.612319335704));
#7805=CARTESIAN_POINT('Ctrl Pts',(-25.6209954240948,26.0200845325445,-71.6152321848534));
#7806=CARTESIAN_POINT('Ctrl Pts',(-25.5468077257184,26.0805824129723,-71.6215173224361));
#7807=CARTESIAN_POINT('Ctrl Pts',(-25.5058684935094,26.1123549560295,-71.6248772495191));
#7808=CARTESIAN_POINT('Ctrl Pts',(-25.4510367144948,26.1528289204955,-71.629218625523));
#7809=CARTESIAN_POINT('Ctrl Pts',(-25.437821079231,26.1624296645058,-71.6302532059088));
#7810=CARTESIAN_POINT('Ctrl Pts',(-25.4189325863508,26.1759333588546,-71.6317145578727));
#7811=CARTESIAN_POINT('Ctrl Pts',(-25.4133195929927,26.1799190656732,-71.6321466670537));
#7812=CARTESIAN_POINT('Ctrl Pts',(-25.4047114217467,26.185990209573,-71.6328060148139));
#7813=CARTESIAN_POINT('Ctrl Pts',(-25.4017254437196,26.1880885648532,-71.6330341151765));
#7814=CARTESIAN_POINT('Ctrl Pts',(-25.3961867181843,26.1919667906402,-71.6334560782462));
#7815=CARTESIAN_POINT('Ctrl Pts',(-25.3936349491107,26.1937480414553,-71.6336500345758));
#7816=CARTESIAN_POINT('Ctrl Pts',(-25.3894465629054,26.1966627117538,-71.6339676485371));
#7817=CARTESIAN_POINT('Ctrl Pts',(-25.3878114760881,26.1977983106177,-71.6340914562212));
#7818=CARTESIAN_POINT('Ctrl Pts',(-25.3846531207463,26.1999875131186,-71.6343302475276));
#7819=CARTESIAN_POINT('Ctrl Pts',(-25.3831299999663,26.2010413160398,-71.6344452446364));
#7820=CARTESIAN_POINT('Ctrl Pts',(-25.3795726712496,26.2034979963202,-71.6347134542611));
#7821=CARTESIAN_POINT('Ctrl Pts',(-25.3775377519226,26.2048998515042,-71.6348665962116));
#7822=CARTESIAN_POINT('Ctrl Pts',(-25.37102332315,26.2093765995646,-71.6353559532954));
#7823=CARTESIAN_POINT('Ctrl Pts',(-25.3665376186558,26.2124425262755,-71.6356915565095));
#7824=CARTESIAN_POINT('Ctrl Pts',(-25.3265419136952,26.239630981341,-71.6386720186872));
#7825=CARTESIAN_POINT('Ctrl Pts',(-25.2905588844853,26.2630545245981,-71.6412704082359));
#7826=CARTESIAN_POINT('Ctrl Pts',(-25.1766337532785,26.3340151738519,-71.6492764461011));
#7827=CARTESIAN_POINT('Ctrl Pts',(-25.0971289375772,26.3789671573703,-71.6545490450781));
#7828=CARTESIAN_POINT('Ctrl Pts',(-24.9439828394529,26.4571647827935,-71.6643271098377));
#7829=CARTESIAN_POINT('Ctrl Pts',(-24.8707952899996,26.4911351475046,-71.6688468490953));
#7830=CARTESIAN_POINT('Ctrl Pts',(-24.6405984485013,26.5876540626487,-71.6828032991666));
#7831=CARTESIAN_POINT('Ctrl Pts',(-24.4798966767702,26.6406279397683,-71.6921986279449));
#7832=CARTESIAN_POINT('Ctrl Pts',(-24.2048693763618,26.7078835943865,-71.7085062335232));
#7833=CARTESIAN_POINT('Ctrl Pts',(-24.0925947299074,26.7290915832619,-71.7152205745176));
#7834=CARTESIAN_POINT('Ctrl Pts',(-23.9602779342084,26.7468711420569,-71.7233011779076));
#7835=CARTESIAN_POINT('Ctrl Pts',(-23.9410935791098,26.7492734164506,-71.7244767290504));
#7836=CARTESIAN_POINT('Ctrl Pts',(-23.9160486237774,26.7521809119483,-71.7260169136057));
#7837=CARTESIAN_POINT('Ctrl Pts',(-23.9102063442367,26.7528429496796,-71.7263765855721));
#7838=CARTESIAN_POINT('Ctrl Pts',(-23.900710636706,26.7538926764132,-71.7269618213445));
#7839=CARTESIAN_POINT('Ctrl Pts',(-23.8970582817307,26.7542901144618,-71.7271870769296));
#7840=CARTESIAN_POINT('Ctrl Pts',(-23.8900478977173,26.7550408356108,-71.7276197364193));
#7841=CARTESIAN_POINT('Ctrl Pts',(-23.8866899755974,26.7553950885695,-71.7278271094012));
#7842=CARTESIAN_POINT('Ctrl Pts',(-23.8790312450713,26.756190898553,-71.7283003889381));
#7843=CARTESIAN_POINT('Ctrl Pts',(-23.8747300990827,26.7566290788948,-71.7285664016972));
#7844=CARTESIAN_POINT('Ctrl Pts',(-23.8613253039041,26.7579674473011,-71.7293961365713));
#7845=CARTESIAN_POINT('Ctrl Pts',(-23.8522187545565,26.7588375230727,-71.729960807284));
#7846=CARTESIAN_POINT('Ctrl Pts',(-23.7814691751168,26.7652933545638,-71.7343556367807));
#7847=CARTESIAN_POINT('Ctrl Pts',(-23.719684175881,26.7691406451981,-71.7382402623672));
#7848=CARTESIAN_POINT('Ctrl Pts',(-23.6528221305453,26.7713737878153,-71.7424986762539));
#7849=CARTESIAN_POINT('Ctrl Pts',(-23.6478138991513,26.7715293667975,-71.7428179763202));
#7850=CARTESIAN_POINT('Ctrl Pts',(-23.6210474195426,26.772298379375,-71.7445262316271));
#7851=CARTESIAN_POINT('Ctrl Pts',(-23.5992841430064,26.7727030318216,-71.7459213885585));
#7852=CARTESIAN_POINT('Ctrl Pts',(-23.2802578205115,26.775402273929,-71.7664641318538));
#7853=CARTESIAN_POINT('Ctrl Pts',(-22.984104753239,26.7367720038835,-71.7868894697297));
#7854=CARTESIAN_POINT('Ctrl Pts',(-22.6162448270906,26.6358400929353,-71.8124173807241));
#7855=CARTESIAN_POINT('Ctrl Pts',(-22.5358663739045,26.610357744276,-71.8179913257021));
#7856=CARTESIAN_POINT('Ctrl Pts',(-22.4295361182046,26.5719968084711,-71.8252819327593));
#7857=CARTESIAN_POINT('Ctrl Pts',(-22.4026289581061,26.5618806657602,-71.8271194636155));
#7858=CARTESIAN_POINT('Ctrl Pts',(-22.3661423006381,26.5476029300757,-71.8295976565094));
#7859=CARTESIAN_POINT('Ctrl Pts',(-22.356443262228,26.5437531388497,-71.8302551039994));
#7860=CARTESIAN_POINT('Ctrl Pts',(-22.3421747597746,26.5380092357018,-71.8312201663332));
#7861=CARTESIAN_POINT('Ctrl Pts',(-22.3375908010134,26.5361516513995,-71.8315298817148));
#7862=CARTESIAN_POINT('Ctrl Pts',(-22.3303416000514,26.5331945682383,-71.8320191391405));
#7863=CARTESIAN_POINT('Ctrl Pts',(-22.3276735490418,26.5321020426277,-71.8321990941795));
#7864=CARTESIAN_POINT('Ctrl Pts',(-22.3226280956955,26.530028097366,-71.8325391779053));
#7865=CARTESIAN_POINT('Ctrl Pts',(-22.3202503974894,26.529047410097,-71.832699350572));
#7866=CARTESIAN_POINT('Ctrl Pts',(-22.3161419542084,26.5273471150587,-71.8329759488819));
#7867=CARTESIAN_POINT('Ctrl Pts',(-22.3144106606635,26.5266288428544,-71.8330924562878));
#7868=CARTESIAN_POINT('Ctrl Pts',(-22.3110588589118,26.5252348318882,-71.8333179160466));
#7869=CARTESIAN_POINT('Ctrl Pts',(-22.3094382787435,26.5245592803069,-71.8334268796861));
#7870=CARTESIAN_POINT('Ctrl Pts',(-22.3056175452596,26.5229629113973,-71.8336836714568));
#7871=CARTESIAN_POINT('Ctrl Pts',(-22.3034178568115,26.5220409738024,-71.8338314308702));
#7872=CARTESIAN_POINT('Ctrl Pts',(-22.2969109272122,26.5193052807897,-71.8342682836547));
#7873=CARTESIAN_POINT('Ctrl Pts',(-22.292606581973,26.5174845870342,-71.8345569556469));
#7874=CARTESIAN_POINT('Ctrl Pts',(-22.2546895845058,26.5013487589937,-71.8370972898839));
#7875=CARTESIAN_POINT('Ctrl Pts',(-22.2213169284143,26.4864716536712,-71.8393152796189));
#7876=CARTESIAN_POINT('Ctrl Pts',(-22.1501141730033,26.4532675792383,-71.8440238489258));
#7877=CARTESIAN_POINT('Ctrl Pts',(-22.1123848385938,26.4347661416304,-71.8465041983327));
#7878=CARTESIAN_POINT('Ctrl Pts',(-22.0750359824043,26.4155367575959,-71.8489552970435));
#7879=CARTESIAN_POINT('',(-26.7730014767856,23.5476449634564,-71.6875616724776));
#7880=CARTESIAN_POINT('Ctrl Pts',(-22.0750360205127,26.4155367772164,-72.0953994964366));
#7881=CARTESIAN_POINT('Ctrl Pts',(-22.1819509304425,26.470582848358,-72.0875905907636));
#7882=CARTESIAN_POINT('Ctrl Pts',(-22.2918594983669,26.519599931717,-72.0795991983618));
#7883=CARTESIAN_POINT('Ctrl Pts',(-22.6337869481824,26.6496917839157,-72.0549904497339));
#7884=CARTESIAN_POINT('Ctrl Pts',(-22.8725623929651,26.710502408185,-72.0380895041274));
#7885=CARTESIAN_POINT('Ctrl Pts',(-23.1522977768553,26.7485483776874,-72.0199440442071));
#7886=CARTESIAN_POINT('Ctrl Pts',(-23.1887447833961,26.7528728244459,-72.0176129189538));
#7887=CARTESIAN_POINT('Ctrl Pts',(-23.2299151189397,26.7570458523138,-72.015022870123));
#7888=CARTESIAN_POINT('Ctrl Pts',(-23.2345717110298,26.7575076009555,-72.0147305429394));
#7889=CARTESIAN_POINT('Ctrl Pts',(-23.2416048413163,26.7581895419619,-72.0142899790898));
#7890=CARTESIAN_POINT('Ctrl Pts',(-23.2439806201013,26.7584172367679,-72.0141413219657));
#7891=CARTESIAN_POINT('Ctrl Pts',(-23.2481050639217,26.7588079004803,-72.0138835356537));
#7892=CARTESIAN_POINT('Ctrl Pts',(-23.249853608928,26.7589720791278,-72.0137743378471));
#7893=CARTESIAN_POINT('Ctrl Pts',(-23.2535066048616,26.759312062963,-72.0135463948183));
#7894=CARTESIAN_POINT('Ctrl Pts',(-23.2554110765952,26.7594876020332,-72.0134276652749));
#7895=CARTESIAN_POINT('Ctrl Pts',(-23.2599535901904,26.7599022171677,-72.0131447275792));
#7896=CARTESIAN_POINT('Ctrl Pts',(-23.2625917805339,26.760139737074,-72.0129806079157));
#7897=CARTESIAN_POINT('Ctrl Pts',(-23.2714752004608,26.7609284836812,-72.0124286561463));
#7898=CARTESIAN_POINT('Ctrl Pts',(-23.2777217956614,26.7614647433921,-72.0120416665226));
#7899=CARTESIAN_POINT('Ctrl Pts',(-23.3991177989233,26.7715296103938,-72.004542168137));
#7900=CARTESIAN_POINT('Ctrl Pts',(-23.5147110585094,26.774878304985,-71.9977714576884));
#7901=CARTESIAN_POINT('Ctrl Pts',(-23.6619362323438,26.7712227391739,-71.9893401023769));
#7902=CARTESIAN_POINT('Ctrl Pts',(-23.6936117462741,26.7699684410239,-71.9875375207124));
#7903=CARTESIAN_POINT('Ctrl Pts',(-23.7507387905546,26.7668615689717,-71.9842994866458));
#7904=CARTESIAN_POINT('Ctrl Pts',(-23.7761963407392,26.7651736599611,-71.9828611684297));
#7905=CARTESIAN_POINT('Ctrl Pts',(-23.8230122160864,26.7615107981696,-71.9802207439004));
#7906=CARTESIAN_POINT('Ctrl Pts',(-23.8443759112048,26.7596245805155,-71.9790176000795));
#7907=CARTESIAN_POINT('Ctrl Pts',(-23.8840844495161,26.7557188557649,-71.9767823330282));
#7908=CARTESIAN_POINT('Ctrl Pts',(-23.9024337955236,26.7537547504446,-71.9757498161742));
#7909=CARTESIAN_POINT('Ctrl Pts',(-24.0741360247475,26.7338827396877,-71.9660847826646));
#7910=CARTESIAN_POINT('Ctrl Pts',(-24.2260293219561,26.7051341908807,-71.9574980327719));
#7911=CARTESIAN_POINT('Ctrl Pts',(-24.419680021313,26.6538510737702,-71.9460232244059));
#7912=CARTESIAN_POINT('Ctrl Pts',(-24.4638315080081,26.641142578506,-71.9433713650675));
#7913=CARTESIAN_POINT('Ctrl Pts',(-24.5990746592239,26.5990634957281,-71.9351157939515));
#7914=CARTESIAN_POINT('Ctrl Pts',(-24.6891345360214,26.5665783039343,-71.9294289240575));
#7915=CARTESIAN_POINT('Ctrl Pts',(-24.787013245412,26.5262639441243,-71.9229853546441));
#7916=CARTESIAN_POINT('Ctrl Pts',(-24.7963982974406,26.5223463587285,-71.9223648068401));
#7917=CARTESIAN_POINT('Ctrl Pts',(-24.8096116433367,26.5167571479975,-71.921487246525));
#7918=CARTESIAN_POINT('Ctrl Pts',(-24.8134555393248,26.5151223723232,-71.9212314901779));
#7919=CARTESIAN_POINT('Ctrl Pts',(-24.8201725713095,26.512250242943,-71.920783749227));
#7920=CARTESIAN_POINT('Ctrl Pts',(-24.8230471107394,26.5110161676348,-71.9205918767531));
#7921=CARTESIAN_POINT('Ctrl Pts',(-24.8288376943503,26.5085202072138,-71.9202048295779));
#7922=CARTESIAN_POINT('Ctrl Pts',(-24.8317536776283,26.5072581913176,-71.9200096505886));
#7923=CARTESIAN_POINT('Ctrl Pts',(-24.8377393819307,26.504657106103,-71.9196084404333));
#7924=CARTESIAN_POINT('Ctrl Pts',(-24.8408088903945,26.5033175603893,-71.9194023931283));
#7925=CARTESIAN_POINT('Ctrl Pts',(-24.8511054186184,26.498804994692,-71.9187101914128));
#7926=CARTESIAN_POINT('Ctrl Pts',(-24.858322825577,26.4956102289789,-71.9182232911356));
#7927=CARTESIAN_POINT('Ctrl Pts',(-24.9109190236838,26.4720972106927,-71.9146625352952));
#7928=CARTESIAN_POINT('Ctrl Pts',(-24.955831813811,26.4507587057636,-71.9115536421922));
#7929=CARTESIAN_POINT('Ctrl Pts',(-25.1002455404749,26.3780044486529,-71.9013250673531));
#7930=CARTESIAN_POINT('Ctrl Pts',(-25.1975550860571,26.3224445933505,-71.8940630623985));
#7931=CARTESIAN_POINT('Ctrl Pts',(-25.3358341005038,26.2336382275399,-71.8831998233624));
#7932=CARTESIAN_POINT('Ctrl Pts',(-25.3792026372575,26.2042686394421,-71.879709780857));
#7933=CARTESIAN_POINT('Ctrl Pts',(-25.655000731967,26.0075244217124,-71.8570000669935));
#7934=CARTESIAN_POINT('Ctrl Pts',(-25.8649558794357,25.8108521435721,-71.8371523588841));
#7935=CARTESIAN_POINT('Ctrl Pts',(-26.0469270226487,25.5880787073612,-71.8189541869717));
#7936=CARTESIAN_POINT('Ctrl Pts',(-26.0476944169045,25.5871381607917,-71.8188774246931));
#7937=CARTESIAN_POINT('Ctrl Pts',(-26.0502162651769,25.5840437233147,-71.8186251048704));
#7938=CARTESIAN_POINT('Ctrl Pts',(-26.0519684715928,25.5818879901434,-71.8184496949777));
#7939=CARTESIAN_POINT('Ctrl Pts',(-26.0615588713071,25.5700577362658,-71.8174891077348));
#7940=CARTESIAN_POINT('Ctrl Pts',(-26.0693438804661,25.5603399388437,-71.8167074735066));
#7941=CARTESIAN_POINT('Ctrl Pts',(-26.0793125842562,25.5477474222682,-71.815704422678));
#7942=CARTESIAN_POINT('Ctrl Pts',(-26.0815479041501,25.5449139879374,-71.8154793625923));
#7943=CARTESIAN_POINT('Ctrl Pts',(-26.0849578017679,25.5405767257302,-71.8151358317497));
#7944=CARTESIAN_POINT('Ctrl Pts',(-26.0861358018862,25.539075611686,-71.815017115397));
#7945=CARTESIAN_POINT('Ctrl Pts',(-26.0883467293317,25.536253090468,-71.8147942318552));
#7946=CARTESIAN_POINT('Ctrl Pts',(-26.0893799542326,25.5349319283924,-71.8146900434126));
#7947=CARTESIAN_POINT('Ctrl Pts',(-26.0917554631376,25.531889525773,-71.814450434498));
#7948=CARTESIAN_POINT('Ctrl Pts',(-26.0930970277136,25.5301677308804,-71.8143150660899));
#7949=CARTESIAN_POINT('Ctrl Pts',(-26.096826370712,25.5253713633959,-71.8139386201053));
#7950=CARTESIAN_POINT('Ctrl Pts',(-26.0992103392914,25.5222938122918,-71.8136978151944));
#7951=CARTESIAN_POINT('Ctrl Pts',(-26.1124755446422,25.5051050379774,-71.8123569355295));
#7952=CARTESIAN_POINT('Ctrl Pts',(-26.1232454555291,25.4909077142549,-71.8112646718845));
#7953=CARTESIAN_POINT('Ctrl Pts',(-26.2973028190546,25.2574620802049,-71.7935390696248));
#7954=CARTESIAN_POINT('Ctrl Pts',(-26.4321889122551,25.018362273839,-71.778674267329));
#7955=CARTESIAN_POINT('Ctrl Pts',(-26.5569493949703,24.7118024759663,-71.7601002042237));
#7956=CARTESIAN_POINT('Ctrl Pts',(-26.5771956499849,24.657970630244,-71.7568587218997));
#7957=CARTESIAN_POINT('Ctrl Pts',(-26.6023819104174,24.5851468206001,-71.7524763406382));
#7958=CARTESIAN_POINT('Ctrl Pts',(-26.6086049571469,24.5666089455675,-71.7513610267112));
#7959=CARTESIAN_POINT('Ctrl Pts',(-26.6589273087568,24.4120551132626,-71.7420593635531));
#7960=CARTESIAN_POINT('Ctrl Pts',(-26.6940930097462,24.2733163970913,-71.7336795079067));
#7961=CARTESIAN_POINT('Ctrl Pts',(-26.7219339810059,24.1218094058783,-71.7243092318042));
#7962=CARTESIAN_POINT('Ctrl Pts',(-26.723881417089,24.1108951712689,-71.7236330734398));
#7963=CARTESIAN_POINT('Ctrl Pts',(-26.7265186365875,24.0956609370378,-71.7226876203253));
#7964=CARTESIAN_POINT('Ctrl Pts',(-26.7272560146339,24.0913491652035,-71.7224198417323));
#7965=CARTESIAN_POINT('Ctrl Pts',(-26.728514000102,24.083901951222,-71.7219570146538));
#7966=CARTESIAN_POINT('Ctrl Pts',(-26.7290387534146,24.0807672072871,-71.7217620983237));
#7967=CARTESIAN_POINT('Ctrl Pts',(-26.7301150540854,24.0742787266205,-71.7213584413241));
#7968=CARTESIAN_POINT('Ctrl Pts',(-26.7306659347774,24.0709248851257,-71.7211496797484));
#7969=CARTESIAN_POINT('Ctrl Pts',(-26.7317467873486,24.0642787796954,-71.7207357600284));
#7970=CARTESIAN_POINT('Ctrl Pts',(-26.7322769569193,24.0609865520355,-71.720530608472));
#7971=CARTESIAN_POINT('Ctrl Pts',(-26.7334935356628,24.0533564587628,-71.7200548867378));
#7972=CARTESIAN_POINT('Ctrl Pts',(-26.7341761880694,24.0490180084929,-71.7197841974273));
#7973=CARTESIAN_POINT('Ctrl Pts',(-26.7359198412538,24.0377871321686,-71.719082956958));
#7974=CARTESIAN_POINT('Ctrl Pts',(-26.7369673384183,24.0308926603085,-71.7186519774751));
#7975=CARTESIAN_POINT('Ctrl Pts',(-26.7614327531121,23.8662686233218,-71.7083490817075));
#7976=CARTESIAN_POINT('Ctrl Pts',(-26.7731304536971,23.7070502666355,-71.6981022652118));
#7977=CARTESIAN_POINT('Ctrl Pts',(-26.7730014767856,23.5476449634564,-71.6875616724776));
#7978=CARTESIAN_POINT('Ctrl Pts',(-26.7730014799568,23.547648885711,-71.6875619318346));
#7979=CARTESIAN_POINT('Ctrl Pts',(-26.7727984241538,23.2963098481987,-71.6709422755845));
#7980=CARTESIAN_POINT('Ctrl Pts',(-26.7431956845923,23.0458728685053,-71.6536303384008));
#7981=CARTESIAN_POINT('Ctrl Pts',(-26.6681982469996,22.7319401547143,-71.6322143859523));
#7982=CARTESIAN_POINT('Ctrl Pts',(-26.6492926480794,22.6630250719862,-71.627538329957));
#7983=CARTESIAN_POINT('Ctrl Pts',(-26.6193024310339,22.5664167070907,-71.6210710084051));
#7984=CARTESIAN_POINT('Ctrl Pts',(-26.6101020192241,22.5381648459333,-71.6191906070202));
#7985=CARTESIAN_POINT('Ctrl Pts',(-26.599060805269,22.5057881315206,-71.6170514996445));
#7986=CARTESIAN_POINT('Ctrl Pts',(-26.597600869188,22.501536229348,-71.6167708959201));
#7987=CARTESIAN_POINT('Ctrl Pts',(-26.595376660822,22.4951023311725,-71.6163467864058));
#7988=CARTESIAN_POINT('Ctrl Pts',(-26.5946189373499,22.4929181022667,-71.6162028929383));
#7989=CARTESIAN_POINT('Ctrl Pts',(-26.5933041211787,22.4891411174585,-71.6159542232738));
#7990=CARTESIAN_POINT('Ctrl Pts',(-26.5927481289417,22.4875479864589,-71.6158493813996));
#7991=CARTESIAN_POINT('Ctrl Pts',(-26.5915863812581,22.4842275185812,-71.6156309639871));
#7992=CARTESIAN_POINT('Ctrl Pts',(-26.5909804070489,22.4825002658729,-71.6155174021068));
#7993=CARTESIAN_POINT('Ctrl Pts',(-26.5893032493548,22.4777327469817,-71.6152041016831));
#7994=CARTESIAN_POINT('Ctrl Pts',(-26.5882289718043,22.4746935595009,-71.6150045483498));
#7995=CARTESIAN_POINT('Ctrl Pts',(-26.5840140606707,22.462826051303,-71.6142259673887));
#7996=CARTESIAN_POINT('Ctrl Pts',(-26.5808394496311,22.4540097196656,-71.6136489487729));
#7997=CARTESIAN_POINT('Ctrl Pts',(-26.52321221848,22.2961345875922,-71.6033389873893));
#7998=CARTESIAN_POINT('Ctrl Pts',(-26.4578527497856,22.1512610321307,-71.5942386101509));
#7999=CARTESIAN_POINT('Ctrl Pts',(-26.2988864532468,21.8586573009056,-71.5754732371789));
#8000=CARTESIAN_POINT('Ctrl Pts',(-26.2034192503403,21.7125393552298,-71.565862302377));
#8001=CARTESIAN_POINT('Ctrl Pts',(-26.055900040713,21.5223820710765,-71.552204431212));
#8002=CARTESIAN_POINT('Ctrl Pts',(-26.013582252558,21.4711820473899,-71.5484008779054));
#8003=CARTESIAN_POINT('Ctrl Pts',(-25.899880438966,21.3419631961191,-71.5384064354533));
#8004=CARTESIAN_POINT('Ctrl Pts',(-25.8261903774889,21.2660904644569,-71.5321394105468));
#8005=CARTESIAN_POINT('Ctrl Pts',(-25.7417847705233,21.1873308195238,-71.5251098668673));
#8006=CARTESIAN_POINT('Ctrl Pts',(-25.7346281143957,21.1807133608662,-71.5245149715753));
#8007=CARTESIAN_POINT('Ctrl Pts',(-25.7248203790968,21.1717267532111,-71.5237011990923));
#8008=CARTESIAN_POINT('Ctrl Pts',(-25.7221951849842,21.1693293257665,-71.5234835251041));
#8009=CARTESIAN_POINT('Ctrl Pts',(-25.7172494851197,21.164827710259,-71.5230737105314));
#8010=CARTESIAN_POINT('Ctrl Pts',(-25.7149298662775,21.1627225503315,-71.5228816114488));
#8011=CARTESIAN_POINT('Ctrl Pts',(-25.7100910198412,21.1583439249956,-71.5224811116568));
#8012=CARTESIAN_POINT('Ctrl Pts',(-25.7075712644598,21.1560710509375,-71.5222726863114));
#8013=CARTESIAN_POINT('Ctrl Pts',(-25.7017530158239,21.1508395069903,-71.5217917148934));
#8014=CARTESIAN_POINT('Ctrl Pts',(-25.698452006636,21.1478836566304,-71.5215190505276));
#8015=CARTESIAN_POINT('Ctrl Pts',(-25.6881603380773,21.1387062744476,-71.520669621159));
#8016=CARTESIAN_POINT('Ctrl Pts',(-25.6811487151363,21.1325084195389,-71.5200918645438));
#8017=CARTESIAN_POINT('Ctrl Pts',(-25.6214473146192,21.0801973959269,-71.5151803290809));
#8018=CARTESIAN_POINT('Ctrl Pts',(-25.5672982318415,21.0357852712132,-71.5107765591166));
#8019=CARTESIAN_POINT('Ctrl Pts',(-25.5049638050972,20.9879694616461,-71.5057568606334));
#8020=CARTESIAN_POINT('Ctrl Pts',(-25.4981578842387,20.9827916403157,-71.5052094443436));
#8021=CARTESIAN_POINT('Ctrl Pts',(-25.4492876799623,20.9459182437194,-71.5012833568309));
#8022=CARTESIAN_POINT('Ctrl Pts',(-25.4064744990272,20.9152323987471,-71.4978682822105));
#8023=CARTESIAN_POINT('Ctrl Pts',(-25.2931513295494,20.8381419609986,-71.4888939404068));
#8024=CARTESIAN_POINT('Ctrl Pts',(-25.221538666748,20.7934353333824,-71.4832851113866));
#8025=CARTESIAN_POINT('Ctrl Pts',(-25.094022835964,20.7206251243107,-71.4734337360726));
#8026=CARTESIAN_POINT('Ctrl Pts',(-25.0389000355938,20.6912411083891,-71.469217309668));
#8027=CARTESIAN_POINT('Ctrl Pts',(-24.8700820920327,20.6074567249871,-71.4564670264848));
#8028=CARTESIAN_POINT('Ctrl Pts',(-24.754012921954,20.5581027945711,-71.4479132654968));
#8029=CARTESIAN_POINT('Ctrl Pts',(-24.563828650898,20.4900972740889,-71.4344764452376));
#8030=CARTESIAN_POINT('Ctrl Pts',(-24.4914206595373,20.4670575769851,-71.4294904243623));
#8031=CARTESIAN_POINT('Ctrl Pts',(-24.3870860164065,20.4378780097799,-71.4225508819997));
#8032=CARTESIAN_POINT('Ctrl Pts',(-24.3557801331197,20.4296290476998,-71.4204995956354));
#8033=CARTESIAN_POINT('Ctrl Pts',(-24.3198979855948,20.4207502537141,-71.4181878090742));
#8034=CARTESIAN_POINT('Ctrl Pts',(-24.3154397697522,20.4196572011016,-71.4179012691486));
#8035=CARTESIAN_POINT('Ctrl Pts',(-24.3087135251834,20.4180233063594,-71.4174700143657));
#8036=CARTESIAN_POINT('Ctrl Pts',(-24.306447244181,20.4174754002059,-71.4173248919046));
#8037=CARTESIAN_POINT('Ctrl Pts',(-24.3025374699571,20.4165346456164,-71.4170748414792));
#8038=CARTESIAN_POINT('Ctrl Pts',(-24.300894264491,20.4161406308689,-71.4169698456022));
#8039=CARTESIAN_POINT('Ctrl Pts',(-24.2974791876764,20.4153245891924,-71.4167518317465));
#8040=CARTESIAN_POINT('Ctrl Pts',(-24.2957072731602,20.4149027731259,-71.4166388263206));
#8041=CARTESIAN_POINT('Ctrl Pts',(-24.2908424197197,20.413749019466,-71.4163288687149));
#8042=CARTESIAN_POINT('Ctrl Pts',(-24.2877487434761,20.4130201523063,-71.4161320950558));
#8043=CARTESIAN_POINT('Ctrl Pts',(-24.2758450337367,20.410234230586,-71.4153762314205));
#8044=CARTESIAN_POINT('Ctrl Pts',(-24.2670273225602,20.408209674869,-71.4148190041085));
#8045=CARTESIAN_POINT('Ctrl Pts',(-24.2502457691316,20.4044309337968,-71.4137633990485));
#8046=CARTESIAN_POINT('Ctrl Pts',(-24.2422835929154,20.4026697969918,-71.4132646440288));
#8047=CARTESIAN_POINT('Ctrl Pts',(-23.9551854363941,20.3403092272776,-71.3953529886996));
#8048=CARTESIAN_POINT('Ctrl Pts',(-23.6691823992768,20.3170461829979,-71.379892110277));
#8049=CARTESIAN_POINT('Ctrl Pts',(-23.2700704773358,20.337685193692,-71.3574244618303));
#8050=CARTESIAN_POINT('Ctrl Pts',(-23.156720518798,20.3495931256951,-71.3509539521676));
#8051=CARTESIAN_POINT('Ctrl Pts',(-22.9779959448537,20.3780072983004,-71.3404130508502));
#8052=CARTESIAN_POINT('Ctrl Pts',(-22.9120957354779,20.3906050194246,-71.336452737286));
#8053=CARTESIAN_POINT('Ctrl Pts',(-22.8123525809333,20.4129199581823,-71.330319653314));
#8054=CARTESIAN_POINT('Ctrl Pts',(-22.7781942493942,20.4211507639194,-71.3281942098128));
#8055=CARTESIAN_POINT('Ctrl Pts',(-22.7372362328648,20.4317314929742,-71.325613194918));
#8056=CARTESIAN_POINT('Ctrl Pts',(-22.7303002014443,20.4335479987126,-71.3251749868323));
#8057=CARTESIAN_POINT('Ctrl Pts',(-22.720206236866,20.436227575473,-71.3245356046553));
#8058=CARTESIAN_POINT('Ctrl Pts',(-22.7170434311509,20.4370723451048,-71.3243350251251));
#8059=CARTESIAN_POINT('Ctrl Pts',(-22.7107579079904,20.43876144163,-71.3239359329842));
#8060=CARTESIAN_POINT('Ctrl Pts',(-22.7076351635345,20.439605654029,-71.3237374242975));
#8061=CARTESIAN_POINT('Ctrl Pts',(-22.701410858797,20.4412984122862,-71.323341285468));
#8062=CARTESIAN_POINT('Ctrl Pts',(-22.6983092866325,20.4421469013627,-71.3231436573608));
#8063=CARTESIAN_POINT('Ctrl Pts',(-22.6908566217321,20.4441977011988,-71.3226682228132));
#8064=CARTESIAN_POINT('Ctrl Pts',(-22.6865067835128,20.4454045125023,-71.32239026993));
#8065=CARTESIAN_POINT('Ctrl Pts',(-22.6732007508227,20.4491262404023,-71.3215386035544));
#8066=CARTESIAN_POINT('Ctrl Pts',(-22.6642529573395,20.4516707831839,-71.3209639243285));
#8067=CARTESIAN_POINT('Ctrl Pts',(-22.5622749512569,20.4811487701997,-71.3143915861999));
#8068=CARTESIAN_POINT('Ctrl Pts',(-22.470502308384,20.512221294842,-71.3082585695236));
#8069=CARTESIAN_POINT('Ctrl Pts',(-22.2302128276252,20.6058426057763,-71.2915856277272));
#8070=CARTESIAN_POINT('Ctrl Pts',(-22.0847613751605,20.6754691791696,-71.2808326711107));
#8071=CARTESIAN_POINT('Ctrl Pts',(-21.842904345346,20.8143835122696,-71.2619923361145));
#8072=CARTESIAN_POINT('Ctrl Pts',(-21.7439696744951,20.8786687471491,-71.253980748827));
#8073=CARTESIAN_POINT('Ctrl Pts',(-21.5887249086116,20.9921166045432,-71.2410860709034));
#8074=CARTESIAN_POINT('Ctrl Pts',(-21.5302040987066,21.0380710655074,-71.2361444842696));
#8075=CARTESIAN_POINT('Ctrl Pts',(-21.4467037075505,21.1084474967784,-71.229028669011));
#8076=CARTESIAN_POINT('Ctrl Pts',(-21.4204486643998,21.1313136767297,-71.2267813694454));
#8077=CARTESIAN_POINT('Ctrl Pts',(-21.3747975354672,21.1723920449945,-71.2228639343417));
#8078=CARTESIAN_POINT('Ctrl Pts',(-21.3552470743839,21.1904270953873,-71.2211829348023));
#8079=CARTESIAN_POINT('Ctrl Pts',(-21.3327462100764,21.2117054670375,-71.2192466975512));
#8080=CARTESIAN_POINT('Ctrl Pts',(-21.3295771402601,21.2147145922794,-71.2189739574236));
#8081=CARTESIAN_POINT('Ctrl Pts',(-21.3247599270849,21.2193073471502,-71.2185593313556));
#8082=CARTESIAN_POINT('Ctrl Pts',(-21.3231073475098,21.2208862841579,-71.218417083432));
#8083=CARTESIAN_POINT('Ctrl Pts',(-21.3201096770173,21.223756478225,-71.2181590438643));
#8084=CARTESIAN_POINT('Ctrl Pts',(-21.3187640315217,21.2250471401804,-71.2180432067232));
#8085=CARTESIAN_POINT('Ctrl Pts',(-21.3158489014319,21.2278480183647,-71.2177922552897));
#8086=CARTESIAN_POINT('Ctrl Pts',(-21.3142798318529,21.2293586538758,-71.2176571749946));
#8087=CARTESIAN_POINT('Ctrl Pts',(-21.309999399835,21.2334880471154,-71.2172886556549));
#8088=CARTESIAN_POINT('Ctrl Pts',(-21.3072910877586,21.2361099835408,-71.2170554650276));
#8089=CARTESIAN_POINT('Ctrl Pts',(-21.2942525822178,21.2487770468914,-71.2159326856354));
#8090=CARTESIAN_POINT('Ctrl Pts',(-21.2839850225099,21.2588868309988,-71.2150480940606));
#8091=CARTESIAN_POINT('Ctrl Pts',(-21.0988731909654,21.4436156457803,-71.1990843658078));
#8092=CARTESIAN_POINT('Ctrl Pts',(-20.9445847888198,21.6377362862193,-71.18548517627));
#8093=CARTESIAN_POINT('Ctrl Pts',(-20.7284409129194,21.9850957923487,-71.1626057088043));
#8094=CARTESIAN_POINT('Ctrl Pts',(-20.6533826083418,22.1288184913387,-71.1534942610463));
#8095=CARTESIAN_POINT('Ctrl Pts',(-20.565146364387,22.3340926259622,-71.1404365913821));
#8096=CARTESIAN_POINT('Ctrl Pts',(-20.5424721427305,22.3913046669938,-71.1367947596021));
#8097=CARTESIAN_POINT('Ctrl Pts',(-20.5140720707222,22.4694231732193,-71.1318013206306));
#8098=CARTESIAN_POINT('Ctrl Pts',(-20.5068980731353,22.4897915476394,-71.1304975092768));
#8099=CARTESIAN_POINT('Ctrl Pts',(-20.4967318216469,22.51960855061,-71.1285855794885));
#8100=CARTESIAN_POINT('Ctrl Pts',(-20.4935774945517,22.5290016044873,-71.1279828035802));
#8101=CARTESIAN_POINT('Ctrl Pts',(-20.4880016727925,22.545862729971,-71.1268998701347));
#8102=CARTESIAN_POINT('Ctrl Pts',(-20.4855640453356,22.5533254147435,-71.1264202478617));
#8103=CARTESIAN_POINT('Ctrl Pts',(-20.4818984404577,22.564687998122,-71.1256894710931));
#8104=CARTESIAN_POINT('Ctrl Pts',(-20.4806505642224,22.5685814869489,-71.1254389731326));
#8105=CARTESIAN_POINT('Ctrl Pts',(-20.4784899217689,22.5753672925966,-71.1250022281297));
#8106=CARTESIAN_POINT('Ctrl Pts',(-20.4775738210406,22.5782585491309,-71.1248160911702));
#8107=CARTESIAN_POINT('Ctrl Pts',(-20.4756873161201,22.5842417659109,-71.1244307884116));
#8108=CARTESIAN_POINT('Ctrl Pts',(-20.4747174918361,22.5873339043414,-71.1242316037641));
#8109=CARTESIAN_POINT('Ctrl Pts',(-20.4723803678538,22.5948250220788,-71.1237489060589));
#8110=CARTESIAN_POINT('Ctrl Pts',(-20.4710178356089,22.5992254715348,-71.1234652366147));
#8111=CARTESIAN_POINT('Ctrl Pts',(-20.4659886315635,22.6155919582176,-71.1224097274929));
#8112=CARTESIAN_POINT('Ctrl Pts',(-20.4623822749201,22.6275762810566,-71.1216359116738));
#8113=CARTESIAN_POINT('Ctrl Pts',(-20.3844452515622,22.8921448673834,-71.1045315440814));
#8114=CARTESIAN_POINT('Ctrl Pts',(-20.3412922154416,23.1528162505785,-71.0871228470884));
#8115=CARTESIAN_POINT('Ctrl Pts',(-20.3240132394544,23.566524795566,-71.0591301289729));
#8116=CARTESIAN_POINT('Ctrl Pts',(-20.3283117974109,23.7175421312417,-71.0488664585046));
#8117=CARTESIAN_POINT('Ctrl Pts',(-20.3510489148938,23.9472435580378,-71.0335930866709));
#8118=CARTESIAN_POINT('Ctrl Pts',(-20.3618787915508,24.0264677505785,-71.0283900120778));
#8119=CARTESIAN_POINT('Ctrl Pts',(-20.3783070472814,24.1204441221017,-71.022357914383));
#8120=CARTESIAN_POINT('Ctrl Pts',(-20.3810790834573,24.135655199711,-71.0213859833258));
#8121=CARTESIAN_POINT('Ctrl Pts',(-20.3846535423618,24.1544995250735,-71.0201879002099));
#8122=CARTESIAN_POINT('Ctrl Pts',(-20.3853528643272,24.1581517717847,-71.019955978049));
#8123=CARTESIAN_POINT('Ctrl Pts',(-20.3864653970981,24.1639080760484,-71.0195908963074));
#8124=CARTESIAN_POINT('Ctrl Pts',(-20.3868743863002,24.166012931087,-71.0194574952819));
#8125=CARTESIAN_POINT('Ctrl Pts',(-20.3876434873805,24.1699501050022,-71.019208145893));
#8126=CARTESIAN_POINT('Ctrl Pts',(-20.3880030886792,24.1717825066078,-71.0190921692937));
#8127=CARTESIAN_POINT('Ctrl Pts',(-20.3888149142104,24.1759003406818,-71.0188317064623));
#8128=CARTESIAN_POINT('Ctrl Pts',(-20.3892680231688,24.1781855910955,-71.0186872720412));
#8129=CARTESIAN_POINT('Ctrl Pts',(-20.3904277157938,24.1840014248066,-71.018319977942));
#8130=CARTESIAN_POINT('Ctrl Pts',(-20.3911377410017,24.1875313295665,-71.0180973157263));
#8131=CARTESIAN_POINT('Ctrl Pts',(-20.3951123601556,24.2071213500731,-71.0168630401017));
#8132=CARTESIAN_POINT('Ctrl Pts',(-20.3984935835882,24.22315795329,-71.015858022988));
#8133=CARTESIAN_POINT('Ctrl Pts',(-20.46953507487,24.5478082514731,-70.9956084201467));
#8134=CARTESIAN_POINT('Ctrl Pts',(-20.5821030396575,24.8448970158884,-70.9787187806519));
#8135=CARTESIAN_POINT('Ctrl Pts',(-20.8219996512642,25.2747206437379,-70.9508521107429));
#8136=CARTESIAN_POINT('Ctrl Pts',(-20.9203144205121,25.4212324546322,-70.9406426832417));
#8137=CARTESIAN_POINT('Ctrl Pts',(-21.0356934351114,25.5659883138695,-70.9293974600802));
#8138=CARTESIAN_POINT('Ctrl Pts',(-21.0413195566681,25.5729867005915,-70.9288508125927));
#8139=CARTESIAN_POINT('Ctrl Pts',(-21.0515334744962,25.5855837153704,-70.9278613969213));
#8140=CARTESIAN_POINT('Ctrl Pts',(-21.0561110389804,25.5911905922497,-70.9274190425282));
#8141=CARTESIAN_POINT('Ctrl Pts',(-21.0632207975736,25.5998394122654,-70.9267336186967));
#8142=CARTESIAN_POINT('Ctrl Pts',(-21.0657397923273,25.6028922164009,-70.9264910861314));
#8143=CARTESIAN_POINT('Ctrl Pts',(-21.0701892571456,25.6082643934071,-70.9260632332505));
#8144=CARTESIAN_POINT('Ctrl Pts',(-21.0721173768674,25.6105857142233,-70.9258780089972));
#8145=CARTESIAN_POINT('Ctrl Pts',(-21.0764712056878,25.615812465277,-70.9254601637691));
#8146=CARTESIAN_POINT('Ctrl Pts',(-21.0788987753781,25.6187163334243,-70.925227466793));
#8147=CARTESIAN_POINT('Ctrl Pts',(-21.0854288713786,25.6264997536985,-70.9246022678674));
#8148=CARTESIAN_POINT('Ctrl Pts',(-21.0895407545164,25.631371401931,-70.9242093819337));
#8149=CARTESIAN_POINT('Ctrl Pts',(-21.1075288868192,25.6525554121828,-70.9224940366049));
#8150=CARTESIAN_POINT('Ctrl Pts',(-21.1215528310653,25.6687411285581,-70.921165484296));
#8151=CARTESIAN_POINT('Ctrl Pts',(-21.3681760257171,25.947713427733,-70.8979482160917));
#8152=CARTESIAN_POINT('Ctrl Pts',(-21.6419634531248,26.1708587526071,-70.8740219971911));
#8153=CARTESIAN_POINT('Ctrl Pts',(-21.9886033311619,26.3697847092624,-70.847154366132));
#8154=CARTESIAN_POINT('Ctrl Pts',(-22.0315665040648,26.3931561195988,-70.8438841383696));
#8155=CARTESIAN_POINT('Ctrl Pts',(-22.0750360699906,26.4155368026905,-70.8406447795461));
#8156=CARTESIAN_POINT('Origin',(-23.5502525316942,23.5502525316942,-77.3107734492734));
#8157=CARTESIAN_POINT('',(-22.075036015343,26.4155367745547,-69.3432196869019));
#8158=CARTESIAN_POINT('',(-22.0750360905742,26.4155368132881,-69.5918437005959));
#8159=CARTESIAN_POINT('',(-22.0750360153461,26.4155367745563,-77.3107734492734));
#8160=CARTESIAN_POINT('Ctrl Pts',(-22.075036015343,26.4155367745547,-69.3432196869019));
#8161=CARTESIAN_POINT('Ctrl Pts',(-22.0700252443756,26.4129569355355,-69.3435677364703));
#8162=CARTESIAN_POINT('Ctrl Pts',(-22.0650212677462,26.4103639662412,-69.3439162512079));
#8163=CARTESIAN_POINT('Ctrl Pts',(-21.9680557316067,26.3597951038903,-69.3506879650293));
#8164=CARTESIAN_POINT('Ctrl Pts',(-21.878466134713,26.3074254374581,-69.3572675485728));
#8165=CARTESIAN_POINT('Ctrl Pts',(-21.6267416012296,26.1434958781456,-69.3767445377577));
#8166=CARTESIAN_POINT('Ctrl Pts',(-21.4721100761709,26.0213072430003,-69.3900039017954));
#8167=CARTESIAN_POINT('Ctrl Pts',(-21.3061862398938,25.8635462252343,-69.405502002912));
#8168=CARTESIAN_POINT('Ctrl Pts',(-21.2831098195613,25.8409347825109,-69.4076884173614));
#8169=CARTESIAN_POINT('Ctrl Pts',(-21.2339943888438,25.791339666148,-69.412404608083));
#8170=CARTESIAN_POINT('Ctrl Pts',(-21.2080781314018,25.7642404461029,-69.4149328203265));
#8171=CARTESIAN_POINT('Ctrl Pts',(-21.1460260538257,25.6970466958991,-69.4210743582906));
#8172=CARTESIAN_POINT('Ctrl Pts',(-21.1104120494764,25.6564835275016,-69.4246755728561));
#8173=CARTESIAN_POINT('Ctrl Pts',(-21.029200840972,25.5591610152318,-69.4330382830035));
#8174=CARTESIAN_POINT('Ctrl Pts',(-20.9844716028786,25.5017096785125,-69.4377646379455));
#8175=CARTESIAN_POINT('Ctrl Pts',(-20.9326047720579,25.430220312707,-69.4433494679472));
#8176=CARTESIAN_POINT('Ctrl Pts',(-20.9235773655829,25.4175865259414,-69.4443255817774));
#8177=CARTESIAN_POINT('Ctrl Pts',(-20.9124984979293,25.4018424122081,-69.4455281163117));
#8178=CARTESIAN_POINT('Ctrl Pts',(-20.9103608552575,25.3987934063515,-69.4457603582092));
#8179=CARTESIAN_POINT('Ctrl Pts',(-20.9070000114916,25.3939819801598,-69.446125825153));
#8180=CARTESIAN_POINT('Ctrl Pts',(-20.9057732859736,25.3922220438508,-69.4462592925129));
#8181=CARTESIAN_POINT('Ctrl Pts',(-20.9034821741442,25.3889280667083,-69.4465086938957));
#8182=CARTESIAN_POINT('Ctrl Pts',(-20.9024173708622,25.3873943361701,-69.4466246563016));
#8183=CARTESIAN_POINT('Ctrl Pts',(-20.9000279466759,25.3839462440655,-69.446884994697));
#8184=CARTESIAN_POINT('Ctrl Pts',(-20.8987040696066,25.3820313761837,-69.4470293190714));
#8185=CARTESIAN_POINT('Ctrl Pts',(-20.8953410000555,25.3771557163729,-69.4473961627538));
#8186=CARTESIAN_POINT('Ctrl Pts',(-20.8933046787734,25.3741929348225,-69.4476184854174));
#8187=CARTESIAN_POINT('Ctrl Pts',(-20.8820514033343,25.3577609471945,-69.4488482537072));
#8188=CARTESIAN_POINT('Ctrl Pts',(-20.8729316942325,25.3442249654902,-69.4498491588648));
#8189=CARTESIAN_POINT('Ctrl Pts',(-20.6877069337447,25.064745447452,-69.4702800259876));
#8190=CARTESIAN_POINT('Ctrl Pts',(-20.5519118916773,24.7741356094699,-69.4873108809933));
#8191=CARTESIAN_POINT('Ctrl Pts',(-20.424811613949,24.3464259833338,-69.5125905978506));
#8192=CARTESIAN_POINT('Ctrl Pts',(-20.3958483442435,24.2225637549597,-69.51991432577));
#8193=CARTESIAN_POINT('Ctrl Pts',(-20.3682584012077,24.0623924313075,-69.5295769490699));
#8194=CARTESIAN_POINT('Ctrl Pts',(-20.3628183554681,24.0273658798772,-69.5317010815362));
#8195=CARTESIAN_POINT('Ctrl Pts',(-20.3559923275292,23.9780662411099,-69.5347092823438));
#8196=CARTESIAN_POINT('Ctrl Pts',(-20.3541220542966,23.9638619888815,-69.5355781495236));
#8197=CARTESIAN_POINT('Ctrl Pts',(-20.3514397191732,23.942384779046,-69.5368953091249));
#8198=CARTESIAN_POINT('Ctrl Pts',(-20.3505575995965,23.935120624791,-69.5373413949648));
#8199=CARTESIAN_POINT('Ctrl Pts',(-20.3491687249311,23.9233485016198,-69.5380652866643));
#8200=CARTESIAN_POINT('Ctrl Pts',(-20.3486467311437,23.9188423284133,-69.5383426116148));
#8201=CARTESIAN_POINT('Ctrl Pts',(-20.3476638567574,23.9101979152248,-69.5388750672006));
#8202=CARTESIAN_POINT('Ctrl Pts',(-20.3472014783216,23.9060598520076,-69.5391301500468));
#8203=CARTESIAN_POINT('Ctrl Pts',(-20.3463875023282,23.8986449788287,-69.5395875833411));
#8204=CARTESIAN_POINT('Ctrl Pts',(-20.3460329085611,23.8953684980196,-69.539789838877));
#8205=CARTESIAN_POINT('Ctrl Pts',(-20.3453373457026,23.8888479442368,-69.5401926006131));
#8206=CARTESIAN_POINT('Ctrl Pts',(-20.3449962748506,23.8856038856906,-69.5403931033578));
#8207=CARTESIAN_POINT('Ctrl Pts',(-20.3441774102014,23.8776999633682,-69.5408819180821));
#8208=CARTESIAN_POINT('Ctrl Pts',(-20.3437048508246,23.873039574671,-69.5411703949735));
#8209=CARTESIAN_POINT('Ctrl Pts',(-20.3419568652735,23.8554182130945,-69.5422621361128));
#8210=CARTESIAN_POINT('Ctrl Pts',(-20.3407498616769,23.8424507168828,-69.5430675553196));
#8211=CARTESIAN_POINT('Ctrl Pts',(-20.3212162144471,23.6178448064226,-69.5570537791203));
#8212=CARTESIAN_POINT('Ctrl Pts',(-20.3237837381275,23.4049554090462,-69.5709144030612));
#8213=CARTESIAN_POINT('Ctrl Pts',(-20.3615357901215,23.0656276473282,-69.5938298851374));
#8214=CARTESIAN_POINT('Ctrl Pts',(-20.3834999463886,22.9383272821039,-69.6026042250923));
#8215=CARTESIAN_POINT('Ctrl Pts',(-20.4200818728375,22.7827261558073,-69.6133873773212));
#8216=CARTESIAN_POINT('Ctrl Pts',(-20.4275557080576,22.7528632352101,-69.6154592350294));
#8217=CARTESIAN_POINT('Ctrl Pts',(-20.4688210654069,22.5974687039588,-69.6262400979778));
#8218=CARTESIAN_POINT('Ctrl Pts',(-20.5097621395128,22.473942190946,-69.6348133008615));
#8219=CARTESIAN_POINT('Ctrl Pts',(-20.5610351204619,22.345777137666,-69.6434807911215));
#8220=CARTESIAN_POINT('Ctrl Pts',(-20.5640376800154,22.3383521359083,-69.643982078855));
#8221=CARTESIAN_POINT('Ctrl Pts',(-20.56817382582,22.3282326061923,-69.6446640490418));
#8222=CARTESIAN_POINT('Ctrl Pts',(-20.5692834116707,22.3255283946002,-69.6448461692418));
#8223=CARTESIAN_POINT('Ctrl Pts',(-20.5711460690098,22.3210063732845,-69.6451505066849));
#8224=CARTESIAN_POINT('Ctrl Pts',(-20.5718971260879,22.3191877438301,-69.6452728466501));
#8225=CARTESIAN_POINT('Ctrl Pts',(-20.5733795619881,22.3156074316168,-69.6455135838279));
#8226=CARTESIAN_POINT('Ctrl Pts',(-20.5741108393153,22.3138457103649,-69.6456319869689));
#8227=CARTESIAN_POINT('Ctrl Pts',(-20.5757266261717,22.3099628552812,-69.6458928330769));
#8228=CARTESIAN_POINT('Ctrl Pts',(-20.5766118429178,22.3078420125131,-69.6460352327587));
#8229=CARTESIAN_POINT('Ctrl Pts',(-20.5797119683309,22.3004368839684,-69.6465321745449));
#8230=CARTESIAN_POINT('Ctrl Pts',(-20.5819387169661,22.295157519204,-69.64688599722));
#8231=CARTESIAN_POINT('Ctrl Pts',(-20.6045926978961,22.241845045205,-69.6504545753356));
#8232=CARTESIAN_POINT('Ctrl Pts',(-20.6261713548739,22.1943056128722,-69.6536004119877));
#8233=CARTESIAN_POINT('Ctrl Pts',(-20.7741792290303,21.8882182996788,-69.6737491973082));
#8234=CARTESIAN_POINT('Ctrl Pts',(-20.9336143790115,21.647047594965,-69.6892248578868));
#8235=CARTESIAN_POINT('Ctrl Pts',(-21.2239227235977,21.3146646181717,-69.7142807460709));
#8236=CARTESIAN_POINT('Ctrl Pts',(-21.3329769434172,21.2064642814994,-69.7231852483819));
#8237=CARTESIAN_POINT('Ctrl Pts',(-21.4608049453515,21.0965703950268,-69.7333666947652));
#8238=CARTESIAN_POINT('Ctrl Pts',(-21.4723665163702,21.0867718763855,-69.7342853040387));
#8239=CARTESIAN_POINT('Ctrl Pts',(-21.4898488087919,21.072166130011,-69.7356711619499));
#8240=CARTESIAN_POINT('Ctrl Pts',(-21.4957182939447,21.0672976831511,-69.7361359165018));
#8241=CARTESIAN_POINT('Ctrl Pts',(-21.5052064443329,21.0594844113512,-69.7368863737828));
#8242=CARTESIAN_POINT('Ctrl Pts',(-21.508814345567,21.0565265121382,-69.7371715458267));
#8243=CARTESIAN_POINT('Ctrl Pts',(-21.5157298156449,21.0508820032858,-69.7377177916007));
#8244=CARTESIAN_POINT('Ctrl Pts',(-21.5190363173028,21.0481940970221,-69.7379788121445));
#8245=CARTESIAN_POINT('Ctrl Pts',(-21.5249188324979,21.043431455155,-69.7384429142217));
#8246=CARTESIAN_POINT('Ctrl Pts',(-21.5274927323596,21.0413541086916,-69.7386458900112));
#8247=CARTESIAN_POINT('Ctrl Pts',(-21.532583378152,21.037258469448,-69.7390471542757));
#8248=CARTESIAN_POINT('Ctrl Pts',(-21.5350999661484,21.0352399855055,-69.7392454347383));
#8249=CARTESIAN_POINT('Ctrl Pts',(-21.5411759148189,21.0303816135553,-69.7397239488418));
#8250=CARTESIAN_POINT('Ctrl Pts',(-21.5447382647403,21.0275454893941,-69.7400043331419));
#8251=CARTESIAN_POINT('Ctrl Pts',(-21.5578518052053,21.0171506254148,-69.7410358554184));
#8252=CARTESIAN_POINT('Ctrl Pts',(-21.5674397223444,21.0096385745877,-69.7417888559985));
#8253=CARTESIAN_POINT('Ctrl Pts',(-21.7240079052638,20.888394867784,-69.7540666413049));
#8254=CARTESIAN_POINT('Ctrl Pts',(-21.8804853066364,20.7875525532319,-69.7661049540718));
#8255=CARTESIAN_POINT('Ctrl Pts',(-22.1318220021524,20.654761274217,-69.7850621012348));
#8256=CARTESIAN_POINT('Ctrl Pts',(-22.2209506026328,20.6127757640286,-69.791711825621));
#8257=CARTESIAN_POINT('Ctrl Pts',(-22.5170429721264,20.4895352717375,-69.8134187578874));
#8258=CARTESIAN_POINT('Ctrl Pts',(-22.7305383827999,20.4255756397124,-69.8285154675558));
#8259=CARTESIAN_POINT('Ctrl Pts',(-22.9546402982399,20.3830144124232,-69.8428032229158));
#8260=CARTESIAN_POINT('Ctrl Pts',(-22.9603443162225,20.3819470641969,-69.8431658472457));
#8261=CARTESIAN_POINT('Ctrl Pts',(-22.9685750358209,20.3804299121675,-69.8436875744444));
#8262=CARTESIAN_POINT('Ctrl Pts',(-22.9710993982224,20.3799677185317,-69.8438473810731));
#8263=CARTESIAN_POINT('Ctrl Pts',(-22.9754916107563,20.3791689553197,-69.8441250698399));
#8264=CARTESIAN_POINT('Ctrl Pts',(-22.9773592083617,20.3788310200143,-69.8442430306244));
#8265=CARTESIAN_POINT('Ctrl Pts',(-22.9809753581909,20.3781799887585,-69.8444712106288));
#8266=CARTESIAN_POINT('Ctrl Pts',(-22.9827238663473,20.3778666894666,-69.8445814414945));
#8267=CARTESIAN_POINT('Ctrl Pts',(-22.9868985768621,20.3771222229283,-69.8448443891145));
#8268=CARTESIAN_POINT('Ctrl Pts',(-22.9893250208476,20.3766923916458,-69.8449970289975));
#8269=CARTESIAN_POINT('Ctrl Pts',(-22.9966627812733,20.3754012259567,-69.8454580511843));
#8270=CARTESIAN_POINT('Ctrl Pts',(-23.0015756353927,20.3745485011574,-69.8457659437666));
#8271=CARTESIAN_POINT('Ctrl Pts',(-23.0518132659927,20.36594880758,-69.8489066325906));
#8272=CARTESIAN_POINT('Ctrl Pts',(-23.0972997883876,20.3591608286777,-69.8516859010484));
#8273=CARTESIAN_POINT('Ctrl Pts',(-23.1453689344902,20.3530360961506,-69.8545700659835));
#8274=CARTESIAN_POINT('Ctrl Pts',(-23.1478194095478,20.3527267311312,-69.8547169508741));
#8275=CARTESIAN_POINT('Ctrl Pts',(-23.1570157531917,20.351576459898,-69.8552676587031));
#8276=CARTESIAN_POINT('Ctrl Pts',(-23.1637639669199,20.3507540761559,-69.8556706867813));
#8277=CARTESIAN_POINT('Ctrl Pts',(-23.1743133200474,20.3495023221859,-69.8562991195922));
#8278=CARTESIAN_POINT('Ctrl Pts',(-23.1781126709146,20.3490583609529,-69.856525123019));
#8279=CARTESIAN_POINT('Ctrl Pts',(-23.4706770996191,20.3153995523234,-69.8739037076153));
#8280=CARTESIAN_POINT('Ctrl Pts',(-23.7626367658595,20.3213919892458,-69.8895153890468));
#8281=CARTESIAN_POINT('Ctrl Pts',(-24.1929529271619,20.3889184871989,-69.9143151593598));
#8282=CARTESIAN_POINT('Ctrl Pts',(-24.3343497895245,20.4209906135522,-69.9227446799743));
#8283=CARTESIAN_POINT('Ctrl Pts',(-24.4871734345503,20.4666649213482,-69.9323822916213));
#8284=CARTESIAN_POINT('Ctrl Pts',(-24.5012181999091,20.4709672874008,-69.9332729086044));
#8285=CARTESIAN_POINT('Ctrl Pts',(-24.5223437132542,20.477597028551,-69.9346201314908));
#8286=CARTESIAN_POINT('Ctrl Pts',(-24.529446732089,20.4798532380009,-69.9350744073315));
#8287=CARTESIAN_POINT('Ctrl Pts',(-24.5409144501667,20.4835396951919,-69.9358099564711));
#8288=CARTESIAN_POINT('Ctrl Pts',(-24.5452840580032,20.4849546800023,-69.9360907273139));
#8289=CARTESIAN_POINT('Ctrl Pts',(-24.5536481498758,20.4876829444789,-69.9366291310175));
#8290=CARTESIAN_POINT('Ctrl Pts',(-24.5576431205322,20.4889947110628,-69.9368867135306));
#8291=CARTESIAN_POINT('Ctrl Pts',(-24.5647695065191,20.4913501525195,-69.9373469590184));
#8292=CARTESIAN_POINT('Ctrl Pts',(-24.5679019128772,20.4923908287431,-69.9375495225615));
#8293=CARTESIAN_POINT('Ctrl Pts',(-24.5741107365281,20.4944641768382,-69.9379515519471));
#8294=CARTESIAN_POINT('Ctrl Pts',(-24.5771872042629,20.4954966868786,-69.9381510122382));
#8295=CARTESIAN_POINT('Ctrl Pts',(-24.5855421248606,20.4983147749251,-69.938693392857));
#8296=CARTESIAN_POINT('Ctrl Pts',(-24.59081749663,20.5001093930799,-69.9390366126534));
#8297=CARTESIAN_POINT('Ctrl Pts',(-24.6105891054187,20.5068927203371,-69.9403258257028));
#8298=CARTESIAN_POINT('Ctrl Pts',(-24.6250541595463,20.5119711032113,-69.9412747943593));
#8299=CARTESIAN_POINT('Ctrl Pts',(-24.8594038779881,20.5961294444554,-69.9567446154558));
#8300=CARTESIAN_POINT('Ctrl Pts',(-25.0700366496534,20.6987731383425,-69.9720968042006));
#8301=CARTESIAN_POINT('Ctrl Pts',(-25.3408198647654,20.8693094536751,-69.9936665668001));
#8302=CARTESIAN_POINT('Ctrl Pts',(-25.4120689596462,20.9182900553482,-69.9995279332564));
#8303=CARTESIAN_POINT('Ctrl Pts',(-25.5553065080206,21.025489279465,-70.0116231064213));
#8304=CARTESIAN_POINT('Ctrl Pts',(-25.6269346998095,21.0840684946747,-70.0178489538812));
#8305=CARTESIAN_POINT('Ctrl Pts',(-25.7283111838244,21.1745295794955,-70.0268306845277));
#8306=CARTESIAN_POINT('Ctrl Pts',(-25.7600906410713,21.2040609553409,-70.0296724689211));
#8307=CARTESIAN_POINT('Ctrl Pts',(-25.8143888348437,21.2566004969746,-70.0345602380823));
#8308=CARTESIAN_POINT('Ctrl Pts',(-25.8371767164142,21.2793208266191,-70.0366219274718));
#8309=CARTESIAN_POINT('Ctrl Pts',(-25.8716445230647,21.3147315833281,-70.0397511298857));
#8310=CARTESIAN_POINT('Ctrl Pts',(-25.8835686177228,21.3271801616648,-70.0408357187708));
#8311=CARTESIAN_POINT('Ctrl Pts',(-25.8980347654528,21.3425272354005,-70.0421533706192));
#8312=CARTESIAN_POINT('Ctrl Pts',(-25.9006719509888,21.3453350831669,-70.0423936550143));
#8313=CARTESIAN_POINT('Ctrl Pts',(-25.9047893937255,21.34973476245,-70.0427689205692));
#8314=CARTESIAN_POINT('Ctrl Pts',(-25.9062730744668,21.3513233628658,-70.0429041661341));
#8315=CARTESIAN_POINT('Ctrl Pts',(-25.9088985025783,21.3541401578507,-70.0431435256301));
#8316=CARTESIAN_POINT('Ctrl Pts',(-25.9100408922806,21.355367735678,-70.0432476893965));
#8317=CARTESIAN_POINT('Ctrl Pts',(-25.912485791284,21.357999066242,-70.0434706436662));
#8318=CARTESIAN_POINT('Ctrl Pts',(-25.9137880040213,21.3594030844251,-70.0435894111368));
#8319=CARTESIAN_POINT('Ctrl Pts',(-25.9175640194288,21.3634815891704,-70.0439338513392));
#8320=CARTESIAN_POINT('Ctrl Pts',(-25.9200345496766,21.3661591219277,-70.0441592717809));
#8321=CARTESIAN_POINT('Ctrl Pts',(-25.9311381066062,21.3782340508269,-70.0451727213715));
#8322=CARTESIAN_POINT('Ctrl Pts',(-25.9397199678692,21.3876786517263,-70.0459568814096));
#8323=CARTESIAN_POINT('Ctrl Pts',(-25.9498109416931,21.3989174836971,-70.0468803286512));
#8324=CARTESIAN_POINT('Ctrl Pts',(-25.9513743154294,21.4006625169467,-70.0470234363668));
#8325=CARTESIAN_POINT('Ctrl Pts',(-26.1812518950587,21.6578148985226,-70.0680720734399));
#8326=CARTESIAN_POINT('Ctrl Pts',(-26.3674295842823,21.9480385579401,-70.0861980620253));
#8327=CARTESIAN_POINT('Ctrl Pts',(-26.5484479933871,22.3632042878768,-70.112021235616));
#8328=CARTESIAN_POINT('Ctrl Pts',(-26.5872755173855,22.4663948573075,-70.1184117394526));
#8329=CARTESIAN_POINT('Ctrl Pts',(-26.6357203618694,22.618352275501,-70.1279143731896));
#8330=CARTESIAN_POINT('Ctrl Pts',(-26.6496191056561,22.6656756548402,-70.1308856775448));
#8331=CARTESIAN_POINT('Ctrl Pts',(-26.6644782720238,22.7209286812893,-70.1343747157594));
#8332=CARTESIAN_POINT('Ctrl Pts',(-26.6665024547689,22.7285674181835,-70.134857508466));
#8333=CARTESIAN_POINT('Ctrl Pts',(-26.6695385679286,22.7401975082893,-70.1355932513166));
#8334=CARTESIAN_POINT('Ctrl Pts',(-26.6705709878878,22.7441835219459,-70.1358455364618));
#8335=CARTESIAN_POINT('Ctrl Pts',(-26.672348840822,22.7511021360537,-70.1362836488926));
#8336=CARTESIAN_POINT('Ctrl Pts',(-26.6730977896009,22.7540338347327,-70.1364693619936));
#8337=CARTESIAN_POINT('Ctrl Pts',(-26.6746462203631,22.760130832826,-70.1368557271043));
#8338=CARTESIAN_POINT('Ctrl Pts',(-26.6754450233196,22.7632962997588,-70.1370564008647));
#8339=CARTESIAN_POINT('Ctrl Pts',(-26.6776181846773,22.7719635151973,-70.1376060752315));
#8340=CARTESIAN_POINT('Ctrl Pts',(-26.6789828288816,22.7774676667662,-70.1379553896221));
#8341=CARTESIAN_POINT('Ctrl Pts',(-26.6841412823517,22.798511397466,-70.1392918469077));
#8342=CARTESIAN_POINT('Ctrl Pts',(-26.6878338551131,22.8140753393836,-70.1402822528392));
#8343=CARTESIAN_POINT('Ctrl Pts',(-26.7458671042957,23.0670519942177,-70.1564138368025));
#8344=CARTESIAN_POINT('Ctrl Pts',(-26.7732275270404,23.3097940514145,-70.1724632836176));
#8345=CARTESIAN_POINT('Ctrl Pts',(-26.7727713000577,23.8004142718755,-70.2055803345265));
#8346=CARTESIAN_POINT('Ctrl Pts',(-26.7441088293428,24.0467514073952,-70.2225345037189));
#8347=CARTESIAN_POINT('Ctrl Pts',(-26.6843247594727,24.3011915346032,-70.2390459835505));
#8348=CARTESIAN_POINT('Ctrl Pts',(-26.6809945986695,24.3149565546434,-70.2399358490089));
#8349=CARTESIAN_POINT('Ctrl Pts',(-26.6766691087743,24.3323337136085,-70.2410545399636));
#8350=CARTESIAN_POINT('Ctrl Pts',(-26.6757581410027,24.3359663950477,-70.2412881417185));
#8351=CARTESIAN_POINT('Ctrl Pts',(-26.6743087717276,24.3417036613345,-70.2416566604289));
#8352=CARTESIAN_POINT('Ctrl Pts',(-26.673774574792,24.3438092894938,-70.2417918207073));
#8353=CARTESIAN_POINT('Ctrl Pts',(-26.6727778470958,24.3477214619212,-70.2420427748023));
#8354=CARTESIAN_POINT('Ctrl Pts',(-26.6723158802198,24.3495281336152,-70.2421586003891));
#8355=CARTESIAN_POINT('Ctrl Pts',(-26.6712825230233,24.3535548475896,-70.2424166040518));
#8356=CARTESIAN_POINT('Ctrl Pts',(-26.6707103333404,24.3557746764691,-70.2425587346177));
#8357=CARTESIAN_POINT('Ctrl Pts',(-26.6690323276068,24.3622559366416,-70.2429734262373));
#8358=CARTESIAN_POINT('Ctrl Pts',(-26.667920141628,24.3665157365218,-70.2432456171354));
#8359=CARTESIAN_POINT('Ctrl Pts',(-26.6598317145208,24.3972376420547,-70.2452061285938));
#8360=CARTESIAN_POINT('Ctrl Pts',(-26.6525271229582,24.4236132545441,-70.2468756540591));
#8361=CARTESIAN_POINT('Ctrl Pts',(-26.6286584436974,24.5057180384982,-70.2520392229694));
#8362=CARTESIAN_POINT('Ctrl Pts',(-26.610921093037,24.56109680291,-70.2554734790134));
#8363=CARTESIAN_POINT('Ctrl Pts',(-26.5643876032176,24.693898455406,-70.263658288867));
#8364=CARTESIAN_POINT('Ctrl Pts',(-26.5340946061728,24.7707541349276,-70.2683527472317));
#8365=CARTESIAN_POINT('Ctrl Pts',(-26.3983109742341,25.0798685836107,-70.2873686658508));
#8366=CARTESIAN_POINT('Ctrl Pts',(-26.2683941139236,25.3003566998763,-70.3013326076835));
#8367=CARTESIAN_POINT('Ctrl Pts',(-26.0992935653018,25.5223286179826,-70.3176449710777));
#8368=CARTESIAN_POINT('Ctrl Pts',(-26.0845277947892,25.5412681345318,-70.3190558560882));
#8369=CARTESIAN_POINT('Ctrl Pts',(-26.0660276196305,25.5644583821631,-70.3208081727972));
#8370=CARTESIAN_POINT('Ctrl Pts',(-26.0624916474726,25.5688669390884,-70.321142415333));
#8371=CARTESIAN_POINT('Ctrl Pts',(-26.0564317940648,25.5763816206832,-70.3217140892147));
#8372=CARTESIAN_POINT('Ctrl Pts',(-26.0539136818858,25.5794923955847,-70.3219513084563));
#8373=CARTESIAN_POINT('Ctrl Pts',(-26.0478990935079,25.5868943397411,-70.3225171277646));
#8374=CARTESIAN_POINT('Ctrl Pts',(-26.0443973511884,25.5911811979813,-70.3228459227988));
#8375=CARTESIAN_POINT('Ctrl Pts',(-26.0365225776462,25.6007710187896,-70.3235839357552));
#8376=CARTESIAN_POINT('Ctrl Pts',(-26.0321435993699,25.6060690445317,-70.3239933768843));
#8377=CARTESIAN_POINT('Ctrl Pts',(-26.0248990257956,25.6147772063091,-70.3246692224832));
#8378=CARTESIAN_POINT('Ctrl Pts',(-26.022043236208,25.6181954989083,-70.3249352496621));
#8379=CARTESIAN_POINT('Ctrl Pts',(-26.0148305388406,25.6267925895438,-70.3256061717206));
#8380=CARTESIAN_POINT('Ctrl Pts',(-26.0104644017425,25.6319635871977,-70.3260114241569));
#8381=CARTESIAN_POINT('Ctrl Pts',(-26.0014342076304,25.6425903324593,-70.326847797595));
#8382=CARTESIAN_POINT('Ctrl Pts',(-25.9967681508325,25.6480443242752,-70.3272789961894));
#8383=CARTESIAN_POINT('Ctrl Pts',(-25.9730515156712,25.6755791261767,-70.3294658869556));
#8384=CARTESIAN_POINT('Ctrl Pts',(-25.9537205395439,25.6974156598916,-70.3312327891465));
#8385=CARTESIAN_POINT('Ctrl Pts',(-25.9297611094909,25.7237515523123,-70.3334052258832));
#8386=CARTESIAN_POINT('Ctrl Pts',(-25.9254116093061,25.728503761356,-70.3337989107911));
#8387=CARTESIAN_POINT('Ctrl Pts',(-25.9182171942355,25.7363171198167,-70.3344489769237));
#8388=CARTESIAN_POINT('Ctrl Pts',(-25.915380507959,25.7393858492691,-70.3347050066766));
#8389=CARTESIAN_POINT('Ctrl Pts',(-25.9102582607758,25.7449055229732,-70.3351668156039));
#8390=CARTESIAN_POINT('Ctrl Pts',(-25.9079748267202,25.7473584401178,-70.3353725034032));
#8391=CARTESIAN_POINT('Ctrl Pts',(-25.9030970596168,25.7525818886174,-70.3358115017229));
#8392=CARTESIAN_POINT('Ctrl Pts',(-25.9005016517379,25.7553514053228,-70.3360448583447));
#8393=CARTESIAN_POINT('Ctrl Pts',(-25.8935008303259,25.7627954651905,-70.3366736988925));
#8394=CARTESIAN_POINT('Ctrl Pts',(-25.8890863409604,25.7674614152416,-70.3370695746497));
#8395=CARTESIAN_POINT('Ctrl Pts',(-25.8675801120637,25.790056998115,-70.3389950651255));
#8396=CARTESIAN_POINT('Ctrl Pts',(-25.8502963619595,25.8078019743841,-70.340533019152));
#8397=CARTESIAN_POINT('Ctrl Pts',(-25.6182854776305,26.0405740879293,-70.3610584189883));
#8398=CARTESIAN_POINT('Ctrl Pts',(-25.3744413431208,26.2243337719409,-70.3815107714623));
#8399=CARTESIAN_POINT('Ctrl Pts',(-24.9814541353119,26.4414234148219,-70.4118758134113));
#8400=CARTESIAN_POINT('Ctrl Pts',(-24.8497243614881,26.5029780065853,-70.4216448297848));
#8401=CARTESIAN_POINT('Ctrl Pts',(-24.7131301523167,26.5558863625713,-70.4310984914138));
#8402=CARTESIAN_POINT('Ctrl Pts',(-24.7119789723293,26.5563314998846,-70.4311781167516));
#8403=CARTESIAN_POINT('Ctrl Pts',(-24.7079918478755,26.5578706054534,-70.4314537344056));
#8404=CARTESIAN_POINT('Ctrl Pts',(-24.705154602333,26.558961226336,-70.4316495745268));
#8405=CARTESIAN_POINT('Ctrl Pts',(-24.6660398962727,26.5739332134065,-70.4343454235395));
#8406=CARTESIAN_POINT('Ctrl Pts',(-24.6295138497505,26.5871624171628,-70.4368151094385));
#8407=CARTESIAN_POINT('Ctrl Pts',(-24.5878210460335,26.6014156436657,-70.4395732250138));
#8408=CARTESIAN_POINT('Ctrl Pts',(-24.5828823897317,26.6030906104339,-70.4398989711606));
#8409=CARTESIAN_POINT('Ctrl Pts',(-24.5756013273432,26.6055403244312,-70.4403777797364));
#8410=CARTESIAN_POINT('Ctrl Pts',(-24.5732620942583,26.6063243705401,-70.4405313911459));
#8411=CARTESIAN_POINT('Ctrl Pts',(-24.5691716417384,26.6076901540877,-70.4407996160293));
#8412=CARTESIAN_POINT('Ctrl Pts',(-24.5674208214995,26.6082730741243,-70.440914300176));
#8413=CARTESIAN_POINT('Ctrl Pts',(-24.5640742488086,26.6093840937031,-70.4411332748865));
#8414=CARTESIAN_POINT('Ctrl Pts',(-24.5624785888148,26.6099124469607,-70.4412375806105));
#8415=CARTESIAN_POINT('Ctrl Pts',(-24.5581812942722,26.6113316329999,-70.4415182141942));
#8416=CARTESIAN_POINT('Ctrl Pts',(-24.5554788843313,26.6122201401113,-70.4416944032691));
#8417=CARTESIAN_POINT('Ctrl Pts',(-24.5496696224129,26.6141216084974,-70.442072531881));
#8418=CARTESIAN_POINT('Ctrl Pts',(-24.5465623952858,26.6151334261082,-70.4422744039766));
#8419=CARTESIAN_POINT('Ctrl Pts',(-24.5378371260596,26.6179599960635,-70.4428402221975));
#8420=CARTESIAN_POINT('Ctrl Pts',(-24.5322155930431,26.619764050715,-70.443203548117));
#8421=CARTESIAN_POINT('Ctrl Pts',(-24.4812089082402,26.6359785815578,-70.4464893804643));
#8422=CARTESIAN_POINT('Ctrl Pts',(-24.4355116713999,26.6493978754957,-70.4493558598061));
#8423=CARTESIAN_POINT('Ctrl Pts',(-24.3321874209905,26.6772675478434,-70.4556993895046));
#8424=CARTESIAN_POINT('Ctrl Pts',(-24.2744239915123,26.6911475571649,-70.4591510517077));
#8425=CARTESIAN_POINT('Ctrl Pts',(-23.8387652513709,26.7831731355364,-70.4846989671614));
#8426=CARTESIAN_POINT('Ctrl Pts',(-23.4499915480244,26.7944776709091,-70.5052222929952));
#8427=CARTESIAN_POINT('Ctrl Pts',(-23.0486087575204,26.7337839447468,-70.5297769508713));
#8428=CARTESIAN_POINT('Ctrl Pts',(-23.0288333261363,26.7306048263253,-70.5309941847827));
#8429=CARTESIAN_POINT('Ctrl Pts',(-23.0029672781317,26.7261988439782,-70.5325965142103));
#8430=CARTESIAN_POINT('Ctrl Pts',(-22.9968484632859,26.7251383664122,-70.5329763070903));
#8431=CARTESIAN_POINT('Ctrl Pts',(-22.9874109180102,26.7234745942296,-70.5335632621162));
#8432=CARTESIAN_POINT('Ctrl Pts',(-22.9840899821133,26.7228837594877,-70.5337700268358));
#8433=CARTESIAN_POINT('Ctrl Pts',(-22.9774790468936,26.7216968835623,-70.5341820782333));
#8434=CARTESIAN_POINT('Ctrl Pts',(-22.9741890352289,26.7211009339034,-70.5343873617584));
#8435=CARTESIAN_POINT('Ctrl Pts',(-22.9668985420328,26.7197686195803,-70.534842752281));
#8436=CARTESIAN_POINT('Ctrl Pts',(-22.9628985200832,26.7190297995729,-70.5350929373806));
#8437=CARTESIAN_POINT('Ctrl Pts',(-22.9513633741587,26.7168766202313,-70.5358153699812));
#8438=CARTESIAN_POINT('Ctrl Pts',(-22.9438319228895,26.7154429500903,-70.5362882338329));
#8439=CARTESIAN_POINT('Ctrl Pts',(-22.8931372104116,26.7056052399919,-70.5394791386778));
#8440=CARTESIAN_POINT('Ctrl Pts',(-22.8501465250665,26.6963457486338,-70.5422244491292));
#8441=CARTESIAN_POINT('Ctrl Pts',(-22.7383682877288,26.6698660606305,-70.5494700621659));
#8442=CARTESIAN_POINT('Ctrl Pts',(-22.669939006162,26.6512509912246,-70.5540138063868));
#8443=CARTESIAN_POINT('Ctrl Pts',(-22.4599210496119,26.5866073808458,-70.568298840626));
#8444=CARTESIAN_POINT('Ctrl Pts',(-22.3208775763164,26.5330201220393,-70.5782540667229));
#8445=CARTESIAN_POINT('Ctrl Pts',(-22.1486907581259,26.4525692505281,-70.5910943196805));
#8446=CARTESIAN_POINT('Ctrl Pts',(-22.1116802286532,26.4344033675362,-70.5938850984888));
#8447=CARTESIAN_POINT('Ctrl Pts',(-22.0750359531635,26.415536742541,-70.5966750543042));
#8448=CARTESIAN_POINT('Ctrl Pts',(-22.0750360699906,26.4155368026905,-70.8406447795461));
#8449=CARTESIAN_POINT('Ctrl Pts',(-22.1568434848462,26.4576560598637,-70.8345484782489));
#8450=CARTESIAN_POINT('Ctrl Pts',(-22.2404443674471,26.496266412956,-70.828560865941));
#8451=CARTESIAN_POINT('Ctrl Pts',(-22.3331656296512,26.5343577118191,-70.8222657796152));
#8452=CARTESIAN_POINT('Ctrl Pts',(-22.3407313430195,26.5374322636108,-70.8217545830891));
#8453=CARTESIAN_POINT('Ctrl Pts',(-22.3510418599516,26.5415766538885,-70.8210613492461));
#8454=CARTESIAN_POINT('Ctrl Pts',(-22.3537764790467,26.5426715021678,-70.8208778121836));
#8455=CARTESIAN_POINT('Ctrl Pts',(-22.3583448235514,26.5444932482402,-70.8205717524333));
#8456=CARTESIAN_POINT('Ctrl Pts',(-22.360177715015,26.5452222116924,-70.8204491040594));
#8457=CARTESIAN_POINT('Ctrl Pts',(-22.3637811833146,26.5466515250489,-70.8202082687369));
#8458=CARTESIAN_POINT('Ctrl Pts',(-22.3655517111024,26.5473519884394,-70.8200900750433));
#8459=CARTESIAN_POINT('Ctrl Pts',(-22.3694480743911,26.5488894913646,-70.8198302706933));
#8460=CARTESIAN_POINT('Ctrl Pts',(-22.3715741852132,26.5497258417773,-70.8196887020245));
#8461=CARTESIAN_POINT('Ctrl Pts',(-22.3787590864162,26.552543354788,-70.8192109514106));
#8462=CARTESIAN_POINT('Ctrl Pts',(-22.383822032616,26.5545140001093,-70.8188754040773));
#8463=CARTESIAN_POINT('Ctrl Pts',(-22.4308167155575,26.5726689845069,-70.8157708640787));
#8464=CARTESIAN_POINT('Ctrl Pts',(-22.4730803274987,26.5879882518044,-70.8130528741506));
#8465=CARTESIAN_POINT('Ctrl Pts',(-22.5267828017507,26.6061918923568,-70.8096754184062));
#8466=CARTESIAN_POINT('Ctrl Pts',(-22.5379331442031,26.609903676736,-70.8089782486736));
#8467=CARTESIAN_POINT('Ctrl Pts',(-22.7993159653002,26.6953288540924,-70.7927257076985));
#8468=CARTESIAN_POINT('Ctrl Pts',(-23.0586315226244,26.7461488067811,-70.7784651185817));
#8469=CARTESIAN_POINT('Ctrl Pts',(-23.5065209382037,26.7780534544468,-70.7531071974504));
#8470=CARTESIAN_POINT('Ctrl Pts',(-23.692541691839,26.775209832435,-70.7423774027068));
#8471=CARTESIAN_POINT('Ctrl Pts',(-23.8863084304576,26.7554462237052,-70.7305466914208));
#8472=CARTESIAN_POINT('Ctrl Pts',(-23.8953463922374,26.7544857309435,-70.7299934316467));
#8473=CARTESIAN_POINT('Ctrl Pts',(-23.9116567044336,26.7526825750465,-70.7289923539003));
#8474=CARTESIAN_POINT('Ctrl Pts',(-23.9189305004199,26.7518533363886,-70.7285449610337));
#8475=CARTESIAN_POINT('Ctrl Pts',(-23.9301452383441,26.7505360914262,-70.7278536851682));
#8476=CARTESIAN_POINT('Ctrl Pts',(-23.9340882423245,26.7500655697134,-70.7276103551273));
#8477=CARTESIAN_POINT('Ctrl Pts',(-23.941349118929,26.7491855097309,-70.7271617470212));
#8478=CARTESIAN_POINT('Ctrl Pts',(-23.9446672472856,26.7487780936537,-70.7269565363545));
#8479=CARTESIAN_POINT('Ctrl Pts',(-23.9513416884471,26.7479480291313,-70.7265433437022));
#8480=CARTESIAN_POINT('Ctrl Pts',(-23.9546979814377,26.7475252576337,-70.726335358065));
#8481=CARTESIAN_POINT('Ctrl Pts',(-23.9642610271745,26.7463053609559,-70.7257421490837));
#8482=CARTESIAN_POINT('Ctrl Pts',(-23.9704661070976,26.7454954445138,-70.7253565211746));
#8483=CARTESIAN_POINT('Ctrl Pts',(-23.9969101901692,26.7419654754151,-70.7237100038563));
#8484=CARTESIAN_POINT('Ctrl Pts',(-24.0171251009287,26.7390712082845,-70.7224436060411));
#8485=CARTESIAN_POINT('Ctrl Pts',(-24.3755022789662,26.6842798673052,-70.6998512072786));
#8486=CARTESIAN_POINT('Ctrl Pts',(-24.7032382458937,26.5790584024982,-70.6766016889036));
#8487=CARTESIAN_POINT('Ctrl Pts',(-25.1458053302644,26.3545600222801,-70.6431762828056));
#8488=CARTESIAN_POINT('Ctrl Pts',(-25.2782516741849,26.2749473155368,-70.6329273010685));
#8489=CARTESIAN_POINT('Ctrl Pts',(-25.409191273214,26.182836290899,-70.6229005116117));
#8490=CARTESIAN_POINT('Ctrl Pts',(-25.4138760814877,26.1795219663123,-70.6225419279107));
#8491=CARTESIAN_POINT('Ctrl Pts',(-25.4206336580176,26.1747141014772,-70.6220249504299));
#8492=CARTESIAN_POINT('Ctrl Pts',(-25.4227135081198,26.1732306064876,-70.6218658705311));
#8493=CARTESIAN_POINT('Ctrl Pts',(-25.4263339287671,26.1706417678853,-70.621589023588));
#8494=CARTESIAN_POINT('Ctrl Pts',(-25.4278752895813,26.1695375365627,-70.6214711792857));
#8495=CARTESIAN_POINT('Ctrl Pts',(-25.430861527955,26.1673942040228,-70.6212429086787));
#8496=CARTESIAN_POINT('Ctrl Pts',(-25.4323065154895,26.1663552689686,-70.6211324712407));
#8497=CARTESIAN_POINT('Ctrl Pts',(-25.4357602564367,26.1638677130091,-70.6208685515591));
#8498=CARTESIAN_POINT('Ctrl Pts',(-25.4377682057396,26.1624179698686,-70.620715147479));
#8499=CARTESIAN_POINT('Ctrl Pts',(-25.4449638996919,26.1572100363396,-70.6201655243324));
#8500=CARTESIAN_POINT('Ctrl Pts',(-25.4501421521942,26.1534386623107,-70.6197702148695));
#8501=CARTESIAN_POINT('Ctrl Pts',(-25.5275203311578,26.0967294780353,-70.6138658294026));
#8502=CARTESIAN_POINT('Ctrl Pts',(-25.5975027934258,26.0408152382713,-70.6085606978806));
#8503=CARTESIAN_POINT('Ctrl Pts',(-25.8902445655522,25.7862317903975,-70.5860818100272));
#8504=CARTESIAN_POINT('Ctrl Pts',(-26.0871374555623,25.5600806093899,-70.5700667804063));
#8505=CARTESIAN_POINT('Ctrl Pts',(-26.2948877096018,25.241352581633,-70.5481095922781));
#8506=CARTESIAN_POINT('Ctrl Pts',(-26.337023228474,25.1709774098234,-70.5433049373713));
#8507=CARTESIAN_POINT('Ctrl Pts',(-26.3970718102084,25.0614053487511,-70.5358369958345));
#8508=CARTESIAN_POINT('Ctrl Pts',(-26.4169603498093,25.0233271581647,-70.5332442313067));
#8509=CARTESIAN_POINT('Ctrl Pts',(-26.4394724278771,24.9780424289846,-70.5301596689538));
#8510=CARTESIAN_POINT('Ctrl Pts',(-26.4428394527522,24.9712087244939,-70.529694165817));
#8511=CARTESIAN_POINT('Ctrl Pts',(-26.4479625776008,24.96071717696,-70.5289794311797));
#8512=CARTESIAN_POINT('Ctrl Pts',(-26.4497360684655,24.9570678164584,-70.5287308074063));
#8513=CARTESIAN_POINT('Ctrl Pts',(-26.4529582921737,24.9504053833599,-70.5282768833974));
#8514=CARTESIAN_POINT('Ctrl Pts',(-26.454409239218,24.9473933828464,-70.5280716606924));
#8515=CARTESIAN_POINT('Ctrl Pts',(-26.4573175139039,24.9413320312493,-70.5276586489568));
#8516=CARTESIAN_POINT('Ctrl Pts',(-26.4587747367852,24.9382826348356,-70.5274508566037));
#8517=CARTESIAN_POINT('Ctrl Pts',(-26.4629097602464,24.9295945476515,-70.5268587975263));
#8518=CARTESIAN_POINT('Ctrl Pts',(-26.4655759678214,24.9239503841758,-70.5264741287578));
#8519=CARTESIAN_POINT('Ctrl Pts',(-26.4768397958023,24.8999252065921,-70.5248365270691));
#8520=CARTESIAN_POINT('Ctrl Pts',(-26.4852799560693,24.8814712709094,-70.5235781591521));
#8521=CARTESIAN_POINT('Ctrl Pts',(-26.6424991168747,24.5289560777802,-70.4995265927446));
#8522=CARTESIAN_POINT('Ctrl Pts',(-26.7334890350843,24.1721084327779,-70.4744903825534));
#8523=CARTESIAN_POINT('Ctrl Pts',(-26.7695858619726,23.7218455905839,-70.4442180147743));
#8524=CARTESIAN_POINT('Ctrl Pts',(-26.7730246589785,23.6356536313015,-70.4385046968183));
#8525=CARTESIAN_POINT('Ctrl Pts',(-26.7729907852082,23.5042804733903,-70.4300140636944));
#8526=CARTESIAN_POINT('Ctrl Pts',(-26.7720307068816,23.4591416663388,-70.4271360544965));
#8527=CARTESIAN_POINT('Ctrl Pts',(-26.7698925606029,23.4086007306609,-70.4239686538314));
#8528=CARTESIAN_POINT('Ctrl Pts',(-26.7696488954935,23.4031668346537,-70.4236288257262));
#8529=CARTESIAN_POINT('Ctrl Pts',(-26.7692832932904,23.3954502596045,-70.4231472815852));
#8530=CARTESIAN_POINT('Ctrl Pts',(-26.7691726848207,23.3931670918134,-70.4230049323471));
#8531=CARTESIAN_POINT('Ctrl Pts',(-26.7689654751555,23.3889820241303,-70.4227442442523));
#8532=CARTESIAN_POINT('Ctrl Pts',(-26.7688696172047,23.3870800893672,-70.4226258632761));
#8533=CARTESIAN_POINT('Ctrl Pts',(-26.7686710585271,23.3832087115309,-70.4223850854739));
#8534=CARTESIAN_POINT('Ctrl Pts',(-26.7685682358629,23.3812392775772,-70.4222626957298));
#8535=CARTESIAN_POINT('Ctrl Pts',(-26.7683074276147,23.3763303804245,-70.4219578754441));
#8536=CARTESIAN_POINT('Ctrl Pts',(-26.7681472218615,23.3733910293306,-70.4217755707522));
#8537=CARTESIAN_POINT('Ctrl Pts',(-26.7675281322249,23.3623117387532,-70.4210892093462));
#8538=CARTESIAN_POINT('Ctrl Pts',(-26.7670423828434,23.3541732406579,-70.4205866564937));
#8539=CARTESIAN_POINT('Ctrl Pts',(-26.7576558439059,23.2063411444308,-70.4114861566057));
#8540=CARTESIAN_POINT('Ctrl Pts',(-26.7396926774909,23.0673511729968,-70.4033843704302));
#8541=CARTESIAN_POINT('Ctrl Pts',(-26.6447873028743,22.5834926157689,-70.3754362690836));
#8542=CARTESIAN_POINT('Ctrl Pts',(-26.5203772922803,22.2505870940093,-70.3563715356991));
#8543=CARTESIAN_POINT('Ctrl Pts',(-26.3342669732415,21.9267379737192,-70.3337839927446));
#8544=CARTESIAN_POINT('Ctrl Pts',(-26.3239070427488,21.9091015471656,-70.3325411310172));
#8545=CARTESIAN_POINT('Ctrl Pts',(-26.310157332583,21.8861965646208,-70.3309097856292));
#8546=CARTESIAN_POINT('Ctrl Pts',(-26.3069189289913,21.8808373213106,-70.3305268470205));
#8547=CARTESIAN_POINT('Ctrl Pts',(-26.3019065784676,21.8725967212578,-70.3299360965051));
#8548=CARTESIAN_POINT('Ctrl Pts',(-26.3001436655819,21.8697086426385,-70.3297286903959));
#8549=CARTESIAN_POINT('Ctrl Pts',(-26.2966299688226,21.8639726880741,-70.3293160343098));
#8550=CARTESIAN_POINT('Ctrl Pts',(-26.294879295434,21.86112474914,-70.3291107885816));
#8551=CARTESIAN_POINT('Ctrl Pts',(-26.2909972798832,21.8548315810051,-70.3286564534698));
#8552=CARTESIAN_POINT('Ctrl Pts',(-26.2888638687847,21.8513876403974,-70.3284072878832));
#8553=CARTESIAN_POINT('Ctrl Pts',(-26.2827154698159,21.8415040294614,-70.3276906872481));
#8554=CARTESIAN_POINT('Ctrl Pts',(-26.2786842425549,21.835074538108,-70.3272226512513));
#8555=CARTESIAN_POINT('Ctrl Pts',(-26.2520026432515,21.7928515784222,-70.3241365891549));
#8556=CARTESIAN_POINT('Ctrl Pts',(-26.2286720828989,21.7574948215304,-70.3214933022386));
#8557=CARTESIAN_POINT('Ctrl Pts',(-26.1578474666666,21.6546318228771,-70.3136222322753));
#8558=CARTESIAN_POINT('Ctrl Pts',(-26.1084523159659,21.5884826354331,-70.3083233744047));
#8559=CARTESIAN_POINT('Ctrl Pts',(-25.8691902383273,21.292488459127,-70.2834878438769));
#8560=CARTESIAN_POINT('Ctrl Pts',(-25.6505876051953,21.0878308124263,-70.2628606417758));
#8561=CARTESIAN_POINT('Ctrl Pts',(-25.3334292928987,20.8642700355719,-70.2371946342417));
#8562=CARTESIAN_POINT('Ctrl Pts',(-25.2577013936905,20.8155051494572,-70.2313498034771));
#8563=CARTESIAN_POINT('Ctrl Pts',(-25.1744897620466,20.7667274071141,-70.2253030747068));
#8564=CARTESIAN_POINT('Ctrl Pts',(-25.1689467996445,20.7635003776245,-70.2249020238984));
#8565=CARTESIAN_POINT('Ctrl Pts',(-25.1612490436761,20.7590495758212,-70.2243475135749));
#8566=CARTESIAN_POINT('Ctrl Pts',(-25.1591024648436,20.7578117364044,-70.2241931470206));
#8567=CARTESIAN_POINT('Ctrl Pts',(-25.1554113936087,20.7556889237034,-70.223928166054));
#8568=CARTESIAN_POINT('Ctrl Pts',(-25.1538675960381,20.7548027545503,-70.223817473633));
#8569=CARTESIAN_POINT('Ctrl Pts',(-25.1506780338116,20.752975396867,-70.223589060378));
#8570=CARTESIAN_POINT('Ctrl Pts',(-25.1490321759769,20.7520343833191,-70.2234713514695));
#8571=CARTESIAN_POINT('Ctrl Pts',(-25.145167640129,20.7498293708869,-70.2231953292544));
#8572=CARTESIAN_POINT('Ctrl Pts',(-25.1429482826786,20.7485665522161,-70.2230370930785));
#8573=CARTESIAN_POINT('Ctrl Pts',(-25.1360771244657,20.7446676530103,-70.2225480506317));
#8574=CARTESIAN_POINT('Ctrl Pts',(-25.1314202323325,20.7420404930526,-70.222217820715));
#8575=CARTESIAN_POINT('Ctrl Pts',(-25.1204323587239,20.7358777424988,-70.2214414572104));
#8576=CARTESIAN_POINT('Ctrl Pts',(-25.1140959091309,20.7323518882253,-70.2209959365115));
#8577=CARTESIAN_POINT('Ctrl Pts',(-25.0483780790752,20.6960737969633,-70.2163973247492));
#8578=CARTESIAN_POINT('Ctrl Pts',(-24.9879838837496,20.6651794812264,-70.2123571893629));
#8579=CARTESIAN_POINT('Ctrl Pts',(-24.8869146166182,20.6174409696595,-70.2058239457316));
#8580=CARTESIAN_POINT('Ctrl Pts',(-24.846793087314,20.5994844867096,-70.2032876258301));
#8581=CARTESIAN_POINT('Ctrl Pts',(-24.5380927814879,20.4688375136681,-70.1841152455068));
#8582=CARTESIAN_POINT('Ctrl Pts',(-24.2557246272593,20.3922041578629,-70.1683990101405));
#8583=CARTESIAN_POINT('Ctrl Pts',(-23.8679499868752,20.3416482215355,-70.1456452288007));
#8584=CARTESIAN_POINT('Ctrl Pts',(-23.7684722534536,20.3333517972032,-70.1397229675672));
#8585=CARTESIAN_POINT('Ctrl Pts',(-23.6594109589498,20.3293380900479,-70.1330802995748));
#8586=CARTESIAN_POINT('Ctrl Pts',(-23.6500436117652,20.3290342621462,-70.132508572211));
#8587=CARTESIAN_POINT('Ctrl Pts',(-23.6361456577979,20.328644165389,-70.1316585232879));
#8588=CARTESIAN_POINT('Ctrl Pts',(-23.6316159213539,20.3285265822315,-70.1313811847045));
#8589=CARTESIAN_POINT('Ctrl Pts',(-23.6238667159252,20.3283417812433,-70.130906239806));
#8590=CARTESIAN_POINT('Ctrl Pts',(-23.6206473571777,20.3282698345924,-70.130708782147));
#8591=CARTESIAN_POINT('Ctrl Pts',(-23.6143885523189,20.3281393469914,-70.1303246181164));
#8592=CARTESIAN_POINT('Ctrl Pts',(-23.6113491201028,20.3280802813381,-70.1301379284605));
#8593=CARTESIAN_POINT('Ctrl Pts',(-23.60408642782,20.3279494244053,-70.1296915227256));
#8594=CARTESIAN_POINT('Ctrl Pts',(-23.5998631094838,20.3278816353021,-70.1294316812858));
#8595=CARTESIAN_POINT('Ctrl Pts',(-23.5873940382827,20.3277060114427,-70.1286637638229));
#8596=CARTESIAN_POINT('Ctrl Pts',(-23.5791480371971,20.3276215235842,-70.1281549556894));
#8597=CARTESIAN_POINT('Ctrl Pts',(-23.5167913918398,20.3272219736655,-70.1242998572468));
#8598=CARTESIAN_POINT('Ctrl Pts',(-23.4626836377807,20.3282381401279,-70.1209119896705));
#8599=CARTESIAN_POINT('Ctrl Pts',(-23.2790364336706,20.3363162714833,-70.1092581570401));
#8600=CARTESIAN_POINT('Ctrl Pts',(-23.1499211179655,20.3498350401953,-70.1007959728171));
#8601=CARTESIAN_POINT('Ctrl Pts',(-22.7907392180615,20.4095188907948,-70.0765658497809));
#8602=CARTESIAN_POINT('Ctrl Pts',(-22.5643929998235,20.4730555631309,-70.0604409076954));
#8603=CARTESIAN_POINT('Ctrl Pts',(-22.2604450512975,20.5953906309131,-70.0387407774199));
#8604=CARTESIAN_POINT('Ctrl Pts',(-22.1754852917749,20.6339481752089,-70.0326790631893));
#8605=CARTESIAN_POINT('Ctrl Pts',(-22.0865438772052,20.6790652638132,-70.0264266033907));
#8606=CARTESIAN_POINT('Ctrl Pts',(-22.0807874485577,20.6820071231527,-70.0260223670662));
#8607=CARTESIAN_POINT('Ctrl Pts',(-22.0728293885409,20.6861043860963,-70.0254641655527));
#8608=CARTESIAN_POINT('Ctrl Pts',(-22.0706202338591,20.6872450208479,-70.025309277587));
#8609=CARTESIAN_POINT('Ctrl Pts',(-22.0668296962131,20.6892077172628,-70.0250436366114));
#8610=CARTESIAN_POINT('Ctrl Pts',(-22.0652476756486,20.690028534073,-70.0249328047202));
#8611=CARTESIAN_POINT('Ctrl Pts',(-22.0621536215228,20.6916371146009,-70.0247161160105));
#8612=CARTESIAN_POINT('Ctrl Pts',(-22.0606415358581,20.6924247638974,-70.0246102525814));
#8613=CARTESIAN_POINT('Ctrl Pts',(-22.0569719596457,20.6943399591972,-70.0243534207472));
#8614=CARTESIAN_POINT('Ctrl Pts',(-22.0548151150017,20.6954687532875,-70.0242025320468));
#8615=CARTESIAN_POINT('Ctrl Pts',(-22.048232751481,20.6989231687534,-70.0237422433672));
#8616=CARTESIAN_POINT('Ctrl Pts',(-22.0438113365543,20.7012566590219,-70.0234333420699));
#8617=CARTESIAN_POINT('Ctrl Pts',(-21.9997705414853,20.7246312584567,-70.0203590318891));
#8618=CARTESIAN_POINT('Ctrl Pts',(-21.9605867014153,20.7464884490534,-70.0176447073522));
#8619=CARTESIAN_POINT('Ctrl Pts',(-21.8501714376273,20.8111386528365,-70.0100194533269));
#8620=CARTESIAN_POINT('Ctrl Pts',(-21.780117864996,20.855879520925,-70.0052096887058));
#8621=CARTESIAN_POINT('Ctrl Pts',(-21.5234094871498,21.0341696885261,-69.9873918105921));
#8622=CARTESIAN_POINT('Ctrl Pts',(-21.3494672165008,21.18481040924,-69.9748711948285));
#8623=CARTESIAN_POINT('Ctrl Pts',(-21.0895719395568,21.4635874314477,-69.9531234034569));
#8624=CARTESIAN_POINT('Ctrl Pts',(-20.9941239734929,21.5816699427553,-69.944258149534));
#8625=CARTESIAN_POINT('Ctrl Pts',(-20.9009332523282,21.7152182888218,-69.9343531599254));
#8626=CARTESIAN_POINT('Ctrl Pts',(-20.8945641016132,21.7244479764672,-69.93366927389));
#8627=CARTESIAN_POINT('Ctrl Pts',(-20.8857655242585,21.7373416476576,-69.9327147443955));
#8628=CARTESIAN_POINT('Ctrl Pts',(-20.8832951755805,21.7409777193421,-69.9324456558294));
#8629=CARTESIAN_POINT('Ctrl Pts',(-20.879048351611,21.7472561565554,-69.9319811733108));
#8630=CARTESIAN_POINT('Ctrl Pts',(-20.8772683338622,21.7498961285093,-69.9317859137423));
#8631=CARTESIAN_POINT('Ctrl Pts',(-20.8735981520945,21.7553568733975,-69.9313821171932));
#8632=CARTESIAN_POINT('Ctrl Pts',(-20.8717085288561,21.7581780029079,-69.9311735601583));
#8633=CARTESIAN_POINT('Ctrl Pts',(-20.8673130978452,21.7647626828779,-69.9306868948891));
#8634=CARTESIAN_POINT('Ctrl Pts',(-20.8648107494876,21.7685285238932,-69.9304086567612));
#8635=CARTESIAN_POINT('Ctrl Pts',(-20.8569889518525,21.7803536361193,-69.9295352358262));
#8636=CARTESIAN_POINT('Ctrl Pts',(-20.8516978325178,21.7884315012388,-69.9289389904849));
#8637=CARTESIAN_POINT('Ctrl Pts',(-20.8008600368129,21.8668110272988,-69.9231572201251));
#8638=CARTESIAN_POINT('Ctrl Pts',(-20.7580380981302,21.9388336449791,-69.9178709842721));
#8639=CARTESIAN_POINT('Ctrl Pts',(-20.6848790194872,22.0735700180661,-69.9080153995873));
#8640=CARTESIAN_POINT('Ctrl Pts',(-20.6536752100424,22.1357577983018,-69.9034792300966));
#8641=CARTESIAN_POINT('Ctrl Pts',(-20.5400404612068,22.3817830441713,-69.8855972627026));
#8642=CARTESIAN_POINT('Ctrl Pts',(-20.4729092667373,22.5721706731769,-69.8718592193798));
#8643=CARTESIAN_POINT('Ctrl Pts',(-20.3874640202931,22.9134573920773,-69.8481565870541));
#8644=CARTESIAN_POINT('Ctrl Pts',(-20.3611892283964,23.0617582858008,-69.8381578137268));
#8645=CARTESIAN_POINT('Ctrl Pts',(-20.3443779686358,23.2207457145788,-69.8281030122695));
#8646=CARTESIAN_POINT('Ctrl Pts',(-20.3434276800245,23.2301262556892,-69.827512224363));
#8647=CARTESIAN_POINT('Ctrl Pts',(-20.3422068941983,23.2427282267751,-69.8267219794453));
#8648=CARTESIAN_POINT('Ctrl Pts',(-20.3419000689391,23.2459459669852,-69.8265205012553));
#8649=CARTESIAN_POINT('Ctrl Pts',(-20.3414269049889,23.2509884058773,-69.8262052456934));
#8650=CARTESIAN_POINT('Ctrl Pts',(-20.3412572815605,23.2528127827339,-69.8260912823823));
#8651=CARTESIAN_POINT('Ctrl Pts',(-20.3409344753468,23.2563171281779,-69.8258725651676));
#8652=CARTESIAN_POINT('Ctrl Pts',(-20.34078105677,23.257997061427,-69.8257677986879));
#8653=CARTESIAN_POINT('Ctrl Pts',(-20.340420840475,23.2619759209309,-69.82551985991));
#8654=CARTESIAN_POINT('Ctrl Pts',(-20.3402151936876,23.2642749469916,-69.825376753665));
#8655=CARTESIAN_POINT('Ctrl Pts',(-20.3396257815547,23.2709450183455,-69.8249620107601));
#8656=CARTESIAN_POINT('Ctrl Pts',(-20.3392484710037,23.2753166509965,-69.824690738884));
#8657=CARTESIAN_POINT('Ctrl Pts',(-20.3365877649467,23.3068971094282,-69.8227350031928));
#8658=CARTESIAN_POINT('Ctrl Pts',(-20.3346412192299,23.3341342740311,-69.8210692477161));
#8659=CARTESIAN_POINT('Ctrl Pts',(-20.3296538775864,23.4190937949285,-69.8159296134922));
#8660=CARTESIAN_POINT('Ctrl Pts',(-20.3278193857779,23.476878147688,-69.8125147198375));
#8661=CARTESIAN_POINT('Ctrl Pts',(-20.3264883972116,23.7523985662997,-69.7964858632678));
#8662=CARTESIAN_POINT('Ctrl Pts',(-20.3475008460763,23.9696751011115,-69.7845670812664));
#8663=CARTESIAN_POINT('Ctrl Pts',(-20.4305871968124,24.3844918948921,-69.7607722444885));
#8664=CARTESIAN_POINT('Ctrl Pts',(-20.4900437167122,24.5814508194212,-69.7489813346355));
#8665=CARTESIAN_POINT('Ctrl Pts',(-20.5725955817651,24.783068651061,-69.7357426286716));
#8666=CARTESIAN_POINT('Ctrl Pts',(-20.5774408797817,24.7947071796445,-69.7349742724588));
#8667=CARTESIAN_POINT('Ctrl Pts',(-20.5841552373398,24.810572235037,-69.7339211136233));
#8668=CARTESIAN_POINT('Ctrl Pts',(-20.5859653296447,24.814823722895,-69.7336383210512));
#8669=CARTESIAN_POINT('Ctrl Pts',(-20.5890619582041,24.822053804361,-69.7331564287968));
#8670=CARTESIAN_POINT('Ctrl Pts',(-20.5903438644285,24.8250343840177,-69.7329574874337));
#8671=CARTESIAN_POINT('Ctrl Pts',(-20.5928322858199,24.8307962611718,-69.7325723565989));
#8672=CARTESIAN_POINT('Ctrl Pts',(-20.5940382291064,24.833577802578,-69.7323861868843));
#8673=CARTESIAN_POINT('Ctrl Pts',(-20.596909589863,24.8401751512617,-69.7319440323076));
#8674=CARTESIAN_POINT('Ctrl Pts',(-20.5985784772506,24.8439894340826,-69.7316879287443));
#8675=CARTESIAN_POINT('Ctrl Pts',(-20.603438172643,24.8550380361116,-69.7309447185005));
#8676=CARTESIAN_POINT('Ctrl Pts',(-20.6066482016818,24.8622638219634,-69.7304569524115));
#8677=CARTESIAN_POINT('Ctrl Pts',(-20.6305953771663,24.9156387166601,-69.7268412073946));
#8678=CARTESIAN_POINT('Ctrl Pts',(-20.6523891177638,24.9613033804865,-69.7236769203354));
#8679=CARTESIAN_POINT('Ctrl Pts',(-20.7273626230876,25.1093269424432,-69.7131768208526));
#8680=CARTESIAN_POINT('Ctrl Pts',(-20.7849578018111,25.2093367382236,-69.7056892046097));
#8681=CARTESIAN_POINT('Ctrl Pts',(-20.9333841637604,25.4377918353639,-69.6876564650926));
#8682=CARTESIAN_POINT('Ctrl Pts',(-21.0285013279266,25.5631036187459,-69.6770040138043));
#8683=CARTESIAN_POINT('Ctrl Pts',(-21.2531133407459,25.8179875226884,-69.6540230220447));
#8684=CARTESIAN_POINT('Ctrl Pts',(-21.3853024261898,25.9445120998659,-69.6417424715827));
#8685=CARTESIAN_POINT('Ctrl Pts',(-21.5362479854762,26.0662074351165,-69.6295268339463));
#8686=CARTESIAN_POINT('Ctrl Pts',(-21.5450174463286,26.0732023230106,-69.6288231773924));
#8687=CARTESIAN_POINT('Ctrl Pts',(-21.5565434756871,26.0822979042653,-69.627906401276));
#8688=CARTESIAN_POINT('Ctrl Pts',(-21.5592670234869,26.0844400297183,-69.62769035684));
#8689=CARTESIAN_POINT('Ctrl Pts',(-21.5634729299505,26.0877370947517,-69.6273576338531));
#8690=CARTESIAN_POINT('Ctrl Pts',(-21.5649528420535,26.0888951288345,-69.6272407333328));
#8691=CARTESIAN_POINT('Ctrl Pts',(-21.5677570994235,26.0910855138363,-69.6270195497289));
#8692=CARTESIAN_POINT('Ctrl Pts',(-21.5690812319002,26.09211811882,-69.6269152486059));
#8693=CARTESIAN_POINT('Ctrl Pts',(-21.5721611450506,26.0945160745441,-69.6266729677339));
#8694=CARTESIAN_POINT('Ctrl Pts',(-21.5739175296328,26.0958806406464,-69.6265350446998));
#8695=CARTESIAN_POINT('Ctrl Pts',(-21.5775362330363,26.0986860724774,-69.6262513758983));
#8696=CARTESIAN_POINT('Ctrl Pts',(-21.5793987218562,26.10012671822,-69.6261056458687));
#8697=CARTESIAN_POINT('Ctrl Pts',(-21.588839034558,26.107412331672,-69.6253683462196));
#8698=CARTESIAN_POINT('Ctrl Pts',(-21.5964413942384,26.1132256478236,-69.624779010673));
#8699=CARTESIAN_POINT('Ctrl Pts',(-21.6158851787148,26.1279569851182,-69.6232826277794));
#8700=CARTESIAN_POINT('Ctrl Pts',(-21.6277625868296,26.136827436156,-69.6223787744855));
#8701=CARTESIAN_POINT('Ctrl Pts',(-21.6769670915504,26.1730488549657,-69.6186743800444));
#8702=CARTESIAN_POINT('Ctrl Pts',(-21.7148218037523,26.1996776426251,-69.6159185185576));
#8703=CARTESIAN_POINT('Ctrl Pts',(-21.804750299189,26.2600846643298,-69.6095552841573));
#8704=CARTESIAN_POINT('Ctrl Pts',(-21.8572529567166,26.2931928257681,-69.6059791495121));
#8705=CARTESIAN_POINT('Ctrl Pts',(-21.9645883187378,26.3566215932559,-69.5988755996711));
#8706=CARTESIAN_POINT('Ctrl Pts',(-22.0193969537009,26.3868905215353,-69.5953515269656));
#8707=CARTESIAN_POINT('Ctrl Pts',(-22.0750360905742,26.4155368132881,-69.5918437005959));
#8708=CARTESIAN_POINT('Origin',(-23.5502525316942,23.5502525316942,-77.3107734492734));
#8709=CARTESIAN_POINT('',(-22.0750358851076,26.4155367075019,-68.0965974740783));
#8710=CARTESIAN_POINT('',(-22.0750360157945,26.4155367747871,-68.3458849806668));
#8711=CARTESIAN_POINT('',(-22.0750360153461,26.4155367745563,-77.3107734492734));
#8712=CARTESIAN_POINT('',(-26.7730025010771,23.5498082993017,-68.9362096369654));
#8713=CARTESIAN_POINT('Ctrl Pts',(-22.0750358851076,26.4155367075019,-68.0965974740783));
#8714=CARTESIAN_POINT('Ctrl Pts',(-21.9058636254286,26.3284368883194,-68.1072292468121));
#8715=CARTESIAN_POINT('Ctrl Pts',(-21.7446756452602,26.2264947685448,-68.1178689864256));
#8716=CARTESIAN_POINT('Ctrl Pts',(-21.5250098919503,26.0586210667221,-68.1340512927263));
#8717=CARTESIAN_POINT('Ctrl Pts',(-21.4587723498944,26.0036642502873,-68.1391782460546));
#8718=CARTESIAN_POINT('Ctrl Pts',(-21.3873648520484,25.9394228739606,-68.1450261979675));
#8719=CARTESIAN_POINT('Ctrl Pts',(-21.379944287117,25.9326840961005,-68.1456379302412));
#8720=CARTESIAN_POINT('Ctrl Pts',(-21.3692469938658,25.9228781972286,-68.1465256858236));
#8721=CARTESIAN_POINT('Ctrl Pts',(-21.3659449931704,25.919838630914,-68.1468005351226));
#8722=CARTESIAN_POINT('Ctrl Pts',(-21.3602017462695,25.9145296368036,-68.1472800242483));
#8723=CARTESIAN_POINT('Ctrl Pts',(-21.3577576457835,25.912263295346,-68.1474845318119));
#8724=CARTESIAN_POINT('Ctrl Pts',(-21.3527443059223,25.9076000890446,-68.1479049578816));
#8725=CARTESIAN_POINT('Ctrl Pts',(-21.3501754625055,25.9052028067436,-68.1481208941756));
#8726=CARTESIAN_POINT('Ctrl Pts',(-21.3449707947261,25.9003297857386,-68.1485594349083));
#8727=CARTESIAN_POINT('Ctrl Pts',(-21.3423352070932,25.8978538025531,-68.1487820497302));
#8728=CARTESIAN_POINT('Ctrl Pts',(-21.3359776767361,25.8918610919549,-68.1493203545271));
#8729=CARTESIAN_POINT('Ctrl Pts',(-21.3322599461595,25.8883399280107,-68.1496362362988));
#8730=CARTESIAN_POINT('Ctrl Pts',(-21.3222314156805,25.8787961896121,-68.1504912982551));
#8731=CARTESIAN_POINT('Ctrl Pts',(-21.3159366848155,25.8727568598306,-68.1510312064061));
#8732=CARTESIAN_POINT('Ctrl Pts',(-21.1977632492247,25.7584531061814,-68.1612280009303));
#8733=CARTESIAN_POINT('Ctrl Pts',(-21.0938677304,25.6422650103483,-68.1712414689084));
#8734=CARTESIAN_POINT('Ctrl Pts',(-20.8357977984593,25.3078171295318,-68.1991767975091));
#8735=CARTESIAN_POINT('Ctrl Pts',(-20.6996870655115,25.0771961115418,-68.2176063925051));
#8736=CARTESIAN_POINT('Ctrl Pts',(-20.586043536998,24.8151394130983,-68.2364398246966));
#8737=CARTESIAN_POINT('Ctrl Pts',(-20.5786864800503,24.7977576478982,-68.2376791711917));
#8738=CARTESIAN_POINT('Ctrl Pts',(-20.5687076949423,24.773592549043,-68.23938767852));
#8739=CARTESIAN_POINT('Ctrl Pts',(-20.5659557016669,24.7668637447017,-68.2398618670843));
#8740=CARTESIAN_POINT('Ctrl Pts',(-20.5628863940264,24.7592860062701,-68.2403940995751));
#8741=CARTESIAN_POINT('Ctrl Pts',(-20.562546663013,24.7584462352803,-68.2404530574361));
#8742=CARTESIAN_POINT('Ctrl Pts',(-20.5610880273173,24.7548362996531,-68.2407063945501));
#8743=CARTESIAN_POINT('Ctrl Pts',(-20.5599726175589,24.7520647148134,-68.2409006301762));
#8744=CARTESIAN_POINT('Ctrl Pts',(-20.5568346564899,24.7442360539812,-68.2414485074656));
#8745=CARTESIAN_POINT('Ctrl Pts',(-20.5548210592668,24.7391753726937,-68.2418017733164));
#8746=CARTESIAN_POINT('Ctrl Pts',(-20.5519319034874,24.7318602591712,-68.2423110919702));
#8747=CARTESIAN_POINT('Ctrl Pts',(-20.5510460485315,24.7296099340909,-68.2424675919954));
#8748=CARTESIAN_POINT('Ctrl Pts',(-20.5333523014502,24.6845138876407,-68.2456001856944));
#8749=CARTESIAN_POINT('Ctrl Pts',(-20.51746050167,24.6413111342092,-68.2485356299763));
#8750=CARTESIAN_POINT('Ctrl Pts',(-20.5008775199454,24.5930633849036,-68.2517301857399));
#8751=CARTESIAN_POINT('Ctrl Pts',(-20.4992673076188,24.5883428943877,-68.2520418563191));
#8752=CARTESIAN_POINT('Ctrl Pts',(-20.4968778044284,24.5812842534532,-68.2525065690145));
#8753=CARTESIAN_POINT('Ctrl Pts',(-20.4960902362059,24.5789489442941,-68.2526600985484));
#8754=CARTESIAN_POINT('Ctrl Pts',(-20.4947395977771,24.5749287873382,-68.252924016909));
#8755=CARTESIAN_POINT('Ctrl Pts',(-20.4941752419335,24.5732443778296,-68.2530344823545));
#8756=CARTESIAN_POINT('Ctrl Pts',(-20.4930108308903,24.5697594454971,-68.2532627911486));
#8757=CARTESIAN_POINT('Ctrl Pts',(-20.4924109745079,24.567958862413,-68.2533806220496));
#8758=CARTESIAN_POINT('Ctrl Pts',(-20.4910038265747,24.5637225643674,-68.2536575413108));
#8759=CARTESIAN_POINT('Ctrl Pts',(-20.4901978506868,24.5612864066244,-68.253816551057));
#8760=CARTESIAN_POINT('Ctrl Pts',(-20.4875792069138,24.5533394286967,-68.2543344895819));
#8761=CARTESIAN_POINT('Ctrl Pts',(-20.4857784959072,24.5478246355987,-68.254692711441));
#8762=CARTESIAN_POINT('Ctrl Pts',(-20.4186855997601,24.3404522742705,-68.2681188838046));
#8763=CARTESIAN_POINT('Ctrl Pts',(-20.3734578409923,24.1326053723328,-68.280027200704));
#8764=CARTESIAN_POINT('Ctrl Pts',(-20.3258451910703,23.7223625712184,-68.3031225818594));
#8765=CARTESIAN_POINT('Ctrl Pts',(-20.3213866639944,23.5212244485327,-68.3142748694118));
#8766=CARTESIAN_POINT('Ctrl Pts',(-20.3425413127634,23.2246130715782,-68.3316004063359));
#8767=CARTESIAN_POINT('Ctrl Pts',(-20.3537442694885,23.1286076444589,-68.3373402087703));
#8768=CARTESIAN_POINT('Ctrl Pts',(-20.3707324812254,23.0240812403174,-68.3437862229456));
#8769=CARTESIAN_POINT('Ctrl Pts',(-20.3722634424237,23.0149121494745,-68.3443533225711));
#8770=CARTESIAN_POINT('Ctrl Pts',(-20.3745964408629,23.0013023361239,-68.345197576675));
#8771=CARTESIAN_POINT('Ctrl Pts',(-20.3753681782888,22.9968564108051,-68.3454737664673));
#8772=CARTESIAN_POINT('Ctrl Pts',(-20.3767057401221,22.9892457044706,-68.345947243892));
#8773=CARTESIAN_POINT('Ctrl Pts',(-20.3772669690588,22.9860801132935,-68.3461443848693));
#8774=CARTESIAN_POINT('Ctrl Pts',(-20.3784154786972,22.9796579101137,-68.3465447498011));
#8775=CARTESIAN_POINT('Ctrl Pts',(-20.3790030401019,22.9764013533479,-68.3467479824616));
#8776=CARTESIAN_POINT('Ctrl Pts',(-20.3803640400305,22.9689239440949,-68.3472151267567));
#8777=CARTESIAN_POINT('Ctrl Pts',(-20.3811408938465,22.9647037267973,-68.3474791471202));
#8778=CARTESIAN_POINT('Ctrl Pts',(-20.3827875023543,22.9558578788056,-68.3480333238869));
#8779=CARTESIAN_POINT('Ctrl Pts',(-20.3836589656437,22.9512325799867,-68.3483235343973));
#8780=CARTESIAN_POINT('Ctrl Pts',(-20.3859874236818,22.9390213495532,-68.3490908981324));
#8781=CARTESIAN_POINT('Ctrl Pts',(-20.3874615589543,22.931438752846,-68.3495685989714));
#8782=CARTESIAN_POINT('Ctrl Pts',(-20.3919605925668,22.9087328881181,-68.3510027082182));
#8783=CARTESIAN_POINT('Ctrl Pts',(-20.3950667726421,22.893626124683,-68.3519617135873));
#8784=CARTESIAN_POINT('Ctrl Pts',(-20.4064383043499,22.8402656905905,-68.3553666407485));
#8785=CARTESIAN_POINT('Ctrl Pts',(-20.4152916358423,22.8021421288071,-68.3578312748854));
#8786=CARTESIAN_POINT('Ctrl Pts',(-20.4457042291217,22.6812203666782,-68.365753694121));
#8787=CARTESIAN_POINT('Ctrl Pts',(-20.4698656914929,22.5991206390235,-68.3712919623326));
#8788=CARTESIAN_POINT('Ctrl Pts',(-20.5499603288698,22.3622132927529,-68.3877335317863));
#8789=CARTESIAN_POINT('Ctrl Pts',(-20.6145137805871,22.2106182357555,-68.3988578573489));
#8790=CARTESIAN_POINT('Ctrl Pts',(-20.7666508900472,21.917746735208,-68.4211959001607));
#8791=CARTESIAN_POINT('Ctrl Pts',(-20.8541601935616,21.7769478307404,-68.4323745731446));
#8792=CARTESIAN_POINT('Ctrl Pts',(-20.974937338046,21.6123778985137,-68.4455118522025));
#8793=CARTESIAN_POINT('Ctrl Pts',(-20.9983251876517,21.5816810694138,-68.4479649473576));
#8794=CARTESIAN_POINT('Ctrl Pts',(-21.0252042376177,21.5476863756114,-68.4506776774405));
#8795=CARTESIAN_POINT('Ctrl Pts',(-21.0281567360848,21.5439691779872,-68.4509742509853));
#8796=CARTESIAN_POINT('Ctrl Pts',(-21.0326167201244,21.5383794588241,-68.4514201233923));
#8797=CARTESIAN_POINT('Ctrl Pts',(-21.0341180887413,21.5365020987663,-68.4515698570223));
#8798=CARTESIAN_POINT('Ctrl Pts',(-21.0367226814265,21.533252691861,-68.4518289899099));
#8799=CARTESIAN_POINT('Ctrl Pts',(-21.0378249290585,21.5318798694678,-68.4519384595416));
#8800=CARTESIAN_POINT('Ctrl Pts',(-21.0401246031371,21.5290204845374,-68.4521664466848));
#8801=CARTESIAN_POINT('Ctrl Pts',(-21.0413222241621,21.5275340841239,-68.4522849492619));
#8802=CARTESIAN_POINT('Ctrl Pts',(-21.0441724463008,21.524003020946,-68.4525664341196));
#8803=CARTESIAN_POINT('Ctrl Pts',(-21.0458262349608,21.5219593086712,-68.4527293302929));
#8804=CARTESIAN_POINT('Ctrl Pts',(-21.0513605804057,21.5151371860563,-68.4532730299902));
#8805=CARTESIAN_POINT('Ctrl Pts',(-21.0552523573808,21.5103678325207,-68.4536530250435));
#8806=CARTESIAN_POINT('Ctrl Pts',(-21.1643257927368,21.3774779982382,-68.4642389047057));
#8807=CARTESIAN_POINT('Ctrl Pts',(-21.2792406652269,21.2576299934558,-68.4737381390724));
#8808=CARTESIAN_POINT('Ctrl Pts',(-21.503742417469,21.05702005893,-68.4906942176977));
#8809=CARTESIAN_POINT('Ctrl Pts',(-21.6101728185252,20.9733351545359,-68.4981885093841));
#8810=CARTESIAN_POINT('Ctrl Pts',(-21.8898580130681,20.7805974719578,-68.517296381042));
#8811=CARTESIAN_POINT('Ctrl Pts',(-22.06879364077,20.6809042414171,-68.5290393120136));
#8812=CARTESIAN_POINT('Ctrl Pts',(-22.2674753949123,20.5937750939409,-68.5422224733009));
#8813=CARTESIAN_POINT('Ctrl Pts',(-22.2790330690148,20.5887871692002,-68.5429896914775));
#8814=CARTESIAN_POINT('Ctrl Pts',(-22.2948699439409,20.5820622675187,-68.5440415195785));
#8815=CARTESIAN_POINT('Ctrl Pts',(-22.2991242025228,20.5802665402181,-68.5443241259523));
#8816=CARTESIAN_POINT('Ctrl Pts',(-22.3063732979,20.5772250284158,-68.544805773771));
#8817=CARTESIAN_POINT('Ctrl Pts',(-22.3093661920335,20.5759746066437,-68.5450046572192));
#8818=CARTESIAN_POINT('Ctrl Pts',(-22.3154090021421,20.5734606480455,-68.5454062723513));
#8819=CARTESIAN_POINT('Ctrl Pts',(-22.3184589811948,20.5721972753473,-68.5456090092766));
#8820=CARTESIAN_POINT('Ctrl Pts',(-22.3254077356022,20.5693314397561,-68.5460709754418));
#8821=CARTESIAN_POINT('Ctrl Pts',(-22.3293077184872,20.5677319376818,-68.5463303047418));
#8822=CARTESIAN_POINT('Ctrl Pts',(-22.3374715151494,20.5644024112861,-68.5468732679235));
#8823=CARTESIAN_POINT('Ctrl Pts',(-22.3417359156785,20.5626738592416,-68.5471569510526));
#8824=CARTESIAN_POINT('Ctrl Pts',(-22.3529355154231,20.5581620637123,-68.5479021623777));
#8825=CARTESIAN_POINT('Ctrl Pts',(-22.3598766890141,20.5553938108705,-68.548364196654));
#8826=CARTESIAN_POINT('Ctrl Pts',(-22.3805403578621,20.5472359903918,-68.5497402114108));
#8827=CARTESIAN_POINT('Ctrl Pts',(-22.3942901341515,20.5419164732122,-68.5506565461458));
#8828=CARTESIAN_POINT('Ctrl Pts',(-22.4425200121628,20.5236367544383,-68.5538735445131));
#8829=CARTESIAN_POINT('Ctrl Pts',(-22.4771843559801,20.5111739037259,-68.5561907015506));
#8830=CARTESIAN_POINT('Ctrl Pts',(-22.6398817883655,20.4558099594653,-68.5670930000249));
#8831=CARTESIAN_POINT('Ctrl Pts',(-22.7703015498735,20.4203933879633,-68.5759170084932));
#8832=CARTESIAN_POINT('Ctrl Pts',(-23.2052705149168,20.3311523784487,-68.6055192030266));
#8833=CARTESIAN_POINT('Ctrl Pts',(-23.5153440177527,20.3129078258319,-68.6270450846501));
#8834=CARTESIAN_POINT('Ctrl Pts',(-23.8394162639224,20.340460546158,-68.6476283576837));
#8835=CARTESIAN_POINT('Ctrl Pts',(-23.8555555941309,20.3419554256334,-68.648647921971));
#8836=CARTESIAN_POINT('Ctrl Pts',(-23.8752514992914,20.3439297012358,-68.6498848579311));
#8837=CARTESIAN_POINT('Ctrl Pts',(-23.8788190629481,20.3442933215815,-68.650108613836));
#8838=CARTESIAN_POINT('Ctrl Pts',(-23.884698784567,20.3449025238657,-68.650476895652));
#8839=CARTESIAN_POINT('Ctrl Pts',(-23.8870112839392,20.3451446533843,-68.6506216158127));
#8840=CARTESIAN_POINT('Ctrl Pts',(-23.8911800749013,20.3455857068698,-68.6508822772995));
#8841=CARTESIAN_POINT('Ctrl Pts',(-23.8930364512133,20.3457837407047,-68.6509982688233));
#8842=CARTESIAN_POINT('Ctrl Pts',(-23.8970276598182,20.3462130213372,-68.6512474741189));
#8843=CARTESIAN_POINT('Ctrl Pts',(-23.8991624274529,20.3464447880678,-68.6513806576683));
#8844=CARTESIAN_POINT('Ctrl Pts',(-23.9050075792497,20.3470852939922,-68.6517450315093));
#8845=CARTESIAN_POINT('Ctrl Pts',(-23.9087175022022,20.3474983479163,-68.6519759770003));
#8846=CARTESIAN_POINT('Ctrl Pts',(-23.9279704133344,20.3496757928681,-68.6531728476588));
#8847=CARTESIAN_POINT('Ctrl Pts',(-23.9435014714727,20.3515469256761,-68.6541328055749));
#8848=CARTESIAN_POINT('Ctrl Pts',(-24.0947402592146,20.3708858937837,-68.6634320301399));
#8849=CARTESIAN_POINT('Ctrl Pts',(-24.2292376413564,20.396868924638,-68.6713217829587));
#8850=CARTESIAN_POINT('Ctrl Pts',(-24.4935588054859,20.4656363564986,-68.6867741515009));
#8851=CARTESIAN_POINT('Ctrl Pts',(-24.623120246657,20.5082729018273,-68.6943245275661));
#8852=CARTESIAN_POINT('Ctrl Pts',(-24.8248664953339,20.5891626547212,-68.7065177793488));
#8853=CARTESIAN_POINT('Ctrl Pts',(-24.8989685371041,20.6221715338371,-68.7110943476401));
#8854=CARTESIAN_POINT('Ctrl Pts',(-25.0987337267806,20.7203505797276,-68.7238389289412));
#8855=CARTESIAN_POINT('Ctrl Pts',(-25.2214590024225,20.7910497539876,-68.7321352727002));
#8856=CARTESIAN_POINT('Ctrl Pts',(-25.3483324759706,20.875715486634,-68.7414135918751));
#8857=CARTESIAN_POINT('Ctrl Pts',(-25.3575006022925,20.8819020491041,-68.7420881477478));
#8858=CARTESIAN_POINT('Ctrl Pts',(-25.3702462124476,20.8905984828731,-68.743031709413));
#8859=CARTESIAN_POINT('Ctrl Pts',(-25.3738507857663,20.8930686718847,-68.7432992070227));
#8860=CARTESIAN_POINT('Ctrl Pts',(-25.3800673735743,20.8973474635477,-68.7437616725831));
#8861=CARTESIAN_POINT('Ctrl Pts',(-25.3826817650288,20.8991526163998,-68.7439565088454));
#8862=CARTESIAN_POINT('Ctrl Pts',(-25.3880320204405,20.9028584901966,-68.7443559456217));
#8863=CARTESIAN_POINT('Ctrl Pts',(-25.3907676139811,20.9047595923806,-68.7445605605388));
#8864=CARTESIAN_POINT('Ctrl Pts',(-25.3971215476363,20.909189887663,-68.7450367099658));
#8865=CARTESIAN_POINT('Ctrl Pts',(-25.4007376418388,20.9117222763119,-68.7453083667574));
#8866=CARTESIAN_POINT('Ctrl Pts',(-25.4083378075222,20.9170680606944,-68.745880752323));
#8867=CARTESIAN_POINT('Ctrl Pts',(-25.412320715415,20.9198830843885,-68.7461815433369));
#8868=CARTESIAN_POINT('Ctrl Pts',(-25.4229293130872,20.9274171567157,-68.746984934149));
#8869=CARTESIAN_POINT('Ctrl Pts',(-25.4295435199946,20.9321522450075,-68.7474881525465));
#8870=CARTESIAN_POINT('Ctrl Pts',(-25.4495553366796,20.9465935440393,-68.7490177915468));
#8871=CARTESIAN_POINT('Ctrl Pts',(-25.4628960384992,20.9563778106588,-68.7500472358163));
#8872=CARTESIAN_POINT('Ctrl Pts',(-25.7200367833645,21.148030937166,-68.77008120539));
#8873=CARTESIAN_POINT('Ctrl Pts',(-25.9369016867115,21.3633708285556,-68.7905582849646));
#8874=CARTESIAN_POINT('Ctrl Pts',(-26.2033160982451,21.7155075814947,-68.8204211139728));
#8875=CARTESIAN_POINT('Ctrl Pts',(-26.2792015973723,21.8304040920889,-68.8296738478804));
#8876=CARTESIAN_POINT('Ctrl Pts',(-26.35241433982,21.9583656029755,-68.8392272503183));
#8877=CARTESIAN_POINT('Ctrl Pts',(-26.3572719241504,21.9669468354047,-68.8398644128024));
#8878=CARTESIAN_POINT('Ctrl Pts',(-26.3816676333692,22.0105085779592,-68.8430807304864));
#8879=CARTESIAN_POINT('Ctrl Pts',(-26.4005926756583,22.0458309307211,-68.8456296287692));
#8880=CARTESIAN_POINT('Ctrl Pts',(-26.4212837676865,22.0862424214369,-68.8484717083514));
#8881=CARTESIAN_POINT('Ctrl Pts',(-26.4237006969254,22.0909918957284,-68.8488045865178));
#8882=CARTESIAN_POINT('Ctrl Pts',(-26.427212286108,22.0979350237288,-68.8492895179026));
#8883=CARTESIAN_POINT('Ctrl Pts',(-26.4283162251884,22.1001239343809,-68.8494421535204));
#8884=CARTESIAN_POINT('Ctrl Pts',(-26.4302652229485,22.1039994351109,-68.8497119606848));
#8885=CARTESIAN_POINT('Ctrl Pts',(-26.4311112989708,22.1056855085893,-68.8498291967788));
#8886=CARTESIAN_POINT('Ctrl Pts',(-26.4328740508249,22.1092060558736,-68.8500736817176));
#8887=CARTESIAN_POINT('Ctrl Pts',(-26.4337904542976,22.1110406581345,-68.8502009131364));
#8888=CARTESIAN_POINT('Ctrl Pts',(-26.4361773434937,22.1158305438829,-68.8505326487636));
#8889=CARTESIAN_POINT('Ctrl Pts',(-26.4376450458078,22.1187872236447,-68.8507369769917));
#8890=CARTESIAN_POINT('Ctrl Pts',(-26.4439862228812,22.1316109294938,-68.8516212882347));
#8891=CARTESIAN_POINT('Ctrl Pts',(-26.4488137577405,22.1415007799124,-68.8522984124451));
#8892=CARTESIAN_POINT('Ctrl Pts',(-26.4833267153623,22.2131336936917,-68.8571691534399));
#8893=CARTESIAN_POINT('Ctrl Pts',(-26.5110898137452,22.2757898494736,-68.8612491846057));
#8894=CARTESIAN_POINT('Ctrl Pts',(-26.6927522813078,22.7238215175353,-68.8894944968044));
#8895=CARTESIAN_POINT('Ctrl Pts',(-26.7729452984221,23.1348231300911,-68.9111907440968));
#8896=CARTESIAN_POINT('Ctrl Pts',(-26.7730025010771,23.5498082993017,-68.9362096369654));
#8897=CARTESIAN_POINT('Ctrl Pts',(-26.7730025012977,23.5498099025822,-68.936209733625));
#8898=CARTESIAN_POINT('Ctrl Pts',(-26.7730047857272,23.5664426653496,-68.9372125005807));
#8899=CARTESIAN_POINT('Ctrl Pts',(-26.772878306465,23.58307501592,-68.9382191818676));
#8900=CARTESIAN_POINT('Ctrl Pts',(-26.7724443818348,23.6113496939998,-68.9399375387905));
#8901=CARTESIAN_POINT('Ctrl Pts',(-26.7722025683611,23.6229927406453,-68.9406471532271));
#8902=CARTESIAN_POINT('Ctrl Pts',(-26.7717888541505,23.6387881371692,-68.9416126668269));
#8903=CARTESIAN_POINT('Ctrl Pts',(-26.7716720174634,23.6429419420569,-68.9418668383947));
#8904=CARTESIAN_POINT('Ctrl Pts',(-26.7714493519704,23.6503484808087,-68.9423205218401));
#8905=CARTESIAN_POINT('Ctrl Pts',(-26.7713466290917,23.6536013080502,-68.942519936029));
#8906=CARTESIAN_POINT('Ctrl Pts',(-26.7711312513569,23.6601089951004,-68.9429192195149));
#8907=CARTESIAN_POINT('Ctrl Pts',(-26.7710185894345,23.6633638508018,-68.9431190888013));
#8908=CARTESIAN_POINT('Ctrl Pts',(-26.7707837590673,23.6698632246213,-68.9435185251654));
#8909=CARTESIAN_POINT('Ctrl Pts',(-26.7706616209194,23.6731077402234,-68.9437180910701));
#8910=CARTESIAN_POINT('Ctrl Pts',(-26.7703162116814,23.6819286709191,-68.9442611079359));
#8911=CARTESIAN_POINT('Ctrl Pts',(-26.7700833589032,23.6875046804617,-68.9446048596047));
#8912=CARTESIAN_POINT('Ctrl Pts',(-26.7691540744085,23.7084523906252,-68.9458981199291));
#8913=CARTESIAN_POINT('Ctrl Pts',(-26.7683620463268,23.723819451571,-68.9468506280402));
#8914=CARTESIAN_POINT('Ctrl Pts',(-26.7662646518848,23.7595355479009,-68.9490734664427));
#8915=CARTESIAN_POINT('Ctrl Pts',(-26.7648761573847,23.7798788637678,-68.9503463773295));
#8916=CARTESIAN_POINT('Ctrl Pts',(-26.7353843105202,24.1589817036011,-68.9741978283998));
#8917=CARTESIAN_POINT('Ctrl Pts',(-26.6475757806062,24.5104963231395,-68.9989194497197));
#8918=CARTESIAN_POINT('Ctrl Pts',(-26.4844888954227,24.8839168194867,-69.0261657804982));
#8919=CARTESIAN_POINT('Ctrl Pts',(-26.4643798809675,24.9273021383577,-69.0293406201353));
#8920=CARTESIAN_POINT('Ctrl Pts',(-26.4133699584253,25.0312299947696,-69.0369436560686));
#8921=CARTESIAN_POINT('Ctrl Pts',(-26.3815029812796,25.0912775542513,-69.0413348146074));
#8922=CARTESIAN_POINT('Ctrl Pts',(-26.3423214543282,25.159783088812,-69.0463045707472));
#8923=CARTESIAN_POINT('Ctrl Pts',(-26.3368361010281,25.1692613341405,-69.0469912584852));
#8924=CARTESIAN_POINT('Ctrl Pts',(-26.329637524234,25.1815549200339,-69.0478805348423));
#8925=CARTESIAN_POINT('Ctrl Pts',(-26.3279682322108,25.1843957036023,-69.0480859312124));
#8926=CARTESIAN_POINT('Ctrl Pts',(-26.3252535946822,25.1889992671449,-69.0484186186806));
#8927=CARTESIAN_POINT('Ctrl Pts',(-26.3242109246451,25.1907636096113,-69.0485460842482));
#8928=CARTESIAN_POINT('Ctrl Pts',(-26.322205030417,25.1941504809885,-69.048790693558));
#8929=CARTESIAN_POINT('Ctrl Pts',(-26.3212420670504,25.1957731538166,-69.0489078535295));
#8930=CARTESIAN_POINT('Ctrl Pts',(-26.3190232345048,25.1995045991043,-69.0491771942288));
#8931=CARTESIAN_POINT('Ctrl Pts',(-26.3177663779144,25.2016127884749,-69.0493293099522));
#8932=CARTESIAN_POINT('Ctrl Pts',(-26.3137651341339,25.2083068796249,-69.049812148015));
#8933=CARTESIAN_POINT('Ctrl Pts',(-26.311011729127,25.2128874222515,-69.0501422812382));
#8934=CARTESIAN_POINT('Ctrl Pts',(-26.2873084037128,25.2520988552947,-69.0529663493015));
#8935=CARTESIAN_POINT('Ctrl Pts',(-26.2657180274317,25.2863410285963,-69.0554190226764));
#8936=CARTESIAN_POINT('Ctrl Pts',(-26.2376568933535,25.3290408991718,-69.0584722976328));
#8937=CARTESIAN_POINT('Ctrl Pts',(-26.2317828376824,25.3378837808995,-69.0591043250443));
#8938=CARTESIAN_POINT('Ctrl Pts',(-26.2240361610296,25.349421626437,-69.0599288163941));
#8939=CARTESIAN_POINT('Ctrl Pts',(-26.222203036043,25.3521428808695,-69.0601232652824));
#8940=CARTESIAN_POINT('Ctrl Pts',(-26.2187551941726,25.3572443344973,-69.0604877811128));
#8941=CARTESIAN_POINT('Ctrl Pts',(-26.2171414421803,25.3596251782998,-69.0606578955518));
#8942=CARTESIAN_POINT('Ctrl Pts',(-26.0677040316585,25.5794629306854,-69.0763654654895));
#8943=CARTESIAN_POINT('Ctrl Pts',(-25.8938104024267,25.7780376692195,-69.0906110560752));
#8944=CARTESIAN_POINT('Ctrl Pts',(-25.5954822153969,26.0446353437266,-69.1132057281776));
#8945=CARTESIAN_POINT('Ctrl Pts',(-25.4875506000165,26.1293571049431,-69.1210744989442));
#8946=CARTESIAN_POINT('Ctrl Pts',(-25.3439069814071,26.2279948667579,-69.1314210853924));
#8947=CARTESIAN_POINT('Ctrl Pts',(-25.3128921676622,26.24851153353,-69.1336475276948));
#8948=CARTESIAN_POINT('Ctrl Pts',(-25.269007453273,26.2764622663053,-69.1367908814048));
#8949=CARTESIAN_POINT('Ctrl Pts',(-25.256429878296,26.2843514414055,-69.1376909897331));
#8950=CARTESIAN_POINT('Ctrl Pts',(-25.2374075927188,26.2961006313164,-69.1390513196822));
#8951=CARTESIAN_POINT('Ctrl Pts',(-25.2310030480904,26.3000255561954,-69.1395091562692));
#8952=CARTESIAN_POINT('Ctrl Pts',(-25.2206393462675,26.306327054413,-69.1402497722269));
#8953=CARTESIAN_POINT('Ctrl Pts',(-25.2166886749389,26.3087175877024,-69.1405320396322));
#8954=CARTESIAN_POINT('Ctrl Pts',(-25.2091127943546,26.3132795037896,-69.1410732175398));
#8955=CARTESIAN_POINT('Ctrl Pts',(-25.2054884228306,26.315452264803,-69.1413320769522));
#8956=CARTESIAN_POINT('Ctrl Pts',(-25.1990235922908,26.3193105775899,-69.1417937314407));
#8957=CARTESIAN_POINT('Ctrl Pts',(-25.1961847904749,26.3209989060804,-69.1419964247152));
#8958=CARTESIAN_POINT('Ctrl Pts',(-25.1905571631761,26.3243341397778,-69.1423981937817));
#8959=CARTESIAN_POINT('Ctrl Pts',(-25.1877684400636,26.3259812111722,-69.1425972632179));
#8960=CARTESIAN_POINT('Ctrl Pts',(-25.1810127965991,26.3299574949305,-69.1430794511156));
#8961=CARTESIAN_POINT('Ctrl Pts',(-25.1770433707906,26.3322824182561,-69.14336272528));
#8962=CARTESIAN_POINT('Ctrl Pts',(-25.1622908936194,26.3408806888472,-69.1444153619796));
#8963=CARTESIAN_POINT('Ctrl Pts',(-25.151476530137,26.3470998445792,-69.1451866869078));
#8964=CARTESIAN_POINT('Ctrl Pts',(-24.9649559844927,26.4529282590483,-69.1584856072429));
#8965=CARTESIAN_POINT('Ctrl Pts',(-24.7803397180759,26.5358462630855,-69.1716245620863));
#8966=CARTESIAN_POINT('Ctrl Pts',(-24.496742596601,26.6324297467823,-69.1916844879187));
#8967=CARTESIAN_POINT('Ctrl Pts',(-24.4028920249507,26.6597001777809,-69.1982960438932));
#8968=CARTESIAN_POINT('Ctrl Pts',(-24.2788949017737,26.6896938055823,-69.2069313823461));
#8969=CARTESIAN_POINT('Ctrl Pts',(-24.2497423287454,26.6963175745166,-69.2089543340347));
#8970=CARTESIAN_POINT('Ctrl Pts',(-24.127174113375,26.722378453355,-69.2174211347823));
#8971=CARTESIAN_POINT('Ctrl Pts',(-24.0330060972836,26.7380687610298,-69.2238343968652));
#8972=CARTESIAN_POINT('Ctrl Pts',(-23.8826539866267,26.7563040246646,-69.2338096230969));
#8973=CARTESIAN_POINT('Ctrl Pts',(-23.8268615332397,26.7615988515387,-69.2374537281834));
#8974=CARTESIAN_POINT('Ctrl Pts',(-23.743803416906,26.7673003010701,-69.242766835119));
#8975=CARTESIAN_POINT('Ctrl Pts',(-23.7166272603371,26.7688202047084,-69.244487504083));
#8976=CARTESIAN_POINT('Ctrl Pts',(-23.6850418372695,26.7701855640726,-69.2464642176118));
#8977=CARTESIAN_POINT('Ctrl Pts',(-23.6806492301382,26.7703664414001,-69.2467386012553));
#8978=CARTESIAN_POINT('Ctrl Pts',(-23.6739669273225,26.7706279072942,-69.2471552064107));
#8979=CARTESIAN_POINT('Ctrl Pts',(-23.6716775155677,26.7707150427051,-69.247297795218));
#8980=CARTESIAN_POINT('Ctrl Pts',(-23.6675245464164,26.770868670617,-69.2475561870839));
#8981=CARTESIAN_POINT('Ctrl Pts',(-23.6656610302617,26.7709359868383,-69.2476720362983));
#8982=CARTESIAN_POINT('Ctrl Pts',(-23.6616254011732,26.7710782596815,-69.2479227109524));
#8983=CARTESIAN_POINT('Ctrl Pts',(-23.6594532765641,26.771152636247,-69.2480575029532));
#8984=CARTESIAN_POINT('Ctrl Pts',(-23.6535334272755,26.7713493448072,-69.2484245101867));
#8985=CARTESIAN_POINT('Ctrl Pts',(-23.6497855468011,26.7714673339204,-69.2486564803599));
#8986=CARTESIAN_POINT('Ctrl Pts',(-23.6318357024983,26.7720010657349,-69.2497656619702));
#8987=CARTESIAN_POINT('Ctrl Pts',(-23.6176310121315,26.7723294377139,-69.2506380202415));
#8988=CARTESIAN_POINT('Ctrl Pts',(-23.5942080303515,26.7727159433589,-69.252068288187));
#8989=CARTESIAN_POINT('Ctrl Pts',(-23.5849910218605,26.7728284838172,-69.2526290054951));
#8990=CARTESIAN_POINT('Ctrl Pts',(-23.5707753235361,26.7729410616666,-69.2534907581141));
#8991=CARTESIAN_POINT('Ctrl Pts',(-23.5657769920613,26.7729690159653,-69.2537931724743));
#8992=CARTESIAN_POINT('Ctrl Pts',(-23.5565209192551,26.7729992480387,-69.2543521460652));
#8993=CARTESIAN_POINT('Ctrl Pts',(-23.5522632081041,26.7730047170143,-69.2546088586567));
#8994=CARTESIAN_POINT('Ctrl Pts',(-23.2600292273571,26.772800957288,-69.2722012879213));
#8995=CARTESIAN_POINT('Ctrl Pts',(-22.9733344466731,26.7340030985608,-69.2877244865341));
#8996=CARTESIAN_POINT('Ctrl Pts',(-22.5776010697416,26.625157151951,-69.3108910344547));
#8997=CARTESIAN_POINT('Ctrl Pts',(-22.461576891171,26.5860177755781,-69.3178958131221));
#8998=CARTESIAN_POINT('Ctrl Pts',(-22.3032582707111,26.5223654272652,-69.3279515706952));
#8999=CARTESIAN_POINT('Ctrl Pts',(-22.2588638310277,26.5033466058835,-69.3308274326826));
#9000=CARTESIAN_POINT('Ctrl Pts',(-22.198504047799,26.4758667824886,-69.3348232483214));
#9001=CARTESIAN_POINT('Ctrl Pts',(-22.1821562272589,26.468257876046,-69.3359142481335));
#9002=CARTESIAN_POINT('Ctrl Pts',(-22.1580452288087,26.4567885343138,-69.3375367370518));
#9003=CARTESIAN_POINT('Ctrl Pts',(-22.1502322029151,26.453033230514,-69.3380645944178));
#9004=CARTESIAN_POINT('Ctrl Pts',(-22.1378485580156,26.4470194481036,-69.3389046270686));
#9005=CARTESIAN_POINT('Ctrl Pts',(-22.133267945313,26.4447815494024,-69.3392160858091));
#9006=CARTESIAN_POINT('Ctrl Pts',(-22.124588497545,26.4405155885311,-69.3398076538194));
#9007=CARTESIAN_POINT('Ctrl Pts',(-22.1204886276497,26.4384896504801,-69.3400876883751));
#9008=CARTESIAN_POINT('Ctrl Pts',(-22.1133852226176,26.4349606935177,-69.3405739186372));
#9009=CARTESIAN_POINT('Ctrl Pts',(-22.110379691644,26.4334616894092,-69.3407799732988));
#9010=CARTESIAN_POINT('Ctrl Pts',(-22.1045714964856,26.4305535138229,-69.3411788060404));
#9011=CARTESIAN_POINT('Ctrl Pts',(-22.1017685344648,26.4291449424779,-69.3413715628621));
#9012=CARTESIAN_POINT('Ctrl Pts',(-22.0952060469638,26.4258350881028,-69.341823529226));
#9013=CARTESIAN_POINT('Ctrl Pts',(-22.0914481903326,26.4239305242344,-69.342082854101));
#9014=CARTESIAN_POINT('Ctrl Pts',(-22.0834699473044,26.4198672940224,-69.3426345265533));
#9015=CARTESIAN_POINT('Ctrl Pts',(-22.0792505779957,26.4177066787971,-69.3429269421883));
#9016=CARTESIAN_POINT('Ctrl Pts',(-22.075036015343,26.4155367745547,-69.3432196869019));
#9017=CARTESIAN_POINT('',(-26.7730011432084,23.5532287591033,-69.1857955693508));
#9018=CARTESIAN_POINT('Ctrl Pts',(-22.0750360905742,26.4155368132881,-69.5918437005959));
#9019=CARTESIAN_POINT('Ctrl Pts',(-22.1526654206688,26.455504946574,-69.5869494799723));
#9020=CARTESIAN_POINT('Ctrl Pts',(-22.2319114232218,26.4923143489673,-69.5820862962769));
#9021=CARTESIAN_POINT('Ctrl Pts',(-22.44915197364,26.5826729369313,-69.5689009104334));
#9022=CARTESIAN_POINT('Ctrl Pts',(-22.5894619030909,26.630004415548,-69.5605298696121));
#9023=CARTESIAN_POINT('Ctrl Pts',(-22.7520381357013,26.6726520380195,-69.5506819137278));
#9024=CARTESIAN_POINT('Ctrl Pts',(-22.7716075670712,26.6775895607603,-69.5494943265321));
#9025=CARTESIAN_POINT('Ctrl Pts',(-22.7959524371243,26.6834892963067,-69.548013626738));
#9026=CARTESIAN_POINT('Ctrl Pts',(-22.8006856549551,26.6846249972324,-69.5477255891229));
#9027=CARTESIAN_POINT('Ctrl Pts',(-22.8093737704392,26.6866888416268,-69.5471965828521));
#9028=CARTESIAN_POINT('Ctrl Pts',(-22.8133278900566,26.6876202400569,-69.5469557104002));
#9029=CARTESIAN_POINT('Ctrl Pts',(-22.8230998256346,26.6899025403004,-69.5463601492596));
#9030=CARTESIAN_POINT('Ctrl Pts',(-22.8289196406151,26.6912447465899,-69.5460052044055));
#9031=CARTESIAN_POINT('Ctrl Pts',(-22.8414939534858,26.6941079318187,-69.5452377454647));
#9032=CARTESIAN_POINT('Ctrl Pts',(-22.8482496792331,26.6956233354519,-69.5448250666928));
#9033=CARTESIAN_POINT('Ctrl Pts',(-22.8627027654149,26.6988164814011,-69.5439414031395));
#9034=CARTESIAN_POINT('Ctrl Pts',(-22.8704014880375,26.7004877901034,-69.5434702268306));
#9035=CARTESIAN_POINT('Ctrl Pts',(-22.8975403951096,26.7062752332475,-69.5418075172284));
#9036=CARTESIAN_POINT('Ctrl Pts',(-22.9170121558457,26.7102397192776,-69.5406113725651));
#9037=CARTESIAN_POINT('Ctrl Pts',(-22.9563188402286,26.7178647425853,-69.5381896836691));
#9038=CARTESIAN_POINT('Ctrl Pts',(-22.9761539284892,26.7215196465053,-69.5369640228348));
#9039=CARTESIAN_POINT('Ctrl Pts',(-23.0021561750857,26.7260590001987,-69.535352138365));
#9040=CARTESIAN_POINT('Ctrl Pts',(-23.0082937346417,26.7271121450482,-69.5349712964485));
#9041=CARTESIAN_POINT('Ctrl Pts',(-23.0177639625179,26.7287089004688,-69.5343830707604));
#9042=CARTESIAN_POINT('Ctrl Pts',(-23.0210945210074,26.729265077139,-69.5341760871908));
#9043=CARTESIAN_POINT('Ctrl Pts',(-23.0277246209186,26.7303615430132,-69.5337638221453));
#9044=CARTESIAN_POINT('Ctrl Pts',(-23.0310241414461,26.730901933945,-69.533558544184));
#9045=CARTESIAN_POINT('Ctrl Pts',(-23.0383344573878,26.7320875290667,-69.5331034880886));
#9046=CARTESIAN_POINT('Ctrl Pts',(-23.0423456390098,26.7327302854936,-69.5328536324775));
#9047=CARTESIAN_POINT('Ctrl Pts',(-23.0506164299402,26.7340395718234,-69.5323381012382));
#9048=CARTESIAN_POINT('Ctrl Pts',(-23.0548761810921,26.7347051411775,-69.5320723955862));
#9049=CARTESIAN_POINT('Ctrl Pts',(-23.0773794142197,26.7381749375841,-69.5306677282192));
#9050=CARTESIAN_POINT('Ctrl Pts',(-23.0956451041122,26.7408308985702,-69.5295240683848));
#9051=CARTESIAN_POINT('Ctrl Pts',(-23.221749670685,26.7580625436592,-69.5216031247671));
#9052=CARTESIAN_POINT('Ctrl Pts',(-23.330232201697,26.7673235133517,-69.5146584174444));
#9053=CARTESIAN_POINT('Ctrl Pts',(-23.6038113319815,26.7767762877768,-69.4968017051579));
#9054=CARTESIAN_POINT('Ctrl Pts',(-23.768835155235,26.7698077088262,-69.4857073897485));
#9055=CARTESIAN_POINT('Ctrl Pts',(-24.1270260032621,26.7270114879794,-69.4612936574412));
#9056=CARTESIAN_POINT('Ctrl Pts',(-24.3189644709451,26.6861035175699,-69.447992579817));
#9057=CARTESIAN_POINT('Ctrl Pts',(-24.5091463157055,26.6270448588762,-69.4352497852357));
#9058=CARTESIAN_POINT('Ctrl Pts',(-24.5122762234432,26.626067664359,-69.4350402020583));
#9059=CARTESIAN_POINT('Ctrl Pts',(-24.5210231841025,26.6233221015398,-69.4344548688866));
#9060=CARTESIAN_POINT('Ctrl Pts',(-24.5266369232218,26.6215431011206,-69.434079640099));
#9061=CARTESIAN_POINT('Ctrl Pts',(-24.553136092147,26.6130654865465,-69.4323105602391));
#9062=CARTESIAN_POINT('Ctrl Pts',(-24.5739583129835,26.6061689522566,-69.4309268036991));
#9063=CARTESIAN_POINT('Ctrl Pts',(-24.5984792687022,26.5977685943256,-69.4293061008247));
#9064=CARTESIAN_POINT('Ctrl Pts',(-24.6022469825688,26.59647004197,-69.4290573235621));
#9065=CARTESIAN_POINT('Ctrl Pts',(-24.6083000377138,26.5943712712385,-69.4286580587353));
#9066=CARTESIAN_POINT('Ctrl Pts',(-24.6105868876512,26.5935754654476,-69.4285073104458));
#9067=CARTESIAN_POINT('Ctrl Pts',(-24.6146496443481,26.592156522811,-69.4282396655508));
#9068=CARTESIAN_POINT('Ctrl Pts',(-24.6164259025886,26.5915344074608,-69.4281227078813));
#9069=CARTESIAN_POINT('Ctrl Pts',(-24.6201505221503,26.5902262354033,-69.427877583209));
#9070=CARTESIAN_POINT('Ctrl Pts',(-24.6220987646433,26.5895398629934,-69.427749435716));
#9071=CARTESIAN_POINT('Ctrl Pts',(-24.6260552333066,26.5881417082894,-69.4274893354236));
#9072=CARTESIAN_POINT('Ctrl Pts',(-24.6280634165674,26.5874298064977,-69.4273573898581));
#9073=CARTESIAN_POINT('Ctrl Pts',(-24.6330271800261,26.5856646072229,-69.4270314292175));
#9074=CARTESIAN_POINT('Ctrl Pts',(-24.6359819386083,26.5846089811732,-69.4268375523524));
#9075=CARTESIAN_POINT('Ctrl Pts',(-24.6648192100615,26.5742589752997,-69.4249468751775));
#9076=CARTESIAN_POINT('Ctrl Pts',(-24.6905843284826,26.564637604443,-69.4232693009594));
#9077=CARTESIAN_POINT('Ctrl Pts',(-24.7720607432397,26.533017949571,-69.4179921267483));
#9078=CARTESIAN_POINT('Ctrl Pts',(-24.8272862343931,26.5097948496602,-69.4144568066649));
#9079=CARTESIAN_POINT('Ctrl Pts',(-24.9639619637344,26.4477818921222,-69.4057362316423));
#9080=CARTESIAN_POINT('Ctrl Pts',(-25.0444925043024,26.4070863494505,-69.400623844108));
#9081=CARTESIAN_POINT('Ctrl Pts',(-25.1955577619493,26.3226086699534,-69.3908958354119));
#9082=CARTESIAN_POINT('Ctrl Pts',(-25.2663145947021,26.2793767709488,-69.3862772145548));
#9083=CARTESIAN_POINT('Ctrl Pts',(-25.5386973541227,26.0981673361259,-69.3679811940941));
#9084=CARTESIAN_POINT('Ctrl Pts',(-25.7259934010847,25.9402126340196,-69.3541597507562));
#9085=CARTESIAN_POINT('Ctrl Pts',(-25.9039914836604,25.7516742872414,-69.3384289345038));
#9086=CARTESIAN_POINT('Ctrl Pts',(-25.9142627162647,25.7406407701064,-69.3375111215199));
#9087=CARTESIAN_POINT('Ctrl Pts',(-25.9281979548689,25.7254591305463,-69.3362518462503));
#9088=CARTESIAN_POINT('Ctrl Pts',(-25.9319293567771,25.7213729068797,-69.3359132575238));
#9089=CARTESIAN_POINT('Ctrl Pts',(-25.9378271949678,25.714880738044,-69.3353758576808));
#9090=CARTESIAN_POINT('Ctrl Pts',(-25.9400005734878,25.7124810906239,-69.3351773410354));
#9091=CARTESIAN_POINT('Ctrl Pts',(-25.9442035992433,25.7078264130088,-69.3347924978296));
#9092=CARTESIAN_POINT('Ctrl Pts',(-25.9462336862373,25.705571782786,-69.3346061901252));
#9093=CARTESIAN_POINT('Ctrl Pts',(-25.9510531905909,25.7002039803247,-69.3341628716662));
#9094=CARTESIAN_POINT('Ctrl Pts',(-25.9538397355973,25.6970882469265,-69.3339057403805));
#9095=CARTESIAN_POINT('Ctrl Pts',(-25.9595965152841,25.6906261326891,-69.333372836069));
#9096=CARTESIAN_POINT('Ctrl Pts',(-25.9625658568267,25.6872789714372,-69.3330970263072));
#9097=CARTESIAN_POINT('Ctrl Pts',(-25.9702752065525,25.678552140372,-69.3323784828483));
#9098=CARTESIAN_POINT('Ctrl Pts',(-25.9750042301088,25.6731628385201,-69.3319352909789));
#9099=CARTESIAN_POINT('Ctrl Pts',(-26.0162936474098,25.6257905378528,-69.328044312553));
#9100=CARTESIAN_POINT('Ctrl Pts',(-26.0517765300322,25.5828847805752,-69.3245522224528));
#9101=CARTESIAN_POINT('Ctrl Pts',(-26.164353259825,25.4393428558225,-69.3129623477816));
#9102=CARTESIAN_POINT('Ctrl Pts',(-26.2366162140843,25.3350854297851,-69.3046829454011));
#9103=CARTESIAN_POINT('Ctrl Pts',(-26.3256596253924,25.1889126025371,-69.2932871026055));
#9104=CARTESIAN_POINT('Ctrl Pts',(-26.3479849621949,25.1504976479136,-69.2903115574893));
#9105=CARTESIAN_POINT('Ctrl Pts',(-26.3913505825243,25.0721959883959,-69.2842918449286));
#9106=CARTESIAN_POINT('Ctrl Pts',(-26.4123623754852,25.0323042027475,-69.2812479509936));
#9107=CARTESIAN_POINT('Ctrl Pts',(-26.5341153268384,24.7888986226874,-69.2628410576715));
#9108=CARTESIAN_POINT('Ctrl Pts',(-26.6139622893896,24.5756233741797,-69.2473531455926));
#9109=CARTESIAN_POINT('Ctrl Pts',(-26.6741330520243,24.3425111998598,-69.2321513448168));
#9110=CARTESIAN_POINT('Ctrl Pts',(-26.6774555611289,24.3292933079112,-69.2312952252948));
#9111=CARTESIAN_POINT('Ctrl Pts',(-26.6815714281676,24.3124684852463,-69.2302132597225));
#9112=CARTESIAN_POINT('Ctrl Pts',(-26.6824425102604,24.3088809847302,-69.2299830039435));
#9113=CARTESIAN_POINT('Ctrl Pts',(-26.6838134769649,24.3031921243742,-69.2296185957857));
#9114=CARTESIAN_POINT('Ctrl Pts',(-26.6843174133755,24.3010917591116,-69.2294842090159));
#9115=CARTESIAN_POINT('Ctrl Pts',(-26.6852093652762,24.2973576339207,-69.2292455677689));
#9116=CARTESIAN_POINT('Ctrl Pts',(-26.6855982132651,24.2957240866685,-69.2291412652521));
#9117=CARTESIAN_POINT('Ctrl Pts',(-26.6864992267176,24.2919257609363,-69.2288989603356));
#9118=CARTESIAN_POINT('Ctrl Pts',(-26.6870104268223,24.2897607591288,-69.2287610146917));
#9119=CARTESIAN_POINT('Ctrl Pts',(-26.6880582266442,24.2853025503532,-69.228477291748));
#9120=CARTESIAN_POINT('Ctrl Pts',(-26.688594555266,24.2830092801167,-69.2283315302066));
#9121=CARTESIAN_POINT('Ctrl Pts',(-26.6899610312855,24.2771373889373,-69.2279587742636));
#9122=CARTESIAN_POINT('Ctrl Pts',(-26.6907875773205,24.2735579205878,-69.2277319861788));
#9123=CARTESIAN_POINT('Ctrl Pts',(-26.6931594201572,24.263205623926,-69.227077340584));
#9124=CARTESIAN_POINT('Ctrl Pts',(-26.6946889527264,24.2564291508383,-69.2266503708514));
#9125=CARTESIAN_POINT('Ctrl Pts',(-26.6997851973655,24.2335057722964,-69.2252111030123));
#9126=CARTESIAN_POINT('Ctrl Pts',(-26.7032496120129,24.2173360651036,-69.2242043809806));
#9127=CARTESIAN_POINT('Ctrl Pts',(-26.7505442485847,23.987991038212,-69.2100365037298));
#9128=CARTESIAN_POINT('Ctrl Pts',(-26.7728001214968,23.770912029779,-69.197959250513));
#9129=CARTESIAN_POINT('Ctrl Pts',(-26.7730011573562,23.5532288202234,-69.185795593234));
#9130=CARTESIAN_POINT('Ctrl Pts',(-26.7730011574137,23.5532287579762,-69.1857955897558));
#9131=CARTESIAN_POINT('Ctrl Pts',(-26.7732054564558,23.3320075218539,-69.173434235357));
#9132=CARTESIAN_POINT('Ctrl Pts',(-26.7506327281678,23.1113721182886,-69.1610278023702));
#9133=CARTESIAN_POINT('Ctrl Pts',(-26.6957738384993,22.8472819083673,-69.1449756089575));
#9134=CARTESIAN_POINT('Ctrl Pts',(-26.6848338097548,22.8000046968289,-69.1420561916178));
#9135=CARTESIAN_POINT('Ctrl Pts',(-26.6711261504128,22.7463166407036,-69.1386825548652));
#9136=CARTESIAN_POINT('Ctrl Pts',(-26.6693997950522,22.739644482657,-69.1382622576606));
#9137=CARTESIAN_POINT('Ctrl Pts',(-26.6665470351507,22.7287629593386,-69.1375750931814));
#9138=CARTESIAN_POINT('Ctrl Pts',(-26.6654334659043,22.7245502266217,-69.1373086419016));
#9139=CARTESIAN_POINT('Ctrl Pts',(-26.6632566903651,22.7163823715248,-69.1367912148915));
#9140=CARTESIAN_POINT('Ctrl Pts',(-26.6621944812802,22.7124269901385,-69.1365402719437));
#9141=CARTESIAN_POINT('Ctrl Pts',(-26.6603350152416,22.7055551602477,-69.136103647351));
#9142=CARTESIAN_POINT('Ctrl Pts',(-26.6595411867571,22.7026377824156,-69.1359180774591));
#9143=CARTESIAN_POINT('Ctrl Pts',(-26.6578788088884,22.6965621823505,-69.1355311897376));
#9144=CARTESIAN_POINT('Ctrl Pts',(-26.657009548073,22.6934041598527,-69.1353298489175));
#9145=CARTESIAN_POINT('Ctrl Pts',(-26.6546079598432,22.6847308946379,-69.1347762155896));
#9146=CARTESIAN_POINT('Ctrl Pts',(-26.653065755952,22.6792184203156,-69.1344236014498));
#9147=CARTESIAN_POINT('Ctrl Pts',(-26.6470575178138,22.6579609360606,-69.1330609500813));
#9148=CARTESIAN_POINT('Ctrl Pts',(-26.6424863169952,22.6422461358809,-69.1320474841022));
#9149=CARTESIAN_POINT('Ctrl Pts',(-26.5643782701371,22.3811594630158,-69.1151058043699));
#9150=CARTESIAN_POINT('Ctrl Pts',(-26.4619812884204,22.1454344618131,-69.0981648042478));
#9151=CARTESIAN_POINT('Ctrl Pts',(-26.3100444919523,21.8854098902804,-69.0778085857863));
#9152=CARTESIAN_POINT('Ctrl Pts',(-26.2864698453787,21.8469417935336,-69.0747534967972));
#9153=CARTESIAN_POINT('Ctrl Pts',(-26.2387812909853,21.7726719841405,-69.0687801124473));
#9154=CARTESIAN_POINT('Ctrl Pts',(-26.21473993205,21.7368340865593,-69.0658622234479));
#9155=CARTESIAN_POINT('Ctrl Pts',(-26.125634952176,21.609606645508,-69.055395730578));
#9156=CARTESIAN_POINT('Ctrl Pts',(-26.0565246181369,21.5211380394106,-69.0479103490364));
#9157=CARTESIAN_POINT('Ctrl Pts',(-25.9531289354647,21.4021446022513,-69.0377241156348));
#9158=CARTESIAN_POINT('Ctrl Pts',(-25.9225982140616,21.3684736284577,-69.0348277388908));
#9159=CARTESIAN_POINT('Ctrl Pts',(-25.8889201513319,21.3328748081639,-69.0317608990171));
#9160=CARTESIAN_POINT('Ctrl Pts',(-25.8864724042136,21.3302960205248,-69.0315387098154));
#9161=CARTESIAN_POINT('Ctrl Pts',(-25.8824304113453,21.3260517279102,-69.031172984435));
#9162=CARTESIAN_POINT('Ctrl Pts',(-25.8808386450638,21.3243838819002,-69.0310292591087));
#9163=CARTESIAN_POINT('Ctrl Pts',(-25.8777320295428,21.321135769037,-69.0307493403345));
#9164=CARTESIAN_POINT('Ctrl Pts',(-25.8762173577638,21.3195553352059,-69.0306131332645));
#9165=CARTESIAN_POINT('Ctrl Pts',(-25.8735391891196,21.3167665828567,-69.0303727788705));
#9166=CARTESIAN_POINT('Ctrl Pts',(-25.8723763650497,21.3155576355581,-69.0302685799365));
#9167=CARTESIAN_POINT('Ctrl Pts',(-25.8698920198838,21.3129787821633,-69.0300463018101));
#9168=CARTESIAN_POINT('Ctrl Pts',(-25.8685702327196,21.3116091427938,-69.0299282444383));
#9169=CARTESIAN_POINT('Ctrl Pts',(-25.8647550876547,21.3076628820449,-69.0295880766785));
#9170=CARTESIAN_POINT('Ctrl Pts',(-25.862258632085,21.3050892391217,-69.029366208838));
#9171=CARTESIAN_POINT('Ctrl Pts',(-25.8512192622192,21.2937464834782,-69.0283882592297));
#9172=CARTESIAN_POINT('Ctrl Pts',(-25.8426305687554,21.285021773659,-69.0276357235385));
#9173=CARTESIAN_POINT('Ctrl Pts',(-25.6864115514974,21.1281272087986,-69.0140926395539));
#9174=CARTESIAN_POINT('Ctrl Pts',(-25.5247255038059,20.9946014998495,-69.0023806990977));
#9175=CARTESIAN_POINT('Ctrl Pts',(-25.29662468742,20.8408919410459,-68.9870047288095));
#9176=CARTESIAN_POINT('Ctrl Pts',(-25.2409229168375,20.8057882684458,-68.9833322874066));
#9177=CARTESIAN_POINT('Ctrl Pts',(-25.1284920881933,20.7396560833252,-68.9760170442883));
#9178=CARTESIAN_POINT('Ctrl Pts',(-25.0718272940134,20.7085800743964,-68.972376638843));
#9179=CARTESIAN_POINT('Ctrl Pts',(-24.9123068813412,20.6272361352512,-68.9621843669601));
#9180=CARTESIAN_POINT('Ctrl Pts',(-24.807657461768,20.5807162187292,-68.9555574778011));
#9181=CARTESIAN_POINT('Ctrl Pts',(-24.6697707422643,20.5280187026143,-68.9467673547709));
#9182=CARTESIAN_POINT('Ctrl Pts',(-24.6385988385386,20.5166539202363,-68.9447767753158));
#9183=CARTESIAN_POINT('Ctrl Pts',(-24.587795553332,20.4990156545212,-68.9415243201679));
#9184=CARTESIAN_POINT('Ctrl Pts',(-24.568269251572,20.4924454858257,-68.9402722900324));
#9185=CARTESIAN_POINT('Ctrl Pts',(-24.5444434316439,20.4846821302062,-68.9387418084519));
#9186=CARTESIAN_POINT('Ctrl Pts',(-24.5402023756834,20.4833099599962,-68.9384692729771));
#9187=CARTESIAN_POINT('Ctrl Pts',(-24.5319904220197,20.4806718359171,-68.9379413520671));
#9188=CARTESIAN_POINT('Ctrl Pts',(-24.5280198864919,20.4794047769494,-68.9376860035972));
#9189=CARTESIAN_POINT('Ctrl Pts',(-24.5211563656972,20.4772291828694,-68.9372444364809));
#9190=CARTESIAN_POINT('Ctrl Pts',(-24.5182645285773,20.4763170198311,-68.9370583375375));
#9191=CARTESIAN_POINT('Ctrl Pts',(-24.5122775444319,20.4744378506011,-68.9366729475509));
#9192=CARTESIAN_POINT('Ctrl Pts',(-24.5091822176633,20.473471432102,-68.9364736374142));
#9193=CARTESIAN_POINT('Ctrl Pts',(-24.5007761467483,20.4708608178706,-68.9359321995467));
#9194=CARTESIAN_POINT('Ctrl Pts',(-24.4954626161897,20.4692256954772,-68.9355897742052));
#9195=CARTESIAN_POINT('Ctrl Pts',(-24.4755631049716,20.4631583800688,-68.9343066810395));
#9196=CARTESIAN_POINT('Ctrl Pts',(-24.4609501457871,20.4588160046311,-68.9333630741039));
#9197=CARTESIAN_POINT('Ctrl Pts',(-24.2105540254591,20.386337920182,-68.9171689827774));
#9198=CARTESIAN_POINT('Ctrl Pts',(-23.9678294973073,20.3452665866028,-68.900994467619));
#9199=CARTESIAN_POINT('Ctrl Pts',(-23.566312469373,20.3237321235846,-68.8738500861061));
#9200=CARTESIAN_POINT('Ctrl Pts',(-23.4093689591525,20.3267690235554,-68.8631694872695));
#9201=CARTESIAN_POINT('Ctrl Pts',(-23.1549473069267,20.3503148935474,-68.8462090337969));
#9202=CARTESIAN_POINT('Ctrl Pts',(-23.0570858717645,20.3639289059037,-68.8397756024135));
#9203=CARTESIAN_POINT('Ctrl Pts',(-22.9532715709775,20.3832700476603,-68.8331530916662));
#9204=CARTESIAN_POINT('Ctrl Pts',(-22.9465531061393,20.3845438705476,-68.8327254277066));
#9205=CARTESIAN_POINT('Ctrl Pts',(-22.9377584459771,20.3862403563334,-68.8321668545844));
#9206=CARTESIAN_POINT('Ctrl Pts',(-22.935678607299,20.3866436838143,-68.8320348500308));
#9207=CARTESIAN_POINT('Ctrl Pts',(-22.9315799292667,20.387442704064,-68.8317748953788));
#9208=CARTESIAN_POINT('Ctrl Pts',(-22.9295610684081,20.3878382795429,-68.8316469386188));
#9209=CARTESIAN_POINT('Ctrl Pts',(-22.9256935726164,20.388599922605,-68.8314019836878));
#9210=CARTESIAN_POINT('Ctrl Pts',(-22.9238448857191,20.3889656774206,-68.8312849682221));
#9211=CARTESIAN_POINT('Ctrl Pts',(-22.9196050641498,20.3898083731706,-68.831016771518));
#9212=CARTESIAN_POINT('Ctrl Pts',(-22.9172141437238,20.3902864073637,-68.830865653456));
#9213=CARTESIAN_POINT('Ctrl Pts',(-22.9096687311686,20.3918039241972,-68.8303891290036));
#9214=CARTESIAN_POINT('Ctrl Pts',(-22.9045162056152,20.392853315598,-68.8300642900469));
#9215=CARTESIAN_POINT('Ctrl Pts',(-22.8619302032348,20.401635218107,-68.8273839705886));
#9216=CARTESIAN_POINT('Ctrl Pts',(-22.8246324541351,20.4100209424876,-68.8250652452798));
#9217=CARTESIAN_POINT('Ctrl Pts',(-22.6264503396226,20.4582984475591,-68.8128558338109));
#9218=CARTESIAN_POINT('Ctrl Pts',(-22.468655968898,20.5098985066632,-68.8035203906868));
#9219=CARTESIAN_POINT('Ctrl Pts',(-22.1690608476923,20.6341649479403,-68.785368005679));
#9220=CARTESIAN_POINT('Ctrl Pts',(-22.0272895418607,20.7056367829793,-68.7765676565949));
#9221=CARTESIAN_POINT('Ctrl Pts',(-21.8023962496162,20.8406615327062,-68.7615727199061));
#9222=CARTESIAN_POINT('Ctrl Pts',(-21.7160719219068,20.898335589781,-68.755540453925));
#9223=CARTESIAN_POINT('Ctrl Pts',(-21.6074411569875,20.9787572428591,-68.7474815141315));
#9224=CARTESIAN_POINT('Ctrl Pts',(-21.5824727918744,20.997813139757,-68.7455953601906));
#9225=CARTESIAN_POINT('Ctrl Pts',(-21.5422671963951,21.0294386989259,-68.7425001217097));
#9226=CARTESIAN_POINT('Ctrl Pts',(-21.5268596300861,21.0417891325277,-68.7412997244604));
#9227=CARTESIAN_POINT('Ctrl Pts',(-21.5081582683963,21.0570642212532,-68.7398248084924));
#9228=CARTESIAN_POINT('Ctrl Pts',(-21.5047554599435,21.0598552419691,-68.7395557075462));
#9229=CARTESIAN_POINT('Ctrl Pts',(-21.4981728135297,21.0652769935985,-68.7390337113095));
#9230=CARTESIAN_POINT('Ctrl Pts',(-21.4949922892913,21.0679068808265,-68.7387808506076));
#9231=CARTESIAN_POINT('Ctrl Pts',(-21.4894876407385,21.0724763532925,-68.7383420849296));
#9232=CARTESIAN_POINT('Ctrl Pts',(-21.4871611760068,21.0744131217086,-68.7381562951631));
#9233=CARTESIAN_POINT('Ctrl Pts',(-21.4823344593196,21.0784428625924,-68.7377701044611));
#9234=CARTESIAN_POINT('Ctrl Pts',(-21.479834648984,21.0805363566772,-68.7375696822722));
#9235=CARTESIAN_POINT('Ctrl Pts',(-21.4737552272873,21.0856433533145,-68.7370812633407));
#9236=CARTESIAN_POINT('Ctrl Pts',(-21.4701790010589,21.0886608587815,-68.7367931022605));
#9237=CARTESIAN_POINT('Ctrl Pts',(-21.4567004610959,21.1000839659831,-68.7357038241347));
#9238=CARTESIAN_POINT('Ctrl Pts',(-21.4468425272232,21.1085415295775,-68.7349005646103));
#9239=CARTESIAN_POINT('Ctrl Pts',(-21.2848928897728,21.2491939434784,-68.7215940869746));
#9240=CARTESIAN_POINT('Ctrl Pts',(-21.1455078637019,21.3952814394197,-68.7084827251768));
#9241=CARTESIAN_POINT('Ctrl Pts',(-20.9344557323106,21.6626364538485,-68.6856744553058));
#9242=CARTESIAN_POINT('Ctrl Pts',(-20.8553894982721,21.7773457337308,-68.6762098595937));
#9243=CARTESIAN_POINT('Ctrl Pts',(-20.6997948022966,22.0376594262543,-68.6557485569511));
#9244=CARTESIAN_POINT('Ctrl Pts',(-20.6264702153756,22.1847638390257,-68.6448089919531));
#9245=CARTESIAN_POINT('Ctrl Pts',(-20.5623425906333,22.3425481778775,-68.6341357379712));
#9246=CARTESIAN_POINT('Ctrl Pts',(-20.5600361577521,22.3482701438751,-68.6337500894727));
#9247=CARTESIAN_POINT('Ctrl Pts',(-20.5567583789032,22.3564697201795,-68.6331995099653));
#9248=CARTESIAN_POINT('Ctrl Pts',(-20.5557736671606,22.3589419198697,-68.633033775177));
#9249=CARTESIAN_POINT('Ctrl Pts',(-20.5540856692534,22.3631950936009,-68.6327491070246));
#9250=CARTESIAN_POINT('Ctrl Pts',(-20.5533809073319,22.3649754771267,-68.6326300836762));
#9251=CARTESIAN_POINT('Ctrl Pts',(-20.5520337772088,22.3683875065671,-68.6324022482081));
#9252=CARTESIAN_POINT('Ctrl Pts',(-20.5513911549291,22.3700190461712,-68.632293420522));
#9253=CARTESIAN_POINT('Ctrl Pts',(-20.5498808810348,22.3738626446177,-68.6320373168004));
#9254=CARTESIAN_POINT('Ctrl Pts',(-20.5490143421539,22.3760751438068,-68.6318901085708));
#9255=CARTESIAN_POINT('Ctrl Pts',(-20.546463444579,22.382609521938,-68.6314559687205));
#9256=CARTESIAN_POINT('Ctrl Pts',(-20.544785959525,22.386934104816,-68.6311694511217));
#9257=CARTESIAN_POINT('Ctrl Pts',(-20.5303105558753,22.4244922211805,-68.628687958453));
#9258=CARTESIAN_POINT('Ctrl Pts',(-20.5180543377325,22.4579338126701,-68.6265249641485));
#9259=CARTESIAN_POINT('Ctrl Pts',(-20.4598465109826,22.6252920670263,-68.6158979464249));
#9260=CARTESIAN_POINT('Ctrl Pts',(-20.4221950968812,22.7619461145281,-68.6078411699737));
#9261=CARTESIAN_POINT('Ctrl Pts',(-20.351355410499,23.1061746118789,-68.5880913564939));
#9262=CARTESIAN_POINT('Ctrl Pts',(-20.329234423668,23.3153319300588,-68.5765370200261));
#9263=CARTESIAN_POINT('Ctrl Pts',(-20.3272670541395,23.5679376182818,-68.561972758975));
#9264=CARTESIAN_POINT('Ctrl Pts',(-20.3277858848855,23.6107227685876,-68.5594865754545));
#9265=CARTESIAN_POINT('Ctrl Pts',(-20.3317549958391,23.7345699195833,-68.5522183979401));
#9266=CARTESIAN_POINT('Ctrl Pts',(-20.3374143615516,23.8155230570439,-68.5473777719861));
#9267=CARTESIAN_POINT('Ctrl Pts',(-20.3471831677087,23.906008204228,-68.5418365721243));
#9268=CARTESIAN_POINT('Ctrl Pts',(-20.3482904128051,23.9158397782012,-68.5412327766843));
#9269=CARTESIAN_POINT('Ctrl Pts',(-20.3499744658075,23.9301981679349,-68.5403484042372));
#9270=CARTESIAN_POINT('Ctrl Pts',(-20.35051565203,23.9347291708695,-68.5400689534336));
#9271=CARTESIAN_POINT('Ctrl Pts',(-20.3514771385252,23.94263642828,-68.5395806127939));
#9272=CARTESIAN_POINT('Ctrl Pts',(-20.3518931664677,23.9460132030191,-68.5393718583824));
#9273=CARTESIAN_POINT('Ctrl Pts',(-20.3527074703625,23.9525375163742,-68.538968113238));
#9274=CARTESIAN_POINT('Ctrl Pts',(-20.35310504863,23.9556851396105,-68.5387731448036));
#9275=CARTESIAN_POINT('Ctrl Pts',(-20.3540590702268,23.9631494471666,-68.538310356779));
#9276=CARTESIAN_POINT('Ctrl Pts',(-20.3546196105906,23.967465593815,-68.5380424076923));
#9277=CARTESIAN_POINT('Ctrl Pts',(-20.3566220815938,23.9826437590434,-68.5370989066085));
#9278=CARTESIAN_POINT('Ctrl Pts',(-20.3581106509294,23.9934994533959,-68.5364218786832));
#9279=CARTESIAN_POINT('Ctrl Pts',(-20.3787263421843,24.1383511377345,-68.5273579042963));
#9280=CARTESIAN_POINT('Ctrl Pts',(-20.406218496205,24.2710018614856,-68.5187039035601));
#9281=CARTESIAN_POINT('Ctrl Pts',(-20.4895788516676,24.5753818994669,-68.4979914060277));
#9282=CARTESIAN_POINT('Ctrl Pts',(-20.5516950624083,24.7449305587953,-68.4857818347036));
#9283=CARTESIAN_POINT('Ctrl Pts',(-20.7076333505371,25.0804996381276,-68.4607471234247));
#9284=CARTESIAN_POINT('Ctrl Pts',(-20.8026768411822,25.2452414211013,-68.4479752544551));
#9285=CARTESIAN_POINT('Ctrl Pts',(-20.9161667668792,25.4070699014729,-68.4355665400562));
#9286=CARTESIAN_POINT('Ctrl Pts',(-20.9206744529099,25.4134480908651,-68.4350777425127));
#9287=CARTESIAN_POINT('Ctrl Pts',(-20.9268978197079,25.4221863257839,-68.4344085249116));
#9288=CARTESIAN_POINT('Ctrl Pts',(-20.9285935369433,25.424560454571,-68.4342267475036));
#9289=CARTESIAN_POINT('Ctrl Pts',(-20.9314376300577,25.4285309830028,-68.4339228205729));
#9290=CARTESIAN_POINT('Ctrl Pts',(-20.9325842430391,25.4301286340751,-68.4338005490517));
#9291=CARTESIAN_POINT('Ctrl Pts',(-20.9348465129014,25.4332747200059,-68.4335598172978));
#9292=CARTESIAN_POINT('Ctrl Pts',(-20.9359620829553,25.4348232134354,-68.4334413513428));
#9293=CARTESIAN_POINT('Ctrl Pts',(-20.9384261553047,25.4382371291764,-68.4331802182592));
#9294=CARTESIAN_POINT('Ctrl Pts',(-20.9397752842585,25.4401021028061,-68.4330375947565));
#9295=CARTESIAN_POINT('Ctrl Pts',(-20.9445023637839,25.4466218793069,-68.4325390942446));
#9296=CARTESIAN_POINT('Ctrl Pts',(-20.9478908016322,25.4512691195356,-68.4321839426802));
#9297=CARTESIAN_POINT('Ctrl Pts',(-20.9825985447377,25.4986040651552,-68.4285680223459));
#9298=CARTESIAN_POINT('Ctrl Pts',(-21.0149550564518,25.5405259316187,-68.425378177054));
#9299=CARTESIAN_POINT('Ctrl Pts',(-21.0500078055271,25.5836981146262,-68.4220842515412));
#9300=CARTESIAN_POINT('Ctrl Pts',(-21.0516860069556,25.5857598274346,-68.4219269263743));
#9301=CARTESIAN_POINT('Ctrl Pts',(-21.0558601057756,25.5908748731096,-68.4215365465891));
#9302=CARTESIAN_POINT('Ctrl Pts',(-21.0583590660969,25.5939257127944,-68.4213036527697));
#9303=CARTESIAN_POINT('Ctrl Pts',(-21.0632948537146,25.5999290245701,-68.4208452504473));
#9304=CARTESIAN_POINT('Ctrl Pts',(-21.0657313534115,25.6028817559857,-68.4206197257744));
#9305=CARTESIAN_POINT('Ctrl Pts',(-21.0782132507519,25.6179534614436,-68.4194682299248));
#9306=CARTESIAN_POINT('Ctrl Pts',(-21.0883422291366,25.6300032425262,-68.4185464718938));
#9307=CARTESIAN_POINT('Ctrl Pts',(-21.1235507570112,25.6712708426543,-68.4153838205948));
#9308=CARTESIAN_POINT('Ctrl Pts',(-21.1490660277703,25.7001138614991,-68.4131631185877));
#9309=CARTESIAN_POINT('Ctrl Pts',(-21.3197387950159,25.8862158926064,-68.3987146211547));
#9310=CARTESIAN_POINT('Ctrl Pts',(-21.4797387776913,26.029142824665,-68.3870084901483));
#9311=CARTESIAN_POINT('Ctrl Pts',(-21.7177415225729,26.2025137702741,-68.3703281466061));
#9312=CARTESIAN_POINT('Ctrl Pts',(-21.7844974519291,26.2474166211357,-68.3657237322359));
#9313=CARTESIAN_POINT('Ctrl Pts',(-21.9252348712095,26.3346167649304,-68.356080755321));
#9314=CARTESIAN_POINT('Ctrl Pts',(-21.9993515053438,26.3765699462487,-68.3510364005855));
#9315=CARTESIAN_POINT('Ctrl Pts',(-22.0750360157945,26.4155367747871,-68.3458849806668));
#9316=CARTESIAN_POINT('Origin',(-23.5502525316942,23.5502525316942,-77.3107734492734));
#9317=CARTESIAN_POINT('',(-22.0750360151859,26.4155367744738,-66.8490341587423));
#9318=CARTESIAN_POINT('',(-22.0750362583504,26.4155368996692,-67.093261398997));
#9319=CARTESIAN_POINT('',(-22.0750360153461,26.4155367745563,-77.3107734492734));
#9320=CARTESIAN_POINT('Ctrl Pts',(-22.0750360151859,26.4155367744738,-66.8490341587423));
#9321=CARTESIAN_POINT('Ctrl Pts',(-22.071751051794,26.4138454824967,-66.8492740680067));
#9322=CARTESIAN_POINT('Ctrl Pts',(-22.0684689450228,26.4121485146271,-66.8495137316808));
#9323=CARTESIAN_POINT('Ctrl Pts',(-22.0349331677317,26.3947361476878,-66.8519621261606));
#9324=CARTESIAN_POINT('Ctrl Pts',(-22.0049264016203,26.3785465723192,-66.8541492954419));
#9325=CARTESIAN_POINT('Ctrl Pts',(-21.964865452227,26.3561044828296,-66.8570588277654));
#9326=CARTESIAN_POINT('Ctrl Pts',(-21.9545817318059,26.3502689730423,-66.8578047646124));
#9327=CARTESIAN_POINT('Ctrl Pts',(-21.9373738941877,26.3403787722159,-66.8590510549417));
#9328=CARTESIAN_POINT('Ctrl Pts',(-21.9304324762743,26.33635463476,-66.8595532715316));
#9329=CARTESIAN_POINT('Ctrl Pts',(-21.9209876518421,26.3308319721612,-66.8602358228901));
#9330=CARTESIAN_POINT('Ctrl Pts',(-21.9184712210249,26.3293559532637,-66.8604176017749));
#9331=CARTESIAN_POINT('Ctrl Pts',(-21.9144516998785,26.3269909512494,-66.8607078321521));
#9332=CARTESIAN_POINT('Ctrl Pts',(-21.9129473294202,26.3261041643728,-66.8608164270686));
#9333=CARTESIAN_POINT('Ctrl Pts',(-21.9098154495445,26.3242545716661,-66.861042445296));
#9334=CARTESIAN_POINT('Ctrl Pts',(-21.9081880702867,26.32329155826,-66.8611598539729));
#9335=CARTESIAN_POINT('Ctrl Pts',(-21.904428276986,26.3210622032338,-66.861431029932));
#9336=CARTESIAN_POINT('Ctrl Pts',(-21.9022964706173,26.3197948285625,-66.861584729307));
#9337=CARTESIAN_POINT('Ctrl Pts',(-21.8956311006471,26.3158217960736,-66.8620651167713));
#9338=CARTESIAN_POINT('Ctrl Pts',(-21.8911026918383,26.3131074402995,-66.8623912372227));
#9339=CARTESIAN_POINT('Ctrl Pts',(-21.8518358796182,26.2894393181381,-66.8652170937012));
#9340=CARTESIAN_POINT('Ctrl Pts',(-21.8174873797379,26.2678412933784,-66.8676753559295));
#9341=CARTESIAN_POINT('Ctrl Pts',(-21.7782668974541,26.2421337395313,-66.8704774438764));
#9342=CARTESIAN_POINT('Ctrl Pts',(-21.7729899996083,26.2386526913302,-66.8708543459155));
#9343=CARTESIAN_POINT('Ctrl Pts',(-21.7654881496936,26.2336721525225,-66.8713900690177));
#9344=CARTESIAN_POINT('Ctrl Pts',(-21.7632548080461,26.2321853974609,-66.871549544547));
#9345=CARTESIAN_POINT('Ctrl Pts',(-21.7531504520879,26.2254406143342,-66.8722710205149));
#9346=CARTESIAN_POINT('Ctrl Pts',(-21.7453006928116,26.2201506618071,-66.8728313954879));
#9347=CARTESIAN_POINT('Ctrl Pts',(-21.7308608046311,26.210326832863,-66.8738622294787));
#9348=CARTESIAN_POINT('Ctrl Pts',(-21.7242640556973,26.2058028761522,-66.874333160156));
#9349=CARTESIAN_POINT('Ctrl Pts',(-21.5120675976051,26.059117003706,-66.8894839192787));
#9350=CARTESIAN_POINT('Ctrl Pts',(-21.3236662234413,25.8935276903796,-66.9030665896908));
#9351=CARTESIAN_POINT('Ctrl Pts',(-21.1321606329539,25.6810382666368,-66.9192090352863));
#9352=CARTESIAN_POINT('Ctrl Pts',(-21.1084853449075,25.6538658999633,-66.9212510764056));
#9353=CARTESIAN_POINT('Ctrl Pts',(-21.0539628711192,25.5891290779866,-66.9260746124904));
#9354=CARTESIAN_POINT('Ctrl Pts',(-21.0235004978678,25.5512531647835,-66.9288651041417));
#9355=CARTESIAN_POINT('Ctrl Pts',(-20.9520944112749,25.4582375507148,-66.935664541135));
#9356=CARTESIAN_POINT('Ctrl Pts',(-20.912035480991,25.4024518423534,-66.9396993171218));
#9357=CARTESIAN_POINT('Ctrl Pts',(-20.8492623044331,25.3088623054611,-66.94643113152));
#9358=CARTESIAN_POINT('Ctrl Pts',(-20.8254870293839,25.2717952147458,-66.9490880873586));
#9359=CARTESIAN_POINT('Ctrl Pts',(-20.7984718782925,25.2277147876981,-66.9522413434687));
#9360=CARTESIAN_POINT('Ctrl Pts',(-20.7944876405969,25.2211613407394,-66.9527099722501));
#9361=CARTESIAN_POINT('Ctrl Pts',(-20.7884258489683,25.2111099873883,-66.9534285016709));
#9362=CARTESIAN_POINT('Ctrl Pts',(-20.7863314431698,25.2076222338793,-66.9536777843918));
#9363=CARTESIAN_POINT('Ctrl Pts',(-20.7825277638771,25.2012608150456,-66.9541323857964));
#9364=CARTESIAN_POINT('Ctrl Pts',(-20.7808163452368,25.1983884335812,-66.9543376256966));
#9365=CARTESIAN_POINT('Ctrl Pts',(-20.7773875797564,25.1926133008575,-66.9547502237295));
#9366=CARTESIAN_POINT('Ctrl Pts',(-20.7756703135225,25.1897105068309,-66.9549575844667));
#9367=CARTESIAN_POINT('Ctrl Pts',(-20.7708049971634,25.1814568436622,-66.9555471128667));
#9368=CARTESIAN_POINT('Ctrl Pts',(-20.7676678602695,25.1760995878717,-66.955929677077));
#9369=CARTESIAN_POINT('Ctrl Pts',(-20.7544825273087,25.1534331884865,-66.9575479682772));
#9370=CARTESIAN_POINT('Ctrl Pts',(-20.7445803801854,25.136039996924,-66.9587889732221));
#9371=CARTESIAN_POINT('Ctrl Pts',(-20.5471565920339,24.7816256852889,-66.9840643800981));
#9372=CARTESIAN_POINT('Ctrl Pts',(-20.4215136068534,24.4137811638311,-67.0106387641172));
#9373=CARTESIAN_POINT('Ctrl Pts',(-20.3516565360621,23.9523693850203,-67.041736694716));
#9374=CARTESIAN_POINT('Ctrl Pts',(-20.3425375520877,23.8716263032723,-67.0470763542266));
#9375=CARTESIAN_POINT('Ctrl Pts',(-20.3348873412828,23.7693405300435,-67.0536452722395));
#9376=CARTESIAN_POINT('Ctrl Pts',(-20.3335072014444,23.7480463505507,-67.0550021280944));
#9377=CARTESIAN_POINT('Ctrl Pts',(-20.3318795093429,23.7183683735257,-67.0568768781347));
#9378=CARTESIAN_POINT('Ctrl Pts',(-20.3314530598292,23.7099954840798,-67.0574039839134));
#9379=CARTESIAN_POINT('Ctrl Pts',(-20.3308614440077,23.697413427129,-67.0581932617872));
#9380=CARTESIAN_POINT('Ctrl Pts',(-20.3306718529067,23.6932055235595,-67.0584567531634));
#9381=CARTESIAN_POINT('Ctrl Pts',(-20.330344477475,23.6856083254168,-67.0589316088834));
#9382=CARTESIAN_POINT('Ctrl Pts',(-20.3302037937746,23.6822191721242,-67.0591431332316));
#9383=CARTESIAN_POINT('Ctrl Pts',(-20.3299844317609,23.6767253071739,-67.0594855053579));
#9384=CARTESIAN_POINT('Ctrl Pts',(-20.3299024657812,23.6746207407398,-67.0596165380963));
#9385=CARTESIAN_POINT('Ctrl Pts',(-20.3297517455885,23.6706507611359,-67.0598634820847));
#9386=CARTESIAN_POINT('Ctrl Pts',(-20.3296825494338,23.6687853809422,-67.0599794173715));
#9387=CARTESIAN_POINT('Ctrl Pts',(-20.3295309201338,23.6645996097572,-67.0602393513081));
#9388=CARTESIAN_POINT('Ctrl Pts',(-20.3294493740323,23.6622791942414,-67.0603832990458));
#9389=CARTESIAN_POINT('Ctrl Pts',(-20.3292486230738,23.6563853115175,-67.0607485548853));
#9390=CARTESIAN_POINT('Ctrl Pts',(-20.3291328568721,23.652811719765,-67.0609696692688));
#9391=CARTESIAN_POINT('Ctrl Pts',(-20.3285292586741,23.6331691412746,-67.0621831667186));
#9392=CARTESIAN_POINT('Ctrl Pts',(-20.3281557110311,23.6170964964791,-67.0631692092188));
#9393=CARTESIAN_POINT('Ctrl Pts',(-20.3278091554453,23.5951002452893,-67.0645100272));
#9394=CARTESIAN_POINT('Ctrl Pts',(-20.3277321868415,23.5891788562458,-67.0648701194979));
#9395=CARTESIAN_POINT('Ctrl Pts',(-20.3242828337794,23.2523838765508,-67.085304367825));
#9396=CARTESIAN_POINT('Ctrl Pts',(-20.3718685107923,22.9229043021577,-67.1028787001028));
#9397=CARTESIAN_POINT('Ctrl Pts',(-20.4977740286207,22.5118546766074,-67.1273582830588));
#9398=CARTESIAN_POINT('Ctrl Pts',(-20.5310674179644,22.4186987619381,-67.1330730897336));
#9399=CARTESIAN_POINT('Ctrl Pts',(-20.5763410767344,22.3083243574325,-67.1401313089737));
#9400=CARTESIAN_POINT('Ctrl Pts',(-20.5842734977606,22.2894974901052,-67.1413454995848));
#9401=CARTESIAN_POINT('Ctrl Pts',(-20.6101175801385,22.2297529822681,-67.1452327994348));
#9402=CARTESIAN_POINT('Ctrl Pts',(-20.6287005104431,22.1891331115147,-67.147927394233));
#9403=CARTESIAN_POINT('Ctrl Pts',(-20.6514687183023,22.1419808096554,-67.1511209150155));
#9404=CARTESIAN_POINT('Ctrl Pts',(-20.654841340632,22.1350596568794,-67.1515913453299));
#9405=CARTESIAN_POINT('Ctrl Pts',(-20.6600367049817,22.1244942633115,-67.1523120660817));
#9406=CARTESIAN_POINT('Ctrl Pts',(-20.6618416272569,22.1208412501776,-67.1525617327008));
#9407=CARTESIAN_POINT('Ctrl Pts',(-20.6651403993394,22.1141965690248,-67.1530167366055));
#9408=CARTESIAN_POINT('Ctrl Pts',(-20.6666319889595,22.1112037800658,-67.1532219943883));
#9409=CARTESIAN_POINT('Ctrl Pts',(-20.6696356736158,22.1052004810458,-67.1536343753121));
#9410=CARTESIAN_POINT('Ctrl Pts',(-20.671147836676,22.1021900098686,-67.1538415006528));
#9411=CARTESIAN_POINT('Ctrl Pts',(-20.6754515241984,22.0936554570164,-67.1544296290452));
#9412=CARTESIAN_POINT('Ctrl Pts',(-20.6782542345898,22.0881370604565,-67.1548110256027));
#9413=CARTESIAN_POINT('Ctrl Pts',(-20.6901171594478,22.0649452733546,-67.1564186270837));
#9414=CARTESIAN_POINT('Ctrl Pts',(-20.6993245944035,22.0473480546261,-67.1576500240077));
#9415=CARTESIAN_POINT('Ctrl Pts',(-20.8898527224905,21.6912631792552,-67.1828086426594));
#9416=CARTESIAN_POINT('Ctrl Pts',(-21.130048976372,21.3878442960755,-67.2092502191314));
#9417=CARTESIAN_POINT('Ctrl Pts',(-21.5015603771647,21.0599791741555,-67.2422889545621));
#9418=CARTESIAN_POINT('Ctrl Pts',(-21.589131135369,20.9904459012406,-67.2496037491309));
#9419=CARTESIAN_POINT('Ctrl Pts',(-21.6839723599596,20.9228701956236,-67.2569071892691));
#9420=CARTESIAN_POINT('Ctrl Pts',(-21.6878032162492,20.9201532622064,-67.25720117977));
#9421=CARTESIAN_POINT('Ctrl Pts',(-21.6939118655706,20.9158409034196,-67.2576683471058));
#9422=CARTESIAN_POINT('Ctrl Pts',(-21.696185789952,20.9142400481883,-67.2578418907974));
#9423=CARTESIAN_POINT('Ctrl Pts',(-21.7004400201947,20.9112532749489,-67.2581658969187));
#9424=CARTESIAN_POINT('Ctrl Pts',(-21.7024198161109,20.9098666394216,-67.2583164084264));
#9425=CARTESIAN_POINT('Ctrl Pts',(-21.7059340486127,20.9074111833929,-67.2585830894818));
#9426=CARTESIAN_POINT('Ctrl Pts',(-21.7074678578092,20.9063414694437,-67.2586993208817));
#9427=CARTESIAN_POINT('Ctrl Pts',(-21.7104478408215,20.9042670134367,-67.2589248246702));
#9428=CARTESIAN_POINT('Ctrl Pts',(-21.7118939045229,20.9032621234517,-67.2590341074075));
#9429=CARTESIAN_POINT('Ctrl Pts',(-21.7153171301786,20.9008874341177,-67.2592924682951));
#9430=CARTESIAN_POINT('Ctrl Pts',(-21.7172950068385,20.8995186596967,-67.2594414756641));
#9431=CARTESIAN_POINT('Ctrl Pts',(-21.7231855766921,20.8954518814136,-67.2598844604298));
#9432=CARTESIAN_POINT('Ctrl Pts',(-21.72710272977,20.8927603019372,-67.2601779996104));
#9433=CARTESIAN_POINT('Ctrl Pts',(-21.7630097728024,20.8682043810405,-67.262859398056));
#9434=CARTESIAN_POINT('Ctrl Pts',(-21.7953873245048,20.8469087884076,-67.2652093414131));
#9435=CARTESIAN_POINT('Ctrl Pts',(-21.9259093773667,20.7643944499013,-67.2744486117063));
#9436=CARTESIAN_POINT('Ctrl Pts',(-22.0269425287747,20.7078894589182,-67.2810849149984));
#9437=CARTESIAN_POINT('Ctrl Pts',(-22.262067571359,20.592538203951,-67.2958828648194));
#9438=CARTESIAN_POINT('Ctrl Pts',(-22.3975620943591,20.5371477059052,-67.3039721913078));
#9439=CARTESIAN_POINT('Ctrl Pts',(-22.7267607808419,20.4280389775623,-67.3234757196262));
#9440=CARTESIAN_POINT('Ctrl Pts',(-22.9226162703508,20.3828543723098,-67.3349856079639));
#9441=CARTESIAN_POINT('Ctrl Pts',(-23.1382557662779,20.3539005451125,-67.3481725507862));
#9442=CARTESIAN_POINT('Ctrl Pts',(-23.1551451316106,20.3517689094322,-67.3492084622403));
#9443=CARTESIAN_POINT('Ctrl Pts',(-23.1776167155095,20.3491134331594,-67.350591095949));
#9444=CARTESIAN_POINT('Ctrl Pts',(-23.1831847660175,20.3484701789342,-67.3509340406014));
#9445=CARTESIAN_POINT('Ctrl Pts',(-23.1923445467277,20.3474361944824,-67.351498795709));
#9446=CARTESIAN_POINT('Ctrl Pts',(-23.1959353220984,20.3470369706635,-67.3517203375232));
#9447=CARTESIAN_POINT('Ctrl Pts',(-23.2029052318732,20.3462739164794,-67.3521506557007));
#9448=CARTESIAN_POINT('Ctrl Pts',(-23.2062842867353,20.3459093915537,-67.3523594098266));
#9449=CARTESIAN_POINT('Ctrl Pts',(-23.2141024765704,20.345078491738,-67.3528427196324));
#9450=CARTESIAN_POINT('Ctrl Pts',(-23.2185420087843,20.3446159935571,-67.3531173973127));
#9451=CARTESIAN_POINT('Ctrl Pts',(-23.2304808782954,20.3433973020056,-67.3538566959056));
#9452=CARTESIAN_POINT('Ctrl Pts',(-23.2379818973771,20.3426581957637,-67.3543218550933));
#9453=CARTESIAN_POINT('Ctrl Pts',(-23.273342085281,20.3392992207581,-67.3565178455768));
#9454=CARTESIAN_POINT('Ctrl Pts',(-23.3012313257525,20.3370160138398,-67.3582592536592));
#9455=CARTESIAN_POINT('Ctrl Pts',(-23.3370482099445,20.3345528848333,-67.3605083291293));
#9456=CARTESIAN_POINT('Ctrl Pts',(-23.3449522690451,20.3340385926062,-67.3610054434393));
#9457=CARTESIAN_POINT('Ctrl Pts',(-23.3570955233167,20.3332934153709,-67.3617704001531));
#9458=CARTESIAN_POINT('Ctrl Pts',(-23.36133345261,20.3330417572404,-67.3620375947915));
#9459=CARTESIAN_POINT('Ctrl Pts',(-23.3690222317799,20.33260042414,-67.3625227772735));
#9460=CARTESIAN_POINT('Ctrl Pts',(-23.372472918515,20.332407924532,-67.3627406772435));
#9461=CARTESIAN_POINT('Ctrl Pts',(-23.3828768238727,20.3318443195515,-67.3633981121929));
#9462=CARTESIAN_POINT('Ctrl Pts',(-23.3898309085838,20.3314901998071,-67.3638381699023));
#9463=CARTESIAN_POINT('Ctrl Pts',(-23.4030417205749,20.3308603899949,-67.3646753430994));
#9464=CARTESIAN_POINT('Ctrl Pts',(-23.4092982187891,20.3305803953213,-67.3650723247186));
#9465=CARTESIAN_POINT('Ctrl Pts',(-23.4196371531477,20.3301478944543,-67.3657291802957));
#9466=CARTESIAN_POINT('Ctrl Pts',(-23.423719153876,20.3299849099055,-67.365988734928));
#9467=CARTESIAN_POINT('Ctrl Pts',(-23.4334470095938,20.3296150247619,-67.3666077981251));
#9468=CARTESIAN_POINT('Ctrl Pts',(-23.4390931066583,20.3294152084763,-67.3669675197026));
#9469=CARTESIAN_POINT('Ctrl Pts',(-23.4654739110495,20.328551037455,-67.3686502217297));
#9470=CARTESIAN_POINT('Ctrl Pts',(-23.4862138374949,20.3280720670423,-67.3699787234017));
#9471=CARTESIAN_POINT('Ctrl Pts',(-23.5329382121105,20.3274442928584,-67.3729843306236));
#9472=CARTESIAN_POINT('Ctrl Pts',(-23.5589225365494,20.3274094542109,-67.3746646308278));
#9473=CARTESIAN_POINT('Ctrl Pts',(-23.6430720573178,20.3283142912047,-67.3801345173751));
#9474=CARTESIAN_POINT('Ctrl Pts',(-23.7012099266834,20.3305145350434,-67.3839576085634));
#9475=CARTESIAN_POINT('Ctrl Pts',(-23.9980600324472,20.3498064370695,-67.4036846520479));
#9476=CARTESIAN_POINT('Ctrl Pts',(-24.2343727315032,20.3918741136768,-67.4201457873064));
#9477=CARTESIAN_POINT('Ctrl Pts',(-24.4886744942841,20.4670476477931,-67.4377576368294));
#9478=CARTESIAN_POINT('Ctrl Pts',(-24.5134188492056,20.4746877310232,-67.439469361579));
#9479=CARTESIAN_POINT('Ctrl Pts',(-24.6036801529953,20.5037530630241,-67.4457000023894));
#9480=CARTESIAN_POINT('Ctrl Pts',(-24.6686025004669,20.5269821569794,-67.4501559133535));
#9481=CARTESIAN_POINT('Ctrl Pts',(-24.7395454230503,20.5549639682586,-67.4549587808422));
#9482=CARTESIAN_POINT('Ctrl Pts',(-24.7463467231649,20.5576734020386,-67.4554185451053));
#9483=CARTESIAN_POINT('Ctrl Pts',(-24.7566790302439,20.5618303346241,-67.4561158924241));
#9484=CARTESIAN_POINT('Ctrl Pts',(-24.7602167410417,20.5632609453658,-67.4563544606313));
#9485=CARTESIAN_POINT('Ctrl Pts',(-24.7659890453827,20.5656071384672,-67.4567433857277));
#9486=CARTESIAN_POINT('Ctrl Pts',(-24.7682251528049,20.5665189496962,-67.4568939675727));
#9487=CARTESIAN_POINT('Ctrl Pts',(-24.7724173703301,20.568233896433,-67.4571761189404));
#9488=CARTESIAN_POINT('Ctrl Pts',(-24.7743737170115,20.569036444665,-67.45730772392));
#9489=CARTESIAN_POINT('Ctrl Pts',(-24.778024225884,20.5705381849039,-67.4575531746687));
#9490=CARTESIAN_POINT('Ctrl Pts',(-24.7797185789884,20.5712368955936,-67.4576670493902));
#9491=CARTESIAN_POINT('Ctrl Pts',(-24.7831243447033,20.5726447524607,-67.4578958460064));
#9492=CARTESIAN_POINT('Ctrl Pts',(-24.7848357355404,20.5733539262515,-67.4580107656039));
#9493=CARTESIAN_POINT('Ctrl Pts',(-24.7896248236885,20.5753432901539,-67.4583322138294));
#9494=CARTESIAN_POINT('Ctrl Pts',(-24.7927011590756,20.576626784879,-67.4585385405241));
#9495=CARTESIAN_POINT('Ctrl Pts',(-24.8051639181609,20.5818491571695,-67.4593737780938));
#9496=CARTESIAN_POINT('Ctrl Pts',(-24.8145337789328,20.5858277786903,-67.4600002902994));
#9497=CARTESIAN_POINT('Ctrl Pts',(-24.9754185188145,20.6550440577152,-67.4707355176587));
#9498=CARTESIAN_POINT('Ctrl Pts',(-25.1217474526536,20.731786553067,-67.4801642266036));
#9499=CARTESIAN_POINT('Ctrl Pts',(-25.3332568178811,20.8643318796997,-67.4942066115237));
#9500=CARTESIAN_POINT('Ctrl Pts',(-25.4031445689615,20.9120589346875,-67.498920790241));
#9501=CARTESIAN_POINT('Ctrl Pts',(-25.539309842123,21.013130137849,-67.5084025450122));
#9502=CARTESIAN_POINT('Ctrl Pts',(-25.6055139479192,21.0664572755107,-67.5131665683818));
#9503=CARTESIAN_POINT('Ctrl Pts',(-25.760197156275,21.2014771634436,-67.5248274306774));
#9504=CARTESIAN_POINT('Ctrl Pts',(-25.8463503498309,21.2856264148833,-67.5317798649994));
#9505=CARTESIAN_POINT('Ctrl Pts',(-25.9626848560045,21.412733038289,-67.5420326543951));
#9506=CARTESIAN_POINT('Ctrl Pts',(-25.9968439326092,21.4519176334225,-67.545161885981));
#9507=CARTESIAN_POINT('Ctrl Pts',(-26.035153800727,21.498071405352,-67.5488192657515));
#9508=CARTESIAN_POINT('Ctrl Pts',(-26.0402454838774,21.5042523390233,-67.5493084868189));
#9509=CARTESIAN_POINT('Ctrl Pts',(-26.0479342234198,21.5136571210728,-67.5500520304206));
#9510=CARTESIAN_POINT('Ctrl Pts',(-26.0505482185001,21.5168671333914,-67.5503056660621));
#9511=CARTESIAN_POINT('Ctrl Pts',(-26.0552651099531,21.5226823714651,-67.5507648869279));
#9512=CARTESIAN_POINT('Ctrl Pts',(-26.0573701485495,21.5252858586339,-67.5509703852374));
#9513=CARTESIAN_POINT('Ctrl Pts',(-26.0615621424405,21.5304870243109,-67.5513807358947));
#9514=CARTESIAN_POINT('Ctrl Pts',(-26.0636491336283,21.5330846687992,-67.5515855864451));
#9515=CARTESIAN_POINT('Ctrl Pts',(-26.0694871206834,21.5403742437401,-67.5521601861726));
#9516=CARTESIAN_POINT('Ctrl Pts',(-26.0732290181079,21.5450734137672,-67.5525302999729));
#9517=CARTESIAN_POINT('Ctrl Pts',(-26.0883944406577,21.5642281928463,-67.554037777636));
#9518=CARTESIAN_POINT('Ctrl Pts',(-26.0997068643056,21.5787709548677,-67.5551795652177));
#9519=CARTESIAN_POINT('Ctrl Pts',(-26.3524216448012,21.9094627578509,-67.5810854230835));
#9520=CARTESIAN_POINT('Ctrl Pts',(-26.5333078805176,22.2674707544445,-67.6085842138839));
#9521=CARTESIAN_POINT('Ctrl Pts',(-26.6649475526173,22.7194932560586,-67.6398489527027));
#9522=CARTESIAN_POINT('Ctrl Pts',(-26.683031076185,22.7905247362341,-67.6446490201181));
#9523=CARTESIAN_POINT('Ctrl Pts',(-26.7051164100945,22.8915716196957,-67.651263941748));
#9524=CARTESIAN_POINT('Ctrl Pts',(-26.7111409669596,22.9211173337465,-67.6531726554586));
#9525=CARTESIAN_POINT('Ctrl Pts',(-26.717589536486,22.9551775643618,-67.6553404317211));
#9526=CARTESIAN_POINT('Ctrl Pts',(-26.7184195308325,22.9596123833538,-67.6556220544685));
#9527=CARTESIAN_POINT('Ctrl Pts',(-26.7196613443168,22.9663255660196,-67.6560473866775));
#9528=CARTESIAN_POINT('Ctrl Pts',(-26.7200800216135,22.9686026309767,-67.6561914872142));
#9529=CARTESIAN_POINT('Ctrl Pts',(-26.720831743408,22.9727159463238,-67.6564514840381));
#9530=CARTESIAN_POINT('Ctrl Pts',(-26.7211656458436,22.9745520299008,-67.6565674293454));
#9531=CARTESIAN_POINT('Ctrl Pts',(-26.7218318120067,22.9782333480822,-67.6567996752139));
#9532=CARTESIAN_POINT('Ctrl Pts',(-26.7221640590032,22.980078575172,-67.656915974505));
#9533=CARTESIAN_POINT('Ctrl Pts',(-26.7231020964033,22.9853144240414,-67.6572456602924));
#9534=CARTESIAN_POINT('Ctrl Pts',(-26.7237040641018,22.9887057415903,-67.6574588273678));
#9535=CARTESIAN_POINT('Ctrl Pts',(-26.7262142214823,23.0029802126301,-67.6583545248056));
#9536=CARTESIAN_POINT('Ctrl Pts',(-26.7280719018647,23.0138723445563,-67.6590341997011));
#9537=CARTESIAN_POINT('Ctrl Pts',(-26.7584198765389,23.1975050770158,-67.6704325206091));
#9538=CARTESIAN_POINT('Ctrl Pts',(-26.772848032414,23.3723036917934,-67.6803894010009));
#9539=CARTESIAN_POINT('Ctrl Pts',(-26.7732050218955,23.7802177939754,-67.703286709911));
#9540=CARTESIAN_POINT('Ctrl Pts',(-26.7481879453314,24.0123239489652,-67.7161030452746));
#9541=CARTESIAN_POINT('Ctrl Pts',(-26.6781518770707,24.3321171492653,-67.7351934171007));
#9542=CARTESIAN_POINT('Ctrl Pts',(-26.6538566894063,24.4235824524446,-67.7408166252732));
#9543=CARTESIAN_POINT('Ctrl Pts',(-26.6225041918604,24.5236449799105,-67.7471996671686));
#9544=CARTESIAN_POINT('Ctrl Pts',(-26.6193854133437,24.5334343422323,-67.7478266062952));
#9545=CARTESIAN_POINT('Ctrl Pts',(-26.6149489598046,24.5471328563189,-67.7487074204629));
#9546=CARTESIAN_POINT('Ctrl Pts',(-26.6136704855726,24.5510547187893,-67.7489600017864));
#9547=CARTESIAN_POINT('Ctrl Pts',(-26.6113160478814,24.5582304370356,-67.7494228899342));
#9548=CARTESIAN_POINT('Ctrl Pts',(-26.6102424153966,24.5614850565324,-67.7496331195022));
#9549=CARTESIAN_POINT('Ctrl Pts',(-26.6080610625296,24.5680623461763,-67.7500585473707));
#9550=CARTESIAN_POINT('Ctrl Pts',(-26.6069531132843,24.5713849344991,-67.7502737529827));
#9551=CARTESIAN_POINT('Ctrl Pts',(-26.6042212328238,24.5795331830353,-67.750802249253));
#9552=CARTESIAN_POINT('Ctrl Pts',(-26.6025912817329,24.5843568016986,-67.7511157390762));
#9553=CARTESIAN_POINT('Ctrl Pts',(-26.5966572988239,24.6017813548035,-67.7522504624634));
#9554=CARTESIAN_POINT('Ctrl Pts',(-26.592286656865,24.6143593138189,-67.753073904751));
#9555=CARTESIAN_POINT('Ctrl Pts',(-26.5290596319906,24.7927424773087,-67.7648148322503));
#9556=CARTESIAN_POINT('Ctrl Pts',(-26.4568105201193,24.9534542286004,-67.7761899271129));
#9557=CARTESIAN_POINT('Ctrl Pts',(-26.2190176758691,25.3843246831993,-67.8089339146691));
#9558=CARTESIAN_POINT('Ctrl Pts',(-26.0263021806489,25.6371886486296,-67.8309963779814));
#9559=CARTESIAN_POINT('Ctrl Pts',(-25.7881142690445,25.8693819625022,-67.852051117757));
#9560=CARTESIAN_POINT('Ctrl Pts',(-25.7762844832101,25.8807392298604,-67.8530827821655));
#9561=CARTESIAN_POINT('Ctrl Pts',(-25.7617514503933,25.89448013669,-67.8543326170052));
#9562=CARTESIAN_POINT('Ctrl Pts',(-25.7591305127118,25.8969499124231,-67.8545573265785));
#9563=CARTESIAN_POINT('Ctrl Pts',(-25.7548071145975,25.9010102992609,-67.8549268558224));
#9564=CARTESIAN_POINT('Ctrl Pts',(-25.7531070689303,25.9026034576033,-67.8550718720046));
#9565=CARTESIAN_POINT('Ctrl Pts',(-25.7500414104437,25.9054701305853,-67.8553328523499));
#9566=CARTESIAN_POINT('Ctrl Pts',(-25.7486764216167,25.9067442990198,-67.8554488672698));
#9567=CARTESIAN_POINT('Ctrl Pts',(-25.7457418388022,25.9094788585167,-67.8556978855248));
#9568=CARTESIAN_POINT('Ctrl Pts',(-25.7441718990837,25.9109388658469,-67.8558308590629));
#9569=CARTESIAN_POINT('Ctrl Pts',(-25.7398757322299,25.9149262135952,-67.8561940754672));
#9570=CARTESIAN_POINT('Ctrl Pts',(-25.7371465763807,25.917450415236,-67.8564240761353));
#9571=CARTESIAN_POINT('Ctrl Pts',(-25.7230531224797,25.930440304171,-67.8576080677669));
#9572=CARTESIAN_POINT('Ctrl Pts',(-25.71161779156,25.9408291306661,-67.8585562435994));
#9573=CARTESIAN_POINT('Ctrl Pts',(-25.6396851604433,26.0052407462451,-67.8644462974042));
#9574=CARTESIAN_POINT('Ctrl Pts',(-25.5772356739585,26.0570508146548,-67.8692343574641));
#9575=CARTESIAN_POINT('Ctrl Pts',(-25.386876903964,26.2032074151032,-67.8831216776298));
#9576=CARTESIAN_POINT('Ctrl Pts',(-25.2538713563161,26.2905167893736,-67.8919424957213));
#9577=CARTESIAN_POINT('Ctrl Pts',(-24.8966057948266,26.4889317200474,-67.9147877020739));
#9578=CARTESIAN_POINT('Ctrl Pts',(-24.664931977241,26.5843861364605,-67.9288874924147));
#9579=CARTESIAN_POINT('Ctrl Pts',(-24.4094598853148,26.6563959654596,-67.9449843920653));
#9580=CARTESIAN_POINT('Ctrl Pts',(-24.3943101485948,26.6605468961141,-67.9459405519521));
#9581=CARTESIAN_POINT('Ctrl Pts',(-24.373691506772,26.6660345361635,-67.9472442390154));
#9582=CARTESIAN_POINT('Ctrl Pts',(-24.3682483797659,26.667467961682,-67.9475886228678));
#9583=CARTESIAN_POINT('Ctrl Pts',(-24.3596504283398,26.6697081269951,-67.948132971767));
#9584=CARTESIAN_POINT('Ctrl Pts',(-24.3564980707704,26.6705243622792,-67.9483326286105));
#9585=CARTESIAN_POINT('Ctrl Pts',(-24.3501531630389,26.6721569827243,-67.9487346439706));
#9586=CARTESIAN_POINT('Ctrl Pts',(-24.3469605871147,26.6729732517857,-67.9489370059866));
#9587=CARTESIAN_POINT('Ctrl Pts',(-24.3397129197359,26.6748144774001,-67.9493965833787));
#9588=CARTESIAN_POINT('Ctrl Pts',(-24.3356570796745,26.6758364375571,-67.9496538953936));
#9589=CARTESIAN_POINT('Ctrl Pts',(-24.3271787994683,26.6779551866641,-67.9501920527244));
#9590=CARTESIAN_POINT('Ctrl Pts',(-24.3227560026073,26.6790504974548,-67.9504729452809));
#9591=CARTESIAN_POINT('Ctrl Pts',(-24.3111776945373,26.6818918322999,-67.9512087014476));
#9592=CARTESIAN_POINT('Ctrl Pts',(-24.3040185244873,26.683622704401,-67.9516640538967));
#9593=CARTESIAN_POINT('Ctrl Pts',(-24.282791797508,26.6886777311922,-67.9530154213757));
#9594=CARTESIAN_POINT('Ctrl Pts',(-24.2687078816998,26.6919317654591,-67.9539136914976));
#9595=CARTESIAN_POINT('Ctrl Pts',(-24.1172557803307,26.7258525288661,-67.963591615875));
#9596=CARTESIAN_POINT('Ctrl Pts',(-23.9780605426976,26.7475793384602,-67.9726583067093));
#9597=CARTESIAN_POINT('Ctrl Pts',(-23.496658752439,26.7907201907011,-68.0045849088361));
#9598=CARTESIAN_POINT('Ctrl Pts',(-23.1527573792706,26.766690978291,-68.0286145521784));
#9599=CARTESIAN_POINT('Ctrl Pts',(-22.8168138996899,26.6884352691511,-68.0504163696479));
#9600=CARTESIAN_POINT('Ctrl Pts',(-22.8145183953754,26.687897891085,-68.0505652477791));
#9601=CARTESIAN_POINT('Ctrl Pts',(-22.7998120974257,26.6844381173085,-68.0515184345704));
#9602=CARTESIAN_POINT('Ctrl Pts',(-22.7874179093343,26.6814445542802,-68.0523189746117));
#9603=CARTESIAN_POINT('Ctrl Pts',(-22.7715065231558,26.6775013994235,-68.053342811172));
#9604=CARTESIAN_POINT('Ctrl Pts',(-22.7679729428501,26.6766193482592,-68.05356993695));
#9605=CARTESIAN_POINT('Ctrl Pts',(-22.7625839280838,26.6752644355901,-68.0539159389616));
#9606=CARTESIAN_POINT('Ctrl Pts',(-22.7607274224574,26.6747959112192,-68.0540350663526));
#9607=CARTESIAN_POINT('Ctrl Pts',(-22.7572457636202,26.6739139474559,-68.0542583436697));
#9608=CARTESIAN_POINT('Ctrl Pts',(-22.7556205214727,26.6735008956411,-68.0543625155747));
#9609=CARTESIAN_POINT('Ctrl Pts',(-22.7518890041494,26.6725494372758,-68.0546015674004));
#9610=CARTESIAN_POINT('Ctrl Pts',(-22.7497829547693,26.67201016886,-68.0547363962404));
#9611=CARTESIAN_POINT('Ctrl Pts',(-22.7439454141031,26.6705091306908,-68.0551098666797));
#9612=CARTESIAN_POINT('Ctrl Pts',(-22.7402150840443,26.669542794756,-68.0553482425941));
#9613=CARTESIAN_POINT('Ctrl Pts',(-22.7197893057333,26.6642124181877,-68.056651999071));
#9614=CARTESIAN_POINT('Ctrl Pts',(-22.703126967369,26.6597209193522,-68.057710068957));
#9615=CARTESIAN_POINT('Ctrl Pts',(-22.514395727657,26.6072168555052,-68.0696408052974));
#9616=CARTESIAN_POINT('Ctrl Pts',(-22.3465420371194,26.5451031631022,-68.0797511401937));
#9617=CARTESIAN_POINT('Ctrl Pts',(-22.1477807606247,26.4521226584926,-68.0920478323319));
#9618=CARTESIAN_POINT('Ctrl Pts',(-22.1112256544791,26.4341693271435,-68.0943230976292));
#9619=CARTESIAN_POINT('Ctrl Pts',(-22.0750358851076,26.4155367075019,-68.0965974740783));
#9620=CARTESIAN_POINT('Ctrl Pts',(-22.0750360157945,26.4155367747871,-68.3458849806668));
#9621=CARTESIAN_POINT('Ctrl Pts',(-22.0784800904417,26.4173099865772,-68.3456505618322));
#9622=CARTESIAN_POINT('Ctrl Pts',(-22.0819274119822,26.4190770143301,-68.3454159240608));
#9623=CARTESIAN_POINT('Ctrl Pts',(-22.1000493232814,26.4283247196044,-68.3441824765203));
#9624=CARTESIAN_POINT('Ctrl Pts',(-22.1147776462151,26.4356988926478,-68.3431800025512));
#9625=CARTESIAN_POINT('Ctrl Pts',(-22.1345180773245,26.4453939805772,-68.3418361501642));
#9626=CARTESIAN_POINT('Ctrl Pts',(-22.1394807380538,26.4478154732018,-68.3414982920684));
#9627=CARTESIAN_POINT('Ctrl Pts',(-22.1477066037292,26.451803079866,-68.3409382335229));
#9628=CARTESIAN_POINT('Ctrl Pts',(-22.1509662810733,26.4533764788072,-68.340716287486));
#9629=CARTESIAN_POINT('Ctrl Pts',(-22.1572895536721,26.4564155068332,-68.3402857225853));
#9630=CARTESIAN_POINT('Ctrl Pts',(-22.1603528298417,26.4578817919093,-68.3400771269128));
#9631=CARTESIAN_POINT('Ctrl Pts',(-22.167433093088,26.4612571251992,-68.3395949643483));
#9632=CARTESIAN_POINT('Ctrl Pts',(-22.1714517188969,26.4631627022122,-68.339321277289));
#9633=CARTESIAN_POINT('Ctrl Pts',(-22.1843408556698,26.4692419049337,-68.3384433930214));
#9634=CARTESIAN_POINT('Ctrl Pts',(-22.193226406766,26.4733833465295,-68.3378380818868));
#9635=CARTESIAN_POINT('Ctrl Pts',(-22.2739725679157,26.5105705876087,-68.3323361470576));
#9636=CARTESIAN_POINT('Ctrl Pts',(-22.3470024779112,26.5409984354011,-68.3273499512269));
#9637=CARTESIAN_POINT('Ctrl Pts',(-22.6564194201477,26.6567488357286,-68.3061548249634));
#9638=CARTESIAN_POINT('Ctrl Pts',(-22.9012234463537,26.7169508790242,-68.2891287255201));
#9639=CARTESIAN_POINT('Ctrl Pts',(-23.3228565381973,26.7696603634558,-68.2604080780132));
#9640=CARTESIAN_POINT('Ctrl Pts',(-23.4967179673015,26.7772396510975,-68.2487643023647));
#9641=CARTESIAN_POINT('Ctrl Pts',(-23.6808931592916,26.770370797301,-68.2371622998617));
#9642=CARTESIAN_POINT('Ctrl Pts',(-23.6914223141958,26.769926384422,-68.2365016165205));
#9643=CARTESIAN_POINT('Ctrl Pts',(-23.7051855390367,26.7692778224324,-68.2356415612344));
#9644=CARTESIAN_POINT('Ctrl Pts',(-23.7084215905964,26.7691204395468,-68.2354395997703));
#9645=CARTESIAN_POINT('Ctrl Pts',(-23.7137068327937,26.7688554063312,-68.2351101751449));
#9646=CARTESIAN_POINT('Ctrl Pts',(-23.7157561575824,26.7687506788188,-68.2349825472355));
#9647=CARTESIAN_POINT('Ctrl Pts',(-23.7196890228894,26.7685459297002,-68.2347378190075));
#9648=CARTESIAN_POINT('Ctrl Pts',(-23.7215725700187,26.7684462121119,-68.2346207021154));
#9649=CARTESIAN_POINT('Ctrl Pts',(-23.7259017343548,26.7682132087198,-68.2343517235821));
#9650=CARTESIAN_POINT('Ctrl Pts',(-23.7283472938307,26.7680787882024,-68.2341999263548));
#9651=CARTESIAN_POINT('Ctrl Pts',(-23.7361008319568,26.7676437476764,-68.2337191277751));
#9652=CARTESIAN_POINT('Ctrl Pts',(-23.7414082563328,26.7673327789503,-68.2333907084708));
#9653=CARTESIAN_POINT('Ctrl Pts',(-23.7863714986409,26.7645866626437,-68.2306141261715));
#9654=CARTESIAN_POINT('Ctrl Pts',(-23.8259821122112,26.7614313842311,-68.2282057061306));
#9655=CARTESIAN_POINT('Ctrl Pts',(-23.8728775071728,26.7568216091346,-68.2253883366565));
#9656=CARTESIAN_POINT('Ctrl Pts',(-23.8802261584932,26.7560737261433,-68.2249478383477));
#9657=CARTESIAN_POINT('Ctrl Pts',(-23.8890469371909,26.7551453711082,-68.2244202191382));
#9658=CARTESIAN_POINT('Ctrl Pts',(-23.8905215303371,26.7549891464438,-68.2243320533106));
#9659=CARTESIAN_POINT('Ctrl Pts',(-23.9024548386151,26.7537165518442,-68.2236188628334));
#9660=CARTESIAN_POINT('Ctrl Pts',(-23.9129082593774,26.7525499916206,-68.2229959902271));
#9661=CARTESIAN_POINT('Ctrl Pts',(-23.9283451153248,26.750750741518,-68.2220787008993));
#9662=CARTESIAN_POINT('Ctrl Pts',(-23.9333329860731,26.7501575551131,-68.2217827012626));
#9663=CARTESIAN_POINT('Ctrl Pts',(-23.9709267436019,26.7455975282852,-68.2195545453931));
#9664=CARTESIAN_POINT('Ctrl Pts',(-24.0034726606456,26.7411439569627,-68.2176414698609));
#9665=CARTESIAN_POINT('Ctrl Pts',(-24.3250060409816,26.6921265413384,-68.1988499944521));
#9666=CARTESIAN_POINT('Ctrl Pts',(-24.6067325817623,26.6089269571759,-68.1831276867525));
#9667=CARTESIAN_POINT('Ctrl Pts',(-24.9734276884765,26.4438189216082,-68.1599211303569));
#9668=CARTESIAN_POINT('Ctrl Pts',(-25.0710904728618,26.3937014967322,-68.1534605827957));
#9669=CARTESIAN_POINT('Ctrl Pts',(-25.18225261423,26.3292894300583,-68.1456822957136));
#9670=CARTESIAN_POINT('Ctrl Pts',(-25.198421245754,26.319730861378,-68.1445401007965));
#9671=CARTESIAN_POINT('Ctrl Pts',(-25.2194747788549,26.3070347738638,-68.1430382390958));
#9672=CARTESIAN_POINT('Ctrl Pts',(-25.2244362908768,26.3040244868406,-68.1426832387379));
#9673=CARTESIAN_POINT('Ctrl Pts',(-25.2325335867233,26.2990816610022,-68.1421021091637));
#9674=CARTESIAN_POINT('Ctrl Pts',(-25.2356742510349,26.297157109221,-68.1418762741044));
#9675=CARTESIAN_POINT('Ctrl Pts',(-25.2416854406524,26.2934593524039,-68.141443191835));
#9676=CARTESIAN_POINT('Ctrl Pts',(-25.2445564958741,26.2916870145009,-68.1412359768192));
#9677=CARTESIAN_POINT('Ctrl Pts',(-25.2510842204731,26.2876431979735,-68.1407640074133));
#9678=CARTESIAN_POINT('Ctrl Pts',(-25.2547391270093,26.2853688984127,-68.1404991489235));
#9679=CARTESIAN_POINT('Ctrl Pts',(-25.2660644041576,26.2782901228092,-68.1396765725892));
#9680=CARTESIAN_POINT('Ctrl Pts',(-25.2737190501793,26.2734606833423,-68.1391179296153));
#9681=CARTESIAN_POINT('Ctrl Pts',(-25.3316843564147,26.236547148918,-68.1348670737323));
#9682=CARTESIAN_POINT('Ctrl Pts',(-25.3811126830478,26.2031054210016,-68.1311242991763));
#9683=CARTESIAN_POINT('Ctrl Pts',(-25.6985041993822,25.9752714099105,-68.1062808534322));
#9684=CARTESIAN_POINT('Ctrl Pts',(-25.9360447515623,25.7419650368599,-68.0835106180908));
#9685=CARTESIAN_POINT('Ctrl Pts',(-26.2058460910446,25.3801296670172,-68.0533429093268));
#9686=CARTESIAN_POINT('Ctrl Pts',(-26.2723901226845,25.2795882198733,-68.0454351638608));
#9687=CARTESIAN_POINT('Ctrl Pts',(-26.3363334801124,25.170101365381,-68.0374888059718));
#9688=CARTESIAN_POINT('Ctrl Pts',(-26.3394964476948,25.1646489123233,-68.0370947555206));
#9689=CARTESIAN_POINT('Ctrl Pts',(-26.3439687554558,25.1568869863472,-68.0365362194115));
#9690=CARTESIAN_POINT('Ctrl Pts',(-26.3452912447253,25.1545851663327,-68.0363708856159));
#9691=CARTESIAN_POINT('Ctrl Pts',(-26.3475621455862,25.1506212855754,-68.036086692442));
#9692=CARTESIAN_POINT('Ctrl Pts',(-26.3485119222728,25.1489600119676,-68.0359677438524));
#9693=CARTESIAN_POINT('Ctrl Pts',(-26.3503298791325,25.1457736035065,-68.0357398976184));
#9694=CARTESIAN_POINT('Ctrl Pts',(-26.3511982918493,25.1442486078939,-68.0356309846625));
#9695=CARTESIAN_POINT('Ctrl Pts',(-26.3532422838618,25.1406523819512,-68.0353744586498));
#9696=CARTESIAN_POINT('Ctrl Pts',(-26.3544168156778,25.1385805529072,-68.0352269139529));
#9697=CARTESIAN_POINT('Ctrl Pts',(-26.3578825924931,25.1324512288149,-68.0347911282637));
#9698=CARTESIAN_POINT('Ctrl Pts',(-26.3601673479413,25.1283900420373,-68.0345033057377));
#9699=CARTESIAN_POINT('Ctrl Pts',(-26.3801109719946,25.0927593347981,-68.0319860424262));
#9700=CARTESIAN_POINT('Ctrl Pts',(-26.3972468705161,25.0608979347183,-68.029789605925));
#9701=CARTESIAN_POINT('Ctrl Pts',(-26.5523131082429,24.7605623935644,-68.0095265364863));
#9702=CARTESIAN_POINT('Ctrl Pts',(-26.6524414014193,24.4742113244679,-67.9933497485836));
#9703=CARTESIAN_POINT('Ctrl Pts',(-26.7323108665828,24.072076712465,-67.9700912053233));
#9704=CARTESIAN_POINT('Ctrl Pts',(-26.7480167369792,23.9650980305409,-67.9638691624895));
#9705=CARTESIAN_POINT('Ctrl Pts',(-26.7647437242686,23.7904683663333,-67.95350672074));
#9706=CARTESIAN_POINT('Ctrl Pts',(-26.7690627938796,23.723217138511,-67.9494678271452));
#9707=CARTESIAN_POINT('Ctrl Pts',(-26.7715497343834,23.6473825387869,-67.9448431257346));
#9708=CARTESIAN_POINT('Ctrl Pts',(-26.7717948598616,23.6388805857829,-67.9443236565793));
#9709=CARTESIAN_POINT('Ctrl Pts',(-26.7721118002692,23.6261367453701,-67.9435434989027));
#9710=CARTESIAN_POINT('Ctrl Pts',(-26.7722089014323,23.6218954770629,-67.9432836047076));
#9711=CARTESIAN_POINT('Ctrl Pts',(-26.7723612634414,23.6146120016928,-67.9428368573164));
#9712=CARTESIAN_POINT('Ctrl Pts',(-26.7724205911742,23.6115698778603,-67.9426501320736));
#9713=CARTESIAN_POINT('Ctrl Pts',(-26.7725337133575,23.6053149836192,-67.9422659379238));
#9714=CARTESIAN_POINT('Ctrl Pts',(-26.7725870112654,23.6021022082078,-67.9420684536102));
#9715=CARTESIAN_POINT('Ctrl Pts',(-26.7727035004709,23.5943843371599,-67.9415936946047));
#9716=CARTESIAN_POINT('Ctrl Pts',(-26.7727620491826,23.5898791868663,-67.9413162743871));
#9717=CARTESIAN_POINT('Ctrl Pts',(-26.772940640945,23.5734925341815,-67.9403061474606));
#9718=CARTESIAN_POINT('Ctrl Pts',(-26.7730044201929,23.5616106268333,-67.9395716764783));
#9719=CARTESIAN_POINT('Ctrl Pts',(-26.7729724555403,23.3649313425468,-67.9273797248113));
#9720=CARTESIAN_POINT('Ctrl Pts',(-26.7570482654972,23.1805131479998,-67.9154146073358));
#9721=CARTESIAN_POINT('Ctrl Pts',(-26.6724960515322,22.6939394884019,-67.88249156417));
#9722=CARTESIAN_POINT('Ctrl Pts',(-26.5760327321624,22.3985878083025,-67.8609585946284));
#9723=CARTESIAN_POINT('Ctrl Pts',(-26.431766003029,22.1069012557221,-67.8403630474853));
#9724=CARTESIAN_POINT('Ctrl Pts',(-26.4244352069993,22.0923578966375,-67.8393385293104));
#9725=CARTESIAN_POINT('Ctrl Pts',(-26.4153530307913,22.0746748150265,-67.8380963028427));
#9726=CARTESIAN_POINT('Ctrl Pts',(-26.4137064133397,22.0714819829437,-67.8378721471503));
#9727=CARTESIAN_POINT('Ctrl Pts',(-26.4109843098647,22.0662253514631,-67.8375033380698));
#9728=CARTESIAN_POINT('Ctrl Pts',(-26.4099119269796,22.0641599634715,-67.8373584894936));
#9729=CARTESIAN_POINT('Ctrl Pts',(-26.4079751125296,22.060439556932,-67.8370976838086));
#9730=CARTESIAN_POINT('Ctrl Pts',(-26.4071114818975,22.058784131932,-67.8369816762687));
#9731=CARTESIAN_POINT('Ctrl Pts',(-26.4052521303924,22.0552276290854,-67.836732533029));
#9732=CARTESIAN_POINT('Ctrl Pts',(-26.4042559519176,22.0533268002683,-67.8365994273819));
#9733=CARTESIAN_POINT('Ctrl Pts',(-26.4015246290244,22.0481277437843,-67.8362355040214));
#9734=CARTESIAN_POINT('Ctrl Pts',(-26.3997856541154,22.0448315154915,-67.836004930075));
#9735=CARTESIAN_POINT('Ctrl Pts',(-26.3907544838809,22.0277846411699,-67.8348132529836));
#9736=CARTESIAN_POINT('Ctrl Pts',(-26.3833682984153,22.0140836303522,-67.8338580553604));
#9737=CARTESIAN_POINT('Ctrl Pts',(-26.3428082480562,21.9401344009479,-67.8287136258538));
#9738=CARTESIAN_POINT('Ctrl Pts',(-26.3078088799976,21.880901652121,-67.8246330857041));
#9739=CARTESIAN_POINT('Ctrl Pts',(-26.2272503068992,21.7540221538762,-67.8158801878081));
#9740=CARTESIAN_POINT('Ctrl Pts',(-26.1809657664963,21.686892668817,-67.8112408980541));
#9741=CARTESIAN_POINT('Ctrl Pts',(-25.9338895648346,21.3561283728473,-67.7879681945281));
#9742=CARTESIAN_POINT('Ctrl Pts',(-25.695873410596,21.1228657480223,-67.7699206021056));
#9743=CARTESIAN_POINT('Ctrl Pts',(-25.4083276543581,20.9169707138947,-67.7485570882266));
#9744=CARTESIAN_POINT('Ctrl Pts',(-25.3900359432607,20.9041585702133,-67.7472009858479));
#9745=CARTESIAN_POINT('Ctrl Pts',(-25.3662677687759,20.8878761120852,-67.7454420269248));
#9746=CARTESIAN_POINT('Ctrl Pts',(-25.3609116357219,20.8842305608477,-67.745045852273));
#9747=CARTESIAN_POINT('Ctrl Pts',(-25.3523899799521,20.8784679815824,-67.7444158446686));
#9748=CARTESIAN_POINT('Ctrl Pts',(-25.3492316156388,20.876340356629,-67.7441824134903));
#9749=CARTESIAN_POINT('Ctrl Pts',(-25.3433143835967,20.8723694560562,-67.7437451998622));
#9750=CARTESIAN_POINT('Ctrl Pts',(-25.3405564234429,20.8705248316107,-67.7435414687391));
#9751=CARTESIAN_POINT('Ctrl Pts',(-25.3343460849178,20.8663849971854,-67.7430828185093));
#9752=CARTESIAN_POINT('Ctrl Pts',(-25.330892121227,20.8640921862613,-67.7428278094452));
#9753=CARTESIAN_POINT('Ctrl Pts',(-25.3207299329009,20.8573745333545,-67.7420777415618));
#9754=CARTESIAN_POINT('Ctrl Pts',(-25.3140096071705,20.8529681345723,-67.7415819910714));
#9755=CARTESIAN_POINT('Ctrl Pts',(-25.2639358181646,20.8204027909067,-67.7378900332445));
#9756=CARTESIAN_POINT('Ctrl Pts',(-25.2199290336381,20.7932668787175,-67.7346559114194));
#9757=CARTESIAN_POINT('Ctrl Pts',(-25.0720873538491,20.7069413214544,-67.7238164528791));
#9758=CARTESIAN_POINT('Ctrl Pts',(-24.965623608188,20.6524742558125,-67.7160471172952));
#9759=CARTESIAN_POINT('Ctrl Pts',(-24.5602369249156,20.4727543754862,-67.6866481181042));
#9760=CARTESIAN_POINT('Ctrl Pts',(-24.2460061689139,20.3868719699905,-67.6640112847241));
#9761=CARTESIAN_POINT('Ctrl Pts',(-23.9205661935998,20.3488467147471,-67.6431997757606));
#9762=CARTESIAN_POINT('Ctrl Pts',(-23.9168689506292,20.348421209674,-67.6429637054893));
#9763=CARTESIAN_POINT('Ctrl Pts',(-23.8976629752918,20.3462445521866,-67.6417393166993));
#9764=CARTESIAN_POINT('Ctrl Pts',(-23.8821420563685,20.344599631626,-67.6407563498027));
#9765=CARTESIAN_POINT('Ctrl Pts',(-23.8620262347386,20.3426154059132,-67.6394913228578));
#9766=CARTESIAN_POINT('Ctrl Pts',(-23.857442037681,20.3421731404327,-67.6392036365385));
#9767=CARTESIAN_POINT('Ctrl Pts',(-23.8504997194681,20.3415183896475,-67.6387688894562));
#9768=CARTESIAN_POINT('Ctrl Pts',(-23.8481423107699,20.3412986760408,-67.6386214235823));
#9769=CARTESIAN_POINT('Ctrl Pts',(-23.8440406582373,20.3409209554131,-67.6383651314467));
#9770=CARTESIAN_POINT('Ctrl Pts',(-23.8422965279682,20.3407617723856,-67.6382562384827));
#9771=CARTESIAN_POINT('Ctrl Pts',(-23.8386433609161,20.3404313581955,-67.6380283447823));
#9772=CARTESIAN_POINT('Ctrl Pts',(-23.8367343020654,20.3402604084193,-67.6379093605524));
#9773=CARTESIAN_POINT('Ctrl Pts',(-23.8322179210524,20.3398600428479,-67.6376281243656));
#9774=CARTESIAN_POINT('Ctrl Pts',(-23.8296104621964,20.3396320994384,-67.637465956101));
#9775=CARTESIAN_POINT('Ctrl Pts',(-23.8208947780506,20.3388808744318,-67.6369245488817));
#9776=CARTESIAN_POINT('Ctrl Pts',(-23.8147852894696,20.3383718414899,-67.6365461117739));
#9777=CARTESIAN_POINT('Ctrl Pts',(-23.8002712315641,20.3372042467812,-67.6356495520246));
#9778=CARTESIAN_POINT('Ctrl Pts',(-23.7918654087687,20.3365612190829,-67.6351322810191));
#9779=CARTESIAN_POINT('Ctrl Pts',(-23.4893182597477,20.3146107686271,-67.6165821986766));
#9780=CARTESIAN_POINT('Ctrl Pts',(-23.1935848608708,20.3337409499986,-67.6006669207868));
#9781=CARTESIAN_POINT('Ctrl Pts',(-22.7062875388641,20.4333969679613,-67.5726752017353));
#9782=CARTESIAN_POINT('Ctrl Pts',(-22.5123262064374,20.492515493757,-67.5610422136581));
#9783=CARTESIAN_POINT('Ctrl Pts',(-22.3135573905142,20.5742046137529,-67.5479834331375));
#9784=CARTESIAN_POINT('Ctrl Pts',(-22.3019403161464,20.5790587164807,-67.5472160717762));
#9785=CARTESIAN_POINT('Ctrl Pts',(-22.2861013960118,20.5857861721426,-67.5461640681359));
#9786=CARTESIAN_POINT('Ctrl Pts',(-22.2818545838601,20.5876007572986,-67.5458814302069));
#9787=CARTESIAN_POINT('Ctrl Pts',(-22.2746314761734,20.5907054366342,-67.5453997352248));
#9788=CARTESIAN_POINT('Ctrl Pts',(-22.271653192098,20.5919909114457,-67.5452008362138));
#9789=CARTESIAN_POINT('Ctrl Pts',(-22.2658949725214,20.5944865708474,-67.5448157344249));
#9790=CARTESIAN_POINT('Ctrl Pts',(-22.2631147934568,20.5956961863503,-67.5446295513194));
#9791=CARTESIAN_POINT('Ctrl Pts',(-22.2565194612862,20.5985767953232,-67.5441872824828));
#9792=CARTESIAN_POINT('Ctrl Pts',(-22.2527058394233,20.6002512619884,-67.5439310778709));
#9793=CARTESIAN_POINT('Ctrl Pts',(-22.2414586774558,20.6052156404535,-67.5431740785274));
#9794=CARTESIAN_POINT('Ctrl Pts',(-22.2340343680099,20.6085262719434,-67.5426725725559));
#9795=CARTESIAN_POINT('Ctrl Pts',(-22.1772312105312,20.6341138944913,-67.5388215791154));
#9796=CARTESIAN_POINT('Ctrl Pts',(-22.1284111481715,20.6576034685148,-67.5354303922328));
#9797=CARTESIAN_POINT('Ctrl Pts',(-21.9655303438327,20.7410926039189,-67.5238280683185));
#9798=CARTESIAN_POINT('Ctrl Pts',(-21.8544946713792,20.8066923947994,-67.5154239235716));
#9799=CARTESIAN_POINT('Ctrl Pts',(-21.5467146396444,21.0143629943626,-67.4907232530375));
#9800=CARTESIAN_POINT('Ctrl Pts',(-21.3616936751148,21.1722068188466,-67.4740247324406));
#9801=CARTESIAN_POINT('Ctrl Pts',(-21.1370673056003,21.4124656417287,-67.4523018067626));
#9802=CARTESIAN_POINT('Ctrl Pts',(-21.0805687684105,21.4779926534535,-67.4466948514009));
#9803=CARTESIAN_POINT('Ctrl Pts',(-21.0228159398043,21.5506970211882,-67.4408744017903));
#9804=CARTESIAN_POINT('Ctrl Pts',(-21.0188770221142,21.555685912914,-67.440476962787));
#9805=CARTESIAN_POINT('Ctrl Pts',(-21.0134290174882,21.5626282933148,-67.4399266446035));
#9806=CARTESIAN_POINT('Ctrl Pts',(-21.0119074094616,21.5645718686067,-67.4397728760596));
#9807=CARTESIAN_POINT('Ctrl Pts',(-21.0092938988829,21.5679180623408,-67.4395086515489));
#9808=CARTESIAN_POINT('Ctrl Pts',(-21.0082009240872,21.5693198356284,-67.4393981185718));
#9809=CARTESIAN_POINT('Ctrl Pts',(-21.0059436617677,21.5722197875276,-67.4391697720245));
#9810=CARTESIAN_POINT('Ctrl Pts',(-21.0047795396782,21.5737180873919,-67.4390519707571));
#9811=CARTESIAN_POINT('Ctrl Pts',(-21.002077877186,21.5772016459136,-67.4387784911596));
#9812=CARTESIAN_POINT('Ctrl Pts',(-21.0005413286407,21.5791876801776,-67.438622884126));
#9813=CARTESIAN_POINT('Ctrl Pts',(-20.9956101654458,21.585576768818,-67.4381232773985));
#9814=CARTESIAN_POINT('Ctrl Pts',(-20.9922245991069,21.5899868431047,-67.4377799203959));
#9815=CARTESIAN_POINT('Ctrl Pts',(-20.9843252167714,21.6003319755168,-67.4369779149572));
#9816=CARTESIAN_POINT('Ctrl Pts',(-20.9798205305044,21.6062740105482,-67.4365198967684));
#9817=CARTESIAN_POINT('Ctrl Pts',(-20.9325757480855,21.6690449299231,-67.431708537571));
#9818=CARTESIAN_POINT('Ctrl Pts',(-20.8917032761629,21.7272628456203,-67.4274792581145));
#9819=CARTESIAN_POINT('Ctrl Pts',(-20.7463138654006,21.9496565464433,-67.4119816426558));
#9820=CARTESIAN_POINT('Ctrl Pts',(-20.6548005518103,22.1218442828833,-67.4012533462879));
#9821=CARTESIAN_POINT('Ctrl Pts',(-20.4900276155911,22.5137725959933,-67.3774436502248));
#9822=CARTESIAN_POINT('Ctrl Pts',(-20.4237548263139,22.7352334912072,-67.3643312298726));
#9823=CARTESIAN_POINT('Ctrl Pts',(-20.3790195206746,22.9761359468739,-67.3494608389825));
#9824=CARTESIAN_POINT('Ctrl Pts',(-20.3764634650916,22.9904386223948,-67.3485760215916));
#9825=CARTESIAN_POINT('Ctrl Pts',(-20.3730818253398,23.0101288761372,-67.3473550828118));
#9826=CARTESIAN_POINT('Ctrl Pts',(-20.3721730355804,23.0155021446788,-67.3470216125165));
#9827=CARTESIAN_POINT('Ctrl Pts',(-20.3707487905723,23.0240549473731,-67.3464903495333));
#9828=CARTESIAN_POINT('Ctrl Pts',(-20.370224462968,23.0272330105053,-67.3462928393996));
#9829=CARTESIAN_POINT('Ctrl Pts',(-20.3692145899599,23.0334117288786,-67.3459086431043));
#9830=CARTESIAN_POINT('Ctrl Pts',(-20.368728523456,23.0364122966847,-67.3457219737242));
#9831=CARTESIAN_POINT('Ctrl Pts',(-20.3675775344247,23.0435817842597,-67.3452757275852));
#9832=CARTESIAN_POINT('Ctrl Pts',(-20.3669165581984,23.0477513236105,-67.345016025713));
#9833=CARTESIAN_POINT('Ctrl Pts',(-20.364964341459,23.0602246468661,-67.3442385743345));
#9834=CARTESIAN_POINT('Ctrl Pts',(-20.3636973930665,23.0685321469252,-67.3437200542545));
#9835=CARTESIAN_POINT('Ctrl Pts',(-20.3532573399508,23.1388323664442,-67.3393259684584));
#9836=CARTESIAN_POINT('Ctrl Pts',(-20.3458623071218,23.2010717693076,-67.3353943454099));
#9837=CARTESIAN_POINT('Ctrl Pts',(-20.3317768545752,23.358738287029,-67.3253200568328));
#9838=CARTESIAN_POINT('Ctrl Pts',(-20.3275119781658,23.4543159449296,-67.3191063655647));
#9839=CARTESIAN_POINT('Ctrl Pts',(-20.3274812262668,23.7661090666804,-67.2985136376937));
#9840=CARTESIAN_POINT('Ctrl Pts',(-20.3492114590003,23.9817287369676,-67.2837255805823));
#9841=CARTESIAN_POINT('Ctrl Pts',(-20.4075866607376,24.2683001928947,-67.2640922445584));
#9842=CARTESIAN_POINT('Ctrl Pts',(-20.4254711337805,24.3425175424531,-67.2590152556615));
#9843=CARTESIAN_POINT('Ctrl Pts',(-20.4499336198544,24.4302283029197,-67.2530740826799));
#9844=CARTESIAN_POINT('Ctrl Pts',(-20.4539897844793,24.4443955449898,-67.2521163278671));
#9845=CARTESIAN_POINT('Ctrl Pts',(-20.4584434809282,24.4595574818779,-67.2510936950582));
#9846=CARTESIAN_POINT('Ctrl Pts',(-20.4587444205512,24.4605801087623,-67.2510247331369));
#9847=CARTESIAN_POINT('Ctrl Pts',(-20.4598796893785,24.4644308251162,-67.2507651000937));
#9848=CARTESIAN_POINT('Ctrl Pts',(-20.4607173949955,24.4672579274898,-67.2505745733691));
#9849=CARTESIAN_POINT('Ctrl Pts',(-20.4620317087834,24.4716712501025,-67.2502772906579));
#9850=CARTESIAN_POINT('Ctrl Pts',(-20.4625056597182,24.4732582523257,-67.2501704188354));
#9851=CARTESIAN_POINT('Ctrl Pts',(-20.4637647093861,24.4774622978841,-67.2498873886278));
#9852=CARTESIAN_POINT('Ctrl Pts',(-20.4645519149317,24.4800787152306,-67.249711323339));
#9853=CARTESIAN_POINT('Ctrl Pts',(-20.4766938118817,24.5202492310955,-67.2470094188855));
#9854=CARTESIAN_POINT('Ctrl Pts',(-20.4887306640684,24.557596068969,-67.2445144727868));
#9855=CARTESIAN_POINT('Ctrl Pts',(-20.5029930314779,24.5992281518378,-67.2417597158957));
#9856=CARTESIAN_POINT('Ctrl Pts',(-20.5045489007792,24.6037370862277,-67.241461714977));
#9857=CARTESIAN_POINT('Ctrl Pts',(-20.5069058677466,24.6105187493381,-67.2410140535087));
#9858=CARTESIAN_POINT('Ctrl Pts',(-20.507699504782,24.6127940357109,-67.2408639533456));
#9859=CARTESIAN_POINT('Ctrl Pts',(-20.5090779171421,24.6167316132686,-67.2406043555559));
#9860=CARTESIAN_POINT('Ctrl Pts',(-20.5096615037599,24.6183943146574,-67.240494786963));
#9861=CARTESIAN_POINT('Ctrl Pts',(-20.5108797626747,24.6218561772695,-67.2402667637747));
#9862=CARTESIAN_POINT('Ctrl Pts',(-20.5115146681793,24.6236552516118,-67.2401483238742));
#9863=CARTESIAN_POINT('Ctrl Pts',(-20.5127814154034,24.6272345875969,-67.239912800371));
#9864=CARTESIAN_POINT('Ctrl Pts',(-20.5134132263574,24.6290148617016,-67.2397957147644));
#9865=CARTESIAN_POINT('Ctrl Pts',(-20.5155889250968,24.6351283390905,-67.2393938377594));
#9866=CARTESIAN_POINT('Ctrl Pts',(-20.5171405343001,24.6394588182017,-67.2391095068396));
#9867=CARTESIAN_POINT('Ctrl Pts',(-20.5299441892682,24.6749537855123,-67.2367816393382));
#9868=CARTESIAN_POINT('Ctrl Pts',(-20.5416674876997,24.7059478360198,-67.2347658146481));
#9869=CARTESIAN_POINT('Ctrl Pts',(-20.5853844978037,24.816350287395,-67.2276273370274));
#9870=CARTESIAN_POINT('Ctrl Pts',(-20.6200633509712,24.8946631223495,-67.2226420781215));
#9871=CARTESIAN_POINT('Ctrl Pts',(-20.7224673267849,25.1030678141482,-67.209352287892));
#9872=CARTESIAN_POINT('Ctrl Pts',(-20.7960152118884,25.2300695081362,-67.2012221498421));
#9873=CARTESIAN_POINT('Ctrl Pts',(-20.9492551310031,25.4573972048921,-67.1858836133517));
#9874=CARTESIAN_POINT('Ctrl Pts',(-21.0267669136445,25.5588355234877,-67.1787068237312));
#9875=CARTESIAN_POINT('Ctrl Pts',(-21.186853587769,25.744398397129,-67.1645497882724));
#9876=CARTESIAN_POINT('Ctrl Pts',(-21.2684278439646,25.8291123010345,-67.1576097116778));
#9877=CARTESIAN_POINT('Ctrl Pts',(-21.3622113556713,25.9164110477373,-67.1498133925124));
#9878=CARTESIAN_POINT('Ctrl Pts',(-21.3700191669768,25.9236072843914,-67.149165656741));
#9879=CARTESIAN_POINT('Ctrl Pts',(-21.3810342056437,25.9336593068333,-67.1482536562228));
#9880=CARTESIAN_POINT('Ctrl Pts',(-21.3842118546138,25.9365475232648,-67.1479907692776));
#9881=CARTESIAN_POINT('Ctrl Pts',(-21.3897361276291,25.9415484984581,-67.1475341043721));
#9882=CARTESIAN_POINT('Ctrl Pts',(-21.3920801077105,25.9436641806056,-67.1473404503256));
#9883=CARTESIAN_POINT('Ctrl Pts',(-21.3969636858578,25.9480591030036,-67.146937210183));
#9884=CARTESIAN_POINT('Ctrl Pts',(-21.3995038008015,25.9503377600644,-67.1467275999003));
#9885=CARTESIAN_POINT('Ctrl Pts',(-21.4054935856725,25.9556938626975,-67.1462336223557));
#9886=CARTESIAN_POINT('Ctrl Pts',(-21.4089462608603,25.9587679224631,-67.1459491133352));
#9887=CARTESIAN_POINT('Ctrl Pts',(-21.4202562563183,25.9687941376048,-67.1450178925139));
#9888=CARTESIAN_POINT('Ctrl Pts',(-21.42814085088,25.9757153004477,-67.1443698862664));
#9889=CARTESIAN_POINT('Ctrl Pts',(-21.4466447157441,25.9917988523318,-67.1428517927588));
#9890=CARTESIAN_POINT('Ctrl Pts',(-21.4572902201461,26.0009306075651,-67.1419804491104));
#9891=CARTESIAN_POINT('Ctrl Pts',(-21.4942860978958,26.0322489388862,-67.1389590701081));
#9892=CARTESIAN_POINT('Ctrl Pts',(-21.5209316187593,26.0540817243844,-67.1367946954634));
#9893=CARTESIAN_POINT('Ctrl Pts',(-21.6431555301754,26.1509967653548,-67.1269160036735));
#9894=CARTESIAN_POINT('Ctrl Pts',(-21.7425745621809,26.2210546553216,-67.1190091605272));
#9895=CARTESIAN_POINT('Ctrl Pts',(-21.9203700980134,26.3318602657314,-67.1051092180637));
#9896=CARTESIAN_POINT('Ctrl Pts',(-21.9968806582552,26.3752978175026,-67.0991996102356));
#9897=CARTESIAN_POINT('Ctrl Pts',(-22.0750362583504,26.4155368996692,-67.093261398997));
#9898=CARTESIAN_POINT('Origin',(-23.5502525316942,23.5502525316942,-77.3107734492734));
#9899=CARTESIAN_POINT('',(-22.0750359980476,26.41553676565,-65.5942565421953));
#9900=CARTESIAN_POINT('',(-22.0750360187516,26.4155367763096,-65.8398919625532));
#9901=CARTESIAN_POINT('',(-22.0750360153461,26.4155367745563,-77.3107734492734));
#9902=CARTESIAN_POINT('',(-26.7730026852622,23.5520333435677,-66.4414554149513));
#9903=CARTESIAN_POINT('Ctrl Pts',(-22.0750359980476,26.41553676565,-65.5942565421953));
#9904=CARTESIAN_POINT('Ctrl Pts',(-22.0582209726656,26.4068794034368,-65.5955036844597));
#9905=CARTESIAN_POINT('Ctrl Pts',(-22.0414809647859,26.3980734084878,-65.5967547895065));
#9906=CARTESIAN_POINT('Ctrl Pts',(-21.7587436008458,26.2461475428026,-65.6180454325648));
#9907=CARTESIAN_POINT('Ctrl Pts',(-21.5141120649862,26.0664943349157,-65.6390626962724));
#9908=CARTESIAN_POINT('Ctrl Pts',(-21.2701080519116,25.8280996323232,-65.6610241028595));
#9909=CARTESIAN_POINT('Ctrl Pts',(-21.2426395348813,25.8002678345547,-65.6635103461838));
#9910=CARTESIAN_POINT('Ctrl Pts',(-21.2120810939885,25.7681567648208,-65.666285134475));
#9911=CARTESIAN_POINT('Ctrl Pts',(-21.2084885232806,25.764363231103,-65.6666114914255));
#9912=CARTESIAN_POINT('Ctrl Pts',(-21.2032117580814,25.7587640815493,-65.6670910308153));
#9913=CARTESIAN_POINT('Ctrl Pts',(-21.2015204111308,25.7569652644205,-65.6672447646115));
#9914=CARTESIAN_POINT('Ctrl Pts',(-21.1985385975009,25.7537866710393,-65.6675158416826));
#9915=CARTESIAN_POINT('Ctrl Pts',(-21.197247275747,25.7524077026796,-65.6676332515294));
#9916=CARTESIAN_POINT('Ctrl Pts',(-21.1945903197741,25.7495654044041,-65.6678748589556));
#9917=CARTESIAN_POINT('Ctrl Pts',(-21.1932248390091,25.7481019407083,-65.6679990446844));
#9918=CARTESIAN_POINT('Ctrl Pts',(-21.1897070267681,25.7443246517358,-65.6683190248789));
#9919=CARTESIAN_POINT('Ctrl Pts',(-21.1875567270587,25.7420089241184,-65.6685146619978));
#9920=CARTESIAN_POINT('Ctrl Pts',(-21.1828832046859,25.7369609858585,-65.6689399751534));
#9921=CARTESIAN_POINT('Ctrl Pts',(-21.1803612943494,25.7342275584416,-65.6691695512294));
#9922=CARTESIAN_POINT('Ctrl Pts',(-21.1730617245074,25.7262882289616,-65.6698342750738));
#9923=CARTESIAN_POINT('Ctrl Pts',(-21.1682964099864,25.7210709317426,-65.6702685014859));
#9924=CARTESIAN_POINT('Ctrl Pts',(-21.0559203874699,25.5972206633023,-65.6805163302563));
#9925=CARTESIAN_POINT('Ctrl Pts',(-20.9572680900283,25.4707260156077,-65.689688718354));
#9926=CARTESIAN_POINT('Ctrl Pts',(-20.7262480933336,25.1240528382958,-65.7131492052165));
#9927=CARTESIAN_POINT('Ctrl Pts',(-20.6100488272049,24.8945168092446,-65.7271874896071));
#9928=CARTESIAN_POINT('Ctrl Pts',(-20.5148784801808,24.6333446197269,-65.7434505356548));
#9929=CARTESIAN_POINT('Ctrl Pts',(-20.5076876810741,24.6129769566681,-65.7447199638977));
#9930=CARTESIAN_POINT('Ctrl Pts',(-20.4990934454001,24.5878317038046,-65.7462893152019));
#9931=CARTESIAN_POINT('Ctrl Pts',(-20.4974955196083,24.5831208355218,-65.7465834196329));
#9932=CARTESIAN_POINT('Ctrl Pts',(-20.4946397806468,24.5746372706644,-65.7471132361183));
#9933=CARTESIAN_POINT('Ctrl Pts',(-20.4933780294012,24.5708659035602,-65.7473488293377));
#9934=CARTESIAN_POINT('Ctrl Pts',(-20.4879152975852,24.5544368241394,-65.7483754271492));
#9935=CARTESIAN_POINT('Ctrl Pts',(-20.4837859731803,24.5417555657204,-65.7491685882956));
#9936=CARTESIAN_POINT('Ctrl Pts',(-20.4790081943181,24.5267675175551,-65.7501070623543));
#9937=CARTESIAN_POINT('Ctrl Pts',(-20.4782834089402,24.5244850533629,-65.7502500066031));
#9938=CARTESIAN_POINT('Ctrl Pts',(-20.476806263114,24.5198152486466,-65.7505425221624));
#9939=CARTESIAN_POINT('Ctrl Pts',(-20.4760541387286,24.5174278356541,-65.7506921006782));
#9940=CARTESIAN_POINT('Ctrl Pts',(-20.4733513365484,24.5088135246728,-65.7512319291571));
#9941=CARTESIAN_POINT('Ctrl Pts',(-20.4714167995651,24.5025816111569,-65.7516226802922));
#9942=CARTESIAN_POINT('Ctrl Pts',(-20.4675380249681,24.4899511820378,-65.7524150990565));
#9943=CARTESIAN_POINT('Ctrl Pts',(-20.4655947506359,24.4835524064316,-65.7528167946758));
#9944=CARTESIAN_POINT('Ctrl Pts',(-20.4558425973306,24.4510775221143,-65.7548567732224));
#9945=CARTESIAN_POINT('Ctrl Pts',(-20.4483445770606,24.4249098796529,-65.7565048206926));
#9946=CARTESIAN_POINT('Ctrl Pts',(-20.4389348735107,24.3904267205913,-65.7586832493702));
#9947=CARTESIAN_POINT('Ctrl Pts',(-20.4367233058081,24.3821936324742,-65.7592038590087));
#9948=CARTESIAN_POINT('Ctrl Pts',(-20.4334440470817,24.3697895771016,-65.7599889918));
#9949=CARTESIAN_POINT('Ctrl Pts',(-20.4323519930396,24.3656250412377,-65.7602527236829));
#9950=CARTESIAN_POINT('Ctrl Pts',(-20.4304213776608,24.358202068131,-65.7607230448587));
#9951=CARTESIAN_POINT('Ctrl Pts',(-20.4295795662572,24.3549444763286,-65.7609295284191));
#9952=CARTESIAN_POINT('Ctrl Pts',(-20.4278178390746,24.3480827073556,-65.7613646387786));
#9953=CARTESIAN_POINT('Ctrl Pts',(-20.4268990593167,24.3444782460052,-65.7615933020424));
#9954=CARTESIAN_POINT('Ctrl Pts',(-20.4244938665298,24.3349737241332,-65.7621965303873));
#9955=CARTESIAN_POINT('Ctrl Pts',(-20.4230179234487,24.3290710515639,-65.762571433735));
#9956=CARTESIAN_POINT('Ctrl Pts',(-20.4164659850116,24.3025492530772,-65.7642572089972));
#9957=CARTESIAN_POINT('Ctrl Pts',(-20.4115772316131,24.2818848184839,-65.7655741141248));
#9958=CARTESIAN_POINT('Ctrl Pts',(-20.3775478617192,24.1314229903325,-65.7751893818957));
#9959=CARTESIAN_POINT('Ctrl Pts',(-20.3562682103828,23.9999969096772,-65.7837398180584));
#9960=CARTESIAN_POINT('Ctrl Pts',(-20.3100028549861,23.5325117224265,-65.8146838240708));
#9961=CARTESIAN_POINT('Ctrl Pts',(-20.3295699811221,23.1942970741518,-65.8382653709866));
#9962=CARTESIAN_POINT('Ctrl Pts',(-20.4027425255166,22.8578977068628,-65.8602502824653));
#9963=CARTESIAN_POINT('Ctrl Pts',(-20.4043714099219,22.8505337220397,-65.8607306730568));
#9964=CARTESIAN_POINT('Ctrl Pts',(-20.4097524865003,22.8266051811846,-65.8622886669215));
#9965=CARTESIAN_POINT('Ctrl Pts',(-20.4136098529752,22.8100642061375,-65.8633609919435));
#9966=CARTESIAN_POINT('Ctrl Pts',(-20.4191689596851,22.7870500697052,-65.8648457123287));
#9967=CARTESIAN_POINT('Ctrl Pts',(-20.420760284114,22.7805508965555,-65.8652641874501));
#9968=CARTESIAN_POINT('Ctrl Pts',(-20.4229794705685,22.771608114635,-65.8658388444892));
#9969=CARTESIAN_POINT('Ctrl Pts',(-20.423589963603,22.7691602756424,-65.8659960211494));
#9970=CARTESIAN_POINT('Ctrl Pts',(-20.4246390301877,22.7649748654176,-65.8662645599438));
#9971=CARTESIAN_POINT('Ctrl Pts',(-20.4250761785647,22.763236943647,-65.8663760048269));
#9972=CARTESIAN_POINT('Ctrl Pts',(-20.4259548714067,22.7597558992927,-65.8665991038513));
#9973=CARTESIAN_POINT('Ctrl Pts',(-20.4263964240286,22.7580127860818,-65.8667107567695));
#9974=CARTESIAN_POINT('Ctrl Pts',(-20.4274330822529,22.7539347215117,-65.8669718269298));
#9975=CARTESIAN_POINT('Ctrl Pts',(-20.4280293493357,22.7516000614312,-65.8671211762725));
#9976=CARTESIAN_POINT('Ctrl Pts',(-20.4298771717933,22.7443986820033,-65.8675815147821));
#9977=CARTESIAN_POINT('Ctrl Pts',(-20.431137499454,22.739534189604,-65.8678919954399));
#9978=CARTESIAN_POINT('Ctrl Pts',(-20.4340754326698,22.7283028983563,-65.8686077858909));
#9979=CARTESIAN_POINT('Ctrl Pts',(-20.435761188543,22.7219382269582,-65.869012632014));
#9980=CARTESIAN_POINT('Ctrl Pts',(-20.441449185863,22.700725726665,-65.8703594374309));
#9981=CARTESIAN_POINT('Ctrl Pts',(-20.4455382637657,22.685901115199,-65.8712965993889));
#9982=CARTESIAN_POINT('Ctrl Pts',(-20.4629614035547,22.6244542719402,-65.8751663025215));
#9983=CARTESIAN_POINT('Ctrl Pts',(-20.4772414281265,22.5781042752581,-65.8780498780985));
#9984=CARTESIAN_POINT('Ctrl Pts',(-20.5389797959708,22.3926947160612,-65.8895068709393));
#9985=CARTESIAN_POINT('Ctrl Pts',(-20.5948789207734,22.2566228790572,-65.897741778693));
#9986=CARTESIAN_POINT('Ctrl Pts',(-20.7847719916005,21.8715696983216,-65.9217438131538));
#9987=CARTESIAN_POINT('Ctrl Pts',(-20.9423913826442,21.6358614309835,-65.9374685357283));
#9988=CARTESIAN_POINT('Ctrl Pts',(-21.1407510656897,21.4099828887004,-65.955670756922));
#9989=CARTESIAN_POINT('Ctrl Pts',(-21.1529248049126,21.3963557819931,-65.9567819539234));
#9990=CARTESIAN_POINT('Ctrl Pts',(-21.1692401192267,21.378402329817,-65.9582637219795));
#9991=CARTESIAN_POINT('Ctrl Pts',(-21.173278976214,21.3739827590094,-65.958629935503));
#9992=CARTESIAN_POINT('Ctrl Pts',(-21.1795821034396,21.3671239601925,-65.9592005396602));
#9993=CARTESIAN_POINT('Ctrl Pts',(-21.1818378910468,21.3646769258317,-65.9594045681934));
#9994=CARTESIAN_POINT('Ctrl Pts',(-21.1863492710179,21.359798255239,-65.9598122482485));
#9995=CARTESIAN_POINT('Ctrl Pts',(-21.1886048347874,21.3573665978977,-65.9600158984176));
#9996=CARTESIAN_POINT('Ctrl Pts',(-21.1936789662507,21.3519132339002,-65.9604736336871));
#9997=CARTESIAN_POINT('Ctrl Pts',(-21.1964995960121,21.3488934616907,-65.9607278072272));
#9998=CARTESIAN_POINT('Ctrl Pts',(-21.2047790164483,21.34006360144,-65.9614730896347));
#9999=CARTESIAN_POINT('Ctrl Pts',(-21.2102535380461,21.3342683652269,-65.9619648768608));
#10000=CARTESIAN_POINT('Ctrl Pts',(-21.2509461260023,21.291510815117,-65.9656130413122));
#10001=CARTESIAN_POINT('Ctrl Pts',(-21.2870148672163,21.2553715151228,-65.9688063904725));
#10002=CARTESIAN_POINT('Ctrl Pts',(-21.4084251449381,21.1393706575511,-65.9794345358521));
#10003=CARTESIAN_POINT('Ctrl Pts',(-21.4972448554269,21.0633005525426,-65.9870254776888));
#10004=CARTESIAN_POINT('Ctrl Pts',(-21.6948135121426,20.9119000134298,-66.0035107328305));
#10005=CARTESIAN_POINT('Ctrl Pts',(-21.8044689970814,20.8380958430611,-66.0124321525728));
#10006=CARTESIAN_POINT('Ctrl Pts',(-22.0707516512634,20.6817274270887,-66.0333355275552));
#10007=CARTESIAN_POINT('Ctrl Pts',(-22.2302872335823,20.6049066836124,-66.045303181188));
#10008=CARTESIAN_POINT('Ctrl Pts',(-22.4300574065046,20.5282227347728,-66.0590615162919));
#10009=CARTESIAN_POINT('Ctrl Pts',(-22.4650143350972,20.5154939636604,-66.0614248896733));
#10010=CARTESIAN_POINT('Ctrl Pts',(-22.5050555433346,20.501694290353,-66.0640757901158));
#10011=CARTESIAN_POINT('Ctrl Pts',(-22.5099295052411,20.5000276060807,-66.0643975261929));
#10012=CARTESIAN_POINT('Ctrl Pts',(-22.517131587097,20.4975840761345,-66.0648715336559));
#10013=CARTESIAN_POINT('Ctrl Pts',(-22.5194566011791,20.4967982033205,-66.0650243385446));
#10014=CARTESIAN_POINT('Ctrl Pts',(-22.5235707180809,20.4954128343725,-66.0652943410553));
#10015=CARTESIAN_POINT('Ctrl Pts',(-22.5253594508772,20.4948122531575,-66.0654116035372));
#10016=CARTESIAN_POINT('Ctrl Pts',(-22.5290530172931,20.4935757173974,-66.065653472307));
#10017=CARTESIAN_POINT('Ctrl Pts',(-22.5309579138164,20.4929399736964,-66.065778065796));
#10018=CARTESIAN_POINT('Ctrl Pts',(-22.5358890336922,20.4912993734819,-66.0661002196831));
#10019=CARTESIAN_POINT('Ctrl Pts',(-22.5389161657091,20.4902972239713,-66.0662976186808));
#10020=CARTESIAN_POINT('Ctrl Pts',(-22.5514977740422,20.4861527195812,-66.0671165643373));
#10021=CARTESIAN_POINT('Ctrl Pts',(-22.561065581394,20.4830505643916,-66.0677357492925));
#10022=CARTESIAN_POINT('Ctrl Pts',(-22.5857110550573,20.4751871178672,-66.0693218486954));
#10023=CARTESIAN_POINT('Ctrl Pts',(-22.6008097165177,20.4704918391863,-66.0702850638));
#10024=CARTESIAN_POINT('Ctrl Pts',(-22.6639183367668,20.4513749728996,-66.0742781350361));
#10025=CARTESIAN_POINT('Ctrl Pts',(-22.7122294534766,20.4379626433799,-66.0772557738976));
#10026=CARTESIAN_POINT('Ctrl Pts',(-22.8595246362911,20.4007488352297,-66.0861504968));
#10027=CARTESIAN_POINT('Ctrl Pts',(-22.9593455613922,20.380503276868,-66.0919309632075));
#10028=CARTESIAN_POINT('Ctrl Pts',(-23.3140806539183,20.3259005098677,-66.1121118656555));
#10029=CARTESIAN_POINT('Ctrl Pts',(-23.571945409682,20.3173364810395,-66.126215567801));
#10030=CARTESIAN_POINT('Ctrl Pts',(-23.8399061240362,20.3405237078021,-66.1420030143103));
#10031=CARTESIAN_POINT('Ctrl Pts',(-23.8517205064034,20.3416117942996,-66.1427011968122));
#10032=CARTESIAN_POINT('Ctrl Pts',(-23.9316858338088,20.3494220246755,-66.1474418281404));
#10033=CARTESIAN_POINT('Ctrl Pts',(-23.9996093862104,20.3582492963055,-66.1515429766519));
#10034=CARTESIAN_POINT('Ctrl Pts',(-24.0764933518689,20.3707436273136,-66.1562873932975));
#10035=CARTESIAN_POINT('Ctrl Pts',(-24.0857833166872,20.3722951611156,-66.1568623643496));
#10036=CARTESIAN_POINT('Ctrl Pts',(-24.0993785171449,20.3746270252545,-66.1577063259992));
#10037=CARTESIAN_POINT('Ctrl Pts',(-24.1036892369134,20.3753754446144,-66.1579742998851));
#10038=CARTESIAN_POINT('Ctrl Pts',(-24.1113316772106,20.3767183489973,-66.1584500560234));
#10039=CARTESIAN_POINT('Ctrl Pts',(-24.1146640170896,20.3773093094959,-66.1586577256299));
#10040=CARTESIAN_POINT('Ctrl Pts',(-24.121588153071,20.378548495774,-66.1590897048721));
#10041=CARTESIAN_POINT('Ctrl Pts',(-24.1251797895836,20.3791975760544,-66.1593140415018));
#10042=CARTESIAN_POINT('Ctrl Pts',(-24.1344481520235,20.3808888177802,-66.1598936355988));
#10043=CARTESIAN_POINT('Ctrl Pts',(-24.1401231768074,20.3819401267652,-66.1602491847034));
#10044=CARTESIAN_POINT('Ctrl Pts',(-24.1638723088497,20.3864057176512,-66.161739906545));
#10045=CARTESIAN_POINT('Ctrl Pts',(-24.1819195591316,20.389959406442,-66.1628795269972));
#10046=CARTESIAN_POINT('Ctrl Pts',(-24.3032099581798,20.4149231737606,-66.170585531538));
#10047=CARTESIAN_POINT('Ctrl Pts',(-24.405368485011,20.4412321678718,-66.1773087506991));
#10048=CARTESIAN_POINT('Ctrl Pts',(-24.6547413008138,20.5186745718332,-66.1943193529348));
#10049=CARTESIAN_POINT('Ctrl Pts',(-24.7998807766709,20.5755625238544,-66.2047630940263));
#10050=CARTESIAN_POINT('Ctrl Pts',(-25.0028633048507,20.6726069380651,-66.2199794332023));
#10051=CARTESIAN_POINT('Ctrl Pts',(-25.0644187029652,20.7045148265419,-66.2246779580549));
#10052=CARTESIAN_POINT('Ctrl Pts',(-25.206141098889,20.7838792607388,-66.2356422694246));
#10053=CARTESIAN_POINT('Ctrl Pts',(-25.2853796834973,20.8328781048237,-66.2418879669155));
#10054=CARTESIAN_POINT('Ctrl Pts',(-25.3926250637381,20.9058021274034,-66.2504062796723));
#10055=CARTESIAN_POINT('Ctrl Pts',(-25.4225103783518,20.9268758398528,-66.2527872470204));
#10056=CARTESIAN_POINT('Ctrl Pts',(-25.4837002505563,20.9716024577889,-66.257667125981));
#10057=CARTESIAN_POINT('Ctrl Pts',(-25.5149452784734,20.9953280625822,-66.2601616461832));
#10058=CARTESIAN_POINT('Ctrl Pts',(-25.5494961172242,21.0225726874404,-66.2629159636358));
#10059=CARTESIAN_POINT('Ctrl Pts',(-25.5532346819891,21.0255341680693,-66.2632139383201));
#10060=CARTESIAN_POINT('Ctrl Pts',(-25.5588521147189,21.0300043130716,-66.2636615627419));
#10061=CARTESIAN_POINT('Ctrl Pts',(-25.5607358665872,21.0315067865647,-66.2638116520133));
#10062=CARTESIAN_POINT('Ctrl Pts',(-25.5639942325197,21.0341116315058,-66.2640712320745));
#10063=CARTESIAN_POINT('Ctrl Pts',(-25.5653696272736,21.0352130174156,-66.2641807938175));
#10064=CARTESIAN_POINT('Ctrl Pts',(-25.5681310488031,21.0374280225238,-66.2644007427861));
#10065=CARTESIAN_POINT('Ctrl Pts',(-25.5695170553419,21.0385416591516,-66.2645111280591));
#10066=CARTESIAN_POINT('Ctrl Pts',(-25.5723534726861,21.0408245455266,-66.2647370068496));
#10067=CARTESIAN_POINT('Ctrl Pts',(-25.5738037945885,21.0419939087044,-66.2648524923042));
#10068=CARTESIAN_POINT('Ctrl Pts',(-25.57864300849,21.0459025911811,-66.2652377920346));
#10069=CARTESIAN_POINT('Ctrl Pts',(-25.5820273777565,21.0486475416243,-66.265507199849));
#10070=CARTESIAN_POINT('Ctrl Pts',(-25.6060157837334,21.0681845408122,-66.2674164433851));
#10071=CARTESIAN_POINT('Ctrl Pts',(-25.6264177371056,21.0852247001698,-66.2690385671186));
#10072=CARTESIAN_POINT('Ctrl Pts',(-25.6730770170003,21.1251858655287,-66.2727507111292));
#10073=CARTESIAN_POINT('Ctrl Pts',(-25.6991783890386,21.1482845889815,-66.27482906605));
#10074=CARTESIAN_POINT('Ctrl Pts',(-25.7725620408777,21.2153802554537,-66.2806947291003));
#10075=CARTESIAN_POINT('Ctrl Pts',(-25.8189051876307,21.2603826319328,-66.2844264779381));
#10076=CARTESIAN_POINT('Ctrl Pts',(-26.0745311943659,21.5239971977784,-66.3053840845503));
#10077=CARTESIAN_POINT('Ctrl Pts',(-26.2535431578115,21.7698241700775,-66.3217040956676));
#10078=CARTESIAN_POINT('Ctrl Pts',(-26.4051554223153,22.0549072981952,-66.3406220550871));
#10079=CARTESIAN_POINT('Ctrl Pts',(-26.4144977344831,22.0728807858263,-66.3418139457116));
#10080=CARTESIAN_POINT('Ctrl Pts',(-26.4258066511183,22.0951482958974,-66.3432901972283));
#10081=CARTESIAN_POINT('Ctrl Pts',(-26.4279342034909,22.099360383308,-66.3435694252613));
#10082=CARTESIAN_POINT('Ctrl Pts',(-26.4318681338264,22.1071913952035,-66.3440885380035));
#10083=CARTESIAN_POINT('Ctrl Pts',(-26.4336769668516,22.1108090806933,-66.3443283436209));
#10084=CARTESIAN_POINT('Ctrl Pts',(-26.4371462630953,22.1177804898347,-66.3447904483801));
#10085=CARTESIAN_POINT('Ctrl Pts',(-26.4388077053942,22.1211337208757,-66.3450127155576));
#10086=CARTESIAN_POINT('Ctrl Pts',(-26.4638910142021,22.1719809263763,-66.3483830766325));
#10087=CARTESIAN_POINT('Ctrl Pts',(-26.4861435033679,22.2200399450037,-66.3515685704321));
#10088=CARTESIAN_POINT('Ctrl Pts',(-26.5106740174188,22.2766362400392,-66.3553276249764));
#10089=CARTESIAN_POINT('Ctrl Pts',(-26.5141144452889,22.2846631882311,-66.3558609368523));
#10090=CARTESIAN_POINT('Ctrl Pts',(-26.5191954788754,22.2966522255265,-66.3566577816941));
#10091=CARTESIAN_POINT('Ctrl Pts',(-26.5208608916696,22.300603812012,-66.3569204686973));
#10092=CARTESIAN_POINT('Ctrl Pts',(-26.523818141712,22.3076599064786,-66.3573896203881));
#10093=CARTESIAN_POINT('Ctrl Pts',(-26.525113018785,22.3107631402389,-66.3575959812947));
#10094=CARTESIAN_POINT('Ctrl Pts',(-26.5278336764274,22.3173121457651,-66.3580315481102));
#10095=CARTESIAN_POINT('Ctrl Pts',(-26.5292583368283,22.3207583749303,-66.3582607917057));
#10096=CARTESIAN_POINT('Ctrl Pts',(-26.5330076616705,22.3298727020612,-66.3588671847354));
#10097=CARTESIAN_POINT('Ctrl Pts',(-26.5353221426211,22.3355449491599,-66.3592446788801));
#10098=CARTESIAN_POINT('Ctrl Pts',(-26.5457402824454,22.3612869466681,-66.3609583607167));
#10099=CARTESIAN_POINT('Ctrl Pts',(-26.553657653799,22.3814310470441,-66.3623008296803));
#10100=CARTESIAN_POINT('Ctrl Pts',(-26.6103284194216,22.5299966716802,-66.3722141645426));
#10101=CARTESIAN_POINT('Ctrl Pts',(-26.6510232232312,22.6613213713506,-66.3810542451801));
#10102=CARTESIAN_POINT('Ctrl Pts',(-26.7430104087554,23.042817882465,-66.4069449877869));
#10103=CARTESIAN_POINT('Ctrl Pts',(-26.7731425913759,23.2969902927874,-66.424513397672));
#10104=CARTESIAN_POINT('Ctrl Pts',(-26.7730020423193,23.5520285569696,-66.4414562157347));
#10105=CARTESIAN_POINT('Ctrl Pts',(-26.773002039719,23.5520332692001,-66.4414565287797));
#10106=CARTESIAN_POINT('Ctrl Pts',(-26.7729453408972,23.6546458662236,-66.4482733316772));
#10107=CARTESIAN_POINT('Ctrl Pts',(-26.7679878384078,23.7572120994706,-66.4549625706889));
#10108=CARTESIAN_POINT('Ctrl Pts',(-26.7577653228673,23.8632936085473,-66.4616370519691));
#10109=CARTESIAN_POINT('Ctrl Pts',(-26.757381021648,23.8672065830185,-66.4618829019462));
#10110=CARTESIAN_POINT('Ctrl Pts',(-26.7567442964397,23.8735700124737,-66.4622821353406));
#10111=CARTESIAN_POINT('Ctrl Pts',(-26.7564962235519,23.8760208838679,-66.4624357605224));
#10112=CARTESIAN_POINT('Ctrl Pts',(-26.7560555759835,23.8803250623757,-66.4627053067962));
#10113=CARTESIAN_POINT('Ctrl Pts',(-26.7558642041094,23.8821784872966,-66.4628212956041));
#10114=CARTESIAN_POINT('Ctrl Pts',(-26.7554870989613,23.8857999826482,-66.4630477726126));
#10115=CARTESIAN_POINT('Ctrl Pts',(-26.7553015096936,23.8875680690343,-66.4631582690861));
#10116=CARTESIAN_POINT('Ctrl Pts',(-26.7549290923121,23.8910879877591,-66.4633780975537));
#10117=CARTESIAN_POINT('Ctrl Pts',(-26.7547422910305,23.8928398178431,-66.463487430893));
#10118=CARTESIAN_POINT('Ctrl Pts',(-26.7542967143381,23.8969862032602,-66.4637460392282));
#10119=CARTESIAN_POINT('Ctrl Pts',(-26.7540366904872,23.8993806275095,-66.4638952431161));
#10120=CARTESIAN_POINT('Ctrl Pts',(-26.7532542130701,23.9065115652908,-66.4643391964043));
#10121=CARTESIAN_POINT('Ctrl Pts',(-26.7527239352616,23.911247240711,-66.4646335048976));
#10122=CARTESIAN_POINT('Ctrl Pts',(-26.7477451243082,23.9548363390854,-66.4673377762807));
#10123=CARTESIAN_POINT('Ctrl Pts',(-26.7425999836289,23.9936090700557,-66.4697091109559));
#10124=CARTESIAN_POINT('Ctrl Pts',(-26.7355098906049,24.0404788765626,-66.4725446296912));
#10125=CARTESIAN_POINT('Ctrl Pts',(-26.7342380786684,24.0486723859798,-66.4730391648288));
#10126=CARTESIAN_POINT('Ctrl Pts',(-26.7313480841914,24.0668282888138,-66.4741326202887));
#10127=CARTESIAN_POINT('Ctrl Pts',(-26.7297146897169,24.0767882070042,-66.4747308744348));
#10128=CARTESIAN_POINT('Ctrl Pts',(-26.727341744739,24.0908438869464,-66.4755731037343));
#10129=CARTESIAN_POINT('Ctrl Pts',(-26.7266410245999,24.0949460450309,-66.4758186628769));
#10130=CARTESIAN_POINT('Ctrl Pts',(-26.7201860629443,24.1322986390939,-66.478052477427));
#10131=CARTESIAN_POINT('Ctrl Pts',(-26.7139176772514,24.1654592102627,-66.4800200952918));
#10132=CARTESIAN_POINT('Ctrl Pts',(-26.7044914802644,24.2113623554518,-66.4827297176055));
#10133=CARTESIAN_POINT('Ctrl Pts',(-26.7017751219382,24.2241923762255,-66.4834855241049));
#10134=CARTESIAN_POINT('Ctrl Pts',(-26.6390657724993,24.5117115652518,-66.5003954752968));
#10135=CARTESIAN_POINT('Ctrl Pts',(-26.5434612698304,24.7773993447194,-66.5155679285083));
#10136=CARTESIAN_POINT('Ctrl Pts',(-26.376986752372,25.1002267167793,-66.5365304372054));
#10137=CARTESIAN_POINT('Ctrl Pts',(-26.3366234921934,25.1716659909652,-66.5413367737022));
#10138=CARTESIAN_POINT('Ctrl Pts',(-26.2710478810099,25.2780355051333,-66.5488054443128));
#10139=CARTESIAN_POINT('Ctrl Pts',(-26.2477869291491,25.3141315637175,-66.5513971652073));
#10140=CARTESIAN_POINT('Ctrl Pts',(-26.2195594424802,25.3560698529034,-66.5544805910169));
#10141=CARTESIAN_POINT('Ctrl Pts',(-26.2152839379331,25.3623737152076,-66.5549460232644));
#10142=CARTESIAN_POINT('Ctrl Pts',(-26.2086969698946,25.3720118987769,-66.5556606631608));
#10143=CARTESIAN_POINT('Ctrl Pts',(-26.2064014709131,25.3753571410242,-66.5559092632962));
#10144=CARTESIAN_POINT('Ctrl Pts',(-26.2023867056021,25.3811842621792,-66.5563432872559));
#10145=CARTESIAN_POINT('Ctrl Pts',(-26.2006702533382,25.3836680816462,-66.5565286035318));
#10146=CARTESIAN_POINT('Ctrl Pts',(-26.19680155733,25.3892495531813,-66.5569457401907));
#10147=CARTESIAN_POINT('Ctrl Pts',(-26.1946473633074,25.3923458421638,-66.5571776350067));
#10148=CARTESIAN_POINT('Ctrl Pts',(-26.1888705756707,25.4006179802422,-66.5577984906114));
#10149=CARTESIAN_POINT('Ctrl Pts',(-26.1852382035554,25.4057869515729,-66.5581878261843));
#10150=CARTESIAN_POINT('Ctrl Pts',(-26.1695086725674,25.4280312028943,-66.5598693147173));
#10151=CARTESIAN_POINT('Ctrl Pts',(-26.1572607752796,25.4449988086725,-66.5611672692849));
#10152=CARTESIAN_POINT('Ctrl Pts',(-25.9337053533548,25.7484295194022,-66.5846607650994));
#10153=CARTESIAN_POINT('Ctrl Pts',(-25.676572082334,25.9979976636996,-66.6089625633056));
#10154=CARTESIAN_POINT('Ctrl Pts',(-25.3279889752494,26.2391949593515,-66.6374318425259));
#10155=CARTESIAN_POINT('Ctrl Pts',(-25.2707514854744,26.2761730262208,-66.6419713430421));
#10156=CARTESIAN_POINT('Ctrl Pts',(-25.1694340936191,26.3371650924372,-66.6497264723703));
#10157=CARTESIAN_POINT('Ctrl Pts',(-25.125885855192,26.3620154657123,-66.6529739212147));
#10158=CARTESIAN_POINT('Ctrl Pts',(-25.0607045202194,26.3972203434076,-66.6576902154815));
#10159=CARTESIAN_POINT('Ctrl Pts',(-25.0395090954947,26.4083648283991,-66.6592018269723));
#10160=CARTESIAN_POINT('Ctrl Pts',(-25.0144197383457,26.4212018339314,-66.6609636389405));
#10161=CARTESIAN_POINT('Ctrl Pts',(-25.010644977508,26.4231238148793,-66.6612279811058));
#10162=CARTESIAN_POINT('Ctrl Pts',(-25.0052160457243,26.4258745788889,-66.6616071072701));
#10163=CARTESIAN_POINT('Ctrl Pts',(-25.003564954101,26.4267093779533,-66.6617222702242));
#10164=CARTESIAN_POINT('Ctrl Pts',(-25.00031708957,26.428348002016,-66.6619485308413));
#10165=CARTESIAN_POINT('Ctrl Pts',(-24.9987203637366,26.429151921721,-66.662059634519));
#10166=CARTESIAN_POINT('Ctrl Pts',(-24.9955353820572,26.4307521761328,-66.6622809898053));
#10167=CARTESIAN_POINT('Ctrl Pts',(-24.9939471399595,26.4315485243455,-66.6623912422478));
#10168=CARTESIAN_POINT('Ctrl Pts',(-24.9901533199767,26.433446829909,-66.6626542931486));
#10169=CARTESIAN_POINT('Ctrl Pts',(-24.9879471305079,26.4345475724262,-66.6628070145965));
#10170=CARTESIAN_POINT('Ctrl Pts',(-24.9800633065217,26.4384697857764,-66.663351886097));
#10171=CARTESIAN_POINT('Ctrl Pts',(-24.974378563609,26.4412770569157,-66.6637431469159));
#10172=CARTESIAN_POINT('Ctrl Pts',(-24.8918941259207,26.4817076462584,-66.6693972598639));
#10173=CARTESIAN_POINT('Ctrl Pts',(-24.8136267525672,26.5162801565671,-66.6744740813416));
#10174=CARTESIAN_POINT('Ctrl Pts',(-24.6025077453349,26.5996597796819,-66.6876543849707));
#10175=CARTESIAN_POINT('Ctrl Pts',(-24.4676593107816,26.6429044493942,-66.69555659579));
#10176=CARTESIAN_POINT('Ctrl Pts',(-24.3142149719278,26.6811880368407,-66.7043937341486));
#10177=CARTESIAN_POINT('Ctrl Pts',(-24.2980010643669,26.6850998771355,-66.7053255507264));
#10178=CARTESIAN_POINT('Ctrl Pts',(-24.2630368230461,26.6932488120214,-66.7073318557541));
#10179=CARTESIAN_POINT('Ctrl Pts',(-24.2442774937518,26.697444361483,-66.7084063896779));
#10180=CARTESIAN_POINT('Ctrl Pts',(-24.2034822227336,26.7061857907588,-66.7107407057408));
#10181=CARTESIAN_POINT('Ctrl Pts',(-24.1814339920301,26.7106692321189,-66.7120007781898));
#10182=CARTESIAN_POINT('Ctrl Pts',(-24.1328804434403,26.7200140938005,-66.7147749112308));
#10183=CARTESIAN_POINT('Ctrl Pts',(-24.106357555101,26.7247746726938,-66.7162898339661));
#10184=CARTESIAN_POINT('Ctrl Pts',(-24.0466927892136,26.7347131857336,-66.7197010010988));
#10185=CARTESIAN_POINT('Ctrl Pts',(-24.0135237376521,26.7397073930787,-66.7215996065667));
#10186=CARTESIAN_POINT('Ctrl Pts',(-23.8804282414592,26.7576273676666,-66.7292407186346));
#10187=CARTESIAN_POINT('Ctrl Pts',(-23.7800051021913,26.7663807234197,-66.735059358282));
#10188=CARTESIAN_POINT('Ctrl Pts',(-23.6147561657635,26.7730052297384,-66.7448407972053));
#10189=CARTESIAN_POINT('Ctrl Pts',(-23.5501103046843,26.7736505448982,-66.7487184468738));
#10190=CARTESIAN_POINT('Ctrl Pts',(-23.4770650262638,26.7721824183442,-66.7531718122301));
#10191=CARTESIAN_POINT('Ctrl Pts',(-23.4686387915671,26.7719799876928,-66.7536866106322));
#10192=CARTESIAN_POINT('Ctrl Pts',(-23.4559885567267,26.771626420224,-66.7544611180973));
#10193=CARTESIAN_POINT('Ctrl Pts',(-23.4517638553899,26.7715000240565,-66.7547200498865));
#10194=CARTESIAN_POINT('Ctrl Pts',(-23.4445007075638,26.77126842073,-66.7551656859412));
#10195=CARTESIAN_POINT('Ctrl Pts',(-23.4414621313609,26.7711672238925,-66.7553522639929));
#10196=CARTESIAN_POINT('Ctrl Pts',(-23.4352067928245,26.7709500340231,-66.755736659301));
#10197=CARTESIAN_POINT('Ctrl Pts',(-23.4319900526409,26.7708335211216,-66.7559344927059));
#10198=CARTESIAN_POINT('Ctrl Pts',(-23.4242498800362,26.7705415539009,-66.7564109156523));
#10199=CARTESIAN_POINT('Ctrl Pts',(-23.419726640974,26.7703613879747,-66.7566896530004));
#10200=CARTESIAN_POINT('Ctrl Pts',(-23.4058572920852,26.7697796846202,-66.7575453284505));
#10201=CARTESIAN_POINT('Ctrl Pts',(-23.3965126011422,26.7693469857978,-66.7581232448087));
#10202=CARTESIAN_POINT('Ctrl Pts',(-23.2882485258053,26.7638614133981,-66.76483515588));
#10203=CARTESIAN_POINT('Ctrl Pts',(-23.1896206564721,26.7542920622106,-66.7711108041114));
#10204=CARTESIAN_POINT('Ctrl Pts',(-22.8029283642046,26.6986929285994,-66.7963919260849));
#10205=CARTESIAN_POINT('Ctrl Pts',(-22.5212493860532,26.6181952366371,-66.8164604755562));
#10206=CARTESIAN_POINT('Ctrl Pts',(-22.1936910076554,26.474332169919,-66.8403569096297));
#10207=CARTESIAN_POINT('Ctrl Pts',(-22.1339047982687,26.4458458795231,-66.8447348211984));
#10208=CARTESIAN_POINT('Ctrl Pts',(-22.0750360151859,26.4155367744738,-66.8490341587423));
#10209=CARTESIAN_POINT('',(-26.7730013023275,23.5474375926689,-66.6850863746791));
#10210=CARTESIAN_POINT('Ctrl Pts',(-22.0750362583504,26.4155368996692,-67.093261398997));
#10211=CARTESIAN_POINT('Ctrl Pts',(-22.1505511773086,26.4544164044654,-67.0875238249795));
#10212=CARTESIAN_POINT('Ctrl Pts',(-22.2276018483777,26.4903099549655,-67.081759723405));
#10213=CARTESIAN_POINT('Ctrl Pts',(-22.4545604981318,26.5852993095174,-67.0651565858544));
#10214=CARTESIAN_POINT('Ctrl Pts',(-22.6075825615071,26.6362592309213,-67.0544127197646));
#10215=CARTESIAN_POINT('Ctrl Pts',(-22.7729459163076,26.6778716094321,-67.0436883118301));
#10216=CARTESIAN_POINT('Ctrl Pts',(-22.7821104012551,26.6801350123157,-67.0430968116143));
#10217=CARTESIAN_POINT('Ctrl Pts',(-22.7944278757522,26.6831197664715,-67.0423057540625));
#10218=CARTESIAN_POINT('Ctrl Pts',(-22.7975720783738,26.6838766566779,-67.0421041703756));
#10219=CARTESIAN_POINT('Ctrl Pts',(-22.8024997567178,26.6850550307932,-67.0417887883655));
#10220=CARTESIAN_POINT('Ctrl Pts',(-22.804282450609,26.6854797258555,-67.0416748038514));
#10221=CARTESIAN_POINT('Ctrl Pts',(-22.8077067710442,26.6862924232297,-67.0414560704241));
#10222=CARTESIAN_POINT('Ctrl Pts',(-22.8093483292713,26.6866806547044,-67.0413513088939));
#10223=CARTESIAN_POINT('Ctrl Pts',(-22.8127379548925,26.6874794976309,-67.0411351847337));
#10224=CARTESIAN_POINT('Ctrl Pts',(-22.8144860554825,26.6878899357478,-67.0410238325259));
#10225=CARTESIAN_POINT('Ctrl Pts',(-22.8184329611372,26.6888131534297,-67.0407726595012));
#10226=CARTESIAN_POINT('Ctrl Pts',(-22.8206319667729,26.6893250844523,-67.0406328878849));
#10227=CARTESIAN_POINT('Ctrl Pts',(-22.8309752453531,26.6917215556337,-67.0399762407764));
#10228=CARTESIAN_POINT('Ctrl Pts',(-22.8391263914278,26.6935767369449,-67.0394610496647));
#10229=CARTESIAN_POINT('Ctrl Pts',(-22.9289550481959,26.7136542201972,-67.0338076922075));
#10230=CARTESIAN_POINT('Ctrl Pts',(-23.0113137464413,26.7287220701921,-67.0288446981667));
#10231=CARTESIAN_POINT('Ctrl Pts',(-23.2287302703402,26.759803361815,-67.0160970370804));
#10232=CARTESIAN_POINT('Ctrl Pts',(-23.3643784978459,26.770508558548,-67.0084934787041));
#10233=CARTESIAN_POINT('Ctrl Pts',(-23.7762002888445,26.7768919030031,-66.9854753483792));
#10234=CARTESIAN_POINT('Ctrl Pts',(-24.0514568117553,26.7457215561494,-66.970068567576));
#10235=CARTESIAN_POINT('Ctrl Pts',(-24.3367278049164,26.6756155225269,-66.952277087987));
#10236=CARTESIAN_POINT('Ctrl Pts',(-24.3540529920767,26.6712046267555,-66.9511897530952));
#10237=CARTESIAN_POINT('Ctrl Pts',(-24.3770792246922,26.6651378271145,-66.9497352341898));
#10238=CARTESIAN_POINT('Ctrl Pts',(-24.3828139161051,26.6636099355787,-66.9493722078512));
#10239=CARTESIAN_POINT('Ctrl Pts',(-24.3917478585975,26.6612032199407,-66.9488054328442));
#10240=CARTESIAN_POINT('Ctrl Pts',(-24.3949500487826,26.6603352756729,-66.9486020381742));
#10241=CARTESIAN_POINT('Ctrl Pts',(-24.4013525614472,26.6585892758269,-66.9481948734571));
#10242=CARTESIAN_POINT('Ctrl Pts',(-24.4045528793908,26.657711218687,-66.9479911035682));
#10243=CARTESIAN_POINT('Ctrl Pts',(-24.41175498237,26.6557232425883,-66.947531973584));
#10244=CARTESIAN_POINT('Ctrl Pts',(-24.4157559841133,26.654610530111,-66.9472765227323));
#10245=CARTESIAN_POINT('Ctrl Pts',(-24.4275259390017,26.6513126831422,-66.9465238969655));
#10246=CARTESIAN_POINT('Ctrl Pts',(-24.4352888052014,26.649106107897,-66.9460260231885));
#10247=CARTESIAN_POINT('Ctrl Pts',(-24.4936154633616,26.632289858447,-66.9422739699456));
#10248=CARTESIAN_POINT('Ctrl Pts',(-24.5438203103723,26.6164733724153,-66.9389804651138));
#10249=CARTESIAN_POINT('Ctrl Pts',(-24.7100091715604,26.5596073500084,-66.9278543266071));
#10250=CARTESIAN_POINT('Ctrl Pts',(-24.824015933098,26.5131518823701,-66.919847082871));
#10251=CARTESIAN_POINT('Ctrl Pts',(-25.005512358643,26.4267818297944,-66.9065035696559));
#10252=CARTESIAN_POINT('Ctrl Pts',(-25.0747034225353,26.3907191339648,-66.9012675710791));
#10253=CARTESIAN_POINT('Ctrl Pts',(-25.2106930926289,26.313439814816,-66.8907112468174));
#10254=CARTESIAN_POINT('Ctrl Pts',(-25.2774336891162,26.2722209251642,-66.885394020666));
#10255=CARTESIAN_POINT('Ctrl Pts',(-25.4688488739672,26.1441262433553,-66.8698251493757));
#10256=CARTESIAN_POINT('Ctrl Pts',(-25.5889768697811,26.0508135920372,-66.8596309255803));
#10257=CARTESIAN_POINT('Ctrl Pts',(-25.7042648428269,25.9474085780935,-66.8497218415432));
#10258=CARTESIAN_POINT('Ctrl Pts',(-25.7064433504623,25.9454492460579,-66.8495345518188));
#10259=CARTESIAN_POINT('Ctrl Pts',(-25.7139116372128,25.9387138836178,-66.8488923444932));
#10260=CARTESIAN_POINT('Ctrl Pts',(-25.7191882894192,25.9339232378656,-66.8484383448836));
#10261=CARTESIAN_POINT('Ctrl Pts',(-25.7261598639978,25.9275514644086,-66.8478382292061));
#10262=CARTESIAN_POINT('Ctrl Pts',(-25.7278689853072,25.9259860005958,-66.8476910845236));
#10263=CARTESIAN_POINT('Ctrl Pts',(-25.7435573817223,25.9115851142038,-66.8463402131384));
#10264=CARTESIAN_POINT('Ctrl Pts',(-25.7574251163073,25.8986279177598,-66.8451446625162));
#10265=CARTESIAN_POINT('Ctrl Pts',(-25.7739264696091,25.8829347147107,-66.8437211995362));
#10266=CARTESIAN_POINT('Ctrl Pts',(-25.7766703643264,25.8803159608796,-66.8434844728169));
#10267=CARTESIAN_POINT('Ctrl Pts',(-25.7811350492552,25.8760398098567,-66.8430992490486));
#10268=CARTESIAN_POINT('Ctrl Pts',(-25.7828586199841,25.8743853430946,-66.8429505260404));
#10269=CARTESIAN_POINT('Ctrl Pts',(-25.7859300859509,25.8714304533042,-66.8426854824972));
#10270=CARTESIAN_POINT('Ctrl Pts',(-25.787278685953,25.8701307732418,-66.84256910423));
#10271=CARTESIAN_POINT('Ctrl Pts',(-25.790140823725,25.867367641943,-66.8423221051491));
#10272=CARTESIAN_POINT('Ctrl Pts',(-25.7916540566739,25.8659038868856,-66.842191509194));
#10273=CARTESIAN_POINT('Ctrl Pts',(-25.7947366010381,25.8629162793644,-66.8419254630813));
#10274=CARTESIAN_POINT('Ctrl Pts',(-25.7963057978945,25.8613923095498,-66.841790022246));
#10275=CARTESIAN_POINT('Ctrl Pts',(-25.8002197033979,25.857583458769,-66.8414521814976));
#10276=CARTESIAN_POINT('Ctrl Pts',(-25.8025624908468,25.8552965939422,-66.8412499360102));
#10277=CARTESIAN_POINT('Ctrl Pts',(-25.8288512793811,25.8295569762198,-66.8389802186312));
#10278=CARTESIAN_POINT('Ctrl Pts',(-25.8524346391535,25.8057344679384,-66.8369413837415));
#10279=CARTESIAN_POINT('Ctrl Pts',(-25.9448069499592,25.7094667241729,-66.8289230946981));
#10280=CARTESIAN_POINT('Ctrl Pts',(-26.0105886562705,25.6342023148557,-66.8231386030559));
#10281=CARTESIAN_POINT('Ctrl Pts',(-26.1175374910903,25.4996983215217,-66.8133599100091));
#10282=CARTESIAN_POINT('Ctrl Pts',(-26.1604062637903,25.4419155598186,-66.8093210668536));
#10283=CARTESIAN_POINT('Ctrl Pts',(-26.2624073287804,25.2943513566348,-66.7992819542795));
#10284=CARTESIAN_POINT('Ctrl Pts',(-26.3190485158035,25.2029572239175,-66.7933030096132));
#10285=CARTESIAN_POINT('Ctrl Pts',(-26.4651265642402,24.9385932114365,-66.7762780167469));
#10286=CARTESIAN_POINT('Ctrl Pts',(-26.5436031744961,24.7601348511216,-66.7650648308309));
#10287=CARTESIAN_POINT('Ctrl Pts',(-26.609565460328,24.5636058144705,-66.7524691348085));
#10288=CARTESIAN_POINT('Ctrl Pts',(-26.6135547586185,24.5514817413134,-66.7516912805668));
#10289=CARTESIAN_POINT('Ctrl Pts',(-26.6188974329064,24.534913695648,-66.7506271004287));
#10290=CARTESIAN_POINT('Ctrl Pts',(-26.6203134144978,24.5304899075612,-66.7503428394148));
#10291=CARTESIAN_POINT('Ctrl Pts',(-26.6227042419424,24.5229645244729,-66.7498590731801));
#10292=CARTESIAN_POINT('Ctrl Pts',(-26.6236839701504,24.5198644776272,-66.7496597289118));
#10293=CARTESIAN_POINT('Ctrl Pts',(-26.6255676328128,24.5138726698851,-66.7492743178349));
#10294=CARTESIAN_POINT('Ctrl Pts',(-26.6264721839222,24.5109811057688,-66.7490882715864));
#10295=CARTESIAN_POINT('Ctrl Pts',(-26.6286055178869,24.5041276082937,-66.7486471848317));
#10296=CARTESIAN_POINT('Ctrl Pts',(-26.6298307293967,24.500164576748,-66.7483920273059));
#10297=CARTESIAN_POINT('Ctrl Pts',(-26.6334104416078,24.4885060314283,-66.7476411002953));
#10298=CARTESIAN_POINT('Ctrl Pts',(-26.6357437595273,24.4808040930317,-66.7471446367313));
#10299=CARTESIAN_POINT('Ctrl Pts',(-26.6409405476884,24.4634158110116,-66.7460229026759));
#10300=CARTESIAN_POINT('Ctrl Pts',(-26.6437873667097,24.4537246163261,-66.7453970915488));
#10301=CARTESIAN_POINT('Ctrl Pts',(-26.6527342900554,24.4227292253103,-66.7433934852256));
#10302=CARTESIAN_POINT('Ctrl Pts',(-26.6586601321783,24.4013757845281,-66.7420100313259));
#10303=CARTESIAN_POINT('Ctrl Pts',(-26.736743252748,24.1083102646871,-66.7229771510973));
#10304=CARTESIAN_POINT('Ctrl Pts',(-26.773246729524,23.8284206579786,-66.7041027857559));
#10305=CARTESIAN_POINT('Ctrl Pts',(-26.7730013023275,23.5474375926689,-66.6850863746791));
#10306=CARTESIAN_POINT('Ctrl Pts',(-26.7730013006479,23.5474356704599,-66.6850862445875));
#10307=CARTESIAN_POINT('Ctrl Pts',(-26.7728538349007,23.3787212695974,-66.673667968088));
#10308=CARTESIAN_POINT('Ctrl Pts',(-26.7594579767268,23.2102566127178,-66.6622840767911));
#10309=CARTESIAN_POINT('Ctrl Pts',(-26.7280225822497,23.012787796804,-66.6494702834752));
#10310=CARTESIAN_POINT('Ctrl Pts',(-26.7226706477898,22.9820498303895,-66.6474916045324));
#10311=CARTESIAN_POINT('Ctrl Pts',(-26.7161312057531,22.9474708818912,-66.645287346235));
#10312=CARTESIAN_POINT('Ctrl Pts',(-26.7153821662279,22.9435500566689,-66.6450377261054));
#10313=CARTESIAN_POINT('Ctrl Pts',(-26.7141543342157,22.9371871687715,-66.6446331552387));
#10314=CARTESIAN_POINT('Ctrl Pts',(-26.7136799973535,22.9347442662529,-66.644477953824));
#10315=CARTESIAN_POINT('Ctrl Pts',(-26.7128438051381,22.9304642569679,-66.6442062609315));
#10316=CARTESIAN_POINT('Ctrl Pts',(-26.7124831782526,22.9286269157797,-66.6440896994001));
#10317=CARTESIAN_POINT('Ctrl Pts',(-26.7117536539914,22.924927159698,-66.6438551321121));
#10318=CARTESIAN_POINT('Ctrl Pts',(-26.7113847112272,22.9230647522015,-66.6437371289139));
#10319=CARTESIAN_POINT('Ctrl Pts',(-26.7106675528228,22.9194612752106,-66.643508956589));
#10320=CARTESIAN_POINT('Ctrl Pts',(-26.710319545023,22.9177201717781,-66.6433987756693));
#10321=CARTESIAN_POINT('Ctrl Pts',(-26.7094857646807,22.9135665823217,-66.6431360824067));
#10322=CARTESIAN_POINT('Ctrl Pts',(-26.7089986665251,22.9111543590166,-66.6429836465839));
#10323=CARTESIAN_POINT('Ctrl Pts',(-26.7075189469428,22.9038694612276,-66.642523662486));
#10324=CARTESIAN_POINT('Ctrl Pts',(-26.7065178042862,22.8989984948894,-66.642216600866));
#10325=CARTESIAN_POINT('Ctrl Pts',(-26.6962380275353,22.8495636945561,-66.6391051889979));
#10326=CARTESIAN_POINT('Ctrl Pts',(-26.686026918792,22.8051960907119,-66.6363532880314));
#10327=CARTESIAN_POINT('Ctrl Pts',(-26.637757451749,22.6140849800131,-66.6246174541903));
#10328=CARTESIAN_POINT('Ctrl Pts',(-26.5903086846143,22.4698985209697,-66.6160611961401));
#10329=CARTESIAN_POINT('Ctrl Pts',(-26.521641441517,22.3021155781672,-66.6059073940391));
#10330=CARTESIAN_POINT('Ctrl Pts',(-26.5100244128222,22.274812085168,-66.604248796313));
#10331=CARTESIAN_POINT('Ctrl Pts',(-26.4874619147879,22.2237524324373,-66.6011293758084));
#10332=CARTESIAN_POINT('Ctrl Pts',(-26.4766010907327,22.1999616063984,-66.5996685506246));
#10333=CARTESIAN_POINT('Ctrl Pts',(-26.4427270397673,22.1280886597394,-66.5952267129182));
#10334=CARTESIAN_POINT('Ctrl Pts',(-26.4188096582066,22.0804434460837,-66.592242675412));
#10335=CARTESIAN_POINT('Ctrl Pts',(-26.3198391295674,21.8949130535386,-66.5804031420904));
#10336=CARTESIAN_POINT('Ctrl Pts',(-26.2359445814555,21.7620107835425,-66.5714197444653));
#10337=CARTESIAN_POINT('Ctrl Pts',(-26.1129226451039,21.595424292625,-66.5590871712984));
#10338=CARTESIAN_POINT('Ctrl Pts',(-26.0822009891195,21.5557931724937,-66.5560672680176));
#10339=CARTESIAN_POINT('Ctrl Pts',(-26.0455055930862,21.5106706833333,-66.5525210156025));
#10340=CARTESIAN_POINT('Ctrl Pts',(-26.0404193736614,21.504463917521,-66.5520307915641));
#10341=CARTESIAN_POINT('Ctrl Pts',(-26.0326719558048,21.4950813630937,-66.5512860229376));
#10342=CARTESIAN_POINT('Ctrl Pts',(-26.0300277006719,21.4918915719702,-66.551032168671));
#10343=CARTESIAN_POINT('Ctrl Pts',(-26.0252549730742,21.4861567283552,-66.5505745851002));
#10344=CARTESIAN_POINT('Ctrl Pts',(-26.0231287043421,21.4836098424959,-66.550370946086));
#10345=CARTESIAN_POINT('Ctrl Pts',(-26.0188651836227,21.4785189153098,-66.5499630458426));
#10346=CARTESIAN_POINT('Ctrl Pts',(-26.0167279226205,21.4759748867433,-66.5497587843827));
#10347=CARTESIAN_POINT('Ctrl Pts',(-26.0107465063935,21.4688773914026,-66.5491877269604));
#10348=CARTESIAN_POINT('Ctrl Pts',(-26.0068936646777,21.4643312922593,-66.5488205738133));
#10349=CARTESIAN_POINT('Ctrl Pts',(-25.9913131858863,21.4460503960531,-66.5473385733511));
#10350=CARTESIAN_POINT('Ctrl Pts',(-25.9794829726389,21.4324038146009,-66.546219487416));
#10351=CARTESIAN_POINT('Ctrl Pts',(-25.7832836150021,21.2098875543304,-66.5277581572107));
#10352=CARTESIAN_POINT('Ctrl Pts',(-25.5727500397149,21.025738507981,-66.5092005090331));
#10353=CARTESIAN_POINT('Ctrl Pts',(-25.278981920928,20.829366775303,-66.4852832238685));
#10354=CARTESIAN_POINT('Ctrl Pts',(-25.215297174336,20.7899352970996,-66.4802112787161));
#10355=CARTESIAN_POINT('Ctrl Pts',(-25.0726632541683,20.7083549988295,-66.4691622130525));
#10356=CARTESIAN_POINT('Ctrl Pts',(-24.993210110548,20.6672000431357,-66.4632050091617));
#10357=CARTESIAN_POINT('Ctrl Pts',(-24.8768208207622,20.6129318105343,-66.4548514764427));
#10358=CARTESIAN_POINT('Ctrl Pts',(-24.8412011801104,20.5971036461663,-66.4523434907402));
#10359=CARTESIAN_POINT('Ctrl Pts',(-24.793288737847,20.5768456212321,-66.4490424678556));
#10360=CARTESIAN_POINT('Ctrl Pts',(-24.7812450805936,20.5718393597389,-66.4482187339925));
#10361=CARTESIAN_POINT('Ctrl Pts',(-24.7611544469397,20.5636308432856,-66.4468550425463));
#10362=CARTESIAN_POINT('Ctrl Pts',(-24.7531244841774,20.5603877140049,-66.4463127469483));
#10363=CARTESIAN_POINT('Ctrl Pts',(-24.7429607553265,20.5563303767688,-66.4456299137494));
#10364=CARTESIAN_POINT('Ctrl Pts',(-24.740839166715,20.5554860564811,-66.4454875741169));
#10365=CARTESIAN_POINT('Ctrl Pts',(-24.7370405158981,20.5539789969895,-66.4452330711583));
#10366=CARTESIAN_POINT('Ctrl Pts',(-24.7353637942921,20.5533154103111,-66.4451208565448));
#10367=CARTESIAN_POINT('Ctrl Pts',(-24.7319650146108,20.5519735927565,-66.4448936432375));
#10368=CARTESIAN_POINT('Ctrl Pts',(-24.7302429313415,20.5512954388438,-66.444778649588));
#10369=CARTESIAN_POINT('Ctrl Pts',(-24.7267896123728,20.5499389618272,-66.444548312224));
#10370=CARTESIAN_POINT('Ctrl Pts',(-24.7250583805269,20.5492606561086,-66.4444329697345));
#10371=CARTESIAN_POINT('Ctrl Pts',(-24.7201905130804,20.5473582579889,-66.444109016382));
#10372=CARTESIAN_POINT('Ctrl Pts',(-24.717052533025,20.5461375777547,-66.4439006126907));
#10373=CARTESIAN_POINT('Ctrl Pts',(-24.7041802346993,20.5411534407962,-66.4430474466909));
#10374=CARTESIAN_POINT('Ctrl Pts',(-24.6944294351111,20.5374323074917,-66.4424052139725));
#10375=CARTESIAN_POINT('Ctrl Pts',(-24.5158515734184,20.4702748182372,-66.4307140261803));
#10376=CARTESIAN_POINT('Ctrl Pts',(-24.3419828773798,20.4210628707826,-66.4204768713474));
#10377=CARTESIAN_POINT('Ctrl Pts',(-24.0127956027335,20.3571073847874,-66.4016676881555));
#10378=CARTESIAN_POINT('Ctrl Pts',(-23.8587762695352,20.3385654020417,-66.3930873236593));
#10379=CARTESIAN_POINT('Ctrl Pts',(-23.6791967553484,20.3299872250672,-66.382873880477));
#10380=CARTESIAN_POINT('Ctrl Pts',(-23.6543590213605,20.3290886014673,-66.3814569341318));
#10381=CARTESIAN_POINT('Ctrl Pts',(-23.5299430702583,20.3260277570807,-66.3743311665365));
#10382=CARTESIAN_POINT('Ctrl Pts',(-23.4303203272242,20.3281955091975,-66.3685331090287));
#10383=CARTESIAN_POINT('Ctrl Pts',(-23.2839594681288,20.3381776172323,-66.3597834008424));
#10384=CARTESIAN_POINT('Ctrl Pts',(-23.2370330573755,20.3424136242046,-66.3569432147358));
#10385=CARTESIAN_POINT('Ctrl Pts',(-23.1824176809717,20.3485534981174,-66.3535916535463));
#10386=CARTESIAN_POINT('Ctrl Pts',(-23.1746204850187,20.3494589202903,-66.3531120719566));
#10387=CARTESIAN_POINT('Ctrl Pts',(-23.1627493133096,20.3508813931315,-66.3523802199701));
#10388=CARTESIAN_POINT('Ctrl Pts',(-23.1586728505169,20.3513777639725,-66.352128603742));
#10389=CARTESIAN_POINT('Ctrl Pts',(-23.15159552604,20.3522532660188,-66.3516912293978));
#10390=CARTESIAN_POINT('Ctrl Pts',(-23.1485942219393,20.3526288337707,-66.3515055842478));
#10391=CARTESIAN_POINT('Ctrl Pts',(-23.1423491713852,20.3534192383938,-66.351118949559));
#10392=CARTESIAN_POINT('Ctrl Pts',(-23.1391055200145,20.3538347881633,-66.3509179376462));
#10393=CARTESIAN_POINT('Ctrl Pts',(-23.1311880692332,20.3548613574252,-66.3504268060882));
#10394=CARTESIAN_POINT('Ctrl Pts',(-23.1265149769655,20.3554776938319,-66.3501365182975));
#10395=CARTESIAN_POINT('Ctrl Pts',(-23.1087437947588,20.3578612209542,-66.3490310232826));
#10396=CARTESIAN_POINT('Ctrl Pts',(-23.095655408496,20.3596987094098,-66.3482135911825));
#10397=CARTESIAN_POINT('Ctrl Pts',(-23.0781775686289,20.362262164749,-66.3471175997147));
#10398=CARTESIAN_POINT('Ctrl Pts',(-23.0737776463472,20.3629168051347,-66.3468413169962));
#10399=CARTESIAN_POINT('Ctrl Pts',(-22.8077250584586,20.403064526239,-66.3301123794968));
#10400=CARTESIAN_POINT('Ctrl Pts',(-22.5519883997415,20.4746146394046,-66.3125690605697));
#10401=CARTESIAN_POINT('Ctrl Pts',(-22.1545878240723,20.6406383934355,-66.2834382967805));
#10402=CARTESIAN_POINT('Ctrl Pts',(-22.0064253966681,20.7164674310688,-66.2721368524191));
#10403=CARTESIAN_POINT('Ctrl Pts',(-21.8230355555805,20.8289961560531,-66.258038586554));
#10404=CARTESIAN_POINT('Ctrl Pts',(-21.7818907212416,20.8555518378362,-66.2548690527379));
#10405=CARTESIAN_POINT('Ctrl Pts',(-21.7219335953938,20.8962143526388,-66.2502585419626));
#10406=CARTESIAN_POINT('Ctrl Pts',(-21.7026464225244,20.9096047830807,-66.2487767274542));
#10407=CARTESIAN_POINT('Ctrl Pts',(-21.680071821555,20.9256460032597,-66.24704554672));
#10408=CARTESIAN_POINT('Ctrl Pts',(-21.676641769872,20.9280934916388,-66.2467825942319));
#10409=CARTESIAN_POINT('Ctrl Pts',(-21.6713706534647,20.9318702818103,-66.2463786517707));
#10410=CARTESIAN_POINT('Ctrl Pts',(-21.6695261933851,20.9331948022367,-66.2462373329917));
#10411=CARTESIAN_POINT('Ctrl Pts',(-21.6663171806874,20.9355043625586,-66.2459915161325));
#10412=CARTESIAN_POINT('Ctrl Pts',(-21.6649520034552,20.936488519195,-66.2458869570627));
#10413=CARTESIAN_POINT('Ctrl Pts',(-21.662086573457,20.9385576213973,-66.2456675278944));
#10414=CARTESIAN_POINT('Ctrl Pts',(-21.6605864890141,20.939642787305,-66.2455526739214));
#10415=CARTESIAN_POINT('Ctrl Pts',(-21.656392827625,20.9426820038979,-66.2452316386186));
#10416=CARTESIAN_POINT('Ctrl Pts',(-21.6537013309078,20.9446389419303,-66.2450256583456));
#10417=CARTESIAN_POINT('Ctrl Pts',(-21.6428244343126,20.9525731166164,-66.2441934731213));
#10418=CARTESIAN_POINT('Ctrl Pts',(-21.6346641070276,20.958584867049,-66.2435696447985));
#10419=CARTESIAN_POINT('Ctrl Pts',(-21.4963063532975,21.0615241606773,-66.2329988990883));
#10420=CARTESIAN_POINT('Ctrl Pts',(-21.3735656624489,21.1681286920354,-66.2237104419028));
#10421=CARTESIAN_POINT('Ctrl Pts',(-21.0992543793937,21.4453658795981,-66.2017562007693));
#10422=CARTESIAN_POINT('Ctrl Pts',(-20.9567445012981,21.6236873340018,-66.1892583239405));
#10423=CARTESIAN_POINT('Ctrl Pts',(-20.7991668063294,21.8704061444507,-66.1723166568256));
#10424=CARTESIAN_POINT('Ctrl Pts',(-20.7657938792965,21.9263234180558,-66.1685018631107));
#10425=CARTESIAN_POINT('Ctrl Pts',(-20.7090689018598,22.0282632450615,-66.1615603765381));
#10426=CARTESIAN_POINT('Ctrl Pts',(-20.6850849961981,22.0739089617636,-66.1584567733095));
#10427=CARTESIAN_POINT('Ctrl Pts',(-20.6585312498045,22.1275318245967,-66.1548089848591));
#10428=CARTESIAN_POINT('Ctrl Pts',(-20.6548838856454,22.1349693148091,-66.1543030018873));
#10429=CARTESIAN_POINT('Ctrl Pts',(-20.6494318253231,22.1461961200596,-66.1535391441968));
#10430=CARTESIAN_POINT('Ctrl Pts',(-20.6476057709668,22.1499750735673,-66.1532820149934));
#10431=CARTESIAN_POINT('Ctrl Pts',(-20.6444714390372,22.1564939361144,-66.1528384274493));
#10432=CARTESIAN_POINT('Ctrl Pts',(-20.6431596387454,22.1592321533896,-66.1526520920368));
#10433=CARTESIAN_POINT('Ctrl Pts',(-20.6404600236735,22.1648877566394,-66.1522672092819));
#10434=CARTESIAN_POINT('Ctrl Pts',(-20.6390727226082,22.1678053830705,-66.1520686443257));
#10435=CARTESIAN_POINT('Ctrl Pts',(-20.6357336102024,22.1748551697919,-66.1515888285306));
#10436=CARTESIAN_POINT('Ctrl Pts',(-20.633786200317,22.178989397037,-66.1513074252707));
#10437=CARTESIAN_POINT('Ctrl Pts',(-20.626637096128,22.1942506087418,-66.1502685478638));
#10438=CARTESIAN_POINT('Ctrl Pts',(-20.6214902841984,22.2054030527326,-66.1495091767296));
#10439=CARTESIAN_POINT('Ctrl Pts',(-20.5393810004906,22.3860296555652,-66.1372064211835));
#10440=CARTESIAN_POINT('Ctrl Pts',(-20.4771926693296,22.5617974894936,-66.1251478992167));
#10441=CARTESIAN_POINT('Ctrl Pts',(-20.3952509043306,22.8780492991186,-66.103358340398));
#10442=CARTESIAN_POINT('Ctrl Pts',(-20.3689286290004,23.0163353492703,-66.0938095313974));
#10443=CARTESIAN_POINT('Ctrl Pts',(-20.3386688434436,23.2617618703957,-66.0770958621618));
#10444=CARTESIAN_POINT('Ctrl Pts',(-20.3308792220191,23.368222552258,-66.0699243602965));
#10445=CARTESIAN_POINT('Ctrl Pts',(-20.3271925380916,23.525811506521,-66.0595813255431));
#10446=CARTESIAN_POINT('Ctrl Pts',(-20.327208838471,23.5767681946769,-66.0562793311494));
#10447=CARTESIAN_POINT('Ctrl Pts',(-20.3288190679311,23.6437485863689,-66.0520127188152));
#10448=CARTESIAN_POINT('Ctrl Pts',(-20.3293245606241,23.6597883855573,-66.0509965633325));
#10449=CARTESIAN_POINT('Ctrl Pts',(-20.3303461945029,23.6859883444558,-66.0493465705868));
#10450=CARTESIAN_POINT('Ctrl Pts',(-20.3307906617731,23.6961508041276,-66.048708988274));
#10451=CARTESIAN_POINT('Ctrl Pts',(-20.3314383767592,23.70951100598,-66.0478741142288));
#10452=CARTESIAN_POINT('Ctrl Pts',(-20.3315982807305,23.712710645089,-66.0476744213109));
#10453=CARTESIAN_POINT('Ctrl Pts',(-20.3318680094599,23.7179510898089,-66.0473477771433));
#10454=CARTESIAN_POINT('Ctrl Pts',(-20.3319750044374,23.7199920290454,-66.0472206663492));
#10455=CARTESIAN_POINT('Ctrl Pts',(-20.3321846289019,23.7239191773237,-66.0469762829433));
#10456=CARTESIAN_POINT('Ctrl Pts',(-20.3322869750421,23.7258053926814,-66.0468589949062));
#10457=CARTESIAN_POINT('Ctrl Pts',(-20.3325268216191,23.7301550177445,-66.0465887329923));
#10458=CARTESIAN_POINT('Ctrl Pts',(-20.3326654929226,23.7326183667406,-66.0464358255604));
#10459=CARTESIAN_POINT('Ctrl Pts',(-20.3331060860646,23.740288073287,-66.0459602093124));
#10460=CARTESIAN_POINT('Ctrl Pts',(-20.333417818543,23.7454938922348,-66.0456380522005));
#10461=CARTESIAN_POINT('Ctrl Pts',(-20.3361580519968,23.7894656839561,-66.0429223695984));
#10462=CARTESIAN_POINT('Ctrl Pts',(-20.339274699465,23.8281876823985,-66.040566829082));
#10463=CARTESIAN_POINT('Ctrl Pts',(-20.3509521209117,23.9464825570983,-66.0334549623437));
#10464=CARTESIAN_POINT('Ctrl Pts',(-20.3617774855371,24.0258050545676,-66.0288028831895));
#10465=CARTESIAN_POINT('Ctrl Pts',(-20.376597460673,24.1106706183992,-66.0238746054057));
#10466=CARTESIAN_POINT('Ctrl Pts',(-20.3776663405971,24.1166903503323,-66.0235252986384));
#10467=CARTESIAN_POINT('Ctrl Pts',(-20.4168161095592,24.3335870648009,-66.0109480129169));
#10468=CARTESIAN_POINT('Ctrl Pts',(-20.4758177940231,24.5401487425338,-65.999225405155));
#10469=CARTESIAN_POINT('Ctrl Pts',(-20.5839751111098,24.8126037914481,-65.9825878293227));
#10470=CARTESIAN_POINT('Ctrl Pts',(-20.6157395292472,24.8847804459965,-65.9780642828652));
#10471=CARTESIAN_POINT('Ctrl Pts',(-20.6902557313299,25.0385425272825,-65.9680903897113));
#10472=CARTESIAN_POINT('Ctrl Pts',(-20.7339210691164,25.119603807354,-65.9626159874945));
#10473=CARTESIAN_POINT('Ctrl Pts',(-20.7862491274754,25.2075118283918,-65.9563889441812));
#10474=CARTESIAN_POINT('Ctrl Pts',(-20.7915483464408,25.2163180794572,-65.955761829817));
#10475=CARTESIAN_POINT('Ctrl Pts',(-20.79929975123,25.2290609992165,-65.9548494941112));
#10476=CARTESIAN_POINT('Ctrl Pts',(-20.8017184910905,25.2330180228588,-65.9545655021346));
#10477=CARTESIAN_POINT('Ctrl Pts',(-20.8059330822063,25.239879704705,-65.9540718454801));
#10478=CARTESIAN_POINT('Ctrl Pts',(-20.8077250290423,25.2427867622688,-65.9538623249818));
#10479=CARTESIAN_POINT('Ctrl Pts',(-20.8111808851454,25.2483732652159,-65.9534589637519));
#10480=CARTESIAN_POINT('Ctrl Pts',(-20.8128441148118,25.2510531283566,-65.9532651482984));
#10481=CARTESIAN_POINT('Ctrl Pts',(-20.8167737117797,25.2573639586262,-65.9528079693355));
#10482=CARTESIAN_POINT('Ctrl Pts',(-20.8190433800895,25.2609928547121,-65.9525444837134));
#10483=CARTESIAN_POINT('Ctrl Pts',(-20.8257739466888,25.2717065964667,-65.9517648146901));
#10484=CARTESIAN_POINT('Ctrl Pts',(-20.8302552056885,25.2787785516528,-65.9512478755268));
#10485=CARTESIAN_POINT('Ctrl Pts',(-20.870072421047,25.3410765560734,-65.9466736298149));
#10486=CARTESIAN_POINT('Ctrl Pts',(-20.9070561832937,25.395226286189,-65.942554861094));
#10487=CARTESIAN_POINT('Ctrl Pts',(-20.9604878088709,25.4685512238273,-65.9367697573062));
#10488=CARTESIAN_POINT('Ctrl Pts',(-20.9755497043263,25.4887200931725,-65.9351559316431));
#10489=CARTESIAN_POINT('Ctrl Pts',(-21.0411390212128,25.5744353703378,-65.9281996764234));
#10490=CARTESIAN_POINT('Ctrl Pts',(-21.0939415722647,25.6381944589174,-65.9227756631486));
#10491=CARTESIAN_POINT('Ctrl Pts',(-21.2836306839833,25.8500789202452,-65.9038972433279));
#10492=CARTESIAN_POINT('Ctrl Pts',(-21.4319252662477,25.9873526558733,-65.8901091452807));
#10493=CARTESIAN_POINT('Ctrl Pts',(-21.6534421512529,26.1568214640361,-65.8713947368684));
#10494=CARTESIAN_POINT('Ctrl Pts',(-21.7165013708092,26.20156341534,-65.8662574186317));
#10495=CARTESIAN_POINT('Ctrl Pts',(-21.8258949496183,26.2734086115919,-65.8577322747955));
#10496=CARTESIAN_POINT('Ctrl Pts',(-21.8714075916385,26.3017009857231,-65.8542927731693));
#10497=CARTESIAN_POINT('Ctrl Pts',(-21.9230549128523,26.3320478851358,-65.8505258811924));
#10498=CARTESIAN_POINT('Ctrl Pts',(-21.9285115990882,26.3352325726073,-65.8501295683718));
#10499=CARTESIAN_POINT('Ctrl Pts',(-21.938180106578,26.3408373546107,-65.8494303534324));
#10500=CARTESIAN_POINT('Ctrl Pts',(-21.9423880793123,26.3432639998438,-65.8491270378504));
#10501=CARTESIAN_POINT('Ctrl Pts',(-21.9486638510636,26.3468642160915,-65.8486761791317));
#10502=CARTESIAN_POINT('Ctrl Pts',(-21.9507274635199,26.3480450135629,-65.8485281687665));
#10503=CARTESIAN_POINT('Ctrl Pts',(-21.9542719978574,26.3500679899822,-65.8482743584731));
#10504=CARTESIAN_POINT('Ctrl Pts',(-21.9557522812448,26.3509112785297,-65.848168486018));
#10505=CARTESIAN_POINT('Ctrl Pts',(-21.9587848209065,26.3526356735627,-65.8479518498738));
#10506=CARTESIAN_POINT('Ctrl Pts',(-21.9603371373238,26.3535166625052,-65.8478410939265));
#10507=CARTESIAN_POINT('Ctrl Pts',(-21.9640619537037,26.3556265250596,-65.8475756595906));
#10508=CARTESIAN_POINT('Ctrl Pts',(-21.9662351549828,26.3568541676111,-65.8474210614054));
#10509=CARTESIAN_POINT('Ctrl Pts',(-21.974094335219,26.3612817866544,-65.8468629256106));
#10510=CARTESIAN_POINT('Ctrl Pts',(-21.979788652505,26.3644670470569,-65.846460334859));
#10511=CARTESIAN_POINT('Ctrl Pts',(-22.0150892582465,26.3840728234639,-65.8439754576728));
#10512=CARTESIAN_POINT('Ctrl Pts',(-22.0449407953315,26.4000419887913,-65.8419214485363));
#10513=CARTESIAN_POINT('Ctrl Pts',(-22.0750360187516,26.4155367763096,-65.8398919625532));
#10514=CARTESIAN_POINT('Origin',(-23.5502525316942,23.5502525316942,-77.3107734492734));
#10515=CARTESIAN_POINT('',(-22.0750359910842,26.4155367620648,-64.3441594845823));
#10516=CARTESIAN_POINT('',(-22.0750364910777,26.4155370194908,-64.5943742034087));
#10517=CARTESIAN_POINT('',(-22.0750360153461,26.4155367745563,-77.3107734492734));
#10518=CARTESIAN_POINT('Ctrl Pts',(-22.0750359910842,26.4155367620648,-64.3441594845823));
#10519=CARTESIAN_POINT('Ctrl Pts',(-22.0084775746858,26.3812685817053,-64.3484810791895));
#10520=CARTESIAN_POINT('Ctrl Pts',(-21.9431278129034,26.3446888022705,-64.3528636214976));
#10521=CARTESIAN_POINT('Ctrl Pts',(-21.8515820913567,26.2891706466032,-64.3592437283574));
#10522=CARTESIAN_POINT('Ctrl Pts',(-21.8243111707936,26.2720681043922,-64.3611759736847));
#10523=CARTESIAN_POINT('Ctrl Pts',(-21.7861117718246,26.2473069932409,-64.3639298983731));
#10524=CARTESIAN_POINT('Ctrl Pts',(-21.7749670867899,26.2399842971329,-64.3647391556141));
#10525=CARTESIAN_POINT('Ctrl Pts',(-21.7555470637995,26.2270509552216,-64.3661596662074));
#10526=CARTESIAN_POINT('Ctrl Pts',(-21.7472517372968,26.2214705401223,-64.3667697805453));
#10527=CARTESIAN_POINT('Ctrl Pts',(-21.7352452175298,26.2133121309472,-64.3676577640849));
#10528=CARTESIAN_POINT('Ctrl Pts',(-21.7315132110083,26.2107647498029,-64.3679344709718));
#10529=CARTESIAN_POINT('Ctrl Pts',(-21.7249740185168,26.2062810596693,-64.3684205385899));
#10530=CARTESIAN_POINT('Ctrl Pts',(-21.7221645192869,26.2043481235735,-64.3686297706183));
#10531=CARTESIAN_POINT('Ctrl Pts',(-21.7167573910592,26.2006153594685,-64.3690332259458));
#10532=CARTESIAN_POINT('Ctrl Pts',(-21.7141593296882,26.1988161618546,-64.3692274250124));
#10533=CARTESIAN_POINT('Ctrl Pts',(-21.7080284530673,26.1945570789215,-64.3696865084634));
#10534=CARTESIAN_POINT('Ctrl Pts',(-21.704497917967,26.1920939349554,-64.3699515174799));
#10535=CARTESIAN_POINT('Ctrl Pts',(-21.6922246468617,26.1834946454349,-64.3708750150888));
#10536=CARTESIAN_POINT('Ctrl Pts',(-21.6835075622683,26.1773221663067,-64.37153489844));
#10537=CARTESIAN_POINT('Ctrl Pts',(-21.5768025895898,26.1009662047092,-64.3796618097773));
#10538=CARTESIAN_POINT('Ctrl Pts',(-21.4828077900383,26.025391102516,-64.3873395839952));
#10539=CARTESIAN_POINT('Ctrl Pts',(-21.2498789545496,25.815566319872,-64.4078021367379));
#10540=CARTESIAN_POINT('Ctrl Pts',(-21.1183904879827,25.6737866426231,-64.4208607883527));
#10541=CARTESIAN_POINT('Ctrl Pts',(-20.8887423269359,25.3766725275494,-64.446270166219));
#10542=CARTESIAN_POINT('Ctrl Pts',(-20.7895581058479,25.222983601362,-64.4585674495632));
#10543=CARTESIAN_POINT('Ctrl Pts',(-20.6964671288916,25.0476765591401,-64.4711222455995));
#10544=CARTESIAN_POINT('Ctrl Pts',(-20.6891215500973,25.0335931446805,-64.4721209451804));
#10545=CARTESIAN_POINT('Ctrl Pts',(-20.6801699156034,25.0161165819596,-64.4733475352088));
#10546=CARTESIAN_POINT('Ctrl Pts',(-20.6784654364786,25.0127745032014,-64.4735815263109));
#10547=CARTESIAN_POINT('Ctrl Pts',(-20.6757926564775,25.007511128204,-64.4739491256729));
#10548=CARTESIAN_POINT('Ctrl Pts',(-20.6748204438805,25.0055918391305,-64.4740829809821));
#10549=CARTESIAN_POINT('Ctrl Pts',(-20.673008384112,25.0020056655004,-64.4743327321288));
#10550=CARTESIAN_POINT('Ctrl Pts',(-20.6721680686603,25.0003390360046,-64.4744486571299));
#10551=CARTESIAN_POINT('Ctrl Pts',(-20.6702867582708,24.9965996844143,-64.4747084321549));
#10552=CARTESIAN_POINT('Ctrl Pts',(-20.6692465550754,24.9945265725363,-64.4748522315438));
#10553=CARTESIAN_POINT('Ctrl Pts',(-20.6666120101656,24.9892617859158,-64.4752168623901));
#10554=CARTESIAN_POINT('Ctrl Pts',(-20.6650207239631,24.9860685739065,-64.475437501277));
#10555=CARTESIAN_POINT('Ctrl Pts',(-20.6563303676989,24.9685569713673,-64.4766446868571));
#10556=CARTESIAN_POINT('Ctrl Pts',(-20.6493324135397,24.954188238129,-64.4776249696025));
#10557=CARTESIAN_POINT('Ctrl Pts',(-20.5098795455314,24.6623579628047,-64.4973399133489));
#10558=CARTESIAN_POINT('Ctrl Pts',(-20.4176714462195,24.3673543489121,-64.5138332240417));
#10559=CARTESIAN_POINT('Ctrl Pts',(-20.3469327428879,23.9290283165571,-64.5389124052299));
#10560=CARTESIAN_POINT('Ctrl Pts',(-20.3337731321219,23.7931171707693,-64.5467450929553));
#10561=CARTESIAN_POINT('Ctrl Pts',(-20.3280383951876,23.6197368363614,-64.5570465088034));
#10562=CARTESIAN_POINT('Ctrl Pts',(-20.3274523232119,23.5826663728547,-64.5592663933931));
#10563=CARTESIAN_POINT('Ctrl Pts',(-20.3275273054129,23.5307812835165,-64.5624010924372));
#10564=CARTESIAN_POINT('Ctrl Pts',(-20.3276508546704,23.5159679355008,-64.5632992090104));
#10565=CARTESIAN_POINT('Ctrl Pts',(-20.3280423601303,23.4902719908224,-64.5648628157977));
#10566=CARTESIAN_POINT('Ctrl Pts',(-20.3282633342853,23.4793888440484,-64.5655268300316));
#10567=CARTESIAN_POINT('Ctrl Pts',(-20.3286581482601,23.4638286129281,-64.5664788064188));
#10568=CARTESIAN_POINT('Ctrl Pts',(-20.3287870479838,23.4591503802086,-64.5667653570792));
#10569=CARTESIAN_POINT('Ctrl Pts',(-20.3290283686361,23.4510341551103,-64.5672630801536));
#10570=CARTESIAN_POINT('Ctrl Pts',(-20.3291361047578,23.4475960224315,-64.5674741051214));
#10571=CARTESIAN_POINT('Ctrl Pts',(-20.3293522008616,23.441035394379,-64.567877134347));
#10572=CARTESIAN_POINT('Ctrl Pts',(-20.3294595975921,23.4379128692212,-64.5680691081167));
#10573=CARTESIAN_POINT('Ctrl Pts',(-20.3297206372422,23.4306314665606,-64.568517128443));
#10574=CARTESIAN_POINT('Ctrl Pts',(-20.3298777953998,23.4264727272431,-64.5687732852181));
#10575=CARTESIAN_POINT('Ctrl Pts',(-20.3304598049535,23.4118235253342,-64.5696765661007));
#10576=CARTESIAN_POINT('Ctrl Pts',(-20.3309278606915,23.4013349321328,-64.5703250463653));
#10577=CARTESIAN_POINT('Ctrl Pts',(-20.3365452090676,23.2879049411231,-64.5773573359795));
#10578=CARTESIAN_POINT('Ctrl Pts',(-20.3465782443687,23.1852756028663,-64.5838943922424));
#10579=CARTESIAN_POINT('Ctrl Pts',(-20.4060154570113,22.7793781670115,-64.6104853455971));
#10580=CARTESIAN_POINT('Ctrl Pts',(-20.4937502045334,22.4833821449497,-64.6317241747065));
#10581=CARTESIAN_POINT('Ctrl Pts',(-20.6518914266499,22.1393149607181,-64.6568511046693));
#10582=CARTESIAN_POINT('Ctrl Pts',(-20.6839480802668,22.0752805648507,-64.6615372176698));
#10583=CARTESIAN_POINT('Ctrl Pts',(-20.7323073995062,21.9862232721645,-64.6680164563072));
#10584=CARTESIAN_POINT('Ctrl Pts',(-20.7468632105,21.9602805940074,-64.6698990991851));
#10585=CARTESIAN_POINT('Ctrl Pts',(-20.7640311246103,21.9306513298193,-64.6720404667309));
#10586=CARTESIAN_POINT('Ctrl Pts',(-20.7662936582714,21.9267653053561,-64.6723211412749));
#10587=CARTESIAN_POINT('Ctrl Pts',(-20.7697318467019,21.9208883524733,-64.6727453314218));
#10588=CARTESIAN_POINT('Ctrl Pts',(-20.7709015108361,21.9188939533509,-64.6728892349461));
#10589=CARTESIAN_POINT('Ctrl Pts',(-20.7729284809082,21.9154462659832,-64.6731379109511));
#10590=CARTESIAN_POINT('Ctrl Pts',(-20.7737847804196,21.9139923947776,-64.6732427491346));
#10591=CARTESIAN_POINT('Ctrl Pts',(-20.7755722933839,21.9109629028236,-64.6734611477751));
#10592=CARTESIAN_POINT('Ctrl Pts',(-20.776503704683,21.9093874071681,-64.6735746945929));
#10593=CARTESIAN_POINT('Ctrl Pts',(-20.7790788108016,21.9050400359595,-64.6738879260228));
#10594=CARTESIAN_POINT('Ctrl Pts',(-20.7807253276463,21.9022698213049,-64.6740874255486));
#10595=CARTESIAN_POINT('Ctrl Pts',(-20.78717294842,21.8914588486191,-64.6748656288738));
#10596=CARTESIAN_POINT('Ctrl Pts',(-20.7920049981257,21.8834364604938,-64.6754423260525));
#10597=CARTESIAN_POINT('Ctrl Pts',(-20.8789081821557,21.7405686269903,-64.6857007361399));
#10598=CARTESIAN_POINT('Ctrl Pts',(-20.9707556639953,21.6118905156386,-64.6947565376803));
#10599=CARTESIAN_POINT('Ctrl Pts',(-21.1930141557245,21.3444457292551,-64.7143569741985));
#10600=CARTESIAN_POINT('Ctrl Pts',(-21.3270095794678,21.2094519330233,-64.7248084373697));
#10601=CARTESIAN_POINT('Ctrl Pts',(-21.5274882734812,21.0403138282139,-64.7397589892878));
#10602=CARTESIAN_POINT('Ctrl Pts',(-21.5844256504558,20.9954744038096,-64.7439350265669));
#10603=CARTESIAN_POINT('Ctrl Pts',(-21.7053186096723,20.9067041795223,-64.7527190482942));
#10604=CARTESIAN_POINT('Ctrl Pts',(-21.7694451687668,20.8630880947484,-64.7573339473016));
#10605=CARTESIAN_POINT('Ctrl Pts',(-21.8436777602657,20.8164231135643,-64.7626541752363));
#10606=CARTESIAN_POINT('Ctrl Pts',(-21.8523026932483,20.8110579273722,-64.7632719803187));
#10607=CARTESIAN_POINT('Ctrl Pts',(-21.8677795977599,20.8015316197536,-64.764380055032));
#10608=CARTESIAN_POINT('Ctrl Pts',(-21.8746220312211,20.7973551036713,-64.7648697547831));
#10609=CARTESIAN_POINT('Ctrl Pts',(-21.8850055717176,20.7910702055615,-64.7656126297876));
#10610=CARTESIAN_POINT('Ctrl Pts',(-21.8885352926462,20.7889429938562,-64.7658651140137));
#10611=CARTESIAN_POINT('Ctrl Pts',(-21.8946734647236,20.785259811889,-64.7663041101236));
#10612=CARTESIAN_POINT('Ctrl Pts',(-21.897280059026,20.7837007443487,-64.7664905083976));
#10613=CARTESIAN_POINT('Ctrl Pts',(-21.9026605916014,20.780492835461,-64.7668752265745));
#10614=CARTESIAN_POINT('Ctrl Pts',(-21.905434809492,20.7788444714209,-64.7670735636509));
#10615=CARTESIAN_POINT('Ctrl Pts',(-21.9129272587672,20.7744078766154,-64.7676091572903));
#10616=CARTESIAN_POINT('Ctrl Pts',(-21.9176501187945,20.7716275193373,-64.7679467002215));
#10617=CARTESIAN_POINT('Ctrl Pts',(-21.9350924264228,20.7614190194848,-64.7691930694488));
#10618=CARTESIAN_POINT('Ctrl Pts',(-21.9478555137149,20.7540661449043,-64.7701046225956));
#10619=CARTESIAN_POINT('Ctrl Pts',(-22.1677017608547,20.6294111904787,-64.785799947218));
#10620=CARTESIAN_POINT('Ctrl Pts',(-22.3870562334042,20.5353411152424,-64.8014488807902));
#10621=CARTESIAN_POINT('Ctrl Pts',(-22.7401388933511,20.4282320765578,-64.8263312982326));
#10622=CARTESIAN_POINT('Ctrl Pts',(-22.8677648278742,20.3978714285454,-64.8352487519946));
#10623=CARTESIAN_POINT('Ctrl Pts',(-23.1259038387993,20.3528790371021,-64.8528230810683));
#10624=CARTESIAN_POINT('Ctrl Pts',(-23.256191406017,20.338273989027,-64.8614630370889));
#10625=CARTESIAN_POINT('Ctrl Pts',(-23.3950345738884,20.3312325997467,-64.8701922570326));
#10626=CARTESIAN_POINT('Ctrl Pts',(-23.4030492212365,20.3308561402308,-64.8706944486077));
#10627=CARTESIAN_POINT('Ctrl Pts',(-23.4139876204163,20.3303832808681,-64.8713774465911));
#10628=CARTESIAN_POINT('Ctrl Pts',(-23.4169101330973,20.3302609286989,-64.8715596963508));
#10629=CARTESIAN_POINT('Ctrl Pts',(-23.421799257455,20.330062911183,-64.8718641907764));
#10630=CARTESIAN_POINT('Ctrl Pts',(-23.4237657716375,20.3299850683783,-64.8719865584346));
#10631=CARTESIAN_POINT('Ctrl Pts',(-23.4276380685225,20.3298353393001,-64.8722273028572));
#10632=CARTESIAN_POINT('Ctrl Pts',(-23.429543843673,20.3297633433386,-64.8723456856256));
#10633=CARTESIAN_POINT('Ctrl Pts',(-23.4337450111862,20.3296083669575,-64.8726064326707));
#10634=CARTESIAN_POINT('Ctrl Pts',(-23.4360404346669,20.3295261485382,-64.8727487537845));
#10635=CARTESIAN_POINT('Ctrl Pts',(-23.4440544510336,20.3292476774796,-64.8732451389146));
#10636=CARTESIAN_POINT('Ctrl Pts',(-23.4497735207077,20.3290641992999,-64.8735984856536));
#10637=CARTESIAN_POINT('Ctrl Pts',(-23.5073974232693,20.3273691344772,-64.877150021335));
#10638=CARTESIAN_POINT('Ctrl Pts',(-23.5593347415253,20.3270969005148,-64.8802800062925));
#10639=CARTESIAN_POINT('Ctrl Pts',(-23.6153102502501,20.3281567121641,-64.883598443716));
#10640=CARTESIAN_POINT('Ctrl Pts',(-23.6193608730062,20.3282410459234,-64.8838382695989));
#10641=CARTESIAN_POINT('Ctrl Pts',(-23.6386744084126,20.3286795904975,-64.8849803353228));
#10642=CARTESIAN_POINT('Ctrl Pts',(-23.6539350651345,20.3291346215477,-64.8858784725239));
#10643=CARTESIAN_POINT('Ctrl Pts',(-23.7236106389784,20.331707838893,-64.8899618954145));
#10644=CARTESIAN_POINT('Ctrl Pts',(-23.7779719198492,20.3350966444877,-64.8930999500953));
#10645=CARTESIAN_POINT('Ctrl Pts',(-24.0754586274404,20.3612251160705,-64.9101323130097));
#10646=CARTESIAN_POINT('Ctrl Pts',(-24.3154784023278,20.4101610528416,-64.9234219151308));
#10647=CARTESIAN_POINT('Ctrl Pts',(-24.6678242733373,20.5248408861135,-64.9446601460147));
#10648=CARTESIAN_POINT('Ctrl Pts',(-24.7855551141297,20.5709734163339,-64.9520593529787));
#10649=CARTESIAN_POINT('Ctrl Pts',(-24.9125952590026,20.6295806521088,-64.9605212875044));
#10650=CARTESIAN_POINT('Ctrl Pts',(-24.9248886397403,20.6353464446022,-64.9613451697864));
#10651=CARTESIAN_POINT('Ctrl Pts',(-24.9463086210551,20.6455583973451,-64.962789708507));
#10652=CARTESIAN_POINT('Ctrl Pts',(-24.9554513925886,20.6499703425965,-64.9634091756339));
#10653=CARTESIAN_POINT('Ctrl Pts',(-24.968655581336,20.6564192618527,-64.9643080690396));
#10654=CARTESIAN_POINT('Ctrl Pts',(-24.9727338403987,20.6584217740381,-64.9645862909656));
#10655=CARTESIAN_POINT('Ctrl Pts',(-24.9798697105791,20.6619443860795,-64.9650741432868));
#10656=CARTESIAN_POINT('Ctrl Pts',(-24.9829291728245,20.6634607373312,-64.9652836421277));
#10657=CARTESIAN_POINT('Ctrl Pts',(-24.9888100104368,20.6663870890744,-64.965686984105));
#10658=CARTESIAN_POINT('Ctrl Pts',(-24.9916317386184,20.6677963754775,-64.965880802002));
#10659=CARTESIAN_POINT('Ctrl Pts',(-24.9982783307557,20.6711281555412,-64.9663380210937));
#10660=CARTESIAN_POINT('Ctrl Pts',(-25.0021014355396,20.6730541290403,-64.9666015444737));
#10661=CARTESIAN_POINT('Ctrl Pts',(-25.0133927590193,20.6787706180989,-64.9673814271176));
#10662=CARTESIAN_POINT('Ctrl Pts',(-25.020850008822,20.6825826129165,-64.9678985427631));
#10663=CARTESIAN_POINT('Ctrl Pts',(-25.0866306501116,20.716532406551,-64.9724783304947));
#10664=CARTESIAN_POINT('Ctrl Pts',(-25.1440316224621,20.7484148034575,-64.9766026292053));
#10665=CARTESIAN_POINT('Ctrl Pts',(-25.2184300823927,20.7927643540135,-64.9821256712295));
#10666=CARTESIAN_POINT('Ctrl Pts',(-25.2363387576014,20.8036781931366,-64.9834690697035));
#10667=CARTESIAN_POINT('Ctrl Pts',(-25.3657100929598,20.8842613338654,-64.993275683542));
#10668=CARTESIAN_POINT('Ctrl Pts',(-25.4729128456745,20.9605100884085,-65.0019640912593));
#10669=CARTESIAN_POINT('Ctrl Pts',(-25.6479902492708,21.1019102060086,-65.017069013421));
#10670=CARTESIAN_POINT('Ctrl Pts',(-25.7182290019193,21.1638827065062,-65.0234113527737));
#10671=CARTESIAN_POINT('Ctrl Pts',(-25.9288228742058,21.366673677364,-65.0431971872683));
#10672=CARTESIAN_POINT('Ctrl Pts',(-26.0589397445547,21.5174900122687,-65.0565987601438));
#10673=CARTESIAN_POINT('Ctrl Pts',(-26.177921314709,21.6843714203939,-65.0694416680976));
#10674=CARTESIAN_POINT('Ctrl Pts',(-26.1814852000778,21.6894005222466,-65.0698269501758));
#10675=CARTESIAN_POINT('Ctrl Pts',(-26.1865493999315,21.6965903984527,-65.0703752433461));
#10676=CARTESIAN_POINT('Ctrl Pts',(-26.1880615028128,21.6987427926714,-65.070539061005));
#10677=CARTESIAN_POINT('Ctrl Pts',(-26.1906664955088,21.702460523155,-65.0708214571442));
#10678=CARTESIAN_POINT('Ctrl Pts',(-26.1917606311474,21.7040249813298,-65.0709401219274));
#10679=CARTESIAN_POINT('Ctrl Pts',(-26.1938609160099,21.7070337787279,-65.0711680119013));
#10680=CARTESIAN_POINT('Ctrl Pts',(-26.1948672701956,21.7084779673543,-65.0712772514315));
#10681=CARTESIAN_POINT('Ctrl Pts',(-26.1972444204015,21.7118953096053,-65.0715354007722));
#10682=CARTESIAN_POINT('Ctrl Pts',(-26.1986141964559,21.7138691764011,-65.0716842400786));
#10683=CARTESIAN_POINT('Ctrl Pts',(-26.2026809556031,21.719743448047,-65.0721263972778));
#10684=CARTESIAN_POINT('Ctrl Pts',(-26.2053715538687,21.7236482975918,-65.0724192792467));
#10685=CARTESIAN_POINT('Ctrl Pts',(-26.2297959281024,21.7592632427426,-65.075081280745));
#10686=CARTESIAN_POINT('Ctrl Pts',(-26.2509704725904,21.7913556129217,-65.0774130830908));
#10687=CARTESIAN_POINT('Ctrl Pts',(-26.4396209105045,22.0887187542884,-65.0984884994713));
#10688=CARTESIAN_POINT('Ctrl Pts',(-26.5681213071658,22.3767700032099,-65.1152300366911));
#10689=CARTESIAN_POINT('Ctrl Pts',(-26.6794214422486,22.7730835381143,-65.138680670615));
#10690=CARTESIAN_POINT('Ctrl Pts',(-26.7015696531645,22.8684257599818,-65.1443375690071));
#10691=CARTESIAN_POINT('Ctrl Pts',(-26.7308926452289,23.0271049178819,-65.1538864016768));
#10692=CARTESIAN_POINT('Ctrl Pts',(-26.7405880006278,23.0899116826497,-65.157699358001));
#10693=CARTESIAN_POINT('Ctrl Pts',(-26.7494553997721,23.1612935654842,-65.1620839835335));
#10694=CARTESIAN_POINT('Ctrl Pts',(-26.7504579544631,23.1696302537192,-65.1625968416013));
#10695=CARTESIAN_POINT('Ctrl Pts',(-26.751915400691,23.1821625360444,-65.1633690042969));
#10696=CARTESIAN_POINT('Ctrl Pts',(-26.7523946554713,23.1863553065399,-65.163627538691));
#10697=CARTESIAN_POINT('Ctrl Pts',(-26.7532049032219,23.1935693308576,-65.1640727202607));
#10698=CARTESIAN_POINT('Ctrl Pts',(-26.7535398609064,23.1965901412174,-65.164259241945));
#10699=CARTESIAN_POINT('Ctrl Pts',(-26.7542210321389,23.2028136338694,-65.1646437347373));
#10700=CARTESIAN_POINT('Ctrl Pts',(-26.7545667179524,23.2060163697634,-65.16484172231));
#10701=CARTESIAN_POINT('Ctrl Pts',(-26.7553876055673,23.213730175321,-65.1653188672145));
#10702=CARTESIAN_POINT('Ctrl Pts',(-26.7558580854776,23.2182417316635,-65.1655981733355));
#10703=CARTESIAN_POINT('Ctrl Pts',(-26.7572734846272,23.2320978769842,-65.1664567375372));
#10704=CARTESIAN_POINT('Ctrl Pts',(-26.7581870733668,23.2414455528069,-65.1670369829208));
#10705=CARTESIAN_POINT('Ctrl Pts',(-26.7684121882538,23.3510124847005,-65.1738506383671));
#10706=CARTESIAN_POINT('Ctrl Pts',(-26.7730637826178,23.4516008112041,-65.1802303852552));
#10707=CARTESIAN_POINT('Ctrl Pts',(-26.7729350406849,23.6610365978374,-65.1937925066299));
#10708=CARTESIAN_POINT('Ctrl Pts',(-26.7673583309661,23.7697571657355,-65.2009897763069));
#10709=CARTESIAN_POINT('Ctrl Pts',(-26.7270989511482,24.1636012495447,-65.2275235236627));
#10710=CARTESIAN_POINT('Ctrl Pts',(-26.659866716583,24.444042878652,-65.2474229664955));
#10711=CARTESIAN_POINT('Ctrl Pts',(-26.5507991379999,24.726295342832,-65.2665680271834));
#10712=CARTESIAN_POINT('Ctrl Pts',(-26.5451221681728,24.7406778815255,-65.2675406787582));
#10713=CARTESIAN_POINT('Ctrl Pts',(-26.537922087815,24.7585416560827,-65.2687446221201));
#10714=CARTESIAN_POINT('Ctrl Pts',(-26.5364961691152,24.7620614782761,-65.2689816425189));
#10715=CARTESIAN_POINT('Ctrl Pts',(-26.534162549184,24.7677927915935,-65.2693672446922));
#10716=CARTESIAN_POINT('Ctrl Pts',(-26.5332586089696,24.7700057936145,-65.2695160531767));
#10717=CARTESIAN_POINT('Ctrl Pts',(-26.5316420250063,24.7739509258093,-65.2697811858601));
#10718=CARTESIAN_POINT('Ctrl Pts',(-26.530930334254,24.7756834387575,-65.2698975679619));
#10719=CARTESIAN_POINT('Ctrl Pts',(-26.5294158455725,24.7793611273311,-65.2701445078536));
#10720=CARTESIAN_POINT('Ctrl Pts',(-26.5286126548516,24.781306132263,-65.2702750409053));
#10721=CARTESIAN_POINT('Ctrl Pts',(-26.5264531684644,24.7865210559381,-65.2706248534712));
#10722=CARTESIAN_POINT('Ctrl Pts',(-26.5250933841461,24.7897895409103,-65.2708439200457));
#10723=CARTESIAN_POINT('Ctrl Pts',(-26.51856952824,24.8053982276568,-65.2718892419742));
#10724=CARTESIAN_POINT('Ctrl Pts',(-26.5133339436695,24.8177086732732,-65.2727111883452));
#10725=CARTESIAN_POINT('Ctrl Pts',(-26.4701358269832,24.9175497899187,-65.2793598978412));
#10726=CARTESIAN_POINT('Ctrl Pts',(-26.4283760123026,25.0033971733467,-65.284967353444));
#10727=CARTESIAN_POINT('Ctrl Pts',(-26.195407156903,25.4327409028723,-65.3130707163497));
#10728=CARTESIAN_POINT('Ctrl Pts',(-25.9463529969348,25.7409944884951,-65.3339114055139));
#10729=CARTESIAN_POINT('Ctrl Pts',(-25.6333752698002,26.0093345444917,-65.3588609965977));
#10730=CARTESIAN_POINT('Ctrl Pts',(-25.6187185311786,26.0216758204029,-65.3600257966169));
#10731=CARTESIAN_POINT('Ctrl Pts',(-25.5992503583751,26.037773929074,-65.3615686288551));
#10732=CARTESIAN_POINT('Ctrl Pts',(-25.5945368512947,26.0416490107781,-65.3619418374649));
#10733=CARTESIAN_POINT('Ctrl Pts',(-25.5872176048275,26.0476315747174,-65.3625208637987));
#10734=CARTESIAN_POINT('Ctrl Pts',(-25.5846195179861,26.0497484326003,-65.3627263013991));
#10735=CARTESIAN_POINT('Ctrl Pts',(-25.5794211522793,26.0539704600855,-65.3631371581688));
#10736=CARTESIAN_POINT('Ctrl Pts',(-25.5768208876912,26.056075640785,-65.3633425765327));
#10737=CARTESIAN_POINT('Ctrl Pts',(-25.5710230100465,26.0607546898062,-65.3638003934027));
#10738=CARTESIAN_POINT('Ctrl Pts',(-25.5678237521995,26.0633265023534,-65.3640528742376));
#10739=CARTESIAN_POINT('Ctrl Pts',(-25.5584982857068,26.0707937533083,-65.3647884211801));
#10740=CARTESIAN_POINT('Ctrl Pts',(-25.5523591438132,26.0756729264667,-65.365272138872));
#10741=CARTESIAN_POINT('Ctrl Pts',(-25.5086157646266,26.110178865844,-65.3687152860815));
#10742=CARTESIAN_POINT('Ctrl Pts',(-25.47037500251,26.1389855590292,-65.3717071468882));
#10743=CARTESIAN_POINT('Ctrl Pts',(-25.3469472302823,26.2277237953631,-65.3813139794789));
#10744=CARTESIAN_POINT('Ctrl Pts',(-25.2594971712277,26.2843781960521,-65.3880499131564));
#10745=CARTESIAN_POINT('Ctrl Pts',(-25.0244234204579,26.4209804670512,-65.4059645346111));
#10746=CARTESIAN_POINT('Ctrl Pts',(-24.8730317143905,26.4938057603953,-65.4173281181204));
#10747=CARTESIAN_POINT('Ctrl Pts',(-24.542985623257,26.6219481622529,-65.4412827409213));
#10748=CARTESIAN_POINT('Ctrl Pts',(-24.3637519180212,26.6742035221455,-65.453825618138));
#10749=CARTESIAN_POINT('Ctrl Pts',(-24.1701065142083,26.7128498345631,-65.4662648202726));
#10750=CARTESIAN_POINT('Ctrl Pts',(-24.1592148256802,26.7149650925464,-65.4669607545297));
#10751=CARTESIAN_POINT('Ctrl Pts',(-24.144922231777,26.7176643161578,-65.4678689318156));
#10752=CARTESIAN_POINT('Ctrl Pts',(-24.1415311760027,26.7182990953681,-65.468084032759));
#10753=CARTESIAN_POINT('Ctrl Pts',(-24.1362945362004,26.7192706526495,-65.4684156200827));
#10754=CARTESIAN_POINT('Ctrl Pts',(-24.1344496797699,26.7196112640266,-65.4685323260258));
#10755=CARTESIAN_POINT('Ctrl Pts',(-24.1308053417288,26.7202808191979,-65.4687626458208));
#10756=CARTESIAN_POINT('Ctrl Pts',(-24.1290058881236,26.720609839832,-65.4688762632045));
#10757=CARTESIAN_POINT('Ctrl Pts',(-24.1252070837139,26.721301089216,-65.4691158944927));
#10758=CARTESIAN_POINT('Ctrl Pts',(-24.1232076765211,26.7216629581638,-65.4692418872324));
#10759=CARTESIAN_POINT('Ctrl Pts',(-24.1173152410103,26.7227236647679,-65.4696128161012));
#10760=CARTESIAN_POINT('Ctrl Pts',(-24.1134212487841,26.7234172300627,-65.4698574502076));
#10761=CARTESIAN_POINT('Ctrl Pts',(-24.1046992139936,26.7249541649067,-65.470404315691));
#10762=CARTESIAN_POINT('Ctrl Pts',(-24.0998704920695,26.7257936953081,-65.4707063307718));
#10763=CARTESIAN_POINT('Ctrl Pts',(-23.9168811976172,26.7571786581925,-65.4821240272049));
#10764=CARTESIAN_POINT('Ctrl Pts',(-23.7364364486107,26.7726970580989,-65.4924048748776));
#10765=CARTESIAN_POINT('Ctrl Pts',(-23.4809634182051,26.7731223422212,-65.506743911095));
#10766=CARTESIAN_POINT('Ctrl Pts',(-23.4063271725404,26.7706525756122,-65.510905695665));
#10767=CARTESIAN_POINT('Ctrl Pts',(-23.0879113990273,26.749023506195,-65.5287528544426));
#10768=CARTESIAN_POINT('Ctrl Pts',(-22.8466985244271,26.7047543808934,-65.5425816558037));
#10769=CARTESIAN_POINT('Ctrl Pts',(-22.597867796705,26.6291038221533,-65.5583548142092));
#10770=CARTESIAN_POINT('Ctrl Pts',(-22.5829442922181,26.6244478261717,-65.5593064272317));
#10771=CARTESIAN_POINT('Ctrl Pts',(-22.562705066674,26.6179714113744,-65.5606048596276));
#10772=CARTESIAN_POINT('Ctrl Pts',(-22.5573591899102,26.616245345062,-65.5609485683036));
#10773=CARTESIAN_POINT('Ctrl Pts',(-22.5489237998476,26.6134973672529,-65.5614921063162));
#10774=CARTESIAN_POINT('Ctrl Pts',(-22.5458312570651,26.6124847330051,-65.5616916290606));
#10775=CARTESIAN_POINT('Ctrl Pts',(-22.5398633786689,26.6105205746805,-65.5620771525766));
#10776=CARTESIAN_POINT('Ctrl Pts',(-22.536987838921,26.6095696773584,-65.5622631324607));
#10777=CARTESIAN_POINT('Ctrl Pts',(-22.5301840478873,26.6073091221488,-65.5627037027011));
#10778=CARTESIAN_POINT('Ctrl Pts',(-22.5262569788714,26.6059959463877,-65.5629584092901));
#10779=CARTESIAN_POINT('Ctrl Pts',(-22.5147376242487,26.6021192806462,-65.5637067694691));
#10780=CARTESIAN_POINT('Ctrl Pts',(-22.5071523974263,26.5995350513916,-65.5642011099872));
#10781=CARTESIAN_POINT('Ctrl Pts',(-22.4503080688531,26.5799316983751,-65.5679175901888));
#10782=CARTESIAN_POINT('Ctrl Pts',(-22.4014611003064,26.561749071201,-65.5711782838609));
#10783=CARTESIAN_POINT('Ctrl Pts',(-22.2584255701523,26.504519633226,-65.5809342208569));
#10784=CARTESIAN_POINT('Ctrl Pts',(-22.1656416631724,26.4621858811723,-65.5875364717936));
#10785=CARTESIAN_POINT('Ctrl Pts',(-22.0750359980476,26.41553676565,-65.5942565421953));
#10786=CARTESIAN_POINT('Ctrl Pts',(-22.0750360187516,26.4155367763096,-65.8398919625532));
#10787=CARTESIAN_POINT('Ctrl Pts',(-22.1314774174797,26.4445961213201,-65.8360858094642));
#10788=CARTESIAN_POINT('Ctrl Pts',(-22.1887759126829,26.471986968196,-65.8323658270479));
#10789=CARTESIAN_POINT('Ctrl Pts',(-22.512340525602,26.6150723552368,-65.8119484436766));
#10790=CARTESIAN_POINT('Ctrl Pts',(-22.7924736465595,26.6960712839078,-65.7963290618333));
#10791=CARTESIAN_POINT('Ctrl Pts',(-23.1612705816343,26.750504389791,-65.7748150913148));
#10792=CARTESIAN_POINT('Ctrl Pts',(-23.2432836255907,26.7594093343291,-65.769982713062));
#10793=CARTESIAN_POINT('Ctrl Pts',(-23.3679980260237,26.7681263728235,-65.7625092541809));
#10794=CARTESIAN_POINT('Ctrl Pts',(-23.4105056052571,26.770252422188,-65.7599403299434));
#10795=CARTESIAN_POINT('Ctrl Pts',(-23.4606764310766,26.7717664665596,-65.7568788778994));
#10796=CARTESIAN_POINT('Ctrl Pts',(-23.4683122732181,26.7719697295236,-65.756412134515));
#10797=CARTESIAN_POINT('Ctrl Pts',(-23.4800094694729,26.772239492129,-65.7556958905477));
#10798=CARTESIAN_POINT('Ctrl Pts',(-23.4840703831691,26.7723254644472,-65.75544700172));
#10799=CARTESIAN_POINT('Ctrl Pts',(-23.4914742764207,26.7724682069644,-65.7549928011584));
#10800=CARTESIAN_POINT('Ctrl Pts',(-23.4948172071824,26.7725274526021,-65.7547875674522));
#10801=CARTESIAN_POINT('Ctrl Pts',(-23.501536784661,26.7726360815994,-65.7543747107968));
#10802=CARTESIAN_POINT('Ctrl Pts',(-23.5049134286529,26.7726853599011,-65.7541670848094));
#10803=CARTESIAN_POINT('Ctrl Pts',(-23.5145185033408,26.7728104351126,-65.7535760154035));
#10804=CARTESIAN_POINT('Ctrl Pts',(-23.5207470597465,26.7728734817781,-65.7531921721055));
#10805=CARTESIAN_POINT('Ctrl Pts',(-23.5471574610716,26.7730642399325,-65.7515622104544));
#10806=CARTESIAN_POINT('Ctrl Pts',(-23.5673397404734,26.7730204233788,-65.7503107195909));
#10807=CARTESIAN_POINT('Ctrl Pts',(-23.5922482618142,26.7727323658301,-65.7487586128242));
#10808=CARTESIAN_POINT('Ctrl Pts',(-23.5969764628257,26.772667277911,-65.7484636524649));
#10809=CARTESIAN_POINT('Ctrl Pts',(-23.6133326716906,26.7724061139555,-65.7474421317708));
#10810=CARTESIAN_POINT('Ctrl Pts',(-23.6249596448422,26.772157504418,-65.7467139311696));
#10811=CARTESIAN_POINT('Ctrl Pts',(-23.6413024748774,26.7717195487347,-65.7456874630577));
#10812=CARTESIAN_POINT('Ctrl Pts',(-23.6460197500507,26.7715827652374,-65.7453908371267));
#10813=CARTESIAN_POINT('Ctrl Pts',(-23.6572498467769,26.7712324446381,-65.744683863835));
#10814=CARTESIAN_POINT('Ctrl Pts',(-23.6637623358899,26.7710095154437,-65.7442732265932));
#10815=CARTESIAN_POINT('Ctrl Pts',(-23.672156800396,26.7706966720861,-65.7437430760183));
#10816=CARTESIAN_POINT('Ctrl Pts',(-23.6740394698188,26.7706248558266,-65.7436241214735));
#10817=CARTESIAN_POINT('Ctrl Pts',(-23.6828619587963,26.7702805653793,-65.7430664235186));
#10818=CARTESIAN_POINT('Ctrl Pts',(-23.6898009081286,26.769987310725,-65.7426270419655));
#10819=CARTESIAN_POINT('Ctrl Pts',(-23.7016143350283,26.7694497898516,-65.7418777228726));
#10820=CARTESIAN_POINT('Ctrl Pts',(-23.7064893261831,26.7692168754028,-65.7415681334758));
#10821=CARTESIAN_POINT('Ctrl Pts',(-23.7153710777188,26.7687723043821,-65.7410034134315));
#10822=CARTESIAN_POINT('Ctrl Pts',(-23.719378014702,26.7685642369506,-65.7407483923209));
#10823=CARTESIAN_POINT('Ctrl Pts',(-23.99917912757,26.7535110732843,-65.7229228557281));
#10824=CARTESIAN_POINT('Ctrl Pts',(-24.2718791504951,26.7032826107241,-65.7042041508269));
#10825=CARTESIAN_POINT('Ctrl Pts',(-24.6986824843514,26.5663524062377,-65.673923930312));
#10826=CARTESIAN_POINT('Ctrl Pts',(-24.8581408151541,26.5007091863637,-65.6624080022885));
#10827=CARTESIAN_POINT('Ctrl Pts',(-25.0184237292761,26.4191633638485,-65.6511201129068));
#10828=CARTESIAN_POINT('Ctrl Pts',(-25.0252264501066,26.4156718676909,-65.6506416227527));
#10829=CARTESIAN_POINT('Ctrl Pts',(-25.0345590548929,26.4108398671108,-65.6499860649508));
#10830=CARTESIAN_POINT('Ctrl Pts',(-25.0370996043509,26.4095201898614,-65.649807696919));
#10831=CARTESIAN_POINT('Ctrl Pts',(-25.0413832355585,26.4072878233483,-65.6495071058993));
#10832=CARTESIAN_POINT('Ctrl Pts',(-25.0431272399276,26.4063769231259,-65.6493847693261));
#10833=CARTESIAN_POINT('Ctrl Pts',(-25.0465605481488,26.4045796891342,-65.6491440210579));
#10834=CARTESIAN_POINT('Ctrl Pts',(-25.0482498992065,26.4036934525414,-65.6490256034622));
#10835=CARTESIAN_POINT('Ctrl Pts',(-25.0519731796792,26.4017359951345,-65.6487647050373));
#10836=CARTESIAN_POINT('Ctrl Pts',(-25.0540067554474,26.4006640952197,-65.6486222675436));
#10837=CARTESIAN_POINT('Ctrl Pts',(-25.0611078771453,26.3969113722204,-65.648125086871));
#10838=CARTESIAN_POINT('Ctrl Pts',(-25.0661694539003,26.3942191832906,-65.6477710640184));
#10839=CARTESIAN_POINT('Ctrl Pts',(-25.1173343843339,26.3668297973865,-65.6441958033327));
#10840=CARTESIAN_POINT('Ctrl Pts',(-25.1628404717761,26.3410255311583,-65.6410437648488));
#10841=CARTESIAN_POINT('Ctrl Pts',(-25.2113263328911,26.3119493389905,-65.6376935661277));
#10842=CARTESIAN_POINT('Ctrl Pts',(-25.2149470381323,26.3097683640534,-65.6374434390298));
#10843=CARTESIAN_POINT('Ctrl Pts',(-25.2265368853065,26.3027559699556,-65.6366429122394));
#10844=CARTESIAN_POINT('Ctrl Pts',(-25.2344894276581,26.2978970672107,-65.6360938134113));
#10845=CARTESIAN_POINT('Ctrl Pts',(-25.3259209822222,26.2414874361403,-65.629781664611));
#10846=CARTESIAN_POINT('Ctrl Pts',(-25.4070311544467,26.1861811378678,-65.6241900169108));
#10847=CARTESIAN_POINT('Ctrl Pts',(-25.542601059139,26.0843726693974,-65.6146362363909));
#10848=CARTESIAN_POINT('Ctrl Pts',(-25.5982654136853,26.0396020560029,-65.6106478055526));
#10849=CARTESIAN_POINT('Ctrl Pts',(-25.7739224121444,25.888438828471,-65.5976990712599));
#10850=CARTESIAN_POINT('Ctrl Pts',(-25.8874689116535,25.7749407931563,-65.5887375817911));
#10851=CARTESIAN_POINT('Ctrl Pts',(-26.0432893493065,25.5940331251387,-65.57492121108));
#10852=CARTESIAN_POINT('Ctrl Pts',(-26.0922952639063,25.5327481847895,-65.5703135740271));
#10853=CARTESIAN_POINT('Ctrl Pts',(-26.1627246385627,25.4377619558782,-65.5632347871806));
#10854=CARTESIAN_POINT('Ctrl Pts',(-26.1858398109791,25.4053487049488,-65.5608298025226));
#10855=CARTESIAN_POINT('Ctrl Pts',(-26.2125647979794,25.3663655726633,-65.5579465997368));
#10856=CARTESIAN_POINT('Ctrl Pts',(-26.2167603078255,25.360199895334,-65.5574908568229));
#10857=CARTESIAN_POINT('Ctrl Pts',(-26.223186077618,25.3506858148184,-65.5567880088567));
#10858=CARTESIAN_POINT('Ctrl Pts',(-26.2254315512978,25.347347676851,-65.5565414802568));
#10859=CARTESIAN_POINT('Ctrl Pts',(-26.2295133194141,25.3412550869365,-65.5560916615716));
#10860=CARTESIAN_POINT('Ctrl Pts',(-26.2313516341703,25.3385019897034,-65.5558884481435));
#10861=CARTESIAN_POINT('Ctrl Pts',(-26.2350653345793,25.3329216782839,-65.5554766472879));
#10862=CARTESIAN_POINT('Ctrl Pts',(-26.2369405039706,25.3300943258498,-65.5552680520602));
#10863=CARTESIAN_POINT('Ctrl Pts',(-26.2422886511229,25.3220027589538,-65.5546712155981));
#10864=CARTESIAN_POINT('Ctrl Pts',(-26.2457506314776,25.3167313255839,-65.5542825618004));
#10865=CARTESIAN_POINT('Ctrl Pts',(-26.2605810346517,25.294004492594,-65.5526076444245));
#10866=CARTESIAN_POINT('Ctrl Pts',(-26.2717953401025,25.2764495668755,-65.5513156350807));
#10867=CARTESIAN_POINT('Ctrl Pts',(-26.4700106112287,24.9594292678118,-65.5280107266666));
#10868=CARTESIAN_POINT('Ctrl Pts',(-26.6066807566537,24.6313990096662,-65.5039308927914));
#10869=CARTESIAN_POINT('Ctrl Pts',(-26.7193997442931,24.1520093008839,-65.4708344970097));
#10870=CARTESIAN_POINT('Ctrl Pts',(-26.7424932825477,24.014164935585,-65.4615962731825));
#10871=CARTESIAN_POINT('Ctrl Pts',(-26.7573960492333,23.867134849688,-65.4523156917197));
#10872=CARTESIAN_POINT('Ctrl Pts',(-26.7581869347573,23.859025611195,-65.4518056819921));
#10873=CARTESIAN_POINT('Ctrl Pts',(-26.7592216258119,23.8479832429826,-65.4511137953029));
#10874=CARTESIAN_POINT('Ctrl Pts',(-26.7594921706662,23.8450527407568,-65.4509304260897));
#10875=CARTESIAN_POINT('Ctrl Pts',(-26.7599372923853,23.8401580129626,-65.4506245699247));
#10876=CARTESIAN_POINT('Ctrl Pts',(-26.7601140805964,23.8381939979885,-65.4505019576399));
#10877=CARTESIAN_POINT('Ctrl Pts',(-26.76045806278,23.8343328683161,-65.4502611330765));
#10878=CARTESIAN_POINT('Ctrl Pts',(-26.760625377734,23.8324357681029,-65.4501429141497));
#10879=CARTESIAN_POINT('Ctrl Pts',(-26.7609898518722,23.8282608956167,-65.4498829858334));
#10880=CARTESIAN_POINT('Ctrl Pts',(-26.7611862694014,23.8259830554392,-65.4497413185837));
#10881=CARTESIAN_POINT('Ctrl Pts',(-26.7618420034747,23.8182828292119,-65.4492629194358));
#10882=CARTESIAN_POINT('Ctrl Pts',(-26.7622900132213,23.8128594507389,-65.4489268244761));
#10883=CARTESIAN_POINT('Ctrl Pts',(-26.7663327098574,23.7623620235274,-65.445805102344));
#10884=CARTESIAN_POINT('Ctrl Pts',(-26.76899235934,23.7172153464584,-65.443071098864));
#10885=CARTESIAN_POINT('Ctrl Pts',(-26.7708284766172,23.6686565330669,-65.4401772796194));
#10886=CARTESIAN_POINT('Ctrl Pts',(-26.7709505576056,23.6652879637579,-65.4399767746132));
#10887=CARTESIAN_POINT('Ctrl Pts',(-26.7711697273477,23.6589664249128,-65.4396009456666));
#10888=CARTESIAN_POINT('Ctrl Pts',(-26.7712680405932,23.6560135046231,-65.4394255698778));
#10889=CARTESIAN_POINT('Ctrl Pts',(-26.7715691168757,23.6465803808073,-65.4388658990904));
#10890=CARTESIAN_POINT('Ctrl Pts',(-26.7717563871692,23.6400996622086,-65.43848225231));
#10891=CARTESIAN_POINT('Ctrl Pts',(-26.7726273147288,23.6064426820705,-65.4364940671712));
#10892=CARTESIAN_POINT('Ctrl Pts',(-26.7729866680792,23.5792584294255,-65.4349026124946));
#10893=CARTESIAN_POINT('Ctrl Pts',(-26.773048947276,23.4689556087308,-65.4284919347338));
#10894=CARTESIAN_POINT('Ctrl Pts',(-26.7698804175324,23.3858637622659,-65.4237700562543));
#10895=CARTESIAN_POINT('Ctrl Pts',(-26.744464316596,23.0555827727251,-65.4051213362025));
#10896=CARTESIAN_POINT('Ctrl Pts',(-26.6969206326827,22.8112240568182,-65.3915218427683));
#10897=CARTESIAN_POINT('Ctrl Pts',(-26.5934761572848,22.4855120939023,-65.3715850037452));
#10898=CARTESIAN_POINT('Ctrl Pts',(-26.561265720256,22.3975690477003,-65.3660184613766));
#10899=CARTESIAN_POINT('Ctrl Pts',(-26.5213357508337,22.3016985358388,-65.3596965290186));
#10900=CARTESIAN_POINT('Ctrl Pts',(-26.5173506599199,22.2922575916068,-65.3590712056871));
#10901=CARTESIAN_POINT('Ctrl Pts',(-26.5117000674537,22.2790471839711,-65.3581922731352));
#10902=CARTESIAN_POINT('Ctrl Pts',(-26.5100722309835,22.2752615942449,-65.3579399501656));
#10903=CARTESIAN_POINT('Ctrl Pts',(-26.5070776569435,22.2683342504457,-65.3574773798299));
#10904=CARTESIAN_POINT('Ctrl Pts',(-26.5057131592454,22.2651915292661,-65.357267209307));
#10905=CARTESIAN_POINT('Ctrl Pts',(-26.5029430097323,22.2588390495612,-65.356841741466));
#10906=CARTESIAN_POINT('Ctrl Pts',(-26.5015371297971,22.2556293966555,-65.3566264365744));
#10907=CARTESIAN_POINT('Ctrl Pts',(-26.4980727518136,22.247755119588,-65.3560974051145));
#10908=CARTESIAN_POINT('Ctrl Pts',(-26.4960084184231,22.2430930869391,-65.3557834784944));
#10909=CARTESIAN_POINT('Ctrl Pts',(-26.4884945158184,22.226232094565,-65.3546455282839));
#10910=CARTESIAN_POINT('Ctrl Pts',(-26.4829802192011,22.214062284201,-65.353819279461));
#10911=CARTESIAN_POINT('Ctrl Pts',(-26.4027771521693,22.0399459596659,-65.3419264287031));
#10912=CARTESIAN_POINT('Ctrl Pts',(-26.3148609170175,21.8844663146546,-65.3303891464609));
#10913=CARTESIAN_POINT('Ctrl Pts',(-26.0378542119916,21.4774298548182,-65.2976085076084));
#10914=CARTESIAN_POINT('Ctrl Pts',(-25.8241605116071,21.2450201493666,-65.2757082140626));
#10915=CARTESIAN_POINT('Ctrl Pts',(-25.5676911866201,21.0370236232647,-65.2548115534631));
#10916=CARTESIAN_POINT('Ctrl Pts',(-25.5550738725924,21.026947221276,-65.253795875369));
#10917=CARTESIAN_POINT('Ctrl Pts',(-25.5395659747303,21.0147521051388,-65.2525630765468));
#10918=CARTESIAN_POINT('Ctrl Pts',(-25.5367471952011,21.0125430645028,-65.2523396209909));
#10919=CARTESIAN_POINT('Ctrl Pts',(-25.5320933607234,21.0089084206918,-65.2519717278193));
#10920=CARTESIAN_POINT('Ctrl Pts',(-25.5302604459347,21.0074801034676,-65.251827096672));
#10921=CARTESIAN_POINT('Ctrl Pts',(-25.5269521579819,21.004907832985,-65.2515665249041));
#10922=CARTESIAN_POINT('Ctrl Pts',(-25.5254773392298,21.0037631821056,-65.2514505342646));
#10923=CARTESIAN_POINT('Ctrl Pts',(-25.5223030463105,21.001303935389,-65.2512012523059));
#10924=CARTESIAN_POINT('Ctrl Pts',(-25.5206032566311,20.9999897609958,-65.2510679913537));
#10925=CARTESIAN_POINT('Ctrl Pts',(-25.5159425222562,20.9963938047554,-65.2507032117953));
#10926=CARTESIAN_POINT('Ctrl Pts',(-25.5129789079462,20.9941154640748,-65.2504719388862));
#10927=CARTESIAN_POINT('Ctrl Pts',(-25.4975408665927,20.9822898246688,-65.2492706816478));
#10928=CARTESIAN_POINT('Ctrl Pts',(-25.4850004400856,20.9728284535584,-65.2483067167228));
#10929=CARTESIAN_POINT('Ctrl Pts',(-25.3610303505454,20.8807114473335,-65.2388874391317));
#10930=CARTESIAN_POINT('Ctrl Pts',(-25.2444269185878,20.8052298981961,-65.2308942656801));
#10931=CARTESIAN_POINT('Ctrl Pts',(-24.8223759056835,20.5691952039373,-65.2035513064225));
#10932=CARTESIAN_POINT('Ctrl Pts',(-24.4964249388996,20.4502922040981,-65.1848663588641));
#10933=CARTESIAN_POINT('Ctrl Pts',(-24.1374760858233,20.3813859882865,-65.1627668381719));
#10934=CARTESIAN_POINT('Ctrl Pts',(-24.1170957673541,20.3776770184089,-65.161508237918));
#10935=CARTESIAN_POINT('Ctrl Pts',(-24.0904797131951,20.373097868301,-65.1598591047469));
#10936=CARTESIAN_POINT('Ctrl Pts',(-24.0842748779539,20.3720490618765,-65.1594742684868));
#10937=CARTESIAN_POINT('Ctrl Pts',(-24.0747229152818,20.3704632508328,-65.1588812328935));
#10938=CARTESIAN_POINT('Ctrl Pts',(-24.071377921615,20.369913338812,-65.1586734444511));
#10939=CARTESIAN_POINT('Ctrl Pts',(-24.064798858475,20.3688424086849,-65.1582645318546));
#10940=CARTESIAN_POINT('Ctrl Pts',(-24.0615648493096,20.3683210417163,-65.1580634190625));
#10941=CARTESIAN_POINT('Ctrl Pts',(-24.0546797221818,20.3672218317804,-65.1576350238742));
#10942=CARTESIAN_POINT('Ctrl Pts',(-24.0510283958283,20.3666453384586,-65.157407698852));
#10943=CARTESIAN_POINT('Ctrl Pts',(-24.0406154254572,20.3650196335093,-65.1567590079164));
#10944=CARTESIAN_POINT('Ctrl Pts',(-24.0338514512466,20.3639856773472,-65.1563371580788));
#10945=CARTESIAN_POINT('Ctrl Pts',(-24.0188104367931,20.3617354718901,-65.1553980095788));
#10946=CARTESIAN_POINT('Ctrl Pts',(-24.0105318716633,20.3605298982718,-65.1548803746077));
#10947=CARTESIAN_POINT('Ctrl Pts',(-23.8049418323461,20.3314076938647,-65.1420069706271));
#10948=CARTESIAN_POINT('Ctrl Pts',(-23.6055067651159,20.3218242900325,-65.1290556153913));
#10949=CARTESIAN_POINT('Ctrl Pts',(-23.1116825070307,20.3438742037201,-65.0959819656097));
#10950=CARTESIAN_POINT('Ctrl Pts',(-22.8200766453763,20.39746684796,-65.0754908449453));
#10951=CARTESIAN_POINT('Ctrl Pts',(-22.5250321516334,20.494882873062,-65.0558376635838));
#10952=CARTESIAN_POINT('Ctrl Pts',(-22.5102644817434,20.4998778894677,-65.0548573490044));
#10953=CARTESIAN_POINT('Ctrl Pts',(-22.4921922814233,20.5061371313517,-65.0536623249617));
#10954=CARTESIAN_POINT('Ctrl Pts',(-22.4888531623401,20.50729978102,-65.0534417213696));
#10955=CARTESIAN_POINT('Ctrl Pts',(-22.4833361055669,20.5092309539891,-65.0530775608557));
#10956=CARTESIAN_POINT('Ctrl Pts',(-22.4811570803788,20.5099963233369,-65.0529338170877));
#10957=CARTESIAN_POINT('Ctrl Pts',(-22.4773949769507,20.5113222840426,-65.0526857926726));
#10958=CARTESIAN_POINT('Ctrl Pts',(-22.4758115169745,20.5118817694605,-65.05258144593));
#10959=CARTESIAN_POINT('Ctrl Pts',(-22.4722549455138,20.5131415442243,-65.0523471793031));
#10960=CARTESIAN_POINT('Ctrl Pts',(-22.4702820821845,20.5138425175052,-65.0522173011713));
#10961=CARTESIAN_POINT('Ctrl Pts',(-22.4650203324588,20.5157178339126,-65.0518710960493));
#10962=CARTESIAN_POINT('Ctrl Pts',(-22.4617326576667,20.5168956053798,-65.0516549743802));
#10963=CARTESIAN_POINT('Ctrl Pts',(-22.4463414882515,20.5224375586926,-65.0506440963381));
#10964=CARTESIAN_POINT('Ctrl Pts',(-22.4342620622151,20.5268689325222,-65.0498533118508));
#10965=CARTESIAN_POINT('Ctrl Pts',(-22.1461507940612,20.6345254099814,-65.0310464958532));
#10966=CARTESIAN_POINT('Ctrl Pts',(-21.8854918079104,20.775075804062,-65.0151415840458));
#10967=CARTESIAN_POINT('Ctrl Pts',(-21.4842623796865,21.0685740144185,-64.987165346172));
#10968=CARTESIAN_POINT('Ctrl Pts',(-21.3326171932744,21.203101399134,-64.9755360819718));
#10969=CARTESIAN_POINT('Ctrl Pts',(-21.1859237217119,21.3602232742047,-64.962474847009));
#10970=CARTESIAN_POINT('Ctrl Pts',(-21.1773113889522,21.3695578725966,-64.96170080284));
#10971=CARTESIAN_POINT('Ctrl Pts',(-21.1656315793049,21.3823683185759,-64.9606410422588));
#10972=CARTESIAN_POINT('Ctrl Pts',(-21.162516011038,21.3858003248711,-64.9603573686448));
#10973=CARTESIAN_POINT('Ctrl Pts',(-21.157229568178,21.3916489989557,-64.9598743521947));
#10974=CARTESIAN_POINT('Ctrl Pts',(-21.1550549168633,21.3940622568669,-64.9596751692562));
#10975=CARTESIAN_POINT('Ctrl Pts',(-21.150678575865,21.3989335682461,-64.959273340364));
#10976=CARTESIAN_POINT('Ctrl Pts',(-21.1484770059282,21.4013917228725,-64.9590706897684));
#10977=CARTESIAN_POINT('Ctrl Pts',(-21.1434794160074,21.4069890378138,-64.9586095157574));
#10978=CARTESIAN_POINT('Ctrl Pts',(-21.1406857592119,21.4101302914296,-64.958350893556));
#10979=CARTESIAN_POINT('Ctrl Pts',(-21.1348577956934,21.4167092682944,-64.9578096365377));
#10980=CARTESIAN_POINT('Ctrl Pts',(-21.1318246655402,21.4201480170378,-64.957526953227));
#10981=CARTESIAN_POINT('Ctrl Pts',(-21.1238931695244,21.4291789651012,-64.9567851428361));
#10982=CARTESIAN_POINT('Ctrl Pts',(-21.1190068176912,21.4347816370838,-64.9563255159311));
#10983=CARTESIAN_POINT('Ctrl Pts',(-21.104556311858,21.4514667265362,-64.9549584088274));
#10984=CARTESIAN_POINT('Ctrl Pts',(-21.0950483326351,21.4625973434099,-64.9540486105264));
#10985=CARTESIAN_POINT('Ctrl Pts',(-20.9928681589549,21.5838791806839,-64.9441581113895));
#10986=CARTESIAN_POINT('Ctrl Pts',(-20.9076128407668,21.7000406025292,-64.9348768766767));
#10987=CARTESIAN_POINT('Ctrl Pts',(-20.6865613096335,22.0478192387665,-64.9076259889112));
#10988=CARTESIAN_POINT('Ctrl Pts',(-20.5715335169468,22.2911860129293,-64.8890965198917));
#10989=CARTESIAN_POINT('Ctrl Pts',(-20.4842355155918,22.5573772704944,-64.8706368809147));
#10990=CARTESIAN_POINT('Ctrl Pts',(-20.4805589068136,22.568803254552,-64.869848058172));
#10991=CARTESIAN_POINT('Ctrl Pts',(-20.4718861830261,22.596281458557,-64.8679599148547));
#10992=CARTESIAN_POINT('Ctrl Pts',(-20.4669516178185,22.6123529205461,-64.8668628251323));
#10993=CARTESIAN_POINT('Ctrl Pts',(-20.4468774448962,22.6796038641365,-64.8623042449955));
#10994=CARTESIAN_POINT('Ctrl Pts',(-20.4328835542232,22.7311203531664,-64.8588896541004));
#10995=CARTESIAN_POINT('Ctrl Pts',(-20.4188205057784,22.7884891902786,-64.8551900844616));
#10996=CARTESIAN_POINT('Ctrl Pts',(-20.417480783404,22.7940177166079,-64.8548346145241));
#10997=CARTESIAN_POINT('Ctrl Pts',(-20.4156129516195,22.801815697793,-64.8543347328912));
#10998=CARTESIAN_POINT('Ctrl Pts',(-20.41507266458,22.8040821810121,-64.8541896217017));
#10999=CARTESIAN_POINT('Ctrl Pts',(-20.4141327293404,22.8080442170253,-64.8539362689303));
#11000=CARTESIAN_POINT('Ctrl Pts',(-20.4137319980008,22.8097395076144,-64.853827964419));
#11001=CARTESIAN_POINT('Ctrl Pts',(-20.4128911562052,22.8133096094255,-64.8536001004833));
#11002=CARTESIAN_POINT('Ctrl Pts',(-20.4124513515922,22.8151844904408,-64.8534805592613));
#11003=CARTESIAN_POINT('Ctrl Pts',(-20.4113946973694,22.8197072216796,-64.8531924898637));
#11004=CARTESIAN_POINT('Ctrl Pts',(-20.4107795155661,22.8223554680786,-64.853024058738));
#11005=CARTESIAN_POINT('Ctrl Pts',(-20.4086634809459,22.831517200304,-64.8524422019772));
#11006=CARTESIAN_POINT('Ctrl Pts',(-20.4071795281557,22.8380346319696,-64.8520297484857));
#11007=CARTESIAN_POINT('Ctrl Pts',(-20.397336533033,22.8818944054731,-64.8492636541942));
#11008=CARTESIAN_POINT('Ctrl Pts',(-20.3896224462525,22.9193803930908,-64.8469460734877));
#11009=CARTESIAN_POINT('Ctrl Pts',(-20.3668264358056,23.0410991670066,-64.8395447335085));
#11010=CARTESIAN_POINT('Ctrl Pts',(-20.3544297506129,23.1258023622658,-64.8345846477775));
#11011=CARTESIAN_POINT('Ctrl Pts',(-20.3069259080677,23.5744334521769,-64.8088491730745));
#11012=CARTESIAN_POINT('Ctrl Pts',(-20.3305580267071,23.9418344115491,-64.7892652971447));
#11013=CARTESIAN_POINT('Ctrl Pts',(-20.417050699122,24.304718952733,-64.7667666458128));
#11014=CARTESIAN_POINT('Ctrl Pts',(-20.4188069406612,24.3119754557785,-64.7663155791612));
#11015=CARTESIAN_POINT('Ctrl Pts',(-20.4251254987021,24.3376915201718,-64.7647128541929));
#11016=CARTESIAN_POINT('Ctrl Pts',(-20.4298258887457,24.3561164623674,-64.7635568390067));
#11017=CARTESIAN_POINT('Ctrl Pts',(-20.4362449131748,24.3803797054856,-64.7620239857019));
#11018=CARTESIAN_POINT('Ctrl Pts',(-20.4378174912044,24.3862565333552,-64.7616518931398));
#11019=CARTESIAN_POINT('Ctrl Pts',(-20.4402812148434,24.3953603225264,-64.7610742032586));
#11020=CARTESIAN_POINT('Ctrl Pts',(-20.4411607701951,24.3985904291168,-64.7608689831508));
#11021=CARTESIAN_POINT('Ctrl Pts',(-20.4429254534457,24.4050315002317,-64.7604592566783));
#11022=CARTESIAN_POINT('Ctrl Pts',(-20.4438105294087,24.4082424748608,-64.7602547522192));
#11023=CARTESIAN_POINT('Ctrl Pts',(-20.4457753252544,24.4153276802746,-64.7598029476627));
#11024=CARTESIAN_POINT('Ctrl Pts',(-20.4468573216618,24.4192012690255,-64.7595555736223));
#11025=CARTESIAN_POINT('Ctrl Pts',(-20.4499917991371,24.4303422890537,-64.7588430304223));
#11026=CARTESIAN_POINT('Ctrl Pts',(-20.4520625668063,24.4376045085088,-64.7583772650268));
#11027=CARTESIAN_POINT('Ctrl Pts',(-20.4567799190851,24.4539305242151,-64.7573272388287));
#11028=CARTESIAN_POINT('Ctrl Pts',(-20.4594408427573,24.4629900731631,-64.7567425116486));
#11029=CARTESIAN_POINT('Ctrl Pts',(-20.4679297547791,24.4914291314351,-64.7549004533933));
#11030=CARTESIAN_POINT('Ctrl Pts',(-20.4739004014279,24.5107652247049,-64.7536384597835));
#11031=CARTESIAN_POINT('Ctrl Pts',(-20.4971994900216,24.5837735138577,-64.7488365415595));
#11032=CARTESIAN_POINT('Ctrl Pts',(-20.5157528873839,24.6370412701138,-64.7452567628918));
#11033=CARTESIAN_POINT('Ctrl Pts',(-20.5925692038498,24.8402525517416,-64.7312979845225));
#11034=CARTESIAN_POINT('Ctrl Pts',(-20.6606224119458,24.9862249375739,-64.7206110241176));
#11035=CARTESIAN_POINT('Ctrl Pts',(-20.8640342690094,25.3489780177236,-64.6925706915598));
#11036=CARTESIAN_POINT('Ctrl Pts',(-21.0147722782517,25.5558800523545,-64.6750341957923));
#11037=CARTESIAN_POINT('Ctrl Pts',(-21.1906876975557,25.7453796934671,-64.6586885307075));
#11038=CARTESIAN_POINT('Ctrl Pts',(-21.1930387648057,25.7479041693053,-64.6584707341213));
#11039=CARTESIAN_POINT('Ctrl Pts',(-21.2036191260345,25.7592283980989,-64.6574935744861));
#11040=CARTESIAN_POINT('Ctrl Pts',(-21.2118938171755,25.7679858907968,-64.6567374252627));
#11041=CARTESIAN_POINT('Ctrl Pts',(-21.222679295567,25.7792731888629,-64.6557624772415));
#11042=CARTESIAN_POINT('Ctrl Pts',(-21.2251452963097,25.7818453717697,-64.6555402782733));
#11043=CARTESIAN_POINT('Ctrl Pts',(-21.2289320158149,25.7857820508649,-64.6552001761265));
#11044=CARTESIAN_POINT('Ctrl Pts',(-21.2302496727268,25.7871494678431,-64.6550820349613));
#11045=CARTESIAN_POINT('Ctrl Pts',(-21.2328507938901,25.7898440472917,-64.6548492207611));
#11046=CARTESIAN_POINT('Ctrl Pts',(-21.2341341832591,25.7911712645339,-64.6547345434827));
#11047=CARTESIAN_POINT('Ctrl Pts',(-21.2369959845428,25.7941257118783,-64.6544792560685));
#11048=CARTESIAN_POINT('Ctrl Pts',(-21.2385749694671,25.7957523758403,-64.6543386921994));
#11049=CARTESIAN_POINT('Ctrl Pts',(-21.2431414655628,25.800446840543,-64.6539330063323));
#11050=CARTESIAN_POINT('Ctrl Pts',(-21.2461333910172,25.8035103698279,-64.6536682302395));
#11051=CARTESIAN_POINT('Ctrl Pts',(-21.2663911048564,25.8241703592835,-64.651882324415));
#11052=CARTESIAN_POINT('Ctrl Pts',(-21.283852813003,25.8415747935159,-64.6503763881162));
#11053=CARTESIAN_POINT('Ctrl Pts',(-21.3384865036833,25.8947935886847,-64.6457603629969));
#11054=CARTESIAN_POINT('Ctrl Pts',(-21.3763220456454,25.9299181847254,-64.642697665052));
#11055=CARTESIAN_POINT('Ctrl Pts',(-21.5397509046883,26.074484470923,-64.6299394068529));
#11056=CARTESIAN_POINT('Ctrl Pts',(-21.6728939802513,26.1750187877095,-64.6206709613844));
#11057=CARTESIAN_POINT('Ctrl Pts',(-21.8981479585447,26.3191572699258,-64.6057278828375));
#11058=CARTESIAN_POINT('Ctrl Pts',(-21.9855177837693,26.3694475531502,-64.6000934786598));
#11059=CARTESIAN_POINT('Ctrl Pts',(-22.0750364910777,26.4155370194908,-64.5943742034087));
#11060=CARTESIAN_POINT('Origin',(-23.5502525316942,23.5502525316942,-77.3107734492734));
#11061=CARTESIAN_POINT('',(-22.0750360104957,26.415536772059,-63.0988976931332));
#11062=CARTESIAN_POINT('',(-22.0750360636209,26.415536799411,-63.3454515897691));
#11063=CARTESIAN_POINT('',(-22.0750360153461,26.4155367745563,-77.3107734492734));
#11064=CARTESIAN_POINT('',(-26.7730015586105,23.5477481335051,-63.9376071674064));
#11065=CARTESIAN_POINT('Ctrl Pts',(-22.0750360104957,26.415536772059,-63.0988976931332));
#11066=CARTESIAN_POINT('Ctrl Pts',(-22.0301551534622,26.3924294723194,-63.1018341048178));
#11067=CARTESIAN_POINT('Ctrl Pts',(-21.9858167660497,26.3682674425502,-63.1047303870157));
#11068=CARTESIAN_POINT('Ctrl Pts',(-21.645912760162,26.1725397346903,-63.1270342225087));
#11069=CARTESIAN_POINT('Ctrl Pts',(-21.3787938250415,25.9560113334665,-63.1454359720157));
#11070=CARTESIAN_POINT('Ctrl Pts',(-21.1475892577515,25.6981231034343,-63.166177027197));
#11071=CARTESIAN_POINT('Ctrl Pts',(-21.1445202841832,25.6946851265449,-63.1664532973355));
#11072=CARTESIAN_POINT('Ctrl Pts',(-21.1388395952117,25.6882938678697,-63.1669664628214));
#11073=CARTESIAN_POINT('Ctrl Pts',(-21.1362259013136,25.6853423501882,-63.1672032778995));
#11074=CARTESIAN_POINT('Ctrl Pts',(-21.120110041865,25.6670760700166,-63.1686678573895));
#11075=CARTESIAN_POINT('Ctrl Pts',(-21.1067484835751,25.6516383484345,-63.1699012468026));
#11076=CARTESIAN_POINT('Ctrl Pts',(-21.0844261845881,25.6253467582129,-63.1719950409862));
#11077=CARTESIAN_POINT('Ctrl Pts',(-21.0753881122835,25.6145591268285,-63.1728522528438));
#11078=CARTESIAN_POINT('Ctrl Pts',(-21.0629948840193,25.5995684835867,-63.1740409946307));
#11079=CARTESIAN_POINT('Ctrl Pts',(-21.0595790639225,25.5954156432777,-63.1743700526592));
#11080=CARTESIAN_POINT('Ctrl Pts',(-21.0541428008188,25.5887725971272,-63.1748960246155));
#11081=CARTESIAN_POINT('Ctrl Pts',(-21.0521156432332,25.5862878781786,-63.175092666101));
#11082=CARTESIAN_POINT('Ctrl Pts',(-21.0481707408952,25.5814377884834,-63.1754763317806));
#11083=CARTESIAN_POINT('Ctrl Pts',(-21.0462526327908,25.5790727162945,-63.1756633410165));
#11084=CARTESIAN_POINT('Ctrl Pts',(-21.0417132680198,25.5734593297433,-63.1761070124693));
#11085=CARTESIAN_POINT('Ctrl Pts',(-21.0390949693512,25.5702086405962,-63.1763637934765));
#11086=CARTESIAN_POINT('Ctrl Pts',(-21.0313260701538,25.5605248905896,-63.1771283089979));
#11087=CARTESIAN_POINT('Ctrl Pts',(-21.0261938506064,25.5540771866951,-63.1776367804371));
#11088=CARTESIAN_POINT('Ctrl Pts',(-21.0145642430654,25.5393511246037,-63.1787968466262));
#11089=CARTESIAN_POINT('Ctrl Pts',(-21.0080825853661,25.5310605156137,-63.1794490631095));
#11090=CARTESIAN_POINT('Ctrl Pts',(-20.9512170781906,25.4575856937487,-63.1852217288918));
#11091=CARTESIAN_POINT('Ctrl Pts',(-20.9033134590413,25.3905287658824,-63.1904391755171));
#11092=CARTESIAN_POINT('Ctrl Pts',(-20.794074657468,25.224510763073,-63.2032510446905));
#11093=CARTESIAN_POINT('Ctrl Pts',(-20.7354321874675,25.1239230542687,-63.2109310196733));
#11094=CARTESIAN_POINT('Ctrl Pts',(-20.5498436287947,24.7618843991332,-63.2381773223736));
#11095=CARTESIAN_POINT('Ctrl Pts',(-20.4528852974654,24.486645597089,-63.2583274810434));
#11096=CARTESIAN_POINT('Ctrl Pts',(-20.3908918254272,24.1865012295665,-63.2777193655171));
#11097=CARTESIAN_POINT('Ctrl Pts',(-20.3877784341178,24.170841030711,-63.2787235959971));
#11098=CARTESIAN_POINT('Ctrl Pts',(-20.384112053227,24.1516548537664,-63.2799441681011));
#11099=CARTESIAN_POINT('Ctrl Pts',(-20.3834484390684,24.1481506180055,-63.2801667002449));
#11100=CARTESIAN_POINT('Ctrl Pts',(-20.3823629216087,24.1423659995565,-63.2805333808749));
#11101=CARTESIAN_POINT('Ctrl Pts',(-20.3819376625254,24.1400862628306,-63.280677720726));
#11102=CARTESIAN_POINT('Ctrl Pts',(-20.3811745796632,24.1359708770974,-63.2809379738082));
#11103=CARTESIAN_POINT('Ctrl Pts',(-20.3808358906848,24.1341353983216,-63.2810539365173));
#11104=CARTESIAN_POINT('Ctrl Pts',(-20.3801101745535,24.130183241356,-63.2813033879504));
#11105=CARTESIAN_POINT('Ctrl Pts',(-20.3797236737425,24.1280664753704,-63.2814368458983));
#11106=CARTESIAN_POINT('Ctrl Pts',(-20.3786688956442,24.122256802769,-63.2818027332029));
#11107=CARTESIAN_POINT('Ctrl Pts',(-20.3780049457602,24.1185630986069,-63.2820349143377));
#11108=CARTESIAN_POINT('Ctrl Pts',(-20.3745618554222,24.0992143644919,-63.2832488612489));
#11109=CARTESIAN_POINT('Ctrl Pts',(-20.3718920807936,24.0835397281584,-63.2842244548524));
#11110=CARTESIAN_POINT('Ctrl Pts',(-20.3400262407354,23.8877053765299,-63.2963227657731));
#11111=CARTESIAN_POINT('Ctrl Pts',(-20.3260649266678,23.7053714613306,-63.306642365193));
#11112=CARTESIAN_POINT('Ctrl Pts',(-20.3296240298868,23.2873739331184,-63.330059540505));
#11113=CARTESIAN_POINT('Ctrl Pts',(-20.3574216320898,23.0528845765,-63.34306672695));
#11114=CARTESIAN_POINT('Ctrl Pts',(-20.4131995793952,22.8119040354237,-63.3575855399289));
#11115=CARTESIAN_POINT('Ctrl Pts',(-20.4159527103446,22.8003029652243,-63.3582871898052));
#11116=CARTESIAN_POINT('Ctrl Pts',(-20.4349444715038,22.7222075832218,-63.3630294085441));
#11117=CARTESIAN_POINT('Ctrl Pts',(-20.4532325950998,22.6562339640932,-63.3671286051469));
#11118=CARTESIAN_POINT('Ctrl Pts',(-20.4764095696033,22.5819056447239,-63.3718709218751));
#11119=CARTESIAN_POINT('Ctrl Pts',(-20.4792523221489,22.5729276322311,-63.3724458130778));
#11120=CARTESIAN_POINT('Ctrl Pts',(-20.4834732769373,22.5597972295947,-63.3732896793406));
#11121=CARTESIAN_POINT('Ctrl Pts',(-20.4848206672027,22.5556349234018,-63.3735576380188));
#11122=CARTESIAN_POINT('Ctrl Pts',(-20.4872253688208,22.5482577135852,-63.374033376593));
#11123=CARTESIAN_POINT('Ctrl Pts',(-20.4882792786965,22.5450417011689,-63.3742410438714));
#11124=CARTESIAN_POINT('Ctrl Pts',(-20.490318407154,22.5388522509025,-63.374641245611));
#11125=CARTESIAN_POINT('Ctrl Pts',(-20.4913028993855,22.5358785762917,-63.3748337558462));
#11126=CARTESIAN_POINT('Ctrl Pts',(-20.4939334536495,22.5279716002884,-63.3753462704954));
#11127=CARTESIAN_POINT('Ctrl Pts',(-20.4955871195197,22.523040855021,-63.375666526439));
#11128=CARTESIAN_POINT('Ctrl Pts',(-20.5017791887359,22.5047251071461,-63.3768586006951));
#11129=CARTESIAN_POINT('Ctrl Pts',(-20.5063936410173,22.4913661536413,-63.3777329386884));
#11130=CARTESIAN_POINT('Ctrl Pts',(-20.5179214612466,22.4586909222095,-63.3798836805679));
#11131=CARTESIAN_POINT('Ctrl Pts',(-20.5249316231792,22.4394096817924,-63.381163285861));
#11132=CARTESIAN_POINT('Ctrl Pts',(-20.5522694506815,22.3663964155993,-63.3860494806778));
#11133=CARTESIAN_POINT('Ctrl Pts',(-20.5738474612456,22.3131470245561,-63.3896974630876));
#11134=CARTESIAN_POINT('Ctrl Pts',(-20.6641086150541,22.106456293385,-63.4041984933293));
#11135=CARTESIAN_POINT('Ctrl Pts',(-20.7433222049716,21.9579261622564,-63.415390190971));
#11136=CARTESIAN_POINT('Ctrl Pts',(-20.9666127783519,21.6081132263309,-63.4434029360249));
#11137=CARTESIAN_POINT('Ctrl Pts',(-21.1229747383331,21.4159041668097,-63.460341833443));
#11138=CARTESIAN_POINT('Ctrl Pts',(-21.3100590745428,21.2333887920073,-63.4768563215546));
#11139=CARTESIAN_POINT('Ctrl Pts',(-21.3204186712893,21.2234166356407,-63.4777599426763));
#11140=CARTESIAN_POINT('Ctrl Pts',(-21.333575863148,21.2109200850646,-63.4788935715632));
#11141=CARTESIAN_POINT('Ctrl Pts',(-21.3363113955375,21.2083310140703,-63.4791285090593));
#11142=CARTESIAN_POINT('Ctrl Pts',(-21.3406354177513,21.2042528486557,-63.4794986698731));
#11143=CARTESIAN_POINT('Ctrl Pts',(-21.3422208774871,21.2027605685273,-63.4796341401154));
#11144=CARTESIAN_POINT('Ctrl Pts',(-21.3451668380155,21.1999933710111,-63.4798853855385));
#11145=CARTESIAN_POINT('Ctrl Pts',(-21.3465269245834,21.1987180353626,-63.4800011931034));
#11146=CARTESIAN_POINT('Ctrl Pts',(-21.3495572592048,21.1958814676431,-63.4802588021786));
#11147=CARTESIAN_POINT('Ctrl Pts',(-21.3512280582278,21.1943208360009,-63.4804005568849));
#11148=CARTESIAN_POINT('Ctrl Pts',(-21.356099897741,21.189779928584,-63.4808130856425));
#11149=CARTESIAN_POINT('Ctrl Pts',(-21.3593053622352,21.1868043743838,-63.4810834954298));
#11150=CARTESIAN_POINT('Ctrl Pts',(-21.3821099214642,21.1657217238201,-63.4830001448988));
#11151=CARTESIAN_POINT('Ctrl Pts',(-21.4019279220865,21.1478514337128,-63.4846285318492));
#11152=CARTESIAN_POINT('Ctrl Pts',(-21.4293547842209,21.1237309231788,-63.4868354429079));
#11153=CARTESIAN_POINT('Ctrl Pts',(-21.4367730196159,21.1172669729836,-63.4874277685858));
#11154=CARTESIAN_POINT('Ctrl Pts',(-21.518271278153,21.0469067107706,-63.4938867041588));
#11155=CARTESIAN_POINT('Ctrl Pts',(-21.5952013215871,20.9863753187256,-63.4995480745962));
#11156=CARTESIAN_POINT('Ctrl Pts',(-21.8691045028307,20.7903679702629,-63.5187110824417));
#11157=CARTESIAN_POINT('Ctrl Pts',(-22.0782987305988,20.6733480545255,-63.5317373458434));
#11158=CARTESIAN_POINT('Ctrl Pts',(-22.3508088361478,20.5584849682122,-63.5486955513083));
#11159=CARTESIAN_POINT('Ctrl Pts',(-22.4036759750995,20.5378282490587,-63.551981546353));
#11160=CARTESIAN_POINT('Ctrl Pts',(-22.4743062501571,20.5123596262334,-63.5563836432989));
#11161=CARTESIAN_POINT('Ctrl Pts',(-22.4916059411943,20.5062878335387,-63.5574627779333));
#11162=CARTESIAN_POINT('Ctrl Pts',(-22.51313020436,20.4989389959765,-63.5588070250674));
#11163=CARTESIAN_POINT('Ctrl Pts',(-22.5173070516366,20.4975224994001,-63.5590679539582));
#11164=CARTESIAN_POINT('Ctrl Pts',(-22.525281552246,20.494836342695,-63.5595662731713));
#11165=CARTESIAN_POINT('Ctrl Pts',(-22.5290786922107,20.4935651767198,-63.559803617626));
#11166=CARTESIAN_POINT('Ctrl Pts',(-22.537986211887,20.4906016626653,-63.5603605518315));
#11167=CARTESIAN_POINT('Ctrl Pts',(-22.543098472267,20.4889150392498,-63.560680314175));
#11168=CARTESIAN_POINT('Ctrl Pts',(-22.5547584423909,20.4851005809968,-63.5614099229132));
#11169=CARTESIAN_POINT('Ctrl Pts',(-22.5613087780052,20.4829809079735,-63.5618200170746));
#11170=CARTESIAN_POINT('Ctrl Pts',(-22.5709033461129,20.4799100578105,-63.5624210387485));
#11171=CARTESIAN_POINT('Ctrl Pts',(-22.5739423065505,20.4789423750337,-63.5626114544927));
#11172=CARTESIAN_POINT('Ctrl Pts',(-22.5781209528972,20.4776186157072,-63.5628733512343));
#11173=CARTESIAN_POINT('Ctrl Pts',(-22.5792594144885,20.4772586569035,-63.5629447115072));
#11174=CARTESIAN_POINT('Ctrl Pts',(-22.5869333763851,20.474836993768,-63.5634257744358));
#11175=CARTESIAN_POINT('Ctrl Pts',(-22.5934752019205,20.4727955188241,-63.5638361053001));
#11176=CARTESIAN_POINT('Ctrl Pts',(-22.6058354316685,20.4689815440914,-63.5646118708173));
#11177=CARTESIAN_POINT('Ctrl Pts',(-22.6116524466462,20.4672046181105,-63.5649771643711));
#11178=CARTESIAN_POINT('Ctrl Pts',(-22.6422131915426,20.4579637219404,-63.5668974040785));
#11179=CARTESIAN_POINT('Ctrl Pts',(-22.6670404706536,20.4507812990952,-63.5684611938968));
#11180=CARTESIAN_POINT('Ctrl Pts',(-22.7005903620495,20.4415112914972,-63.570580454431));
#11181=CARTESIAN_POINT('Ctrl Pts',(-22.7092396672428,20.4391602379326,-63.5711273471674));
#11182=CARTESIAN_POINT('Ctrl Pts',(-22.7221781777228,20.4357011915164,-63.5719462868049));
#11183=CARTESIAN_POINT('Ctrl Pts',(-22.7264600932906,20.4345658971915,-63.5722174469699));
#11184=CARTESIAN_POINT('Ctrl Pts',(-22.7338322466006,20.4326275261675,-63.5726845435035));
#11185=CARTESIAN_POINT('Ctrl Pts',(-22.7369213705381,20.4318202045176,-63.5728803419315));
#11186=CARTESIAN_POINT('Ctrl Pts',(-22.7432931448948,20.4301650962022,-63.5732843573954));
#11187=CARTESIAN_POINT('Ctrl Pts',(-22.7465759419849,20.4293178966731,-63.5734925931475));
#11188=CARTESIAN_POINT('Ctrl Pts',(-22.7530747789813,20.4276516595302,-63.5739049971667));
#11189=CARTESIAN_POINT('Ctrl Pts',(-22.7562907594769,20.4268324061931,-63.5741091581341));
#11190=CARTESIAN_POINT('Ctrl Pts',(-22.7668823262403,20.4241516778889,-63.5747818152304));
#11191=CARTESIAN_POINT('Ctrl Pts',(-22.7742631962656,20.4223113595066,-63.5752509954441));
#11192=CARTESIAN_POINT('Ctrl Pts',(-22.82362788675,20.4101884299898,-63.5783919213651));
#11193=CARTESIAN_POINT('Ctrl Pts',(-22.8658067062213,20.4007256535867,-63.5810900011819));
#11194=CARTESIAN_POINT('Ctrl Pts',(-22.9873382356944,20.3760166943649,-63.588909847546));
#11195=CARTESIAN_POINT('Ctrl Pts',(-23.0670861971151,20.3629034583346,-63.5940974776461));
#11196=CARTESIAN_POINT('Ctrl Pts',(-23.2491804851409,20.339951813884,-63.606070421336));
#11197=CARTESIAN_POINT('Ctrl Pts',(-23.3516723458384,20.3319862064312,-63.6129009116404));
#11198=CARTESIAN_POINT('Ctrl Pts',(-23.7098477013597,20.3213243303132,-63.6369805722327));
#11199=CARTESIAN_POINT('Ctrl Pts',(-23.9653350569952,20.3441388637953,-63.6546005567174));
#11200=CARTESIAN_POINT('Ctrl Pts',(-24.2235464293843,20.3986082982474,-63.6715136187067));
#11201=CARTESIAN_POINT('Ctrl Pts',(-24.2316372395491,20.4003476236201,-63.6720425604478));
#11202=CARTESIAN_POINT('Ctrl Pts',(-24.2640491440968,20.4074461126367,-63.6741572025787));
#11203=CARTESIAN_POINT('Ctrl Pts',(-24.2883152796707,20.4130561297622,-63.6757306606294));
#11204=CARTESIAN_POINT('Ctrl Pts',(-24.3165523130673,20.4199299485038,-63.6775482663191));
#11205=CARTESIAN_POINT('Ctrl Pts',(-24.3205879172099,20.4209206183223,-63.6778077173996));
#11206=CARTESIAN_POINT('Ctrl Pts',(-24.3270208478082,20.422512987778,-63.6782207722871));
#11207=CARTESIAN_POINT('Ctrl Pts',(-24.3294194004502,20.4231096404551,-63.6783746662615));
#11208=CARTESIAN_POINT('Ctrl Pts',(-24.3336504637385,20.4241673100229,-63.6786459290528));
#11209=CARTESIAN_POINT('Ctrl Pts',(-24.3354832568803,20.4246271796436,-63.6787633647369));
#11210=CARTESIAN_POINT('Ctrl Pts',(-24.3392954315849,20.4255872643828,-63.6790074845737));
#11211=CARTESIAN_POINT('Ctrl Pts',(-24.3412747386611,20.4260877475077,-63.6791341526239));
#11212=CARTESIAN_POINT('Ctrl Pts',(-24.3464133462509,20.42739228066,-63.6794627975166));
#11213=CARTESIAN_POINT('Ctrl Pts',(-24.3495719147223,20.4281992467126,-63.6796646044222));
#11214=CARTESIAN_POINT('Ctrl Pts',(-24.3630343989446,20.4316604753123,-63.6805239051905));
#11215=CARTESIAN_POINT('Ctrl Pts',(-24.373326514114,20.4343610052092,-63.6811787371725));
#11216=CARTESIAN_POINT('Ctrl Pts',(-24.5381911313162,20.478493415982,-63.6916371404394));
#11217=CARTESIAN_POINT('Ctrl Pts',(-24.6895045606705,20.5313376831255,-63.7008021472877));
#11218=CARTESIAN_POINT('Ctrl Pts',(-24.9169516437348,20.6303225793272,-63.7147716447462));
#11219=CARTESIAN_POINT('Ctrl Pts',(-24.9961494052048,20.668718212602,-63.719673817853));
#11220=CARTESIAN_POINT('Ctrl Pts',(-25.1652820033998,20.7594455967726,-63.7304045938781));
#11221=CARTESIAN_POINT('Ctrl Pts',(-25.254452193926,20.8129864247453,-63.7362342701892));
#11222=CARTESIAN_POINT('Ctrl Pts',(-25.3932382584673,20.9057322787311,-63.7457659596978));
#11223=CARTESIAN_POINT('Ctrl Pts',(-25.4445610543022,20.9422497783605,-63.7493982772262));
#11224=CARTESIAN_POINT('Ctrl Pts',(-25.5131049775109,20.9941117043254,-63.7544241880185));
#11225=CARTESIAN_POINT('Ctrl Pts',(-25.5312815800207,21.0081727676195,-63.7557743522765));
#11226=CARTESIAN_POINT('Ctrl Pts',(-25.553206854687,21.0255116982045,-63.7574251861631));
#11227=CARTESIAN_POINT('Ctrl Pts',(-25.5571006024925,21.0286056260707,-63.7577192230305));
#11228=CARTESIAN_POINT('Ctrl Pts',(-25.5640949401086,21.0341897083405,-63.758248968692));
#11229=CARTESIAN_POINT('Ctrl Pts',(-25.5671981170502,21.0366766162889,-63.7584845587877));
#11230=CARTESIAN_POINT('Ctrl Pts',(-25.5805503230972,21.047417815452,-63.7595006675458));
#11231=CARTESIAN_POINT('Ctrl Pts',(-25.5907532432506,21.0557290145861,-63.7602832805404));
#11232=CARTESIAN_POINT('Ctrl Pts',(-25.6023887222068,21.0653263118808,-63.7611830175948));
#11233=CARTESIAN_POINT('Ctrl Pts',(-25.6038714788543,21.0665515669705,-63.7612978103889));
#11234=CARTESIAN_POINT('Ctrl Pts',(-25.6099606158738,21.0715924202583,-63.761769781487));
#11235=CARTESIAN_POINT('Ctrl Pts',(-25.6145574455267,21.0754194944818,-63.7621274002556));
#11236=CARTESIAN_POINT('Ctrl Pts',(-25.6220054196052,21.081655467448,-63.76270898971));
#11237=CARTESIAN_POINT('Ctrl Pts',(-25.6248630937489,21.0840565723653,-63.7629326560072));
#11238=CARTESIAN_POINT('Ctrl Pts',(-25.6341478867354,21.0918854962583,-63.7636610643951));
#11239=CARTESIAN_POINT('Ctrl Pts',(-25.6405578880618,21.0973334855759,-63.7641665985672));
#11240=CARTESIAN_POINT('Ctrl Pts',(-25.668258817615,21.1210644969308,-63.7663629553014));
#11241=CARTESIAN_POINT('Ctrl Pts',(-25.6893312579413,21.1395996613051,-63.7680638507021));
#11242=CARTESIAN_POINT('Ctrl Pts',(-25.7148729846291,21.162664583735,-63.7701639051844));
#11243=CARTESIAN_POINT('Ctrl Pts',(-25.7195748967614,21.1669358531951,-63.7705521220615));
#11244=CARTESIAN_POINT('Ctrl Pts',(-25.7273283587484,21.1740211380327,-63.771194998021));
#11245=CARTESIAN_POINT('Ctrl Pts',(-25.7303871696702,21.17682721098,-63.7714493190161));
#11246=CARTESIAN_POINT('Ctrl Pts',(-25.7359039553514,21.1819078287484,-63.7719092775714));
#11247=CARTESIAN_POINT('Ctrl Pts',(-25.7383638261394,21.184180313715,-63.7721148269393));
#11248=CARTESIAN_POINT('Ctrl Pts',(-25.7431293325022,21.1885965849534,-63.7725139320604));
#11249=CARTESIAN_POINT('Ctrl Pts',(-25.7454353784346,21.1907399244886,-63.7727074685279));
#11250=CARTESIAN_POINT('Ctrl Pts',(-25.7504736057915,21.1954364515697,-63.7731312011814));
#11251=CARTESIAN_POINT('Ctrl Pts',(-25.7532044888232,21.1979910197642,-63.773361456652));
#11252=CARTESIAN_POINT('Ctrl Pts',(-25.7643598815582,21.2084626482572,-63.7743044054872));
#11253=CARTESIAN_POINT('Ctrl Pts',(-25.7727461268446,21.2164201836428,-63.775018845801));
#11254=CARTESIAN_POINT('Ctrl Pts',(-25.8616075729008,21.3016522877886,-63.7826491241886));
#11255=CARTESIAN_POINT('Ctrl Pts',(-25.9380520132177,21.3830022284673,-63.7897446784749));
#11256=CARTESIAN_POINT('Ctrl Pts',(-26.0539064112616,21.5198761086836,-63.8014145119917));
#11257=CARTESIAN_POINT('Ctrl Pts',(-26.0960491169722,21.57297409619,-63.8058817119423));
#11258=CARTESIAN_POINT('Ctrl Pts',(-26.324513739653,21.8802518529808,-63.8313665341198));
#11259=CARTESIAN_POINT('Ctrl Pts',(-26.4744259188162,22.1593411357999,-63.8533463801359));
#11260=CARTESIAN_POINT('Ctrl Pts',(-26.5869938083489,22.4710924935984,-63.8743247543954));
#11261=CARTESIAN_POINT('Ctrl Pts',(-26.5924205168948,22.4864866054808,-63.8753515643297));
#11262=CARTESIAN_POINT('Ctrl Pts',(-26.5988996404045,22.5053212927182,-63.876596225667));
#11263=CARTESIAN_POINT('Ctrl Pts',(-26.6000634285163,22.5087228962198,-63.8768205538468));
#11264=CARTESIAN_POINT('Ctrl Pts',(-26.6019714253797,22.5143303454824,-63.8771895842546));
#11265=CARTESIAN_POINT('Ctrl Pts',(-26.6027189362507,22.5165350504218,-63.8773344820882));
#11266=CARTESIAN_POINT('Ctrl Pts',(-26.6040616743462,22.5205094720401,-63.8775953348541));
#11267=CARTESIAN_POINT('Ctrl Pts',(-26.6046577511417,22.5222788918951,-63.8777113403204));
#11268=CARTESIAN_POINT('Ctrl Pts',(-26.6059353968032,22.5260824323006,-63.877960432883));
#11269=CARTESIAN_POINT('Ctrl Pts',(-26.6066164705472,22.5281167100166,-63.8780934900129));
#11270=CARTESIAN_POINT('Ctrl Pts',(-26.608474146703,22.5336838025361,-63.8784571670253));
#11271=CARTESIAN_POINT('Ctrl Pts',(-26.6096466630747,22.537217992887,-63.878687543676));
#11272=CARTESIAN_POINT('Ctrl Pts',(-26.6156764187877,22.5554987886701,-63.8798766420982));
#11273=CARTESIAN_POINT('Ctrl Pts',(-26.6204332807995,22.5702786506548,-63.8808294886697));
#11274=CARTESIAN_POINT('Ctrl Pts',(-26.6469165927349,22.6546498556362,-63.886223442358));
#11275=CARTESIAN_POINT('Ctrl Pts',(-26.6663853187895,22.7249339655637,-63.8905415926922));
#11276=CARTESIAN_POINT('Ctrl Pts',(-26.7427465550266,23.0420681797853,-63.9094968911549));
#11277=CARTESIAN_POINT('Ctrl Pts',(-26.772804718694,23.2944474994768,-63.9232316158934));
#11278=CARTESIAN_POINT('Ctrl Pts',(-26.7730015586105,23.5477481335051,-63.9376071674064));
#11279=CARTESIAN_POINT('Ctrl Pts',(-26.7730015615053,23.5477518614343,-63.9376073789773));
#11280=CARTESIAN_POINT('Ctrl Pts',(-26.7731347904089,23.7194511561076,-63.9473518193325));
#11281=CARTESIAN_POINT('Ctrl Pts',(-26.7595469903421,23.8908673797861,-63.9573375528294));
#11282=CARTESIAN_POINT('Ctrl Pts',(-26.7312784852756,24.0672044259549,-63.9682105578638));
#11283=CARTESIAN_POINT('Ctrl Pts',(-26.7301619710957,24.0740285662475,-63.9686322487113));
#11284=CARTESIAN_POINT('Ctrl Pts',(-26.7283045162005,24.0851564644852,-63.9693213939651));
#11285=CARTESIAN_POINT('Ctrl Pts',(-26.7275767709856,24.0894624274258,-63.9695884289721));
#11286=CARTESIAN_POINT('Ctrl Pts',(-26.7262793924432,24.097044999596,-63.9700593184265));
#11287=CARTESIAN_POINT('Ctrl Pts',(-26.72571343387,24.1003222379813,-63.9702630557172));
#11288=CARTESIAN_POINT('Ctrl Pts',(-26.7245596525089,24.1069421980216,-63.9706750396583));
#11289=CARTESIAN_POINT('Ctrl Pts',(-26.7239716201346,24.1102848784175,-63.9708832927453));
#11290=CARTESIAN_POINT('Ctrl Pts',(-26.7228213350131,24.1167636986026,-63.9712873719911));
#11291=CARTESIAN_POINT('Ctrl Pts',(-26.7222597094878,24.1198999471429,-63.9714831779299));
#11292=CARTESIAN_POINT('Ctrl Pts',(-26.720910637082,24.1273696255038,-63.9719500136222));
#11293=CARTESIAN_POINT('Ctrl Pts',(-26.7201189572045,24.1317022761708,-63.9722211782684));
#11294=CARTESIAN_POINT('Ctrl Pts',(-26.717270713963,24.1471112334778,-63.9731869478697));
#11295=CARTESIAN_POINT('Ctrl Pts',(-26.7151649750293,24.1581782652703,-63.9738831220685));
#11296=CARTESIAN_POINT('Ctrl Pts',(-26.6831920253362,24.3215473243091,-63.9841980127897));
#11297=CARTESIAN_POINT('Ctrl Pts',(-26.642424015365,24.4714843332734,-63.9941703802944));
#11298=CARTESIAN_POINT('Ctrl Pts',(-26.5844352657248,24.6366447535082,-64.0057368878791));
#11299=CARTESIAN_POINT('Ctrl Pts',(-26.5776748125846,24.6553440372302,-64.0070548570558));
#11300=CARTESIAN_POINT('Ctrl Pts',(-26.5022367382458,24.8581156530629,-64.0214362764283));
#11301=CARTESIAN_POINT('Ctrl Pts',(-26.4170379823137,25.0355977637447,-64.0348663633243));
#11302=CARTESIAN_POINT('Ctrl Pts',(-26.2463000278234,25.3211298096228,-64.0571914078849));
#11303=CARTESIAN_POINT('Ctrl Pts',(-26.1690266904687,25.4335237533714,-64.0661829110351));
#11304=CARTESIAN_POINT('Ctrl Pts',(-26.0812741598373,25.5452665118788,-64.0750823080167));
#11305=CARTESIAN_POINT('Ctrl Pts',(-26.0776763427416,25.5498225214328,-64.0754450754333));
#11306=CARTESIAN_POINT('Ctrl Pts',(-26.0724700428257,25.5563788929013,-64.0759669709197));
#11307=CARTESIAN_POINT('Ctrl Pts',(-26.0708714769055,25.5583870599916,-64.0761268033778));
#11308=CARTESIAN_POINT('Ctrl Pts',(-26.0680866670928,25.5618768583202,-64.0764045222856));
#11309=CARTESIAN_POINT('Ctrl Pts',(-26.0669015120199,25.56335935319,-64.0765224874309));
#11310=CARTESIAN_POINT('Ctrl Pts',(-26.0646046887291,25.5662272210027,-64.0767506648602));
#11311=CARTESIAN_POINT('Ctrl Pts',(-26.0634931876341,25.5676127183956,-64.0768608888079));
#11312=CARTESIAN_POINT('Ctrl Pts',(-26.0608372118056,25.5709178173695,-64.0771238033051));
#11313=CARTESIAN_POINT('Ctrl Pts',(-26.0592916773286,25.5728365716076,-64.0772764170272));
#11314=CARTESIAN_POINT('Ctrl Pts',(-26.0546126822582,25.578631846478,-64.0777373082798));
#11315=CARTESIAN_POINT('Ctrl Pts',(-26.0514724082362,25.5825028948026,-64.0780450964729));
#11316=CARTESIAN_POINT('Ctrl Pts',(-26.0193083197012,25.6219644174305,-64.0811821430463));
#11317=CARTESIAN_POINT('Ctrl Pts',(-25.9895340573297,25.6569401673688,-64.0839580083613));
#11318=CARTESIAN_POINT('Ctrl Pts',(-25.780569757103,25.8920370752181,-64.1026800415497));
#11319=CARTESIAN_POINT('Ctrl Pts',(-25.5776967119744,26.0697324670794,-64.1172252101184));
#11320=CARTESIAN_POINT('Ctrl Pts',(-25.271731464199,26.2765602915612,-64.1380555047595));
#11321=CARTESIAN_POINT('Ctrl Pts',(-25.1857745113537,26.3289769635747,-64.1437949684118));
#11322=CARTESIAN_POINT('Ctrl Pts',(-25.0500634284825,26.4032527889375,-64.1528154827761));
#11323=CARTESIAN_POINT('Ctrl Pts',(-25.0019717465166,26.4280214651708,-64.1560040533003));
#11324=CARTESIAN_POINT('Ctrl Pts',(-24.9129931351249,26.4710500833843,-64.1619059019375));
#11325=CARTESIAN_POINT('Ctrl Pts',(-24.8723050178916,26.4896907786571,-64.1646055401226));
#11326=CARTESIAN_POINT('Ctrl Pts',(-24.8241976041084,26.5105296258366,-64.1678029390358));
#11327=CARTESIAN_POINT('Ctrl Pts',(-24.8171409190449,26.5135564874198,-64.1682720865791));
#11328=CARTESIAN_POINT('Ctrl Pts',(-24.8070119844279,26.5178583519208,-64.1689456996727));
#11329=CARTESIAN_POINT('Ctrl Pts',(-24.8039484349128,26.5191538787247,-64.1691494654674));
#11330=CARTESIAN_POINT('Ctrl Pts',(-24.797754630989,26.521761844446,-64.1695614927389));
#11331=CARTESIAN_POINT('Ctrl Pts',(-24.7946242982573,26.5230740853622,-64.1697697606314));
#11332=CARTESIAN_POINT('Ctrl Pts',(-24.7885519642523,26.525608346812,-64.17017382755));
#11333=CARTESIAN_POINT('Ctrl Pts',(-24.7856102113238,26.5268309557386,-64.1703696062909));
#11334=CARTESIAN_POINT('Ctrl Pts',(-24.7785985651787,26.529732850239,-64.1708363120416));
#11335=CARTESIAN_POINT('Ctrl Pts',(-24.7745270414497,26.5314081584667,-64.1711073737709));
#11336=CARTESIAN_POINT('Ctrl Pts',(-24.760034381496,26.537336750307,-64.1720724270894));
#11337=CARTESIAN_POINT('Ctrl Pts',(-24.7495945031162,26.541543738448,-64.1727679848753));
#11338=CARTESIAN_POINT('Ctrl Pts',(-24.5954752786078,26.6027130874594,-64.183042285239));
#11339=CARTESIAN_POINT('Ctrl Pts',(-24.4479248691563,26.6493132853519,-64.192971663129));
#11340=CARTESIAN_POINT('Ctrl Pts',(-24.1397474168328,26.7227836351276,-64.2139015556458));
#11341=CARTESIAN_POINT('Ctrl Pts',(-23.9792671244738,26.7484390923787,-64.2249021758243));
#11342=CARTESIAN_POINT('Ctrl Pts',(-23.7969867016134,26.763609909018,-64.2372758869747));
#11343=CARTESIAN_POINT('Ctrl Pts',(-23.7764062803604,26.7651238937147,-64.2386709477898));
#11344=CARTESIAN_POINT('Ctrl Pts',(-23.7312827380956,26.7680079297472,-64.2417238752259));
#11345=CARTESIAN_POINT('Ctrl Pts',(-23.7067354599254,26.7692950683045,-64.2433809154697));
#11346=CARTESIAN_POINT('Ctrl Pts',(-23.595444845031,26.7738545659571,-64.2508710544743));
#11347=CARTESIAN_POINT('Ctrl Pts',(-23.5085998115634,26.7739025566554,-64.2566551702134));
#11348=CARTESIAN_POINT('Ctrl Pts',(-23.3808723154963,26.7688096680634,-64.2649832745104));
#11349=CARTESIAN_POINT('Ctrl Pts',(-23.3399237487836,26.7663933644623,-64.2676258843719));
#11350=CARTESIAN_POINT('Ctrl Pts',(-23.2785097319228,26.7615913623375,-64.2715373330146));
#11351=CARTESIAN_POINT('Ctrl Pts',(-23.2580042662203,26.7597902303192,-64.2728346027502));
#11352=CARTESIAN_POINT('Ctrl Pts',(-23.2334682470377,26.7573979643734,-64.2743752799697));
#11353=CARTESIAN_POINT('Ctrl Pts',(-23.2294203861404,26.7569955591559,-64.2746290770401));
#11354=CARTESIAN_POINT('Ctrl Pts',(-23.2231637280651,26.7563616080116,-64.2750207675545));
#11355=CARTESIAN_POINT('Ctrl Pts',(-23.2209544086028,26.7561354429847,-64.2751589643834));
#11356=CARTESIAN_POINT('Ctrl Pts',(-23.2170753494578,26.7557342967884,-64.2754014024003));
#11357=CARTESIAN_POINT('Ctrl Pts',(-23.2154055194739,26.7555602953197,-64.2755056988807));
#11358=CARTESIAN_POINT('Ctrl Pts',(-23.2115847019372,26.7551591359306,-64.2757441923877));
#11359=CARTESIAN_POINT('Ctrl Pts',(-23.2094338106437,26.7549311177989,-64.2758783397777));
#11360=CARTESIAN_POINT('Ctrl Pts',(-23.203599402602,26.7543066660653,-64.2762419268376));
#11361=CARTESIAN_POINT('Ctrl Pts',(-23.1999163229079,26.753906044331,-64.2764711290104));
#11362=CARTESIAN_POINT('Ctrl Pts',(-23.182558825884,26.751987716497,-64.2775498360929));
#11363=CARTESIAN_POINT('Ctrl Pts',(-23.1688932611161,26.7503887752986,-64.2783948027208));
#11364=CARTESIAN_POINT('Ctrl Pts',(-22.913597109621,26.7188592286028,-64.2941067873799));
#11365=CARTESIAN_POINT('Ctrl Pts',(-22.6760717109806,26.6617229661908,-64.3075303778215));
#11366=CARTESIAN_POINT('Ctrl Pts',(-22.3516685669515,26.5435542909854,-64.3268327551247));
#11367=CARTESIAN_POINT('Ctrl Pts',(-22.2578217065855,26.504246488997,-64.3325345382842));
#11368=CARTESIAN_POINT('Ctrl Pts',(-22.135434649349,26.4460344653975,-64.3402661806216));
#11369=CARTESIAN_POINT('Ctrl Pts',(-22.1051119255198,26.4310216188492,-64.3422066737569));
#11370=CARTESIAN_POINT('Ctrl Pts',(-22.0750359910842,26.4155367620648,-64.3441594845823));
#11371=CARTESIAN_POINT('',(-26.7730019592961,23.5521733105916,-64.1880685683874));
#11372=CARTESIAN_POINT('Ctrl Pts',(-22.0750364910777,26.4155370194908,-64.5943742034087));
#11373=CARTESIAN_POINT('Ctrl Pts',(-22.1780646657283,26.4685819497682,-64.5877918196014));
#11374=CARTESIAN_POINT('Ctrl Pts',(-22.2839391375605,26.5160625361067,-64.5810957300875));
#11375=CARTESIAN_POINT('Ctrl Pts',(-22.3983059545719,26.5600995864398,-64.5738161306072));
#11376=CARTESIAN_POINT('Ctrl Pts',(-22.4044073340023,26.5624276579996,-64.573427647464));
#11377=CARTESIAN_POINT('Ctrl Pts',(-22.4157079779317,26.5667002821916,-64.5727078670987));
#11378=CARTESIAN_POINT('Ctrl Pts',(-22.4209052800273,26.5686499807631,-64.5723767327745));
#11379=CARTESIAN_POINT('Ctrl Pts',(-22.427897220166,26.5712523270788,-64.571931113021));
#11380=CARTESIAN_POINT('Ctrl Pts',(-22.4296874592215,26.5719168292892,-64.5718170024157));
#11381=CARTESIAN_POINT('Ctrl Pts',(-22.4378856077802,26.5749515362713,-64.5712943893195));
#11382=CARTESIAN_POINT('Ctrl Pts',(-22.444300419849,26.5773029387656,-64.5708852931883));
#11383=CARTESIAN_POINT('Ctrl Pts',(-22.4567063676291,26.5818057427713,-64.5700937691596));
#11384=CARTESIAN_POINT('Ctrl Pts',(-22.4626965001124,26.5839598283584,-64.5697114292238));
#11385=CARTESIAN_POINT('Ctrl Pts',(-22.49506883275,26.5954929016213,-64.5676442442464));
#11386=CARTESIAN_POINT('Ctrl Pts',(-22.5215653955865,26.6045452892871,-64.5659489773829));
#11387=CARTESIAN_POINT('Ctrl Pts',(-22.5553300575076,26.615591581873,-64.563783405865));
#11388=CARTESIAN_POINT('Ctrl Pts',(-22.562492324645,26.617907009312,-64.5633237391642));
#11389=CARTESIAN_POINT('Ctrl Pts',(-22.573911822327,26.6215545812972,-64.5625903487252));
#11390=CARTESIAN_POINT('Ctrl Pts',(-22.5781638506545,26.6229030254114,-64.5623171622451));
#11391=CARTESIAN_POINT('Ctrl Pts',(-22.5856601236553,26.6252631979477,-64.5618353391164));
#11392=CARTESIAN_POINT('Ctrl Pts',(-22.5889032016043,26.6262786331138,-64.5616268247688));
#11393=CARTESIAN_POINT('Ctrl Pts',(-22.5951389192696,26.628220264406,-64.561225769946));
#11394=CARTESIAN_POINT('Ctrl Pts',(-22.5981313166868,26.6291472307829,-64.5610332550633));
#11395=CARTESIAN_POINT('Ctrl Pts',(-22.6059911447151,26.6315694454926,-64.5605274445954));
#11396=CARTESIAN_POINT('Ctrl Pts',(-22.6108607616456,26.6330575193781,-64.5602139138593));
#11397=CARTESIAN_POINT('Ctrl Pts',(-22.6285507061487,26.6384174657231,-64.5590743796717));
#11398=CARTESIAN_POINT('Ctrl Pts',(-22.6413914732721,26.6422209149028,-64.5582461376998));
#11399=CARTESIAN_POINT('Ctrl Pts',(-22.6726781065922,26.6512763171637,-64.5562253475893));
#11400=CARTESIAN_POINT('Ctrl Pts',(-22.6911476935113,26.6564438073532,-64.5550300698933));
#11401=CARTESIAN_POINT('Ctrl Pts',(-22.7603164597583,26.6751320087141,-64.5505444757247));
#11402=CARTESIAN_POINT('Ctrl Pts',(-22.8112950505543,26.6875781548456,-64.5472198126345));
#11403=CARTESIAN_POINT('Ctrl Pts',(-22.9788697514073,26.7241798252357,-64.5362256255348));
#11404=CARTESIAN_POINT('Ctrl Pts',(-23.09649368909,26.7431180920163,-64.528401711457));
#11405=CARTESIAN_POINT('Ctrl Pts',(-23.5145610656521,26.7868606978103,-64.5003235005832));
#11406=CARTESIAN_POINT('Ctrl Pts',(-23.8171464286231,26.7760360307752,-64.4793710460604));
#11407=CARTESIAN_POINT('Ctrl Pts',(-24.1297921637471,26.7205071603411,-64.4592750637541));
#11408=CARTESIAN_POINT('Ctrl Pts',(-24.145739316751,26.7175504511665,-64.458254831787));
#11409=CARTESIAN_POINT('Ctrl Pts',(-24.1651857145036,26.7137928917528,-64.4570171756147));
#11410=CARTESIAN_POINT('Ctrl Pts',(-24.1687064486964,26.7131064932127,-64.4567933587123));
#11411=CARTESIAN_POINT('Ctrl Pts',(-24.1745078341283,26.7119654041509,-64.4564249928107));
#11412=CARTESIAN_POINT('Ctrl Pts',(-24.1767891394709,26.7115141231577,-64.4562802494256));
#11413=CARTESIAN_POINT('Ctrl Pts',(-24.1809011110833,26.7106960793037,-64.4560195569655));
#11414=CARTESIAN_POINT('Ctrl Pts',(-24.182731942712,26.710330195773,-64.4559035576588));
#11415=CARTESIAN_POINT('Ctrl Pts',(-24.1866677232706,26.7095400901692,-64.4556543475747));
#11416=CARTESIAN_POINT('Ctrl Pts',(-24.1887725606375,26.7091153564948,-64.4555211670015));
#11417=CARTESIAN_POINT('Ctrl Pts',(-24.1945347602722,26.7079466115926,-64.4551568306267));
#11418=CARTESIAN_POINT('Ctrl Pts',(-24.1981912716282,26.7071983471801,-64.454925919522));
#11419=CARTESIAN_POINT('Ctrl Pts',(-24.217157503107,26.7032827789512,-64.4537296317806));
#11420=CARTESIAN_POINT('Ctrl Pts',(-24.2324456712568,26.7000103834488,-64.4527702153299));
#11421=CARTESIAN_POINT('Ctrl Pts',(-24.3810285697346,26.6670739901047,-64.4434880310266));
#11422=CARTESIAN_POINT('Ctrl Pts',(-24.5123526628997,26.6290734043046,-64.4356129942025));
#11423=CARTESIAN_POINT('Ctrl Pts',(-24.749909048627,26.5436395086538,-64.4213287727328));
#11424=CARTESIAN_POINT('Ctrl Pts',(-24.8567423901237,26.4985786292396,-64.4148886623379));
#11425=CARTESIAN_POINT('Ctrl Pts',(-25.0186296967779,26.4197657266678,-64.4048138697507));
#11426=CARTESIAN_POINT('Ctrl Pts',(-25.075487202531,26.3899525833706,-64.4012120710736));
#11427=CARTESIAN_POINT('Ctrl Pts',(-25.2185705374298,26.309389483884,-64.3919163838454));
#11428=CARTESIAN_POINT('Ctrl Pts',(-25.3033879943403,26.2562893892899,-64.3861810027071));
#11429=CARTESIAN_POINT('Ctrl Pts',(-25.398408001405,26.1904574282723,-64.379399861288));
#11430=CARTESIAN_POINT('Ctrl Pts',(-25.4111562014552,26.1814876136609,-64.3784824213674));
#11431=CARTESIAN_POINT('Ctrl Pts',(-25.4279939483844,26.1694567650092,-64.3772601518843));
#11432=CARTESIAN_POINT('Ctrl Pts',(-25.4321421373304,26.1664778957545,-64.3769581756646));
#11433=CARTESIAN_POINT('Ctrl Pts',(-25.4395092932312,26.1611608564406,-64.3764203310538));
#11434=CARTESIAN_POINT('Ctrl Pts',(-25.4427310502689,26.1588265574366,-64.3761845991356));
#11435=CARTESIAN_POINT('Ctrl Pts',(-25.4546079283243,26.150187674129,-64.3753136287829));
#11436=CARTESIAN_POINT('Ctrl Pts',(-25.4632358690446,26.1438459787512,-64.374677073599));
#11437=CARTESIAN_POINT('Ctrl Pts',(-25.4750117129926,26.1350997892198,-64.3738029028046));
#11438=CARTESIAN_POINT('Ctrl Pts',(-25.4781870879252,26.13273226974,-64.3735666430997));
#11439=CARTESIAN_POINT('Ctrl Pts',(-25.4867013526749,26.1263596860219,-64.3729316947079));
#11440=CARTESIAN_POINT('Ctrl Pts',(-25.4920321593862,26.12234389542,-64.3725326103673));
#11441=CARTESIAN_POINT('Ctrl Pts',(-25.5013500907741,26.1152790561357,-64.3718323026586));
#11442=CARTESIAN_POINT('Ctrl Pts',(-25.5053426505667,26.112237188713,-64.3715313498147));
#11443=CARTESIAN_POINT('Ctrl Pts',(-25.5188891430615,26.1018662266614,-64.3705072061383));
#11444=CARTESIAN_POINT('Ctrl Pts',(-25.5284090163246,26.0944929826612,-64.3697823425302));
#11445=CARTESIAN_POINT('Ctrl Pts',(-25.5562851608059,26.0726515743902,-64.367644379668));
#11446=CARTESIAN_POINT('Ctrl Pts',(-25.5745253250545,26.0580371024075,-64.3662256107699));
#11447=CARTESIAN_POINT('Ctrl Pts',(-25.5976444672417,26.0390968967569,-64.3644011194768));
#11448=CARTESIAN_POINT('Ctrl Pts',(-25.60267182314,26.0349527273649,-64.3640027688925));
#11449=CARTESIAN_POINT('Ctrl Pts',(-25.610653082668,26.0283328343849,-64.3633677816671));
#11450=CARTESIAN_POINT('Ctrl Pts',(-25.613615189994,26.0258669922203,-64.3631315485092));
#11451=CARTESIAN_POINT('Ctrl Pts',(-25.6191333424658,26.0212565555665,-64.3626904005233));
#11452=CARTESIAN_POINT('Ctrl Pts',(-25.6216904967599,26.0191132916244,-64.3624855403691));
#11453=CARTESIAN_POINT('Ctrl Pts',(-25.626699215275,26.0149020036599,-64.3620834348067));
#11454=CARTESIAN_POINT('Ctrl Pts',(-25.6291510303761,26.0128342829208,-64.361886202002));
#11455=CARTESIAN_POINT('Ctrl Pts',(-25.636545993412,26.0065788792235,-64.3612901171786));
#11456=CARTESIAN_POINT('Ctrl Pts',(-25.6414795823003,26.0023799663527,-64.3608908025617));
#11457=CARTESIAN_POINT('Ctrl Pts',(-25.6657977429401,25.9815563311956,-64.3589144085593));
#11458=CARTESIAN_POINT('Ctrl Pts',(-25.6849964604655,25.9647168624245,-64.3573284393562));
#11459=CARTESIAN_POINT('Ctrl Pts',(-25.7366662393825,25.9182985235305,-64.3529885504479));
#11460=CARTESIAN_POINT('Ctrl Pts',(-25.7687350277746,25.8882820073453,-64.350216288159));
#11461=CARTESIAN_POINT('Ctrl Pts',(-25.8562926991825,25.8029040677121,-64.3424208715681));
#11462=CARTESIAN_POINT('Ctrl Pts',(-25.9103875456094,25.7461626638787,-64.3373400830642));
#11463=CARTESIAN_POINT('Ctrl Pts',(-26.0715152812713,25.5643141749668,-64.3213657804476));
#11464=CARTESIAN_POINT('Ctrl Pts',(-26.1710664721605,25.4329463392836,-64.3102370109255));
#11465=CARTESIAN_POINT('Ctrl Pts',(-26.3499348240832,25.1550639360616,-64.2878690354011));
#11466=CARTESIAN_POINT('Ctrl Pts',(-26.4288313082328,25.0088255016172,-64.2766650016213));
#11467=CARTESIAN_POINT('Ctrl Pts',(-26.5115508950291,24.8223678775062,-64.2635420867628));
#11468=CARTESIAN_POINT('Ctrl Pts',(-26.5263651183379,24.7873134190912,-64.2611235630608));
#11469=CARTESIAN_POINT('Ctrl Pts',(-26.5425141385358,24.7471299772286,-64.2584127964122));
#11470=CARTESIAN_POINT('Ctrl Pts',(-26.5444605980969,24.7422521958828,-64.2580847664786));
#11471=CARTESIAN_POINT('Ctrl Pts',(-26.5472928226342,24.7351039974642,-64.2576055726203));
#11472=CARTESIAN_POINT('Ctrl Pts',(-26.5481879369135,24.7328373310562,-64.2574538455939));
#11473=CARTESIAN_POINT('Ctrl Pts',(-26.5497706101838,24.728816238083,-64.2571850790434));
#11474=CARTESIAN_POINT('Ctrl Pts',(-26.5504592018574,24.7270622230143,-64.2570679766538));
#11475=CARTESIAN_POINT('Ctrl Pts',(-26.5518965742178,24.7233914148583,-64.2568231867984));
#11476=CARTESIAN_POINT('Ctrl Pts',(-26.5526450558276,24.7214745124877,-64.2566955177541));
#11477=CARTESIAN_POINT('Ctrl Pts',(-26.5546007548049,24.7164516660621,-64.2563614047447));
#11478=CARTESIAN_POINT('Ctrl Pts',(-26.555804995818,24.7133445539983,-64.2561551414442));
#11479=CARTESIAN_POINT('Ctrl Pts',(-26.5610685554054,24.6997010632646,-64.2552512368258));
#11480=CARTESIAN_POINT('Ctrl Pts',(-26.5650773687746,24.6891450929245,-64.2545566137816));
#11481=CARTESIAN_POINT('Ctrl Pts',(-26.5940491188967,24.6116319486059,-64.2494890156958));
#11482=CARTESIAN_POINT('Ctrl Pts',(-26.6168365543966,24.5438762741761,-64.2452395640017));
#11483=CARTESIAN_POINT('Ctrl Pts',(-26.7271183623599,24.1758849465667,-64.2228374271424));
#11484=CARTESIAN_POINT('Ctrl Pts',(-26.7728155786524,23.8648892164005,-64.2061317082339));
#11485=CARTESIAN_POINT('Ctrl Pts',(-26.7730019592961,23.5521733105916,-64.1880685683874));
#11486=CARTESIAN_POINT('Ctrl Pts',(-26.7730019617299,23.5521692227448,-64.1880683322646));
#11487=CARTESIAN_POINT('Ctrl Pts',(-26.7730705287399,23.4368797543027,-64.1814089624338));
#11488=CARTESIAN_POINT('Ctrl Pts',(-26.7669527001803,23.3216786349966,-64.1746044679484));
#11489=CARTESIAN_POINT('Ctrl Pts',(-26.7537718069693,23.1986077503722,-64.1670816578786));
#11490=CARTESIAN_POINT('Ctrl Pts',(-26.7528332958108,23.190160534511,-64.1665640493305));
#11491=CARTESIAN_POINT('Ctrl Pts',(-26.7512863760238,23.1767218447392,-64.1657385339867));
#11492=CARTESIAN_POINT('Ctrl Pts',(-26.7506996767062,23.1717278717666,-64.1654313116746));
#11493=CARTESIAN_POINT('Ctrl Pts',(-26.7496753844482,23.1631817617928,-64.1649047866224));
#11494=CARTESIAN_POINT('Ctrl Pts',(-26.7492435562446,23.1596289324079,-64.1646856661647));
#11495=CARTESIAN_POINT('Ctrl Pts',(-26.7484226643033,23.1529677742654,-64.1642744037089));
#11496=CARTESIAN_POINT('Ctrl Pts',(-26.7480349846954,23.1498592765489,-64.1640823056801));
#11497=CARTESIAN_POINT('Ctrl Pts',(-26.7472190114404,23.1433934095522,-64.1636823570839));
#11498=CARTESIAN_POINT('Ctrl Pts',(-26.7467899600381,23.1400361412994,-64.1634744827644));
#11499=CARTESIAN_POINT('Ctrl Pts',(-26.7457940840224,23.1323399844659,-64.1629974717991));
#11500=CARTESIAN_POINT('Ctrl Pts',(-26.7452237105887,23.1280015689735,-64.1627282230921));
#11501=CARTESIAN_POINT('Ctrl Pts',(-26.7433975020945,23.1143264932296,-64.1618784091012));
#11502=CARTESIAN_POINT('Ctrl Pts',(-26.7421095708715,23.1049942342591,-64.1612968279706));
#11503=CARTESIAN_POINT('Ctrl Pts',(-26.7311149402433,23.0278278017878,-64.1564740561185));
#11504=CARTESIAN_POINT('Ctrl Pts',(-26.7192885460338,22.9603179288108,-64.1521659018376));
#11505=CARTESIAN_POINT('Ctrl Pts',(-26.7029014511981,22.8816247409082,-64.1470334688314));
#11506=CARTESIAN_POINT('Ctrl Pts',(-26.700418542194,22.8700228405997,-64.1462739551814));
#11507=CARTESIAN_POINT('Ctrl Pts',(-26.6922833644443,22.8330095514438,-64.1438418371539));
#11508=CARTESIAN_POINT('Ctrl Pts',(-26.6863873435955,22.8076532936505,-64.1421620155736));
#11509=CARTESIAN_POINT('Ctrl Pts',(-26.6756982682776,22.7640839196378,-64.1392520669069));
#11510=CARTESIAN_POINT('Ctrl Pts',(-26.6710514943295,22.7458360026547,-64.1380261469508));
#11511=CARTESIAN_POINT('Ctrl Pts',(-26.5869685102774,22.4273399880419,-64.116504830388));
#11512=CARTESIAN_POINT('Ctrl Pts',(-26.4647201024252,22.1401423477394,-64.0949388877303));
#11513=CARTESIAN_POINT('Ctrl Pts',(-26.2760375579856,21.8300885540783,-64.0710959493273));
#11514=CARTESIAN_POINT('Ctrl Pts',(-26.2476820355212,21.7859558206728,-64.0676931377554));
#11515=CARTESIAN_POINT('Ctrl Pts',(-26.2041085302775,21.7216458453609,-64.0627429431857));
#11516=CARTESIAN_POINT('Ctrl Pts',(-26.1897115346993,21.7009255345114,-64.0611493645717));
#11517=CARTESIAN_POINT('Ctrl Pts',(-26.1725719836609,21.676866073317,-64.0593025944261));
#11518=CARTESIAN_POINT('Ctrl Pts',(-26.1700647569084,21.6733614757914,-64.059033677503));
#11519=CARTESIAN_POINT('Ctrl Pts',(-26.1662244272954,21.668016157295,-64.0586236698543));
#11520=CARTESIAN_POINT('Ctrl Pts',(-26.1648964063172,21.6661718177491,-64.0584822293488));
#11521=CARTESIAN_POINT('Ctrl Pts',(-26.1624858797467,21.662831564512,-64.0582261215776));
#11522=CARTESIAN_POINT('Ctrl Pts',(-26.1614040434038,21.6613351817333,-64.0581114086065));
#11523=CARTESIAN_POINT('Ctrl Pts',(-26.1590409811853,21.658072532469,-64.0578613358065));
#11524=CARTESIAN_POINT('Ctrl Pts',(-26.1577592507941,21.6563066418698,-64.0577260122036));
#11525=CARTESIAN_POINT('Ctrl Pts',(-26.1542483825853,21.6514798994808,-64.0573561991558));
#11526=CARTESIAN_POINT('Ctrl Pts',(-26.1520156332272,21.6484216600992,-64.057121961034));
#11527=CARTESIAN_POINT('Ctrl Pts',(-26.1411581357811,21.6336048429315,-64.0559874385039));
#11528=CARTESIAN_POINT('Ctrl Pts',(-26.1324588573702,21.6219007166078,-64.0550922774014));
#11529=CARTESIAN_POINT('Ctrl Pts',(-26.1183830893925,21.6032290506122,-64.0536651532135));
#11530=CARTESIAN_POINT('Ctrl Pts',(-26.1130571136743,21.5962239557053,-64.0531299482134));
#11531=CARTESIAN_POINT('Ctrl Pts',(-26.1045092496733,21.5850762749948,-64.0522784242872));
#11532=CARTESIAN_POINT('Ctrl Pts',(-26.1013058642982,21.580919650687,-64.0519609585373));
#11533=CARTESIAN_POINT('Ctrl Pts',(-26.0953314460543,21.5732064499163,-64.0513718941258));
#11534=CARTESIAN_POINT('Ctrl Pts',(-26.0925630806866,21.5696478354548,-64.051100134468));
#11535=CARTESIAN_POINT('Ctrl Pts',(-25.8970870582046,21.3194569403249,-64.0319940167032));
#11536=CARTESIAN_POINT('Ctrl Pts',(-25.6694571300877,21.1021675974939,-64.0152769791579));
#11537=CARTESIAN_POINT('Ctrl Pts',(-25.3563507809447,20.8802103790905,-63.9934677852187));
#11538=CARTESIAN_POINT('Ctrl Pts',(-25.2973460683086,20.8412343809095,-63.9894094864369));
#11539=CARTESIAN_POINT('Ctrl Pts',(-25.1806798013622,20.7695672835645,-63.9814302668747));
#11540=CARTESIAN_POINT('Ctrl Pts',(-25.1231978877306,20.7366524274511,-63.9775188885714));
#11541=CARTESIAN_POINT('Ctrl Pts',(-25.0340302718407,20.6891807018647,-63.9714562613091));
#11542=CARTESIAN_POINT('Ctrl Pts',(-25.0030530761247,20.6733272928093,-63.9693510342015));
#11543=CARTESIAN_POINT('Ctrl Pts',(-24.9654104574199,20.6548256697856,-63.9667918701821));
#11544=CARTESIAN_POINT('Ctrl Pts',(-24.9589843242541,20.6516936824145,-63.9663549528071));
#11545=CARTESIAN_POINT('Ctrl Pts',(-24.9496022686101,20.6471595984169,-63.965716995902));
#11546=CARTESIAN_POINT('Ctrl Pts',(-24.9466545159541,20.6457405651702,-63.9655165467038));
#11547=CARTESIAN_POINT('Ctrl Pts',(-24.9407857025368,20.6429263473029,-63.9651174427771));
#11548=CARTESIAN_POINT('Ctrl Pts',(-24.9378646900798,20.6415310703925,-63.9649187915497));
#11549=CARTESIAN_POINT('Ctrl Pts',(-24.9320349983477,20.6387571876583,-63.9645223054992));
#11550=CARTESIAN_POINT('Ctrl Pts',(-24.9291263457955,20.6373785337065,-63.9643244726193));
#11551=CARTESIAN_POINT('Ctrl Pts',(-24.9221225438031,20.6340716867194,-63.9638480778172));
#11552=CARTESIAN_POINT('Ctrl Pts',(-24.9180253959663,20.6321477628146,-63.9635693681469));
#11553=CARTESIAN_POINT('Ctrl Pts',(-24.9054503450736,20.6262751178796,-63.9627138650032));
#11554=CARTESIAN_POINT('Ctrl Pts',(-24.8969593519087,20.6223546906975,-63.9621360938527));
#11555=CARTESIAN_POINT('Ctrl Pts',(-24.798450267718,20.5773906420531,-63.9554314511367));
#11556=CARTESIAN_POINT('Ctrl Pts',(-24.706614192966,20.5404801744819,-63.9491632588301));
#11557=CARTESIAN_POINT('Ctrl Pts',(-24.4515056107939,20.4513479872491,-63.9316767772493));
#11558=CARTESIAN_POINT('Ctrl Pts',(-24.2855480110023,20.4078339992852,-63.920206275327));
#11559=CARTESIAN_POINT('Ctrl Pts',(-24.0984010274011,20.3744053370231,-63.9073502830479));
#11560=CARTESIAN_POINT('Ctrl Pts',(-24.0798345943667,20.371256618963,-63.9060759795227));
#11561=CARTESIAN_POINT('Ctrl Pts',(-24.0400091674661,20.364861120029,-63.9033458209433));
#11562=CARTESIAN_POINT('Ctrl Pts',(-24.0187430595912,20.3616640299179,-63.9018899381512));
#11563=CARTESIAN_POINT('Ctrl Pts',(-23.9726839482421,20.3552103589659,-63.8987424266396));
#11564=CARTESIAN_POINT('Ctrl Pts',(-23.9478817041959,20.3520289874423,-63.8970510918087));
#11565=CARTESIAN_POINT('Ctrl Pts',(-23.7509057044796,20.3290897560119,-63.8836560086442));
#11566=CARTESIAN_POINT('Ctrl Pts',(-23.5774040922814,20.3229578260456,-63.8720677024364));
#11567=CARTESIAN_POINT('Ctrl Pts',(-23.3981300478816,20.3310890370325,-63.8608231382064));
#11568=CARTESIAN_POINT('Ctrl Pts',(-23.3920302638334,20.3313830763026,-63.8604414352876));
#11569=CARTESIAN_POINT('Ctrl Pts',(-23.3833141402341,20.3318280719158,-63.8598973222624));
#11570=CARTESIAN_POINT('Ctrl Pts',(-23.3806971400581,20.3319648815412,-63.8597341222876));
#11571=CARTESIAN_POINT('Ctrl Pts',(-23.3761756236782,20.3322067845418,-63.8594524492695));
#11572=CARTESIAN_POINT('Ctrl Pts',(-23.3742710313197,20.3323103767962,-63.8593338911152));
#11573=CARTESIAN_POINT('Ctrl Pts',(-23.3706065260107,20.3325129551915,-63.8591059565364));
#11574=CARTESIAN_POINT('Ctrl Pts',(-23.3688466057643,20.33261169412,-63.8589965661811));
#11575=CARTESIAN_POINT('Ctrl Pts',(-23.3646788386604,20.3328489536766,-63.8587376950889));
#11576=CARTESIAN_POINT('Ctrl Pts',(-23.3622710604257,20.3329887336921,-63.8585882857958));
#11577=CARTESIAN_POINT('Ctrl Pts',(-23.3550937191874,20.3334134884345,-63.8581433358596));
#11578=CARTESIAN_POINT('Ctrl Pts',(-23.3503246035648,20.3337063690241,-63.8578482388794));
#11579=CARTESIAN_POINT('Ctrl Pts',(-23.306162805618,20.3365170280623,-63.8551206783509));
#11580=CARTESIAN_POINT('Ctrl Pts',(-23.2668166795536,20.3397478758041,-63.8527275748206));
#11581=CARTESIAN_POINT('Ctrl Pts',(-22.9865928048519,20.367950260551,-63.8358852588362));
#11582=CARTESIAN_POINT('Ctrl Pts',(-22.7491153052075,20.4192827474275,-63.8226332760825));
#11583=CARTESIAN_POINT('Ctrl Pts',(-22.4165045867567,20.5315484604748,-63.8029538420744));
#11584=CARTESIAN_POINT('Ctrl Pts',(-22.3152359230958,20.5715463418504,-63.7968083420412));
#11585=CARTESIAN_POINT('Ctrl Pts',(-22.1427337938606,20.6499904795538,-63.7858679392452));
#11586=CARTESIAN_POINT('Ctrl Pts',(-22.0705641230587,20.6861384169175,-63.7811390921964));
#11587=CARTESIAN_POINT('Ctrl Pts',(-21.9749264968325,20.7386208981422,-63.7746199851272));
#11588=CARTESIAN_POINT('Ctrl Pts',(-21.9502046603625,20.7526157985357,-63.772911320248));
#11589=CARTESIAN_POINT('Ctrl Pts',(-21.9151779193311,20.7730603869728,-63.7704551427186));
#11590=CARTESIAN_POINT('Ctrl Pts',(-21.9047190337172,20.7792446469253,-63.7697171814));
#11591=CARTESIAN_POINT('Ctrl Pts',(-21.8887288906729,20.7888219502665,-63.7685818289633));
#11592=CARTESIAN_POINT('Ctrl Pts',(-21.8831724155348,20.7921728462872,-63.7681859739347));
#11593=CARTESIAN_POINT('Ctrl Pts',(-21.8728787535881,20.7984230279495,-63.7674501460662));
#11594=CARTESIAN_POINT('Ctrl Pts',(-21.8681388605158,20.8013178278895,-63.7671103384819));
#11595=CARTESIAN_POINT('Ctrl Pts',(-21.8603629806659,20.806094441098,-63.7665512507349));
#11596=CARTESIAN_POINT('Ctrl Pts',(-21.8573225839227,20.8079690830634,-63.7663322351592));
#11597=CARTESIAN_POINT('Ctrl Pts',(-21.8514058872887,20.811630778334,-63.7659052218427));
#11598=CARTESIAN_POINT('Ctrl Pts',(-21.8485292740805,20.8134173186164,-63.7656972432565));
#11599=CARTESIAN_POINT('Ctrl Pts',(-21.8419328394238,20.8175285001512,-63.7652194674915));
#11600=CARTESIAN_POINT('Ctrl Pts',(-21.8382149437047,20.8198562050452,-63.7649495570465));
#11601=CARTESIAN_POINT('Ctrl Pts',(-21.82647934245,20.8272370391897,-63.7640955926265));
#11602=CARTESIAN_POINT('Ctrl Pts',(-21.8184792235889,20.8323179138948,-63.7635105085979));
#11603=CARTESIAN_POINT('Ctrl Pts',(-21.7516147202846,20.8751986197399,-63.7585955080922));
#11604=CARTESIAN_POINT('Ctrl Pts',(-21.6939770742644,20.9148680064451,-63.7541957612489));
#11605=CARTESIAN_POINT('Ctrl Pts',(-21.6317022968779,20.9607858485135,-63.7492521478341));
#11606=CARTESIAN_POINT('Ctrl Pts',(-21.625740732974,20.9652134523057,-63.7487769219705));
#11607=CARTESIAN_POINT('Ctrl Pts',(-21.38639132393,21.1442631291757,-63.7296174940043));
#11608=CARTESIAN_POINT('Ctrl Pts',(-21.1777833691933,21.3497046968137,-63.7096775556436));
#11609=CARTESIAN_POINT('Ctrl Pts',(-20.9752499967116,21.6119347115869,-63.6874130259167));
#11610=CARTESIAN_POINT('Ctrl Pts',(-20.9514161569602,21.6440091877463,-63.6847399501044));
#11611=CARTESIAN_POINT('Ctrl Pts',(-20.8852383737793,21.7366171747634,-63.6771791611519));
#11612=CARTESIAN_POINT('Ctrl Pts',(-20.844367722759,21.7981786775426,-63.6723387859319));
#11613=CARTESIAN_POINT('Ctrl Pts',(-20.7897666933114,21.8868964752515,-63.6656757659608));
#11614=CARTESIAN_POINT('Ctrl Pts',(-20.7742511734583,21.9129217593063,-63.6637577115796));
#11615=CARTESIAN_POINT('Ctrl Pts',(-20.7568460347575,21.9430754687577,-63.6615804674114));
#11616=CARTESIAN_POINT('Ctrl Pts',(-20.7545959827465,21.9469925934194,-63.6612984969028));
#11617=CARTESIAN_POINT('Ctrl Pts',(-20.7512045808096,21.952925546657,-63.6608727410235));
#11618=CARTESIAN_POINT('Ctrl Pts',(-20.7500571678572,21.9549378752999,-63.6607285634278));
#11619=CARTESIAN_POINT('Ctrl Pts',(-20.7479891984159,21.9585737774107,-63.6604684781199));
#11620=CARTESIAN_POINT('Ctrl Pts',(-20.7470678850446,21.9601969091706,-63.6603525212478));
#11621=CARTESIAN_POINT('Ctrl Pts',(-20.7450863575523,21.9636949571812,-63.6601029429255));
#11622=CARTESIAN_POINT('Ctrl Pts',(-20.7440266158362,21.9655701310136,-63.6599693525064));
#11623=CARTESIAN_POINT('Ctrl Pts',(-20.7411683870409,21.9706395195118,-63.6596087352707));
#11624=CARTESIAN_POINT('Ctrl Pts',(-20.7393734617399,21.9738357548205,-63.6593819394515));
#11625=CARTESIAN_POINT('Ctrl Pts',(-20.7310542713298,21.9887091755037,-63.6583291888951));
#11626=CARTESIAN_POINT('Ctrl Pts',(-20.7245971693526,22.0004240661892,-63.657507512998));
#11627=CARTESIAN_POINT('Ctrl Pts',(-20.6101705098749,22.2111167425203,-63.6428576504378));
#11628=CARTESIAN_POINT('Ctrl Pts',(-20.5233708623193,22.4209211035782,-63.6302824706869));
#11629=CARTESIAN_POINT('Ctrl Pts',(-20.4155552430319,22.786280755243,-63.6089976397962));
#11630=CARTESIAN_POINT('Ctrl Pts',(-20.3825453478305,22.9373846372241,-63.6003619625065));
#11631=CARTESIAN_POINT('Ctrl Pts',(-20.3488509014325,23.1710363277222,-63.5867271118006));
#11632=CARTESIAN_POINT('Ctrl Pts',(-20.340275900134,23.2522160021309,-63.5819414628024));
#11633=CARTESIAN_POINT('Ctrl Pts',(-20.3329668243196,23.3607086887941,-63.5754372235408));
#11634=CARTESIAN_POINT('Ctrl Pts',(-20.3314846938707,23.3878095276511,-63.5738036343527));
#11635=CARTESIAN_POINT('Ctrl Pts',(-20.3298518885951,23.42665965181,-63.5714478470625));
#11636=CARTESIAN_POINT('Ctrl Pts',(-20.3294228661545,23.4383965442188,-63.5707343241441));
#11637=CARTESIAN_POINT('Ctrl Pts',(-20.3287777064455,23.4591540797623,-63.5694690742153));
#11638=CARTESIAN_POINT('Ctrl Pts',(-20.3285352783116,23.4681738237055,-63.5689181744574));
#11639=CARTESIAN_POINT('Ctrl Pts',(-20.3282326278722,23.4815209482628,-63.5681012868246));
#11640=CARTESIAN_POINT('Ctrl Pts',(-20.3281432371977,23.4858476777182,-63.567836215073));
#11641=CARTESIAN_POINT('Ctrl Pts',(-20.3280026692474,23.4933868240555,-63.5673738777901));
#11642=CARTESIAN_POINT('Ctrl Pts',(-20.3279475800626,23.4965991691428,-63.5671767353543));
#11643=CARTESIAN_POINT('Ctrl Pts',(-20.3278474708148,23.5029945197416,-63.5667839588131));
#11644=CARTESIAN_POINT('Ctrl Pts',(-20.3278023630571,23.5061775205948,-63.5665883276749));
#11645=CARTESIAN_POINT('Ctrl Pts',(-20.3277062275509,23.5137534786727,-63.5661223546301));
#11646=CARTESIAN_POINT('Ctrl Pts',(-20.3276594664604,23.5181464757379,-63.5658518789999));
#11647=CARTESIAN_POINT('Ctrl Pts',(-20.3275253910226,23.5337375606902,-63.5648909503702));
#11648=CARTESIAN_POINT('Ctrl Pts',(-20.3274874617954,23.5449358939998,-63.5641989487157));
#11649=CARTESIAN_POINT('Ctrl Pts',(-20.3277827164481,23.7067180442737,-63.5541748757634));
#11650=CARTESIAN_POINT('Ctrl Pts',(-20.3386109575935,23.8570743859712,-63.5445104736917));
#11651=CARTESIAN_POINT('Ctrl Pts',(-20.383242116857,24.1694315288084,-63.5236926312479));
#11652=CARTESIAN_POINT('Ctrl Pts',(-20.4190849993574,24.3307138271311,-63.5125132354459));
#11653=CARTESIAN_POINT('Ctrl Pts',(-20.5209831463022,24.6655470477836,-63.4888345211913));
#11654=CARTESIAN_POINT('Ctrl Pts',(-20.5900065332292,24.8376204989938,-63.4763831031391));
#11655=CARTESIAN_POINT('Ctrl Pts',(-20.6785543885421,25.0129885654721,-63.464006812399));
#11656=CARTESIAN_POINT('Ctrl Pts',(-20.6837347623607,25.0231146492112,-63.4632934129737));
#11657=CARTESIAN_POINT('Ctrl Pts',(-20.6905061934833,25.0361797194081,-63.4623747614039));
#11658=CARTESIAN_POINT('Ctrl Pts',(-20.6920482787161,25.0391437885016,-63.46216646784));
#11659=CARTESIAN_POINT('Ctrl Pts',(-20.6945485030537,25.0439313145061,-63.4618302366219));
#11660=CARTESIAN_POINT('Ctrl Pts',(-20.6955037805067,25.045756250535,-63.4617021176151));
#11661=CARTESIAN_POINT('Ctrl Pts',(-20.6973360154508,25.0492483496673,-63.4614570488109));
#11662=CARTESIAN_POINT('Ctrl Pts',(-20.6982126822449,25.0509156544913,-63.4613400813654));
#11663=CARTESIAN_POINT('Ctrl Pts',(-20.7002249508003,25.0547345919815,-63.461072261053));
#11664=CARTESIAN_POINT('Ctrl Pts',(-20.7013615300407,25.0568857127884,-63.4609214707655));
#11665=CARTESIAN_POINT('Ctrl Pts',(-20.7049491906215,25.0636572414902,-63.4604470009825));
#11666=CARTESIAN_POINT('Ctrl Pts',(-20.7074091004057,25.0682730007409,-63.4601238819635));
#11667=CARTESIAN_POINT('Ctrl Pts',(-20.7276044065669,25.1059460913777,-63.4574889190918));
#11668=CARTESIAN_POINT('Ctrl Pts',(-20.7459054601704,25.1386991601131,-63.4552124639472));
#11669=CARTESIAN_POINT('Ctrl Pts',(-20.7685316002909,25.1775822475626,-63.4525182583337));
#11670=CARTESIAN_POINT('Ctrl Pts',(-20.7723104414398,25.1840245750366,-63.4520721474949));
#11671=CARTESIAN_POINT('Ctrl Pts',(-20.7777491995604,25.193223373798,-63.4514354721573));
#11672=CARTESIAN_POINT('Ctrl Pts',(-20.779390873138,25.1959905375744,-63.4512439893964));
#11673=CARTESIAN_POINT('Ctrl Pts',(-20.9230350018789,25.437289258005,-63.4345496835121));
#11674=CARTESIAN_POINT('Ctrl Pts',(-21.0952746094889,25.656506257936,-63.419566435846));
#11675=CARTESIAN_POINT('Ctrl Pts',(-21.4236109891949,25.9785704188034,-63.3935584218942));
#11676=CARTESIAN_POINT('Ctrl Pts',(-21.5642871937126,26.094905502202,-63.3830085985986));
#11677=CARTESIAN_POINT('Ctrl Pts',(-21.720765885027,26.2033947132951,-63.3714322668509));
#11678=CARTESIAN_POINT('Ctrl Pts',(-21.7275236265351,26.2080418691839,-63.3709326720764));
#11679=CARTESIAN_POINT('Ctrl Pts',(-21.7383512948461,26.2154271096762,-63.3701327074382));
#11680=CARTESIAN_POINT('Ctrl Pts',(-21.7424098921548,26.2181818061423,-63.3698329674857));
#11681=CARTESIAN_POINT('Ctrl Pts',(-21.750146871013,26.2234073735587,-63.3692617791981));
#11682=CARTESIAN_POINT('Ctrl Pts',(-21.7538240936852,26.2258799469002,-63.3689903960166));
#11683=CARTESIAN_POINT('Ctrl Pts',(-21.7602778753613,26.2302001832959,-63.3685142530566));
#11684=CARTESIAN_POINT('Ctrl Pts',(-21.7630522309862,26.2320511390944,-63.3683096179469));
#11685=CARTESIAN_POINT('Ctrl Pts',(-21.7684700755802,26.2356535999541,-63.3679100945696));
#11686=CARTESIAN_POINT('Ctrl Pts',(-21.7711132872709,26.2374055171343,-63.3677152221218));
#11687=CARTESIAN_POINT('Ctrl Pts',(-21.7773855351155,26.2415494433325,-63.367252897615));
#11688=CARTESIAN_POINT('Ctrl Pts',(-21.7810168267222,26.2439380133561,-63.3669853166727));
#11689=CARTESIAN_POINT('Ctrl Pts',(-21.793790316946,26.252303114041,-63.3660443412977));
#11690=CARTESIAN_POINT('Ctrl Pts',(-21.8029579781024,26.2582404562732,-63.3653694813257));
#11691=CARTESIAN_POINT('Ctrl Pts',(-21.8973802780614,26.3187129920576,-63.358423383883));
#11692=CARTESIAN_POINT('Ctrl Pts',(-21.9851050021773,26.3692350120708,-63.3520057379053));
#11693=CARTESIAN_POINT('Ctrl Pts',(-22.0750360636209,26.415536799411,-63.3454515897691));
#11694=CARTESIAN_POINT('Origin',(-23.5502525316942,23.5502525316942,-77.3107734492734));
#11695=CARTESIAN_POINT('',(-22.0750358661665,26.4155366977499,-61.8467738923868));
#11696=CARTESIAN_POINT('',(-22.0750361387181,26.4155368380754,-62.0907209741597));
#11697=CARTESIAN_POINT('',(-22.0750360153461,26.4155367745563,-77.3107734492734));
#11698=CARTESIAN_POINT('Ctrl Pts',(-22.0750358661665,26.4155366977499,-61.8467738923868));
#11699=CARTESIAN_POINT('Ctrl Pts',(-22.0129928290477,26.3835932963163,-61.8514971515873));
#11700=CARTESIAN_POINT('Ctrl Pts',(-21.9519838212122,26.3496329512428,-61.8562169656468));
#11701=CARTESIAN_POINT('Ctrl Pts',(-21.8373123293699,26.2808269866894,-61.8651844232319));
#11702=CARTESIAN_POINT('Ctrl Pts',(-21.7835048400784,26.2463245648821,-61.8694349606208));
#11703=CARTESIAN_POINT('Ctrl Pts',(-21.6934078442242,26.1846961059217,-61.8765849758899));
#11704=CARTESIAN_POINT('Ctrl Pts',(-21.6565993848976,26.158363601384,-61.8795157905653));
#11705=CARTESIAN_POINT('Ctrl Pts',(-21.6064397654188,26.1208577951366,-61.8835101114855));
#11706=CARTESIAN_POINT('Ctrl Pts',(-21.5926077685641,26.1103397378112,-61.8846116248033));
#11707=CARTESIAN_POINT('Ctrl Pts',(-21.5703016825142,26.093091352665,-61.8863871260411));
#11708=CARTESIAN_POINT('Ctrl Pts',(-21.5617754331277,26.0864294717038,-61.8870655873375));
#11709=CARTESIAN_POINT('Ctrl Pts',(-21.5513643027722,26.0782100837868,-61.8878936144888));
#11710=CARTESIAN_POINT('Ctrl Pts',(-21.5494475683152,26.076693315785,-61.8880460403279));
#11711=CARTESIAN_POINT('Ctrl Pts',(-21.5457396459331,26.0737522622679,-61.8883408709369));
#11712=CARTESIAN_POINT('Ctrl Pts',(-21.5439482466329,26.0723282472925,-61.8884832948846));
#11713=CARTESIAN_POINT('Ctrl Pts',(-21.5406999781058,26.0697404903059,-61.8887415132444));
#11714=CARTESIAN_POINT('Ctrl Pts',(-21.5392426069797,26.0685773959592,-61.8888573534907));
#11715=CARTESIAN_POINT('Ctrl Pts',(-21.5363096647928,26.0662325127808,-61.8890904558248));
#11716=CARTESIAN_POINT('Ctrl Pts',(-21.5348341301348,26.0650506951802,-61.8892077149119));
#11717=CARTESIAN_POINT('Ctrl Pts',(-21.5306129876552,26.0616637038761,-61.8895431315617));
#11718=CARTESIAN_POINT('Ctrl Pts',(-21.5278699422708,26.0594553186138,-61.8897610571771));
#11719=CARTESIAN_POINT('Ctrl Pts',(-21.5160367778353,26.0498966036187,-61.8907010168086));
#11720=CARTESIAN_POINT('Ctrl Pts',(-21.5069829207361,26.0425012204043,-61.8914198336178));
#11721=CARTESIAN_POINT('Ctrl Pts',(-21.3537252064486,25.915920523576,-61.903585079186));
#11722=CARTESIAN_POINT('Ctrl Pts',(-21.2201044370545,25.7844301338131,-61.9141651539333));
#11723=CARTESIAN_POINT('Ctrl Pts',(-21.0042306133337,25.5314248576174,-61.9327968648602));
#11724=CARTESIAN_POINT('Ctrl Pts',(-20.9174253597454,25.4145195206886,-61.9408650345672));
#11725=CARTESIAN_POINT('Ctrl Pts',(-20.7736815747476,25.1907685421282,-61.9559679589358));
#11726=CARTESIAN_POINT('Ctrl Pts',(-20.714291973527,25.0858183633581,-61.9629291043031));
#11727=CARTESIAN_POINT('Ctrl Pts',(-20.6379033760903,24.9312087942067,-61.9731902315352));
#11728=CARTESIAN_POINT('Ctrl Pts',(-20.6160167922721,24.8840733417468,-61.9763185172515));
#11729=CARTESIAN_POINT('Ctrl Pts',(-20.592103434601,24.8291328396221,-61.9799719750568));
#11730=CARTESIAN_POINT('Ctrl Pts',(-20.5889537600267,24.8218226264068,-61.9804582327944));
#11731=CARTESIAN_POINT('Ctrl Pts',(-20.5841935944931,24.8106609458197,-61.9812009206874));
#11732=CARTESIAN_POINT('Ctrl Pts',(-20.5825634353728,24.8068178569613,-61.9814566794468));
#11733=CARTESIAN_POINT('Ctrl Pts',(-20.5797617763984,24.8001771032373,-61.9818987023175));
#11734=CARTESIAN_POINT('Ctrl Pts',(-20.5785867477028,24.7973809252438,-61.9820848459707));
#11735=CARTESIAN_POINT('Ctrl Pts',(-20.5761648426371,24.7915947388131,-61.9824700882057));
#11736=CARTESIAN_POINT('Ctrl Pts',(-20.5749185242576,24.7886045016277,-61.9826692055228));
#11737=CARTESIAN_POINT('Ctrl Pts',(-20.571912271326,24.7813609930827,-61.9831516157349));
#11738=CARTESIAN_POINT('Ctrl Pts',(-20.5701569398472,24.7771058290956,-61.9834350646395));
#11739=CARTESIAN_POINT('Ctrl Pts',(-20.5636712424566,24.7612875630612,-61.9844889965752));
#11740=CARTESIAN_POINT('Ctrl Pts',(-20.5589990583004,24.7497008612477,-61.9852614482217));
#11741=CARTESIAN_POINT('Ctrl Pts',(-20.4848186567125,24.5626092366427,-61.997742513382));
#11742=CARTESIAN_POINT('Ctrl Pts',(-20.4308074762157,24.3813906609703,-62.0099815479479));
#11743=CARTESIAN_POINT('Ctrl Pts',(-20.3513804906614,23.9933544786537,-62.0364187489923));
#11744=CARTESIAN_POINT('Ctrl Pts',(-20.3295031678759,23.7866639580283,-62.0506333474106));
#11745=CARTESIAN_POINT('Ctrl Pts',(-20.3267327588802,23.479409023347,-62.0710991096281));
#11746=CARTESIAN_POINT('Ctrl Pts',(-20.3304777694658,23.3795089421442,-62.0776414127557));
#11747=CARTESIAN_POINT('Ctrl Pts',(-20.3400050391837,23.2663244713403,-62.0848122597754));
#11748=CARTESIAN_POINT('Ctrl Pts',(-20.3412371879281,23.2527216157348,-62.085670068894));
#11749=CARTESIAN_POINT('Ctrl Pts',(-20.3429032318838,23.2355447582734,-62.0867478441924));
#11750=CARTESIAN_POINT('Ctrl Pts',(-20.3432566604662,23.2319633614828,-62.0869722640727));
#11751=CARTESIAN_POINT('Ctrl Pts',(-20.343827567743,23.2262756858819,-62.0873281880227));
#11752=CARTESIAN_POINT('Ctrl Pts',(-20.3440411231885,23.2241690299619,-62.0874599137077));
#11753=CARTESIAN_POINT('Ctrl Pts',(-20.3444472656888,23.2202015375728,-62.087707794933));
#11754=CARTESIAN_POINT('Ctrl Pts',(-20.3446393954115,23.2183406717345,-62.0878239753032));
#11755=CARTESIAN_POINT('Ctrl Pts',(-20.3450785134423,23.2141235563539,-62.0880870777551));
#11756=CARTESIAN_POINT('Ctrl Pts',(-20.3453264792661,23.2117674154667,-62.0882339434872));
#11757=CARTESIAN_POINT('Ctrl Pts',(-20.3459713399025,23.2057042683597,-62.0886115438097));
#11758=CARTESIAN_POINT('Ctrl Pts',(-20.3463720707907,23.201997661811,-62.0888420614012));
#11759=CARTESIAN_POINT('Ctrl Pts',(-20.3477047032801,23.1898683205135,-62.0895953668878));
#11760=CARTESIAN_POINT('Ctrl Pts',(-20.3486634036319,23.1814484755917,-62.0901166633395));
#11761=CARTESIAN_POINT('Ctrl Pts',(-20.3693639182988,23.0058109526296,-62.1009587418149));
#11762=CARTESIAN_POINT('Ctrl Pts',(-20.4021507860894,22.8403639021743,-62.1105693997701));
#11763=CARTESIAN_POINT('Ctrl Pts',(-20.5081273151466,22.4633210359709,-62.1325879161485));
#11764=CARTESIAN_POINT('Ctrl Pts',(-20.5906876834503,22.2552936385596,-62.1448622759723));
#11765=CARTESIAN_POINT('Ctrl Pts',(-20.7088431593804,22.0292246008702,-62.1596327993634));
#11766=CARTESIAN_POINT('Ctrl Pts',(-20.7240226705109,22.0012018968284,-62.1614894936866));
#11767=CARTESIAN_POINT('Ctrl Pts',(-20.7792674353832,21.902731084158,-62.1681136090971));
#11768=CARTESIAN_POINT('Ctrl Pts',(-20.8215688465413,21.8335787287641,-62.1729500132687));
#11769=CARTESIAN_POINT('Ctrl Pts',(-20.8717725277658,21.7580595716378,-62.1784722270905));
#11770=CARTESIAN_POINT('Ctrl Pts',(-20.8771524358705,21.7500451514076,-62.1790613782181));
#11771=CARTESIAN_POINT('Ctrl Pts',(-20.8851045870198,21.7383131201855,-62.1799284427673));
#11772=CARTESIAN_POINT('Ctrl Pts',(-20.8876488116961,21.7345765066547,-62.1802052931658));
#11773=CARTESIAN_POINT('Ctrl Pts',(-20.8921176547927,21.728042865872,-62.1806905997266));
#11774=CARTESIAN_POINT('Ctrl Pts',(-20.8940388514819,21.7252434974902,-62.1808989254227));
#11775=CARTESIAN_POINT('Ctrl Pts',(-20.8977702961308,21.7198247974091,-62.1813029451845));
#11776=CARTESIAN_POINT('Ctrl Pts',(-20.8995800100092,21.7172051010254,-62.1814986187122));
#11777=CARTESIAN_POINT('Ctrl Pts',(-20.9038977064244,21.7109746764893,-62.1819648214144));
#11778=CARTESIAN_POINT('Ctrl Pts',(-20.9064091963405,21.7073663963932,-62.1822354846383));
#11779=CARTESIAN_POINT('Ctrl Pts',(-20.9153550660107,21.6945697096346,-62.18319776773));
#11780=CARTESIAN_POINT('Ctrl Pts',(-20.9218299695554,21.6854098518756,-62.1838909420388));
#11781=CARTESIAN_POINT('Ctrl Pts',(-21.016699183305,21.5526767772343,-62.1939999406068));
#11782=CARTESIAN_POINT('Ctrl Pts',(-21.1136623173755,21.4354907574709,-62.2037542518211));
#11783=CARTESIAN_POINT('Ctrl Pts',(-21.3930926163032,21.1426108747191,-62.2304735866183));
#11784=CARTESIAN_POINT('Ctrl Pts',(-21.5885806467701,20.9808358139375,-62.2478871123605));
#11785=CARTESIAN_POINT('Ctrl Pts',(-21.8636517967265,20.8030596873818,-62.2696505202607));
#11786=CARTESIAN_POINT('Ctrl Pts',(-21.9277439989716,20.7647259403196,-62.2745441919646));
#11787=CARTESIAN_POINT('Ctrl Pts',(-22.0197788868993,20.713935289081,-62.2812686352434));
#11788=CARTESIAN_POINT('Ctrl Pts',(-22.0466516300653,20.6995982955594,-62.2831969257403));
#11789=CARTESIAN_POINT('Ctrl Pts',(-22.0777324507544,20.6835780642153,-62.2853836406415));
#11790=CARTESIAN_POINT('Ctrl Pts',(-22.081744501315,20.6815207462935,-62.2856650865714));
#11791=CARTESIAN_POINT('Ctrl Pts',(-22.0878397184095,20.6784113501128,-62.2860914010768));
#11792=CARTESIAN_POINT('Ctrl Pts',(-22.0899197108676,20.6773531145224,-62.2862366576556));
#11793=CARTESIAN_POINT('Ctrl Pts',(-22.0935079289406,20.6755324443012,-62.2864868543271));
#11794=CARTESIAN_POINT('Ctrl Pts',(-22.0950156029074,20.674768937643,-62.2865918625836));
#11795=CARTESIAN_POINT('Ctrl Pts',(-22.0981484773234,20.673185502358,-62.2868098197411));
#11796=CARTESIAN_POINT('Ctrl Pts',(-22.0997737675708,20.6723657669166,-62.2869227562161));
#11797=CARTESIAN_POINT('Ctrl Pts',(-22.1037452255707,20.6703669314353,-62.2871983894458));
#11798=CARTESIAN_POINT('Ctrl Pts',(-22.1060921464365,20.6691893183969,-62.2873609919339));
#11799=CARTESIAN_POINT('Ctrl Pts',(-22.1150308437734,20.6647178204092,-62.2879792313528));
#11800=CARTESIAN_POINT('Ctrl Pts',(-22.1216325381559,20.6614436456489,-62.2884336347802));
#11801=CARTESIAN_POINT('Ctrl Pts',(-22.230842276655,20.6077459370177,-62.2959153895035));
#11802=CARTESIAN_POINT('Ctrl Pts',(-22.3360642199086,20.5627884214963,-62.302611188023));
#11803=CARTESIAN_POINT('Ctrl Pts',(-22.6690472797993,20.4410265493185,-62.3229049184307));
#11804=CARTESIAN_POINT('Ctrl Pts',(-22.9031468271983,20.3840129468366,-62.3359772564061));
#11805=CARTESIAN_POINT('Ctrl Pts',(-23.2343049398447,20.3416603243391,-62.3550312894282));
#11806=CARTESIAN_POINT('Ctrl Pts',(-23.3276598442164,20.3338357040676,-62.360455106484));
#11807=CARTESIAN_POINT('Ctrl Pts',(-23.4622360027322,20.3284431262117,-62.3684309047034));
#11808=CARTESIAN_POINT('Ctrl Pts',(-23.5032803639214,20.3275834294528,-62.3708840939603));
#11809=CARTESIAN_POINT('Ctrl Pts',(-23.5685923387425,20.3274633756572,-62.374825992673));
#11810=CARTESIAN_POINT('Ctrl Pts',(-23.5928552597299,20.3276927959466,-62.3762987621908));
#11811=CARTESIAN_POINT('Ctrl Pts',(-23.6234727235933,20.3283281327724,-62.3781685398715));
#11812=CARTESIAN_POINT('Ctrl Pts',(-23.6298322316303,20.3284789364037,-62.3785575227649));
#11813=CARTESIAN_POINT('Ctrl Pts',(-23.6400005541772,20.3287501839772,-62.3791804701335));
#11814=CARTESIAN_POINT('Ctrl Pts',(-23.6438096963675,20.3288585569333,-62.3794140552171));
#11815=CARTESIAN_POINT('Ctrl Pts',(-23.6509664739983,20.3290748770682,-62.3798533482555));
#11816=CARTESIAN_POINT('Ctrl Pts',(-23.6543141536537,20.329181287599,-62.3800590076558));
#11817=CARTESIAN_POINT('Ctrl Pts',(-23.6618161336828,20.3294314556131,-62.3805202728352));
#11818=CARTESIAN_POINT('Ctrl Pts',(-23.6659703284949,20.3295780320494,-62.3807759668515));
#11819=CARTESIAN_POINT('Ctrl Pts',(-23.676490800429,20.3299696168554,-62.3814241998514));
#11820=CARTESIAN_POINT('Ctrl Pts',(-23.6828566345688,20.3302254661149,-62.3818170788938));
#11821=CARTESIAN_POINT('Ctrl Pts',(-23.7174903061648,20.3317203047429,-62.3839580800118));
#11822=CARTESIAN_POINT('Ctrl Pts',(-23.7457409289805,20.333312623438,-62.3857172724736));
#11823=CARTESIAN_POINT('Ctrl Pts',(-24.091829914779,20.357395181265,-62.4074317872797));
#11824=CARTESIAN_POINT('Ctrl Pts',(-24.4045950293081,20.4265295130346,-62.4290099421752));
#11825=CARTESIAN_POINT('Ctrl Pts',(-24.7786221275252,20.569657068396,-62.4560425755213));
#11826=CARTESIAN_POINT('Ctrl Pts',(-24.8540616491972,20.6018759880461,-62.4615467381371));
#11827=CARTESIAN_POINT('Ctrl Pts',(-24.9988732268713,20.6703690472296,-62.472120824355));
#11828=CARTESIAN_POINT('Ctrl Pts',(-25.068320166187,20.7063636856155,-62.4771955609474));
#11829=CARTESIAN_POINT('Ctrl Pts',(-25.1432570223598,20.74873215936,-62.4826215037508));
#11830=CARTESIAN_POINT('Ctrl Pts',(-25.1501049739293,20.7526371417596,-62.4831168673716));
#11831=CARTESIAN_POINT('Ctrl Pts',(-25.1618891822604,20.7594143989086,-62.4839683946189));
#11832=CARTESIAN_POINT('Ctrl Pts',(-25.1668322215718,20.7622747189556,-62.4843253003983));
#11833=CARTESIAN_POINT('Ctrl Pts',(-25.1740409734131,20.7664717251891,-62.4848453620297));
#11834=CARTESIAN_POINT('Ctrl Pts',(-25.1763126587578,20.7677980495115,-62.4850091848551));
#11835=CARTESIAN_POINT('Ctrl Pts',(-25.1802302218914,20.7700917563712,-62.4852915870889));
#11836=CARTESIAN_POINT('Ctrl Pts',(-25.1818768662564,20.7710578213288,-62.4854102528117));
#11837=CARTESIAN_POINT('Ctrl Pts',(-25.1850400806851,20.7729174185853,-62.4856381425463));
#11838=CARTESIAN_POINT('Ctrl Pts',(-25.1865567743211,20.7738107285148,-62.4857473809007));
#11839=CARTESIAN_POINT('Ctrl Pts',(-25.1901418630547,20.7759262503383,-62.4860055244796));
#11840=CARTESIAN_POINT('Ctrl Pts',(-25.1922096283363,20.777149535517,-62.4861543592084));
#11841=CARTESIAN_POINT('Ctrl Pts',(-25.1983543800792,20.7807940387998,-62.4865964938784));
#11842=CARTESIAN_POINT('Ctrl Pts',(-25.2024274158445,20.7832219573462,-62.4868893579577));
#11843=CARTESIAN_POINT('Ctrl Pts',(-25.2394591385469,20.8054073210776,-62.4895503358395));
#11844=CARTESIAN_POINT('Ctrl Pts',(-25.272069117675,20.8257448412113,-62.491881164575));
#11845=CARTESIAN_POINT('Ctrl Pts',(-25.3141120154441,20.8530217617458,-62.4948804968314));
#11846=CARTESIAN_POINT('Ctrl Pts',(-25.3238802412992,20.8594350239051,-62.495576949496));
#11847=CARTESIAN_POINT('Ctrl Pts',(-25.585061092671,21.0329517169793,-62.5141936240352));
#11848=CARTESIAN_POINT('Ctrl Pts',(-25.8118198727742,21.2345209136155,-62.5303571584884));
#11849=CARTESIAN_POINT('Ctrl Pts',(-26.0705907974369,21.5393821136638,-62.553136679786));
#11850=CARTESIAN_POINT('Ctrl Pts',(-26.1305141550632,21.6168740396499,-62.5587978570835));
#11851=CARTESIAN_POINT('Ctrl Pts',(-26.2233705947597,21.7489756352637,-62.5683528354367));
#11852=CARTESIAN_POINT('Ctrl Pts',(-26.2583781256126,21.8020495837787,-62.5721674979254));
#11853=CARTESIAN_POINT('Ctrl Pts',(-26.2962061472483,21.8632650320275,-62.5765539364127));
#11854=CARTESIAN_POINT('Ctrl Pts',(-26.30059263444,21.8704259335206,-62.5770668462303));
#11855=CARTESIAN_POINT('Ctrl Pts',(-26.3071414192618,21.8812111796943,-62.5778390714714));
#11856=CARTESIAN_POINT('Ctrl Pts',(-26.309324691286,21.8848228000702,-62.5780976164736));
#11857=CARTESIAN_POINT('Ctrl Pts',(-26.3130681012696,21.8910428015224,-62.5785428101684));
#11858=CARTESIAN_POINT('Ctrl Pts',(-26.3146316588432,21.8936491266925,-62.5787293333504));
#11859=CARTESIAN_POINT('Ctrl Pts',(-26.3178447622879,21.8990223283942,-62.5791138235098));
#11860=CARTESIAN_POINT('Ctrl Pts',(-26.3194938510238,21.9017894734719,-62.5793118069436));
#11861=CARTESIAN_POINT('Ctrl Pts',(-26.3234549781928,21.9084589007506,-62.5797889324758));
#11862=CARTESIAN_POINT('Ctrl Pts',(-26.3257629280068,21.912363592997,-62.5800682233375));
#11863=CARTESIAN_POINT('Ctrl Pts',(-26.3328241096206,21.9243677966459,-62.5809267099883));
#11864=CARTESIAN_POINT('Ctrl Pts',(-26.3375501553278,21.9324831685786,-62.5815068928365));
#11865=CARTESIAN_POINT('Ctrl Pts',(-26.3548417410275,21.9624762699824,-62.5836505324463));
#11866=CARTESIAN_POINT('Ctrl Pts',(-26.3671854592183,21.98448022584,-62.5852219731323));
#11867=CARTESIAN_POINT('Ctrl Pts',(-26.3821602589964,22.0119246679084,-62.5871809053969));
#11868=CARTESIAN_POINT('Ctrl Pts',(-26.38503633115,22.0172310700057,-62.5875596176597));
#11869=CARTESIAN_POINT('Ctrl Pts',(-26.3911517994245,22.028590268529,-62.5883702156668));
#11870=CARTESIAN_POINT('Ctrl Pts',(-26.3943867912183,22.0346453909224,-62.5888022542491));
#11871=CARTESIAN_POINT('Ctrl Pts',(-26.3983128664709,22.042050889778,-62.5893305787049));
#11872=CARTESIAN_POINT('Ctrl Pts',(-26.3990223949101,22.0433915130109,-62.5894262191064));
#11873=CARTESIAN_POINT('Ctrl Pts',(-26.4028668559724,22.05066787578,-62.5899453028994));
#11874=CARTESIAN_POINT('Ctrl Pts',(-26.4059841654655,22.0566128635963,-62.5903693589371));
#11875=CARTESIAN_POINT('Ctrl Pts',(-26.4117177282151,22.0676308431104,-62.5911551866483));
#11876=CARTESIAN_POINT('Ctrl Pts',(-26.4143391269476,22.0727011394984,-62.5915167787588));
#11877=CARTESIAN_POINT('Ctrl Pts',(-26.4233210091737,22.0901875665082,-62.5927637294659));
#11878=CARTESIAN_POINT('Ctrl Pts',(-26.4296142669598,22.1026378845407,-62.593651371961));
#11879=CARTESIAN_POINT('Ctrl Pts',(-26.4418201580501,22.1271800148201,-62.5954007725723));
#11880=CARTESIAN_POINT('Ctrl Pts',(-26.4477382730089,22.139268798126,-62.5962623260977));
#11881=CARTESIAN_POINT('Ctrl Pts',(-26.5189800641106,22.2871309996907,-62.6067985072832));
#11882=CARTESIAN_POINT('Ctrl Pts',(-26.5747724853271,22.4272706406842,-62.6167795648067));
#11883=CARTESIAN_POINT('Ctrl Pts',(-26.702982982022,22.8291665877747,-62.6451666043849));
#11884=CARTESIAN_POINT('Ctrl Pts',(-26.7524699199394,23.0969343249204,-62.6638799285124));
#11885=CARTESIAN_POINT('Ctrl Pts',(-26.768514041884,23.3797943424662,-62.6817396378307));
#11886=CARTESIAN_POINT('Ctrl Pts',(-26.7691296772904,23.3918445937908,-62.6824967211706));
#11887=CARTESIAN_POINT('Ctrl Pts',(-26.7698326388904,23.4073079755048,-62.6834631657312));
#11888=CARTESIAN_POINT('Ctrl Pts',(-26.7699822283031,23.4107179702774,-62.6836759701472));
#11889=CARTESIAN_POINT('Ctrl Pts',(-26.7702140841203,23.4162022695238,-62.6840177077187));
#11890=CARTESIAN_POINT('Ctrl Pts',(-26.7702997637458,23.4182764152723,-62.6841468331699));
#11891=CARTESIAN_POINT('Ctrl Pts',(-26.7704591843564,23.4222282843805,-62.6843926278519));
#11892=CARTESIAN_POINT('Ctrl Pts',(-26.7705332865564,23.4241059755363,-62.6845093164454));
#11893=CARTESIAN_POINT('Ctrl Pts',(-26.7706983377364,23.4283831806955,-62.6847748997444));
#11894=CARTESIAN_POINT('Ctrl Pts',(-26.7707882471821,23.4307827291293,-62.684923734947));
#11895=CARTESIAN_POINT('Ctrl Pts',(-26.7710594895735,23.4382446611005,-62.6853860821668));
#11896=CARTESIAN_POINT('Ctrl Pts',(-26.7712315697593,23.4433074047653,-62.6856990738291));
#11897=CARTESIAN_POINT('Ctrl Pts',(-26.7724552319534,23.4819951796002,-62.6880856453007));
#11898=CARTESIAN_POINT('Ctrl Pts',(-26.7729922391513,23.5156360039366,-62.6901308417443));
#11899=CARTESIAN_POINT('Ctrl Pts',(-26.7730296419443,23.6396655684802,-62.6975807248413));
#11900=CARTESIAN_POINT('Ctrl Pts',(-26.7692544859915,23.7300197869808,-62.7028311695884));
#11901=CARTESIAN_POINT('Ctrl Pts',(-26.7363864459781,24.1211752484018,-62.7252426017645));
#11902=CARTESIAN_POINT('Ctrl Pts',(-26.6688805455199,24.4171860465191,-62.7415343484805));
#11903=CARTESIAN_POINT('Ctrl Pts',(-26.5537003617462,24.7189497494565,-62.7604473963805));
#11904=CARTESIAN_POINT('Ctrl Pts',(-26.5460786432166,24.7383509859413,-62.7616732994514));
#11905=CARTESIAN_POINT('Ctrl Pts',(-26.5361900199105,24.7628223984125,-62.7632328820045));
#11906=CARTESIAN_POINT('Ctrl Pts',(-26.5340973894631,24.7679627720399,-62.7635612299817));
#11907=CARTESIAN_POINT('Ctrl Pts',(-26.5304557374567,24.7768424373042,-62.7641297412657));
#11908=CARTESIAN_POINT('Ctrl Pts',(-26.528912926646,24.7805842737531,-62.7643697121258));
#11909=CARTESIAN_POINT('Ctrl Pts',(-26.5259493637181,24.7877336654344,-62.7648289952333));
#11910=CARTESIAN_POINT('Ctrl Pts',(-26.5245297963266,24.7911417070074,-62.7650482702017));
#11911=CARTESIAN_POINT('Ctrl Pts',(-26.5026524000153,24.8434108799967,-62.7684165475364));
#11912=CARTESIAN_POINT('Ctrl Pts',(-26.4809997975422,24.8917604362934,-62.7716029759637));
#11913=CARTESIAN_POINT('Ctrl Pts',(-26.4544013119957,24.9474331597046,-62.775363038213));
#11914=CARTESIAN_POINT('Ctrl Pts',(-26.4506041641618,24.955298527771,-62.775896398483));
#11915=CARTESIAN_POINT('Ctrl Pts',(-26.444895042529,24.9670025756601,-62.7766933016317));
#11916=CARTESIAN_POINT('Ctrl Pts',(-26.4430072814539,24.9708530772631,-62.7769559983644));
#11917=CARTESIAN_POINT('Ctrl Pts',(-26.4396255958531,24.9777160743321,-62.7774251609249));
#11918=CARTESIAN_POINT('Ctrl Pts',(-26.4381346285709,24.980730026746,-62.777631522954));
#11919=CARTESIAN_POINT('Ctrl Pts',(-26.4349802734148,24.9870814443392,-62.7780670854253));
#11920=CARTESIAN_POINT('Ctrl Pts',(-26.4333158054882,24.9904183649158,-62.7782963235422));
#11921=CARTESIAN_POINT('Ctrl Pts',(-26.4289017080804,24.9992294150238,-62.7789026866957));
#11922=CARTESIAN_POINT('Ctrl Pts',(-26.4261422653967,25.0046985870319,-62.7792801563821));
#11923=CARTESIAN_POINT('Ctrl Pts',(-26.4135642632315,25.0294522432237,-62.7809935726485));
#11924=CARTESIAN_POINT('Ctrl Pts',(-26.4035673955934,25.0486450400871,-62.7823357981142));
#11925=CARTESIAN_POINT('Ctrl Pts',(-26.3287178626129,25.188881639354,-62.7922462555966));
#11926=CARTESIAN_POINT('Ctrl Pts',(-26.2563896371225,25.3057547256251,-62.8010835337991));
#11927=CARTESIAN_POINT('Ctrl Pts',(-26.0142863146747,25.6462853194517,-62.8286491044187));
#11928=CARTESIAN_POINT('Ctrl Pts',(-25.8225997747101,25.8526928507429,-62.848067056912));
#11929=CARTESIAN_POINT('Ctrl Pts',(-25.5964981336581,26.0400657048609,-62.8673736752427));
#11930=CARTESIAN_POINT('Ctrl Pts',(-25.5863152584952,26.0483997016849,-62.8682361720479));
#11931=CARTESIAN_POINT('Ctrl Pts',(-25.5730428972445,26.0591271727087,-62.8693510113248));
#11932=CARTESIAN_POINT('Ctrl Pts',(-25.5699998283481,26.0615776172243,-62.869605988426));
#11933=CARTESIAN_POINT('Ctrl Pts',(-25.5591255267451,26.0703016458713,-62.8705148679604));
#11934=CARTESIAN_POINT('Ctrl Pts',(-25.5512693806771,26.0765442454336,-62.8711672944525));
#11935=CARTESIAN_POINT('Ctrl Pts',(-25.503895134036,26.1138288247311,-62.8750758424063));
#11936=CARTESIAN_POINT('Ctrl Pts',(-25.4636818136582,26.1439818767783,-62.8782866710628));
#11937=CARTESIAN_POINT('Ctrl Pts',(-25.4186205381457,26.1761513561175,-62.8817540334784));
#11938=CARTESIAN_POINT('Ctrl Pts',(-25.4144569966578,26.1791088148145,-62.8820732048896));
#11939=CARTESIAN_POINT('Ctrl Pts',(-25.4082495643326,26.1834959329452,-62.8825472480335));
#11940=CARTESIAN_POINT('Ctrl Pts',(-25.4062110409021,26.1849331187345,-62.8827026344115));
#11941=CARTESIAN_POINT('Ctrl Pts',(-25.4027113003732,26.1873944043916,-62.8829689027244));
#11942=CARTESIAN_POINT('Ctrl Pts',(-25.4012509016124,26.1884196569889,-62.8830798643828));
#11943=CARTESIAN_POINT('Ctrl Pts',(-25.3983944021739,26.1904214830782,-62.8832966102955));
#11944=CARTESIAN_POINT('Ctrl Pts',(-25.396998382076,26.1913981598979,-62.8834024014528));
#11945=CARTESIAN_POINT('Ctrl Pts',(-25.3936113619773,26.1937637721693,-62.8836587427707));
#11946=CARTESIAN_POINT('Ctrl Pts',(-25.3916195611401,26.1951515692122,-62.8838092139799));
#11947=CARTESIAN_POINT('Ctrl Pts',(-25.3854650708664,26.1994294187365,-62.8842733144337));
#11948=CARTESIAN_POINT('Ctrl Pts',(-25.3812971056927,26.2023119223632,-62.884586426134));
#11949=CARTESIAN_POINT('Ctrl Pts',(-25.3340669038983,26.2348112204905,-62.8881213126561));
#11950=CARTESIAN_POINT('Ctrl Pts',(-25.2902940809684,26.2633882176537,-62.8912734879278));
#11951=CARTESIAN_POINT('Ctrl Pts',(-25.196313939655,26.3215322798282,-62.8978267114756));
#11952=CARTESIAN_POINT('Ctrl Pts',(-25.1459610853148,26.3508282862131,-62.9012138446932));
#11953=CARTESIAN_POINT('Ctrl Pts',(-24.7541040524248,26.5648140701814,-62.9268505478225));
#11954=CARTESIAN_POINT('Ctrl Pts',(-24.3825738590906,26.6877861475458,-62.9474804942564));
#11955=CARTESIAN_POINT('Ctrl Pts',(-23.9787156275817,26.7444533208138,-62.9721553109128));
#11956=CARTESIAN_POINT('Ctrl Pts',(-23.9593429708257,26.7469921664156,-62.9733429127609));
#11957=CARTESIAN_POINT('Ctrl Pts',(-23.9338444105501,26.7500982543653,-62.9749116467279));
#11958=CARTESIAN_POINT('Ctrl Pts',(-23.9277379868606,26.7508243725893,-62.9752877497374));
#11959=CARTESIAN_POINT('Ctrl Pts',(-23.9182910665249,26.7519202994187,-62.9758702614111));
#11960=CARTESIAN_POINT('Ctrl Pts',(-23.9149519837663,26.7523023700833,-62.9760762823862));
#11961=CARTESIAN_POINT('Ctrl Pts',(-23.9082887793482,26.753054241827,-62.9764876590106));
#11962=CARTESIAN_POINT('Ctrl Pts',(-23.9049646673983,26.7534240927746,-62.9766930128162));
#11963=CARTESIAN_POINT('Ctrl Pts',(-23.8976579043937,26.7542255523907,-62.9771446867289));
#11964=CARTESIAN_POINT('Ctrl Pts',(-23.8936750166733,26.754654910752,-62.9773910775577));
#11965=CARTESIAN_POINT('Ctrl Pts',(-23.8822530248263,26.7558646705007,-62.9780982052926));
#11966=CARTESIAN_POINT('Ctrl Pts',(-23.8748120271274,26.7566265966336,-62.9785595245487));
#11967=CARTESIAN_POINT('Ctrl Pts',(-23.8580818229134,26.7582808631508,-62.9795982385057));
#11968=CARTESIAN_POINT('Ctrl Pts',(-23.8487912866435,26.7591587716467,-62.9801760851831));
#11969=CARTESIAN_POINT('Ctrl Pts',(-23.7728664832735,26.7660007011019,-62.9849070135689));
#11970=CARTESIAN_POINT('Ctrl Pts',(-23.7060694212423,26.769928489853,-62.9891238419397));
#11971=CARTESIAN_POINT('Ctrl Pts',(-23.5170219692526,26.7751482996902,-63.0012239128181));
#11972=CARTESIAN_POINT('Ctrl Pts',(-23.3947615790465,26.7715680858433,-63.0092488539537));
#11973=CARTESIAN_POINT('Ctrl Pts',(-23.0554202310777,26.7422671312002,-63.0319944215086));
#11974=CARTESIAN_POINT('Ctrl Pts',(-22.8403137068418,26.7014108521678,-63.0469896945684));
#11975=CARTESIAN_POINT('Ctrl Pts',(-22.5978067973046,26.6292399916863,-63.0637641899935));
#11976=CARTESIAN_POINT('Ctrl Pts',(-22.5647776581904,26.6188281116729,-63.0660447134939));
#11977=CARTESIAN_POINT('Ctrl Pts',(-22.5269223294283,26.6062205658002,-63.0686490018587));
#11978=CARTESIAN_POINT('Ctrl Pts',(-22.521927032972,26.6045432836831,-63.0689924657047));
#11979=CARTESIAN_POINT('Ctrl Pts',(-22.5143130469968,26.6019659215525,-63.0695156687644));
#11980=CARTESIAN_POINT('Ctrl Pts',(-22.511691387665,26.6010747126819,-63.0696957617399));
#11981=CARTESIAN_POINT('Ctrl Pts',(-22.457650155535,26.5826261633041,-63.0734068620372));
#11982=CARTESIAN_POINT('Ctrl Pts',(-22.4066776556992,26.5637732594062,-63.076884487792));
#11983=CARTESIAN_POINT('Ctrl Pts',(-22.3513599449896,26.5417072466894,-63.0806148034183));
#11984=CARTESIAN_POINT('Ctrl Pts',(-22.3465218563873,26.5397637306284,-63.0809406848808));
#11985=CARTESIAN_POINT('Ctrl Pts',(-22.339351921695,26.5368632575939,-63.0814230581751));
#11986=CARTESIAN_POINT('Ctrl Pts',(-22.3370164778092,26.5359153045163,-63.0815800896108));
#11987=CARTESIAN_POINT('Ctrl Pts',(-22.3330230320878,26.5342889116653,-63.0818484440659));
#11988=CARTESIAN_POINT('Ctrl Pts',(-22.331364484321,26.5336118294842,-63.0819598495881));
#11989=CARTESIAN_POINT('Ctrl Pts',(-22.3281327203656,26.532289355876,-63.0821768364364));
#11990=CARTESIAN_POINT('Ctrl Pts',(-22.3265594547524,26.5316441040096,-63.0822824256055));
#11991=CARTESIAN_POINT('Ctrl Pts',(-22.3227605862293,26.5300825401395,-63.0825372829412));
#11992=CARTESIAN_POINT('Ctrl Pts',(-22.3205354929258,26.5291649775485,-63.082686474476));
#11993=CARTESIAN_POINT('Ctrl Pts',(-22.3137258320642,26.5263479451074,-63.0831428055026));
#11994=CARTESIAN_POINT('Ctrl Pts',(-22.3091445945163,26.5244403666656,-63.0834494522744));
#11995=CARTESIAN_POINT('Ctrl Pts',(-22.2615659988413,26.5045000720646,-63.0866306577157));
#11996=CARTESIAN_POINT('Ctrl Pts',(-22.2189576330256,26.4855456964201,-63.0894499294728));
#11997=CARTESIAN_POINT('Ctrl Pts',(-22.1425667982278,26.4495573079125,-63.0944767463532));
#11998=CARTESIAN_POINT('Ctrl Pts',(-22.108649264616,26.4328428484025,-63.0966984848586));
#11999=CARTESIAN_POINT('Ctrl Pts',(-22.0750360104957,26.415536772059,-63.0988976931332));
#12000=CARTESIAN_POINT('Ctrl Pts',(-22.0750360636209,26.415536799411,-63.3454515897691));
#12001=CARTESIAN_POINT('Ctrl Pts',(-22.1035139487319,26.4301988856706,-63.3433761302491));
#12002=CARTESIAN_POINT('Ctrl Pts',(-22.1322130926595,26.4444377881483,-63.3412872344756));
#12003=CARTESIAN_POINT('Ctrl Pts',(-22.3859690724233,26.5656551589085,-63.3228442277982));
#12004=CARTESIAN_POINT('Ctrl Pts',(-22.6225025957412,26.6466157135218,-63.3057439062922));
#12005=CARTESIAN_POINT('Ctrl Pts',(-22.978130535227,26.7238894805538,-63.2813865433741));
#12006=CARTESIAN_POINT('Ctrl Pts',(-23.0915422963139,26.7422559987677,-63.2738263129914));
#12007=CARTESIAN_POINT('Ctrl Pts',(-23.2202814139249,26.7560989991967,-63.2656450607918));
#12008=CARTESIAN_POINT('Ctrl Pts',(-23.2348693926878,26.7575669857108,-63.264723802468));
#12009=CARTESIAN_POINT('Ctrl Pts',(-23.2531043774595,26.7592763524494,-63.2635798902177));
#12010=CARTESIAN_POINT('Ctrl Pts',(-23.256742144084,26.7596111218832,-63.2633520673186));
#12011=CARTESIAN_POINT('Ctrl Pts',(-23.2625015076198,26.7601312593157,-63.2629919856033));
#12012=CARTESIAN_POINT('Ctrl Pts',(-23.2646227184901,26.7603207097498,-63.2628594962701));
#12013=CARTESIAN_POINT('Ctrl Pts',(-23.2686059991718,26.760672486597,-63.2626109514942));
#12014=CARTESIAN_POINT('Ctrl Pts',(-23.270468009301,26.760835294554,-63.262494869667));
#12015=CARTESIAN_POINT('Ctrl Pts',(-23.2746721811723,26.7611992081428,-63.2622330016139));
#12016=CARTESIAN_POINT('Ctrl Pts',(-23.2770144173696,26.761399370686,-63.2620872696178));
#12017=CARTESIAN_POINT('Ctrl Pts',(-23.2830123156982,26.7619053284252,-63.2617144913091));
#12018=CARTESIAN_POINT('Ctrl Pts',(-23.2866682960382,26.762207445888,-63.2614876527409));
#12019=CARTESIAN_POINT('Ctrl Pts',(-23.3059908557881,26.7637709816636,-63.2602907694939));
#12020=CARTESIAN_POINT('Ctrl Pts',(-23.3216663453432,26.7649240504745,-63.2593267481727));
#12021=CARTESIAN_POINT('Ctrl Pts',(-23.6600138783291,26.7873250267285,-63.2386567153596));
#12022=CARTESIAN_POINT('Ctrl Pts',(-23.9841160071203,26.7600082673915,-63.2214197319263));
#12023=CARTESIAN_POINT('Ctrl Pts',(-24.4512899805282,26.6484517226613,-63.1941780772581));
#12024=CARTESIAN_POINT('Ctrl Pts',(-24.6009298841737,26.6009531100718,-63.1850888061931));
#12025=CARTESIAN_POINT('Ctrl Pts',(-24.7607399143834,26.5370690309539,-63.1746955149162));
#12026=CARTESIAN_POINT('Ctrl Pts',(-24.7749316783804,26.5312781067341,-63.173766549716));
#12027=CARTESIAN_POINT('Ctrl Pts',(-24.7961802523034,26.5224303205561,-63.1723664074307));
#12028=CARTESIAN_POINT('Ctrl Pts',(-24.8032684480307,26.5194490232362,-63.1718977865457));
#12029=CARTESIAN_POINT('Ctrl Pts',(-24.8146645151413,26.5146077592847,-63.1711418256016));
#12030=CARTESIAN_POINT('Ctrl Pts',(-24.8189791421654,26.5127636906172,-63.1708550268203));
#12031=CARTESIAN_POINT('Ctrl Pts',(-24.8272189873183,26.5092206841843,-63.1703061839863));
#12032=CARTESIAN_POINT('Ctrl Pts',(-24.8311448835312,26.5075233408975,-63.1700441947972));
#12033=CARTESIAN_POINT('Ctrl Pts',(-24.8381037037438,26.5044982700589,-63.1695789302769));
#12034=CARTESIAN_POINT('Ctrl Pts',(-24.8411379883901,26.5031736721166,-63.1693757623662));
#12035=CARTESIAN_POINT('Ctrl Pts',(-24.8471181423081,26.5005520945917,-63.168974758992));
#12036=CARTESIAN_POINT('Ctrl Pts',(-24.8500641210113,26.4992553724823,-63.1687769325387));
#12037=CARTESIAN_POINT('Ctrl Pts',(-24.8571478756867,26.496124661828,-63.1683005678536));
#12038=CARTESIAN_POINT('Ctrl Pts',(-24.861283732456,26.4942863693993,-63.168021881915));
#12039=CARTESIAN_POINT('Ctrl Pts',(-24.873952466886,26.4886234208464,-63.1671664992016));
#12040=CARTESIAN_POINT('Ctrl Pts',(-24.8824725253425,26.4847703602664,-63.1665888251262));
#12041=CARTESIAN_POINT('Ctrl Pts',(-24.9808813222323,26.4397496491777,-63.1598883800592));
#12042=CARTESIAN_POINT('Ctrl Pts',(-25.0688376918065,26.3945077905284,-63.1536244795885));
#12043=CARTESIAN_POINT('Ctrl Pts',(-25.1863239032119,26.3270724095538,-63.1448589268642));
#12044=CARTESIAN_POINT('Ctrl Pts',(-25.2177650500524,26.3083061951901,-63.1424724823351));
#12045=CARTESIAN_POINT('Ctrl Pts',(-25.3222928713269,26.2434761510015,-63.1344026282554));
#12046=CARTESIAN_POINT('Ctrl Pts',(-25.393842241216,26.195012596739,-63.1286498909912));
#12047=CARTESIAN_POINT('Ctrl Pts',(-25.5163415004817,26.1046501216796,-63.1184220055215));
#12048=CARTESIAN_POINT('Ctrl Pts',(-25.5681170393693,26.0639500881644,-63.1139709549432));
#12049=CARTESIAN_POINT('Ctrl Pts',(-25.7273133536302,25.9307182357265,-63.0999203799137));
#12050=CARTESIAN_POINT('Ctrl Pts',(-25.8299029366639,25.8326654897099,-63.0903097588793));
#12051=CARTESIAN_POINT('Ctrl Pts',(-25.9746713442664,25.6747667368957,-63.0762088016034));
#12052=CARTESIAN_POINT('Ctrl Pts',(-26.0218252535001,25.6197204224106,-63.0715177587804));
#12053=CARTESIAN_POINT('Ctrl Pts',(-26.0741989217383,25.5542340277822,-63.0662350712626));
#12054=CARTESIAN_POINT('Ctrl Pts',(-26.0812637262964,25.5453037988384,-63.0655208768525));
#12055=CARTESIAN_POINT('Ctrl Pts',(-26.0903410872506,25.5337037826833,-63.0646013529052));
#12056=CARTESIAN_POINT('Ctrl Pts',(-26.0923969125697,25.5310681925127,-63.0643929748548));
#12057=CARTESIAN_POINT('Ctrl Pts',(-26.0957131903058,25.5268030223526,-63.064056640423));
#12058=CARTESIAN_POINT('Ctrl Pts',(-26.0969761802651,25.5251754326016,-63.063928502486));
#12059=CARTESIAN_POINT('Ctrl Pts',(-26.0993909705785,25.5220573724472,-63.0636834203105));
#12060=CARTESIAN_POINT('Ctrl Pts',(-26.1005430212296,25.5205671080027,-63.0635664583828));
#12061=CARTESIAN_POINT('Ctrl Pts',(-26.1031796952898,25.5171501843355,-63.0632986815936));
#12062=CARTESIAN_POINT('Ctrl Pts',(-26.1046634478468,25.5152228495679,-63.0631479292423));
#12063=CARTESIAN_POINT('Ctrl Pts',(-26.1085948985283,25.5101040753022,-63.0627483084962));
#12064=CARTESIAN_POINT('Ctrl Pts',(-26.1110388165535,25.5069097174612,-63.0624997083793));
#12065=CARTESIAN_POINT('Ctrl Pts',(-26.122589290469,25.4917537985796,-63.0613238588694));
#12066=CARTESIAN_POINT('Ctrl Pts',(-26.1316182480043,25.4797329356285,-63.0604020040766));
#12067=CARTESIAN_POINT('Ctrl Pts',(-26.3203626568914,25.2247483227428,-63.0410634350453));
#12068=CARTESIAN_POINT('Ctrl Pts',(-26.4651372110138,24.9577196598887,-63.0248169297578));
#12069=CARTESIAN_POINT('Ctrl Pts',(-26.6386900582848,24.4914150159533,-62.9967477022875));
#12070=CARTESIAN_POINT('Ctrl Pts',(-26.6900121573599,24.3026652985737,-62.9854767671159));
#12071=CARTESIAN_POINT('Ctrl Pts',(-26.7256675859307,24.1006664605714,-62.9729875210343));
#12072=CARTESIAN_POINT('Ctrl Pts',(-26.7273492221113,24.0908752060603,-62.9723812038139));
#12073=CARTESIAN_POINT('Ctrl Pts',(-26.7297301665049,24.0766173952489,-62.9714968798542));
#12074=CARTESIAN_POINT('Ctrl Pts',(-26.7304654025858,24.0721568287941,-62.971220016844));
#12075=CARTESIAN_POINT('Ctrl Pts',(-26.7317364112952,24.0643433943958,-62.9707346862915));
#12076=CARTESIAN_POINT('Ctrl Pts',(-26.7322762764907,24.0609911915612,-62.9705263492244));
#12077=CARTESIAN_POINT('Ctrl Pts',(-26.7333121587167,24.0544936570366,-62.970122306027));
#12078=CARTESIAN_POINT('Ctrl Pts',(-26.7338088139923,24.0513484296874,-62.9699266204353));
#12079=CARTESIAN_POINT('Ctrl Pts',(-26.7349801277713,24.043858681727,-62.969460386801));
#12080=CARTESIAN_POINT('Ctrl Pts',(-26.7356505575562,24.0395135143022,-62.969189704688));
#12081=CARTESIAN_POINT('Ctrl Pts',(-26.7380000627026,24.0240764346929,-62.9682273427169));
#12082=CARTESIAN_POINT('Ctrl Pts',(-26.7396300965444,24.0129772405787,-62.9675341081391));
#12083=CARTESIAN_POINT('Ctrl Pts',(-26.762498491901,23.8513981996924,-62.9574227261462));
#12084=CARTESIAN_POINT('Ctrl Pts',(-26.7731218037237,23.6996320371111,-62.9476659204347));
#12085=CARTESIAN_POINT('Ctrl Pts',(-26.7728665898019,23.3772651636872,-62.9263872116026));
#12086=CARTESIAN_POINT('Ctrl Pts',(-26.759211452541,23.2071191544008,-62.9148246348769));
#12087=CARTESIAN_POINT('Ctrl Pts',(-26.7039187291296,22.8630800974918,-62.8912611082392));
#12088=CARTESIAN_POINT('Ctrl Pts',(-26.6611445797017,22.689913216979,-62.879306223084));
#12089=CARTESIAN_POINT('Ctrl Pts',(-26.6006844667297,22.5104885636931,-62.8673772125349));
#12090=CARTESIAN_POINT('Ctrl Pts',(-26.5970365743858,22.4998473215232,-62.8666715567893));
#12091=CARTESIAN_POINT('Ctrl Pts',(-26.5921909229873,22.4859497462818,-62.8657525578943));
#12092=CARTESIAN_POINT('Ctrl Pts',(-26.5910435761106,22.4826761082344,-62.865536272407));
#12093=CARTESIAN_POINT('Ctrl Pts',(-26.5892662855374,22.4776312096369,-62.8652032603495));
#12094=CARTESIAN_POINT('Ctrl Pts',(-26.5886400783641,22.4758586500735,-62.8650863111906));
#12095=CARTESIAN_POINT('Ctrl Pts',(-26.5874516223016,22.4725039219197,-62.8648650835445));
#12096=CARTESIAN_POINT('Ctrl Pts',(-26.5868896907671,22.470921652852,-62.8647607869308));
#12097=CARTESIAN_POINT('Ctrl Pts',(-26.5855809357767,22.46724561416,-62.8645185846458));
#12098=CARTESIAN_POINT('Ctrl Pts',(-26.5848331836357,22.4651521810395,-62.8643807355553));
#12099=CARTESIAN_POINT('Ctrl Pts',(-26.5827078419135,22.4592213785626,-62.8639904256466));
#12100=CARTESIAN_POINT('Ctrl Pts',(-26.581325129184,22.4553858298703,-62.8637382711967));
#12101=CARTESIAN_POINT('Ctrl Pts',(-26.5728640511415,22.4320542659334,-62.8622059784853));
#12102=CARTESIAN_POINT('Ctrl Pts',(-26.565604678674,22.4126237511553,-62.8609365124723));
#12103=CARTESIAN_POINT('Ctrl Pts',(-26.5432795348477,22.3545834813715,-62.8571606157347));
#12104=CARTESIAN_POINT('Ctrl Pts',(-26.527655552367,22.3161914603863,-62.8546844516276));
#12105=CARTESIAN_POINT('Ctrl Pts',(-26.4803758370018,22.2061431182659,-62.8476197956409));
#12106=CARTESIAN_POINT('Ctrl Pts',(-26.4468416806164,22.135323001619,-62.8431143964127));
#12107=CARTESIAN_POINT('Ctrl Pts',(-26.2456394413674,21.7476132820124,-62.818311408195));
#12108=CARTESIAN_POINT('Ctrl Pts',(-26.0286163946755,21.4592391607728,-62.7990023840234));
#12109=CARTESIAN_POINT('Ctrl Pts',(-25.753720002155,21.198387695362,-62.7760860337717));
#12110=CARTESIAN_POINT('Ctrl Pts',(-25.7387281911664,21.1844310338759,-62.7748414463933));
#12111=CARTESIAN_POINT('Ctrl Pts',(-25.7189785277042,21.166393398115,-62.7732081498128));
#12112=CARTESIAN_POINT('Ctrl Pts',(-25.7143401479284,21.162181845365,-62.772825002185));
#12113=CARTESIAN_POINT('Ctrl Pts',(-25.7071773423082,21.1557161720927,-62.7722339999794));
#12114=CARTESIAN_POINT('Ctrl Pts',(-25.7046615791716,21.1534524415522,-62.7720265517588));
#12115=CARTESIAN_POINT('Ctrl Pts',(-25.69965371839,21.1489605301881,-62.7716138564955));
#12116=CARTESIAN_POINT('Ctrl Pts',(-25.6971617101518,21.1467322556852,-62.7714086137748));
#12117=CARTESIAN_POINT('Ctrl Pts',(-25.6916428910609,21.1418129342232,-62.7709543495192));
#12118=CARTESIAN_POINT('Ctrl Pts',(-25.6886144688717,21.1391237107379,-62.7707052519067));
#12119=CARTESIAN_POINT('Ctrl Pts',(-25.6799009155616,21.1314154484729,-62.7699890367332));
#12120=CARTESIAN_POINT('Ctrl Pts',(-25.6742031556735,21.1264107836837,-62.7695213192328));
#12121=CARTESIAN_POINT('Ctrl Pts',(-25.6366426904858,21.0936534368531,-62.7664419905889));
#12122=CARTESIAN_POINT('Ctrl Pts',(-25.6042557294637,21.0665106777939,-62.7638052448538));
#12123=CARTESIAN_POINT('Ctrl Pts',(-25.5070811281415,20.988271546001,-62.7559428242576));
#12124=CARTESIAN_POINT('Ctrl Pts',(-25.440858426241,20.9390206144685,-62.7506460023929));
#12125=CARTESIAN_POINT('Ctrl Pts',(-25.1274617479128,20.7241174857947,-62.7258510622817));
#12126=CARTESIAN_POINT('Ctrl Pts',(-24.8600335440666,20.5906817066048,-62.7052668859013));
#12127=CARTESIAN_POINT('Ctrl Pts',(-24.4921523738601,20.4668823243921,-62.6795854942009));
#12128=CARTESIAN_POINT('Ctrl Pts',(-24.4049799495618,20.4415885434462,-62.673693876368));
#12129=CARTESIAN_POINT('Ctrl Pts',(-24.3106069928732,20.4184766880527,-62.6676027216059));
#12130=CARTESIAN_POINT('Ctrl Pts',(-24.3043619161782,20.4169670548556,-62.6672009766631));
#12131=CARTESIAN_POINT('Ctrl Pts',(-24.2957002693518,20.4149006563931,-62.6666456615151));
#12132=CARTESIAN_POINT('Ctrl Pts',(-24.2932875623938,20.4143280021834,-62.6664911808533));
#12133=CARTESIAN_POINT('Ctrl Pts',(-24.2891413037268,20.4133489444949,-62.6662260554862));
#12134=CARTESIAN_POINT('Ctrl Pts',(-24.2874080766188,20.4129411930729,-62.6661153325817));
#12135=CARTESIAN_POINT('Ctrl Pts',(-24.2838657343958,20.4121109347121,-62.6658892552871));
#12136=CARTESIAN_POINT('Ctrl Pts',(-24.2820565955017,20.4116885565464,-62.6657739089666));
#12137=CARTESIAN_POINT('Ctrl Pts',(-24.2778348910523,20.4107067673773,-62.6655050108711));
#12138=CARTESIAN_POINT('Ctrl Pts',(-24.2754220380741,20.4101485711533,-62.6653515298092));
#12139=CARTESIAN_POINT('Ctrl Pts',(-24.2703278076814,20.4089762423035,-62.6650279120954));
#12140=CARTESIAN_POINT('Ctrl Pts',(-24.2676462804431,20.4083627597949,-62.6648578129903));
#12141=CARTESIAN_POINT('Ctrl Pts',(-24.2604558988529,20.4067274222674,-62.6644023585206));
#12142=CARTESIAN_POINT('Ctrl Pts',(-24.2559456047233,20.4057118301575,-62.6641173595603));
#12143=CARTESIAN_POINT('Ctrl Pts',(-24.1492673494408,20.3819319501476,-62.6573925518916));
#12144=CARTESIAN_POINT('Ctrl Pts',(-24.0460400965875,20.3641461322928,-62.6512323276985));
#12145=CARTESIAN_POINT('Ctrl Pts',(-23.5531680738928,20.3037679866669,-62.6226773451752));
#12146=CARTESIAN_POINT('Ctrl Pts',(-23.1588064848565,20.3274461106527,-62.6018891165103));
#12147=CARTESIAN_POINT('Ctrl Pts',(-22.7595624291082,20.4259447048717,-62.5770051247287));
#12148=CARTESIAN_POINT('Ctrl Pts',(-22.740861936758,20.4307370124734,-62.5758316187693));
#12149=CARTESIAN_POINT('Ctrl Pts',(-22.7162909932846,20.4372695290888,-62.5742788770824));
#12150=CARTESIAN_POINT('Ctrl Pts',(-22.7103805715818,20.438858935272,-62.5739045428731));
#12151=CARTESIAN_POINT('Ctrl Pts',(-22.7012372042796,20.4413456830883,-62.5733241537432));
#12152=CARTESIAN_POINT('Ctrl Pts',(-22.6980010499557,20.4422312590462,-62.573118481869));
#12153=CARTESIAN_POINT('Ctrl Pts',(-22.6915408931245,20.4440099339358,-62.5727074043582));
#12154=CARTESIAN_POINT('Ctrl Pts',(-22.6883168865168,20.4449030026101,-62.572501999925));
#12155=CARTESIAN_POINT('Ctrl Pts',(-22.6811460946831,20.4469013813235,-62.5720445784659));
#12156=CARTESIAN_POINT('Ctrl Pts',(-22.6772000206982,20.4480092023989,-62.5717924798311));
#12157=CARTESIAN_POINT('Ctrl Pts',(-22.6657389075246,20.4512503957857,-62.5710591637199));
#12158=CARTESIAN_POINT('Ctrl Pts',(-22.6582295379145,20.4534035578899,-62.5705773007595));
#12159=CARTESIAN_POINT('Ctrl Pts',(-22.6054329425058,20.4687498948358,-62.5671795399704));
#12160=CARTESIAN_POINT('Ctrl Pts',(-22.5604343489799,20.4829080546418,-62.5642321746569));
#12161=CARTESIAN_POINT('Ctrl Pts',(-22.4203578632667,20.5303843775104,-62.5548884429675));
#12162=CARTESIAN_POINT('Ctrl Pts',(-22.3265289877297,20.567173108523,-62.5483800466649));
#12163=CARTESIAN_POINT('Ctrl Pts',(-22.0833076741205,20.6759436238406,-62.5308488114397));
#12164=CARTESIAN_POINT('Ctrl Pts',(-21.937485711875,20.7551579582102,-62.5196368618988));
#12165=CARTESIAN_POINT('Ctrl Pts',(-21.6377126842389,20.9492978854477,-62.4954659659575));
#12166=CARTESIAN_POINT('Ctrl Pts',(-21.4865842941244,21.0674988789648,-62.4825520171268));
#12167=CARTESIAN_POINT('Ctrl Pts',(-21.3380995147647,21.2066143843359,-62.4697238008891));
#12168=CARTESIAN_POINT('Ctrl Pts',(-21.329413080806,21.2148440277814,-62.4689728702153));
#12169=CARTESIAN_POINT('Ctrl Pts',(-21.3182063534283,21.2255805010668,-62.4680036877972));
#12170=CARTESIAN_POINT('Ctrl Pts',(-21.3156442373354,21.2280432467748,-62.4677820846919));
#12171=CARTESIAN_POINT('Ctrl Pts',(-21.3117206938662,21.2318271237327,-62.4674426968128));
#12172=CARTESIAN_POINT('Ctrl Pts',(-21.3103563611794,21.2331452172593,-62.4673246756239));
#12173=CARTESIAN_POINT('Ctrl Pts',(-21.3076815727431,21.2357339233669,-62.467093283669));
#12174=CARTESIAN_POINT('Ctrl Pts',(-21.3063710394377,21.2370044380026,-62.4669799067896));
#12175=CARTESIAN_POINT('Ctrl Pts',(-21.3034724343946,21.2398193117493,-62.4667291319475));
#12176=CARTESIAN_POINT('Ctrl Pts',(-21.3018848791402,21.2413641912875,-62.4665917761338));
#12177=CARTESIAN_POINT('Ctrl Pts',(-21.2985906646526,21.2445764720802,-62.4663067410332));
#12178=CARTESIAN_POINT('Ctrl Pts',(-21.2968842608815,21.2462441351061,-62.4661590824181));
#12179=CARTESIAN_POINT('Ctrl Pts',(-21.2925027960438,21.250535650393,-62.4657799135583));
#12180=CARTESIAN_POINT('Ctrl Pts',(-21.2898304468607,21.2531622849469,-62.465548619879));
#12181=CARTESIAN_POINT('Ctrl Pts',(-21.2820798459959,21.2608069221761,-62.4648776892639));
#12182=CARTESIAN_POINT('Ctrl Pts',(-21.2770136399607,21.2658371853876,-62.4644389946543));
#12183=CARTESIAN_POINT('Ctrl Pts',(-21.225252969352,21.3175733346556,-62.4599549544061));
#12184=CARTESIAN_POINT('Ctrl Pts',(-21.1799841410761,21.3656911221856,-62.4560168016529));
#12185=CARTESIAN_POINT('Ctrl Pts',(-21.1073131894992,21.4478564954779,-62.4495980669304));
#12186=CARTESIAN_POINT('Ctrl Pts',(-21.0790695146452,21.4811279588523,-62.4470771215526));
#12187=CARTESIAN_POINT('Ctrl Pts',(-20.8888330353287,21.7146831006293,-62.4298317892197));
#12188=CARTESIAN_POINT('Ctrl Pts',(-20.7506852694502,21.9331861954486,-62.4158578580381));
#12189=CARTESIAN_POINT('Ctrl Pts',(-20.62290290992,22.2017980281518,-62.398784580381));
#12190=CARTESIAN_POINT('Ctrl Pts',(-20.6064545648679,22.2380944901982,-62.3964816131576));
#12191=CARTESIAN_POINT('Ctrl Pts',(-20.5527229282712,22.362762572066,-62.3885696984649));
#12192=CARTESIAN_POINT('Ctrl Pts',(-20.5187159551936,22.4524823688718,-62.3828707710595));
#12193=CARTESIAN_POINT('Ctrl Pts',(-20.4855833666699,22.5532450029337,-62.3764141911182));
#12194=CARTESIAN_POINT('Ctrl Pts',(-20.4824507232505,22.5629262614915,-62.3757933044682));
#12195=CARTESIAN_POINT('Ctrl Pts',(-20.4780965779661,22.5766033059459,-62.3749153439588));
#12196=CARTESIAN_POINT('Ctrl Pts',(-20.4768368943547,22.5805869508278,-62.3746595278012));
#12197=CARTESIAN_POINT('Ctrl Pts',(-20.4746475289468,22.587557763318,-62.3742117121664));
#12198=CARTESIAN_POINT('Ctrl Pts',(-20.4737144414339,22.5905438628492,-62.3740198249163));
#12199=CARTESIAN_POINT('Ctrl Pts',(-20.4717655999712,22.596812663837,-62.3736168719164));
#12200=CARTESIAN_POINT('Ctrl Pts',(-20.4707507458951,22.6000956385834,-62.3734057769158));
#12201=CARTESIAN_POINT('Ctrl Pts',(-20.4683438675013,22.6079260674626,-62.372902115283));
#12202=CARTESIAN_POINT('Ctrl Pts',(-20.4669566575854,22.6124749824137,-62.372609391081));
#12203=CARTESIAN_POINT('Ctrl Pts',(-20.4623231982198,22.6277903649141,-62.371623382792));
#12204=CARTESIAN_POINT('Ctrl Pts',(-20.4591232605465,22.6385706564883,-62.3709285834063));
#12205=CARTESIAN_POINT('Ctrl Pts',(-20.4517050611124,22.6640499659495,-62.3692845333739));
#12206=CARTESIAN_POINT('Ctrl Pts',(-20.4475349009567,22.678762597222,-62.3683337259384));
#12207=CARTESIAN_POINT('Ctrl Pts',(-20.4019687158948,22.8439969248488,-62.357637976271));
#12208=CARTESIAN_POINT('Ctrl Pts',(-20.3714635190606,22.9972828950226,-62.3475381313239));
#12209=CARTESIAN_POINT('Ctrl Pts',(-20.3145754926392,23.4542873862186,-62.3169605771201));
#12210=CARTESIAN_POINT('Ctrl Pts',(-20.3199697832875,23.7601993605823,-62.2957649898941));
#12211=CARTESIAN_POINT('Ctrl Pts',(-20.3735452612076,24.094115562082,-62.2740722363186));
#12212=CARTESIAN_POINT('Ctrl Pts',(-20.3794138030826,24.1273470298568,-62.2719317116986));
#12213=CARTESIAN_POINT('Ctrl Pts',(-20.3867635442163,24.1654603800735,-62.2695026387098));
#12214=CARTESIAN_POINT('Ctrl Pts',(-20.387735366568,24.170436739588,-62.2691859912817));
#12215=CARTESIAN_POINT('Ctrl Pts',(-20.3891849250557,24.1777674075226,-62.268720311754));
#12216=CARTESIAN_POINT('Ctrl Pts',(-20.3896535496831,24.1801234773057,-62.2685707606277));
#12217=CARTESIAN_POINT('Ctrl Pts',(-20.3904851010615,24.1842799126488,-62.2683071422649));
#12218=CARTESIAN_POINT('Ctrl Pts',(-20.3908469324937,24.1860804921485,-62.2681930119205));
#12219=CARTESIAN_POINT('Ctrl Pts',(-20.3916101862663,24.1898619289431,-62.2679534719484));
#12220=CARTESIAN_POINT('Ctrl Pts',(-20.3920119319689,24.1918427137264,-62.2678280814847));
#12221=CARTESIAN_POINT('Ctrl Pts',(-20.3930629121485,24.1969996057856,-62.2675018505547));
#12222=CARTESIAN_POINT('Ctrl Pts',(-20.3937150780703,24.2001751237792,-62.2673011790571));
#12223=CARTESIAN_POINT('Ctrl Pts',(-20.3951500869177,24.2071093394906,-62.2668634430012));
#12224=CARTESIAN_POINT('Ctrl Pts',(-20.395934858629,24.2108676395523,-62.2666264883575));
#12225=CARTESIAN_POINT('Ctrl Pts',(-20.3982482684929,24.2218485333336,-62.2659350011615));
#12226=CARTESIAN_POINT('Ctrl Pts',(-20.3997950230051,24.2290673467031,-62.2654814822521));
#12227=CARTESIAN_POINT('Ctrl Pts',(-20.4051890310656,24.2538259687478,-62.2639294849665));
#12228=CARTESIAN_POINT('Ctrl Pts',(-20.4091581444798,24.2713392727152,-62.2628376167247));
#12229=CARTESIAN_POINT('Ctrl Pts',(-20.4258643510753,24.3422970350845,-62.2584345878878));
#12230=CARTESIAN_POINT('Ctrl Pts',(-20.4398214303909,24.3954478476165,-62.2551846048492));
#12231=CARTESIAN_POINT('Ctrl Pts',(-20.4776536665992,24.525848425691,-62.2472723473582));
#12232=CARTESIAN_POINT('Ctrl Pts',(-20.5030896406238,24.6026074511085,-62.2426685708219));
#12233=CARTESIAN_POINT('Ctrl Pts',(-20.6079656375818,24.8832671449607,-62.2257718633631));
#12234=CARTESIAN_POINT('Ctrl Pts',(-20.7052102531172,25.0798649597946,-62.2137677123514));
#12235=CARTESIAN_POINT('Ctrl Pts',(-20.8496149533322,25.3096393451987,-62.1981586879506));
#12236=CARTESIAN_POINT('Ctrl Pts',(-20.8786940365292,25.3534885415055,-62.1951043679517));
#12237=CARTESIAN_POINT('Ctrl Pts',(-20.913766832805,25.4036642251259,-62.1915083867524));
#12238=CARTESIAN_POINT('Ctrl Pts',(-20.9187295560934,25.4107037062092,-62.1910015216658));
#12239=CARTESIAN_POINT('Ctrl Pts',(-20.9642648937927,25.4747475659943,-62.186368210173));
#12240=CARTESIAN_POINT('Ctrl Pts',(-21.0066530898595,25.5304328140481,-62.1821797817258));
#12241=CARTESIAN_POINT('Ctrl Pts',(-21.0568005760059,25.59204212293,-62.1773414108091));
#12242=CARTESIAN_POINT('Ctrl Pts',(-21.0628159796526,25.5993661905116,-62.1767628502344));
#12243=CARTESIAN_POINT('Ctrl Pts',(-21.071662583856,25.6100410341644,-62.1759145927527));
#12244=CARTESIAN_POINT('Ctrl Pts',(-21.0744684963369,25.6134127810209,-62.1756459274161));
#12245=CARTESIAN_POINT('Ctrl Pts',(-21.0794526500611,25.6193772196267,-62.175169362533));
#12246=CARTESIAN_POINT('Ctrl Pts',(-21.0816281145247,25.6219722318721,-62.1749615768943));
#12247=CARTESIAN_POINT('Ctrl Pts',(-21.0861538267782,25.6273534974236,-62.1745297723094));
#12248=CARTESIAN_POINT('Ctrl Pts',(-21.0885047187776,25.6301392004407,-62.1743057270604));
#12249=CARTESIAN_POINT('Ctrl Pts',(-21.0945761019469,25.6373088068375,-62.1737277670591));
#12250=CARTESIAN_POINT('Ctrl Pts',(-21.0983035966248,25.6416867387296,-62.1733735638283));
#12251=CARTESIAN_POINT('Ctrl Pts',(-21.1138835344393,25.659886432085,-62.1718956915996));
#12252=CARTESIAN_POINT('Ctrl Pts',(-21.1258411064956,25.6736173858656,-62.1707676704235));
#12253=CARTESIAN_POINT('Ctrl Pts',(-21.3403937089623,25.915814408338,-62.1506348921258));
#12254=CARTESIAN_POINT('Ctrl Pts',(-21.5742867367526,26.1143953877523,-62.1301401747579));
#12255=CARTESIAN_POINT('Ctrl Pts',(-21.911347402691,26.3267224712512,-62.1031866758546));
#12256=CARTESIAN_POINT('Ctrl Pts',(-21.9922607439807,26.3729192105752,-62.096902306304));
#12257=CARTESIAN_POINT('Ctrl Pts',(-22.0750361387181,26.4155368380754,-62.0907209741597));
#12258=CARTESIAN_POINT('Origin',(-23.5502525316942,23.5502525316942,-77.3107734492734));
#12259=CARTESIAN_POINT('',(-22.0750360153461,26.4155367745563,-60.593221446491));
#12260=CARTESIAN_POINT('',(-22.0750360359093,26.4155367851434,-60.8417499040898));
#12261=CARTESIAN_POINT('',(-22.0750360153461,26.4155367745563,-77.3107734492734));
#12262=CARTESIAN_POINT('',(-26.7730010715128,23.5532478318311,-61.4389926964188));
#12263=CARTESIAN_POINT('Ctrl Pts',(-22.0750360153461,26.4155367745563,-60.593221446491));
#12264=CARTESIAN_POINT('Ctrl Pts',(-22.0629295894779,26.4093036758893,-60.5940645766529));
#12265=CARTESIAN_POINT('Ctrl Pts',(-22.0508629408241,26.4029939895318,-60.5949104149417));
#12266=CARTESIAN_POINT('Ctrl Pts',(-21.9245463063757,26.3359198149904,-60.6038232154706));
#12267=CARTESIAN_POINT('Ctrl Pts',(-21.8140296098913,26.2684109826019,-60.6121320731002));
#12268=CARTESIAN_POINT('Ctrl Pts',(-21.5224687497516,26.0652629397668,-60.6355076782888));
#12269=CARTESIAN_POINT('Ctrl Pts',(-21.3511692352329,25.9169379138015,-60.650966190823));
#12270=CARTESIAN_POINT('Ctrl Pts',(-21.1031706140023,25.6518461502569,-60.6753493770457));
#12271=CARTESIAN_POINT('Ctrl Pts',(-21.0159966639256,25.5458634344544,-60.6844124721604));
#12272=CARTESIAN_POINT('Ctrl Pts',(-20.9311370733983,25.4281279704951,-60.6935268065851));
#12273=CARTESIAN_POINT('Ctrl Pts',(-20.926469584239,25.4216009747837,-60.6940291278711));
#12274=CARTESIAN_POINT('Ctrl Pts',(-20.9202517003813,25.4128369180658,-60.6946995890625));
#12275=CARTESIAN_POINT('Ctrl Pts',(-20.9186797436697,25.4106153002215,-60.6948692007127));
#12276=CARTESIAN_POINT('Ctrl Pts',(-20.9160456183733,25.4068825196206,-60.6951536014764));
#12277=CARTESIAN_POINT('Ctrl Pts',(-20.9149819351257,25.4053724354086,-60.695268495286));
#12278=CARTESIAN_POINT('Ctrl Pts',(-20.9129511920751,25.4024841697756,-60.6954879409646));
#12279=CARTESIAN_POINT('Ctrl Pts',(-20.9119839199713,25.4011061535354,-60.6955925071926));
#12280=CARTESIAN_POINT('Ctrl Pts',(-20.9097101404225,25.3978614280526,-60.6958384099497));
#12281=CARTESIAN_POINT('Ctrl Pts',(-20.9084045341484,25.3959940932206,-60.6959796837129));
#12282=CARTESIAN_POINT('Ctrl Pts',(-20.9046694319182,25.3906399053715,-60.6963840657479));
#12283=CARTESIAN_POINT('Ctrl Pts',(-20.9022448394864,25.3871496125106,-60.696646836774));
#12284=CARTESIAN_POINT('Ctrl Pts',(-20.886875711018,25.3649315017008,-60.6983143057626));
#12285=CARTESIAN_POINT('Ctrl Pts',(-20.8741225976182,25.3460711470696,-60.6997061124847));
#12286=CARTESIAN_POINT('Ctrl Pts',(-20.8354468811579,25.2875472190912,-60.7039577552958));
#12287=CARTESIAN_POINT('Ctrl Pts',(-20.8101971841859,25.2474442585395,-60.7067774464783));
#12288=CARTESIAN_POINT('Ctrl Pts',(-20.745982161243,25.1402833233576,-60.7141085625629));
#12289=CARTESIAN_POINT('Ctrl Pts',(-20.7085357391707,25.0723488908379,-60.7185524641844));
#12290=CARTESIAN_POINT('Ctrl Pts',(-20.5831671367227,24.8241200496182,-60.7343043373909));
#12291=CARTESIAN_POINT('Ctrl Pts',(-20.5096652381694,24.6370670185044,-60.7453120516262));
#12292=CARTESIAN_POINT('Ctrl Pts',(-20.4335546049344,24.3735111861286,-60.760915465919));
#12293=CARTESIAN_POINT('Ctrl Pts',(-20.4155261811194,24.3019509660849,-60.7651574480202));
#12294=CARTESIAN_POINT('Ctrl Pts',(-20.3943309265492,24.2036983724629,-60.7710303546979));
#12295=CARTESIAN_POINT('Ctrl Pts',(-20.38901769181,24.1774900264102,-60.7726014940135));
#12296=CARTESIAN_POINT('Ctrl Pts',(-20.3831329153975,24.1464857997032,-60.7744668933887));
#12297=CARTESIAN_POINT('Ctrl Pts',(-20.3822451259872,24.1417505036741,-60.7747519820622));
#12298=CARTESIAN_POINT('Ctrl Pts',(-20.3806294730297,24.1330249405093,-60.7752776570649));
#12299=CARTESIAN_POINT('Ctrl Pts',(-20.3798985171012,24.1290352512332,-60.7755181529275));
#12300=CARTESIAN_POINT('Ctrl Pts',(-20.3781239373979,24.1192450439116,-60.776108641344));
#12301=CARTESIAN_POINT('Ctrl Pts',(-20.3770886923592,24.1134430374665,-60.7764588781737));
#12302=CARTESIAN_POINT('Ctrl Pts',(-20.3748745787056,24.1008341707082,-60.7772206705075));
#12303=CARTESIAN_POINT('Ctrl Pts',(-20.373701671383,24.0940263048094,-60.7776324005006));
#12304=CARTESIAN_POINT('Ctrl Pts',(-20.3708201829052,24.0769738738393,-60.7786647948808));
#12305=CARTESIAN_POINT('Ctrl Pts',(-20.3691392277362,24.0667247734084,-60.7792862813563));
#12306=CARTESIAN_POINT('Ctrl Pts',(-20.3658750062327,24.0462015218124,-60.780532844986));
#12307=CARTESIAN_POINT('Ctrl Pts',(-20.3642918500155,24.0359274810758,-60.7811579173184));
#12308=CARTESIAN_POINT('Ctrl Pts',(-20.3589085871458,23.9998329238091,-60.7833577236261));
#12309=CARTESIAN_POINT('Ctrl Pts',(-20.3553725256304,23.9739745942572,-60.7849405306397));
#12310=CARTESIAN_POINT('Ctrl Pts',(-20.3513127771927,23.9413383510584,-60.7869477280901));
#12311=CARTESIAN_POINT('Ctrl Pts',(-20.3504958663733,23.9345973673013,-60.7873628220553));
#12312=CARTESIAN_POINT('Ctrl Pts',(-20.3492412002901,23.9239628071937,-60.788018493201));
#12313=CARTESIAN_POINT('Ctrl Pts',(-20.3487892276922,23.9200709015794,-60.78825862069));
#12314=CARTESIAN_POINT('Ctrl Pts',(-20.3480028588396,23.91319004814,-60.7886834731396));
#12315=CARTESIAN_POINT('Ctrl Pts',(-20.3476655466704,23.9102014327875,-60.7888681057238));
#12316=CARTESIAN_POINT('Ctrl Pts',(-20.3469020267589,23.9033505406097,-60.7892915826724));
#12317=CARTESIAN_POINT('Ctrl Pts',(-20.3464786202626,23.8994879617272,-60.7895305152386));
#12318=CARTESIAN_POINT('Ctrl Pts',(-20.3453450091759,23.8889708829131,-60.7901815607649));
#12319=CARTESIAN_POINT('Ctrl Pts',(-20.3446485481271,23.8823149487245,-60.7905941069407));
#12320=CARTESIAN_POINT('Ctrl Pts',(-20.3411282000235,23.8476282001323,-60.7927468019594));
#12321=CARTESIAN_POINT('Ctrl Pts',(-20.3386513029664,23.819564118298,-60.7944978587341));
#12322=CARTESIAN_POINT('Ctrl Pts',(-20.3293711352232,23.6959265759748,-60.802255700593));
#12323=CARTESIAN_POINT('Ctrl Pts',(-20.3264646614019,23.6001180544829,-60.8083835997558));
#12324=CARTESIAN_POINT('Ctrl Pts',(-20.3307555862706,23.299021115464,-60.8280155815751));
#12325=CARTESIAN_POINT('Ctrl Pts',(-20.3532957588069,23.0944815410163,-60.8419331950849));
#12326=CARTESIAN_POINT('Ctrl Pts',(-20.4243873970138,22.7529464204359,-60.8655247859126));
#12327=CARTESIAN_POINT('Ctrl Pts',(-20.4630074539174,22.6144880307889,-60.8751785135582));
#12328=CARTESIAN_POINT('Ctrl Pts',(-20.51114708899,22.4778919603597,-60.8845255697523));
#12329=CARTESIAN_POINT('Ctrl Pts',(-20.5115581342842,22.4767277550888,-60.8846052207176));
#12330=CARTESIAN_POINT('Ctrl Pts',(-20.5129775313339,22.4727149379016,-60.8848797158078));
#12331=CARTESIAN_POINT('Ctrl Pts',(-20.5139892237836,22.4698674989269,-60.8850744098931));
#12332=CARTESIAN_POINT('Ctrl Pts',(-20.5280681914919,22.4304177870292,-60.8877705881564));
#12333=CARTESIAN_POINT('Ctrl Pts',(-20.541793271899,22.3940513115643,-60.8902417167156));
#12334=CARTESIAN_POINT('Ctrl Pts',(-20.558103281076,22.3530943847891,-60.8930012852786));
#12335=CARTESIAN_POINT('Ctrl Pts',(-20.5600447199996,22.3482533592871,-60.8933270848033));
#12336=CARTESIAN_POINT('Ctrl Pts',(-20.5629218554541,22.3411292622027,-60.8938059572501));
#12337=CARTESIAN_POINT('Ctrl Pts',(-20.5638484224314,22.3388425489439,-60.8939595793608));
#12338=CARTESIAN_POINT('Ctrl Pts',(-20.5654889849204,22.3348070576742,-60.8942305270103));
#12339=CARTESIAN_POINT('Ctrl Pts',(-20.5662018924274,22.3330578419129,-60.8943479189146));
#12340=CARTESIAN_POINT('Ctrl Pts',(-20.5676892680153,22.3294175237322,-60.894592114428));
#12341=CARTESIAN_POINT('Ctrl Pts',(-20.5684639954639,22.3275265346802,-60.8947189016522));
#12342=CARTESIAN_POINT('Ctrl Pts',(-20.5704825861371,22.3226127969967,-60.8950482007449));
#12343=CARTESIAN_POINT('Ctrl Pts',(-20.5717292543393,22.3195911919527,-60.8952505414041));
#12344=CARTESIAN_POINT('Ctrl Pts',(-20.5769812275217,22.3069164794498,-60.8960986678618));
#12345=CARTESIAN_POINT('Ctrl Pts',(-20.5810289376823,22.2972808468995,-60.8967418970492));
#12346=CARTESIAN_POINT('Ctrl Pts',(-20.6403727627809,22.1579145993769,-60.9060253789512));
#12347=CARTESIAN_POINT('Ctrl Pts',(-20.7040871932893,22.0319116088658,-60.9141700836784));
#12348=CARTESIAN_POINT('Ctrl Pts',(-20.8559633228212,21.7749478338147,-60.9310674744833));
#12349=CARTESIAN_POINT('Ctrl Pts',(-20.9458884404335,21.6454715007117,-60.9397637518679));
#12350=CARTESIAN_POINT('Ctrl Pts',(-21.1714834303234,21.3666634326872,-60.9599521380771));
#12351=CARTESIAN_POINT('Ctrl Pts',(-21.3123987992193,21.2224647367113,-60.9715234793257));
#12352=CARTESIAN_POINT('Ctrl Pts',(-21.4754453898374,21.0841924984787,-60.9845141646886));
#12353=CARTESIAN_POINT('Ctrl Pts',(-21.4851161151597,21.0760883622566,-60.9852831642865));
#12354=CARTESIAN_POINT('Ctrl Pts',(-21.4983942245457,21.0650932982952,-60.9863370608412));
#12355=CARTESIAN_POINT('Ctrl Pts',(-21.5019606977756,21.0621529575808,-60.9866199440364));
#12356=CARTESIAN_POINT('Ctrl Pts',(-21.5080415903055,21.0571615661509,-60.9871019449916));
#12357=CARTESIAN_POINT('Ctrl Pts',(-21.5105528118186,21.0551066152746,-60.9873009042595));
#12358=CARTESIAN_POINT('Ctrl Pts',(-21.5154160511688,21.0511392390645,-60.9876860332429));
#12359=CARTESIAN_POINT('Ctrl Pts',(-21.5177676726888,21.049226332373,-60.9878721831455));
#12360=CARTESIAN_POINT('Ctrl Pts',(-21.5233544257301,21.0446949184609,-60.9883142338457));
#12361=CARTESIAN_POINT('Ctrl Pts',(-21.5265919318267,21.0420793595474,-60.9885702532075));
#12362=CARTESIAN_POINT('Ctrl Pts',(-21.5360305710426,21.0344841188369,-60.9893162304157));
#12363=CARTESIAN_POINT('Ctrl Pts',(-21.5422450487759,21.029521137708,-60.9898068585601));
#12364=CARTESIAN_POINT('Ctrl Pts',(-21.5886479881317,20.992743496649,-60.9934665112024));
#12365=CARTESIAN_POINT('Ctrl Pts',(-21.6295700144874,20.961870212821,-60.9966728136921));
#12366=CARTESIAN_POINT('Ctrl Pts',(-21.724037803362,20.8940737648434,-61.004033352073));
#12367=CARTESIAN_POINT('Ctrl Pts',(-21.7779987051726,20.8577701649321,-61.0082092463986));
#12368=CARTESIAN_POINT('Ctrl Pts',(-21.9847947371882,20.7275535247361,-61.0241081105888));
#12369=CARTESIAN_POINT('Ctrl Pts',(-22.1442694589494,20.6448289665185,-61.0361842092896));
#12370=CARTESIAN_POINT('Ctrl Pts',(-22.4442066273927,20.5197419291131,-61.0581816837083));
#12371=CARTESIAN_POINT('Ctrl Pts',(-22.5822904639535,20.4728532338643,-61.0680499798475));
#12372=CARTESIAN_POINT('Ctrl Pts',(-22.7454260943733,20.4295304106614,-61.079118871065));
#12373=CARTESIAN_POINT('Ctrl Pts',(-22.7678365076605,20.4238364730539,-61.0806266482866));
#12374=CARTESIAN_POINT('Ctrl Pts',(-22.7950477614833,20.4172336812214,-61.0824404699813));
#12375=CARTESIAN_POINT('Ctrl Pts',(-22.7997913328638,20.4160940558048,-61.0827560405774));
#12376=CARTESIAN_POINT('Ctrl Pts',(-22.8087635021778,20.4139600627138,-61.0833517250838));
#12377=CARTESIAN_POINT('Ctrl Pts',(-22.8129915535108,20.4129634659019,-61.0836319338836));
#12378=CARTESIAN_POINT('Ctrl Pts',(-22.856230382667,20.4028638485818,-61.0864923171289));
#12379=CARTESIAN_POINT('Ctrl Pts',(-22.8954079154917,20.3944798587892,-61.0890406861707));
#12380=CARTESIAN_POINT('Ctrl Pts',(-22.9399643842328,20.3858103478716,-61.0918822333915));
#12381=CARTESIAN_POINT('Ctrl Pts',(-22.9451975657881,20.3848055732236,-61.0922150921786));
#12382=CARTESIAN_POINT('Ctrl Pts',(-22.9528418891064,20.3833575071793,-61.0927000006252));
#12383=CARTESIAN_POINT('Ctrl Pts',(-22.9552510477401,20.3829039865601,-61.0928526326061));
#12384=CARTESIAN_POINT('Ctrl Pts',(-22.9595149986235,20.3821063405991,-61.093122435575));
#12385=CARTESIAN_POINT('Ctrl Pts',(-22.9613695767238,20.3817610946617,-61.0932396711037));
#12386=CARTESIAN_POINT('Ctrl Pts',(-22.9652409277355,20.381043925216,-61.0934841571537));
#12387=CARTESIAN_POINT('Ctrl Pts',(-22.9672577485344,20.3806722990755,-61.0936113902451));
#12388=CARTESIAN_POINT('Ctrl Pts',(-22.9725218736428,20.3797075081967,-61.0939431350412));
#12389=CARTESIAN_POINT('Ctrl Pts',(-22.9757697475294,20.3791174052438,-61.0941474707479));
#12390=CARTESIAN_POINT('Ctrl Pts',(-22.9896116612382,20.376624445265,-61.0950168687151));
#12391=CARTESIAN_POINT('Ctrl Pts',(-23.0002144515361,20.3747696495597,-61.0956792085634));
#12392=CARTESIAN_POINT('Ctrl Pts',(-23.107764701046,20.3565102201632,-61.1023629530546));
#12393=CARTESIAN_POINT('Ctrl Pts',(-23.2054163680483,20.3444955641927,-61.1081460954601));
#12394=CARTESIAN_POINT('Ctrl Pts',(-23.4659661721426,20.3244855566878,-61.1231814455632));
#12395=CARTESIAN_POINT('Ctrl Pts',(-23.6291788038445,20.3243490468427,-61.1322023952955));
#12396=CARTESIAN_POINT('Ctrl Pts',(-24.026524373483,20.3542030399277,-61.1545053321937));
#12397=CARTESIAN_POINT('Ctrl Pts',(-24.2586590555303,20.3975230135828,-61.1678755418505));
#12398=CARTESIAN_POINT('Ctrl Pts',(-24.4978796027487,20.4699390461666,-61.1830446851712));
#12399=CARTESIAN_POINT('Ctrl Pts',(-24.5117428486926,20.4742381308088,-61.1839286100201));
#12400=CARTESIAN_POINT('Ctrl Pts',(-24.5307680742237,20.4802791597701,-61.1851484985942));
#12401=CARTESIAN_POINT('Ctrl Pts',(-24.5359555296671,20.4819408081766,-61.1854818170897));
#12402=CARTESIAN_POINT('Ctrl Pts',(-24.5442031436713,20.4846057623215,-61.1860128906703));
#12403=CARTESIAN_POINT('Ctrl Pts',(-24.5472660701397,20.4856005224688,-61.1862103635405));
#12404=CARTESIAN_POINT('Ctrl Pts',(-24.5532171079751,20.4875431329991,-61.1865945219092));
#12405=CARTESIAN_POINT('Ctrl Pts',(-24.5561053806212,20.4884904820996,-61.1867811906827));
#12406=CARTESIAN_POINT('Ctrl Pts',(-24.563002620158,20.4907635792258,-61.1872274903984));
#12407=CARTESIAN_POINT('Ctrl Pts',(-24.5670103225148,20.4920931201375,-61.1874872465629));
#12408=CARTESIAN_POINT('Ctrl Pts',(-24.5753152254349,20.4948663717017,-61.1880264189107));
#12409=CARTESIAN_POINT('Ctrl Pts',(-24.5796120136838,20.4963112799224,-61.188305874348));
#12410=CARTESIAN_POINT('Ctrl Pts',(-24.6045625642876,20.5047601983882,-61.1899315286279));
#12411=CARTESIAN_POINT('Ctrl Pts',(-24.6251474483064,20.5119645141368,-61.1912843623856));
#12412=CARTESIAN_POINT('Ctrl Pts',(-24.6792509436818,20.5315183438682,-61.1948714763877));
#12413=CARTESIAN_POINT('Ctrl Pts',(-24.712639335826,20.5442168926455,-61.1971172836032));
#12414=CARTESIAN_POINT('Ctrl Pts',(-24.8652815766188,20.6051943319239,-61.2075364452174));
#12415=CARTESIAN_POINT('Ctrl Pts',(-24.9817751779936,20.6600267330605,-61.2159261283969));
#12416=CARTESIAN_POINT('Ctrl Pts',(-25.1777375010472,20.7670228161099,-61.2307784254913));
#12417=CARTESIAN_POINT('Ctrl Pts',(-25.2587638024771,20.8160135558481,-61.2371556158962));
#12418=CARTESIAN_POINT('Ctrl Pts',(-25.4517457494089,20.9446267109967,-61.2528425305402));
#12419=CARTESIAN_POINT('Ctrl Pts',(-25.5610006206194,21.0279803308805,-61.2621671343419));
#12420=CARTESIAN_POINT('Ctrl Pts',(-25.6850094812523,21.135783447527,-61.273065322758));
#12421=CARTESIAN_POINT('Ctrl Pts',(-25.705185696925,21.1537735897954,-61.2748489207406));
#12422=CARTESIAN_POINT('Ctrl Pts',(-25.735113309361,21.1811421865984,-61.277507565198));
#12423=CARTESIAN_POINT('Ctrl Pts',(-25.7450355477209,21.1903313532693,-61.2783912096354));
#12424=CARTESIAN_POINT('Ctrl Pts',(-25.7573989442393,21.2019267417477,-61.2794947113276));
#12425=CARTESIAN_POINT('Ctrl Pts',(-25.7598943651635,21.2042746396173,-61.2797175679266));
#12426=CARTESIAN_POINT('Ctrl Pts',(-25.7680284083514,21.2119523106597,-61.2804443885856));
#12427=CARTESIAN_POINT('Ctrl Pts',(-25.773651571312,21.2172985082201,-61.2809474779172));
#12428=CARTESIAN_POINT('Ctrl Pts',(-25.784303759794,21.2274995248182,-61.2819016100655));
#12429=CARTESIAN_POINT('Ctrl Pts',(-25.7893363980963,21.2323504928552,-61.2823528661239));
#12430=CARTESIAN_POINT('Ctrl Pts',(-25.8230885540194,21.2650967537914,-61.2853822528281));
#12431=CARTESIAN_POINT('Ctrl Pts',(-25.8513035190106,21.2935103587043,-61.2879292058016));
#12432=CARTESIAN_POINT('Ctrl Pts',(-25.8826662480234,21.326293852951,-61.2907693285691));
#12433=CARTESIAN_POINT('Ctrl Pts',(-25.8863397652418,21.3301528971949,-61.2911021354831));
#12434=CARTESIAN_POINT('Ctrl Pts',(-25.8916894505121,21.335800742513,-61.2915869825293));
#12435=CARTESIAN_POINT('Ctrl Pts',(-25.8933731499115,21.3375823484106,-61.291739604775));
#12436=CARTESIAN_POINT('Ctrl Pts',(-25.8963489450772,21.3407383904971,-61.2920093965138));
#12437=CARTESIAN_POINT('Ctrl Pts',(-25.8976418676301,21.3421120409991,-61.2921266305294));
#12438=CARTESIAN_POINT('Ctrl Pts',(-25.9003378963796,21.3449814492349,-61.2923711195549));
#12439=CARTESIAN_POINT('Ctrl Pts',(-25.9017407781476,21.3464774081192,-61.2924983571245));
#12440=CARTESIAN_POINT('Ctrl Pts',(-25.905398226174,21.3503849858643,-61.2928301264722));
#12441=CARTESIAN_POINT('Ctrl Pts',(-25.9076505237505,21.3527987395285,-61.2930344822036));
#12442=CARTESIAN_POINT('Ctrl Pts',(-25.9125390555374,21.3580538717288,-61.2934781458086));
#12443=CARTESIAN_POINT('Ctrl Pts',(-25.9151738851315,21.3608965583744,-61.2937173465585));
#12444=CARTESIAN_POINT('Ctrl Pts',(-25.9489770999678,21.3974986737711,-61.2967872053593));
#12445=CARTESIAN_POINT('Ctrl Pts',(-25.9794271535135,21.4319182997606,-61.2995641939224));
#12446=CARTESIAN_POINT('Ctrl Pts',(-26.0851323930585,21.5566818322005,-61.3092964105691));
#12447=CARTESIAN_POINT('Ctrl Pts',(-26.156174067329,21.6504846087297,-61.3160124975595));
#12448=CARTESIAN_POINT('Ctrl Pts',(-26.2473623310464,21.7856609229995,-61.3252023900886));
#12449=CARTESIAN_POINT('Ctrl Pts',(-26.2719890418996,21.8238877717852,-61.3277503093511));
#12450=CARTESIAN_POINT('Ctrl Pts',(-26.3205902575429,21.9029554312564,-61.3329417979302));
#12451=CARTESIAN_POINT('Ctrl Pts',(-26.344489851636,21.9438289698151,-61.3355843374131));
#12452=CARTESIAN_POINT('Ctrl Pts',(-26.4866582221311,22.1997464591655,-61.3519539813876));
#12453=CARTESIAN_POINT('Ctrl Pts',(-26.5809232315095,22.4271518197624,-61.3658275944521));
#12454=CARTESIAN_POINT('Ctrl Pts',(-26.6500132423966,22.6684178103628,-61.3810450432634));
#12455=CARTESIAN_POINT('Ctrl Pts',(-26.6515412810313,22.6738068505595,-61.3813851469759));
#12456=CARTESIAN_POINT('Ctrl Pts',(-26.656250004848,22.6905799354696,-61.3824443404705));
#12457=CARTESIAN_POINT('Ctrl Pts',(-26.6593820888514,22.7019774189456,-61.383164989052));
#12458=CARTESIAN_POINT('Ctrl Pts',(-26.6636188152573,22.7177333671218,-61.3841625624633));
#12459=CARTESIAN_POINT('Ctrl Pts',(-26.6647771699699,22.722077397892,-61.3844377414432));
#12460=CARTESIAN_POINT('Ctrl Pts',(-26.6667471228288,22.7295276489118,-61.3849099346824));
#12461=CARTESIAN_POINT('Ctrl Pts',(-26.6675631785666,22.7326326930321,-61.3851068040504));
#12462=CARTESIAN_POINT('Ctrl Pts',(-26.6691438171135,22.7386836957279,-61.3854906009021));
#12463=CARTESIAN_POINT('Ctrl Pts',(-26.6699088692646,22.7416295285972,-61.3856775128954));
#12464=CARTESIAN_POINT('Ctrl Pts',(-26.6717320029493,22.7486906015808,-61.3861256972143));
#12465=CARTESIAN_POINT('Ctrl Pts',(-26.6727861188989,22.7528068509272,-61.3863870976995));
#12466=CARTESIAN_POINT('Ctrl Pts',(-26.6749570651585,22.7613545496068,-61.3869301931893));
#12467=CARTESIAN_POINT('Ctrl Pts',(-26.6760726155802,22.7657863116293,-61.3872119290437));
#12468=CARTESIAN_POINT('Ctrl Pts',(-26.6789693141251,22.7773983495921,-61.3879505415985));
#12469=CARTESIAN_POINT('Ctrl Pts',(-26.680735164004,22.7845823815649,-61.3884079123157));
#12470=CARTESIAN_POINT('Ctrl Pts',(-26.7428652624061,23.0411551712546,-61.4047576911774));
#12471=CARTESIAN_POINT('Ctrl Pts',(-26.773239550744,23.2967895314256,-61.4216706112496));
#12472=CARTESIAN_POINT('Ctrl Pts',(-26.7730011391294,23.5532484913554,-61.4389926226415));
#12473=CARTESIAN_POINT('Ctrl Pts',(-26.773001139735,23.5532478398496,-61.4389925786368));
#12474=CARTESIAN_POINT('Ctrl Pts',(-26.7727947908402,23.7752652681641,-61.4539883047879));
#12475=CARTESIAN_POINT('Ctrl Pts',(-26.7496469772921,23.9966896922317,-61.4691737663365));
#12476=CARTESIAN_POINT('Ctrl Pts',(-26.6975990820527,24.2439863218971,-61.48536084801));
#12477=CARTESIAN_POINT('Ctrl Pts',(-26.6908591135464,24.2738873474472,-61.4873040379773));
#12478=CARTESIAN_POINT('Ctrl Pts',(-26.6827770579011,24.3074995290566,-61.4894690586628));
#12479=CARTESIAN_POINT('Ctrl Pts',(-26.6818538544304,24.3113084285396,-61.4897141151567));
#12480=CARTESIAN_POINT('Ctrl Pts',(-26.6803403124962,24.3175035266299,-61.490112225576));
#12481=CARTESIAN_POINT('Ctrl Pts',(-26.6797541915127,24.3198907363365,-61.4902655194065));
#12482=CARTESIAN_POINT('Ctrl Pts',(-26.6786147521033,24.324508731492,-61.490561839627));
#12483=CARTESIAN_POINT('Ctrl Pts',(-26.6780617776622,24.3267395991493,-61.4907048857696));
#12484=CARTESIAN_POINT('Ctrl Pts',(-26.6770557404356,24.330779747765,-61.4909637605727));
#12485=CARTESIAN_POINT('Ctrl Pts',(-26.6766034948985,24.332589221457,-61.4910796362591));
#12486=CARTESIAN_POINT('Ctrl Pts',(-26.675622276029,24.336500725313,-61.4913299765845));
#12487=CARTESIAN_POINT('Ctrl Pts',(-26.6750927542741,24.3386026088715,-61.491464408499));
#12488=CARTESIAN_POINT('Ctrl Pts',(-26.673647569437,24.3443147920615,-61.4918295043768));
#12489=CARTESIAN_POINT('Ctrl Pts',(-26.6727277639275,24.3479240552917,-61.4920599275194));
#12490=CARTESIAN_POINT('Ctrl Pts',(-26.6683319939941,24.3650486878445,-61.4931519826593));
#12491=CARTESIAN_POINT('Ctrl Pts',(-26.6647744556575,24.3785432482421,-61.4940089398389));
#12492=CARTESIAN_POINT('Ctrl Pts',(-26.5989996544595,24.621625370625,-61.5093875114664));
#12493=CARTESIAN_POINT('Ctrl Pts',(-26.5116285132461,24.8436938859164,-61.5225323337839));
#12494=CARTESIAN_POINT('Ctrl Pts',(-26.3803330152951,25.0925385503838,-61.5382579594058));
#12495=CARTESIAN_POINT('Ctrl Pts',(-26.3593038722681,25.1305158703282,-61.5406861603776));
#12496=CARTESIAN_POINT('Ctrl Pts',(-26.3163995347653,25.2044343521008,-61.5454856595986));
#12497=CARTESIAN_POINT('Ctrl Pts',(-26.2945750183057,25.2403947514648,-61.5478559106757));
#12498=CARTESIAN_POINT('Ctrl Pts',(-26.2080421625401,25.3768785073722,-61.5570165434566));
#12499=CARTESIAN_POINT('Ctrl Pts',(-26.1384688842081,25.474191248581,-61.5639027718199));
#12500=CARTESIAN_POINT('Ctrl Pts',(-26.0287888974808,25.6108539554439,-61.5742939569102));
#12501=CARTESIAN_POINT('Ctrl Pts',(-25.9928029353075,25.6533853594035,-61.5776384292615));
#12502=CARTESIAN_POINT('Ctrl Pts',(-25.9509507385277,25.7003263335434,-61.5814661368066));
#12503=CARTESIAN_POINT('Ctrl Pts',(-25.9461491102277,25.7056756496338,-61.5819043915142));
#12504=CARTESIAN_POINT('Ctrl Pts',(-25.9383245841433,25.7143342130285,-61.5826171325561));
#12505=CARTESIAN_POINT('Ctrl Pts',(-25.9353125907253,25.717653317352,-61.5828911581616));
#12506=CARTESIAN_POINT('Ctrl Pts',(-25.929474526241,25.7240597405792,-61.583421646853));
#12507=CARTESIAN_POINT('Ctrl Pts',(-25.9266493439958,25.7271478601279,-61.5836780719226));
#12508=CARTESIAN_POINT('Ctrl Pts',(-25.9217655184609,25.7324653820706,-61.5841208504671));
#12509=CARTESIAN_POINT('Ctrl Pts',(-25.9197097225313,25.7346974020077,-61.5843070822777));
#12510=CARTESIAN_POINT('Ctrl Pts',(-25.9154557560405,25.7393029504051,-61.5846921332623));
#12511=CARTESIAN_POINT('Ctrl Pts',(-25.9132571585111,25.7416760785328,-61.5848909706148));
#12512=CARTESIAN_POINT('Ctrl Pts',(-25.9072964192264,25.74809059701,-61.5854295920117));
#12513=CARTESIAN_POINT('Ctrl Pts',(-25.9035274712297,25.7521256223721,-61.585769668243));
#12514=CARTESIAN_POINT('Ctrl Pts',(-25.889483711881,25.7670835876952,-61.587035048511));
#12515=CARTESIAN_POINT('Ctrl Pts',(-25.8791431926051,25.777944324224,-61.5879631882872));
#12516=CARTESIAN_POINT('Ctrl Pts',(-25.7072542936013,25.9559759004682,-61.6033345214073));
#12517=CARTESIAN_POINT('Ctrl Pts',(-25.5281944278852,26.1052214148002,-61.6186001657496));
#12518=CARTESIAN_POINT('Ctrl Pts',(-25.2633491675955,26.2813248390844,-61.6400325796174));
#12519=CARTESIAN_POINT('Ctrl Pts',(-25.1901522793135,26.3258938185981,-61.645841492262));
#12520=CARTESIAN_POINT('Ctrl Pts',(-25.0359169887877,26.4115736145694,-61.6577718219877));
#12521=CARTESIAN_POINT('Ctrl Pts',(-24.9547355244229,26.4522839216178,-61.6638861916147));
#12522=CARTESIAN_POINT('Ctrl Pts',(-24.810712171946,26.5170464231896,-61.6743425088113));
#12523=CARTESIAN_POINT('Ctrl Pts',(-24.7486337563361,26.5426609734568,-61.6787285098847));
#12524=CARTESIAN_POINT('Ctrl Pts',(-24.6679908439936,26.5730228827407,-61.6842337529714));
#12525=CARTESIAN_POINT('Ctrl Pts',(-24.6501260424632,26.5795689282214,-61.6854414164826));
#12526=CARTESIAN_POINT('Ctrl Pts',(-24.6212789724783,26.5898502746885,-61.687371183226));
#12527=CARTESIAN_POINT('Ctrl Pts',(-24.610332973953,26.5936850579361,-61.6880987600921));
#12528=CARTESIAN_POINT('Ctrl Pts',(-24.5970063191923,26.5982732502294,-61.6889787053505));
#12529=CARTESIAN_POINT('Ctrl Pts',(-24.5946453708702,26.5990830271202,-61.6891343729312));
#12530=CARTESIAN_POINT('Ctrl Pts',(-24.5900828102896,26.6006420088858,-61.6894347676971));
#12531=CARTESIAN_POINT('Ctrl Pts',(-24.5878813242596,26.601391574702,-61.6895795162321));
#12532=CARTESIAN_POINT('Ctrl Pts',(-24.5839110595067,26.6027385833994,-61.6898402082445));
#12533=CARTESIAN_POINT('Ctrl Pts',(-24.5821425772303,26.6033368708432,-61.6899562019728));
#12534=CARTESIAN_POINT('Ctrl Pts',(-24.5783392186607,26.6046198861698,-61.6902053891845));
#12535=CARTESIAN_POINT('Ctrl Pts',(-24.576304183376,26.6053041155712,-61.6903385524866));
#12536=CARTESIAN_POINT('Ctrl Pts',(-24.5708205335342,26.6071417575838,-61.6906969300287));
#12537=CARTESIAN_POINT('Ctrl Pts',(-24.5673706350273,26.6082913721803,-61.690921918089));
#12538=CARTESIAN_POINT('Ctrl Pts',(-24.5514863244174,26.6135546700965,-61.6919556693956));
#12539=CARTESIAN_POINT('Ctrl Pts',(-24.5390286233749,26.6175984452129,-61.6927603383686));
#12540=CARTESIAN_POINT('Ctrl Pts',(-24.3115467563891,26.6899092428435,-61.7073492035655));
#12541=CARTESIAN_POINT('Ctrl Pts',(-24.0899260394759,26.7354998713756,-61.7198867217408));
#12542=CARTESIAN_POINT('Ctrl Pts',(-23.7071500151676,26.7731026460078,-61.7413772570515));
#12543=CARTESIAN_POINT('Ctrl Pts',(-23.548044804176,26.776918044297,-61.7502606007284));
#12544=CARTESIAN_POINT('Ctrl Pts',(-23.286282235583,26.7638299552651,-61.7654177473956));
#12545=CARTESIAN_POINT('Ctrl Pts',(-23.1835640776844,26.7537344582914,-61.7715012318966));
#12546=CARTESIAN_POINT('Ctrl Pts',(-23.0622730692102,26.7359034568069,-61.7789206071396));
#12547=CARTESIAN_POINT('Ctrl Pts',(-23.0430585881178,26.7329008079353,-61.7801029610204));
#12548=CARTESIAN_POINT('Ctrl Pts',(-23.0195516456687,26.7290090992961,-61.7815583839449));
#12549=CARTESIAN_POINT('Ctrl Pts',(-23.0152319891155,26.7282849049121,-61.7818262040267));
#12550=CARTESIAN_POINT('Ctrl Pts',(-23.0068600927136,26.7268637962524,-61.7823459879673));
#12551=CARTESIAN_POINT('Ctrl Pts',(-23.0028076819765,26.7261679280999,-61.7825979181069));
#12552=CARTESIAN_POINT('Ctrl Pts',(-22.9957760806056,26.7249466239421,-61.7830356338216));
#12553=CARTESIAN_POINT('Ctrl Pts',(-22.9927962707597,26.7244247436591,-61.783221305852));
#12554=CARTESIAN_POINT('Ctrl Pts',(-22.9865995584043,26.7233304639753,-61.7836077984385));
#12555=CARTESIAN_POINT('Ctrl Pts',(-22.9833827840009,26.7227573666228,-61.783808641068));
#12556=CARTESIAN_POINT('Ctrl Pts',(-22.9755369615362,26.7213472487683,-61.784299019455));
#12557=CARTESIAN_POINT('Ctrl Pts',(-22.9709088736536,26.720504984853,-61.7845887223181));
#12558=CARTESIAN_POINT('Ctrl Pts',(-22.9533455239478,26.7172688938658,-61.7856898077358));
#12559=CARTESIAN_POINT('Ctrl Pts',(-22.9404232558358,26.7148060326194,-61.7865033926721));
#12560=CARTESIAN_POINT('Ctrl Pts',(-22.7157639893085,26.6705609700712,-61.8007092585757));
#12561=CARTESIAN_POINT('Ctrl Pts',(-22.5087797959071,26.6077019281494,-61.8148044895628));
#12562=CARTESIAN_POINT('Ctrl Pts',(-22.229998003443,26.491425106261,-61.835092358332));
#12563=CARTESIAN_POINT('Ctrl Pts',(-22.1517269529096,26.4550217759146,-61.8409354953986));
#12564=CARTESIAN_POINT('Ctrl Pts',(-22.0750358661665,26.4155366977499,-61.8467738923868));
#12565=CARTESIAN_POINT('',(-26.7730032083997,23.5493289177337,-61.6829767636861));
#12566=CARTESIAN_POINT('Ctrl Pts',(-22.0750361387181,26.4155368380754,-62.0907209741597));
#12567=CARTESIAN_POINT('Ctrl Pts',(-22.1348983042596,26.4463573914597,-62.0862507094239));
#12568=CARTESIAN_POINT('Ctrl Pts',(-22.1957343443035,26.4753060929015,-62.0818347705942));
#12569=CARTESIAN_POINT('Ctrl Pts',(-22.2890802308409,26.5161847309523,-62.0752946354846));
#12570=CARTESIAN_POINT('Ctrl Pts',(-22.3209256529958,26.5295251020064,-62.0731038077036));
#12571=CARTESIAN_POINT('Ctrl Pts',(-22.3572481549109,26.5440593466051,-62.0706554199582));
#12572=CARTESIAN_POINT('Ctrl Pts',(-22.3615191346708,26.5457577644479,-62.0703683104026));
#12573=CARTESIAN_POINT('Ctrl Pts',(-22.3679934679548,26.5483163507416,-62.0699342866162));
#12574=CARTESIAN_POINT('Ctrl Pts',(-22.3701941362364,26.5491832311724,-62.0697869691642));
#12575=CARTESIAN_POINT('Ctrl Pts',(-22.3740254197869,26.5506875683066,-62.0695308627783));
#12576=CARTESIAN_POINT('Ctrl Pts',(-22.3756555999684,26.5513261188846,-62.0694220073787));
#12577=CARTESIAN_POINT('Ctrl Pts',(-22.3790362690513,26.5526471690822,-62.0691965041688));
#12578=CARTESIAN_POINT('Ctrl Pts',(-22.3807868334832,26.5533294659775,-62.0690798690874));
#12579=CARTESIAN_POINT('Ctrl Pts',(-22.3849564955543,26.5549504272834,-62.068802373458));
#12580=CARTESIAN_POINT('Ctrl Pts',(-22.3873761391432,26.5558877043928,-62.0686415973042));
#12581=CARTESIAN_POINT('Ctrl Pts',(-22.3925163477922,26.5578716877665,-62.068300583244));
#12582=CARTESIAN_POINT('Ctrl Pts',(-22.3952372087995,26.5589176282987,-62.0681203914689));
#12583=CARTESIAN_POINT('Ctrl Pts',(-22.4026515583563,26.5617562774942,-62.0676302214017));
#12584=CARTESIAN_POINT('Ctrl Pts',(-22.4073478501987,26.5635417137648,-62.0673206744759));
#12585=CARTESIAN_POINT('Ctrl Pts',(-22.4220208515739,26.5690808577836,-62.066356374561));
#12586=CARTESIAN_POINT('Ctrl Pts',(-22.4320121442184,26.5727961011927,-62.065703848325));
#12587=CARTESIAN_POINT('Ctrl Pts',(-22.4698076656402,26.5866372316084,-62.0632502172207));
#12588=CARTESIAN_POINT('Ctrl Pts',(-22.4977334142995,26.5964299396005,-62.0614674125305));
#12589=CARTESIAN_POINT('Ctrl Pts',(-22.5893792252394,26.6271564972446,-62.0557023313666));
#12590=CARTESIAN_POINT('Ctrl Pts',(-22.6536215535954,26.6464872752498,-62.0517950470289));
#12591=CARTESIAN_POINT('Ctrl Pts',(-23.0927241919434,26.7637997439734,-62.0256999094175));
#12592=CARTESIAN_POINT('Ctrl Pts',(-23.4819674535229,26.7954937877334,-62.0051092222063));
#12593=CARTESIAN_POINT('Ctrl Pts',(-23.8874729132588,26.7553735015161,-61.9804611769144));
#12594=CARTESIAN_POINT('Ctrl Pts',(-23.9073678962075,26.7532178148759,-61.9792450238951));
#12595=CARTESIAN_POINT('Ctrl Pts',(-23.9334066288751,26.7501508176658,-61.9776439057701));
#12596=CARTESIAN_POINT('Ctrl Pts',(-23.9395699416906,26.7494068037124,-61.9772642331572));
#12597=CARTESIAN_POINT('Ctrl Pts',(-23.949078356347,26.7482310963465,-61.976677415551));
#12598=CARTESIAN_POINT('Ctrl Pts',(-23.9524250183405,26.7478119493177,-61.9764706676532));
#12599=CARTESIAN_POINT('Ctrl Pts',(-23.959088216047,26.7469668020992,-61.9760586189606));
#12600=CARTESIAN_POINT('Ctrl Pts',(-23.9624047591763,26.7465408923805,-61.9758533212689));
#12601=CARTESIAN_POINT('Ctrl Pts',(-23.9697553688048,26.7455852978474,-61.9753978546151));
#12602=CARTESIAN_POINT('Ctrl Pts',(-23.973789102262,26.7450531342272,-61.9751476074535));
#12603=CARTESIAN_POINT('Ctrl Pts',(-23.9854247810781,26.7434956350085,-61.9744248616323));
#12604=CARTESIAN_POINT('Ctrl Pts',(-23.9930240487318,26.7424508002183,-61.9739517458308));
#12605=CARTESIAN_POINT('Ctrl Pts',(-24.0442403191113,26.7352225954622,-61.9707556781446));
#12606=CARTESIAN_POINT('Ctrl Pts',(-24.0877285039204,26.7281728437512,-61.968005356302));
#12607=CARTESIAN_POINT('Ctrl Pts',(-24.1979051597372,26.7079862670966,-61.960939936521));
#12608=CARTESIAN_POINT('Ctrl Pts',(-24.2643449674852,26.6936276546812,-61.9565873208804));
#12609=CARTESIAN_POINT('Ctrl Pts',(-24.5019507564445,26.6343559187636,-61.9406852691831));
#12610=CARTESIAN_POINT('Ctrl Pts',(-24.6697871274292,26.5774710992069,-61.9287942516228));
#12611=CARTESIAN_POINT('Ctrl Pts',(-24.9054751209075,26.4752973085792,-61.9114091623848));
#12612=CARTESIAN_POINT('Ctrl Pts',(-24.977652389534,26.4407620354602,-61.9059893068155));
#12613=CARTESIAN_POINT('Ctrl Pts',(-25.1734897905367,26.3379320953801,-61.8911182266855));
#12614=CARTESIAN_POINT('Ctrl Pts',(-25.2940771427177,26.2641322271398,-61.8817676627819));
#12615=CARTESIAN_POINT('Ctrl Pts',(-25.4160790971411,26.1779653607126,-61.8723865830397));
#12616=CARTESIAN_POINT('Ctrl Pts',(-25.4226933688041,26.1732563058107,-61.8718782696924));
#12617=CARTESIAN_POINT('Ctrl Pts',(-25.4315118798352,26.1669275798934,-61.8712010076892));
#12618=CARTESIAN_POINT('Ctrl Pts',(-25.4337318806904,26.1653300802335,-61.8710305497779));
#12619=CARTESIAN_POINT('Ctrl Pts',(-25.4374508910095,26.1626467096814,-61.8707450616491));
#12620=CARTESIAN_POINT('Ctrl Pts',(-25.4389509981492,26.1615623737918,-61.870629925186));
#12621=CARTESIAN_POINT('Ctrl Pts',(-25.4419408429953,26.1593972733161,-61.8704004865963));
#12622=CARTESIAN_POINT('Ctrl Pts',(-25.4434305791984,26.1583165321198,-61.8702861846003));
#12623=CARTESIAN_POINT('Ctrl Pts',(-25.4467797092904,26.155882496946,-61.8700292606121));
#12624=CARTESIAN_POINT('Ctrl Pts',(-25.4486385772807,26.1545284911848,-61.8698866893688));
#12625=CARTESIAN_POINT('Ctrl Pts',(-25.4538913606107,26.1506937335384,-61.8694838899747));
#12626=CARTESIAN_POINT('Ctrl Pts',(-25.4572818894172,26.1482083173969,-61.8692239861287));
#12627=CARTESIAN_POINT('Ctrl Pts',(-25.4650639723633,26.1424802434008,-61.8686276316466));
#12628=CARTESIAN_POINT('Ctrl Pts',(-25.4694521848803,26.1392330366195,-61.8682914931845));
#12629=CARTESIAN_POINT('Ctrl Pts',(-25.4834040274463,26.128853932152,-61.8672231429246));
#12630=CARTESIAN_POINT('Ctrl Pts',(-25.4929364489092,26.1216799749388,-61.8664937546918));
#12631=CARTESIAN_POINT('Ctrl Pts',(-25.5298875130364,26.0935484015138,-61.8636675782526));
#12632=CARTESIAN_POINT('Ctrl Pts',(-25.5570097274758,26.0722030291371,-61.8615957246152));
#12633=CARTESIAN_POINT('Ctrl Pts',(-25.6626739232377,25.9862603336209,-61.8535110758957));
#12634=CARTESIAN_POINT('Ctrl Pts',(-25.7384885022577,25.918392077268,-61.8476804035136));
#12635=CARTESIAN_POINT('Ctrl Pts',(-26.0565060257945,25.6053695221999,-61.8224506829145));
#12636=CARTESIAN_POINT('Ctrl Pts',(-26.261677137006,25.3259170459436,-61.8037785449454));
#12637=CARTESIAN_POINT('Ctrl Pts',(-26.4281728551776,25.0008119090734,-61.7816941450935));
#12638=CARTESIAN_POINT('Ctrl Pts',(-26.4374501167941,24.9822574091092,-61.7804337653922));
#12639=CARTESIAN_POINT('Ctrl Pts',(-26.4493087636323,24.9579563964744,-61.778782622177));
#12640=CARTESIAN_POINT('Ctrl Pts',(-26.4520534846625,24.9522897763206,-61.7783975725911));
#12641=CARTESIAN_POINT('Ctrl Pts',(-26.456250659572,24.943559367785,-61.7778042801224));
#12642=CARTESIAN_POINT('Ctrl Pts',(-26.4577149246208,24.9405012476816,-61.777596448705));
#12643=CARTESIAN_POINT('Ctrl Pts',(-26.460599339484,24.9344526547493,-61.7771853595334));
#12644=CARTESIAN_POINT('Ctrl Pts',(-26.4620197130027,24.931462292738,-61.7769821098694));
#12645=CARTESIAN_POINT('Ctrl Pts',(-26.4651573198628,24.9248302302335,-61.7765313123871));
#12646=CARTESIAN_POINT('Ctrl Pts',(-26.4668723393945,24.9211874938662,-61.7762836881453));
#12647=CARTESIAN_POINT('Ctrl Pts',(-26.4717508164815,24.9107749213434,-61.775575808498));
#12648=CARTESIAN_POINT('Ctrl Pts',(-26.4748975454269,24.9039973166864,-61.77511497477));
#12649=CARTESIAN_POINT('Ctrl Pts',(-26.4947749712628,24.8607913924581,-61.7721767232056));
#12650=CARTESIAN_POINT('Ctrl Pts',(-26.5108477102306,24.8240658843355,-61.7696767393512));
#12651=CARTESIAN_POINT('Ctrl Pts',(-26.5565740976545,24.7140393225136,-61.7621757810922));
#12652=CARTESIAN_POINT('Ctrl Pts',(-26.5842180297521,24.6399408726663,-61.7571088459108));
#12653=CARTESIAN_POINT('Ctrl Pts',(-26.7177887014048,24.237267997524,-61.7294873244182));
#12654=CARTESIAN_POINT('Ctrl Pts',(-26.7731008870704,23.8943916030023,-61.7053486917779));
#12655=CARTESIAN_POINT('Ctrl Pts',(-26.7730024004244,23.5493326950576,-61.6829756068469));
#12656=CARTESIAN_POINT('Ctrl Pts',(-26.7730023993701,23.5493290084874,-61.6829753678154));
#12657=CARTESIAN_POINT('Ctrl Pts',(-26.77298796788,23.4989685168407,-61.6797100738703));
#12658=CARTESIAN_POINT('Ctrl Pts',(-26.7717930925859,23.4486111574792,-61.6764920584389));
#12659=CARTESIAN_POINT('Ctrl Pts',(-26.7692328724598,23.3943725239603,-61.6730914108621));
#12660=CARTESIAN_POINT('Ctrl Pts',(-26.7690403661588,23.3904467491426,-61.6728456432062));
#12661=CARTESIAN_POINT('Ctrl Pts',(-26.7687155509059,23.3840616106022,-61.6724465234169));
#12662=CARTESIAN_POINT('Ctrl Pts',(-26.7685876045742,23.3816020438382,-61.6722929297187));
#12663=CARTESIAN_POINT('Ctrl Pts',(-26.7683579156123,23.3772820954303,-61.6720234226909));
#12664=CARTESIAN_POINT('Ctrl Pts',(-26.768257379174,23.375421654951,-61.6719074416966));
#12665=CARTESIAN_POINT('Ctrl Pts',(-26.7680577452648,23.3717859200148,-61.6716809564883));
#12666=CARTESIAN_POINT('Ctrl Pts',(-26.7679587917668,23.3700106167124,-61.6715704440393));
#12667=CARTESIAN_POINT('Ctrl Pts',(-26.7677588472377,23.3664760997634,-61.6713505784151));
#12668=CARTESIAN_POINT('Ctrl Pts',(-26.7676578827629,23.3647168897093,-61.6712412239035));
#12669=CARTESIAN_POINT('Ctrl Pts',(-26.7674154396115,23.3605522616753,-61.6709825278229));
#12670=CARTESIAN_POINT('Ctrl Pts',(-26.7672727057288,23.3581469136953,-61.6708332574662));
#12671=CARTESIAN_POINT('Ctrl Pts',(-26.7668394262751,23.3509812157547,-61.6703889929946));
#12672=CARTESIAN_POINT('Ctrl Pts',(-26.7665410096811,23.3462213213228,-61.6700944406322));
#12673=CARTESIAN_POINT('Ctrl Pts',(-26.7636913419284,23.3023281615626,-61.667383216405));
#12674=CARTESIAN_POINT('Ctrl Pts',(-26.7604364223237,23.2632417158167,-61.6650053901776));
#12675=CARTESIAN_POINT('Ctrl Pts',(-26.7559160695493,23.2187880830934,-61.6623328016616));
#12676=CARTESIAN_POINT('Ctrl Pts',(-26.7553496617834,23.2133552385687,-61.6620067162069));
#12677=CARTESIAN_POINT('Ctrl Pts',(-26.7535324870158,23.1963447830095,-61.6609873530432));
#12678=CARTESIAN_POINT('Ctrl Pts',(-26.7522327671734,23.1847723740444,-61.6602962251322));
#12679=CARTESIAN_POINT('Ctrl Pts',(-26.71680429906,22.8840314575788,-61.6423908248603));
#12680=CARTESIAN_POINT('Ctrl Pts',(-26.6437033804265,22.6007760681689,-61.626752536299));
#12681=CARTESIAN_POINT('Ctrl Pts',(-26.4952981481866,22.2376065449688,-61.6044334485409));
#12682=CARTESIAN_POINT('Ctrl Pts',(-26.4526877085093,22.1459019181378,-61.598597310402));
#12683=CARTESIAN_POINT('Ctrl Pts',(-26.3758231662176,21.998975049912,-61.5887906099315));
#12684=CARTESIAN_POINT('Ctrl Pts',(-26.3440835948615,21.9425155127872,-61.5849058753863));
#12685=CARTESIAN_POINT('Ctrl Pts',(-26.3063146808832,21.8798303995179,-61.580444959906));
#12686=CARTESIAN_POINT('Ctrl Pts',(-26.3019345219486,21.8726247743425,-61.5799299292277));
#12687=CARTESIAN_POINT('Ctrl Pts',(-26.2953160648788,21.861832668847,-61.57915513239));
#12688=CARTESIAN_POINT('Ctrl Pts',(-26.293098883079,21.8582332271638,-61.5788961443316));
#12689=CARTESIAN_POINT('Ctrl Pts',(-26.2892748873779,21.8520525015314,-61.5784504353641));
#12690=CARTESIAN_POINT('Ctrl Pts',(-26.2876714870989,21.8494691034275,-61.5782638407588));
#12691=CARTESIAN_POINT('Ctrl Pts',(-26.2843631703712,21.8441555419157,-61.5778794335847));
#12692=CARTESIAN_POINT('Ctrl Pts',(-26.2826578152181,21.8414256564661,-61.5776816048979));
#12693=CARTESIAN_POINT('Ctrl Pts',(-26.2785446123238,21.8348632548158,-61.5772052297454));
#12694=CARTESIAN_POINT('Ctrl Pts',(-26.2761327796085,21.8310332547661,-61.5769265355586));
#12695=CARTESIAN_POINT('Ctrl Pts',(-26.2687131782411,21.8193057607094,-61.5760711109888));
#12696=CARTESIAN_POINT('Ctrl Pts',(-26.2636791307752,21.811425024652,-61.5754934031743));
#12697=CARTESIAN_POINT('Ctrl Pts',(-26.2050136701497,21.7204601477895,-61.568791499522));
#12698=CARTESIAN_POINT('Ctrl Pts',(-26.1476251094473,21.6398732243153,-61.5625261077611));
#12699=CARTESIAN_POINT('Ctrl Pts',(-25.9066228427523,21.3324222915602,-61.537247804175));
#12700=CARTESIAN_POINT('Ctrl Pts',(-25.696275748339,21.1283140911703,-61.5171696679778));
#12701=CARTESIAN_POINT('Ctrl Pts',(-25.4259614124385,20.929227555305,-61.494745387239));
#12702=CARTESIAN_POINT('Ctrl Pts',(-25.3899807431336,20.9038481553379,-61.4918242623714));
#12703=CARTESIAN_POINT('Ctrl Pts',(-25.3101847814587,20.8499773384049,-61.4855007852995));
#12704=CARTESIAN_POINT('Ctrl Pts',(-25.2661720418521,20.8217971875919,-61.482111285724));
#12705=CARTESIAN_POINT('Ctrl Pts',(-25.207362350812,20.7861292257318,-61.4777289163152));
#12706=CARTESIAN_POINT('Ctrl Pts',(-25.1931678102999,20.7776688959699,-61.4766821540836));
#12707=CARTESIAN_POINT('Ctrl Pts',(-25.1729172289965,20.76580913142,-61.4752050126637));
#12708=CARTESIAN_POINT('Ctrl Pts',(-25.1669145846239,20.7623196813717,-61.4747691677191));
#12709=CARTESIAN_POINT('Ctrl Pts',(-25.1577199487639,20.7570143480418,-61.4741046744202));
#12710=CARTESIAN_POINT('Ctrl Pts',(-25.1545360988026,20.7551845031523,-61.4738751481009));
#12711=CARTESIAN_POINT('Ctrl Pts',(-25.1486373277577,20.7518077189741,-61.4734509639567));
#12712=CARTESIAN_POINT('Ctrl Pts',(-25.1459232759393,20.7502592812942,-61.4732562102904));
#12713=CARTESIAN_POINT('Ctrl Pts',(-25.141472707935,20.7477286882182,-61.4729375340816));
#12714=CARTESIAN_POINT('Ctrl Pts',(-25.139737532262,20.7467441982753,-61.4728134598668));
#12715=CARTESIAN_POINT('Ctrl Pts',(-25.1363909274929,20.7448495344469,-61.4725744899994));
#12716=CARTESIAN_POINT('Ctrl Pts',(-25.1347796327376,20.7439391397753,-61.4724595802872));
#12717=CARTESIAN_POINT('Ctrl Pts',(-25.1310236056667,20.7418212200615,-61.4721920603812));
#12718=CARTESIAN_POINT('Ctrl Pts',(-25.1288782677416,20.7406147603697,-61.4720395196366));
#12719=CARTESIAN_POINT('Ctrl Pts',(-25.1231381391869,20.7373953716967,-61.4716320639902));
#12720=CARTESIAN_POINT('Ctrl Pts',(-25.1195408520804,20.7353868679806,-61.4713774344176));
#12721=CARTESIAN_POINT('Ctrl Pts',(-25.0947394809378,20.7216016290153,-61.4696267784791));
#12722=CARTESIAN_POINT('Ctrl Pts',(-25.0734061478839,20.7100572898994,-61.4681454461586));
#12723=CARTESIAN_POINT('Ctrl Pts',(-24.8958300525273,20.6165399666368,-61.455999695206));
#12724=CARTESIAN_POINT('Ctrl Pts',(-24.7332052316643,20.5472725859317,-61.4460416360131));
#12725=CARTESIAN_POINT('Ctrl Pts',(-24.5492041631577,20.4861840659201,-61.4351857125989));
#12726=CARTESIAN_POINT('Ctrl Pts',(-24.5326572158684,20.4808387498048,-61.4342130889292));
#12727=CARTESIAN_POINT('Ctrl Pts',(-24.4972920077689,20.4697296688511,-61.4321407115824));
#12728=CARTESIAN_POINT('Ctrl Pts',(-24.4784625870231,20.4640038423793,-61.4310411415158));
#12729=CARTESIAN_POINT('Ctrl Pts',(-24.4378898825118,20.4520710100127,-61.4286781246671));
#12730=CARTESIAN_POINT('Ctrl Pts',(-24.4161313664937,20.445919648689,-61.4274147222222));
#12731=CARTESIAN_POINT('Ctrl Pts',(-24.3687391414372,20.4330584001663,-61.4246684341453));
#12732=CARTESIAN_POINT('Ctrl Pts',(-24.3430838444238,20.4264346624111,-61.4231852416972));
#12733=CARTESIAN_POINT('Ctrl Pts',(-24.286274395182,20.4125124110083,-61.4199042787008));
#12734=CARTESIAN_POINT('Ctrl Pts',(-24.2550874997141,20.405360025295,-61.4181052970364));
#12735=CARTESIAN_POINT('Ctrl Pts',(-24.0456409529083,20.360597672067,-61.4060166067711));
#12736=CARTESIAN_POINT('Ctrl Pts',(-23.8646011426449,20.3377023925571,-61.3955076210613));
#12737=CARTESIAN_POINT('Ctrl Pts',(-23.6646136032446,20.3294818770431,-61.383383536608));
#12738=CARTESIAN_POINT('Ctrl Pts',(-23.6466092679616,20.3288929703637,-61.3822877408049));
#12739=CARTESIAN_POINT('Ctrl Pts',(-23.622876154311,20.3283158209997,-61.3808373233665));
#12740=CARTESIAN_POINT('Ctrl Pts',(-23.6171507551954,20.3281918579474,-61.380486967183));
#12741=CARTESIAN_POINT('Ctrl Pts',(-23.6077857516741,20.3280140643208,-61.3799131351714));
#12742=CARTESIAN_POINT('Ctrl Pts',(-23.6041463156831,20.3279511379856,-61.3796899452571));
#12743=CARTESIAN_POINT('Ctrl Pts',(-23.5971190791077,20.3278415447733,-61.3792586333764));
#12744=CARTESIAN_POINT('Ctrl Pts',(-23.5937312946503,20.3277940542384,-61.3790505375629));
#12745=CARTESIAN_POINT('Ctrl Pts',(-23.5859454374688,20.3276971908968,-61.3785719107915));
#12746=CARTESIAN_POINT('Ctrl Pts',(-23.5815473331898,20.3276514792651,-61.3783012652277));
#12747=CARTESIAN_POINT('Ctrl Pts',(-23.5676092977153,20.3275351502584,-61.3774426760297));
#12748=CARTESIAN_POINT('Ctrl Pts',(-23.5580692059021,20.3274978909561,-61.3768536863905));
#12749=CARTESIAN_POINT('Ctrl Pts',(-23.4768855723816,20.3275413037916,-61.3718301398985));
#12750=CARTESIAN_POINT('Ctrl Pts',(-23.4052682892536,20.3299685987673,-61.3673222932025));
#12751=CARTESIAN_POINT('Ctrl Pts',(-23.2758893200614,20.3386780366423,-61.359030749554));
#12752=CARTESIAN_POINT('Ctrl Pts',(-23.218101812269,20.3441394404512,-61.3552736995221));
#12753=CARTESIAN_POINT('Ctrl Pts',(-23.1570944813177,20.3515721707212,-61.3512516503649));
#12754=CARTESIAN_POINT('Ctrl Pts',(-23.1536936813346,20.3519920072328,-61.351027261994));
#12755=CARTESIAN_POINT('Ctrl Pts',(-22.8910522854692,20.3848410354703,-61.3336838329514));
#12756=CARTESIAN_POINT('Ctrl Pts',(-22.6367259409956,20.4486696273512,-61.3157162825649));
#12757=CARTESIAN_POINT('Ctrl Pts',(-22.3521784229073,20.5581556764268,-61.2953673878405));
#12758=CARTESIAN_POINT('Ctrl Pts',(-22.3117371990433,20.5746676791203,-61.2924721076232));
#12759=CARTESIAN_POINT('Ctrl Pts',(-22.2249782366115,20.6121664242863,-61.2862709184932));
#12760=CARTESIAN_POINT('Ctrl Pts',(-22.1787945632529,20.6334382401077,-61.2829762510978));
#12761=CARTESIAN_POINT('Ctrl Pts',(-22.118747894696,20.662836993012,-61.2787188723746));
#12762=CARTESIAN_POINT('Ctrl Pts',(-22.104417314616,20.6699861259441,-61.2777048283309));
#12763=CARTESIAN_POINT('Ctrl Pts',(-22.0840922002756,20.6803156905262,-61.2762701084281));
#12764=CARTESIAN_POINT('Ctrl Pts',(-22.0780537708292,20.683408552651,-61.2758443078438));
#12765=CARTESIAN_POINT('Ctrl Pts',(-22.0688161183545,20.6881769287432,-61.2751936460567));
#12766=CARTESIAN_POINT('Ctrl Pts',(-22.0656099151044,20.6898387670295,-61.2749679500923));
#12767=CARTESIAN_POINT('Ctrl Pts',(-22.0603405970504,20.6925812046347,-61.2745972559877));
#12768=CARTESIAN_POINT('Ctrl Pts',(-22.0582758588014,20.6936586518928,-61.2744520612587));
#12769=CARTESIAN_POINT('Ctrl Pts',(-22.0543641604898,20.6957053007023,-61.27417710009));
#12770=CARTESIAN_POINT('Ctrl Pts',(-22.0525169714267,20.6966740581567,-61.2740473056566));
#12771=CARTESIAN_POINT('Ctrl Pts',(-22.0490532601842,20.6984948896671,-61.2738040171793));
#12772=CARTESIAN_POINT('Ctrl Pts',(-22.0474365282364,20.6993465421115,-61.2736904971235));
#12773=CARTESIAN_POINT('Ctrl Pts',(-22.0441402472675,20.701086520535,-61.273459123774));
#12774=CARTESIAN_POINT('Ctrl Pts',(-22.0424607658326,20.701974953351,-61.273341278081));
#12775=CARTESIAN_POINT('Ctrl Pts',(-22.0376292608331,20.7045362533843,-61.2730023763507));
#12776=CARTESIAN_POINT('Ctrl Pts',(-22.0344792160151,20.7062128779698,-61.2727815600118));
#12777=CARTESIAN_POINT('Ctrl Pts',(-22.0206665207952,20.7135942101874,-61.2718138878588));
#12778=CARTESIAN_POINT('Ctrl Pts',(-22.0100330617969,20.7193537710198,-61.2710704874358));
#12779=CARTESIAN_POINT('Ctrl Pts',(-21.9963574789405,20.7268609489837,-61.2701160780696));
#12780=CARTESIAN_POINT('Ctrl Pts',(-21.9932856230027,20.7285537685751,-61.2699018046384));
#12781=CARTESIAN_POINT('Ctrl Pts',(-21.7507628691689,20.862718345016,-61.2529930856901));
#12782=CARTESIAN_POINT('Ctrl Pts',(-21.5291113834145,21.0251690425092,-61.2381040094146));
#12783=CARTESIAN_POINT('Ctrl Pts',(-21.3046575496665,21.2383907919833,-61.2207371433525));
#12784=CARTESIAN_POINT('Ctrl Pts',(-21.2790922029574,21.2635010736892,-61.2187216805558));
#12785=CARTESIAN_POINT('Ctrl Pts',(-21.2235379498319,21.3199172053114,-61.2142481800868));
#12786=CARTESIAN_POINT('Ctrl Pts',(-21.1937515672006,21.3514120494542,-61.2117864113642));
#12787=CARTESIAN_POINT('Ctrl Pts',(-21.0964333316423,21.4585614529659,-61.203504096158));
#12788=CARTESIAN_POINT('Ctrl Pts',(-21.0318428471099,21.5367952855778,-61.197604202909));
#12789=CARTESIAN_POINT('Ctrl Pts',(-20.9426911398844,21.6557926162066,-61.1887364618861));
#12790=CARTESIAN_POINT('Ctrl Pts',(-20.9151692044089,21.6942648482234,-61.1858851418246));
#12791=CARTESIAN_POINT('Ctrl Pts',(-20.8840975042437,21.7397840710182,-61.1825241248383));
#12792=CARTESIAN_POINT('Ctrl Pts',(-20.8797136244607,21.746256794239,-61.1820464903697));
#12793=CARTESIAN_POINT('Ctrl Pts',(-20.8730666668809,21.7561482380885,-61.1813170037548));
#12794=CARTESIAN_POINT('Ctrl Pts',(-20.8707864683667,21.7595554645383,-61.1810657992602));
#12795=CARTESIAN_POINT('Ctrl Pts',(-20.8666574289854,21.7657508983119,-61.1806091622433));
#12796=CARTESIAN_POINT('Ctrl Pts',(-20.8648064135042,21.7685376552369,-61.180403812082));
#12797=CARTESIAN_POINT('Ctrl Pts',(-20.861108115814,21.7741244041445,-61.179992231971));
#12798=CARTESIAN_POINT('Ctrl Pts',(-20.8592608592962,21.7769244081134,-61.1797860013945));
#12799=CARTESIAN_POINT('Ctrl Pts',(-20.8540573776195,21.7848385088804,-61.1792032305848));
#12800=CARTESIAN_POINT('Ctrl Pts',(-20.8507113498022,21.7899592642963,-61.178826308423));
#12801=CARTESIAN_POINT('Ctrl Pts',(-20.8368808354316,21.8112576378784,-61.1772592189583));
#12802=CARTESIAN_POINT('Ctrl Pts',(-20.8265272042747,21.8275193783688,-61.176064178685));
#12803=CARTESIAN_POINT('Ctrl Pts',(-20.6086486206086,22.1766006881929,-61.1504381721112));
#12804=CARTESIAN_POINT('Ctrl Pts',(-20.4634993853836,22.544408513569,-61.1233633556784));
#12805=CARTESIAN_POINT('Ctrl Pts',(-20.3731386491286,23.0043932739609,-61.0921837777148));
#12806=CARTESIAN_POINT('Ctrl Pts',(-20.3610327448102,23.0802589132278,-61.0871448907393));
#12807=CARTESIAN_POINT('Ctrl Pts',(-20.3491325452743,23.1769264523618,-61.0809121059813));
#12808=CARTESIAN_POINT('Ctrl Pts',(-20.3468125973796,23.1973868823462,-61.0796035108678));
#12809=CARTESIAN_POINT('Ctrl Pts',(-20.3438465790326,23.2259916485801,-61.07779014952));
#12810=CARTESIAN_POINT('Ctrl Pts',(-20.3430351848222,23.2341178343324,-61.0772768149464));
#12811=CARTESIAN_POINT('Ctrl Pts',(-20.3418597536872,23.2463604131877,-61.0765062664883));
#12812=CARTESIAN_POINT('Ctrl Pts',(-20.3414727380289,23.2504744906828,-61.0762478055664));
#12813=CARTESIAN_POINT('Ctrl Pts',(-20.340859945409,23.2571258049654,-61.0758307335309));
#12814=CARTESIAN_POINT('Ctrl Pts',(-20.3406292634172,23.25966256857,-61.0756718502347));
#12815=CARTESIAN_POINT('Ctrl Pts',(-20.3401988168299,23.2644591503669,-61.0753717825014));
#12816=CARTESIAN_POINT('Ctrl Pts',(-20.3399984305386,23.2667189089752,-61.0752305631692));
#12817=CARTESIAN_POINT('Ctrl Pts',(-20.3396397844556,23.270812488616,-61.0749750132988));
#12818=CARTESIAN_POINT('Ctrl Pts',(-20.3394807095987,23.272646233295,-61.074860636567));
#12819=CARTESIAN_POINT('Ctrl Pts',(-20.3391674385432,23.2762937745336,-61.0746333238387));
#12820=CARTESIAN_POINT('Ctrl Pts',(-20.339013208611,23.2781075592907,-61.0745203861826));
#12821=CARTESIAN_POINT('Ctrl Pts',(-20.3385943690745,23.2830831546975,-61.0742108363067));
#12822=CARTESIAN_POINT('Ctrl Pts',(-20.338332890962,23.2862452378341,-61.0740144017979));
#12823=CARTESIAN_POINT('Ctrl Pts',(-20.3373468077685,23.2983883706379,-61.0732611441404));
#12824=CARTESIAN_POINT('Ctrl Pts',(-20.3366551891144,23.3073721685507,-61.0727061674145));
#12825=CARTESIAN_POINT('Ctrl Pts',(-20.3255375831517,23.460154333673,-61.0633053450626));
#12826=CARTESIAN_POINT('Ctrl Pts',(-20.3247336543253,23.6045115540161,-61.0549823666806));
#12827=CARTESIAN_POINT('Ctrl Pts',(-20.3369578055946,23.8028982024527,-61.0437356743519));
#12828=CARTESIAN_POINT('Ctrl Pts',(-20.3416941626172,23.8572480287291,-61.0406748536807));
#12829=CARTESIAN_POINT('Ctrl Pts',(-20.3662416448557,24.0748892353054,-61.0284172659998));
#12830=CARTESIAN_POINT('Ctrl Pts',(-20.3971597414454,24.2366723897695,-61.0192903463121));
#12831=CARTESIAN_POINT('Ctrl Pts',(-20.4773336689076,24.5317018087349,-61.0017778432566));
#12832=CARTESIAN_POINT('Ctrl Pts',(-20.523296451582,24.6654215242556,-60.9934906497151));
#12833=CARTESIAN_POINT('Ctrl Pts',(-20.581962124228,24.8054343395217,-60.9842517399167));
#12834=CARTESIAN_POINT('Ctrl Pts',(-20.5860952919551,24.8151640573253,-60.9836067638771));
#12835=CARTESIAN_POINT('Ctrl Pts',(-20.5921102740048,24.8291322952589,-60.9826765070969));
#12836=CARTESIAN_POINT('Ctrl Pts',(-20.5939535136893,24.8333874358137,-60.9823925452525));
#12837=CARTESIAN_POINT('Ctrl Pts',(-20.5971700661699,24.8407691630625,-60.9818989240029));
#12838=CARTESIAN_POINT('Ctrl Pts',(-20.5985391798708,24.8438975805958,-60.9816894087184));
#12839=CARTESIAN_POINT('Ctrl Pts',(-20.6011824346483,24.8499113615375,-60.9812860454844));
#12840=CARTESIAN_POINT('Ctrl Pts',(-20.6024558450807,24.8527970436215,-60.9810922227939));
#12841=CARTESIAN_POINT('Ctrl Pts',(-20.6054674504959,24.8595946231108,-60.9806350083226));
#12842=CARTESIAN_POINT('Ctrl Pts',(-20.6072092043423,24.8635049293154,-60.9803714943829));
#12843=CARTESIAN_POINT('Ctrl Pts',(-20.6123812643214,24.875054442719,-60.9795916868885));
#12844=CARTESIAN_POINT('Ctrl Pts',(-20.6158335404669,24.8826837190019,-60.9790746371937));
#12845=CARTESIAN_POINT('Ctrl Pts',(-20.6465974643968,24.949970264493,-60.9744972704739));
#12846=CARTESIAN_POINT('Ctrl Pts',(-20.6756935485709,25.0087901934689,-60.9703753991033));
#12847=CARTESIAN_POINT('Ctrl Pts',(-20.7164230972664,25.0851686310756,-60.9648559333595));
#12848=CARTESIAN_POINT('Ctrl Pts',(-20.7264633803597,25.103562382356,-60.9635136245565));
#12849=CARTESIAN_POINT('Ctrl Pts',(-20.8622295329458,25.3466182758445,-60.9456012242814));
#12850=CARTESIAN_POINT('Ctrl Pts',(-21.0142424484423,25.5554980766441,-60.9280964250937));
#12851=CARTESIAN_POINT('Ctrl Pts',(-21.2988391175304,25.8617637471296,-60.8998792122918));
#12852=CARTESIAN_POINT('Ctrl Pts',(-21.4169086158251,25.9711622806561,-60.889152410606));
#12853=CARTESIAN_POINT('Ctrl Pts',(-21.5482032102938,26.0757160989634,-60.8785859244094));
#12854=CARTESIAN_POINT('Ctrl Pts',(-21.5537576880001,26.0801094557593,-60.8781413002778));
#12855=CARTESIAN_POINT('Ctrl Pts',(-21.5622560012386,26.086785842045,-60.87746473411));
#12856=CARTESIAN_POINT('Ctrl Pts',(-21.5651893445344,26.0890821011879,-60.8772318754741));
#12857=CARTESIAN_POINT('Ctrl Pts',(-21.5700007702767,26.0928351110924,-60.8768510338781));
#12858=CARTESIAN_POINT('Ctrl Pts',(-21.5718764842327,26.0942948714704,-60.8767028387621));
#12859=CARTESIAN_POINT('Ctrl Pts',(-21.5754975667027,26.0971065252749,-60.8764172783773));
#12860=CARTESIAN_POINT('Ctrl Pts',(-21.577242711934,26.0984587022339,-60.8762798929217));
#12861=CARTESIAN_POINT('Ctrl Pts',(-21.5804347946224,26.1009267531469,-60.8760290342565));
#12862=CARTESIAN_POINT('Ctrl Pts',(-21.5818812858526,26.1020431853049,-60.8759155212058));
#12863=CARTESIAN_POINT('Ctrl Pts',(-21.5848352594108,26.1043191175904,-60.875684042229));
#12864=CARTESIAN_POINT('Ctrl Pts',(-21.586342812897,26.1054785091455,-60.8755660840986));
#12865=CARTESIAN_POINT('Ctrl Pts',(-21.5906891729444,26.1088149804132,-60.8752265099603));
#12866=CARTESIAN_POINT('Ctrl Pts',(-21.5935305909549,26.1109886773902,-60.8750051351621));
#12867=CARTESIAN_POINT('Ctrl Pts',(-21.6060555433122,26.1205373004778,-60.8740320162764));
#12868=CARTESIAN_POINT('Ctrl Pts',(-21.6157773605267,26.1278621890223,-60.8732837754835));
#12869=CARTESIAN_POINT('Ctrl Pts',(-21.7674286975885,26.2407824014019,-60.8617175427094));
#12870=CARTESIAN_POINT('Ctrl Pts',(-21.9177699890985,26.3345669943791,-60.8516735527638));
#12871=CARTESIAN_POINT('Ctrl Pts',(-22.0750360359093,26.4155367851434,-60.8417499040898));
#12872=CARTESIAN_POINT('Origin',(-23.5502525316942,23.5502525316942,-77.3107734492734));
#12873=CARTESIAN_POINT('',(-22.0750359236218,26.4155367273312,-59.3465003279648));
#12874=CARTESIAN_POINT('',(-22.075036024144,26.4155367790859,-59.5958634867516));
#12875=CARTESIAN_POINT('',(-22.0750360153461,26.4155367745563,-77.3107734492734));
#12876=CARTESIAN_POINT('Ctrl Pts',(-22.0750359236218,26.4155367273312,-59.3465003279648));
#12877=CARTESIAN_POINT('Ctrl Pts',(-22.0173772946812,26.3858506783378,-59.350124039512));
#12878=CARTESIAN_POINT('Ctrl Pts',(-21.9606093800186,26.3544214700763,-59.3537501044204));
#12879=CARTESIAN_POINT('Ctrl Pts',(-21.7756671778268,26.2446027838705,-59.3658557842911));
#12880=CARTESIAN_POINT('Ctrl Pts',(-21.6520552993429,26.1589910297971,-59.3744380071984));
#12881=CARTESIAN_POINT('Ctrl Pts',(-21.4892612094151,26.0285278464637,-59.3868125885143));
#12882=CARTESIAN_POINT('Ctrl Pts',(-21.4446571477287,25.9907445260588,-59.3903248505198));
#12883=CARTESIAN_POINT('Ctrl Pts',(-21.3949405127218,25.9462525618812,-59.3943921134696));
#12884=CARTESIAN_POINT('Ctrl Pts',(-21.3887952442959,25.9407103197596,-59.3948975869124));
#12885=CARTESIAN_POINT('Ctrl Pts',(-21.3795669399565,25.9323228966746,-59.3956608194333));
#12886=CARTESIAN_POINT('Ctrl Pts',(-21.3764679690478,25.9294952340751,-59.3959178347945));
#12887=CARTESIAN_POINT('Ctrl Pts',(-21.3711359606365,25.9246109184007,-59.3963612841975));
#12888=CARTESIAN_POINT('Ctrl Pts',(-21.3689002863089,25.9225571411892,-59.3965475955051));
#12889=CARTESIAN_POINT('Ctrl Pts',(-21.3642911099066,25.9183109484524,-59.3969324831774));
#12890=CARTESIAN_POINT('Ctrl Pts',(-21.3619179970227,25.9161181168381,-59.3971310772339));
#12891=CARTESIAN_POINT('Ctrl Pts',(-21.3555131659794,25.910181968417,-59.3976682272017));
#12892=CARTESIAN_POINT('Ctrl Pts',(-21.3514877423232,25.9064319030814,-59.3980070724666));
#12893=CARTESIAN_POINT('Ctrl Pts',(-21.3366204468955,25.8925103232021,-59.3992631942189));
#12894=CARTESIAN_POINT('Ctrl Pts',(-21.3258395218915,25.8822742551436,-59.4001832531385));
#12895=CARTESIAN_POINT('Ctrl Pts',(-21.1474322168789,25.7105207081627,-59.4155643009805));
#12896=CARTESIAN_POINT('Ctrl Pts',(-20.9977551063138,25.5314187016644,-59.4308501551163));
#12897=CARTESIAN_POINT('Ctrl Pts',(-20.7974584960904,25.2309472079449,-59.4551849163107));
#12898=CARTESIAN_POINT('Ctrl Pts',(-20.7326787282184,25.1199300049788,-59.4639211022191));
#12899=CARTESIAN_POINT('Ctrl Pts',(-20.6269721687529,24.9110323577736,-59.4796514581286));
#12900=CARTESIAN_POINT('Ctrl Pts',(-20.5839126175309,24.8144207969308,-59.4866694885227));
#12901=CARTESIAN_POINT('Ctrl Pts',(-20.532087943081,24.6808327378886,-59.4958805012161));
#12902=CARTESIAN_POINT('Ctrl Pts',(-20.5191122908156,24.6455690312495,-59.4982667059051));
#12903=CARTESIAN_POINT('Ctrl Pts',(-20.5051994858254,24.6056159292935,-59.5009131986996));
#12904=CARTESIAN_POINT('Ctrl Pts',(-20.5036531952615,24.6011437901395,-59.5012086345051));
#12905=CARTESIAN_POINT('Ctrl Pts',(-20.5014987947507,24.5948681720328,-59.5016220754089));
#12906=CARTESIAN_POINT('Ctrl Pts',(-20.500882433883,24.5930675638004,-59.5017405695249));
#12907=CARTESIAN_POINT('Ctrl Pts',(-20.4996487926663,24.5894532151962,-59.501978157903));
#12908=CARTESIAN_POINT('Ctrl Pts',(-20.4990315331263,24.5876394658374,-59.5020972509772));
#12909=CARTESIAN_POINT('Ctrl Pts',(-20.4978529019578,24.5841660351013,-59.5023250642661));
#12910=CARTESIAN_POINT('Ctrl Pts',(-20.4972912671452,24.5825064487815,-59.5024338003034));
#12911=CARTESIAN_POINT('Ctrl Pts',(-20.4959729263132,24.5786003687439,-59.5026894650902));
#12912=CARTESIAN_POINT('Ctrl Pts',(-20.4952173437589,24.5763534927951,-59.5028363265975));
#12913=CARTESIAN_POINT('Ctrl Pts',(-20.4929974630942,24.5697280458566,-59.5032687891019));
#12914=CARTESIAN_POINT('Ctrl Pts',(-20.4915400862782,24.5653471358282,-59.5035539805623));
#12915=CARTESIAN_POINT('Ctrl Pts',(-20.4790977572962,24.5276751012545,-59.5059999460248));
#12916=CARTESIAN_POINT('Ctrl Pts',(-20.4686467288547,24.494208277285,-59.5081297389497));
#12917=CARTESIAN_POINT('Ctrl Pts',(-20.4569700849623,24.4545537417697,-59.5106100206929));
#12918=CARTESIAN_POINT('Ctrl Pts',(-20.4552143824401,24.4485263372307,-59.510985846726));
#12919=CARTESIAN_POINT('Ctrl Pts',(-20.4526237822133,24.4395349247291,-59.5115447954053));
#12920=CARTESIAN_POINT('Ctrl Pts',(-20.4517755126702,24.4365748245968,-59.5117285363789));
#12921=CARTESIAN_POINT('Ctrl Pts',(-20.4495975911602,24.4289334659643,-59.5122021620603));
#12922=CARTESIAN_POINT('Ctrl Pts',(-20.4482742929807,24.4242503873013,-59.5124917575672));
#12923=CARTESIAN_POINT('Ctrl Pts',(-20.4255545713473,24.3431449559493,-59.5174959003126));
#12924=CARTESIAN_POINT('Ctrl Pts',(-20.4069760578338,24.2659553555244,-59.5220850525385));
#12925=CARTESIAN_POINT('Ctrl Pts',(-20.3458825187809,23.9634104038351,-59.539675164646));
#12926=CARTESIAN_POINT('Ctrl Pts',(-20.3246116535162,23.734464818389,-59.5521875532458));
#12927=CARTESIAN_POINT('Ctrl Pts',(-20.3297447749188,23.3673664092994,-59.5731410623727));
#12928=CARTESIAN_POINT('Ctrl Pts',(-20.340512009612,23.2298212739769,-59.5811820196773));
#12929=CARTESIAN_POINT('Ctrl Pts',(-20.3631230207747,23.0719289624684,-59.5908230836809));
#12930=CARTESIAN_POINT('Ctrl Pts',(-20.366414161883,23.0504914333308,-59.5921407207343));
#12931=CARTESIAN_POINT('Ctrl Pts',(-20.3709128061222,23.023039046798,-59.5938396567481));
#12932=CARTESIAN_POINT('Ctrl Pts',(-20.3719214988249,23.0169918131557,-59.5942146232688));
#12933=CARTESIAN_POINT('Ctrl Pts',(-20.3735716445329,23.007270011344,-59.5948186130557));
#12934=CARTESIAN_POINT('Ctrl Pts',(-20.3742022358028,23.0035935941069,-59.5950472901148));
#12935=CARTESIAN_POINT('Ctrl Pts',(-20.3754133790688,22.9966053309944,-59.5954824861436));
#12936=CARTESIAN_POINT('Ctrl Pts',(-20.3759927344794,22.9932932804597,-59.5956889667109));
#12937=CARTESIAN_POINT('Ctrl Pts',(-20.3773224531287,22.9857610329246,-59.5961590508852));
#12938=CARTESIAN_POINT('Ctrl Pts',(-20.3780760537248,22.9815414205111,-59.5964227574375));
#12939=CARTESIAN_POINT('Ctrl Pts',(-20.3803890156649,22.9687381612904,-59.5972240105418));
#12940=CARTESIAN_POINT('Ctrl Pts',(-20.3819748058899,22.9601593839527,-59.597762399752));
#12941=CARTESIAN_POINT('Ctrl Pts',(-20.3887032756285,22.9245689526593,-59.600002355265));
#12942=CARTESIAN_POINT('Ctrl Pts',(-20.3941565953864,22.8976178675606,-59.6017138232034));
#12943=CARTESIAN_POINT('Ctrl Pts',(-20.4009929694648,22.8659236237925,-59.6037450658337));
#12944=CARTESIAN_POINT('Ctrl Pts',(-20.4020430041073,22.8611091398961,-59.6040541265554));
#12945=CARTESIAN_POINT('Ctrl Pts',(-20.4040925900449,22.8518140886933,-59.6046517958645));
#12946=CARTESIAN_POINT('Ctrl Pts',(-20.405090681758,22.8473332088307,-59.6049403572815));
#12947=CARTESIAN_POINT('Ctrl Pts',(-20.4078150672725,22.8352242013184,-59.605721357564));
#12948=CARTESIAN_POINT('Ctrl Pts',(-20.4095595525197,22.8276002364154,-59.606214372678));
#12949=CARTESIAN_POINT('Ctrl Pts',(-20.4128871468066,22.8132972279942,-59.6071417321269));
#12950=CARTESIAN_POINT('Ctrl Pts',(-20.4144638787303,22.8066167332564,-59.6075758724975));
#12951=CARTESIAN_POINT('Ctrl Pts',(-20.41739339725,22.7943795843902,-59.6083729590447));
#12952=CARTESIAN_POINT('Ctrl Pts',(-20.418739658501,22.7888213837297,-59.6087356987599));
#12953=CARTESIAN_POINT('Ctrl Pts',(-20.4210526448572,22.7793818356274,-59.6093529319674));
#12954=CARTESIAN_POINT('Ctrl Pts',(-20.422011817887,22.775498636521,-59.6096071889998));
#12955=CARTESIAN_POINT('Ctrl Pts',(-20.4243344821483,22.7661699964826,-59.610218817166));
#12956=CARTESIAN_POINT('Ctrl Pts',(-20.4257049732669,22.7607263263077,-59.6105764049872));
#12957=CARTESIAN_POINT('Ctrl Pts',(-20.4330324768955,22.7319389564394,-59.6124709962302));
#12958=CARTESIAN_POINT('Ctrl Pts',(-20.4392367652285,22.7086595008939,-59.6140155897627));
#12959=CARTESIAN_POINT('Ctrl Pts',(-20.4679670446683,22.6055205132541,-59.6209146518101));
#12960=CARTESIAN_POINT('Ctrl Pts',(-20.4933098080248,22.5264840878987,-59.6263519844875));
#12961=CARTESIAN_POINT('Ctrl Pts',(-20.5800073779294,22.2881593067768,-59.6431854392778));
#12962=CARTESIAN_POINT('Ctrl Pts',(-20.6509843749036,22.132693566,-59.6547961756307));
#12963=CARTESIAN_POINT('Ctrl Pts',(-20.8139310313397,21.8397712074789,-59.6774188571261));
#12964=CARTESIAN_POINT('Ctrl Pts',(-20.9048448057909,21.7022712749116,-59.6884001474609));
#12965=CARTESIAN_POINT('Ctrl Pts',(-21.0105154604079,21.5663396680548,-59.6992062730567));
#12966=CARTESIAN_POINT('Ctrl Pts',(-21.0151733744053,21.5603911518994,-59.6996790319789));
#12967=CARTESIAN_POINT('Ctrl Pts',(-21.0216212961037,21.5522160461993,-59.7003285061988));
#12968=CARTESIAN_POINT('Ctrl Pts',(-21.0233933624769,21.5499754353731,-59.7005064870392));
#12969=CARTESIAN_POINT('Ctrl Pts',(-21.0263900024129,21.5461968037248,-59.7008065920719));
#12970=CARTESIAN_POINT('Ctrl Pts',(-21.0276130041124,21.5446575472947,-59.700928829088));
#12971=CARTESIAN_POINT('Ctrl Pts',(-21.0300261651114,21.5416260689448,-59.7011695402527));
#12972=CARTESIAN_POINT('Ctrl Pts',(-21.0312162416839,21.5401337851218,-59.7012880200473));
#12973=CARTESIAN_POINT('Ctrl Pts',(-21.0338451188819,21.5368433336492,-59.7015492379908));
#12974=CARTESIAN_POINT('Ctrl Pts',(-21.0352845250735,21.5350456460915,-59.701691932395));
#12975=CARTESIAN_POINT('Ctrl Pts',(-21.0403300869684,21.5287580232355,-59.702190965878));
#12976=CARTESIAN_POINT('Ctrl Pts',(-21.0439463771026,21.5242761777013,-59.7025465774121));
#12977=CARTESIAN_POINT('Ctrl Pts',(-21.0811029248206,21.4784779870898,-59.7061796672845));
#12978=CARTESIAN_POINT('Ctrl Pts',(-21.1156520445821,21.4379857814073,-59.7093854868471));
#12979=CARTESIAN_POINT('Ctrl Pts',(-21.1666304013744,21.3811518463552,-59.7139068521463));
#12980=CARTESIAN_POINT('Ctrl Pts',(-21.1822553380077,21.3641048729292,-59.7152659288294));
#12981=CARTESIAN_POINT('Ctrl Pts',(-21.3721402340304,21.1613630841721,-59.7314860823134));
#12982=CARTESIAN_POINT('Ctrl Pts',(-21.5676463071214,20.9967720227785,-59.7452950057434));
#12983=CARTESIAN_POINT('Ctrl Pts',(-21.8875410813069,20.7865755134584,-59.7669743011235));
#12984=CARTESIAN_POINT('Ctrl Pts',(-21.9986615908709,20.7226951837666,-59.7743510430123));
#12985=CARTESIAN_POINT('Ctrl Pts',(-22.1615829599092,20.641536920671,-59.785170828009));
#12986=CARTESIAN_POINT('Ctrl Pts',(-22.2104800701052,20.6186934063143,-59.7884176983647));
#12987=CARTESIAN_POINT('Ctrl Pts',(-22.2673669239226,20.5938378066815,-59.7922026749949));
#12988=CARTESIAN_POINT('Ctrl Pts',(-22.2748205622714,20.5906145811383,-59.7926987466116));
#12989=CARTESIAN_POINT('Ctrl Pts',(-22.2861136737287,20.5857816105326,-59.79345059514));
#12990=CARTESIAN_POINT('Ctrl Pts',(-22.2899442533509,20.5841510604171,-59.7937056614641));
#12991=CARTESIAN_POINT('Ctrl Pts',(-22.2965696188065,20.5813460146907,-59.7941469008554));
#12992=CARTESIAN_POINT('Ctrl Pts',(-22.2993629288236,20.580168028839,-59.7943329547171));
#12993=CARTESIAN_POINT('Ctrl Pts',(-22.3051490847142,20.5777375199939,-59.7947184035978));
#12994=CARTESIAN_POINT('Ctrl Pts',(-22.3081421672274,20.5764855719579,-59.7949178179378));
#12995=CARTESIAN_POINT('Ctrl Pts',(-22.3154024569013,20.5734616078253,-59.7954016057109));
#12996=CARTESIAN_POINT('Ctrl Pts',(-22.3196715856441,20.5716942484779,-59.7956861370568));
#12997=CARTESIAN_POINT('Ctrl Pts',(-22.3356022460903,20.5651392743798,-59.7967481231989));
#12998=CARTESIAN_POINT('Ctrl Pts',(-22.3472879177742,20.5604109630301,-59.7975275855451));
#12999=CARTESIAN_POINT('Ctrl Pts',(-22.5467118902965,20.4810775042744,-59.8108383730785));
#13000=CARTESIAN_POINT('Ctrl Pts',(-22.7409909711201,20.424233167802,-59.8239812598038));
#13001=CARTESIAN_POINT('Ctrl Pts',(-23.2295720225636,20.3298964066313,-59.8573012705182));
#13002=CARTESIAN_POINT('Ctrl Pts',(-23.5261978870492,20.3140568723038,-59.8778263065868));
#13003=CARTESIAN_POINT('Ctrl Pts',(-23.8290318680961,20.3395723205871,-59.8969911380142));
#13004=CARTESIAN_POINT('Ctrl Pts',(-23.8372327183176,20.340294944383,-59.8975086596434));
#13005=CARTESIAN_POINT('Ctrl Pts',(-23.8514210754071,20.3415999706347,-59.898401380229));
#13006=CARTESIAN_POINT('Ctrl Pts',(-23.8574098409415,20.3421677232635,-59.8987773716775));
#13007=CARTESIAN_POINT('Ctrl Pts',(-23.8659813534834,20.3430045500236,-59.8993143109849));
#13008=CARTESIAN_POINT('Ctrl Pts',(-23.868565373045,20.3432599779168,-59.8994760231683));
#13009=CARTESIAN_POINT('Ctrl Pts',(-23.8730522516803,20.3437089780271,-59.899756543793));
#13010=CARTESIAN_POINT('Ctrl Pts',(-23.8749552498663,20.3439011214975,-59.8998754335152));
#13011=CARTESIAN_POINT('Ctrl Pts',(-23.878604846555,20.3442728994038,-59.9001032753092));
#13012=CARTESIAN_POINT('Ctrl Pts',(-23.8803514664438,20.3444522667605,-59.9002122425116));
#13013=CARTESIAN_POINT('Ctrl Pts',(-23.8844705725032,20.3448786762148,-59.9004690526229));
#13014=CARTESIAN_POINT('Ctrl Pts',(-23.886842936682,20.3451269254895,-59.9006168267895));
#13015=CARTESIAN_POINT('Ctrl Pts',(-23.8938635855557,20.3458694620634,-59.9010537526299));
#13016=CARTESIAN_POINT('Ctrl Pts',(-23.8985110984906,20.3463712316807,-59.9013424827232));
#13017=CARTESIAN_POINT('Ctrl Pts',(-23.9395100435417,20.3508879548782,-59.9038852438706));
#13018=CARTESIAN_POINT('Ctrl Pts',(-23.9757936397396,20.3555115172861,-59.9061055304805));
#13019=CARTESIAN_POINT('Ctrl Pts',(-24.0154195319105,20.3612481079009,-59.9085051064685));
#13020=CARTESIAN_POINT('Ctrl Pts',(-24.0188457588702,20.3617497575513,-59.9087123771234));
#13021=CARTESIAN_POINT('Ctrl Pts',(-24.3042021182704,20.4039999804145,-59.9259583351109));
#13022=CARTESIAN_POINT('Ctrl Pts',(-24.5793887752279,20.4829618592487,-59.9413170874108));
#13023=CARTESIAN_POINT('Ctrl Pts',(-25.0067341873305,20.6696904647225,-59.9676834281384));
#13024=CARTESIAN_POINT('Ctrl Pts',(-25.166395609331,20.756143809207,-59.9781710891231));
#13025=CARTESIAN_POINT('Ctrl Pts',(-25.329147680033,20.8629063402261,-59.9899946634912));
#13026=CARTESIAN_POINT('Ctrl Pts',(-25.3403177347086,20.8703338646422,-59.9908120852706));
#13027=CARTESIAN_POINT('Ctrl Pts',(-25.3556755254798,20.8806848788377,-59.9919443240949));
#13028=CARTESIAN_POINT('Ctrl Pts',(-25.3599032793545,20.8835489841125,-59.9922568923907));
#13029=CARTESIAN_POINT('Ctrl Pts',(-25.3670217852286,20.8883961623719,-59.9927846769584));
#13030=CARTESIAN_POINT('Ctrl Pts',(-25.3699161511782,20.8903739323477,-59.9929996914498));
#13031=CARTESIAN_POINT('Ctrl Pts',(-25.3756316117088,20.8942930997055,-59.9934251086096));
#13032=CARTESIAN_POINT('Ctrl Pts',(-25.3784528505917,20.896234279316,-59.9936355027935));
#13033=CARTESIAN_POINT('Ctrl Pts',(-25.3846574087252,20.9005179706721,-59.9940990966014));
#13034=CARTESIAN_POINT('Ctrl Pts',(-25.3880393425899,20.9028624708601,-59.9943523720317));
#13035=CARTESIAN_POINT('Ctrl Pts',(-25.3998000234784,20.911048869701,-59.9952351785167));
#13036=CARTESIAN_POINT('Ctrl Pts',(-25.4081554139133,20.9169240732162,-59.9958659852791));
#13037=CARTESIAN_POINT('Ctrl Pts',(-25.4918449343839,20.9763680446748,-60.0022210463195));
#13038=CARTESIAN_POINT('Ctrl Pts',(-25.564862227215,21.0331098364371,-60.0080681703204));
#13039=CARTESIAN_POINT('Ctrl Pts',(-25.8625881822234,21.2857332249386,-60.033265499888));
#13040=CARTESIAN_POINT('Ctrl Pts',(-26.0619745368346,21.509140078756,-60.0537745390458));
#13041=CARTESIAN_POINT('Ctrl Pts',(-26.2938834700108,21.8553453428623,-60.0816122387195));
#13042=CARTESIAN_POINT('Ctrl Pts',(-26.3544812706904,21.9576039424041,-60.0894035845731));
#13043=CARTESIAN_POINT('Ctrl Pts',(-26.4122045720747,22.0685684679297,-60.0972425865282));
#13044=CARTESIAN_POINT('Ctrl Pts',(-26.4150917408016,22.0741585462706,-60.0976358944136));
#13045=CARTESIAN_POINT('Ctrl Pts',(-26.4191728718421,22.0821174287764,-60.0981935588825));
#13046=CARTESIAN_POINT('Ctrl Pts',(-26.4203802847927,22.0844792615227,-60.0983587600566));
#13047=CARTESIAN_POINT('Ctrl Pts',(-26.4224535132973,22.088547108621,-60.0986427911945));
#13048=CARTESIAN_POINT('Ctrl Pts',(-26.4233207268836,22.0902524055211,-60.0987617101218));
#13049=CARTESIAN_POINT('Ctrl Pts',(-26.4249806749187,22.0935237491325,-60.0989895469787));
#13050=CARTESIAN_POINT('Ctrl Pts',(-26.4257736471919,22.0950896687285,-60.0990984801395));
#13051=CARTESIAN_POINT('Ctrl Pts',(-26.4276402372848,22.0987831956224,-60.0993551221038));
#13052=CARTESIAN_POINT('Ctrl Pts',(-26.4287127770296,22.1009113510366,-60.0995027623849));
#13053=CARTESIAN_POINT('Ctrl Pts',(-26.4318782871194,22.1072097950077,-60.0999390323621));
#13054=CARTESIAN_POINT('Ctrl Pts',(-26.433964573851,22.1113834644054,-60.1002272422594));
#13055=CARTESIAN_POINT('Ctrl Pts',(-26.4522220110156,22.148107136472,-60.1027555306236));
#13056=CARTESIAN_POINT('Ctrl Pts',(-26.4678513356023,22.1809256676392,-60.1049622855749));
#13057=CARTESIAN_POINT('Ctrl Pts',(-26.4875046542662,22.2240588660547,-60.1078034809899));
#13058=CARTESIAN_POINT('Ctrl Pts',(-26.4920347311562,22.2341381111733,-60.1084632455988));
#13059=CARTESIAN_POINT('Ctrl Pts',(-26.4970653730707,22.2454868444057,-60.1092016646997));
#13060=CARTESIAN_POINT('Ctrl Pts',(-26.4976170187264,22.2467334480492,-60.1092827164232));
#13061=CARTESIAN_POINT('Ctrl Pts',(-26.5019604704807,22.2565655928052,-60.1099215126411));
#13062=CARTESIAN_POINT('Ctrl Pts',(-26.5057155851707,22.2651674002527,-60.1104775456415));
#13063=CARTESIAN_POINT('Ctrl Pts',(-26.5117820533869,22.2792310427963,-60.1113822254147));
#13064=CARTESIAN_POINT('Ctrl Pts',(-26.5141159779098,22.2846830131811,-60.1117318594899));
#13065=CARTESIAN_POINT('Ctrl Pts',(-26.5188165865334,22.2957478011878,-60.112439320364));
#13066=CARTESIAN_POINT('Ctrl Pts',(-26.5211824337836,22.3013609493878,-60.1127971108396));
#13067=CARTESIAN_POINT('Ctrl Pts',(-26.5695746344609,22.4170907223686,-60.1201518664266));
#13068=CARTESIAN_POINT('Ctrl Pts',(-26.609468438359,22.5296820879871,-60.1268991887596));
#13069=CARTESIAN_POINT('Ctrl Pts',(-26.6906262705954,22.8067216855026,-60.1430863782956));
#13070=CARTESIAN_POINT('Ctrl Pts',(-26.7253460501128,22.9727018429127,-60.1524562065995));
#13071=CARTESIAN_POINT('Ctrl Pts',(-26.7642594881813,23.2763815102056,-60.1699360504974));
#13072=CARTESIAN_POINT('Ctrl Pts',(-26.7729877313807,23.4130779017761,-60.1779220034576));
#13073=CARTESIAN_POINT('Ctrl Pts',(-26.7730047994707,23.571070348832,-60.1874722551341));
#13074=CARTESIAN_POINT('Ctrl Pts',(-26.7727985692626,23.592235427216,-60.188758054415));
#13075=CARTESIAN_POINT('Ctrl Pts',(-26.7722595413803,23.6197410970653,-60.1904378740434));
#13076=CARTESIAN_POINT('Ctrl Pts',(-26.772116469424,23.6260852227331,-60.190825930829));
#13077=CARTESIAN_POINT('Ctrl Pts',(-26.7718583211161,23.6362058631113,-60.1914459760378));
#13078=CARTESIAN_POINT('Ctrl Pts',(-26.7717553387269,23.63998269221,-60.1916775843502));
#13079=CARTESIAN_POINT('Ctrl Pts',(-26.7715581395575,23.6467763815224,-60.1920945947429));
#13080=CARTESIAN_POINT('Ctrl Pts',(-26.7714663255739,23.649793311557,-60.1922799211158));
#13081=CARTESIAN_POINT('Ctrl Pts',(-26.7712414441191,23.6568563655759,-60.1927141284065));
#13082=CARTESIAN_POINT('Ctrl Pts',(-26.7711049909629,23.6609023701423,-60.1929631154232));
#13083=CARTESIAN_POINT('Ctrl Pts',(-26.770691293151,23.6725192104432,-60.1936787432422));
#13084=CARTESIAN_POINT('Ctrl Pts',(-26.7703949770755,23.6800893019452,-60.1941459824795));
#13085=CARTESIAN_POINT('Ctrl Pts',(-26.7682767490844,23.7297256118591,-60.19721561773));
#13086=CARTESIAN_POINT('Ctrl Pts',(-26.7656573484119,23.7717520655879,-60.1998429676425));
#13087=CARTESIAN_POINT('Ctrl Pts',(-26.755477368879,23.8958604127444,-60.2076902056564));
#13088=CARTESIAN_POINT('Ctrl Pts',(-26.7455909387516,23.977711981398,-60.2129812406296));
#13089=CARTESIAN_POINT('Ctrl Pts',(-26.6857718821446,24.3518276798081,-60.2376999764782));
#13090=CARTESIAN_POINT('Ctrl Pts',(-26.598809266847,24.6366520507987,-60.2582056246918));
#13091=CARTESIAN_POINT('Ctrl Pts',(-26.4354853541177,24.9890052290981,-60.2839142862488));
#13092=CARTESIAN_POINT('Ctrl Pts',(-26.3932447932339,25.0707710293686,-60.289890800783));
#13093=CARTESIAN_POINT('Ctrl Pts',(-26.3443587414358,25.1562194005458,-60.2960624935213));
#13094=CARTESIAN_POINT('Ctrl Pts',(-26.3411416456934,25.1618036634371,-60.2964654772798));
#13095=CARTESIAN_POINT('Ctrl Pts',(-26.3366619136796,25.1695259746961,-60.297022223029));
#13096=CARTESIAN_POINT('Ctrl Pts',(-26.3354135530036,25.1716722221841,-60.2971769016029));
#13097=CARTESIAN_POINT('Ctrl Pts',(-26.3332653111698,25.1753557914515,-60.297442273519));
#13098=CARTESIAN_POINT('Ctrl Pts',(-26.3323666359851,25.1768938094011,-60.2975530453968));
#13099=CARTESIAN_POINT('Ctrl Pts',(-26.3305093130978,25.1800664422091,-60.2977814828632));
#13100=CARTESIAN_POINT('Ctrl Pts',(-26.3295505007262,25.1817009534339,-60.2978991367286));
#13101=CARTESIAN_POINT('Ctrl Pts',(-26.3272988317732,25.1855316835662,-60.2981747965668));
#13102=CARTESIAN_POINT('Ctrl Pts',(-26.3260048073851,25.1877272220128,-60.2983327259834));
#13103=CARTESIAN_POINT('Ctrl Pts',(-26.3218055176039,25.1948327691431,-60.298843649404));
#13104=CARTESIAN_POINT('Ctrl Pts',(-26.3188897972028,25.1997366341733,-60.2991959629041));
#13105=CARTESIAN_POINT('Ctrl Pts',(-26.2439788408215,25.3249689503363,-60.3081862023098));
#13106=CARTESIAN_POINT('Ctrl Pts',(-26.1642085689124,25.440497239046,-60.3163174272702));
#13107=CARTESIAN_POINT('Ctrl Pts',(-25.9684216888671,25.6878367757681,-60.3342158289763));
#13108=CARTESIAN_POINT('Ctrl Pts',(-25.8486691711063,25.8161061001435,-60.3438666105886));
#13109=CARTESIAN_POINT('Ctrl Pts',(-25.57808522971,26.0622933616988,-60.3645060287927));
#13110=CARTESIAN_POINT('Ctrl Pts',(-25.4260072723916,26.1777955466537,-60.3755059068929));
#13111=CARTESIAN_POINT('Ctrl Pts',(-25.253945890953,26.2858887857408,-60.3878533271851));
#13112=CARTESIAN_POINT('Ctrl Pts',(-25.2432221417095,26.2925381968471,-60.3886223592442));
#13113=CARTESIAN_POINT('Ctrl Pts',(-25.2285170554604,26.3015371620069,-60.3896762934858));
#13114=CARTESIAN_POINT('Ctrl Pts',(-25.2245692029949,26.3039414416058,-60.3899591817206));
#13115=CARTESIAN_POINT('Ctrl Pts',(-25.2178411971761,26.3080190436573,-60.3904411891045));
#13116=CARTESIAN_POINT('Ctrl Pts',(-25.2150636556672,26.3096966809984,-60.390640149753));
#13117=CARTESIAN_POINT('Ctrl Pts',(-25.2096864230587,26.3129334600724,-60.391025279687));
#13118=CARTESIAN_POINT('Ctrl Pts',(-25.2070870559778,26.3144931346225,-60.3912114291561));
#13119=CARTESIAN_POINT('Ctrl Pts',(-25.2009136280183,26.3181854842478,-60.3916534761466));
#13120=CARTESIAN_POINT('Ctrl Pts',(-25.1973376352752,26.3203149039257,-60.3919094922262));
#13121=CARTESIAN_POINT('Ctrl Pts',(-25.187389247819,26.3262128600497,-60.392621616398));
#13122=CARTESIAN_POINT('Ctrl Pts',(-25.1810080070895,26.3299663568729,-60.3930782715522));
#13123=CARTESIAN_POINT('Ctrl Pts',(-25.1663696653526,26.3385089919616,-60.3941255610623));
#13124=CARTESIAN_POINT('Ctrl Pts',(-25.1581041365088,26.3432834824119,-60.3947167229978));
#13125=CARTESIAN_POINT('Ctrl Pts',(-25.0893885365455,26.3825701740473,-60.3996299771872));
#13126=CARTESIAN_POINT('Ctrl Pts',(-25.0278601885118,26.4151499580849,-60.4040211240789));
#13127=CARTESIAN_POINT('Ctrl Pts',(-24.8978192591042,26.4787039343361,-60.4132943285966));
#13128=CARTESIAN_POINT('Ctrl Pts',(-24.8291807819336,26.5093241518804,-60.418184891596));
#13129=CARTESIAN_POINT('Ctrl Pts',(-24.5069543350152,26.6397659697369,-60.4411058036661));
#13130=CARTESIAN_POINT('Ctrl Pts',(-24.2424546628898,26.7095571241782,-60.459933690785));
#13131=CARTESIAN_POINT('Ctrl Pts',(-23.8870817229542,26.7565058974879,-60.4836035599354));
#13132=CARTESIAN_POINT('Ctrl Pts',(-23.8013906742619,26.7643538537402,-60.4891789756621));
#13133=CARTESIAN_POINT('Ctrl Pts',(-23.7091400280099,26.7690896859965,-60.4949693496883));
#13134=CARTESIAN_POINT('Ctrl Pts',(-23.7027991443989,26.7693964233187,-60.49536627816));
#13135=CARTESIAN_POINT('Ctrl Pts',(-23.693992967616,26.769796340248,-60.4959159982108));
#13136=CARTESIAN_POINT('Ctrl Pts',(-23.6915284654991,26.7699054258342,-60.49606967668));
#13137=CARTESIAN_POINT('Ctrl Pts',(-23.6872884155098,26.7700882242422,-60.4963337833273));
#13138=CARTESIAN_POINT('Ctrl Pts',(-23.6855129323779,26.7701632982374,-60.4964442883717));
#13139=CARTESIAN_POINT('Ctrl Pts',(-23.6818415228435,26.7703154969747,-60.496672613077));
#13140=CARTESIAN_POINT('Ctrl Pts',(-23.6799455938099,26.770392415708,-60.496790420385));
#13141=CARTESIAN_POINT('Ctrl Pts',(-23.6754879096935,26.7705693228126,-60.4970671733987));
#13142=CARTESIAN_POINT('Ctrl Pts',(-23.6729260943449,26.7706679291543,-60.4972260407615));
#13143=CARTESIAN_POINT('Ctrl Pts',(-23.6650823217219,26.7709604691473,-60.4977119126421));
#13144=CARTESIAN_POINT('Ctrl Pts',(-23.6597999689935,26.771144467009,-60.4980383592537));
#13145=CARTESIAN_POINT('Ctrl Pts',(-23.6091585005105,26.7727837125394,-60.5011608790759));
#13146=CARTESIAN_POINT('Ctrl Pts',(-23.5637710429255,26.7732937804024,-60.5039048788171));
#13147=CARTESIAN_POINT('Ctrl Pts',(-23.4316856831945,26.7719876234891,-60.5117707696838));
#13148=CARTESIAN_POINT('Ctrl Pts',(-23.3450491470703,26.7676317440791,-60.516780522324));
#13149=CARTESIAN_POINT('Ctrl Pts',(-22.9996077453542,26.7362506787536,-60.5365195067012));
#13150=CARTESIAN_POINT('Ctrl Pts',(-22.7443348990544,26.6814339857662,-60.5506546108481));
#13151=CARTESIAN_POINT('Ctrl Pts',(-22.3876945332645,26.5582915452666,-60.5724532544106));
#13152=CARTESIAN_POINT('Ctrl Pts',(-22.2791458531908,26.5140546117124,-60.5793712569388));
#13153=CARTESIAN_POINT('Ctrl Pts',(-22.1636614016266,26.4594784025496,-60.5871435566016));
#13154=CARTESIAN_POINT('Ctrl Pts',(-22.1540914150784,26.4548978218904,-60.5877907738047));
#13155=CARTESIAN_POINT('Ctrl Pts',(-22.1406816849293,26.448397803392,-60.5887021543608));
#13156=CARTESIAN_POINT('Ctrl Pts',(-22.1368228185175,26.4465177877668,-60.5889649423587));
#13157=CARTESIAN_POINT('Ctrl Pts',(-22.1301323527134,26.4432416790613,-60.5894214757179));
#13158=CARTESIAN_POINT('Ctrl Pts',(-22.1272990203828,26.4418491207902,-60.5896150973198));
#13159=CARTESIAN_POINT('Ctrl Pts',(-22.1214074079428,26.4389426881056,-60.5900183087608));
#13160=CARTESIAN_POINT('Ctrl Pts',(-22.1183494786592,26.4374281158915,-60.590227922842));
#13161=CARTESIAN_POINT('Ctrl Pts',(-22.1111535680511,26.4338497846713,-60.5907219782565));
#13162=CARTESIAN_POINT('Ctrl Pts',(-22.1070176196294,26.4317819750241,-60.591006561504));
#13163=CARTESIAN_POINT('Ctrl Pts',(-22.0937172089254,26.4250964799109,-60.5919237277604));
#13164=CARTESIAN_POINT('Ctrl Pts',(-22.0845704170188,26.420443955255,-60.5925575356074));
#13165=CARTESIAN_POINT('Ctrl Pts',(-22.0753093910179,26.4156775120256,-60.5932024084344));
#13166=CARTESIAN_POINT('Ctrl Pts',(-22.0751727006468,26.4156071481723,-60.5932119272902));
#13167=CARTESIAN_POINT('Ctrl Pts',(-22.0750360153461,26.4155367745563,-60.593221446491));
#13168=CARTESIAN_POINT('Ctrl Pts',(-22.0750360359093,26.4155367851434,-60.8417499040898));
#13169=CARTESIAN_POINT('Ctrl Pts',(-22.0927192681594,26.4246411509259,-60.8406340740182));
#13170=CARTESIAN_POINT('Ctrl Pts',(-22.1104900562006,26.4335835030538,-60.839519893482));
#13171=CARTESIAN_POINT('Ctrl Pts',(-22.2568456387877,26.5055392472628,-60.8303944504889));
#13172=CARTESIAN_POINT('Ctrl Pts',(-22.3894109364369,26.5600808014567,-60.8224390301533));
#13173=CARTESIAN_POINT('Ctrl Pts',(-22.6334616486051,26.6419610843305,-60.8077854404577));
#13174=CARTESIAN_POINT('Ctrl Pts',(-22.7436098978314,26.6725099112073,-60.8011705620584));
#13175=CARTESIAN_POINT('Ctrl Pts',(-22.90431647976,26.7080081401775,-60.7913698206017));
#13176=CARTESIAN_POINT('Ctrl Pts',(-22.9537383935735,26.7177159198882,-60.7883365259711));
#13177=CARTESIAN_POINT('Ctrl Pts',(-23.0111952847516,26.7276096049513,-60.7847813656634));
#13178=CARTESIAN_POINT('Ctrl Pts',(-23.0190300153356,26.7289288792939,-60.7842959788782));
#13179=CARTESIAN_POINT('Ctrl Pts',(-23.0309413614435,26.7308893390389,-60.7835570786854));
#13180=CARTESIAN_POINT('Ctrl Pts',(-23.0350145018689,26.731551694639,-60.7833042390555));
#13181=CARTESIAN_POINT('Ctrl Pts',(-23.042393777088,26.7327371352749,-60.7828458609202));
#13182=CARTESIAN_POINT('Ctrl Pts',(-23.0456994810719,26.7332628969978,-60.782640407828));
#13183=CARTESIAN_POINT('Ctrl Pts',(-23.0523048490332,26.7343029113359,-60.7822296493488));
#13184=CARTESIAN_POINT('Ctrl Pts',(-23.0556045052754,26.7348171871207,-60.7820243449691));
#13185=CARTESIAN_POINT('Ctrl Pts',(-23.0648771112009,26.736247632011,-60.7814470822878));
#13186=CARTESIAN_POINT('Ctrl Pts',(-23.0708518238472,26.7371521282585,-60.7810747537788));
#13187=CARTESIAN_POINT('Ctrl Pts',(-23.0953239310677,26.7407865210537,-60.7795481549777));
#13188=CARTESIAN_POINT('Ctrl Pts',(-23.1138420805997,26.7433721760827,-60.7783893194858));
#13189=CARTESIAN_POINT('Ctrl Pts',(-23.4383956353691,26.7858130160086,-60.7580125553829));
#13190=CARTESIAN_POINT('Ctrl Pts',(-23.7485055184797,26.7816558253434,-60.7372695635844));
#13191=CARTESIAN_POINT('Ctrl Pts',(-24.2333667577107,26.7050495521258,-60.7040649850076));
#13192=CARTESIAN_POINT('Ctrl Pts',(-24.4108199851544,26.6613343871955,-60.6918006109792));
#13193=CARTESIAN_POINT('Ctrl Pts',(-24.5907718854211,26.6004154369603,-60.6798320249399));
#13194=CARTESIAN_POINT('Ctrl Pts',(-24.5978965488266,26.5979756638311,-60.6793589805478));
#13195=CARTESIAN_POINT('Ctrl Pts',(-24.6086933441368,26.5942360700172,-60.6786434343658));
#13196=CARTESIAN_POINT('Ctrl Pts',(-24.6123717192506,26.5929545491167,-60.6783998853275));
#13197=CARTESIAN_POINT('Ctrl Pts',(-24.6183581414582,26.590856741734,-60.6780039056552));
#13198=CARTESIAN_POINT('Ctrl Pts',(-24.6206675841346,26.5900444935438,-60.677851238634));
#13199=CARTESIAN_POINT('Ctrl Pts',(-24.6251060742812,26.5884777581261,-60.6775580137381));
#13200=CARTESIAN_POINT('Ctrl Pts',(-24.6272352572321,26.5877236629986,-60.6774174326741));
#13201=CARTESIAN_POINT('Ctrl Pts',(-24.6310881323303,26.586354525411,-60.6771631933103));
#13202=CARTESIAN_POINT('Ctrl Pts',(-24.6328120889593,26.5857402547598,-60.6770494892484));
#13203=CARTESIAN_POINT('Ctrl Pts',(-24.6365584671785,26.5844017685712,-60.6768025146374));
#13204=CARTESIAN_POINT('Ctrl Pts',(-24.6385806829775,26.5836770012168,-60.6766692780056));
#13205=CARTESIAN_POINT('Ctrl Pts',(-24.6440286018754,26.5817183040162,-60.6763105324101));
#13206=CARTESIAN_POINT('Ctrl Pts',(-24.6474529539174,26.5804805848686,-60.6760852503993));
#13207=CARTESIAN_POINT('Ctrl Pts',(-24.6632263122969,26.5747491207523,-60.6750484933949));
#13208=CARTESIAN_POINT('Ctrl Pts',(-24.6755500875459,26.5701855902724,-60.6742411414979));
#13209=CARTESIAN_POINT('Ctrl Pts',(-24.8877205342354,26.4901391111063,-60.660382017347));
#13210=CARTESIAN_POINT('Ctrl Pts',(-25.0796376890542,26.3950311487297,-60.6484486051454));
#13211=CARTESIAN_POINT('Ctrl Pts',(-25.3307970859547,26.2377437785704,-60.6318868911879));
#13212=CARTESIAN_POINT('Ctrl Pts',(-25.3991285103761,26.1912003640066,-60.627275931628));
#13213=CARTESIAN_POINT('Ctrl Pts',(-25.5431664239775,26.0847574855856,-60.6171916598343));
#13214=CARTESIAN_POINT('Ctrl Pts',(-25.6181218344529,26.0239816917159,-60.6117075773721));
#13215=CARTESIAN_POINT('Ctrl Pts',(-25.7630241788694,25.8952975022938,-60.6004635560897));
#13216=CARTESIAN_POINT('Ctrl Pts',(-25.8328401377376,25.8273966358836,-60.5947073357034));
#13217=CARTESIAN_POINT('Ctrl Pts',(-25.9114499434178,25.7436905866326,-60.5877495252233));
#13218=CARTESIAN_POINT('Ctrl Pts',(-25.9233237799796,25.7308388174674,-60.5866849576331));
#13219=CARTESIAN_POINT('Ctrl Pts',(-25.9389019295051,25.7136997114076,-60.5852698408547));
#13220=CARTESIAN_POINT('Ctrl Pts',(-25.9427005892125,25.7094982186185,-60.584923298994));
#13221=CARTESIAN_POINT('Ctrl Pts',(-25.9489128860062,25.7025906128873,-60.584354135557));
#13222=CARTESIAN_POINT('Ctrl Pts',(-25.9513330781396,25.6998903896631,-60.5841317909482));
#13223=CARTESIAN_POINT('Ctrl Pts',(-25.9560093564078,25.6946552873362,-60.5837009933367));
#13224=CARTESIAN_POINT('Ctrl Pts',(-25.9582660070903,25.6921209170605,-60.5834925644841));
#13225=CARTESIAN_POINT('Ctrl Pts',(-25.9634602903801,25.6862688034178,-60.5830115664395));
#13226=CARTESIAN_POINT('Ctrl Pts',(-25.9663950863062,25.6829485614017,-60.5827388789108));
#13227=CARTESIAN_POINT('Ctrl Pts',(-25.9755075467889,25.6725963508094,-60.5818893097434));
#13228=CARTESIAN_POINT('Ctrl Pts',(-25.9816613887912,25.6655435616574,-60.5813114360234));
#13229=CARTESIAN_POINT('Ctrl Pts',(-26.0336203652701,25.6054681594473,-60.5763967421438));
#13230=CARTESIAN_POINT('Ctrl Pts',(-26.0777126612788,25.5509951743469,-60.5719898312863));
#13231=CARTESIAN_POINT('Ctrl Pts',(-26.1249876428917,25.4885314563594,-60.5669843921494));
#13232=CARTESIAN_POINT('Ctrl Pts',(-26.1299576138408,25.4819118623706,-60.5664545329812));
#13233=CARTESIAN_POINT('Ctrl Pts',(-26.1678212242771,25.4310738845209,-60.5623897662699));
#13234=CARTESIAN_POINT('Ctrl Pts',(-26.1995996749937,25.3860395513904,-60.5588148302716));
#13235=CARTESIAN_POINT('Ctrl Pts',(-26.3843285365374,25.1094611493674,-60.5370197063914));
#13236=CARTESIAN_POINT('Ctrl Pts',(-26.5079799767612,24.8598079628611,-60.5178710316903));
#13237=CARTESIAN_POINT('Ctrl Pts',(-26.6215600516023,24.5292256698858,-60.4946706302153));
#13238=CARTESIAN_POINT('Ctrl Pts',(-26.6426989019656,24.4602499775515,-60.4899486008065));
#13239=CARTESIAN_POINT('Ctrl Pts',(-26.6692963748976,24.3617791346785,-60.483426596055));
#13240=CARTESIAN_POINT('Ctrl Pts',(-26.6766849165052,24.3328320001674,-60.4815357431533));
#13241=CARTESIAN_POINT('Ctrl Pts',(-26.6847227585383,24.2994082059577,-60.4793860443901));
#13242=CARTESIAN_POINT('Ctrl Pts',(-26.6857661524543,24.2950291168983,-60.4791050574206));
#13243=CARTESIAN_POINT('Ctrl Pts',(-26.6873318084808,24.2883965044521,-60.4786804860559));
#13244=CARTESIAN_POINT('Ctrl Pts',(-26.6878608199647,24.2861446045012,-60.4785365127102));
#13245=CARTESIAN_POINT('Ctrl Pts',(-26.6888122277527,24.2820749687091,-60.4782766458007));
#13246=CARTESIAN_POINT('Ctrl Pts',(-26.6892354686168,24.2802574404497,-60.4781607034631));
#13247=CARTESIAN_POINT('Ctrl Pts',(-26.6901443653973,24.2763389487156,-60.4779109885361));
#13248=CARTESIAN_POINT('Ctrl Pts',(-26.6906294901014,24.2742378709857,-60.4777772472806));
#13249=CARTESIAN_POINT('Ctrl Pts',(-26.6919359630255,24.2685535091901,-60.4774158315639));
#13250=CARTESIAN_POINT('Ctrl Pts',(-26.6927532925958,24.2649692902955,-60.477188389835));
#13251=CARTESIAN_POINT('Ctrl Pts',(-26.6965384370844,24.2482383535136,-60.4761287485988));
#13252=CARTESIAN_POINT('Ctrl Pts',(-26.6994299538781,24.2350742490567,-60.4753008959832));
#13253=CARTESIAN_POINT('Ctrl Pts',(-26.74906901666,24.002119477145,-60.4607486871998));
#13254=CARTESIAN_POINT('Ctrl Pts',(-26.7727935821034,23.7780118663693,-60.4482581935681));
#13255=CARTESIAN_POINT('Ctrl Pts',(-26.7732463754423,23.2876823900882,-60.4208610712342));
#13256=CARTESIAN_POINT('Ctrl Pts',(-26.7406739381063,23.0231686516336,-60.4059680650802));
#13257=CARTESIAN_POINT('Ctrl Pts',(-26.6719080673939,22.7492082193554,-60.3888514686056));
#13258=CARTESIAN_POINT('Ctrl Pts',(-26.6676488242134,22.7327896199245,-60.3878194777504));
#13259=CARTESIAN_POINT('Ctrl Pts',(-26.6617572843645,22.7107946837967,-60.3864284225943));
#13260=CARTESIAN_POINT('Ctrl Pts',(-26.6602391777089,22.7051878210366,-60.3860730707556));
#13261=CARTESIAN_POINT('Ctrl Pts',(-26.6578368700494,22.6964094649833,-60.385515530349));
#13262=CARTESIAN_POINT('Ctrl Pts',(-26.6569629481102,22.6932351509118,-60.385313676611));
#13263=CARTESIAN_POINT('Ctrl Pts',(-26.6552781358949,22.6871519123201,-60.3849263763411));
#13264=CARTESIAN_POINT('Ctrl Pts',(-26.6544680178596,22.6842427758264,-60.3847409551444));
#13265=CARTESIAN_POINT('Ctrl Pts',(-26.6525586641544,22.6774233837778,-60.3843058190168));
#13266=CARTESIAN_POINT('Ctrl Pts',(-26.6514561243334,22.673514065722,-60.3840559965292));
#13267=CARTESIAN_POINT('Ctrl Pts',(-26.6482588983541,22.6622590283134,-60.3833356661077));
#13268=CARTESIAN_POINT('Ctrl Pts',(-26.6461454933531,22.6549186954897,-60.3828645474292));
#13269=CARTESIAN_POINT('Ctrl Pts',(-26.6318564287939,22.6059450804685,-60.3797123224051));
#13270=CARTESIAN_POINT('Ctrl Pts',(-26.6188678717204,22.5645554487225,-60.3770046973106));
#13271=CARTESIAN_POINT('Ctrl Pts',(-26.5794712779629,22.4473492411775,-60.3692076783081));
#13272=CARTESIAN_POINT('Ctrl Pts',(-26.5510619272762,22.372244444364,-60.364053818291));
#13273=CARTESIAN_POINT('Ctrl Pts',(-26.4061930513277,22.0286204290436,-60.3397305670125));
#13274=CARTESIAN_POINT('Ctrl Pts',(-26.2563305119106,21.7757494827836,-60.3195089192671));
#13275=CARTESIAN_POINT('Ctrl Pts',(-26.0587389409155,21.5268271426935,-60.29843339558));
#13276=CARTESIAN_POINT('Ctrl Pts',(-26.0428177301035,21.5072466184985,-60.2967679691044));
#13277=CARTESIAN_POINT('Ctrl Pts',(-26.0077540878592,21.4651441020893,-60.2931736371484));
#13278=CARTESIAN_POINT('Ctrl Pts',(-25.9885281964672,21.4426940005698,-60.291248570365));
#13279=CARTESIAN_POINT('Ctrl Pts',(-25.9679114778802,21.4192796380399,-60.289234526886));
#13280=CARTESIAN_POINT('Ctrl Pts',(-25.9668264535615,21.4180492736216,-60.2891286755375));
#13281=CARTESIAN_POINT('Ctrl Pts',(-25.9639429072803,21.4147845017821,-60.2888477509164));
#13282=CARTESIAN_POINT('Ctrl Pts',(-25.9621427487103,21.4127515335335,-60.2886727699528));
#13283=CARTESIAN_POINT('Ctrl Pts',(-25.9342793988578,21.3813647067349,-60.2859705175049));
#13284=CARTESIAN_POINT('Ctrl Pts',(-25.9076830965851,21.3524854876379,-60.2834741706482));
#13285=CARTESIAN_POINT('Ctrl Pts',(-25.8772690046277,21.3206483840594,-60.2807180082568));
#13286=CARTESIAN_POINT('Ctrl Pts',(-25.8739660214299,21.3172061956836,-60.2804199603599));
#13287=CARTESIAN_POINT('Ctrl Pts',(-25.8689829863096,21.3120361773187,-60.2799722401627));
#13288=CARTESIAN_POINT('Ctrl Pts',(-25.8673086381527,21.3103028961506,-60.2798221280879));
#13289=CARTESIAN_POINT('Ctrl Pts',(-25.8644065981706,21.3073054470718,-60.2795625153158));
#13290=CARTESIAN_POINT('Ctrl Pts',(-25.863179813925,21.3060404082637,-60.2794529436332));
#13291=CARTESIAN_POINT('Ctrl Pts',(-25.8606227285272,21.3034079096273,-60.2792249196519));
#13292=CARTESIAN_POINT('Ctrl Pts',(-25.8592922521642,21.302040626327,-60.27910648204));
#13293=CARTESIAN_POINT('Ctrl Pts',(-25.8561298682358,21.2987965250996,-60.2788254552662));
#13294=CARTESIAN_POINT('Ctrl Pts',(-25.8542968769134,21.2969207549273,-60.2786629514398));
#13295=CARTESIAN_POINT('Ctrl Pts',(-25.8481798467253,21.2906762315511,-60.2781219219332));
#13296=CARTESIAN_POINT('Ctrl Pts',(-25.843885622343,21.2863174071223,-60.2777441938289));
#13297=CARTESIAN_POINT('Ctrl Pts',(-25.7339332116331,21.1753448781149,-60.2681247002332));
#13298=CARTESIAN_POINT('Ctrl Pts',(-25.6209505014655,21.0762130932694,-60.2594621356334));
#13299=CARTESIAN_POINT('Ctrl Pts',(-25.2266298362415,20.7762462886088,-60.2314428530723));
#13300=CARTESIAN_POINT('Ctrl Pts',(-24.9200302400552,20.6127269577628,-60.2127350488086));
#13301=CARTESIAN_POINT('Ctrl Pts',(-24.5736710963128,20.4942480773045,-60.1906023336608));
#13302=CARTESIAN_POINT('Ctrl Pts',(-24.5539588339682,20.4877172402958,-60.1893406636643));
#13303=CARTESIAN_POINT('Ctrl Pts',(-24.5281870217807,20.4794543664092,-60.1876880630845));
#13304=CARTESIAN_POINT('Ctrl Pts',(-24.5221832673577,20.4775488552878,-60.187302858969));
#13305=CARTESIAN_POINT('Ctrl Pts',(-24.512938777715,20.4746445830253,-60.1867093804247));
#13306=CARTESIAN_POINT('Ctrl Pts',(-24.5097019644707,20.473633307936,-60.1865015178778));
#13307=CARTESIAN_POINT('Ctrl Pts',(-24.5035129025046,20.4717103807978,-60.1861039397958));
#13308=CARTESIAN_POINT('Ctrl Pts',(-24.5005609254372,20.4707978614519,-60.1859142530105));
#13309=CARTESIAN_POINT('Ctrl Pts',(-24.4939821344908,20.4687745767321,-60.1854913910076));
#13310=CARTESIAN_POINT('Ctrl Pts',(-24.4903546667502,20.4676659675275,-60.1852581453017));
#13311=CARTESIAN_POINT('Ctrl Pts',(-24.4828235028081,20.4653788593902,-60.1847737135551));
#13312=CARTESIAN_POINT('Ctrl Pts',(-24.4789195122102,20.4642013608137,-60.1845224951607));
#13313=CARTESIAN_POINT('Ctrl Pts',(-24.4690467269631,20.4612440202674,-60.1838869334775));
#13314=CARTESIAN_POINT('Ctrl Pts',(-24.4630750074428,20.4594740724996,-60.1835022666312));
#13315=CARTESIAN_POINT('Ctrl Pts',(-24.4460792567874,20.4544902831809,-60.182406797972));
#13316=CARTESIAN_POINT('Ctrl Pts',(-24.4350432117285,20.4513180587282,-60.1816946385476));
#13317=CARTESIAN_POINT('Ctrl Pts',(-24.3320864241747,20.4223187421607,-60.1750427702001));
#13318=CARTESIAN_POINT('Ctrl Pts',(-24.2390861345507,20.4005320373902,-60.1689724382176));
#13319=CARTESIAN_POINT('Ctrl Pts',(-24.004007049572,20.3563705808468,-60.1534586637642));
#13320=CARTESIAN_POINT('Ctrl Pts',(-23.861148132463,20.3393163339329,-60.1438726191102));
#13321=CARTESIAN_POINT('Ctrl Pts',(-23.4685052022661,20.3188949414558,-60.1173428601809));
#13322=CARTESIAN_POINT('Ctrl Pts',(-23.218688492532,20.3349080054325,-60.1002178852915));
#13323=CARTESIAN_POINT('Ctrl Pts',(-22.9715167725327,20.379892073931,-60.0843396011012));
#13324=CARTESIAN_POINT('Ctrl Pts',(-22.9698276212348,20.3802008863058,-60.0842311444443));
#13325=CARTESIAN_POINT('Ctrl Pts',(-22.9551315079401,20.3828997848357,-60.0832880163971));
#13326=CARTESIAN_POINT('Ctrl Pts',(-22.9421388600796,20.3853686107999,-60.0824574589776));
#13327=CARTESIAN_POINT('Ctrl Pts',(-22.9255800102334,20.3886208128835,-60.0814034046504));
#13328=CARTESIAN_POINT('Ctrl Pts',(-22.9219996836921,20.389330317569,-60.0811757661517));
#13329=CARTESIAN_POINT('Ctrl Pts',(-22.9163120632797,20.3904674648851,-60.0808145785833));
#13330=CARTESIAN_POINT('Ctrl Pts',(-22.9142039923915,20.3908911339368,-60.0806808020035));
#13331=CARTESIAN_POINT('Ctrl Pts',(-22.9102665642947,20.3916865582267,-60.0804311147867));
#13332=CARTESIAN_POINT('Ctrl Pts',(-22.9084371183133,20.3920577906453,-60.0803151751567));
#13333=CARTESIAN_POINT('Ctrl Pts',(-22.9043333061843,20.3928942521003,-60.0800552612188));
#13334=CARTESIAN_POINT('Ctrl Pts',(-22.9020591245228,20.3933603481401,-60.0799113377675));
#13335=CARTESIAN_POINT('Ctrl Pts',(-22.8953375682649,20.3947455079494,-60.0794862823139));
#13336=CARTESIAN_POINT('Ctrl Pts',(-22.8908916067557,20.3956715202934,-60.0792055493185));
#13337=CARTESIAN_POINT('Ctrl Pts',(-22.8561511833587,20.4029839668509,-60.0770150948339));
#13338=CARTESIAN_POINT('Ctrl Pts',(-22.8259468834668,20.4097975326101,-60.0751295237575));
#13339=CARTESIAN_POINT('Ctrl Pts',(-22.721399238305,20.4349703426456,-60.0686538158082));
#13340=CARTESIAN_POINT('Ctrl Pts',(-22.6476107524568,20.4555440508272,-60.0641730975848));
#13341=CARTESIAN_POINT('Ctrl Pts',(-22.2005956387554,20.5975330376361,-60.0371952096772));
#13342=CARTESIAN_POINT('Ctrl Pts',(-21.8514278405479,20.7836368432619,-60.0163814734318));
#13343=CARTESIAN_POINT('Ctrl Pts',(-21.5291801313123,21.039923026942,-59.9914650763811));
#13344=CARTESIAN_POINT('Ctrl Pts',(-21.514227017287,21.0520355776059,-59.9902952741229));
#13345=CARTESIAN_POINT('Ctrl Pts',(-21.4946683069979,21.0681710619137,-59.9887467403859));
#13346=CARTESIAN_POINT('Ctrl Pts',(-21.4899641924846,21.0720743932321,-59.9883728771842));
#13347=CARTESIAN_POINT('Ctrl Pts',(-21.4826965269162,21.0781398772748,-59.9877930552217));
#13348=CARTESIAN_POINT('Ctrl Pts',(-21.4801251802715,21.0802927025087,-59.9875874782779));
#13349=CARTESIAN_POINT('Ctrl Pts',(-21.4750465664753,21.0845582046866,-59.9871805891671));
#13350=CARTESIAN_POINT('Ctrl Pts',(-21.472539153398,21.086670702357,-59.9869792844975));
#13351=CARTESIAN_POINT('Ctrl Pts',(-21.4669882325931,21.0913618600593,-59.9865327110262));
#13352=CARTESIAN_POINT('Ctrl Pts',(-21.4639462837389,21.093942348823,-59.9862873670885));
#13353=CARTESIAN_POINT('Ctrl Pts',(-21.4576440747357,21.099308672978,-59.9857777830139));
#13354=CARTESIAN_POINT('Ctrl Pts',(-21.454384570063,21.1020953799092,-59.9855135071006));
#13355=CARTESIAN_POINT('Ctrl Pts',(-21.4460255395166,21.1092708450883,-59.9848339133412));
#13356=CARTESIAN_POINT('Ctrl Pts',(-21.4409341962258,21.1136690655456,-59.9844182031825));
#13357=CARTESIAN_POINT('Ctrl Pts',(-21.4262184822622,21.126462107367,-59.9832114592914));
#13358=CARTESIAN_POINT('Ctrl Pts',(-21.4166302760253,21.1348981629209,-59.9824187070848));
#13359=CARTESIAN_POINT('Ctrl Pts',(-21.3219449984661,21.2192094884072,-59.9745249400231));
#13360=CARTESIAN_POINT('Ctrl Pts',(-21.2408904697627,21.2994842673907,-59.9672369285417));
#13361=CARTESIAN_POINT('Ctrl Pts',(-20.9518788759671,21.6177936213176,-59.9391271575394));
#13362=CARTESIAN_POINT('Ctrl Pts',(-20.7750808025658,21.8816243356112,-59.9171542691619));
#13363=CARTESIAN_POINT('Ctrl Pts',(-20.6339599973371,22.1785668680963,-59.8956329389504));
#13364=CARTESIAN_POINT('Ctrl Pts',(-20.6284970787806,22.1902419477057,-59.894791883197));
#13365=CARTESIAN_POINT('Ctrl Pts',(-20.6217678309579,22.2048510584192,-59.8937460948862));
#13366=CARTESIAN_POINT('Ctrl Pts',(-20.6204356954141,22.2077544599115,-59.8935385813245));
#13367=CARTESIAN_POINT('Ctrl Pts',(-20.5974696451716,22.2580061642565,-59.8899526460202));
#13368=CARTESIAN_POINT('Ctrl Pts',(-20.5769801645026,22.305873305525,-59.886623986611));
#13369=CARTESIAN_POINT('Ctrl Pts',(-20.5555330361776,22.3595361541265,-59.8830045854945));
#13370=CARTESIAN_POINT('Ctrl Pts',(-20.5534221766376,22.3648588532698,-59.8826467975053));
#13371=CARTESIAN_POINT('Ctrl Pts',(-20.5504841832215,22.3723252431736,-59.8821466380858));
#13372=CARTESIAN_POINT('Ctrl Pts',(-20.5496451549772,22.3744641951248,-59.8820035518201));
#13373=CARTESIAN_POINT('Ctrl Pts',(-20.5481137853683,22.3783804616915,-59.8817419360491));
#13374=CARTESIAN_POINT('Ctrl Pts',(-20.5474207334757,22.3801574961055,-59.8816233633248));
#13375=CARTESIAN_POINT('Ctrl Pts',(-20.5460158306932,22.3837692357584,-59.8813826502418));
#13376=CARTESIAN_POINT('Ctrl Pts',(-20.5453040825019,22.3856039782304,-59.8812605162119));
#13377=CARTESIAN_POINT('Ctrl Pts',(-20.5435389010194,22.3901666482865,-59.8809571532225));
#13378=CARTESIAN_POINT('Ctrl Pts',(-20.5424874964873,22.392895366893,-59.8807760475502));
#13379=CARTESIAN_POINT('Ctrl Pts',(-20.5385674895896,22.4031104117441,-59.8800992614596));
#13380=CARTESIAN_POINT('Ctrl Pts',(-20.5357230802018,22.4106060840939,-59.8796050310142));
#13381=CARTESIAN_POINT('Ctrl Pts',(-20.4870559471141,22.5403122648878,-59.8710926994827));
#13382=CARTESIAN_POINT('Ctrl Pts',(-20.448664598178,22.6652021184694,-59.8635059766248));
#13383=CARTESIAN_POINT('Ctrl Pts',(-20.3325695051864,23.144843102361,-59.8354431374785));
#13384=CARTESIAN_POINT('Ctrl Pts',(-20.3073857211801,23.5094492477192,-59.8159319005925));
#13385=CARTESIAN_POINT('Ctrl Pts',(-20.3454822205398,23.8908067036625,-59.7927534642006));
#13386=CARTESIAN_POINT('Ctrl Pts',(-20.3476915544303,23.9109921176318,-59.7915195411324));
#13387=CARTESIAN_POINT('Ctrl Pts',(-20.3508294299338,23.9373550559754,-59.7898983061721));
#13388=CARTESIAN_POINT('Ctrl Pts',(-20.3515854162371,23.9435529664887,-59.7895164541467));
#13389=CARTESIAN_POINT('Ctrl Pts',(-20.3527783977376,23.9531025655446,-59.788927012087));
#13390=CARTESIAN_POINT('Ctrl Pts',(-20.3532026652215,23.9564558530042,-59.7887198249462));
#13391=CARTESIAN_POINT('Ctrl Pts',(-20.3540485785778,23.9630582817905,-59.7883114734609));
#13392=CARTESIAN_POINT('Ctrl Pts',(-20.3544699055831,23.9663074604516,-59.7881103194403));
#13393=CARTESIAN_POINT('Ctrl Pts',(-20.3554090288439,23.9734641711262,-59.7876668175839));
#13394=CARTESIAN_POINT('Ctrl Pts',(-20.3559290401142,23.9773714031831,-59.7874243998415));
#13395=CARTESIAN_POINT('Ctrl Pts',(-20.3570216128152,23.9854671137423,-59.7869215175256));
#13396=CARTESIAN_POINT('Ctrl Pts',(-20.3575952496855,23.9896554368692,-59.7866610192838));
#13397=CARTESIAN_POINT('Ctrl Pts',(-20.3590833003289,24.0003634535025,-59.7859941662426));
#13398=CARTESIAN_POINT('Ctrl Pts',(-20.3600094509001,24.0068814724731,-59.7855874396385));
#13399=CARTESIAN_POINT('Ctrl Pts',(-20.3627369434881,24.025663499535,-59.7844130758635));
#13400=CARTESIAN_POINT('Ctrl Pts',(-20.3645890631126,24.0379199095502,-59.783643829848));
#13401=CARTESIAN_POINT('Ctrl Pts',(-20.3833396521092,24.157334795555,-59.7761202414873));
#13402=CARTESIAN_POINT('Ctrl Pts',(-20.4055660477846,24.2635746653563,-59.7691968112395));
#13403=CARTESIAN_POINT('Ctrl Pts',(-20.5076589473408,24.6525102416091,-59.742967301939));
#13404=CARTESIAN_POINT('Ctrl Pts',(-20.620665503439,24.9249619521829,-59.7226710832638));
#13405=CARTESIAN_POINT('Ctrl Pts',(-20.7855596407207,25.206654778394,-59.7010354244668));
#13406=CARTESIAN_POINT('Ctrl Pts',(-20.8025757232645,25.2347309308273,-59.6988732390526));
#13407=CARTESIAN_POINT('Ctrl Pts',(-20.8233731137638,25.2678922118154,-59.696316606057));
#13408=CARTESIAN_POINT('Ctrl Pts',(-20.826743629861,25.2732315488106,-59.6959048714288));
#13409=CARTESIAN_POINT('Ctrl Pts',(-20.8325007101426,25.2822924110081,-59.6952060502973));
#13410=CARTESIAN_POINT('Ctrl Pts',(-20.8348792683038,25.2860189756452,-59.6949186072461));
#13411=CARTESIAN_POINT('Ctrl Pts',(-20.8658609259485,25.3343394179612,-59.6911911942636));
#13412=CARTESIAN_POINT('Ctrl Pts',(-20.8955538891357,25.3782296230703,-59.687802258331));
#13413=CARTESIAN_POINT('Ctrl Pts',(-20.9296574274634,25.4260542139122,-59.6841233180694));
#13414=CARTESIAN_POINT('Ctrl Pts',(-20.9330097520276,25.4307287705315,-59.6837638745796));
#13415=CARTESIAN_POINT('Ctrl Pts',(-20.9377211259396,25.437261412281,-59.6832617958988));
#13416=CARTESIAN_POINT('Ctrl Pts',(-20.9390696518484,25.4391270191997,-59.683118438574));
#13417=CARTESIAN_POINT('Ctrl Pts',(-20.9415398818594,25.4425367375025,-59.6828564810674));
#13418=CARTESIAN_POINT('Ctrl Pts',(-20.9426609602028,25.4440812993772,-59.6827378372621));
#13419=CARTESIAN_POINT('Ctrl Pts',(-20.9449399348785,25.4472152889306,-59.6824971451542));
#13420=CARTESIAN_POINT('Ctrl Pts',(-20.9460979142873,25.4488046532217,-59.6823751029067));
#13421=CARTESIAN_POINT('Ctrl Pts',(-20.9489773693219,25.4527492077706,-59.6820722645127));
#13422=CARTESIAN_POINT('Ctrl Pts',(-20.9507005938854,25.4551031283689,-59.6818915907353));
#13423=CARTESIAN_POINT('Ctrl Pts',(-20.9571427979019,25.4638781403062,-59.6812182269761));
#13424=CARTESIAN_POINT('Ctrl Pts',(-20.9618824422396,25.4702841315971,-59.6807269679622));
#13425=CARTESIAN_POINT('Ctrl Pts',(-21.042738075588,25.5787231797695,-59.6724151693296));
#13426=CARTESIAN_POINT('Ctrl Pts',(-21.1248205688843,25.6761900693949,-59.6650049607331));
#13427=CARTESIAN_POINT('Ctrl Pts',(-21.2396954761958,25.7972524485473,-59.6555032889791));
#13428=CARTESIAN_POINT('Ctrl Pts',(-21.2674520610817,25.8254458558071,-59.6532675425095));
#13429=CARTESIAN_POINT('Ctrl Pts',(-21.3194355529443,25.8763382036649,-59.6491738555093));
#13430=CARTESIAN_POINT('Ctrl Pts',(-21.3435073542389,25.8991873340857,-59.6473133430677));
#13431=CARTESIAN_POINT('Ctrl Pts',(-21.519366350419,26.0610242549589,-59.6339376814138));
#13432=CARTESIAN_POINT('Ctrl Pts',(-21.6837944063406,26.185551545305,-59.6225339060881));
#13433=CARTESIAN_POINT('Ctrl Pts',(-21.9294086191048,26.3369764848424,-59.6057496661577));
#13434=CARTESIAN_POINT('Ctrl Pts',(-22.0014847055492,26.377668243201,-59.6008566094396));
#13435=CARTESIAN_POINT('Ctrl Pts',(-22.075036024144,26.4155367790859,-59.5958634867516));
#13436=CARTESIAN_POINT('Origin',(-23.5502525316942,23.5502525316942,-77.3107734492734));
#13437=CARTESIAN_POINT('',(-22.0750360153446,26.4155367745555,-58.0990855609687));
#13438=CARTESIAN_POINT('',(-22.0750360184326,26.4155367761454,-58.3433576442193));
#13439=CARTESIAN_POINT('',(-22.0750360153461,26.4155367745563,-77.3107734492734));
#13440=CARTESIAN_POINT('',(-26.7730012761155,23.5474077415013,-58.9401251418819));
#13441=CARTESIAN_POINT('Ctrl Pts',(-22.0750360153447,26.4155367745556,-58.0990855609687));
#13442=CARTESIAN_POINT('Ctrl Pts',(-22.0676980781123,26.4117587737418,-58.0996197687782));
#13443=CARTESIAN_POINT('Ctrl Pts',(-22.0603745949641,26.40795255408,-58.1001526872996));
#13444=CARTESIAN_POINT('Ctrl Pts',(-22.0472928179374,26.4010896298236,-58.101104098468));
#13445=CARTESIAN_POINT('Ctrl Pts',(-22.04152905953,26.3980435259965,-58.1015231000164));
#13446=CARTESIAN_POINT('Ctrl Pts',(-22.006154855784,26.3792109822164,-58.1040933420527));
#13447=CARTESIAN_POINT('Ctrl Pts',(-21.9767817886019,26.362979605031,-58.1062218758795));
#13448=CARTESIAN_POINT('Ctrl Pts',(-21.9432746360227,26.3437745428648,-58.1086387338298));
#13449=CARTESIAN_POINT('Ctrl Pts',(-21.9388889696207,26.3412470955953,-58.1089548455282));
#13450=CARTESIAN_POINT('Ctrl Pts',(-21.9324322481283,26.33750581313,-58.1094198828372));
#13451=CARTESIAN_POINT('Ctrl Pts',(-21.930356592747,26.3362999957308,-58.1095693254527));
#13452=CARTESIAN_POINT('Ctrl Pts',(-21.9266585544373,26.3341461522102,-58.1098354772508));
#13453=CARTESIAN_POINT('Ctrl Pts',(-21.9250356534901,26.3331990263661,-58.1099522451026));
#13454=CARTESIAN_POINT('Ctrl Pts',(-21.9216212244718,26.3312023584053,-58.1101978408928));
#13455=CARTESIAN_POINT('Ctrl Pts',(-21.9198298863959,26.3301525067484,-58.1103266478328));
#13456=CARTESIAN_POINT('Ctrl Pts',(-21.9151539504061,26.3274060008881,-58.1106627670032));
#13457=CARTESIAN_POINT('Ctrl Pts',(-21.9122709689688,26.3257065778639,-58.1108698981324));
#13458=CARTESIAN_POINT('Ctrl Pts',(-21.8994961879407,26.3181494257741,-58.1117872725112));
#13459=CARTESIAN_POINT('Ctrl Pts',(-21.8896329652453,26.3122431883853,-58.1124943801649));
#13460=CARTESIAN_POINT('Ctrl Pts',(-21.8164728214048,26.267900284789,-58.1177321208777));
#13461=CARTESIAN_POINT('Ctrl Pts',(-21.7544802898064,26.2273415121784,-58.1221301319267));
#13462=CARTESIAN_POINT('Ctrl Pts',(-21.5146177149416,26.0583252013949,-58.1392138911113));
#13463=CARTESIAN_POINT('Ctrl Pts',(-21.3486559233651,25.9139839060101,-58.1512192756305));
#13464=CARTESIAN_POINT('Ctrl Pts',(-21.0584009032197,25.6042376117704,-58.1750957309266));
#13465=CARTESIAN_POINT('Ctrl Pts',(-20.9327933122848,25.4415661769213,-58.1868752194558));
#13466=CARTESIAN_POINT('Ctrl Pts',(-20.8167823733491,25.2574189671903,-58.2001006083787));
#13467=CARTESIAN_POINT('Ctrl Pts',(-20.8101283603662,25.2467182294559,-58.2008686025562));
#13468=CARTESIAN_POINT('Ctrl Pts',(-20.801120909131,25.2320415274055,-58.2019213317536));
#13469=CARTESIAN_POINT('Ctrl Pts',(-20.7987129497811,25.2280990184376,-58.2022040587783));
#13470=CARTESIAN_POINT('Ctrl Pts',(-20.7946284692472,25.2213791317761,-58.2026858605033));
#13471=CARTESIAN_POINT('Ctrl Pts',(-20.7929476443894,25.2186043667002,-58.202884776991));
#13472=CARTESIAN_POINT('Ctrl Pts',(-20.7897042251249,25.2132317258738,-58.2032698765809));
#13473=CARTESIAN_POINT('Ctrl Pts',(-20.7881411007254,25.2106341733627,-58.2034560399559));
#13474=CARTESIAN_POINT('Ctrl Pts',(-20.7844398409519,25.2044638418469,-58.2038982058074));
#13475=CARTESIAN_POINT('Ctrl Pts',(-20.7823049636181,25.2008891237492,-58.2041543270289));
#13476=CARTESIAN_POINT('Ctrl Pts',(-20.7760254800232,25.1903280832651,-58.2049108835963));
#13477=CARTESIAN_POINT('Ctrl Pts',(-20.77190037682,25.1833302550905,-58.2054120289657));
#13478=CARTESIAN_POINT('Ctrl Pts',(-20.7404896447349,25.1295815763913,-58.2092601410414));
#13479=CARTESIAN_POINT('Ctrl Pts',(-20.7143607465427,25.0821679730332,-58.2126487448131));
#13480=CARTESIAN_POINT('Ctrl Pts',(-20.6301858525942,24.9198836275427,-58.2242371249276));
#13481=CARTESIAN_POINT('Ctrl Pts',(-20.57783495408,24.8022132150835,-58.2326293352103));
#13482=CARTESIAN_POINT('Ctrl Pts',(-20.4561958696138,24.4778112538357,-58.2556765888785));
#13483=CARTESIAN_POINT('Ctrl Pts',(-20.4006035785347,24.2666709324352,-58.2706171881914));
#13484=CARTESIAN_POINT('Ctrl Pts',(-20.3600662468127,24.0092337271706,-58.287988379156));
#13485=CARTESIAN_POINT('Ctrl Pts',(-20.3542475297845,23.9667913336922,-58.2908235599343));
#13486=CARTESIAN_POINT('Ctrl Pts',(-20.3483768832184,23.9165447411626,-58.2941373910606));
#13487=CARTESIAN_POINT('Ctrl Pts',(-20.3475050957034,23.9088421499098,-58.2946442052975));
#13488=CARTESIAN_POINT('Ctrl Pts',(-20.3461382922348,23.8963631505231,-58.2954633079041));
#13489=CARTESIAN_POINT('Ctrl Pts',(-20.3456261496483,23.8915886885315,-58.2957762252108));
#13490=CARTESIAN_POINT('Ctrl Pts',(-20.3443979737639,23.8798925440261,-58.2965416071583));
#13491=CARTESIAN_POINT('Ctrl Pts',(-20.3436936805637,23.8729696216578,-58.2969936226092));
#13492=CARTESIAN_POINT('Ctrl Pts',(-20.3427377752082,23.863261270265,-58.2976260387367));
#13493=CARTESIAN_POINT('Ctrl Pts',(-20.3424673624957,23.8604777593476,-58.2978071917035));
#13494=CARTESIAN_POINT('Ctrl Pts',(-20.3420714545763,23.8563465872066,-58.2980757973916));
#13495=CARTESIAN_POINT('Ctrl Pts',(-20.3419431852754,23.8549992004073,-58.2981633633647));
#13496=CARTESIAN_POINT('Ctrl Pts',(-20.341574694818,23.8511024256803,-58.2984164960507));
#13497=CARTESIAN_POINT('Ctrl Pts',(-20.3413366627182,23.8485528258432,-58.2985819724549));
#13498=CARTESIAN_POINT('Ctrl Pts',(-20.3408755492314,23.8435493407495,-58.2989064263341));
#13499=CARTESIAN_POINT('Ctrl Pts',(-20.3406522428451,23.8410954784192,-58.2990654131508));
#13500=CARTESIAN_POINT('Ctrl Pts',(-20.3400483178405,23.8343736817508,-58.2995005464906));
#13501=CARTESIAN_POINT('Ctrl Pts',(-20.3396733949605,23.8301052246053,-58.2997764499088));
#13502=CARTESIAN_POINT('Ctrl Pts',(-20.3361143381287,23.7886370720046,-58.3024527592119));
#13503=CARTESIAN_POINT('Ctrl Pts',(-20.3335681853829,23.7513834179954,-58.3048250615296));
#13504=CARTESIAN_POINT('Ctrl Pts',(-20.3314043717874,23.7088758725424,-58.3074891336274));
#13505=CARTESIAN_POINT('Ctrl Pts',(-20.3311515279812,23.7036590817678,-58.3078153509713));
#13506=CARTESIAN_POINT('Ctrl Pts',(-20.3307995631067,23.6960128053208,-58.3082923906593));
#13507=CARTESIAN_POINT('Ctrl Pts',(-20.3306905092495,23.6935838194159,-58.3084437689834));
#13508=CARTESIAN_POINT('Ctrl Pts',(-20.330501858767,23.6892730839687,-58.3087121298965));
#13509=CARTESIAN_POINT('Ctrl Pts',(-20.3304211627993,23.687391387325,-58.3088291747182));
#13510=CARTESIAN_POINT('Ctrl Pts',(-20.3302556427603,23.6834510411808,-58.3090740639089));
#13511=CARTESIAN_POINT('Ctrl Pts',(-20.3301711435147,23.6813923854026,-58.3092018894841));
#13512=CARTESIAN_POINT('Ctrl Pts',(-20.3299573703595,23.6760594238809,-58.3095327197153));
#13513=CARTESIAN_POINT('Ctrl Pts',(-20.3298311155833,23.6727849891043,-58.3097355536263));
#13514=CARTESIAN_POINT('Ctrl Pts',(-20.329309485935,23.6586984447924,-58.310606890668));
#13515=CARTESIAN_POINT('Ctrl Pts',(-20.3289635592016,23.6478844100164,-58.3112726362608));
#13516=CARTESIAN_POINT('Ctrl Pts',(-20.3282038789085,23.6196941266448,-58.3130003393996));
#13517=CARTESIAN_POINT('Ctrl Pts',(-20.3278762164518,23.6023156584231,-58.3140577169823));
#13518=CARTESIAN_POINT('Ctrl Pts',(-20.3272050082794,23.5399494679859,-58.3178274197463));
#13519=CARTESIAN_POINT('Ctrl Pts',(-20.3276628502538,23.4949563344509,-58.3205005251716));
#13520=CARTESIAN_POINT('Ctrl Pts',(-20.332294622686,23.3461559316025,-58.3292301464952));
#13521=CARTESIAN_POINT('Ctrl Pts',(-20.3405450553807,23.2425359462845,-58.3351316956454));
#13522=CARTESIAN_POINT('Ctrl Pts',(-20.3714627845804,23.001941411725,-58.3487726139861));
#13523=CARTESIAN_POINT('Ctrl Pts',(-20.3979980828437,22.865678559511,-58.3564551792907));
#13524=CARTESIAN_POINT('Ctrl Pts',(-20.4825214360355,22.5438756933861,-58.3752117936975));
#13525=CARTESIAN_POINT('Ctrl Pts',(-20.5486544218391,22.3610678807753,-58.3863955534678));
#13526=CARTESIAN_POINT('Ctrl Pts',(-20.6362185896086,22.1737764310991,-58.3989576945894));
#13527=CARTESIAN_POINT('Ctrl Pts',(-20.6416894765885,22.1622535337556,-58.39973507416));
#13528=CARTESIAN_POINT('Ctrl Pts',(-20.6492450379007,22.1465806875915,-58.4007986944732));
#13529=CARTESIAN_POINT('Ctrl Pts',(-20.6512705393168,22.1424022085144,-58.4010828730705));
#13530=CARTESIAN_POINT('Ctrl Pts',(-20.654729326737,22.1353060665916,-58.4015665271959));
#13531=CARTESIAN_POINT('Ctrl Pts',(-20.6561580137894,22.1323861589814,-58.4017658419087));
#13532=CARTESIAN_POINT('Ctrl Pts',(-20.6589267730689,22.1267490723088,-58.4021512182125));
#13533=CARTESIAN_POINT('Ctrl Pts',(-20.6602662641806,22.124031610919,-58.4023372592822));
#13534=CARTESIAN_POINT('Ctrl Pts',(-20.66344901368,22.1175975762233,-58.4027783683807));
#13535=CARTESIAN_POINT('Ctrl Pts',(-20.6652956171162,22.1138826720039,-58.4030335534906));
#13536=CARTESIAN_POINT('Ctrl Pts',(-20.6707467194409,22.1029693356135,-58.4037846815615));
#13537=CARTESIAN_POINT('Ctrl Pts',(-20.6743710042744,22.0957808713245,-58.4042813192077));
#13538=CARTESIAN_POINT('Ctrl Pts',(-20.6996140922977,22.0461765598818,-58.4077215127817));
#13539=CARTESIAN_POINT('Ctrl Pts',(-20.7221425473017,22.0042326206689,-58.4106970834189));
#13540=CARTESIAN_POINT('Ctrl Pts',(-20.775831885522,21.9093756831314,-58.4175855363224));
#13541=CARTESIAN_POINT('Ctrl Pts',(-20.8075917411919,21.8568247261467,-58.4215189577978));
#13542=CARTESIAN_POINT('Ctrl Pts',(-20.9135434584392,21.6923194320745,-58.4342133596874));
#13543=CARTESIAN_POINT('Ctrl Pts',(-20.9932336035815,21.5840892799823,-58.4431546216494));
#13544=CARTESIAN_POINT('Ctrl Pts',(-21.1681837518019,21.3751721726073,-58.4615191270353));
#13545=CARTESIAN_POINT('Ctrl Pts',(-21.2636604968993,21.2750111636965,-58.4709299819139));
#13546=CARTESIAN_POINT('Ctrl Pts',(-21.4401562561203,21.1122227985673,-58.4870230539101));
#13547=CARTESIAN_POINT('Ctrl Pts',(-21.5182793250062,21.0467381821703,-58.4937608064249));
#13548=CARTESIAN_POINT('Ctrl Pts',(-21.6027894829175,20.982466796878,-58.5005570706663));
#13549=CARTESIAN_POINT('Ctrl Pts',(-21.6062037529446,20.9798809140966,-58.5008308375155));
#13550=CARTESIAN_POINT('Ctrl Pts',(-21.6136169374247,20.9742895736466,-58.5014234847939));
#13551=CARTESIAN_POINT('Ctrl Pts',(-21.6176177243386,20.9712865977674,-58.5017422189163));
#13552=CARTESIAN_POINT('Ctrl Pts',(-21.6290213321349,20.9627685303072,-58.5026475321209));
#13553=CARTESIAN_POINT('Ctrl Pts',(-21.6364409511792,20.9572758602866,-58.5032327547009));
#13554=CARTESIAN_POINT('Ctrl Pts',(-21.6553298711226,20.9434178244581,-58.5047127695208));
#13555=CARTESIAN_POINT('Ctrl Pts',(-21.6668311854552,20.9350961060332,-58.5056047909122));
#13556=CARTESIAN_POINT('Ctrl Pts',(-21.681438736159,20.9246732410709,-58.5067258244309));
#13557=CARTESIAN_POINT('Ctrl Pts',(-21.6844939250301,20.922501319016,-58.5069596367153));
#13558=CARTESIAN_POINT('Ctrl Pts',(-21.6893262740061,20.9190786970072,-58.5073284142693));
#13559=CARTESIAN_POINT('Ctrl Pts',(-21.6911009094257,20.917824464229,-58.5074636234271));
#13560=CARTESIAN_POINT('Ctrl Pts',(-21.6944007243967,20.9154973041331,-58.5077146233263));
#13561=CARTESIAN_POINT('Ctrl Pts',(-21.6959255570916,20.9144239122459,-58.5078304459346));
#13562=CARTESIAN_POINT('Ctrl Pts',(-21.6989170597974,20.9123219522417,-58.5080573533617));
#13563=CARTESIAN_POINT('Ctrl Pts',(-21.7003836490148,20.9112932882716,-58.5081684447912));
#13564=CARTESIAN_POINT('Ctrl Pts',(-21.7048382904648,20.9081743461661,-58.5085054221353));
#13565=CARTESIAN_POINT('Ctrl Pts',(-21.7078290467045,20.9060879070071,-58.5087310431794));
#13566=CARTESIAN_POINT('Ctrl Pts',(-21.7228591893839,20.8956403208729,-58.509861841953));
#13567=CARTESIAN_POINT('Ctrl Pts',(-21.734952231348,20.8873561281092,-58.5107618060829));
#13568=CARTESIAN_POINT('Ctrl Pts',(-21.7686038749483,20.8646392561058,-58.5132402317756));
#13569=CARTESIAN_POINT('Ctrl Pts',(-21.790281356902,20.8503836161156,-58.5148075813584));
#13570=CARTESIAN_POINT('Ctrl Pts',(-21.866371494191,20.8016508351184,-58.5202170375516));
#13571=CARTESIAN_POINT('Ctrl Pts',(-21.9216465968004,20.7685425477515,-58.5239850713193));
#13572=CARTESIAN_POINT('Ctrl Pts',(-22.0928426543215,20.6728545290839,-58.5352870652575));
#13573=CARTESIAN_POINT('Ctrl Pts',(-22.2116421700585,20.6157016403082,-58.542636751523));
#13574=CARTESIAN_POINT('Ctrl Pts',(-22.5807721450828,20.4652133067877,-58.5649100679342));
#13575=CARTESIAN_POINT('Ctrl Pts',(-22.8394504606907,20.3955586653664,-58.5798716557515));
#13576=CARTESIAN_POINT('Ctrl Pts',(-23.1205755740448,20.3562293165899,-58.5970729240216));
#13577=CARTESIAN_POINT('Ctrl Pts',(-23.1374304327121,20.3540071587807,-58.5981072514337));
#13578=CARTESIAN_POINT('Ctrl Pts',(-23.1600717566819,20.3512041845243,-58.599500978182));
#13579=CARTESIAN_POINT('Ctrl Pts',(-23.1658435691969,20.3505054926971,-58.5998566467346));
#13580=CARTESIAN_POINT('Ctrl Pts',(-23.1748877487756,20.3494354971894,-58.600414560685));
#13581=CARTESIAN_POINT('Ctrl Pts',(-23.1781588680212,20.3490535822447,-58.6006164704585));
#13582=CARTESIAN_POINT('Ctrl Pts',(-23.1844301651334,20.3483311279619,-58.6010038025725));
#13583=CARTESIAN_POINT('Ctrl Pts',(-23.1874302490794,20.3479897893986,-58.6011891994542));
#13584=CARTESIAN_POINT('Ctrl Pts',(-23.1944648858495,20.3471994267897,-58.6016241655454));
#13585=CARTESIAN_POINT('Ctrl Pts',(-23.1984998094537,20.3467538093702,-58.6018738420661));
#13586=CARTESIAN_POINT('Ctrl Pts',(-23.210119143314,20.3454927858031,-58.602593382873));
#13587=CARTESIAN_POINT('Ctrl Pts',(-23.2177055823441,20.3446966866574,-58.6030638558612));
#13588=CARTESIAN_POINT('Ctrl Pts',(-23.267419499542,20.3396582312481,-58.6061513599894));
#13589=CARTESIAN_POINT('Ctrl Pts',(-23.3096225974221,20.3362196686117,-58.6087936215734));
#13590=CARTESIAN_POINT('Ctrl Pts',(-23.4587829521134,20.3270208203232,-58.6182125562908));
#13591=CARTESIAN_POINT('Ctrl Pts',(-23.5659374406562,20.3257620073106,-58.6251272880969));
#13592=CARTESIAN_POINT('Ctrl Pts',(-23.6991522900978,20.3308373431878,-58.633902722752));
#13593=CARTESIAN_POINT('Ctrl Pts',(-23.7253442638431,20.3321555583475,-58.6356365385109));
#13594=CARTESIAN_POINT('Ctrl Pts',(-23.7725046255801,20.3351065343673,-58.6387727992104));
#13595=CARTESIAN_POINT('Ctrl Pts',(-23.7934788539564,20.3366251869097,-58.6401727725735));
#13596=CARTESIAN_POINT('Ctrl Pts',(-23.9570387609261,20.3500782365292,-58.6511278055667));
#13597=CARTESIAN_POINT('Ctrl Pts',(-24.0986973695205,20.3712910980207,-58.660850623457));
#13598=CARTESIAN_POINT('Ctrl Pts',(-24.3555192692361,20.4274303866719,-58.6786080096213));
#13599=CARTESIAN_POINT('Ctrl Pts',(-24.4710600086441,20.4595259552132,-58.6866440828384));
#13600=CARTESIAN_POINT('Ctrl Pts',(-24.6357011675498,20.5153167156157,-58.6979394414853));
#13601=CARTESIAN_POINT('Ctrl Pts',(-24.6864098796684,20.5339333354284,-58.701395535482));
#13602=CARTESIAN_POINT('Ctrl Pts',(-24.7414705177401,20.5557334763497,-58.7051046983956));
#13603=CARTESIAN_POINT('Ctrl Pts',(-24.7463061572741,20.5576616159926,-58.7054300782113));
#13604=CARTESIAN_POINT('Ctrl Pts',(-24.7534742919255,20.5605399533349,-58.7059118292773));
#13605=CARTESIAN_POINT('Ctrl Pts',(-24.7558103491087,20.5614811696675,-58.7060687382457));
#13606=CARTESIAN_POINT('Ctrl Pts',(-24.759805658087,20.563096358301,-58.7063369372708));
#13607=CARTESIAN_POINT('Ctrl Pts',(-24.7614654509351,20.5637689750498,-58.7064483096216));
#13608=CARTESIAN_POINT('Ctrl Pts',(-24.7647003329701,20.565083023476,-58.7066652777558));
#13609=CARTESIAN_POINT('Ctrl Pts',(-24.766275470778,20.5657243166405,-58.7067708813128));
#13610=CARTESIAN_POINT('Ctrl Pts',(-24.7695384939546,20.5670558184248,-58.7069895590906));
#13611=CARTESIAN_POINT('Ctrl Pts',(-24.7712263037112,20.5677462138613,-58.7071026219168));
#13612=CARTESIAN_POINT('Ctrl Pts',(-24.775085860061,20.5693287834828,-58.7073610553661));
#13613=CARTESIAN_POINT('Ctrl Pts',(-24.777257222713,20.5702219004372,-58.7075063686105));
#13614=CARTESIAN_POINT('Ctrl Pts',(-24.7881906839086,20.5747329875335,-58.7082376714012));
#13615=CARTESIAN_POINT('Ctrl Pts',(-24.7969378865331,20.5783872827729,-58.7088214705853));
#13616=CARTESIAN_POINT('Ctrl Pts',(-24.8191569847031,20.5877850594732,-58.7103014699764));
#13617=CARTESIAN_POINT('Ctrl Pts',(-24.8326062486783,20.5935819383182,-58.711194562987));
#13618=CARTESIAN_POINT('Ctrl Pts',(-24.8877179443487,20.6177828820176,-58.7148447422309));
#13619=CARTESIAN_POINT('Ctrl Pts',(-24.929029529535,20.6369783551149,-58.7175585226573));
#13620=CARTESIAN_POINT('Ctrl Pts',(-25.038897050783,20.6908893097572,-58.7247513583352));
#13621=CARTESIAN_POINT('Ctrl Pts',(-25.1066434994506,20.7271922919223,-58.7291607476499));
#13622=CARTESIAN_POINT('Ctrl Pts',(-25.2319526421024,20.8002246596876,-58.7373847292117));
#13623=CARTESIAN_POINT('Ctrl Pts',(-25.2897705148839,20.8364275257609,-58.7412082993718));
#13624=CARTESIAN_POINT('Ctrl Pts',(-25.4331866769271,20.9326958650035,-58.7508689873099));
#13625=CARTESIAN_POINT('Ctrl Pts',(-25.5170895952792,20.9951409065211,-58.7566893904664));
#13626=CARTESIAN_POINT('Ctrl Pts',(-25.7453076317367,21.182905193803,-58.7733616153561));
#13627=CARTESIAN_POINT('Ctrl Pts',(-25.881703842901,21.3171115633809,-58.7843820318429));
#13628=CARTESIAN_POINT('Ctrl Pts',(-26.0135945835897,21.4722190222821,-58.7967538034128));
#13629=CARTESIAN_POINT('Ctrl Pts',(-26.0217257936253,21.4818963633081,-58.7975241651298));
#13630=CARTESIAN_POINT('Ctrl Pts',(-26.0327546130788,21.4951801787201,-58.7985796429386));
#13631=CARTESIAN_POINT('Ctrl Pts',(-26.0357017741019,21.4987455190106,-58.7988627374433));
#13632=CARTESIAN_POINT('Ctrl Pts',(-26.0407038256966,21.5048233713511,-58.7993450079952));
#13633=CARTESIAN_POINT('Ctrl Pts',(-26.0427626216106,21.5073326729309,-58.7995440251724));
#13634=CARTESIAN_POINT('Ctrl Pts',(-26.0467366927721,21.5121913001278,-58.7999291940737));
#13635=CARTESIAN_POINT('Ctrl Pts',(-26.0486524517203,21.5145402264696,-58.8001153258686));
#13636=CARTESIAN_POINT('Ctrl Pts',(-26.0531894916415,21.5201191761655,-58.8005572213258));
#13637=CARTESIAN_POINT('Ctrl Pts',(-26.0558078334393,21.523351573004,-58.8008131033081));
#13638=CARTESIAN_POINT('Ctrl Pts',(-26.0635090216723,21.5328965733922,-58.8015682707832));
#13639=CARTESIAN_POINT('Ctrl Pts',(-26.0685742942707,21.5392232566404,-58.8020682623589));
#13640=CARTESIAN_POINT('Ctrl Pts',(-26.104816758271,21.5848428724473,-58.8056696757559));
#13641=CARTESIAN_POINT('Ctrl Pts',(-26.1350952345941,21.6248379635473,-58.8088067228743));
#13642=CARTESIAN_POINT('Ctrl Pts',(-26.2600789027057,21.7981937864426,-58.8223292056579));
#13643=CARTESIAN_POINT('Ctrl Pts',(-26.3454785408393,21.9379354158334,-58.8330632564305));
#13644=CARTESIAN_POINT('Ctrl Pts',(-26.4452775221216,22.1331929204328,-58.8477620356812));
#13645=CARTESIAN_POINT('Ctrl Pts',(-26.46936457035,22.1835000676783,-58.8515222097568));
#13646=CARTESIAN_POINT('Ctrl Pts',(-26.5033554884374,22.259494666039,-58.8571500331254));
#13647=CARTESIAN_POINT('Ctrl Pts',(-26.5142558110974,22.2847259649098,-58.8590100903821));
#13648=CARTESIAN_POINT('Ctrl Pts',(-26.5366289812747,22.3383890617118,-58.8629456575821));
#13649=CARTESIAN_POINT('Ctrl Pts',(-26.548021619838,22.3668515552862,-58.8650210698213));
#13650=CARTESIAN_POINT('Ctrl Pts',(-26.6116287801908,22.5325785827677,-58.8770249118301));
#13651=CARTESIAN_POINT('Ctrl Pts',(-26.6548230597419,22.6731351767959,-58.8868963484685));
#13652=CARTESIAN_POINT('Ctrl Pts',(-26.6971868107076,22.8542276156384,-58.8988695096886));
#13653=CARTESIAN_POINT('Ctrl Pts',(-26.7053992795376,22.8924566793656,-58.9013555691152));
#13654=CARTESIAN_POINT('Ctrl Pts',(-26.7139186509395,22.9359549293574,-58.9041301722673));
#13655=CARTESIAN_POINT('Ctrl Pts',(-26.7149103661261,22.9410845333713,-58.9044565224561));
#13656=CARTESIAN_POINT('Ctrl Pts',(-26.716352383139,22.9486418690403,-58.9049360537566));
#13657=CARTESIAN_POINT('Ctrl Pts',(-26.7168123697432,22.9510677097144,-58.9050897861985));
#13658=CARTESIAN_POINT('Ctrl Pts',(-26.7176193916301,22.9553506018734,-58.9053608616994));
#13659=CARTESIAN_POINT('Ctrl Pts',(-26.7179675821122,22.9572074314237,-58.9054782713284));
#13660=CARTESIAN_POINT('Ctrl Pts',(-26.7186888667761,22.9610726560823,-58.9057224359218));
#13661=CARTESIAN_POINT('Ctrl Pts',(-26.7190616834882,22.9630810960332,-58.9058491746159));
#13662=CARTESIAN_POINT('Ctrl Pts',(-26.7198134643567,22.9671526631359,-58.9061058346743));
#13663=CARTESIAN_POINT('Ctrl Pts',(-26.7201923243909,22.9692158088345,-58.9062357500021));
#13664=CARTESIAN_POINT('Ctrl Pts',(-26.7211185777745,22.9742877474075,-58.9065547879852));
#13665=CARTESIAN_POINT('Ctrl Pts',(-26.7216637046492,22.9772969599771,-58.9067437815476));
#13666=CARTESIAN_POINT('Ctrl Pts',(-26.7231557075468,22.9856004924997,-58.9072644863017));
#13667=CARTESIAN_POINT('Ctrl Pts',(-26.7240936204068,22.9908964436128,-58.9075956941462));
#13668=CARTESIAN_POINT('Ctrl Pts',(-26.7567804302506,23.1781927329344,-58.9192783373812));
#13669=CARTESIAN_POINT('Ctrl Pts',(-26.7728381517533,23.3626106922982,-58.9297616610296));
#13670=CARTESIAN_POINT('Ctrl Pts',(-26.7730012761155,23.5474077415013,-58.9401251418819));
#13671=CARTESIAN_POINT('Ctrl Pts',(-26.7730012739202,23.5474052557013,-58.9401250024774));
#13672=CARTESIAN_POINT('Ctrl Pts',(-26.7732608683829,23.8412326648132,-58.9566029448737));
#13673=CARTESIAN_POINT('Ctrl Pts',(-26.733340782425,24.1336947857609,-58.9727791402557));
#13674=CARTESIAN_POINT('Ctrl Pts',(-26.6484731159184,24.4377339379656,-58.9917388195041));
#13675=CARTESIAN_POINT('Ctrl Pts',(-26.6423911128418,24.4586979038837,-58.9930565541008));
#13676=CARTESIAN_POINT('Ctrl Pts',(-26.6332165092135,24.4891617042596,-58.9949873212806));
#13677=CARTESIAN_POINT('Ctrl Pts',(-26.6302918717469,24.4987117987337,-58.9955948874375));
#13678=CARTESIAN_POINT('Ctrl Pts',(-26.6249523802974,24.5158621825253,-58.9966901671647));
#13679=CARTESIAN_POINT('Ctrl Pts',(-26.6225536117075,24.5234674250893,-58.9971773508757));
#13680=CARTESIAN_POINT('Ctrl Pts',(-26.6188689100004,24.5350002986675,-58.9979184229626));
#13681=CARTESIAN_POINT('Ctrl Pts',(-26.6176035962834,24.5389345271198,-58.99817163142));
#13682=CARTESIAN_POINT('Ctrl Pts',(-26.6152996793209,24.546051081217,-58.9986303938245));
#13683=CARTESIAN_POINT('Ctrl Pts',(-26.6142636770095,24.5492342480703,-58.9988358616533));
#13684=CARTESIAN_POINT('Ctrl Pts',(-26.6121853678175,24.5555863060551,-58.9992464131048));
#13685=CARTESIAN_POINT('Ctrl Pts',(-26.6111430964525,24.558755204592,-58.9994514953448));
#13686=CARTESIAN_POINT('Ctrl Pts',(-26.6082043844088,24.5676434775839,-59.0000274733912));
#13687=CARTESIAN_POINT('Ctrl Pts',(-26.6062968281407,24.5733591379023,-59.0003987367213));
#13688=CARTESIAN_POINT('Ctrl Pts',(-26.598446092336,24.5966646416276,-59.0019161650385));
#13689=CARTESIAN_POINT('Ctrl Pts',(-26.5923670806594,24.6142080451918,-59.0030668271421));
#13690=CARTESIAN_POINT('Ctrl Pts',(-26.483483282007,24.9198718448998,-59.0232653071219));
#13691=CARTESIAN_POINT('Ctrl Pts',(-26.3403431394454,25.1918993412259,-59.0438085161982));
#13692=CARTESIAN_POINT('Ctrl Pts',(-26.122303960735,25.4932001015231,-59.0689707730406));
#13693=CARTESIAN_POINT('Ctrl Pts',(-26.0818794021036,25.5455869908224,-59.073437456734));
#13694=CARTESIAN_POINT('Ctrl Pts',(-25.984628194895,25.6638988908192,-59.0836888373863));
#13695=CARTESIAN_POINT('Ctrl Pts',(-25.9266828685318,25.7288454450501,-59.0894418763274));
#13696=CARTESIAN_POINT('Ctrl Pts',(-25.8378748648088,25.8206176742615,-59.0976685217115));
#13697=CARTESIAN_POINT('Ctrl Pts',(-25.8090207088124,25.8493263731886,-59.1002569382835));
#13698=CARTESIAN_POINT('Ctrl Pts',(-25.7771506412614,25.8798563927381,-59.1030182282174));
#13699=CARTESIAN_POINT('Ctrl Pts',(-25.774668643435,25.8822264384678,-59.1032326448881));
#13700=CARTESIAN_POINT('Ctrl Pts',(-25.770550540708,25.8861462347791,-59.1035873550384));
#13701=CARTESIAN_POINT('Ctrl Pts',(-25.7689165953662,25.8876982345043,-59.1037278216318));
#13702=CARTESIAN_POINT('Ctrl Pts',(-25.7659787357775,25.8904828986998,-59.1039798920019));
#13703=CARTESIAN_POINT('Ctrl Pts',(-25.7646754195635,25.8917161884343,-59.1040915443794));
#13704=CARTESIAN_POINT('Ctrl Pts',(-25.7621453147452,25.8941063501156,-59.1043079565341));
#13705=CARTESIAN_POINT('Ctrl Pts',(-25.7609186494036,25.8952633465734,-59.1044127259398));
#13706=CARTESIAN_POINT('Ctrl Pts',(-25.758355407902,25.8976772092257,-59.1046313321033));
#13707=CARTESIAN_POINT('Ctrl Pts',(-25.7570186702366,25.8989338933148,-59.1047451546845));
#13708=CARTESIAN_POINT('Ctrl Pts',(-25.7533147896002,25.9024100050524,-59.1050600396994));
#13709=CARTESIAN_POINT('Ctrl Pts',(-25.7509453582762,25.9046270080543,-59.1052609137029));
#13710=CARTESIAN_POINT('Ctrl Pts',(-25.7416149468307,25.9133307913392,-59.106049729626));
#13711=CARTESIAN_POINT('Ctrl Pts',(-25.7346285109584,25.9197903942894,-59.1066355956259));
#13712=CARTESIAN_POINT('Ctrl Pts',(-25.6074104340123,26.036374389873,-59.1172196381788));
#13713=CARTESIAN_POINT('Ctrl Pts',(-25.479001893401,26.1372667572527,-59.1265506100821));
#13714=CARTESIAN_POINT('Ctrl Pts',(-25.277203368387,26.2724065855713,-59.1402222894373));
#13715=CARTESIAN_POINT('Ctrl Pts',(-25.2092911492622,26.3143207422279,-59.1446712938905));
#13716=CARTESIAN_POINT('Ctrl Pts',(-25.0726217231457,26.3918172543772,-59.1534524638283));
#13717=CARTESIAN_POINT('Ctrl Pts',(-25.0040005429707,26.427528036855,-59.1577811284583));
#13718=CARTESIAN_POINT('Ctrl Pts',(-24.8147219653582,26.5175284127304,-59.1696351132333));
#13719=CARTESIAN_POINT('Ctrl Pts',(-24.6919101877925,26.5669098684925,-59.177240605954));
#13720=CARTESIAN_POINT('Ctrl Pts',(-24.5141753322916,26.6259640425334,-59.1883679519394));
#13721=CARTESIAN_POINT('Ctrl Pts',(-24.4614964891975,26.6419805841453,-59.1916793675401));
#13722=CARTESIAN_POINT('Ctrl Pts',(-24.4005717565787,26.6588118987026,-59.1955329446685));
#13723=CARTESIAN_POINT('Ctrl Pts',(-24.3926997410072,26.6609545135651,-59.1960313082713));
#13724=CARTESIAN_POINT('Ctrl Pts',(-24.3807910055546,26.6641473281262,-59.1967859334832));
#13725=CARTESIAN_POINT('Ctrl Pts',(-24.376760201977,26.6652196311212,-59.1970414764932));
#13726=CARTESIAN_POINT('Ctrl Pts',(-24.369795191123,26.667058041888,-59.1974832550451));
#13727=CARTESIAN_POINT('Ctrl Pts',(-24.3668619562545,26.6678278405865,-59.1976693705194));
#13728=CARTESIAN_POINT('Ctrl Pts',(-24.360791586831,26.6694117945541,-59.198054676264));
#13729=CARTESIAN_POINT('Ctrl Pts',(-24.3576543028627,26.6702253595841,-59.1982538854516));
#13730=CARTESIAN_POINT('Ctrl Pts',(-24.3500531868292,26.6721842593558,-59.1987367220284));
#13731=CARTESIAN_POINT('Ctrl Pts',(-24.345588123993,26.6733247523471,-59.199020506016));
#13732=CARTESIAN_POINT('Ctrl Pts',(-24.3289756402692,26.6775300754888,-59.2000769255727));
#13733=CARTESIAN_POINT('Ctrl Pts',(-24.3168129487212,26.6805336110345,-59.200851541738));
#13734=CARTESIAN_POINT('Ctrl Pts',(-24.120640510273,26.7277658501111,-59.2133649763101));
#13735=CARTESIAN_POINT('Ctrl Pts',(-23.9331381156756,26.7557647998032,-59.2256370411106));
#13736=CARTESIAN_POINT('Ctrl Pts',(-23.6413925320914,26.7733624945439,-59.2451481356751));
#13737=CARTESIAN_POINT('Ctrl Pts',(-23.5382583912424,26.7746282829246,-59.2521176013932));
#13738=CARTESIAN_POINT('Ctrl Pts',(-23.3047978061391,26.7662916668578,-59.2679311097776));
#13739=CARTESIAN_POINT('Ctrl Pts',(-23.1747474262091,26.7537123939401,-59.276767879306));
#13740=CARTESIAN_POINT('Ctrl Pts',(-22.9674149116868,26.7208547603927,-59.2906061974249));
#13741=CARTESIAN_POINT('Ctrl Pts',(-22.8894946101641,26.7055369285702,-59.2957474900287));
#13742=CARTESIAN_POINT('Ctrl Pts',(-22.8039728888793,26.6854169461879,-59.3012668169912));
#13743=CARTESIAN_POINT('Ctrl Pts',(-22.7957408444709,26.6834460030383,-59.3017968049945));
#13744=CARTESIAN_POINT('Ctrl Pts',(-22.7853144837442,26.680906214575,-59.3024663514521));
#13745=CARTESIAN_POINT('Ctrl Pts',(-22.7831129746409,26.6803674815666,-59.3026076280757));
#13746=CARTESIAN_POINT('Ctrl Pts',(-22.7791659036491,26.6793971764419,-59.3028607456617));
#13747=CARTESIAN_POINT('Ctrl Pts',(-22.7774201340876,26.6789664657174,-59.3029726363895));
#13748=CARTESIAN_POINT('Ctrl Pts',(-22.7740362957976,26.6781286108644,-59.303189393757));
#13749=CARTESIAN_POINT('Ctrl Pts',(-22.7723981875171,26.6777216411832,-59.3032942702751));
#13750=CARTESIAN_POINT('Ctrl Pts',(-22.7689868109876,26.6768712767895,-59.3035125611626));
#13751=CARTESIAN_POINT('Ctrl Pts',(-22.767213605066,26.6764276616185,-59.3036259621796));
#13752=CARTESIAN_POINT('Ctrl Pts',(-22.7623266583237,26.6752006416056,-59.303938318523));
#13753=CARTESIAN_POINT('Ctrl Pts',(-22.7592136984493,26.6744140889889,-59.3041370905232));
#13754=CARTESIAN_POINT('Ctrl Pts',(-22.7471078239427,26.6713360397112,-59.3049093379762));
#13755=CARTESIAN_POINT('Ctrl Pts',(-22.738123534142,26.6690103263835,-59.3054808456753));
#13756=CARTESIAN_POINT('Ctrl Pts',(-22.5891559751387,26.6297605476963,-59.3149321045806));
#13757=CARTESIAN_POINT('Ctrl Pts',(-22.4517861027443,26.5834784875011,-59.3232856239594));
#13758=CARTESIAN_POINT('Ctrl Pts',(-22.2354475935959,26.4939548201463,-59.3365297794421));
#13759=CARTESIAN_POINT('Ctrl Pts',(-22.1543980105665,26.4563969913464,-59.341512604251));
#13760=CARTESIAN_POINT('Ctrl Pts',(-22.0750359236218,26.4155367273312,-59.3465003279648));
#13761=CARTESIAN_POINT('',(-26.77300250248,23.5498185963744,-59.1888436164772));
#13762=CARTESIAN_POINT('Ctrl Pts',(-22.075036024144,26.4155367790859,-59.5958634867516));
#13763=CARTESIAN_POINT('Ctrl Pts',(-22.0907483291231,26.4236263959182,-59.5947968373975));
#13764=CARTESIAN_POINT('Ctrl Pts',(-22.1065279599169,26.431587174871,-59.5937256735317));
#13765=CARTESIAN_POINT('Ctrl Pts',(-22.1307918774813,26.443578851968,-59.5920783195984));
#13766=CARTESIAN_POINT('Ctrl Pts',(-22.1392284698494,26.4477025896608,-59.5915054866377));
#13767=CARTESIAN_POINT('Ctrl Pts',(-22.1517665557862,26.4537633566486,-59.590654055701));
#13768=CARTESIAN_POINT('Ctrl Pts',(-22.1558543625232,26.4557287200167,-59.5903764450999));
#13769=CARTESIAN_POINT('Ctrl Pts',(-22.1628524832533,26.4590751535397,-59.5899011542212));
#13770=CARTESIAN_POINT('Ctrl Pts',(-22.1657607523931,26.4604605058275,-59.5897036230776));
#13771=CARTESIAN_POINT('Ctrl Pts',(-22.1716612791766,26.463260371618,-59.5893028329154));
#13772=CARTESIAN_POINT('Ctrl Pts',(-22.1746536475507,26.4646746402418,-59.589099565736));
#13773=CARTESIAN_POINT('Ctrl Pts',(-22.1815163003733,26.4679051788657,-59.5886333654204));
#13774=CARTESIAN_POINT('Ctrl Pts',(-22.1853880247205,26.4697183591702,-59.5883703255992));
#13775=CARTESIAN_POINT('Ctrl Pts',(-22.1935097129092,26.473502167251,-59.5878184975891));
#13776=CARTESIAN_POINT('Ctrl Pts',(-22.1977603855598,26.4754712418729,-59.5875296563324));
#13777=CARTESIAN_POINT('Ctrl Pts',(-22.208983249528,26.4806404117181,-59.586766956327));
#13778=CARTESIAN_POINT('Ctrl Pts',(-22.2159625689602,26.4838248775529,-59.5862925588625));
#13779=CARTESIAN_POINT('Ctrl Pts',(-22.339286178637,26.5395628068426,-59.5779082834818));
#13780=CARTESIAN_POINT('Ctrl Pts',(-22.4586253320777,26.5851756171509,-59.5697605916704));
#13781=CARTESIAN_POINT('Ctrl Pts',(-22.8920280627309,26.7219526713838,-59.5400135355816));
#13782=CARTESIAN_POINT('Ctrl Pts',(-23.2168045732654,26.772318308575,-59.517216217783));
#13783=CARTESIAN_POINT('Ctrl Pts',(-23.5442440032453,26.772997000431,-59.4959384705226));
#13784=CARTESIAN_POINT('Ctrl Pts',(-23.5449153382013,26.7729981821547,-59.4958948538546));
#13785=CARTESIAN_POINT('Ctrl Pts',(-23.552010314682,26.7730084541849,-59.4954339796293));
#13786=CARTESIAN_POINT('Ctrl Pts',(-23.5584340182969,26.7729985487257,-59.495017461577));
#13787=CARTESIAN_POINT('Ctrl Pts',(-23.5660653312186,26.7729639640564,-59.4945235666053));
#13788=CARTESIAN_POINT('Ctrl Pts',(-23.5672729624807,26.772957812332,-59.4944454368121));
#13789=CARTESIAN_POINT('Ctrl Pts',(-23.5714872604604,26.772933975638,-59.4941728822312));
#13790=CARTESIAN_POINT('Ctrl Pts',(-23.5744939151479,26.7729127617385,-59.493978602301));
#13791=CARTESIAN_POINT('Ctrl Pts',(-23.5790754545199,26.7728740239162,-59.4936828246882));
#13792=CARTESIAN_POINT('Ctrl Pts',(-23.5806503552201,26.7728595532461,-59.4935811992677));
#13793=CARTESIAN_POINT('Ctrl Pts',(-23.5848784273599,26.7728176047228,-59.4933084993324));
#13794=CARTESIAN_POINT('Ctrl Pts',(-23.5875315824257,26.7727880047382,-59.4931375146868));
#13795=CARTESIAN_POINT('Ctrl Pts',(-23.6295165929127,26.7722677405198,-59.4904339588933));
#13796=CARTESIAN_POINT('Ctrl Pts',(-23.6688385264976,26.7710602733632,-59.487932429098));
#13797=CARTESIAN_POINT('Ctrl Pts',(-23.7128982078189,26.7688992552242,-59.4851710666132));
#13798=CARTESIAN_POINT('Ctrl Pts',(-23.717665283605,26.7686548244549,-59.4848728450897));
#13799=CARTESIAN_POINT('Ctrl Pts',(-23.7248390033698,26.7682710116682,-59.4844249078419));
#13800=CARTESIAN_POINT('Ctrl Pts',(-23.727246036089,26.7681395205491,-59.4842747517517));
#13801=CARTESIAN_POINT('Ctrl Pts',(-23.7314125650791,26.767907222731,-59.4840150836169));
#13802=CARTESIAN_POINT('Ctrl Pts',(-23.7331721258571,26.7678076734987,-59.4839055005146));
#13803=CARTESIAN_POINT('Ctrl Pts',(-23.7368361167099,26.7675973636017,-59.4836774735867));
#13804=CARTESIAN_POINT('Ctrl Pts',(-23.7387405280093,26.7674863554724,-59.4835590444187));
#13805=CARTESIAN_POINT('Ctrl Pts',(-23.7432621469397,26.7672187617305,-59.4832780736507));
#13806=CARTESIAN_POINT('Ctrl Pts',(-23.7458792718304,26.7670606726053,-59.4831156172941));
#13807=CARTESIAN_POINT('Ctrl Pts',(-23.7545989677662,26.7665232730429,-59.4825749064491));
#13808=CARTESIAN_POINT('Ctrl Pts',(-23.760700699994,26.766129786426,-59.4821974482459));
#13809=CARTESIAN_POINT('Ctrl Pts',(-23.9155571731543,26.7557008222603,-59.472640216683));
#13810=CARTESIAN_POINT('Ctrl Pts',(-24.0634620104508,26.735370359142,-59.4640318816149));
#13811=CARTESIAN_POINT('Ctrl Pts',(-24.2846963989379,26.6891408062855,-59.4512462551058));
#13812=CARTESIAN_POINT('Ctrl Pts',(-24.3593613296593,26.6707285903472,-59.446947851374));
#13813=CARTESIAN_POINT('Ctrl Pts',(-24.5254719582332,26.62340244332,-59.4372960451423));
#13814=CARTESIAN_POINT('Ctrl Pts',(-24.6164275488084,26.593042959063,-59.4319481483246));
#13815=CARTESIAN_POINT('Ctrl Pts',(-24.8785936220146,26.492335802123,-59.4160763611777));
#13816=CARTESIAN_POINT('Ctrl Pts',(-25.0452343999865,26.4112589529476,-59.4053745386004));
#13817=CARTESIAN_POINT('Ctrl Pts',(-25.2139348036433,26.3103998410281,-59.3934227224401));
#13818=CARTESIAN_POINT('Ctrl Pts',(-25.2238495573209,26.3043993799085,-59.3927160774684));
#13819=CARTESIAN_POINT('Ctrl Pts',(-25.2375331703104,26.2960168122115,-59.3917348776431));
#13820=CARTESIAN_POINT('Ctrl Pts',(-25.2413298593136,26.2936801158123,-59.3914619946004));
#13821=CARTESIAN_POINT('Ctrl Pts',(-25.2478438471795,26.2896523804586,-59.3909927078936));
#13822=CARTESIAN_POINT('Ctrl Pts',(-25.2505635056063,26.2879651531547,-59.3907964451272));
#13823=CARTESIAN_POINT('Ctrl Pts',(-25.2560983145071,26.2845200283113,-59.3903963521842));
#13824=CARTESIAN_POINT('Ctrl Pts',(-25.2589132707787,26.2827618283627,-59.3901925109985));
#13825=CARTESIAN_POINT('Ctrl Pts',(-25.265400351582,26.2786961040705,-59.3897219302221));
#13826=CARTESIAN_POINT('Ctrl Pts',(-25.2690705379152,26.2763855132092,-59.3894550770771));
#13827=CARTESIAN_POINT('Ctrl Pts',(-25.2767676395884,26.2715180274725,-59.3888941389022));
#13828=CARTESIAN_POINT('Ctrl Pts',(-25.280793561601,26.2689595883142,-59.3885999967796));
#13829=CARTESIAN_POINT('Ctrl Pts',(-25.2914520282076,26.2621529564421,-59.3878192763049));
#13830=CARTESIAN_POINT('Ctrl Pts',(-25.2980746736699,26.2578893904064,-59.3873321245409));
#13831=CARTESIAN_POINT('Ctrl Pts',(-25.4339852363564,26.1696856731449,-59.3772922012737));
#13832=CARTESIAN_POINT('Ctrl Pts',(-25.5570814497657,26.0766143080507,-59.3673897719349));
#13833=CARTESIAN_POINT('Ctrl Pts',(-25.9307510065266,25.7494942415673,-59.3345840688599));
#13834=CARTESIAN_POINT('Ctrl Pts',(-26.150827876477,25.4842692820876,-59.3105616140563));
#13835=CARTESIAN_POINT('Ctrl Pts',(-26.3262327535223,25.1873405106943,-59.2887641588798));
#13836=CARTESIAN_POINT('Ctrl Pts',(-26.3274426994265,25.1852870925777,-59.2886136516078));
#13837=CARTESIAN_POINT('Ctrl Pts',(-26.3351018861276,25.172255536497,-59.2876599806532));
#13838=CARTESIAN_POINT('Ctrl Pts',(-26.3414884236967,25.1612403909098,-59.2868605721563));
#13839=CARTESIAN_POINT('Ctrl Pts',(-26.3496167888251,25.1470275844363,-59.2858379708155));
#13840=CARTESIAN_POINT('Ctrl Pts',(-26.3514185956687,25.1438646223585,-59.285610959987));
#13841=CARTESIAN_POINT('Ctrl Pts',(-26.3541598209943,25.1390335551401,-59.2852650914879));
#13842=CARTESIAN_POINT('Ctrl Pts',(-26.3551031108158,25.1373676681278,-59.2851459829773));
#13843=CARTESIAN_POINT('Ctrl Pts',(-26.3568699359783,25.1342408905075,-59.2849227180134));
#13844=CARTESIAN_POINT('Ctrl Pts',(-26.3576938123972,25.1327802029616,-59.2848185396237));
#13845=CARTESIAN_POINT('Ctrl Pts',(-26.359583420729,25.1294239117079,-59.2845794412114));
#13846=CARTESIAN_POINT('Ctrl Pts',(-26.3606483724248,25.1275278754472,-59.2844445723346));
#13847=CARTESIAN_POINT('Ctrl Pts',(-26.3635963558023,25.1222668315239,-59.2840709011512));
#13848=CARTESIAN_POINT('Ctrl Pts',(-26.3654752763796,25.1188995059018,-59.2838323649796));
#13849=CARTESIAN_POINT('Ctrl Pts',(-26.3757462915563,25.1004143140987,-59.2825263178782));
#13850=CARTESIAN_POINT('Ctrl Pts',(-26.3840228673712,25.0852320933438,-59.2814661478453));
#13851=CARTESIAN_POINT('Ctrl Pts',(-26.4763747015305,24.912532496034,-59.2695392206124));
#13852=CARTESIAN_POINT('Ctrl Pts',(-26.5473550593576,24.7483314634637,-59.2594338347735));
#13853=CARTESIAN_POINT('Ctrl Pts',(-26.6803649272072,24.3534834145053,-59.2360854118378));
#13854=CARTESIAN_POINT('Ctrl Pts',(-26.7311246740143,24.1201884594064,-59.2229448018575));
#13855=CARTESIAN_POINT('Ctrl Pts',(-26.7630731735512,23.8128200014024,-59.2048042980629));
#13856=CARTESIAN_POINT('Ctrl Pts',(-26.7680772354701,23.7419845696795,-59.2005735311872));
#13857=CARTESIAN_POINT('Ctrl Pts',(-26.77132769563,23.655323377254,-59.1953143184888));
#13858=CARTESIAN_POINT('Ctrl Pts',(-26.7718022479562,23.6395974042291,-59.1943566445975));
#13859=CARTESIAN_POINT('Ctrl Pts',(-26.7722902779298,23.6182381556008,-59.1930512260462));
#13860=CARTESIAN_POINT('Ctrl Pts',(-26.7724041694362,23.6126072106243,-59.1927066356586));
#13861=CARTESIAN_POINT('Ctrl Pts',(-26.7725606275242,23.60371940819,-59.1921620312279));
#13862=CARTESIAN_POINT('Ctrl Pts',(-26.7726130187481,23.6004627167359,-59.1919623258699));
#13863=CARTESIAN_POINT('Ctrl Pts',(-26.7727080303603,23.5939420817654,-59.191562167882));
#13864=CARTESIAN_POINT('Ctrl Pts',(-26.7727506290721,23.5906781416752,-59.1913617148007));
#13865=CARTESIAN_POINT('Ctrl Pts',(-26.7728257346826,23.5841652255821,-59.1909614226252));
#13866=CARTESIAN_POINT('Ctrl Pts',(-26.7728582872022,23.5809162540493,-59.1907615852135));
#13867=CARTESIAN_POINT('Ctrl Pts',(-26.7729314674546,23.5723138260732,-59.1902320641864));
#13868=CARTESIAN_POINT('Ctrl Pts',(-26.7729636687342,23.566960324726,-59.1899021162766));
#13869=CARTESIAN_POINT('Ctrl Pts',(-26.7729963741845,23.5576773933244,-59.1893292634518));
#13870=CARTESIAN_POINT('Ctrl Pts',(-26.7730030315629,23.5537479876886,-59.1890865530728));
#13871=CARTESIAN_POINT('Ctrl Pts',(-26.77300250248,23.5498185963744,-59.1888436164772));
#13872=CARTESIAN_POINT('Ctrl Pts',(-26.7730025025656,23.5498192324511,-59.1888436558029));
#13873=CARTESIAN_POINT('Ctrl Pts',(-26.773001493321,23.5423127732231,-59.18837956523));
#13874=CARTESIAN_POINT('Ctrl Pts',(-26.7729742579153,23.5348063789239,-59.1879146498276));
#13875=CARTESIAN_POINT('Ctrl Pts',(-26.772760049621,23.5047300513712,-59.1860484802711));
#13876=CARTESIAN_POINT('Ctrl Pts',(-26.7723622029,23.4821627072763,-59.1846406279805));
#13877=CARTESIAN_POINT('Ctrl Pts',(-26.7624295140548,23.1291823529402,-59.1624974702859));
#13878=CARTESIAN_POINT('Ctrl Pts',(-26.7023500228878,22.8022180374915,-59.1399985090511));
#13879=CARTESIAN_POINT('Ctrl Pts',(-26.5476562774506,22.3580846319751,-59.1083315251701));
#13880=CARTESIAN_POINT('Ctrl Pts',(-26.4930734416804,22.2290756608938,-59.0990339118501));
#13881=CARTESIAN_POINT('Ctrl Pts',(-26.4232031559689,22.0899374103821,-59.089187054409));
#13882=CARTESIAN_POINT('Ctrl Pts',(-26.4160331239415,22.0759163541898,-59.0881969728356));
#13883=CARTESIAN_POINT('Ctrl Pts',(-26.4070327165654,22.0586297462103,-59.0869795470382));
#13884=CARTESIAN_POINT('Ctrl Pts',(-26.4052992125504,22.0553144027677,-59.0867462095823));
#13885=CARTESIAN_POINT('Ctrl Pts',(-26.4025607549246,22.0500992123996,-59.0863794023107));
#13886=CARTESIAN_POINT('Ctrl Pts',(-26.4015596741883,22.0481973526393,-59.0862456872293));
#13887=CARTESIAN_POINT('Ctrl Pts',(-26.3996854940338,22.0446453981056,-59.0859960555776));
#13888=CARTESIAN_POINT('Ctrl Pts',(-26.398812869228,22.042995071591,-59.0858801101372));
#13889=CARTESIAN_POINT('Ctrl Pts',(-26.3968512641765,22.0392930305608,-59.0856201074755));
#13890=CARTESIAN_POINT('Ctrl Pts',(-26.3957615018503,22.0372417390399,-59.0854761012659));
#13891=CARTESIAN_POINT('Ctrl Pts',(-26.3929873240509,22.032033421415,-59.0851106127568));
#13892=CARTESIAN_POINT('Ctrl Pts',(-26.3912998616306,22.0288780098104,-59.0848893245861));
#13893=CARTESIAN_POINT('Ctrl Pts',(-26.3819864042907,22.0115321670171,-59.0836735983018));
#13894=CARTESIAN_POINT('Ctrl Pts',(-26.3742591681456,21.9973959289755,-59.0826855278183));
#13895=CARTESIAN_POINT('Ctrl Pts',(-26.2206724689657,21.7213622104056,-59.0634331963671));
#13896=CARTESIAN_POINT('Ctrl Pts',(-26.0390554905465,21.4809746675581,-59.0473022214729));
#13897=CARTESIAN_POINT('Ctrl Pts',(-25.7388581089325,21.1813802753183,-59.0233877385789));
#13898=CARTESIAN_POINT('Ctrl Pts',(-25.6459344015434,21.0987910225589,-59.0162864636352));
#13899=CARTESIAN_POINT('Ctrl Pts',(-25.5092062488695,20.9907361952427,-59.0060282902832));
#13900=CARTESIAN_POINT('Ctrl Pts',(-25.4692146261042,20.9606178818691,-59.0030496950771));
#13901=CARTESIAN_POINT('Ctrl Pts',(-25.405567293561,20.9149681303556,-58.9983325178941));
#13902=CARTESIAN_POINT('Ctrl Pts',(-25.3823800687041,20.8987953189399,-58.9966187188258));
#13903=CARTESIAN_POINT('Ctrl Pts',(-25.3549649188277,20.8802049031615,-58.9945968341571));
#13904=CARTESIAN_POINT('Ctrl Pts',(-25.3509400629459,20.8774888771044,-58.9943001089124));
#13905=CARTESIAN_POINT('Ctrl Pts',(-25.3432571038042,20.8723295458039,-58.993733899174));
#13906=CARTESIAN_POINT('Ctrl Pts',(-25.3396001029525,20.8698846123788,-58.9934644769106));
#13907=CARTESIAN_POINT('Ctrl Pts',(-25.333166978255,20.8656026997601,-58.9929906770902));
#13908=CARTESIAN_POINT('Ctrl Pts',(-25.3303929866641,20.8637625160226,-58.9927864206593));
#13909=CARTESIAN_POINT('Ctrl Pts',(-25.3249620015248,20.8601718667398,-58.9923866144038));
#13910=CARTESIAN_POINT('Ctrl Pts',(-25.3223052560885,20.8584210310031,-58.9921910787959));
#13911=CARTESIAN_POINT('Ctrl Pts',(-25.3159789397954,20.8542653166898,-58.9917255633078));
#13912=CARTESIAN_POINT('Ctrl Pts',(-25.3123070488822,20.8518639959391,-58.9914554503136));
#13913=CARTESIAN_POINT('Ctrl Pts',(-25.2992745000029,20.8433789937982,-58.9904970170305));
#13914=CARTESIAN_POINT('Ctrl Pts',(-25.289887228619,20.8373365153003,-58.9898071585941));
#13915=CARTESIAN_POINT('Ctrl Pts',(-25.1554749916149,20.7518013984008,-58.9799358843084));
#13916=CARTESIAN_POINT('Ctrl Pts',(-25.0251640015263,20.6809856074506,-58.9704330579586));
#13917=CARTESIAN_POINT('Ctrl Pts',(-24.7387144853635,20.5499995875361,-58.9496684935595));
#13918=CARTESIAN_POINT('Ctrl Pts',(-24.5818182177269,20.4925043887988,-58.9383638698499));
#13919=CARTESIAN_POINT('Ctrl Pts',(-24.2489790965615,20.3990793709074,-58.9149747778814));
#13920=CARTESIAN_POINT('Ctrl Pts',(-24.0730198135801,20.3651558245771,-58.902934154453));
#13921=CARTESIAN_POINT('Ctrl Pts',(-23.8780520935766,20.3441707699378,-58.8905173615161));
#13922=CARTESIAN_POINT('Ctrl Pts',(-23.8609529428767,20.3424685455815,-58.8894362249869));
#13923=CARTESIAN_POINT('Ctrl Pts',(-23.8400081922989,20.3405525411167,-58.8881222119395));
#13924=CARTESIAN_POINT('Ctrl Pts',(-23.836175186629,20.3402088235604,-58.8878821608513));
#13925=CARTESIAN_POINT('Ctrl Pts',(-23.8301769474359,20.3396817715871,-58.8875071746285));
#13926=CARTESIAN_POINT('Ctrl Pts',(-23.828012144642,20.3394937612997,-58.8873719757501));
#13927=CARTESIAN_POINT('Ctrl Pts',(-23.8241763027714,20.3391645319003,-58.8871326581322));
#13928=CARTESIAN_POINT('Ctrl Pts',(-23.8225053528891,20.3390224284224,-58.8870284896526));
#13929=CARTESIAN_POINT('Ctrl Pts',(-23.818925306572,20.3387207830438,-58.8868054814773));
#13930=CARTESIAN_POINT('Ctrl Pts',(-23.8170161839889,20.3385616395919,-58.886686664888));
#13931=CARTESIAN_POINT('Ctrl Pts',(-23.8114724715318,20.3381044957956,-58.8863419512227));
#13932=CARTESIAN_POINT('Ctrl Pts',(-23.8078375012695,20.3378109609793,-58.886116307049));
#13933=CARTESIAN_POINT('Ctrl Pts',(-23.7914489263278,20.336515529497,-58.8851006611446));
#13934=CARTESIAN_POINT('Ctrl Pts',(-23.7786896927308,20.3355833890863,-58.8843145488998));
#13935=CARTESIAN_POINT('Ctrl Pts',(-23.763630047216,20.3345733050214,-58.8833917900231));
#13936=CARTESIAN_POINT('Ctrl Pts',(-23.7613349261343,20.3344218340624,-58.8832512989139));
#13937=CARTESIAN_POINT('Ctrl Pts',(-23.4171124108492,20.3120742981944,-58.8622010455887));
#13938=CARTESIAN_POINT('Ctrl Pts',(-23.073767506893,20.3445412287019,-58.8440719261785));
#13939=CARTESIAN_POINT('Ctrl Pts',(-22.6057918403408,20.4657929968855,-58.8165083340587));
#13940=CARTESIAN_POINT('Ctrl Pts',(-22.4721205301946,20.509936676184,-58.8083118917589));
#13941=CARTESIAN_POINT('Ctrl Pts',(-22.3214250898988,20.5708931548459,-58.7984876645301));
#13942=CARTESIAN_POINT('Ctrl Pts',(-22.3011657016223,20.5793299086602,-58.7971545189803));
#13943=CARTESIAN_POINT('Ctrl Pts',(-22.2768457398438,20.5897503654097,-58.7955386893125));
#13944=CARTESIAN_POINT('Ctrl Pts',(-22.2727007949349,20.5915366795579,-58.7952627518792));
#13945=CARTESIAN_POINT('Ctrl Pts',(-22.2647503068868,20.5949828604376,-58.794732417683));
#13946=CARTESIAN_POINT('Ctrl Pts',(-22.2609441895033,20.5966413862766,-58.794478067152));
#13947=CARTESIAN_POINT('Ctrl Pts',(-22.254125306114,20.5996284249456,-58.7940215445662));
#13948=CARTESIAN_POINT('Ctrl Pts',(-22.2511113459824,20.6009542111316,-58.7938194662438));
#13949=CARTESIAN_POINT('Ctrl Pts',(-22.2451081529065,20.6036058941484,-58.7934163780103));
#13950=CARTESIAN_POINT('Ctrl Pts',(-22.2421188954367,20.6049317264847,-58.7932153704933));
#13951=CARTESIAN_POINT('Ctrl Pts',(-22.2348260401936,20.6081796360404,-58.792724259124));
#13952=CARTESIAN_POINT('Ctrl Pts',(-22.2305246402726,20.6101066050235,-58.7924339871553));
#13953=CARTESIAN_POINT('Ctrl Pts',(-22.2141782199864,20.6174726792792,-58.7913285468262));
#13954=CARTESIAN_POINT('Ctrl Pts',(-22.2021626000465,20.6229763648518,-58.790511153796));
#13955=CARTESIAN_POINT('Ctrl Pts',(-21.9951387809537,20.7193474001023,-58.7763431402291));
#13956=CARTESIAN_POINT('Ctrl Pts',(-21.8097179649669,20.8294238408003,-58.7622942973665));
#13957=CARTESIAN_POINT('Ctrl Pts',(-21.5123578952181,21.0488584124524,-58.7374755813763));
#13958=CARTESIAN_POINT('Ctrl Pts',(-21.3948043874316,21.1494132456956,-58.7269434856662));
#13959=CARTESIAN_POINT('Ctrl Pts',(-21.1885849452822,21.3532119939397,-58.7074910834349));
#13960=CARTESIAN_POINT('Ctrl Pts',(-21.0983355838537,21.4544056368952,-58.698554858142));
#13961=CARTESIAN_POINT('Ctrl Pts',(-21.011117776681,21.5655746772111,-58.6897042032825));
#13962=CARTESIAN_POINT('Ctrl Pts',(-21.0075348151863,21.5701671533296,-58.6893402108031));
#13963=CARTESIAN_POINT('Ctrl Pts',(-21.0023887198244,21.5768001848321,-58.6888168693726));
#13964=CARTESIAN_POINT('Ctrl Pts',(-21.0008155720644,21.5788329015405,-58.6886568106564));
#13965=CARTESIAN_POINT('Ctrl Pts',(-20.9980845916661,21.5823704281706,-58.6883788224338));
#13966=CARTESIAN_POINT('Ctrl Pts',(-20.9969256555748,21.5838743810739,-58.6882608138101));
#13967=CARTESIAN_POINT('Ctrl Pts',(-20.9946856021041,21.5867866208807,-58.6880326445753));
#13968=CARTESIAN_POINT('Ctrl Pts',(-20.9936043220335,21.5881947734673,-58.6879224721492));
#13969=CARTESIAN_POINT('Ctrl Pts',(-20.9910273633318,21.591556497699,-58.6876598196002));
#13970=CARTESIAN_POINT('Ctrl Pts',(-20.9895327544445,21.5935108935456,-58.6875074159428));
#13971=CARTESIAN_POINT('Ctrl Pts',(-20.9850253884199,21.5994188705874,-58.6870475926769));
#13972=CARTESIAN_POINT('Ctrl Pts',(-20.9820195205409,21.603377735745,-58.686740659253));
#13973=CARTESIAN_POINT('Ctrl Pts',(-20.9516224535746,21.6436049640416,-58.6836336727583));
#13974=CARTESIAN_POINT('Ctrl Pts',(-20.9249905207913,21.6804442200023,-58.6808859070166));
#13975=CARTESIAN_POINT('Ctrl Pts',(-20.8977793166635,21.7198129187281,-58.6780363888251));
#13976=CARTESIAN_POINT('Ctrl Pts',(-20.8964156489309,21.7217905734019,-58.6778934727619));
#13977=CARTESIAN_POINT('Ctrl Pts',(-20.8864714990291,21.7362466036971,-58.6768504450948));
#13978=CARTESIAN_POINT('Ctrl Pts',(-20.877976711757,21.7487840044718,-58.6759547852332));
#13979=CARTESIAN_POINT('Ctrl Pts',(-20.8512017457157,21.7889071608909,-58.6731151766026));
#13980=CARTESIAN_POINT('Ctrl Pts',(-20.8332574976359,21.8167154589597,-58.6711870238619));
#13981=CARTESIAN_POINT('Ctrl Pts',(-20.6703885784722,22.0778575174049,-58.6534002399766));
#13982=CARTESIAN_POINT('Ctrl Pts',(-20.5554178950077,22.3285528735227,-58.6385759778142));
#13983=CARTESIAN_POINT('Ctrl Pts',(-20.4361480242849,22.7110120429233,-58.6156094117335));
#13984=CARTESIAN_POINT('Ctrl Pts',(-20.4057432964606,22.8332954223543,-58.6082348308084));
#13985=CARTESIAN_POINT('Ctrl Pts',(-20.3787897730317,22.9772225194858,-58.5993782083686));
#13986=CARTESIAN_POINT('Ctrl Pts',(-20.3752022182044,22.9974461452436,-58.5981299046236));
#13987=CARTESIAN_POINT('Ctrl Pts',(-20.3710770630506,23.022066501213,-58.5966051590859));
#13988=CARTESIAN_POINT('Ctrl Pts',(-20.3703548347266,23.0264321619743,-58.596334600014));
#13989=CARTESIAN_POINT('Ctrl Pts',(-20.3689827382897,23.0348335049292,-58.5958135562095));
#13990=CARTESIAN_POINT('Ctrl Pts',(-20.3683315522046,23.0388689656509,-58.5955631138558));
#13991=CARTESIAN_POINT('Ctrl Pts',(-20.3671708615304,23.0461499266162,-58.5951109498225));
#13992=CARTESIAN_POINT('Ctrl Pts',(-20.366658637827,23.0493949928832,-58.5949093148692));
#13993=CARTESIAN_POINT('Ctrl Pts',(-20.3655679060968,23.0563743306451,-58.5944754109343));
#13994=CARTESIAN_POINT('Ctrl Pts',(-20.3649910027322,23.0601088446916,-58.5942430912957));
#13995=CARTESIAN_POINT('Ctrl Pts',(-20.363501949916,23.0698617068008,-58.5936359928289));
#13996=CARTESIAN_POINT('Ctrl Pts',(-20.3626002841209,23.0758816189761,-58.5932608817339));
#13997=CARTESIAN_POINT('Ctrl Pts',(-20.3588037268402,23.1017287443471,-58.5916486351362));
#13998=CARTESIAN_POINT('Ctrl Pts',(-20.3560767780575,23.1215798272964,-58.590406186325));
#13999=CARTESIAN_POINT('Ctrl Pts',(-20.304566254436,23.5243818242112,-58.5651060962574));
#14000=CARTESIAN_POINT('Ctrl Pts',(-20.3248178406907,23.912941330978,-58.5385028384232));
#14001=CARTESIAN_POINT('Ctrl Pts',(-20.4317317993905,24.3672543191509,-58.5074053468197));
#14002=CARTESIAN_POINT('Ctrl Pts',(-20.4532261725621,24.4452907280291,-58.5020870212114));
#14003=CARTESIAN_POINT('Ctrl Pts',(-20.4872977750534,24.5529744949696,-58.4948541146297));
#14004=CARTESIAN_POINT('Ctrl Pts',(-20.4974136910194,24.5833635534687,-58.4928250515242));
#14005=CARTESIAN_POINT('Ctrl Pts',(-20.5094920716253,24.6179202466401,-58.4905356654347));
#14006=CARTESIAN_POINT('Ctrl Pts',(-20.5110119627033,24.6222391405069,-58.4902498608063));
#14007=CARTESIAN_POINT('Ctrl Pts',(-20.5133189258569,24.6287502188104,-58.4898194905888));
#14008=CARTESIAN_POINT('Ctrl Pts',(-20.51409917077,24.6309447896521,-58.4896745198874));
#14009=CARTESIAN_POINT('Ctrl Pts',(-20.5155092374294,24.6348972602851,-58.4894135826168));
#14010=CARTESIAN_POINT('Ctrl Pts',(-20.5161382064185,24.6366554544448,-58.4892975653886));
#14011=CARTESIAN_POINT('Ctrl Pts',(-20.517399270915,24.6401709454559,-58.489065703722));
#14012=CARTESIAN_POINT('Ctrl Pts',(-20.5180313632458,24.641928232501,-58.4889498597008));
#14013=CARTESIAN_POINT('Ctrl Pts',(-20.5198210529933,24.6468902227794,-58.4886229121688));
#14014=CARTESIAN_POINT('Ctrl Pts',(-20.5209822102592,24.6500936531925,-58.4884120221826));
#14015=CARTESIAN_POINT('Ctrl Pts',(-20.5258288092757,24.6633986738973,-58.4875368657291));
#14016=CARTESIAN_POINT('Ctrl Pts',(-20.5295597705822,24.6734837800658,-58.486875294705));
#14017=CARTESIAN_POINT('Ctrl Pts',(-20.59806922492,24.8558603580843,-58.4749408711644));
#14018=CARTESIAN_POINT('Ctrl Pts',(-20.6774516131688,25.0223376568686,-58.464511869666));
#14019=CARTESIAN_POINT('Ctrl Pts',(-20.8559396264169,25.3265447913369,-58.444741518809));
#14020=CARTESIAN_POINT('Ctrl Pts',(-20.9525235738024,25.4650210915975,-58.4354088718012));
#14021=CARTESIAN_POINT('Ctrl Pts',(-21.1054726661663,25.6513043714942,-58.4216410975727));
#14022=CARTESIAN_POINT('Ctrl Pts',(-21.1533239035611,25.7057338271597,-58.4174541957901));
#14023=CARTESIAN_POINT('Ctrl Pts',(-21.2395932606114,25.79743489198,-58.4100593058234));
#14024=CARTESIAN_POINT('Ctrl Pts',(-21.2771811350854,25.8354485335515,-58.4068838419896));
#14025=CARTESIAN_POINT('Ctrl Pts',(-21.33709357661,25.893098415411,-58.4018802634256));
#14026=CARTESIAN_POINT('Ctrl Pts',(-21.3587747315375,25.9133911979107,-58.4000808201304));
#14027=CARTESIAN_POINT('Ctrl Pts',(-21.3843724775686,25.9366945237636,-58.3979680376016));
#14028=CARTESIAN_POINT('Ctrl Pts',(-21.3880198559338,25.9399997245624,-58.3976672642202));
#14029=CARTESIAN_POINT('Ctrl Pts',(-21.3949768861788,25.9462751171864,-58.3970940786593));
#14030=CARTESIAN_POINT('Ctrl Pts',(-21.3982851446142,25.9492468424358,-58.3968217320333));
#14031=CARTESIAN_POINT('Ctrl Pts',(-21.4040864974329,25.9544363953292,-58.3963445228957));
#14032=CARTESIAN_POINT('Ctrl Pts',(-21.4065769108486,25.9566572211087,-58.3961397869388));
#14033=CARTESIAN_POINT('Ctrl Pts',(-21.4114387032384,25.9609791872814,-58.3957403342285));
#14034=CARTESIAN_POINT('Ctrl Pts',(-21.4138097413217,25.9630807071136,-58.3955456337144));
#14035=CARTESIAN_POINT('Ctrl Pts',(-21.4194328182804,25.9680498164752,-58.39508414095));
#14036=CARTESIAN_POINT('Ctrl Pts',(-21.4226875469971,25.970914341401,-58.3948172209147));
#14037=CARTESIAN_POINT('Ctrl Pts',(-21.4341147159336,25.9809306766902,-58.3938807691778));
#14038=CARTESIAN_POINT('Ctrl Pts',(-21.4423174471384,25.9880476778286,-58.3932097904491));
#14039=CARTESIAN_POINT('Ctrl Pts',(-21.4560650976963,25.9998543954388,-58.3920872281015));
#14040=CARTESIAN_POINT('Ctrl Pts',(-21.4615902213282,26.0045671104393,-58.391636605378));
#14041=CARTESIAN_POINT('Ctrl Pts',(-21.6537771844614,26.167376127419,-58.3759800759438));
#14042=CARTESIAN_POINT('Ctrl Pts',(-21.8577372505861,26.3036586156245,-58.3598577180973));
#14043=CARTESIAN_POINT('Ctrl Pts',(-22.0750360184326,26.4155367761454,-58.3433576442193));
#14044=CARTESIAN_POINT('Origin',(-23.5502525316942,23.5502525316942,-77.3107734492734));
#14045=CARTESIAN_POINT('',(-22.075035785626,26.4155366562829,-56.8443273945297));
#14046=CARTESIAN_POINT('',(-22.0750360153845,26.415536774576,-57.0898644896988));
#14047=CARTESIAN_POINT('',(-22.0750360153461,26.4155367745563,-77.3107734492734));
#14048=CARTESIAN_POINT('Ctrl Pts',(-22.075035785626,26.4155366562829,-56.8443273945297));
#14049=CARTESIAN_POINT('Ctrl Pts',(-21.9787534219905,26.3659648340796,-56.8514812887004));
#14050=CARTESIAN_POINT('Ctrl Pts',(-21.8849666919604,26.3115384755299,-56.8587625386307));
#14051=CARTESIAN_POINT('Ctrl Pts',(-21.6524805710828,26.1604409150557,-56.8775039548766));
#14052=CARTESIAN_POINT('Ctrl Pts',(-21.5183623236558,26.0574519636375,-56.8890011346993));
#14053=CARTESIAN_POINT('Ctrl Pts',(-21.3414921867163,25.8980789192696,-56.9046470810564));
#14054=CARTESIAN_POINT('Ctrl Pts',(-21.2915601152839,25.8500832300346,-56.9091233591186));
#14055=CARTESIAN_POINT('Ctrl Pts',(-21.2354754770223,25.7925833335758,-56.9141821068135));
#14056=CARTESIAN_POINT('Ctrl Pts',(-21.2277826134483,25.7846145715778,-56.9148766884109));
#14057=CARTESIAN_POINT('Ctrl Pts',(-21.2178451067199,25.7742138879402,-56.9157746549309));
#14058=CARTESIAN_POINT('Ctrl Pts',(-21.2155630338008,25.7718180740115,-56.9159809157184));
#14059=CARTESIAN_POINT('Ctrl Pts',(-21.2118713112045,25.7679303809027,-56.9163146590561));
#14060=CARTESIAN_POINT('Ctrl Pts',(-21.2104593974295,25.7664406699427,-56.9164423181209));
#14061=CARTESIAN_POINT('Ctrl Pts',(-21.207752913517,25.7635795879329,-56.9166870585693));
#14062=CARTESIAN_POINT('Ctrl Pts',(-21.2064581278343,25.7622084334897,-56.9168041566093));
#14063=CARTESIAN_POINT('Ctrl Pts',(-21.2034855259051,25.7590549616847,-56.9170730268537));
#14064=CARTESIAN_POINT('Ctrl Pts',(-21.201808532147,25.7572718644773,-56.9172247347988));
#14065=CARTESIAN_POINT('Ctrl Pts',(-21.1965006081881,25.7516152081032,-56.9177049973031));
#14066=CARTESIAN_POINT('Ctrl Pts',(-21.1928771936804,25.7477345605566,-56.9180329716304));
#14067=CARTESIAN_POINT('Ctrl Pts',(-21.1623460205189,25.7148735016874,-56.9207977646127));
#14068=CARTESIAN_POINT('Ctrl Pts',(-21.1359627199514,25.6854074447381,-56.9231952121615));
#14069=CARTESIAN_POINT('Ctrl Pts',(-21.0144922833713,25.544612351455,-56.9343147534272));
#14070=CARTESIAN_POINT('Ctrl Pts',(-20.9265108846829,25.4273621334583,-56.9426156445672));
#14071=CARTESIAN_POINT('Ctrl Pts',(-20.7540202926931,25.1615422553739,-56.9603937420091));
#14072=CARTESIAN_POINT('Ctrl Pts',(-20.6727316210886,25.0114305752478,-56.9698206861763));
#14073=CARTESIAN_POINT('Ctrl Pts',(-20.5654324896086,24.7692238746175,-56.9849342846938));
#14074=CARTESIAN_POINT('Ctrl Pts',(-20.530987931669,24.6812171312135,-56.9904039706789));
#14075=CARTESIAN_POINT('Ctrl Pts',(-20.4871250515694,24.5527843056446,-56.9984397469981));
#14076=CARTESIAN_POINT('Ctrl Pts',(-20.4745416806035,24.513487937425,-57.0009051438333));
#14077=CARTESIAN_POINT('Ctrl Pts',(-20.4581189076347,24.458594166653,-57.0043631598827));
#14078=CARTESIAN_POINT('Ctrl Pts',(-20.4536360919854,24.4431923313582,-57.0053349057762));
#14079=CARTESIAN_POINT('Ctrl Pts',(-20.4471034785149,24.4201069678507,-57.0067939334481));
#14080=CARTESIAN_POINT('Ctrl Pts',(-20.4449667879056,24.4124481208705,-57.0072783939308));
#14081=CARTESIAN_POINT('Ctrl Pts',(-20.4415854125159,24.4001521470766,-57.0080568631682));
#14082=CARTESIAN_POINT('Ctrl Pts',(-20.4403226996355,24.3955199765698,-57.0083502861289));
#14083=CARTESIAN_POINT('Ctrl Pts',(-20.4379765054927,24.3868367083081,-57.0089006235809));
#14084=CARTESIAN_POINT('Ctrl Pts',(-20.4368905697082,24.3827862794932,-57.0091574578074));
#14085=CARTESIAN_POINT('Ctrl Pts',(-20.4349543714753,24.3755076918735,-57.0096192099041));
#14086=CARTESIAN_POINT('Ctrl Pts',(-20.4341012119435,24.3722803041849,-57.0098240333822));
#14087=CARTESIAN_POINT('Ctrl Pts',(-20.4324488107321,24.3659899530562,-57.0102234008139));
#14088=CARTESIAN_POINT('Ctrl Pts',(-20.431649064064,24.3629271250098,-57.0104179281284));
#14089=CARTESIAN_POINT('Ctrl Pts',(-20.4297672144003,24.3556764301904,-57.010878608629));
#14090=CARTESIAN_POINT('Ctrl Pts',(-20.428689029257,24.3514875606864,-57.0111448885485));
#14091=CARTESIAN_POINT('Ctrl Pts',(-20.4249481560852,24.3368316888835,-57.0120770222557));
#14092=CARTESIAN_POINT('Ctrl Pts',(-20.4223296773429,24.3263535711146,-57.0127443055706));
#14093=CARTESIAN_POINT('Ctrl Pts',(-20.3896846600831,24.1928719732496,-57.0212562561622));
#14094=CARTESIAN_POINT('Ctrl Pts',(-20.3668833237271,24.068231609945,-57.0293339356465));
#14095=CARTESIAN_POINT('Ctrl Pts',(-20.3287378045079,23.7572230138423,-57.0498331318172));
#14096=CARTESIAN_POINT('Ctrl Pts',(-20.3221600858616,23.5702508970748,-57.0624723194976));
#14097=CARTESIAN_POINT('Ctrl Pts',(-20.3412328894607,23.2015053009378,-57.0874566515334));
#14098=CARTESIAN_POINT('Ctrl Pts',(-20.3661302455586,23.0203343057712,-57.0997511017483));
#14099=CARTESIAN_POINT('Ctrl Pts',(-20.4097319132253,22.8267191611916,-57.112304366618));
#14100=CARTESIAN_POINT('Ctrl Pts',(-20.413339323092,22.8112357255337,-57.1133039639425));
#14101=CARTESIAN_POINT('Ctrl Pts',(-20.4179397879531,22.7921308259813,-57.1145315091528));
#14102=CARTESIAN_POINT('Ctrl Pts',(-20.4188247048631,22.7884839244613,-57.1147655689327));
#14103=CARTESIAN_POINT('Ctrl Pts',(-20.4202270348198,22.7827484070829,-57.1151332520048));
#14104=CARTESIAN_POINT('Ctrl Pts',(-20.4207401694365,22.7806587642292,-57.1152671225329));
#14105=CARTESIAN_POINT('Ctrl Pts',(-20.4217023227931,22.7767574530999,-57.115516887477));
#14106=CARTESIAN_POINT('Ctrl Pts',(-20.4221508196027,22.7749456730487,-57.1156328110875));
#14107=CARTESIAN_POINT('Ctrl Pts',(-20.423160111332,22.7708835977116,-57.1158925643706));
#14108=CARTESIAN_POINT('Ctrl Pts',(-20.4237217601743,22.7686335224734,-57.1160363434464));
#14109=CARTESIAN_POINT('Ctrl Pts',(-20.425153358202,22.7629244936862,-57.1164008887338));
#14110=CARTESIAN_POINT('Ctrl Pts',(-20.4260266241675,22.7594663642543,-57.1166214625311));
#14111=CARTESIAN_POINT('Ctrl Pts',(-20.4308409819686,22.7405339818851,-57.1178277569479));
#14112=CARTESIAN_POINT('Ctrl Pts',(-20.4348913906827,22.7250873771118,-57.1188072244354));
#14113=CARTESIAN_POINT('Ctrl Pts',(-20.5147691336677,22.4294404392087,-57.1374745749625));
#14114=CARTESIAN_POINT('Ctrl Pts',(-20.6280092004573,22.1606711405676,-57.1531557945039));
#14115=CARTESIAN_POINT('Ctrl Pts',(-20.8792886873383,21.7354543153442,-57.1809492399011));
#14116=CARTESIAN_POINT('Ctrl Pts',(-20.999180282478,21.570466722419,-57.1926483494376));
#14117=CARTESIAN_POINT('Ctrl Pts',(-21.1393696894901,21.4116006227812,-57.2055271940008));
#14118=CARTESIAN_POINT('Ctrl Pts',(-21.1449499404476,21.4053265402471,-57.2060385987421));
#14119=CARTESIAN_POINT('Ctrl Pts',(-21.1551297342623,21.3939707024617,-57.2069693305155));
#14120=CARTESIAN_POINT('Ctrl Pts',(-21.1597211046626,21.3888816618329,-57.2073883127261));
#14121=CARTESIAN_POINT('Ctrl Pts',(-21.1669304809689,21.3809419164974,-57.2080449634729));
#14122=CARTESIAN_POINT('Ctrl Pts',(-21.1695374657921,21.3780811946546,-57.2082821641948));
#14123=CARTESIAN_POINT('Ctrl Pts',(-21.1742445642324,21.3729346089454,-57.2087099992382));
#14124=CARTESIAN_POINT('Ctrl Pts',(-21.1763428423395,21.3706470662836,-57.2089005552278));
#14125=CARTESIAN_POINT('Ctrl Pts',(-21.1807349368601,21.3658726708806,-57.2092990941281));
#14126=CARTESIAN_POINT('Ctrl Pts',(-21.1830293696387,21.3633863927993,-57.2095071032583));
#14127=CARTESIAN_POINT('Ctrl Pts',(-21.1895805315942,21.3563098567985,-57.2101004886907));
#14128=CARTESIAN_POINT('Ctrl Pts',(-21.1938467091409,21.3517284014341,-57.2104862699737));
#14129=CARTESIAN_POINT('Ctrl Pts',(-21.2121014262799,21.3322388024099,-57.2121343274996));
#14130=CARTESIAN_POINT('Ctrl Pts',(-21.2262180570752,21.3174517737205,-57.2134021250355));
#14131=CARTESIAN_POINT('Ctrl Pts',(-21.4900409326243,21.0463125837041,-57.2369775133577));
#14132=CARTESIAN_POINT('Ctrl Pts',(-21.7805474204764,20.8332339258834,-57.2614182908657));
#14133=CARTESIAN_POINT('Ctrl Pts',(-22.1812457672801,20.6313101870808,-57.2915447075511));
#14134=CARTESIAN_POINT('Ctrl Pts',(-22.2642425301839,20.5938045378977,-57.2975914483371));
#14135=CARTESIAN_POINT('Ctrl Pts',(-22.3939019077899,20.5417077698589,-57.3066372881044));
#14136=CARTESIAN_POINT('Ctrl Pts',(-22.4394908231572,20.524579478675,-57.3097442733959));
#14137=CARTESIAN_POINT('Ctrl Pts',(-22.4901754858377,20.5068368108302,-57.3131045555496));
#14138=CARTESIAN_POINT('Ctrl Pts',(-22.4949014627243,20.5051947793383,-57.3134169845457));
#14139=CARTESIAN_POINT('Ctrl Pts',(-22.5019142418998,20.5027764900608,-57.3138792482548));
#14140=CARTESIAN_POINT('Ctrl Pts',(-22.5041980948744,20.5019917965404,-57.3140295828663));
#14141=CARTESIAN_POINT('Ctrl Pts',(-22.5080928197179,20.5006585270708,-57.3142855911142));
#14142=CARTESIAN_POINT('Ctrl Pts',(-22.5097032441791,20.5001086599058,-57.3143913421599));
#14143=CARTESIAN_POINT('Ctrl Pts',(-22.5130072497662,20.4989834536204,-57.3146080878458));
#14144=CARTESIAN_POINT('Ctrl Pts',(-22.5147008707371,20.4984082500803,-57.3147190742067));
#14145=CARTESIAN_POINT('Ctrl Pts',(-22.5187724384136,20.4970292053672,-57.3149856138111));
#14146=CARTESIAN_POINT('Ctrl Pts',(-22.5211508516008,20.4962267303313,-57.3151410853452));
#14147=CARTESIAN_POINT('Ctrl Pts',(-22.5297992193545,20.4933200267489,-57.315705589506));
#14148=CARTESIAN_POINT('Ctrl Pts',(-22.5360747659316,20.491232302315,-57.3161136467885));
#14149=CARTESIAN_POINT('Ctrl Pts',(-22.6409607842142,20.4566974728741,-57.3229082672942));
#14150=CARTESIAN_POINT('Ctrl Pts',(-22.7410880546166,20.4290104137616,-57.3290203405196));
#14151=CARTESIAN_POINT('Ctrl Pts',(-22.9831577841715,20.3745098512569,-57.3432953426676));
#14152=CARTESIAN_POINT('Ctrl Pts',(-23.1259042470933,20.3523045906114,-57.3513174689769));
#14153=CARTESIAN_POINT('Ctrl Pts',(-23.4180526323383,20.3267718197978,-57.3677092329405));
#14154=CARTESIAN_POINT('Ctrl Pts',(-23.5671537066462,20.3241070382694,-57.3760645612205));
#14155=CARTESIAN_POINT('Ctrl Pts',(-23.8166056746375,20.336945372979,-57.3905342819759));
#14156=CARTESIAN_POINT('Ctrl Pts',(-23.9170076857217,20.3468520829169,-57.3964902163793));
#14157=CARTESIAN_POINT('Ctrl Pts',(-24.0285123938727,20.3631651745485,-57.4033168076524));
#14158=CARTESIAN_POINT('Ctrl Pts',(-24.0402417686993,20.3649473878158,-57.4040375160963));
#14159=CARTESIAN_POINT('Ctrl Pts',(-24.058260471906,20.3677871092181,-57.4051487818947));
#14160=CARTESIAN_POINT('Ctrl Pts',(-24.0645570323616,20.3687986011385,-57.4055378822683));
#14161=CARTESIAN_POINT('Ctrl Pts',(-24.0762592041456,20.3707141090935,-57.4062624817363));
#14162=CARTESIAN_POINT('Ctrl Pts',(-24.0816656007299,20.3716132395239,-57.4065978247122));
#14163=CARTESIAN_POINT('Ctrl Pts',(-24.0905729342214,20.3731179660284,-57.4071512835643));
#14164=CARTESIAN_POINT('Ctrl Pts',(-24.0940752250131,20.373715570819,-57.4073691446976));
#14165=CARTESIAN_POINT('Ctrl Pts',(-24.1009204603798,20.3748952433054,-57.4077954379789));
#14166=CARTESIAN_POINT('Ctrl Pts',(-24.1042634889696,20.3754768017118,-57.4080038536396));
#14167=CARTESIAN_POINT('Ctrl Pts',(-24.1119698175781,20.3768299492102,-57.4084848150498));
#14168=CARTESIAN_POINT('Ctrl Pts',(-24.1163324498675,20.3776052581688,-57.4087574791071));
#14169=CARTESIAN_POINT('Ctrl Pts',(-24.129904648205,20.3800461383003,-57.4096069525183));
#14170=CARTESIAN_POINT('Ctrl Pts',(-24.13910850554,20.3817428201748,-57.4101847536839));
#14171=CARTESIAN_POINT('Ctrl Pts',(-24.2171353188215,20.3964783601849,-57.4150980914831));
#14172=CARTESIAN_POINT('Ctrl Pts',(-24.2855189839271,20.411716857637,-57.419503676993));
#14173=CARTESIAN_POINT('Ctrl Pts',(-24.3607691900882,20.4310797195666,-57.4244684760952));
#14174=CARTESIAN_POINT('Ctrl Pts',(-24.3681836488256,20.4330157791535,-57.4249589249305));
#14175=CARTESIAN_POINT('Ctrl Pts',(-24.4067534386304,20.4432341841526,-57.4275168160622));
#14176=CARTESIAN_POINT('Ctrl Pts',(-24.4377892763695,20.4519569956387,-57.4295975182437));
#14177=CARTESIAN_POINT('Ctrl Pts',(-24.730714678217,20.5390478537564,-57.4494483225039));
#14178=CARTESIAN_POINT('Ctrl Pts',(-24.9817451911856,20.6499708614781,-57.4682160525611));
#14179=CARTESIAN_POINT('Ctrl Pts',(-25.2768349754446,20.8280975517229,-57.4912957714844));
#14180=CARTESIAN_POINT('Ctrl Pts',(-25.3367176130824,20.8670159725454,-57.4960298636663));
#14181=CARTESIAN_POINT('Ctrl Pts',(-25.4214636029922,20.9261892748994,-57.5027541369589));
#14182=CARTESIAN_POINT('Ctrl Pts',(-25.4473933803156,20.9448743219154,-57.5048149752787));
#14183=CARTESIAN_POINT('Ctrl Pts',(-25.4942911135781,20.9797403943836,-57.5085423832999));
#14184=CARTESIAN_POINT('Ctrl Pts',(-25.5153456343185,20.9957999748593,-57.5102158144696));
#14185=CARTESIAN_POINT('Ctrl Pts',(-25.5396381965608,21.0148075431134,-57.512144308288));
#14186=CARTESIAN_POINT('Ctrl Pts',(-25.5430703041788,21.0175042339154,-57.5124167159445));
#14187=CARTESIAN_POINT('Ctrl Pts',(-25.5482903446001,21.0216229267001,-57.5128309358159));
#14188=CARTESIAN_POINT('Ctrl Pts',(-25.5500822441779,21.0230398571851,-57.5129731089533));
#14189=CARTESIAN_POINT('Ctrl Pts',(-25.5531926295689,21.0255047495548,-57.513219861022));
#14190=CARTESIAN_POINT('Ctrl Pts',(-25.5545117973484,21.0265518372424,-57.5133245025078));
#14191=CARTESIAN_POINT('Ctrl Pts',(-25.557273549318,21.0287475054144,-57.5135435534564));
#14192=CARTESIAN_POINT('Ctrl Pts',(-25.5587159644664,21.0298962866376,-57.5136579476473));
#14193=CARTESIAN_POINT('Ctrl Pts',(-25.5627299546159,21.0330987788582,-57.5139762549411));
#14194=CARTESIAN_POINT('Ctrl Pts',(-25.5652993803058,21.0351551993199,-57.5141799726205));
#14195=CARTESIAN_POINT('Ctrl Pts',(-25.5755559084583,21.0433897403,-57.514993039298));
#14196=CARTESIAN_POINT('Ctrl Pts',(-25.5832178887337,21.0495992798684,-57.515600146482));
#14197=CARTESIAN_POINT('Ctrl Pts',(-25.5963664869716,21.0603557432588,-57.5166417442614));
#14198=CARTESIAN_POINT('Ctrl Pts',(-25.6018666928503,21.0648858241562,-57.5170773805794));
#14199=CARTESIAN_POINT('Ctrl Pts',(-25.827318673629,21.2518310391726,-57.534933020719));
#14200=CARTESIAN_POINT('Ctrl Pts',(-26.0220911337097,21.4627069673224,-57.5503992707049));
#14201=CARTESIAN_POINT('Ctrl Pts',(-26.2760799688016,21.8239186922099,-57.5752244890746));
#14202=CARTESIAN_POINT('Ctrl Pts',(-26.3562861527551,21.9576033908593,-57.5841076447431));
#14203=CARTESIAN_POINT('Ctrl Pts',(-26.4529547948706,22.1488698209321,-57.596818849528));
#14204=CARTESIAN_POINT('Ctrl Pts',(-26.4779632331838,22.2018967543072,-57.600341393175));
#14205=CARTESIAN_POINT('Ctrl Pts',(-26.5048224543494,22.2631231298406,-57.6044173391429));
#14206=CARTESIAN_POINT('Ctrl Pts',(-26.5081052950817,22.2706852012635,-57.6049209027706));
#14207=CARTESIAN_POINT('Ctrl Pts',(-26.513012302238,22.2821083562651,-57.6056818241388));
#14208=CARTESIAN_POINT('Ctrl Pts',(-26.5146580327185,22.2859601869963,-57.6059384449492));
#14209=CARTESIAN_POINT('Ctrl Pts',(-26.5174832292158,22.2926084003576,-57.6063814458069));
#14210=CARTESIAN_POINT('Ctrl Pts',(-26.5186662659232,22.2954032675443,-57.6065677038356));
#14211=CARTESIAN_POINT('Ctrl Pts',(-26.5211016763572,22.3011795236997,-57.606952700072));
#14212=CARTESIAN_POINT('Ctrl Pts',(-26.5223535138616,22.3041611340366,-57.6071514562974));
#14213=CARTESIAN_POINT('Ctrl Pts',(-26.5253681444558,22.3113717283107,-57.6076321881781));
#14214=CARTESIAN_POINT('Ctrl Pts',(-26.5271264074449,22.3156025886634,-57.6079143175325));
#14215=CARTESIAN_POINT('Ctrl Pts',(-26.5335933949118,22.3312580484656,-57.6089585022715));
#14216=CARTESIAN_POINT('Ctrl Pts',(-26.5382453754699,22.3427058390163,-57.609722479712));
#14217=CARTESIAN_POINT('Ctrl Pts',(-26.5446068321449,22.3586222317033,-57.6107853453557));
#14218=CARTESIAN_POINT('Ctrl Pts',(-26.5463724105512,22.3630684180858,-57.611082325424));
#14219=CARTESIAN_POINT('Ctrl Pts',(-26.6369540365441,22.592665634321,-57.626421988852));
#14220=CARTESIAN_POINT('Ctrl Pts',(-26.7001152711013,22.8270532248162,-57.6423642392652));
#14221=CARTESIAN_POINT('Ctrl Pts',(-26.7608689148892,23.2269949487658,-57.6696646844548));
#14222=CARTESIAN_POINT('Ctrl Pts',(-26.7730881305036,23.3893607307603,-57.6807487437269));
#14223=CARTESIAN_POINT('Ctrl Pts',(-26.7729839918252,23.5861380660709,-57.6937944397921));
#14224=CARTESIAN_POINT('Ctrl Pts',(-26.7724221417273,23.6203167171048,-57.696045622921));
#14225=CARTESIAN_POINT('Ctrl Pts',(-26.7710409059422,23.6630022442621,-57.6988338138257));
#14226=CARTESIAN_POINT('Ctrl Pts',(-26.7707313581014,23.6715223995904,-57.6993891830459));
#14227=CARTESIAN_POINT('Ctrl Pts',(-26.7682026125359,23.7342620564598,-57.7034697214162));
#14228=CARTESIAN_POINT('Ctrl Pts',(-26.7646479461816,23.7884231079927,-57.7069427870855));
#14229=CARTESIAN_POINT('Ctrl Pts',(-26.7592542071133,23.8476629809551,-57.7106686201622));
#14230=CARTESIAN_POINT('Ctrl Pts',(-26.7587690123611,23.8528524695099,-57.7109943922837));
#14231=CARTESIAN_POINT('Ctrl Pts',(-26.758030548068,23.8605493426267,-57.7114766299617));
#14232=CARTESIAN_POINT('Ctrl Pts',(-26.7577869267436,23.8630576113967,-57.711633634711));
#14233=CARTESIAN_POINT('Ctrl Pts',(-26.7573651013253,23.8673483169139,-57.7119019552955));
#14234=CARTESIAN_POINT('Ctrl Pts',(-26.7571883532734,23.8691308903167,-57.7120133535878));
#14235=CARTESIAN_POINT('Ctrl Pts',(-26.7568409205414,23.8726053798327,-57.7122303363479));
#14236=CARTESIAN_POINT('Ctrl Pts',(-26.7566703834452,23.874297303562,-57.7123359286436));
#14237=CARTESIAN_POINT('Ctrl Pts',(-26.7562552038427,23.8783839431238,-57.7125908093618));
#14238=CARTESIAN_POINT('Ctrl Pts',(-26.7560092167573,23.8807785265179,-57.7127400211164));
#14239=CARTESIAN_POINT('Ctrl Pts',(-26.7552477362043,23.8881104072836,-57.7131964743414));
#14240=CARTESIAN_POINT('Ctrl Pts',(-26.7547235147357,23.8930468208196,-57.7135032227058));
#14241=CARTESIAN_POINT('Ctrl Pts',(-26.7491482654588,23.9444164564389,-57.7166895480072));
#14242=CARTESIAN_POINT('Ctrl Pts',(-26.7430994569822,23.9907388423935,-57.7195136428977));
#14243=CARTESIAN_POINT('Ctrl Pts',(-26.7226699101142,24.1244745162531,-57.7275666461143));
#14244=CARTESIAN_POINT('Ctrl Pts',(-26.7056893718887,24.2114512237485,-57.7326795210357));
#14245=CARTESIAN_POINT('Ctrl Pts',(-26.6020635110297,24.6461158990387,-57.7580858572473));
#14246=CARTESIAN_POINT('Ctrl Pts',(-26.4614706814001,24.9782876357169,-57.7773551319302));
#14247=CARTESIAN_POINT('Ctrl Pts',(-26.2665308637976,25.2846033512845,-57.7992700346422));
#14248=CARTESIAN_POINT('Ctrl Pts',(-26.2639368253878,25.2886593588334,-57.7995609610588));
#14249=CARTESIAN_POINT('Ctrl Pts',(-26.2506227660785,25.3093746453076,-57.801050654163));
#14250=CARTESIAN_POINT('Ctrl Pts',(-26.2397585713089,25.3259403558809,-57.8022546791669));
#14251=CARTESIAN_POINT('Ctrl Pts',(-26.2253040858814,25.3475435423131,-57.8038420411924));
#14252=CARTESIAN_POINT('Ctrl Pts',(-26.2218508843045,25.3526725814879,-57.8042201984081));
#14253=CARTESIAN_POINT('Ctrl Pts',(-26.2164941373886,25.3605797407435,-57.8048051837565));
#14254=CARTESIAN_POINT('Ctrl Pts',(-26.2146009489332,25.3633648876113,-57.805011618792));
#14255=CARTESIAN_POINT('Ctrl Pts',(-26.2108191851299,25.3689096812193,-57.8054233694646));
#14256=CARTESIAN_POINT('Ctrl Pts',(-26.2089306730903,25.371669366255,-57.8056286825275));
#14257=CARTESIAN_POINT('Ctrl Pts',(-26.2047303562659,25.3777868434388,-57.8060846567146));
#14258=CARTESIAN_POINT('Ctrl Pts',(-26.20241647141,25.3811431942882,-57.806335396964));
#14259=CARTESIAN_POINT('Ctrl Pts',(-26.195708654156,25.3908336612321,-57.8070609916497));
#14260=CARTESIAN_POINT('Ctrl Pts',(-26.1912983774939,25.3971563811165,-57.8075364708455));
#14261=CARTESIAN_POINT('Ctrl Pts',(-26.1610596585181,25.4401778253492,-57.8107858762578));
#14262=CARTESIAN_POINT('Ctrl Pts',(-26.1344908947206,25.4763478625879,-57.8135882274604));
#14263=CARTESIAN_POINT('Ctrl Pts',(-26.0696892736973,25.5608118703052,-57.8203061493385));
#14264=CARTESIAN_POINT('Ctrl Pts',(-26.0308112346643,25.6085863363356,-57.8242463799302));
#14265=CARTESIAN_POINT('Ctrl Pts',(-25.9007339311162,25.7593883303221,-57.8371506140417));
#14266=CARTESIAN_POINT('Ctrl Pts',(-25.8043082770192,25.8576904025229,-57.8463078512442));
#14267=CARTESIAN_POINT('Ctrl Pts',(-25.5632799908262,26.0738434254434,-57.8681274292378));
#14268=CARTESIAN_POINT('Ctrl Pts',(-25.4141373371226,26.1859170265834,-57.8808537986894));
#14269=CARTESIAN_POINT('Ctrl Pts',(-25.2422907110606,26.2931326170471,-57.89420728767));
#14270=CARTESIAN_POINT('Ctrl Pts',(-25.2283668889402,26.3016733618467,-57.8952803119659));
#14271=CARTESIAN_POINT('Ctrl Pts',(-25.2022942740452,26.3173945168335,-57.8972721877345));
#14272=CARTESIAN_POINT('Ctrl Pts',(-25.1901621169953,26.324601689438,-57.8981921232258));
#14273=CARTESIAN_POINT('Ctrl Pts',(-25.1323314396259,26.3584444145324,-57.9025430874346));
#14274=CARTESIAN_POINT('Ctrl Pts',(-25.0860258504828,26.3840338305953,-57.9059264710256));
#14275=CARTESIAN_POINT('Ctrl Pts',(-25.0340087644373,26.4111296808668,-57.9095999144229));
#14276=CARTESIAN_POINT('Ctrl Pts',(-25.0289023266027,26.4137722899805,-57.9099591915946));
#14277=CARTESIAN_POINT('Ctrl Pts',(-25.0217420173093,26.4174535279334,-57.9104610726678));
#14278=CARTESIAN_POINT('Ctrl Pts',(-25.0196941030025,26.4185036238587,-57.9106043979786));
#14279=CARTESIAN_POINT('Ctrl Pts',(-25.0159460356058,26.4204204286569,-57.9108663104874));
#14280=CARTESIAN_POINT('Ctrl Pts',(-25.0142462353083,26.4212878223167,-57.9109849412684));
#14281=CARTESIAN_POINT('Ctrl Pts',(-25.0107932636177,26.4230459805743,-57.911225621371));
#14282=CARTESIAN_POINT('Ctrl Pts',(-25.0090400467947,26.4239366506211,-57.9113476646143));
#14283=CARTESIAN_POINT('Ctrl Pts',(-25.0047365582959,26.4261179576918,-57.9116468451782));
#14284=CARTESIAN_POINT('Ctrl Pts',(-25.002185376599,26.4274068108606,-57.9118238691087));
#14285=CARTESIAN_POINT('Ctrl Pts',(-24.9928276937194,26.4321186822439,-57.9124719729086));
#14286=CARTESIAN_POINT('Ctrl Pts',(-24.9860107050494,26.4355209902968,-57.9129417545804));
#14287=CARTESIAN_POINT('Ctrl Pts',(-24.827336825953,26.514012323736,-57.923823335674));
#14288=CARTESIAN_POINT('Ctrl Pts',(-24.6697802347036,26.5770482404036,-57.9335047091121));
#14289=CARTESIAN_POINT('Ctrl Pts',(-24.2514023455975,26.7072626506412,-57.9581501985443));
#14290=CARTESIAN_POINT('Ctrl Pts',(-23.9858723488591,26.7547106949737,-57.9728743723621));
#14291=CARTESIAN_POINT('Ctrl Pts',(-23.6474302666284,26.7723018910867,-57.9928542828013));
#14292=CARTESIAN_POINT('Ctrl Pts',(-23.5772291821286,26.7736539504963,-57.9970562658172));
#14293=CARTESIAN_POINT('Ctrl Pts',(-23.4985063217779,26.7725983841183,-58.0018514492364));
#14294=CARTESIAN_POINT('Ctrl Pts',(-23.4899694716123,26.7724499827105,-58.0023725352038));
#14295=CARTESIAN_POINT('Ctrl Pts',(-23.4771117755208,26.7721753546429,-58.0031590354219));
#14296=CARTESIAN_POINT('Ctrl Pts',(-23.4727903818424,26.7720743551809,-58.0034236578061));
#14297=CARTESIAN_POINT('Ctrl Pts',(-23.4653054452788,26.771884349723,-58.0038824984673));
#14298=CARTESIAN_POINT('Ctrl Pts',(-23.4621417980661,26.771799377068,-58.0040765899116));
#14299=CARTESIAN_POINT('Ctrl Pts',(-23.4555725617038,26.7716132494772,-58.0044799378538));
#14300=CARTESIAN_POINT('Ctrl Pts',(-23.4521669993963,26.771511353802,-58.0046892173429));
#14301=CARTESIAN_POINT('Ctrl Pts',(-23.4441712164299,26.771259425467,-58.0051810008845));
#14302=CARTESIAN_POINT('Ctrl Pts',(-23.4395811511118,26.7711049810236,-58.0054636431608));
#14303=CARTESIAN_POINT('Ctrl Pts',(-23.4246723981896,26.7705714307768,-58.0063827558865));
#14304=CARTESIAN_POINT('Ctrl Pts',(-23.4143552781397,26.7701525478769,-58.007020474494));
#14305=CARTESIAN_POINT('Ctrl Pts',(-23.343413630214,26.7669306976237,-58.0114172380227));
#14306=CARTESIAN_POINT('Ctrl Pts',(-23.2828803141626,26.7624654825156,-58.0152282595712));
#14307=CARTESIAN_POINT('Ctrl Pts',(-23.1248937859085,26.7463151805447,-58.0253397031238));
#14308=CARTESIAN_POINT('Ctrl Pts',(-23.0277907558668,26.7318837341394,-58.0317213407487));
#14309=CARTESIAN_POINT('Ctrl Pts',(-22.6566498980242,26.6592762177837,-58.0567259048995));
#14310=CARTESIAN_POINT('Ctrl Pts',(-22.390007204309,26.5699157114752,-58.0761208336613));
#14311=CARTESIAN_POINT('Ctrl Pts',(-22.1303320224281,26.4433514851374,-58.0950564513809));
#14312=CARTESIAN_POINT('Ctrl Pts',(-22.1223965075359,26.439443246119,-58.095635028738));
#14313=CARTESIAN_POINT('Ctrl Pts',(-22.1100213987141,26.4332850697999,-58.09653705736));
#14314=CARTESIAN_POINT('Ctrl Pts',(-22.1055708048224,26.4310574610118,-58.0968614151201));
#14315=CARTESIAN_POINT('Ctrl Pts',(-22.0952494798854,26.425861503324,-58.0976134880033));
#14316=CARTESIAN_POINT('Ctrl Pts',(-22.0893826209059,26.4228854604864,-58.098040875331));
#14317=CARTESIAN_POINT('Ctrl Pts',(-22.0806931123954,26.4184440855088,-58.0986736844957));
#14318=CARTESIAN_POINT('Ctrl Pts',(-22.0778634908441,26.4169925249115,-58.0988797184485));
#14319=CARTESIAN_POINT('Ctrl Pts',(-22.0750360153447,26.4155367745556,-58.0990855609687));
#14320=CARTESIAN_POINT('Ctrl Pts',(-22.0750360184326,26.4155367761454,-58.3433576442193));
#14321=CARTESIAN_POINT('Ctrl Pts',(-22.0901281593173,26.4233070961395,-58.3422116577876));
#14322=CARTESIAN_POINT('Ctrl Pts',(-22.1052846701242,26.4309597084949,-58.3410642954237));
#14323=CARTESIAN_POINT('Ctrl Pts',(-22.2364279498317,26.4958787601458,-58.3311691557945));
#14324=CARTESIAN_POINT('Ctrl Pts',(-22.3557039933747,26.5462339055725,-58.3223815510167));
#14325=CARTESIAN_POINT('Ctrl Pts',(-22.553438829202,26.6160205043767,-58.3084134789393));
#14326=CARTESIAN_POINT('Ctrl Pts',(-22.6301712337128,26.6399164859788,-58.3031342509527));
#14327=CARTESIAN_POINT('Ctrl Pts',(-22.7384979791312,26.669256976992,-58.2959478750621));
#14328=CARTESIAN_POINT('Ctrl Pts',(-22.7693970680516,26.6771358233143,-58.2939278535823));
#14329=CARTESIAN_POINT('Ctrl Pts',(-22.8048575644904,26.6856193082998,-58.291647585646));
#14330=CARTESIAN_POINT('Ctrl Pts',(-22.8093080065541,26.6866740104269,-58.2913620829709));
#14331=CARTESIAN_POINT('Ctrl Pts',(-22.8160272434295,26.6882512902686,-58.2909320759643));
#14332=CARTESIAN_POINT('Ctrl Pts',(-22.8182943598796,26.6887808838902,-58.2907871675429));
#14333=CARTESIAN_POINT('Ctrl Pts',(-22.8223807979513,26.6897307985846,-58.290526297396));
#14334=CARTESIAN_POINT('Ctrl Pts',(-22.8241999067386,26.6901519942429,-58.2904102851269));
#14335=CARTESIAN_POINT('Ctrl Pts',(-22.8281098736785,26.6910537266933,-58.2901611796793));
#14336=CARTESIAN_POINT('Ctrl Pts',(-22.8302008401002,26.6915337554198,-58.2900281164676));
#14337=CARTESIAN_POINT('Ctrl Pts',(-22.8358302020877,26.6928201869604,-58.2896702877299));
#14338=CARTESIAN_POINT('Ctrl Pts',(-22.8393694963512,26.6936227045079,-58.2894457471868));
#14339=CARTESIAN_POINT('Ctrl Pts',(-22.8556198879532,26.6972785509023,-58.2884167449272));
#14340=CARTESIAN_POINT('Ctrl Pts',(-22.8683470919545,26.7000608211285,-58.2876163319013));
#14341=CARTESIAN_POINT('Ctrl Pts',(-22.8830293897624,26.7031773274554,-58.2866989188954));
#14342=CARTESIAN_POINT('Ctrl Pts',(-22.8849680927801,26.703586973877,-58.286577899838));
#14343=CARTESIAN_POINT('Ctrl Pts',(-23.2228095006068,26.7746471639641,-58.2655095392069));
#14344=CARTESIAN_POINT('Ctrl Pts',(-23.567906180619,26.7911979030126,-58.2473526331973));
#14345=CARTESIAN_POINT('Ctrl Pts',(-24.0484227221739,26.7373483792487,-58.2197786642857));
#14346=CARTESIAN_POINT('Ctrl Pts',(-24.1864965811402,26.7126787446447,-58.2116105343705));
#14347=CARTESIAN_POINT('Ctrl Pts',(-24.3437776431076,26.6738586274887,-58.2018196559438));
#14348=CARTESIAN_POINT('Ctrl Pts',(-24.364984485872,26.6683944383741,-58.2004893077125));
#14349=CARTESIAN_POINT('Ctrl Pts',(-24.3904898875052,26.6615447221525,-58.1988764772228));
#14350=CARTESIAN_POINT('Ctrl Pts',(-24.3948437016583,26.660365658865,-58.1986007122132));
#14351=CARTESIAN_POINT('Ctrl Pts',(-24.4031981011387,26.6580843543161,-58.1980706805382));
#14352=CARTESIAN_POINT('Ctrl Pts',(-24.4071990635825,26.6569835183369,-58.1978164599886));
#14353=CARTESIAN_POINT('Ctrl Pts',(-24.4143697760223,26.6549956426005,-58.1973601375791));
#14354=CARTESIAN_POINT('Ctrl Pts',(-24.4175403196909,26.6541114668468,-58.197158129304));
#14355=CARTESIAN_POINT('Ctrl Pts',(-24.4238586989297,26.6523390109858,-58.1967550696866));
#14356=CARTESIAN_POINT('Ctrl Pts',(-24.4270065481141,26.6514507928497,-58.1965540205635));
#14357=CARTESIAN_POINT('Ctrl Pts',(-24.4346896016542,26.6492702583277,-58.1960627181127));
#14358=CARTESIAN_POINT('Ctrl Pts',(-24.4392233225043,26.6479727794613,-58.1957722963993));
#14359=CARTESIAN_POINT('Ctrl Pts',(-24.4564666728861,26.6429970341364,-58.1946657759572));
#14360=CARTESIAN_POINT('Ctrl Pts',(-24.4691563185353,26.6392505001654,-58.1938474470882));
#14361=CARTESIAN_POINT('Ctrl Pts',(-24.4870642390771,26.6338431935135,-58.1926868165577));
#14362=CARTESIAN_POINT('Ctrl Pts',(-24.4923020262258,26.6322470634876,-58.1923466481552));
#14363=CARTESIAN_POINT('Ctrl Pts',(-24.767995228377,26.5474656083807,-58.174404519575));
#14364=CARTESIAN_POINT('Ctrl Pts',(-25.0262628201694,26.4290552393175,-58.1555401074952));
#14365=CARTESIAN_POINT('Ctrl Pts',(-25.3366535812373,26.2338907704219,-58.1307215842277));
#14366=CARTESIAN_POINT('Ctrl Pts',(-25.4058438380496,26.1865234483561,-58.1250457319403));
#14367=CARTESIAN_POINT('Ctrl Pts',(-25.5774071144353,26.0589679075857,-58.1107107810837));
#14368=CARTESIAN_POINT('Ctrl Pts',(-25.6769326304905,25.9751750381768,-58.1021397977599));
#14369=CARTESIAN_POINT('Ctrl Pts',(-25.7769390418986,25.8800698827541,-58.0934743383474));
#14370=CARTESIAN_POINT('Ctrl Pts',(-25.7827220558217,25.8745290925033,-58.0929730600201));
#14371=CARTESIAN_POINT('Ctrl Pts',(-25.7905875241015,25.8669366337263,-58.0922910942411));
#14372=CARTESIAN_POINT('Ctrl Pts',(-25.7926878675749,25.8649036655304,-58.0921089691174));
#14373=CARTESIAN_POINT('Ctrl Pts',(-25.7961974548516,25.8614973989647,-58.0918046209484));
#14374=CARTESIAN_POINT('Ctrl Pts',(-25.7976082067034,25.8601256676899,-58.0916822751784));
#14375=CARTESIAN_POINT('Ctrl Pts',(-25.8003841359177,25.8574215686437,-58.0914415245286));
#14376=CARTESIAN_POINT('Ctrl Pts',(-25.8017493866195,25.8560892808329,-58.091323113723));
#14377=CARTESIAN_POINT('Ctrl Pts',(-25.804756945263,25.8531491194955,-58.0910622482918));
#14378=CARTESIAN_POINT('Ctrl Pts',(-25.8063987206155,25.8515406968749,-58.0909198369607));
#14379=CARTESIAN_POINT('Ctrl Pts',(-25.8121278365362,25.8459159445214,-58.0904228417465));
#14380=CARTESIAN_POINT('Ctrl Pts',(-25.8162062156746,25.8418904400254,-58.0900689774717));
#14381=CARTESIAN_POINT('Ctrl Pts',(-25.8573352573519,25.8010774741601,-58.0864994064073));
#14382=CARTESIAN_POINT('Ctrl Pts',(-25.89350007992,25.7634030736092,-58.0833526594184));
#14383=CARTESIAN_POINT('Ctrl Pts',(-26.0197251671016,25.6253442577002,-58.0722669413419));
#14384=CARTESIAN_POINT('Ctrl Pts',(-26.1043877662657,25.5202020001471,-58.0646319539541));
#14385=CARTESIAN_POINT('Ctrl Pts',(-26.2802448607012,25.2713314487629,-58.0475402950951));
#14386=CARTESIAN_POINT('Ctrl Pts',(-26.3671461432866,25.1250793680689,-58.0381428572326));
#14387=CARTESIAN_POINT('Ctrl Pts',(-26.4834383916648,24.8886485932731,-58.0231050411599));
#14388=CARTESIAN_POINT('Ctrl Pts',(-26.5210778983742,24.8028808996638,-58.0176822776558));
#14389=CARTESIAN_POINT('Ctrl Pts',(-26.5773391157622,24.6578198157146,-58.0084684836536));
#14390=CARTESIAN_POINT('Ctrl Pts',(-26.5980766828193,24.5994072504514,-58.0047478451513));
#14391=CARTESIAN_POINT('Ctrl Pts',(-26.6196820529002,24.5324896235127,-58.0004613009016));
#14392=CARTESIAN_POINT('Ctrl Pts',(-26.6222167560286,24.52453333954,-57.999951268762));
#14393=CARTESIAN_POINT('Ctrl Pts',(-26.6259830367819,24.5125503819739,-57.9991825135579));
#14394=CARTESIAN_POINT('Ctrl Pts',(-26.6272377046428,24.5085309556233,-57.9989245505107));
#14395=CARTESIAN_POINT('Ctrl Pts',(-26.629384080169,24.5016071974087,-57.9984800128447));
#14396=CARTESIAN_POINT('Ctrl Pts',(-26.630279566999,24.4987040351864,-57.9982935626666));
#14397=CARTESIAN_POINT('Ctrl Pts',(-26.6321172260473,24.4927163084262,-57.9979088998263));
#14398=CARTESIAN_POINT('Ctrl Pts',(-26.6330588755116,24.4896315878501,-57.9977106702276));
#14399=CARTESIAN_POINT('Ctrl Pts',(-26.6353177923541,24.4821916942684,-57.9972324192043));
#14400=CARTESIAN_POINT('Ctrl Pts',(-26.6366304675756,24.4778351435648,-57.9969522475009));
#14401=CARTESIAN_POINT('Ctrl Pts',(-26.6414167832772,24.4618275128665,-57.9959223242517));
#14402=CARTESIAN_POINT('Ctrl Pts',(-26.6448336771732,24.4501596958517,-57.9951707176092));
#14403=CARTESIAN_POINT('Ctrl Pts',(-26.7017644455523,24.2515967720816,-57.982363702013));
#14404=CARTESIAN_POINT('Ctrl Pts',(-26.7383155668851,24.0602919703251,-57.9697439698004));
#14405=CARTESIAN_POINT('Ctrl Pts',(-26.767892425798,23.7607147165483,-57.9496252658992));
#14406=CARTESIAN_POINT('Ctrl Pts',(-26.7730956465111,23.6540869327372,-57.9424040245025));
#14407=CARTESIAN_POINT('Ctrl Pts',(-26.772861301319,23.3891758802995,-57.924472682241));
#14408=CARTESIAN_POINT('Ctrl Pts',(-26.7610689928926,23.2311617293045,-57.9137800574437));
#14409=CARTESIAN_POINT('Ctrl Pts',(-26.7375014584333,23.0732159274586,-57.9034438545549));
#14410=CARTESIAN_POINT('Ctrl Pts',(-26.7372876447135,23.0717895433905,-57.9033505400698));
#14411=CARTESIAN_POINT('Ctrl Pts',(-26.7367475210625,23.0682027218339,-57.903115965739));
#14412=CARTESIAN_POINT('Ctrl Pts',(-26.7364199709727,23.0660424684068,-57.9029747573949));
#14413=CARTESIAN_POINT('Ctrl Pts',(-26.7355283805128,23.0602023414174,-57.902593200423));
#14414=CARTESIAN_POINT('Ctrl Pts',(-26.7349601585361,23.0565230978398,-57.9023530281587));
#14415=CARTESIAN_POINT('Ctrl Pts',(-26.7281319367873,23.0128125434734,-57.8995022225768));
#14416=CARTESIAN_POINT('Ctrl Pts',(-26.7211235438683,22.9728993822419,-57.8969241338947));
#14417=CARTESIAN_POINT('Ctrl Pts',(-26.7123532079817,22.92794655253,-57.8940569634939));
#14418=CARTESIAN_POINT('Ctrl Pts',(-26.7113298090217,22.9227687738263,-57.8937272650322));
#14419=CARTESIAN_POINT('Ctrl Pts',(-26.7098068704688,22.9151619142421,-57.8932437247713));
#14420=CARTESIAN_POINT('Ctrl Pts',(-26.7093172463778,22.9127308923864,-57.8930893185433));
#14421=CARTESIAN_POINT('Ctrl Pts',(-26.7084493118811,22.9084470814102,-57.8928174557374));
#14422=CARTESIAN_POINT('Ctrl Pts',(-26.7080721763578,22.906594058396,-57.8926999313552));
#14423=CARTESIAN_POINT('Ctrl Pts',(-26.7072851619569,22.9027444713818,-57.8924559331465));
#14424=CARTESIAN_POINT('Ctrl Pts',(-26.706875020726,22.9007479678098,-57.8923294749072));
#14425=CARTESIAN_POINT('Ctrl Pts',(-26.7058071045568,22.8955744227002,-57.892002003269));
#14426=CARTESIAN_POINT('Ctrl Pts',(-26.705146423495,22.8923979729896,-57.8918011575165));
#14427=CARTESIAN_POINT('Ctrl Pts',(-26.7023266115158,22.8789427126154,-57.8909512770584));
#14428=CARTESIAN_POINT('Ctrl Pts',(-26.7001220037738,22.8686733404397,-57.890304831939));
#14429=CARTESIAN_POINT('Ctrl Pts',(-26.6606148672541,22.6889299848492,-57.8790259237698));
#14430=CARTESIAN_POINT('Ctrl Pts',(-26.6097280936876,22.5227027977409,-57.8691455014788));
#14431=CARTESIAN_POINT('Ctrl Pts',(-26.470152647353,22.1710390875331,-57.8478980584581));
#14432=CARTESIAN_POINT('Ctrl Pts',(-26.3766508420507,21.9883574811137,-57.8366110561598));
#14433=CARTESIAN_POINT('Ctrl Pts',(-26.2375277905399,21.7704892579177,-57.8217159749355));
#14434=CARTESIAN_POINT('Ctrl Pts',(-26.2074775234427,21.7259278493467,-57.8185889697756));
#14435=CARTESIAN_POINT('Ctrl Pts',(-26.134396636561,21.6231953032932,-57.8111635804617));
#14436=CARTESIAN_POINT('Ctrl Pts',(-26.090495099956,21.565682863672,-57.8068362661166));
#14437=CARTESIAN_POINT('Ctrl Pts',(-26.0386413826668,21.5022950130842,-57.8018485841127));
#14438=CARTESIAN_POINT('Ctrl Pts',(-26.0325515527776,21.4949178537161,-57.8012646589804));
#14439=CARTESIAN_POINT('Ctrl Pts',(-26.0236107877756,21.4841847961321,-57.8004099991146));
#14440=CARTESIAN_POINT('Ctrl Pts',(-26.020785636533,21.4808074059546,-57.8001403183797));
#14441=CARTESIAN_POINT('Ctrl Pts',(-26.0157739019455,21.4748409050574,-57.7996625773101));
#14442=CARTESIAN_POINT('Ctrl Pts',(-26.0135901352503,21.4722494282528,-57.7994546327627));
#14443=CARTESIAN_POINT('Ctrl Pts',(-26.0090536827059,21.4668832181567,-57.7990231153765));
#14444=CARTESIAN_POINT('Ctrl Pts',(-26.0067003790471,21.4641090155697,-57.7987995172643));
#14445=CARTESIAN_POINT('Ctrl Pts',(-26.0006365353892,21.4569851132792,-57.7982240101578));
#14446=CARTESIAN_POINT('Ctrl Pts',(-25.9969191202143,21.4526413059168,-57.7978718173583));
#14447=CARTESIAN_POINT('Ctrl Pts',(-25.9814923110168,21.434711849466,-57.7964127934644));
#14448=CARTESIAN_POINT('Ctrl Pts',(-25.9696813419681,21.4212143794269,-57.795301748132));
#14449=CARTESIAN_POINT('Ctrl Pts',(-25.8904338557997,21.3321621106129,-57.7878855502183));
#14450=CARTESIAN_POINT('Ctrl Pts',(-25.8195874607473,21.2597309674257,-57.7814359189196));
#14451=CARTESIAN_POINT('Ctrl Pts',(-25.6361430800605,21.0890596460294,-57.7651428214455));
#14452=CARTESIAN_POINT('Ctrl Pts',(-25.5199063930145,20.9950881138442,-57.7551540095863));
#14453=CARTESIAN_POINT('Ctrl Pts',(-25.3100390879029,20.8482746558424,-57.7378481245175));
#14454=CARTESIAN_POINT('Ctrl Pts',(-25.2194989035662,20.7914212427613,-57.7305925085159));
#14455=CARTESIAN_POINT('Ctrl Pts',(-25.0062494922734,20.6718617890272,-57.7141659010924));
#14456=CARTESIAN_POINT('Ctrl Pts',(-24.8819919540363,20.6123041691172,-57.7050601686616));
#14457=CARTESIAN_POINT('Ctrl Pts',(-24.7462495499219,20.5576309623248,-57.6958637039497));
#14458=CARTESIAN_POINT('Ctrl Pts',(-24.7381945573947,20.554424353584,-57.6953207288191));
#14459=CARTESIAN_POINT('Ctrl Pts',(-24.727221300173,20.5501072305708,-57.6945848630776));
#14460=CARTESIAN_POINT('Ctrl Pts',(-24.7243143128069,20.5489684324868,-57.6943902848737));
#14461=CARTESIAN_POINT('Ctrl Pts',(-24.7197192245325,20.5471760269002,-57.6940832944282));
#14462=CARTESIAN_POINT('Ctrl Pts',(-24.7180322295726,20.5465196180406,-57.6939707124067));
#14463=CARTESIAN_POINT('Ctrl Pts',(-24.7146254793751,20.545197357142,-57.6937436124379));
#14464=CARTESIAN_POINT('Ctrl Pts',(-24.7129057176298,20.5445315644982,-57.6936290989763));
#14465=CARTESIAN_POINT('Ctrl Pts',(-24.7089590145325,20.543007522567,-57.6933665947186));
#14466=CARTESIAN_POINT('Ctrl Pts',(-24.7067316931186,20.5421502715355,-57.6932186649969));
#14467=CARTESIAN_POINT('Ctrl Pts',(-24.7020507657025,20.5403546445047,-57.6929082229934));
#14468=CARTESIAN_POINT('Ctrl Pts',(-24.699596958773,20.5394167920313,-57.6927457423099));
#14469=CARTESIAN_POINT('Ctrl Pts',(-24.6931013850175,20.5369432619664,-57.692316306579));
#14470=CARTESIAN_POINT('Ctrl Pts',(-24.6890576526031,20.5354127094695,-57.6920496564556));
#14471=CARTESIAN_POINT('Ctrl Pts',(-24.6768789234974,20.5308310602049,-57.6912486097138));
#14472=CARTESIAN_POINT('Ctrl Pts',(-24.6687345767766,20.5278046879722,-57.6907156537449));
#14473=CARTESIAN_POINT('Ctrl Pts',(-24.5734787401987,20.4928461579931,-57.6845129884456));
#14474=CARTESIAN_POINT('Ctrl Pts',(-24.48503039339,20.4646537972988,-57.6790531313585));
#14475=CARTESIAN_POINT('Ctrl Pts',(-24.012545636256,20.336240566193,-57.6508460337371));
#14476=CARTESIAN_POINT('Ctrl Pts',(-23.6136996045438,20.3037761247706,-57.6298371751098));
#14477=CARTESIAN_POINT('Ctrl Pts',(-23.2005573627612,20.34647794738,-57.6046907376465));
#14478=CARTESIAN_POINT('Ctrl Pts',(-23.1822130988667,20.3485334228294,-57.6035682954636));
#14479=CARTESIAN_POINT('Ctrl Pts',(-23.1579194144522,20.3514670702012,-57.6020736848084));
#14480=CARTESIAN_POINT('Ctrl Pts',(-23.1519530920721,20.3522044927857,-57.6017059696347));
#14481=CARTESIAN_POINT('Ctrl Pts',(-23.1426819877305,20.3533767248028,-57.601133550244));
#14482=CARTESIAN_POINT('Ctrl Pts',(-23.1393757363282,20.3537999773943,-57.6009292119538));
#14483=CARTESIAN_POINT('Ctrl Pts',(-23.1327498146057,20.3546586504959,-57.6005192972483));
#14484=CARTESIAN_POINT('Ctrl Pts',(-23.1294301543508,20.3550941163849,-57.6003137196296));
#14485=CARTESIAN_POINT('Ctrl Pts',(-23.1220088941542,20.3560793875374,-57.5998536780535));
#14486=CARTESIAN_POINT('Ctrl Pts',(-23.1179076679623,20.3566319207738,-57.599599127983));
#14487=CARTESIAN_POINT('Ctrl Pts',(-23.1058806277696,20.3582758426691,-57.5988517133326));
#14488=CARTESIAN_POINT('Ctrl Pts',(-23.0979578431193,20.3593888421716,-57.5983581645011));
#14489=CARTESIAN_POINT('Ctrl Pts',(-23.0387947472441,20.3679248976131,-57.5946635942759));
#14490=CARTESIAN_POINT('Ctrl Pts',(-22.9877383568938,20.376551925934,-57.5914245306387));
#14491=CARTESIAN_POINT('Ctrl Pts',(-22.819517464538,20.4091629497408,-57.5805752693912));
#14492=CARTESIAN_POINT('Ctrl Pts',(-22.7034915364954,20.4384351103793,-57.5728009439833));
#14493=CARTESIAN_POINT('Ctrl Pts',(-22.2941034905325,20.5663127958848,-57.5443653089498));
#14494=CARTESIAN_POINT('Ctrl Pts',(-22.0136788645596,20.7005624071872,-57.5228118047724));
#14495=CARTESIAN_POINT('Ctrl Pts',(-21.728581975593,20.8915350326729,-57.5007993766879));
#14496=CARTESIAN_POINT('Ctrl Pts',(-21.7007679999795,20.9108075999331,-57.4986528704942));
#14497=CARTESIAN_POINT('Ctrl Pts',(-21.6691364050592,20.9334710293991,-57.4962177120585));
#14498=CARTESIAN_POINT('Ctrl Pts',(-21.6650183868341,20.9364362541925,-57.4959008046928));
#14499=CARTESIAN_POINT('Ctrl Pts',(-21.6589606056353,20.940819990431,-57.4954348160416));
#14500=CARTESIAN_POINT('Ctrl Pts',(-21.6570154238762,20.9422309461526,-57.495285214742));
#14501=CARTESIAN_POINT('Ctrl Pts',(-21.6535516593666,20.9447493373241,-57.4950188772084));
#14502=CARTESIAN_POINT('Ctrl Pts',(-21.6520324672996,20.9458559255371,-57.4949020820221));
#14503=CARTESIAN_POINT('Ctrl Pts',(-21.648871758811,20.9481624384528,-57.494659128461));
#14504=CARTESIAN_POINT('Ctrl Pts',(-21.6472304139525,20.9493625847192,-57.4945329863535));
#14505=CARTESIAN_POINT('Ctrl Pts',(-21.6429316638636,20.9525120651939,-57.4942026716492));
#14506=CARTESIAN_POINT('Ctrl Pts',(-21.6402761024094,20.9544639301392,-57.4939986759504));
#14507=CARTESIAN_POINT('Ctrl Pts',(-21.6344702724293,20.9587450077169,-57.4935527953278));
#14508=CARTESIAN_POINT('Ctrl Pts',(-21.6313212421829,20.9610759022885,-57.4933110269172));
#14509=CARTESIAN_POINT('Ctrl Pts',(-21.6220833895435,20.9679398195423,-57.4926019760612));
#14510=CARTESIAN_POINT('Ctrl Pts',(-21.6160062717144,20.9724886572243,-57.4921357703781));
#14511=CARTESIAN_POINT('Ctrl Pts',(-21.3886087076729,21.1439569702839,-57.4746977634172));
#14512=CARTESIAN_POINT('Ctrl Pts',(-21.1896874341797,21.3387476870802,-57.4596194661077));
#14513=CARTESIAN_POINT('Ctrl Pts',(-20.9403891245932,21.6553839403455,-57.4370157889658));
#14514=CARTESIAN_POINT('Ctrl Pts',(-20.8684880099266,21.7585914140504,-57.4299007935136));
#14515=CARTESIAN_POINT('Ctrl Pts',(-20.7509398647797,21.9503118378088,-57.4168125305644));
#14516=CARTESIAN_POINT('Ctrl Pts',(-20.7030175716611,22.0372384363882,-57.4109226251206));
#14517=CARTESIAN_POINT('Ctrl Pts',(-20.6550482255922,22.1346264576388,-57.4043148359424));
#14518=CARTESIAN_POINT('Ctrl Pts',(-20.6509493816541,22.1430402531512,-57.4037439089759));
#14519=CARTESIAN_POINT('Ctrl Pts',(-20.6449219586856,22.1555510126584,-57.4028948606907));
#14520=CARTESIAN_POINT('Ctrl Pts',(-20.6429652453561,22.1596344317056,-57.4026177191693));
#14521=CARTESIAN_POINT('Ctrl Pts',(-20.6396321081082,22.1666280609066,-57.4021430248748));
#14522=CARTESIAN_POINT('Ctrl Pts',(-20.6382514230955,22.1695362430362,-57.4019456204121));
#14523=CARTESIAN_POINT('Ctrl Pts',(-20.635575278848,22.1751949627429,-57.4015614889778));
#14524=CARTESIAN_POINT('Ctrl Pts',(-20.6342793496017,22.1779452747689,-57.40137477861));
#14525=CARTESIAN_POINT('Ctrl Pts',(-20.6311913432075,22.1845229827326,-57.4009282103254));
#14526=CARTESIAN_POINT('Ctrl Pts',(-20.6294029024605,22.1883520705118,-57.4006682267941));
#14527=CARTESIAN_POINT('Ctrl Pts',(-20.6240713338633,22.1998258748409,-57.3998891165285));
#14528=CARTESIAN_POINT('Ctrl Pts',(-20.6205506702282,22.207480935763,-57.3993692143038));
#14529=CARTESIAN_POINT('Ctrl Pts',(-20.5903277807706,22.2738799770066,-57.3948586574146));
#14530=CARTESIAN_POINT('Ctrl Pts',(-20.5653670992528,22.3333961675514,-57.3908085111017));
#14531=CARTESIAN_POINT('Ctrl Pts',(-20.506155759911,22.4873862029339,-57.3802998529767));
#14532=CARTESIAN_POINT('Ctrl Pts',(-20.4745080522996,22.5827802721712,-57.3737607350352));
#14533=CARTESIAN_POINT('Ctrl Pts',(-20.3567110821023,23.0025386569778,-57.3449054566561));
#14534=CARTESIAN_POINT('Ctrl Pts',(-20.3170631103982,23.3377308047378,-57.3214055662827));
#14535=CARTESIAN_POINT('Ctrl Pts',(-20.3301496682481,23.6810996932893,-57.2996748490436));
#14536=CARTESIAN_POINT('Ctrl Pts',(-20.3304893985411,23.6892086416565,-57.2991631426277));
#14537=CARTESIAN_POINT('Ctrl Pts',(-20.3312587739982,23.7060511412434,-57.2981035163414));
#14538=CARTESIAN_POINT('Ctrl Pts',(-20.3316933386075,23.7147844241825,-57.2975558610218));
#14539=CARTESIAN_POINT('Ctrl Pts',(-20.3323318924463,23.7266445338131,-57.2968146552923));
#14540=CARTESIAN_POINT('Ctrl Pts',(-20.3325048999708,23.7297728861042,-57.2966193859177));
#14541=CARTESIAN_POINT('Ctrl Pts',(-20.3327851870622,23.7347104767502,-57.2963115681221));
#14542=CARTESIAN_POINT('Ctrl Pts',(-20.3328894306236,23.7365198749853,-57.2961988483285));
#14543=CARTESIAN_POINT('Ctrl Pts',(-20.3331027740619,23.7401693482807,-57.2959716627221));
#14544=CARTESIAN_POINT('Ctrl Pts',(-20.3332119255056,23.7420094048535,-57.2958572011021));
#14545=CARTESIAN_POINT('Ctrl Pts',(-20.3334658423222,23.7462286501566,-57.2955949340977));
#14546=CARTESIAN_POINT('Ctrl Pts',(-20.3336116683866,23.7486077698811,-57.2954471894972));
#14547=CARTESIAN_POINT('Ctrl Pts',(-20.3339233397548,23.753601879357,-57.2951373440618));
#14548=CARTESIAN_POINT('Ctrl Pts',(-20.3340897351217,23.7562168348512,-57.2949752742858));
#14549=CARTESIAN_POINT('Ctrl Pts',(-20.3345381102975,23.7631301438645,-57.2945472377938));
#14550=CARTESIAN_POINT('Ctrl Pts',(-20.3348255203135,23.7674281581569,-57.2942815733455));
#14551=CARTESIAN_POINT('Ctrl Pts',(-20.3357155924198,23.7803493601208,-57.2934842092417));
#14552=CARTESIAN_POINT('Ctrl Pts',(-20.3363443378491,23.7889707963507,-57.2929539345866));
#14553=CARTESIAN_POINT('Ctrl Pts',(-20.3387148749443,23.8197672819457,-57.291065679137));
#14554=CARTESIAN_POINT('Ctrl Pts',(-20.3406515865325,23.8419272744109,-57.2897179519423));
#14555=CARTESIAN_POINT('Ctrl Pts',(-20.3512547635775,23.9503005297699,-57.2831730026734));
#14556=CARTESIAN_POINT('Ctrl Pts',(-20.3631669343424,24.0361672154874,-57.2781299364639));
#14557=CARTESIAN_POINT('Ctrl Pts',(-20.4293570210763,24.4037013250535,-57.2567680036013));
#14558=CARTESIAN_POINT('Ctrl Pts',(-20.5176305714375,24.6778965084725,-57.2412827874244));
#14559=CARTESIAN_POINT('Ctrl Pts',(-20.6510900054019,24.9579177254986,-57.2232681434173));
#14560=CARTESIAN_POINT('Ctrl Pts',(-20.6613826500207,24.9789216404946,-57.2219034821732));
#14561=CARTESIAN_POINT('Ctrl Pts',(-20.6797923269155,25.0154772380762,-57.2195033325018));
#14562=CARTESIAN_POINT('Ctrl Pts',(-20.6878094617993,25.0310782752427,-57.218470908338));
#14563=CARTESIAN_POINT('Ctrl Pts',(-20.7030611302348,25.0601707482639,-57.2165298340016));
#14564=CARTESIAN_POINT('Ctrl Pts',(-20.7102652325311,25.0736776288064,-57.2156221770147));
#14565=CARTESIAN_POINT('Ctrl Pts',(-20.7208535227341,25.0931933462975,-57.2143010298495));
#14566=CARTESIAN_POINT('Ctrl Pts',(-20.7241612657107,25.0992435789692,-57.213890088024));
#14567=CARTESIAN_POINT('Ctrl Pts',(-20.7336164126128,25.1164070032649,-57.2127203952999));
#14568=CARTESIAN_POINT('Ctrl Pts',(-20.7398100789989,25.1274944501749,-57.211960088756));
#14569=CARTESIAN_POINT('Ctrl Pts',(-20.7522366136755,25.1494339144085,-57.2104460750095));
#14570=CARTESIAN_POINT('Ctrl Pts',(-20.7584674786793,25.1602868118865,-57.2096924469618));
#14571=CARTESIAN_POINT('Ctrl Pts',(-20.7760776391612,25.1905505204419,-57.2075775359374));
#14572=CARTESIAN_POINT('Ctrl Pts',(-20.7875970715632,25.2098785724109,-57.2062113094488));
#14573=CARTESIAN_POINT('Ctrl Pts',(-20.8027026205229,25.2346305383252,-57.2044409813238));
#14574=CARTESIAN_POINT('Ctrl Pts',(-20.8061042629456,25.2401667489687,-57.2040436684296));
#14575=CARTESIAN_POINT('Ctrl Pts',(-20.8115282184863,25.2489347364223,-57.2034122653995));
#14576=CARTESIAN_POINT('Ctrl Pts',(-20.8135395759915,25.25217329786,-57.2031785801177));
#14577=CARTESIAN_POINT('Ctrl Pts',(-20.8173119525095,25.258223362506,-57.2027411434019));
#14578=CARTESIAN_POINT('Ctrl Pts',(-20.8190715770952,25.2610357328517,-57.2025374438066));
#14579=CARTESIAN_POINT('Ctrl Pts',(-20.8230367193929,25.2673514261242,-57.2020791925076));
#14580=CARTESIAN_POINT('Ctrl Pts',(-20.8252446481651,25.2708532217346,-57.2018245515197));
#14581=CARTESIAN_POINT('Ctrl Pts',(-20.8317432178825,25.2811161298966,-57.2010766116614));
#14582=CARTESIAN_POINT('Ctrl Pts',(-20.8360522949027,25.2878654798529,-57.2005826270738));
#14583=CARTESIAN_POINT('Ctrl Pts',(-20.8685091142102,25.3382876023529,-57.1968763195368));
#14584=CARTESIAN_POINT('Ctrl Pts',(-20.8976827744067,25.381287852067,-57.1936256809604));
#14585=CARTESIAN_POINT('Ctrl Pts',(-20.9977911958089,25.521425600096,-57.1827204494532));
#14586=CARTESIAN_POINT('Ctrl Pts',(-21.0731160482794,25.6152879391684,-57.1748996790681));
#14587=CARTESIAN_POINT('Ctrl Pts',(-21.1776884934823,25.7316205482661,-57.1645260543051));
#14588=CARTESIAN_POINT('Ctrl Pts',(-21.2023261213394,25.7581175638018,-57.1621140032997));
#14589=CARTESIAN_POINT('Ctrl Pts',(-21.4160230430489,25.9803192866191,-57.1414740851199));
#14590=CARTESIAN_POINT('Ctrl Pts',(-21.6287181049323,26.1517656440395,-57.1226483325613));
#14591=CARTESIAN_POINT('Ctrl Pts',(-21.8892242215592,26.312180520093,-57.1030232876302));
#14592=CARTESIAN_POINT('Ctrl Pts',(-21.9182997922899,26.3294595665319,-57.1008778232789));
#14593=CARTESIAN_POINT('Ctrl Pts',(-21.9520452983774,26.3488016101807,-57.0984437246965));
#14594=CARTESIAN_POINT('Ctrl Pts',(-21.9564532118967,26.3513143008052,-57.0981268625543));
#14595=CARTESIAN_POINT('Ctrl Pts',(-21.9629574077639,26.3550016338165,-57.0976609276824));
#14596=CARTESIAN_POINT('Ctrl Pts',(-21.9650490716616,26.3561843424658,-57.09751133511));
#14597=CARTESIAN_POINT('Ctrl Pts',(-21.9687791354011,26.3582879644669,-57.0972450074932));
#14598=CARTESIAN_POINT('Ctrl Pts',(-21.9704170180351,26.3592097839042,-57.0971282135124));
#14599=CARTESIAN_POINT('Ctrl Pts',(-21.9738285945352,26.3611259310968,-57.0968852568727));
#14600=CARTESIAN_POINT('Ctrl Pts',(-21.9756024186937,26.3621200105771,-57.0967591104904));
#14601=CARTESIAN_POINT('Ctrl Pts',(-21.9802511101813,26.3647194334157,-57.09642897707));
#14602=CARTESIAN_POINT('Ctrl Pts',(-21.9831275084096,26.3663220560604,-57.0962251664038));
#14603=CARTESIAN_POINT('Ctrl Pts',(-21.9894300107646,26.3698209303043,-57.0957795917737));
#14604=CARTESIAN_POINT('Ctrl Pts',(-21.9928571309974,26.3717153548678,-57.0955379444333));
#14605=CARTESIAN_POINT('Ctrl Pts',(-22.0029332534682,26.3772612256234,-57.0948293362556));
#14606=CARTESIAN_POINT('Ctrl Pts',(-22.0095917608614,26.3808954791918,-57.0943634505653));
#14607=CARTESIAN_POINT('Ctrl Pts',(-22.032646838274,26.3933736298774,-57.0927583035312));
#14608=CARTESIAN_POINT('Ctrl Pts',(-22.0491075775814,26.4020990358464,-57.0916261722981));
#14609=CARTESIAN_POINT('Ctrl Pts',(-22.0687716968809,26.4123050330163,-57.0902890711953));
#14610=CARTESIAN_POINT('Ctrl Pts',(-22.0719025437825,26.413923479465,-57.0900766428938));
#14611=CARTESIAN_POINT('Ctrl Pts',(-22.0750360153845,26.415536774576,-57.0898644896988));
#14612=CARTESIAN_POINT('Origin',(-23.5502525316942,23.5502525316942,-77.3107734492734));
#14613=CARTESIAN_POINT('',(-22.0750357439087,26.4155366348044,-55.5940940905006));
#14614=CARTESIAN_POINT('',(-22.0750360153461,26.4155367745563,-55.8427674868566));
#14615=CARTESIAN_POINT('',(-22.0750360153461,26.4155367745563,-77.3107734492734));
#14616=CARTESIAN_POINT('',(-26.7730018744143,23.5523108070312,-56.4368032791696));
#14617=CARTESIAN_POINT('Ctrl Pts',(-22.0750357439015,26.4155366348007,-55.5940940905011));
#14618=CARTESIAN_POINT('Ctrl Pts',(-21.9838795594224,26.3686040693672,-55.600025320068));
#14619=CARTESIAN_POINT('Ctrl Pts',(-21.8948657812043,26.3172716490372,-55.6060829891755));
#14620=CARTESIAN_POINT('Ctrl Pts',(-21.7924440880926,26.2514713208581,-55.6134516178906));
#14621=CARTESIAN_POINT('Ctrl Pts',(-21.7766619380222,26.2411352593132,-55.6145986091763));
#14622=CARTESIAN_POINT('Ctrl Pts',(-21.7559279749849,26.2272945042548,-55.6161211799293));
#14623=CARTESIAN_POINT('Ctrl Pts',(-21.7508937870136,26.2239134011405,-55.6164920932773));
#14624=CARTESIAN_POINT('Ctrl Pts',(-21.7430987173382,26.2186460248088,-55.6170683558746));
#14625=CARTESIAN_POINT('Ctrl Pts',(-21.7403311590718,26.2167696172624,-55.6172733309547));
#14626=CARTESIAN_POINT('Ctrl Pts',(-21.7348548922085,26.2130442488274,-55.6176796765315));
#14627=CARTESIAN_POINT('Ctrl Pts',(-21.7321460754695,26.2111954532902,-55.6178810405864));
#14628=CARTESIAN_POINT('Ctrl Pts',(-21.7261388697134,26.2070820178816,-55.6183284126075));
#14629=CARTESIAN_POINT('Ctrl Pts',(-21.7228418704403,26.2048153667773,-55.6185744970169));
#14630=CARTESIAN_POINT('Ctrl Pts',(-21.7160026982318,26.2000947307717,-55.619086109891));
#14631=CARTESIAN_POINT('Ctrl Pts',(-21.7124612110051,26.1976397706299,-55.6193516753463));
#14632=CARTESIAN_POINT('Ctrl Pts',(-21.7033622813481,26.1913053333773,-55.620035631653));
#14633=CARTESIAN_POINT('Ctrl Pts',(-21.6978121547805,26.1874154290053,-55.6204544219746));
#14634=CARTESIAN_POINT('Ctrl Pts',(-21.6817334517017,26.1760705827888,-55.6216723180834));
#14635=CARTESIAN_POINT('Ctrl Pts',(-21.6712374087872,26.1685699589431,-55.6224731810303));
#14636=CARTESIAN_POINT('Ctrl Pts',(-21.5668551882934,26.0930260269633,-55.6304966927973));
#14637=CARTESIAN_POINT('Ctrl Pts',(-21.4766717069034,26.0200337264738,-55.6379128419842));
#14638=CARTESIAN_POINT('Ctrl Pts',(-21.1504964090363,25.7255567690064,-55.6666665889065));
#14639=CARTESIAN_POINT('Ctrl Pts',(-20.944420698649,25.4738878582367,-55.6892117691785));
#14640=CARTESIAN_POINT('Ctrl Pts',(-20.7751131358962,25.1887839529248,-55.7108085320634));
#14641=CARTESIAN_POINT('Ctrl Pts',(-20.7709814193324,25.1817659306554,-55.7113377934035));
#14642=CARTESIAN_POINT('Ctrl Pts',(-20.7414883524118,25.1312326430257,-55.7151314461384));
#14643=CARTESIAN_POINT('Ctrl Pts',(-20.7171218053369,25.0871407266879,-55.7183497322672));
#14644=CARTESIAN_POINT('Ctrl Pts',(-20.6914311426112,25.0379635051749,-55.7218244622239));
#14645=CARTESIAN_POINT('Ctrl Pts',(-20.6890757680994,25.0334285844984,-55.7221438281986));
#14646=CARTESIAN_POINT('Ctrl Pts',(-20.6855864519968,25.0266711847788,-55.7226181131022));
#14647=CARTESIAN_POINT('Ctrl Pts',(-20.684444303259,25.0244529879692,-55.7227735473916));
#14648=CARTESIAN_POINT('Ctrl Pts',(-20.6824896390722,25.0206459276338,-55.7230398764086));
#14649=CARTESIAN_POINT('Ctrl Pts',(-20.6816758676216,25.0190577160178,-55.7231508509402));
#14650=CARTESIAN_POINT('Ctrl Pts',(-20.680087794635,25.0159519712353,-55.723367603543));
#14651=CARTESIAN_POINT('Ctrl Pts',(-20.6793133791906,25.0144345038414,-55.7234733885449));
#14652=CARTESIAN_POINT('Ctrl Pts',(-20.6774386704505,25.0107538056879,-55.7237296853884));
#14653=CARTESIAN_POINT('Ctrl Pts',(-20.6763396141801,25.008589939611,-55.7238801183483));
#14654=CARTESIAN_POINT('Ctrl Pts',(-20.6729546872348,25.0019068724516,-55.7243439855108));
#14655=CARTESIAN_POINT('Ctrl Pts',(-20.6706770098204,24.9973834951613,-55.7246569029238));
#14656=CARTESIAN_POINT('Ctrl Pts',(-20.6450974636079,24.9462840135437,-55.7281802636299));
#14657=CARTESIAN_POINT('Ctrl Pts',(-20.6229155803774,24.8991517159277,-55.7313216004657));
#14658=CARTESIAN_POINT('Ctrl Pts',(-20.5785195256159,24.7985590176384,-55.7378425248174));
#14659=CARTESIAN_POINT('Ctrl Pts',(-20.5565834619849,24.7449961756656,-55.7412086701161));
#14660=CARTESIAN_POINT('Ctrl Pts',(-20.3990756803858,24.3287717520528,-55.7667686977408));
#14661=CARTESIAN_POINT('Ctrl Pts',(-20.3284139178172,23.9449678815775,-55.787339419887));
#14662=CARTESIAN_POINT('Ctrl Pts',(-20.3274626654681,23.5369074032937,-55.8120101374411));
#14663=CARTESIAN_POINT('Ctrl Pts',(-20.3276165349103,23.5160499769984,-55.8132773581588));
#14664=CARTESIAN_POINT('Ctrl Pts',(-20.3280806442961,23.4888872201346,-55.8149362135786));
#14665=CARTESIAN_POINT('Ctrl Pts',(-20.3282069617768,23.4825789187939,-55.8153220676715));
#14666=CARTESIAN_POINT('Ctrl Pts',(-20.3284296962321,23.4728788097124,-55.8159163214658));
#14667=CARTESIAN_POINT('Ctrl Pts',(-20.3285129465119,23.469486690595,-55.8161243075208));
#14668=CARTESIAN_POINT('Ctrl Pts',(-20.3286806367598,23.4630673287175,-55.8165182430365));
#14669=CARTESIAN_POINT('Ctrl Pts',(-20.3287639870076,23.4600400591522,-55.8167041580671));
#14670=CARTESIAN_POINT('Ctrl Pts',(-20.3289623512292,23.4531866341488,-55.8171253722893));
#14671=CARTESIAN_POINT('Ctrl Pts',(-20.3290799151622,23.4493605620969,-55.8173607513237));
#14672=CARTESIAN_POINT('Ctrl Pts',(-20.3294212755269,23.4388605506749,-55.8180073375857));
#14673=CARTESIAN_POINT('Ctrl Pts',(-20.3296589979729,23.4321871107737,-55.8184189817236));
#14674=CARTESIAN_POINT('Ctrl Pts',(-20.3302319373418,23.417395657934,-55.8193329402021));
#14675=CARTESIAN_POINT('Ctrl Pts',(-20.3305771158,23.4092780967719,-55.8198355655231));
#14676=CARTESIAN_POINT('Ctrl Pts',(-20.3317171308859,23.3846618472474,-55.8213629716101));
#14677=CARTESIAN_POINT('Ctrl Pts',(-20.3326081080357,23.3681680800315,-55.822390765675));
#14678=CARTESIAN_POINT('Ctrl Pts',(-20.3362702147324,23.3088458930996,-55.82610349676));
#14679=CARTESIAN_POINT('Ctrl Pts',(-20.3397699111697,23.2660685131726,-55.8288110991634));
#14680=CARTESIAN_POINT('Ctrl Pts',(-20.3543571818757,23.1229912646559,-55.8379724806893));
#14681=CARTESIAN_POINT('Ctrl Pts',(-20.3692996213143,23.0231524416621,-55.8445415419931));
#14682=CARTESIAN_POINT('Ctrl Pts',(-20.449093655949,22.6202281378749,-55.8717324764799));
#14683=CARTESIAN_POINT('Ctrl Pts',(-20.5528010600627,22.3265702393382,-55.8933218829525));
#14684=CARTESIAN_POINT('Ctrl Pts',(-20.714522577222,22.0185202148446,-55.9157053549482));
#14685=CARTESIAN_POINT('Ctrl Pts',(-20.7328242457011,21.9851115038259,-55.9181262676892));
#14686=CARTESIAN_POINT('Ctrl Pts',(-20.7543199458152,21.9474717819182,-55.9208394323022));
#14687=CARTESIAN_POINT('Ctrl Pts',(-20.7569361789822,21.9429165645628,-55.9211675412091));
#14688=CARTESIAN_POINT('Ctrl Pts',(-20.7607825226993,21.9362573113983,-55.9216468235589));
#14689=CARTESIAN_POINT('Ctrl Pts',(-20.7620038836986,21.934148271671,-55.9217985604257));
#14690=CARTESIAN_POINT('Ctrl Pts',(-20.7641737719267,21.9304111020053,-55.9220673328983));
#14691=CARTESIAN_POINT('Ctrl Pts',(-20.7651213350593,21.9287824177024,-55.9221844313966));
#14692=CARTESIAN_POINT('Ctrl Pts',(-20.76710660648,21.9253769810468,-55.9224292011152));
#14693=CARTESIAN_POINT('Ctrl Pts',(-20.768144585776,21.923600395113,-55.9225568539366));
#14694=CARTESIAN_POINT('Ctrl Pts',(-20.7708676266075,21.9189499201307,-55.9228908988748));
#14695=CARTESIAN_POINT('Ctrl Pts',(-20.7725554497548,21.9160776382567,-55.9230971104453));
#14696=CARTESIAN_POINT('Ctrl Pts',(-20.7799799241102,21.9034876472217,-55.9240005529012));
#14697=CARTESIAN_POINT('Ctrl Pts',(-20.7857632305311,21.8937973352767,-55.9246947692464));
#14698=CARTESIAN_POINT('Ctrl Pts',(-20.8285059523694,21.8230264574653,-55.9297578875546));
#14699=CARTESIAN_POINT('Ctrl Pts',(-20.8674382103166,21.7631533612404,-55.9340034961394));
#14700=CARTESIAN_POINT('Ctrl Pts',(-20.9357895673577,21.665312236726,-55.9409637089057));
#14701=CARTESIAN_POINT('Ctrl Pts',(-20.9641232964571,21.626622517405,-55.9437221583312));
#14702=CARTESIAN_POINT('Ctrl Pts',(-21.0149621293702,21.5603567145551,-55.9484840212353));
#14703=CARTESIAN_POINT('Ctrl Pts',(-21.0370795819349,21.5324952114008,-55.9504981341233));
#14704=CARTESIAN_POINT('Ctrl Pts',(-21.2452199372087,21.2790324626451,-55.9689876976082));
#14705=CARTESIAN_POINT('Ctrl Pts',(-21.4606560863423,21.0793829418304,-55.9849398400474));
#14706=CARTESIAN_POINT('Ctrl Pts',(-21.7054336156591,20.9077529964041,-56.002673309641));
#14707=CARTESIAN_POINT('Ctrl Pts',(-21.7108182228074,20.9040019673382,-56.0030631544036));
#14708=CARTESIAN_POINT('Ctrl Pts',(-21.7218658596289,20.8963559661733,-56.00386251072));
#14709=CARTESIAN_POINT('Ctrl Pts',(-21.7275299647967,20.8924626140867,-56.0042720768863));
#14710=CARTESIAN_POINT('Ctrl Pts',(-21.7702842403175,20.8632754376662,-56.007361751677));
#14711=CARTESIAN_POINT('Ctrl Pts',(-21.8078853683745,20.8387419966433,-56.0100686931956));
#14712=CARTESIAN_POINT('Ctrl Pts',(-21.8523192132048,20.8110563536344,-56.0132602154625));
#14713=CARTESIAN_POINT('Ctrl Pts',(-21.8586667766723,20.8071318839892,-56.0137159640924));
#14714=CARTESIAN_POINT('Ctrl Pts',(-21.8688138900393,20.800906903123,-56.0144442630828));
#14715=CARTESIAN_POINT('Ctrl Pts',(-21.8726046902539,20.7985921219068,-56.0147162878173));
#14716=CARTESIAN_POINT('Ctrl Pts',(-21.8793014143235,20.7945218750601,-56.0151967454117));
#14717=CARTESIAN_POINT('Ctrl Pts',(-21.8822053555841,20.7927631470027,-56.015405058119));
#14718=CARTESIAN_POINT('Ctrl Pts',(-21.8881504567554,20.7891754141683,-56.0158314659655));
#14719=CARTESIAN_POINT('Ctrl Pts',(-21.8911918686809,20.7873468379141,-56.0160495764252));
#14720=CARTESIAN_POINT('Ctrl Pts',(-21.8989165664418,20.7827199020024,-56.0166034631081));
#14721=CARTESIAN_POINT('Ctrl Pts',(-21.903603935679,20.7799284121731,-56.016939489811));
#14722=CARTESIAN_POINT('Ctrl Pts',(-21.9137592969406,20.7739154246187,-56.0176673561702));
#14723=CARTESIAN_POINT('Ctrl Pts',(-21.9192297538918,20.7706981543014,-56.0180593483607));
#14724=CARTESIAN_POINT('Ctrl Pts',(-21.9348854697905,20.7615528887393,-56.019180933954));
#14725=CARTESIAN_POINT('Ctrl Pts',(-21.9450937097022,20.7556646204742,-56.019911965692));
#14726=CARTESIAN_POINT('Ctrl Pts',(-21.9790265452408,20.7363389080943,-56.0223411272367));
#14727=CARTESIAN_POINT('Ctrl Pts',(-22.0028888593446,20.7231468433,-56.0240480354534));
#14728=CARTESIAN_POINT('Ctrl Pts',(-22.0990714558389,20.6715556792098,-56.0309243336377));
#14729=CARTESIAN_POINT('Ctrl Pts',(-22.1726709117516,20.6356189265752,-56.036178699719));
#14730=CARTESIAN_POINT('Ctrl Pts',(-22.513364249961,20.4850551859137,-56.0604706658564));
#14731=CARTESIAN_POINT('Ctrl Pts',(-22.7938364264267,20.4040856826114,-56.0805441675637));
#14732=CARTESIAN_POINT('Ctrl Pts',(-23.1171472288634,20.3565319184216,-56.1022340171842));
#14733=CARTESIAN_POINT('Ctrl Pts',(-23.1530981791113,20.3518622865729,-56.1046237584023));
#14734=CARTESIAN_POINT('Ctrl Pts',(-23.1954859148836,20.3470823470667,-56.1074099896367));
#14735=CARTESIAN_POINT('Ctrl Pts',(-23.2018525573201,20.3463836137882,-56.1078276503416));
#14736=CARTESIAN_POINT('Ctrl Pts',(-23.2124239645604,20.3452552952761,-56.1085197256729));
#14737=CARTESIAN_POINT('Ctrl Pts',(-23.2166275423312,20.3448149963424,-56.1087945466895));
#14738=CARTESIAN_POINT('Ctrl Pts',(-23.2737291353791,20.3389474970378,-56.1125225529528));
#14739=CARTESIAN_POINT('Ctrl Pts',(-23.3267566801838,20.3348216669469,-56.1159243645876));
#14740=CARTESIAN_POINT('Ctrl Pts',(-23.3856153410031,20.3317054513409,-56.1196160004429));
#14741=CARTESIAN_POINT('Ctrl Pts',(-23.3913657948243,20.33141645027,-56.1199757803214));
#14742=CARTESIAN_POINT('Ctrl Pts',(-23.3994171940089,20.3310334391093,-56.1204782440544));
#14743=CARTESIAN_POINT('Ctrl Pts',(-23.4017174684382,20.330926484177,-56.1206216515405));
#14744=CARTESIAN_POINT('Ctrl Pts',(-23.4059245561861,20.330735387624,-56.1208836677018));
#14745=CARTESIAN_POINT('Ctrl Pts',(-23.4078313321111,20.3306504743829,-56.1210023200823));
#14746=CARTESIAN_POINT('Ctrl Pts',(-23.41170234964,20.3304815344301,-56.1212429940806));
#14747=CARTESIAN_POINT('Ctrl Pts',(-23.4136665933762,20.3303976111623,-56.1213650097029));
#14748=CARTESIAN_POINT('Ctrl Pts',(-23.4185439561983,20.3301936946138,-56.121667718288));
#14749=CARTESIAN_POINT('Ctrl Pts',(-23.4214571710768,20.3300758566711,-56.1218482890927));
#14750=CARTESIAN_POINT('Ctrl Pts',(-23.432322275103,20.3296511369945,-56.1225208818048));
#14751=CARTESIAN_POINT('Ctrl Pts',(-23.4402752181687,20.3293697516721,-56.1230114769578));
#14752=CARTESIAN_POINT('Ctrl Pts',(-23.5747741654176,20.3251097535378,-56.1312804361758));
#14753=CARTESIAN_POINT('Ctrl Pts',(-23.7014630428073,20.3285617935038,-56.1386528939467));
#14754=CARTESIAN_POINT('Ctrl Pts',(-23.8612734438857,20.3423679452839,-56.1477877469958));
#14755=CARTESIAN_POINT('Ctrl Pts',(-23.8948643509231,20.3458024543773,-56.1496984027349));
#14756=CARTESIAN_POINT('Ctrl Pts',(-23.9558167961334,20.3530040884762,-56.1531574479588));
#14757=CARTESIAN_POINT('Ctrl Pts',(-23.9831954462334,20.3565962509917,-56.1547082548693));
#14758=CARTESIAN_POINT('Ctrl Pts',(-24.0338067452319,20.3638994090814,-56.1575745184197));
#14759=CARTESIAN_POINT('Ctrl Pts',(-24.0570513309089,20.3675137919785,-56.1588907251335));
#14760=CARTESIAN_POINT('Ctrl Pts',(-24.1004759911404,20.3747538324374,-56.161352190805));
#14761=CARTESIAN_POINT('Ctrl Pts',(-24.1206650262533,20.3783181956577,-56.1624976250833));
#14762=CARTESIAN_POINT('Ctrl Pts',(-24.1586403638953,20.3853970127006,-56.164656043476));
#14763=CARTESIAN_POINT('Ctrl Pts',(-24.1764336700842,20.3888693864078,-56.1656689766118));
#14764=CARTESIAN_POINT('Ctrl Pts',(-24.3635298895736,20.4270228528824,-56.1763439593797));
#14765=CARTESIAN_POINT('Ctrl Pts',(-24.529795748061,20.475114931625,-56.186057826214));
#14766=CARTESIAN_POINT('Ctrl Pts',(-24.7104125811944,20.5435001885044,-56.1973725537662));
#14767=CARTESIAN_POINT('Ctrl Pts',(-24.7293593767706,20.5508795945102,-56.1985689103523));
#14768=CARTESIAN_POINT('Ctrl Pts',(-24.752475383421,20.5601357040109,-56.2000407371455));
#14769=CARTESIAN_POINT('Ctrl Pts',(-24.756712347831,20.5618427304522,-56.2003110153679));
#14770=CARTESIAN_POINT('Ctrl Pts',(-24.7646792606191,20.5650722167106,-56.200820190399));
#14771=CARTESIAN_POINT('Ctrl Pts',(-24.7684100143864,20.5665926750673,-56.2010590250964));
#14772=CARTESIAN_POINT('Ctrl Pts',(-24.775983250039,20.5696956981808,-56.2015446629261));
#14773=CARTESIAN_POINT('Ctrl Pts',(-24.7798255406509,20.5712787071846,-56.2017914795223));
#14774=CARTESIAN_POINT('Ctrl Pts',(-24.7872193095958,20.5743416533091,-56.2022672634635));
#14775=CARTESIAN_POINT('Ctrl Pts',(-24.7907712222886,20.5758205281303,-56.2024961970525));
#14776=CARTESIAN_POINT('Ctrl Pts',(-24.800485075476,20.5798854153247,-56.203123312724));
#14777=CARTESIAN_POINT('Ctrl Pts',(-24.8066416112257,20.5824842288445,-56.203521900151));
#14778=CARTESIAN_POINT('Ctrl Pts',(-24.8141718909226,20.585690562069,-56.2040108288818));
#14779=CARTESIAN_POINT('Ctrl Pts',(-24.8155533826047,20.5862799314405,-56.2041005847826));
#14780=CARTESIAN_POINT('Ctrl Pts',(-24.8232473027992,20.5895686565504,-56.2046007845587));
#14781=CARTESIAN_POINT('Ctrl Pts',(-24.8295514705077,20.5922871972335,-56.2050118474501));
#14782=CARTESIAN_POINT('Ctrl Pts',(-24.8413831799372,20.597434274004,-56.2057856477019));
#14783=CARTESIAN_POINT('Ctrl Pts',(-24.8469126849512,20.5998582427907,-56.2061482340082));
#14784=CARTESIAN_POINT('Ctrl Pts',(-24.8755169572995,20.6124934402352,-56.208028900367));
#14785=CARTESIAN_POINT('Ctrl Pts',(-24.8984775337773,20.6229596585026,-56.2095553934008));
#14786=CARTESIAN_POINT('Ctrl Pts',(-24.9298089692704,20.6376884132013,-56.2116626079141));
#14787=CARTESIAN_POINT('Ctrl Pts',(-24.9382880204995,20.6417197077988,-56.2122353256777));
#14788=CARTESIAN_POINT('Ctrl Pts',(-24.9508365127292,20.6477531532043,-56.2130866048625));
#14789=CARTESIAN_POINT('Ctrl Pts',(-24.9549195906399,20.6497269615196,-56.2133641793519));
#14790=CARTESIAN_POINT('Ctrl Pts',(-24.9618955348806,20.653117400299,-56.2138394173272));
#14791=CARTESIAN_POINT('Ctrl Pts',(-24.9647904770672,20.6545297654411,-56.214036931732));
#14792=CARTESIAN_POINT('Ctrl Pts',(-24.9705918922675,20.6573708970113,-56.2144333429391));
#14793=CARTESIAN_POINT('Ctrl Pts',(-24.9734983380794,20.6587997089826,-56.2146322411362));
#14794=CARTESIAN_POINT('Ctrl Pts',(-24.980202942142,20.6621082580098,-56.2150917571967));
#14795=CARTESIAN_POINT('Ctrl Pts',(-24.983999549966,20.6639911074156,-56.2153524839062));
#14796=CARTESIAN_POINT('Ctrl Pts',(-24.9954560256224,20.6697008930686,-56.2161408117007));
#14797=CARTESIAN_POINT('Ctrl Pts',(-25.0031043201174,20.6735508509047,-56.2166692207665));
#14798=CARTESIAN_POINT('Ctrl Pts',(-25.0205615029873,20.6824257316408,-56.2178802206822));
#14799=CARTESIAN_POINT('Ctrl Pts',(-25.0303600993239,20.6874705613804,-56.2185635102775));
#14800=CARTESIAN_POINT('Ctrl Pts',(-25.062228180893,20.7040852629906,-56.2207975411282));
#14801=CARTESIAN_POINT('Ctrl Pts',(-25.0841889643059,20.715860630489,-56.2223555405025));
#14802=CARTESIAN_POINT('Ctrl Pts',(-25.171033682565,20.763731633463,-56.2285919426978));
#14803=CARTESIAN_POINT('Ctrl Pts',(-25.2347941438381,20.801807812917,-56.233340290231));
#14804=CARTESIAN_POINT('Ctrl Pts',(-25.3499260299225,20.876073636675,-56.2422361196812));
#14805=CARTESIAN_POINT('Ctrl Pts',(-25.4016650259413,20.9116300693082,-56.2463610268011));
#14806=CARTESIAN_POINT('Ctrl Pts',(-25.6682400166094,21.1065295093652,-56.2682720182018));
#14807=CARTESIAN_POINT('Ctrl Pts',(-25.863640934846,21.2906342932802,-56.2867639652581));
#14808=CARTESIAN_POINT('Ctrl Pts',(-26.0492881014276,21.5151823277497,-56.3058709451657));
#14809=CARTESIAN_POINT('Ctrl Pts',(-26.0643215804226,21.5337837385994,-56.3074302805929));
#14810=CARTESIAN_POINT('Ctrl Pts',(-26.0800290861947,21.5536679049431,-56.3090710349475));
#14811=CARTESIAN_POINT('Ctrl Pts',(-26.0809104407822,21.5547851341495,-56.3091631373156));
#14812=CARTESIAN_POINT('Ctrl Pts',(-26.0864923579264,21.561870571133,-56.3097466981448));
#14813=CARTESIAN_POINT('Ctrl Pts',(-26.0911725884148,21.5678548559452,-56.3102370963472));
#14814=CARTESIAN_POINT('Ctrl Pts',(-26.1200968594941,21.6051090243471,-56.3132744071318));
#14815=CARTESIAN_POINT('Ctrl Pts',(-26.1437858388642,21.6368083925734,-56.3157909711665));
#14816=CARTESIAN_POINT('Ctrl Pts',(-26.1699860921746,21.6732491136832,-56.3186005135982));
#14817=CARTESIAN_POINT('Ctrl Pts',(-26.1730752568516,21.6775681716135,-56.3189322013199));
#14818=CARTESIAN_POINT('Ctrl Pts',(-26.1775729317662,21.6838894720756,-56.3194157233918));
#14819=CARTESIAN_POINT('Ctrl Pts',(-26.1789898374854,21.6858856868429,-56.3195681353772));
#14820=CARTESIAN_POINT('Ctrl Pts',(-26.1814942972349,21.6894226387778,-56.3198376846851));
#14821=CARTESIAN_POINT('Ctrl Pts',(-26.1825827739808,21.6909627170837,-56.3199548861439));
#14822=CARTESIAN_POINT('Ctrl Pts',(-26.1848530176393,21.6941808589483,-56.3201994400194));
#14823=CARTESIAN_POINT('Ctrl Pts',(-26.1860345310423,21.6958590926201,-56.3203267747702));
#14824=CARTESIAN_POINT('Ctrl Pts',(-26.1891163975487,21.7002455031944,-56.3206590768362));
#14825=CARTESIAN_POINT('Ctrl Pts',(-26.1910141912397,21.7029554885201,-56.3208638670555));
#14826=CARTESIAN_POINT('Ctrl Pts',(-26.1992455709247,21.7147482274573,-56.3217528351257));
#14827=CARTESIAN_POINT('Ctrl Pts',(-26.2055365945244,21.7238608084104,-56.3224341166714));
#14828=CARTESIAN_POINT('Ctrl Pts',(-26.250803818078,21.7901588981375,-56.3273513514363));
#14829=CARTESIAN_POINT('Ctrl Pts',(-26.2879793122929,21.8485590945873,-56.331471410409));
#14830=CARTESIAN_POINT('Ctrl Pts',(-26.487626650329,22.1856937876466,-56.354352350173));
#14831=CARTESIAN_POINT('Ctrl Pts',(-26.6094079433382,22.4863923652025,-56.3715432198012));
#14832=CARTESIAN_POINT('Ctrl Pts',(-26.6888556032308,22.818379680284,-56.3913169957944));
#14833=CARTESIAN_POINT('Ctrl Pts',(-26.6930485549052,22.8365997800023,-56.3924039265359));
#14834=CARTESIAN_POINT('Ctrl Pts',(-26.7170541354781,22.9452304444625,-56.3988971574075));
#14835=CARTESIAN_POINT('Ctrl Pts',(-26.7331213899719,23.0364165285247,-56.4044021051064));
#14836=CARTESIAN_POINT('Ctrl Pts',(-26.7465800634763,23.1382910401125,-56.4106575834641));
#14837=CARTESIAN_POINT('Ctrl Pts',(-26.7478700879922,23.1484267972651,-56.4112810829464));
#14838=CARTESIAN_POINT('Ctrl Pts',(-26.7496120859228,23.1626535843466,-56.4121578731054));
#14839=CARTESIAN_POINT('Ctrl Pts',(-26.7501044649097,23.166739681244,-56.4124098858988));
#14840=CARTESIAN_POINT('Ctrl Pts',(-26.7509922159806,23.1742275797011,-56.4128720567723));
#14841=CARTESIAN_POINT('Ctrl Pts',(-26.7513899959649,23.1776290947063,-56.4130821384751));
#14842=CARTESIAN_POINT('Ctrl Pts',(-26.7521429070811,23.1841576112422,-56.4134856035549));
#14843=CARTESIAN_POINT('Ctrl Pts',(-26.7524988813425,23.187284512679,-56.4136789600031));
#14844=CARTESIAN_POINT('Ctrl Pts',(-26.7532330695095,23.1938188206494,-56.4140832556221));
#14845=CARTESIAN_POINT('Ctrl Pts',(-26.7536104274125,23.1972263176715,-56.4142942215946));
#14846=CARTESIAN_POINT('Ctrl Pts',(-26.7544863012855,23.205252398087,-56.4147914548199));
#14847=CARTESIAN_POINT('Ctrl Pts',(-26.754980268767,23.2098714610526,-56.4150778654233));
#14848=CARTESIAN_POINT('Ctrl Pts',(-26.7562537509156,23.2220282636645,-56.4158323268058));
#14849=CARTESIAN_POINT('Ctrl Pts',(-26.7570166658164,23.2295676796906,-56.4163009008134));
#14850=CARTESIAN_POINT('Ctrl Pts',(-26.7679812253469,23.3418768948182,-56.4232910779254));
#14851=CARTESIAN_POINT('Ctrl Pts',(-26.7730690891451,23.4470691876655,-56.429973293957));
#14852=CARTESIAN_POINT('Ctrl Pts',(-26.7730018744143,23.5523108070312,-56.4368032791696));
#14853=CARTESIAN_POINT('Ctrl Pts',(-26.7730018769529,23.5523068283337,-56.4368030209596));
#14854=CARTESIAN_POINT('Ctrl Pts',(-26.772795047506,23.8767777209974,-56.4578605669829));
#14855=CARTESIAN_POINT('Ctrl Pts',(-26.7235944638763,24.1993030980816,-56.4804034481421));
#14856=CARTESIAN_POINT('Ctrl Pts',(-26.6057090741017,24.5776094452741,-56.5064782171832));
#14857=CARTESIAN_POINT('Ctrl Pts',(-26.5820511284921,24.6454584567933,-56.5111274809225));
#14858=CARTESIAN_POINT('Ctrl Pts',(-26.5520584605614,24.7230300120075,-56.5163666614606));
#14859=CARTESIAN_POINT('Ctrl Pts',(-26.5479180592104,24.7335729646986,-56.5170770654102));
#14860=CARTESIAN_POINT('Ctrl Pts',(-26.5424863008555,24.7471926980964,-56.5179924215039));
#14861=CARTESIAN_POINT('Ctrl Pts',(-26.541245697338,24.7502894371971,-56.5182003884329));
#14862=CARTESIAN_POINT('Ctrl Pts',(-26.5392317585472,24.7552940171778,-56.5185362159691));
#14863=CARTESIAN_POINT('Ctrl Pts',(-26.5384614038799,24.7572030429178,-56.518664257155));
#14864=CARTESIAN_POINT('Ctrl Pts',(-26.5369825391173,24.7608577417391,-56.5189092623037));
#14865=CARTESIAN_POINT('Ctrl Pts',(-26.5362743296622,24.7626035262101,-56.5190262437593));
#14866=CARTESIAN_POINT('Ctrl Pts',(-26.5346472300783,24.7666043625157,-56.5192942114077));
#14867=CARTESIAN_POINT('Ctrl Pts',(-26.5337273126147,24.7688589996696,-56.5194451347702));
#14868=CARTESIAN_POINT('Ctrl Pts',(-26.5308190106975,24.7759639601857,-56.5199204648755));
#14869=CARTESIAN_POINT('Ctrl Pts',(-26.5288213340867,24.7808105075839,-56.5202443082064));
#14870=CARTESIAN_POINT('Ctrl Pts',(-26.5123166558212,24.8205767101645,-56.5228983735687));
#14871=CARTESIAN_POINT('Ctrl Pts',(-26.4972071675566,24.8552452802931,-56.5251926344906));
#14872=CARTESIAN_POINT('Ctrl Pts',(-26.4775114027901,24.8983492329477,-56.5280301510296));
#14873=CARTESIAN_POINT('Ctrl Pts',(-26.473493788296,24.9070390935149,-56.5286014292358));
#14874=CARTESIAN_POINT('Ctrl Pts',(-26.4680298672539,24.9187202951576,-56.5293684876796));
#14875=CARTESIAN_POINT('Ctrl Pts',(-26.4666176125471,24.9217274001838,-56.5295658742123));
#14876=CARTESIAN_POINT('Ctrl Pts',(-26.4635963139718,24.9281348634207,-56.5299863047395));
#14877=CARTESIAN_POINT('Ctrl Pts',(-26.4619859597716,24.9315346020478,-56.5302092874632));
#14878=CARTESIAN_POINT('Ctrl Pts',(-26.4591067339186,24.937585740589,-56.5306060172105));
#14879=CARTESIAN_POINT('Ctrl Pts',(-26.4578401834328,24.9402382330135,-56.5307798694545));
#14880=CARTESIAN_POINT('Ctrl Pts',(-26.4000813575423,25.0607761399479,-56.5386780507431));
#14881=CARTESIAN_POINT('Ctrl Pts',(-26.3364669725927,25.1751282683427,-56.5460768510529));
#14882=CARTESIAN_POINT('Ctrl Pts',(-26.1746881567577,25.4283551308489,-56.5629297729614));
#14883=CARTESIAN_POINT('Ctrl Pts',(-26.0721442528753,25.5639536696237,-56.5723214032149));
#14884=CARTESIAN_POINT('Ctrl Pts',(-25.9246523887287,25.7299496403482,-56.5849957302839));
#14885=CARTESIAN_POINT('Ctrl Pts',(-25.8889598993441,25.7682024119219,-56.5880063334643));
#14886=CARTESIAN_POINT('Ctrl Pts',(-25.8040926966018,25.8548301235245,-56.5950622472781));
#14887=CARTESIAN_POINT('Ctrl Pts',(-25.7542661640202,25.9025272343392,-56.5991301921456));
#14888=CARTESIAN_POINT('Ctrl Pts',(-25.6854390088445,25.9643051368157,-56.6046777260879));
#14889=CARTESIAN_POINT('Ctrl Pts',(-25.6677562108489,25.9798305602173,-56.6060968758131));
#14890=CARTESIAN_POINT('Ctrl Pts',(-25.6379599553161,26.0054191665922,-56.6084790618197));
#14891=CARTESIAN_POINT('Ctrl Pts',(-25.625939727593,26.0155898600919,-56.6094376379942));
#14892=CARTESIAN_POINT('Ctrl Pts',(-25.609673564302,26.0291498823676,-56.6107317605479));
#14893=CARTESIAN_POINT('Ctrl Pts',(-25.6054927483823,26.0326172744062,-56.6110641140929));
#14894=CARTESIAN_POINT('Ctrl Pts',(-25.5988833969117,26.0380706485203,-56.6115891093478));
#14895=CARTESIAN_POINT('Ctrl Pts',(-25.5964606796866,26.0400636930695,-56.6117814636095));
#14896=CARTESIAN_POINT('Ctrl Pts',(-25.591434921176,26.0441858355895,-56.6121803102211));
#14897=CARTESIAN_POINT('Ctrl Pts',(-25.5888314508093,26.046314402284,-56.6123868237642));
#14898=CARTESIAN_POINT('Ctrl Pts',(-25.5828985186458,26.0511496238528,-56.6128572156703));
#14899=CARTESIAN_POINT('Ctrl Pts',(-25.5795669784092,26.0538537079815,-56.6131211974846));
#14900=CARTESIAN_POINT('Ctrl Pts',(-25.5694281123333,26.0620495051353,-56.6139240974565));
#14901=CARTESIAN_POINT('Ctrl Pts',(-25.5626038632753,26.0675201331029,-56.6144638633773));
#14902=CARTESIAN_POINT('Ctrl Pts',(-25.5141004807907,26.1060793652963,-56.6182958067153));
#14903=CARTESIAN_POINT('Ctrl Pts',(-25.4716317730295,26.1381572506343,-56.6216280413161));
#14904=CARTESIAN_POINT('Ctrl Pts',(-25.4157979157781,26.1781981367017,-56.6259834511265));
#14905=CARTESIAN_POINT('Ctrl Pts',(-25.403140700652,26.187137645424,-56.6269691361736));
#14906=CARTESIAN_POINT('Ctrl Pts',(-25.3795328679331,26.2035574278932,-56.6288045874966));
#14907=CARTESIAN_POINT('Ctrl Pts',(-25.3685995515184,26.2110620942255,-56.629653441161));
#14908=CARTESIAN_POINT('Ctrl Pts',(-25.2371402059393,26.3001076136953,-56.6398457836409));
#14909=CARTESIAN_POINT('Ctrl Pts',(-25.1112853344877,26.3734529507193,-56.6494745816595));
#14910=CARTESIAN_POINT('Ctrl Pts',(-24.8875655462556,26.4842882380786,-56.6662597418593));
#14911=CARTESIAN_POINT('Ctrl Pts',(-24.792024652263,26.5259831846188,-56.6733292779252));
#14912=CARTESIAN_POINT('Ctrl Pts',(-24.5321834423552,26.6246837582465,-56.6921168627927));
#14913=CARTESIAN_POINT('Ctrl Pts',(-24.3649844631124,26.6731588156584,-56.7037648267124));
#14914=CARTESIAN_POINT('Ctrl Pts',(-24.1842849929204,26.710036194667,-56.7153746934155));
#14915=CARTESIAN_POINT('Ctrl Pts',(-24.1738868259481,26.7121048737872,-56.7160393513066));
#14916=CARTESIAN_POINT('Ctrl Pts',(-24.1602823429093,26.7147417149428,-56.7169043232264));
#14917=CARTESIAN_POINT('Ctrl Pts',(-24.1570852639833,26.7153563525372,-56.7171072591245));
#14918=CARTESIAN_POINT('Ctrl Pts',(-24.1518827444599,26.7163483631067,-56.7174369416389));
#14919=CARTESIAN_POINT('Ctrl Pts',(-24.1498778773046,26.7167286758579,-56.7175638569513));
#14920=CARTESIAN_POINT('Ctrl Pts',(-24.1460154594649,26.717457556374,-56.717808104599));
#14921=CARTESIAN_POINT('Ctrl Pts',(-24.1441579683827,26.7178063933908,-56.7179254519354));
#14922=CARTESIAN_POINT('Ctrl Pts',(-24.1398684058894,26.7186080678363,-56.7181961826111));
#14923=CARTESIAN_POINT('Ctrl Pts',(-24.1374361126518,26.7190597402282,-56.7183494987472));
#14924=CARTESIAN_POINT('Ctrl Pts',(-24.1296452435192,26.7204972121558,-56.7188399671293));
#14925=CARTESIAN_POINT('Ctrl Pts',(-24.1242846501612,26.7214722302502,-56.7191765035259));
#14926=CARTESIAN_POINT('Ctrl Pts',(-24.1056875644726,26.7248060836125,-56.7203408601092));
#14927=CARTESIAN_POINT('Ctrl Pts',(-24.0924385795353,26.7270957185495,-56.721164822986));
#14928=CARTESIAN_POINT('Ctrl Pts',(-23.7745517768539,26.7799849781797,-56.7408098903674));
#14929=CARTESIAN_POINT('Ctrl Pts',(-23.4641677781114,26.7866309711626,-56.7573672548889));
#14930=CARTESIAN_POINT('Ctrl Pts',(-23.0335314588877,26.7337610575943,-56.7818815932684));
#14931=CARTESIAN_POINT('Ctrl Pts',(-22.910525132612,26.7113396304774,-56.7890479320346));
#14932=CARTESIAN_POINT('Ctrl Pts',(-22.7466022986518,26.6714990820688,-56.79901929072));
#14933=CARTESIAN_POINT('Ctrl Pts',(-22.7042832530441,26.6602958482481,-56.8016317207004));
#14934=CARTESIAN_POINT('Ctrl Pts',(-22.6460937033803,26.6436156444302,-56.8052827378224));
#14935=CARTESIAN_POINT('Ctrl Pts',(-22.6300169632677,26.638871157604,-56.806297716353));
#14936=CARTESIAN_POINT('Ctrl Pts',(-22.6061190029991,26.6316153638276,-56.8078161192128));
#14937=CARTESIAN_POINT('Ctrl Pts',(-22.5982690172419,26.629199171296,-56.8083164406409));
#14938=CARTESIAN_POINT('Ctrl Pts',(-22.5840044327246,26.6247488250726,-56.8092284725018));
#14939=CARTESIAN_POINT('Ctrl Pts',(-22.5775867872259,26.622724532415,-56.8096398578396));
#14940=CARTESIAN_POINT('Ctrl Pts',(-22.5675134356821,26.6195124109695,-56.8102872681809));
#14941=CARTESIAN_POINT('Ctrl Pts',(-22.5638534090246,26.6183381087199,-56.8105228471339));
#14942=CARTESIAN_POINT('Ctrl Pts',(-22.5573228075707,26.6162299024264,-56.8109438210773));
#14943=CARTESIAN_POINT('Ctrl Pts',(-22.5544514227968,26.6152985062776,-56.8111291330943));
#14944=CARTESIAN_POINT('Ctrl Pts',(-22.5483688409357,26.6133160389131,-56.811522150884));
#14945=CARTESIAN_POINT('Ctrl Pts',(-22.5451579816624,26.6122639497693,-56.8117298901142));
#14946=CARTESIAN_POINT('Ctrl Pts',(-22.5360234233541,26.60925495047,-56.8123216698612));
#14947=CARTESIAN_POINT('Ctrl Pts',(-22.5301037678797,26.6072858944648,-56.812706111839));
#14948=CARTESIAN_POINT('Ctrl Pts',(-22.504980513387,26.5988480434532,-56.8143417209079));
#14949=CARTESIAN_POINT('Ctrl Pts',(-22.4858327670516,26.5922155033631,-56.8155983068113));
#14950=CARTESIAN_POINT('Ctrl Pts',(-22.45433637735,26.5809717629063,-56.817682184682));
#14951=CARTESIAN_POINT('Ctrl Pts',(-22.4419510186172,26.576464524197,-56.8185059764965));
#14952=CARTESIAN_POINT('Ctrl Pts',(-22.3082743265248,26.5268866462522,-56.8274448655465));
#14953=CARTESIAN_POINT('Ctrl Pts',(-22.1898796467717,26.4746650288207,-56.8357943590103));
#14954=CARTESIAN_POINT('Ctrl Pts',(-22.075035785626,26.4155366562829,-56.8443273945297));
#14955=CARTESIAN_POINT('',(-26.7730021430534,23.5518352458033,-56.6857734492205));
#14956=CARTESIAN_POINT('Ctrl Pts',(-22.0750360153845,26.415536774576,-57.0898644896988));
#14957=CARTESIAN_POINT('Ctrl Pts',(-22.1289579959314,26.4432989753045,-57.0862136761903));
#14958=CARTESIAN_POINT('Ctrl Pts',(-22.1836572224708,26.4695357137267,-57.082644257473));
#14959=CARTESIAN_POINT('Ctrl Pts',(-22.375909911966,26.5551613509025,-57.070447504258));
#14960=CARTESIAN_POINT('Ctrl Pts',(-22.5168434716501,26.6064968463387,-57.0621052936065));
#14961=CARTESIAN_POINT('Ctrl Pts',(-22.6781839966533,26.6528223466479,-57.0527257178279));
#14962=CARTESIAN_POINT('Ctrl Pts',(-22.6955643991644,26.6576551739239,-57.0517175734479));
#14963=CARTESIAN_POINT('Ctrl Pts',(-22.9490516746451,26.7258527058213,-57.0370375909288));
#14964=CARTESIAN_POINT('Ctrl Pts',(-23.1915375512655,26.7622888737644,-57.023206805814));
#14965=CARTESIAN_POINT('Ctrl Pts',(-23.4509605163593,26.7715083405287,-57.007458848676));
#14966=CARTESIAN_POINT('Ctrl Pts',(-23.4661309054112,26.7719401996617,-57.0065348529423));
#14967=CARTESIAN_POINT('Ctrl Pts',(-23.4868514514494,26.7723836057674,-57.0052684056177));
#14968=CARTESIAN_POINT('Ctrl Pts',(-23.492399593684,26.7724879967772,-57.0049288702612));
#14969=CARTESIAN_POINT('Ctrl Pts',(-23.5011881777624,26.7726306525099,-57.0043903346315));
#14970=CARTESIAN_POINT('Ctrl Pts',(-23.5044284730085,26.7726783601439,-57.0041916310542));
#14971=CARTESIAN_POINT('Ctrl Pts',(-23.5107014929228,26.7727612557337,-57.0038066622907));
#14972=CARTESIAN_POINT('Ctrl Pts',(-23.5137342074567,26.7727970500951,-57.0036204163386));
#14973=CARTESIAN_POINT('Ctrl Pts',(-23.5209393935235,26.772871918701,-57.0031776151157));
#14974=CARTESIAN_POINT('Ctrl Pts',(-23.5251118916147,26.7729071705807,-57.0029209401264));
#14975=CARTESIAN_POINT('Ctrl Pts',(-23.5374499685165,26.7729874472131,-57.0021612054212));
#14976=CARTESIAN_POINT('Ctrl Pts',(-23.5456156176842,26.7730095405904,-57.0016574266666));
#14977=CARTESIAN_POINT('Ctrl Pts',(-23.6100709692127,26.77293896674,-56.9976731049053));
#14978=CARTESIAN_POINT('Ctrl Pts',(-23.6663463484709,26.7714025875692,-56.9941474718841));
#14979=CARTESIAN_POINT('Ctrl Pts',(-23.8592825073757,26.7610728992429,-56.9818878262387));
#14980=CARTESIAN_POINT('Ctrl Pts',(-23.9953925163203,26.7450465956179,-56.9729339225174));
#14981=CARTESIAN_POINT('Ctrl Pts',(-24.1598872407253,26.7149614735939,-56.961778659204));
#14982=CARTESIAN_POINT('Ctrl Pts',(-24.1896384210411,26.7090850364896,-56.959747942694));
#14983=CARTESIAN_POINT('Ctrl Pts',(-24.2438547444788,26.697578941967,-56.9560252501412));
#14984=CARTESIAN_POINT('Ctrl Pts',(-24.26834575361,26.6920815632156,-56.9543353158208));
#14985=CARTESIAN_POINT('Ctrl Pts',(-24.3135640204857,26.681375297181,-56.9512011576024));
#14986=CARTESIAN_POINT('Ctrl Pts',(-24.3343086289694,26.6762452105117,-56.9497578190563));
#14987=CARTESIAN_POINT('Ctrl Pts',(-24.3729449782424,26.6662817543009,-56.9470603457249));
#14988=CARTESIAN_POINT('Ctrl Pts',(-24.3908490950885,26.6614996115543,-56.9458065844401));
#14989=CARTESIAN_POINT('Ctrl Pts',(-24.4244145439227,26.6522234820446,-56.9434497737337));
#14990=CARTESIAN_POINT('Ctrl Pts',(-24.440085022567,26.6477646201572,-56.9423468507494));
#14991=CARTESIAN_POINT('Ctrl Pts',(-24.5985362416258,26.6013774174911,-56.9311710076547));
#14992=CARTESIAN_POINT('Ctrl Pts',(-24.7382946168261,26.5497231748332,-56.9211084962021));
#14993=CARTESIAN_POINT('Ctrl Pts',(-24.8775252008891,26.48699900546,-56.9111586061001));
#14994=CARTESIAN_POINT('Ctrl Pts',(-24.8810567143021,26.4854003673905,-56.910906289081));
#14995=CARTESIAN_POINT('Ctrl Pts',(-24.8873795145018,26.4825244183001,-56.9104546548881));
#14996=CARTESIAN_POINT('Ctrl Pts',(-24.8901718715129,26.4812494863237,-56.910255237799));
#14997=CARTESIAN_POINT('Ctrl Pts',(-24.9404129271874,26.4582236656859,-56.9066680204525));
#14998=CARTESIAN_POINT('Ctrl Pts',(-24.9873316206943,26.4353255841775,-56.9033302150377));
#14999=CARTESIAN_POINT('Ctrl Pts',(-25.0387633769651,26.4086587061559,-56.8997017760999));
#15000=CARTESIAN_POINT('Ctrl Pts',(-25.043843217337,26.406007643684,-56.89934373574));
#15001=CARTESIAN_POINT('Ctrl Pts',(-25.0509506644732,26.4022742635281,-56.8988432836884));
#15002=CARTESIAN_POINT('Ctrl Pts',(-25.052984186301,26.4012033237815,-56.8987001560507));
#15003=CARTESIAN_POINT('Ctrl Pts',(-25.0567034270141,26.399239527328,-56.8984384881392));
#15004=CARTESIAN_POINT('Ctrl Pts',(-25.0583895010731,26.3983473480498,-56.8983199045851));
#15005=CARTESIAN_POINT('Ctrl Pts',(-25.0616212318466,26.3966336162769,-56.8980926923638));
#15006=CARTESIAN_POINT('Ctrl Pts',(-25.0631670106381,26.3958123019165,-56.8979840485186));
#15007=CARTESIAN_POINT('Ctrl Pts',(-25.0670947121816,26.3937213019853,-56.897708079418));
#15008=CARTESIAN_POINT('Ctrl Pts',(-25.0694757163648,26.392449879419,-56.8975408655051));
#15009=CARTESIAN_POINT('Ctrl Pts',(-25.0776803584006,26.3880554607897,-56.8969649362471));
#15010=CARTESIAN_POINT('Ctrl Pts',(-25.0834960369084,26.3849175182007,-56.8965571693341));
#15011=CARTESIAN_POINT('Ctrl Pts',(-25.0974369219202,26.3773400350551,-56.8955807279213));
#15012=CARTESIAN_POINT('Ctrl Pts',(-25.1055527821407,26.372883294793,-56.8950131199395));
#15013=CARTESIAN_POINT('Ctrl Pts',(-25.1350045167815,26.3565445868654,-56.8929559663072));
#15014=CARTESIAN_POINT('Ctrl Pts',(-25.156224968094,26.3444548448586,-56.891478824034));
#15015=CARTESIAN_POINT('Ctrl Pts',(-25.2500011312582,26.2896072869363,-56.8849645049247));
#15016=CARTESIAN_POINT('Ctrl Pts',(-25.3210072523645,26.2442532394234,-56.8800676114763));
#15017=CARTESIAN_POINT('Ctrl Pts',(-25.6303302846351,26.0291570664636,-56.8585238616396));
#15018=CARTESIAN_POINT('Ctrl Pts',(-25.8466414938083,25.8302310995459,-56.8427402297917));
#15019=CARTESIAN_POINT('Ctrl Pts',(-26.0956276621019,25.5293398477505,-56.8199987555657));
#15020=CARTESIAN_POINT('Ctrl Pts',(-26.1546221337973,25.4510358381957,-56.8141791980845));
#15021=CARTESIAN_POINT('Ctrl Pts',(-26.2152228800089,25.3624715188693,-56.8076472194698));
#15022=CARTESIAN_POINT('Ctrl Pts',(-26.2204582214526,25.354748634871,-56.8070780485343));
#15023=CARTESIAN_POINT('Ctrl Pts',(-26.2281804279205,25.343250073243,-56.8062311960031));
#15024=CARTESIAN_POINT('Ctrl Pts',(-26.2306930355567,25.339491673425,-56.8059544872497));
#15025=CARTESIAN_POINT('Ctrl Pts',(-26.2349802143327,25.3330495431564,-56.8054803432014));
#15026=CARTESIAN_POINT('Ctrl Pts',(-26.236758695394,25.3303684117129,-56.8052830554586));
#15027=CARTESIAN_POINT('Ctrl Pts',(-26.2402103890779,25.3251478909072,-56.804898995016));
#15028=CARTESIAN_POINT('Ctrl Pts',(-26.2418840283983,25.3226087872225,-56.8047122386739));
#15029=CARTESIAN_POINT('Ctrl Pts',(-26.2458777120233,25.316531205388,-56.804265311129));
#15030=CARTESIAN_POINT('Ctrl Pts',(-26.2481943819237,25.3129905265407,-56.804005013751));
#15031=CARTESIAN_POINT('Ctrl Pts',(-26.2551170602395,25.3023646457585,-56.803224052916));
#15032=CARTESIAN_POINT('Ctrl Pts',(-26.2597021529684,25.2952659200754,-56.8027026084648));
#15033=CARTESIAN_POINT('Ctrl Pts',(-26.2995268850307,25.2330731638249,-56.7981365016736));
#15034=CARTESIAN_POINT('Ctrl Pts',(-26.3331075729474,25.1769398266721,-56.7940307062087));
#15035=CARTESIAN_POINT('Ctrl Pts',(-26.4150117761055,25.0300617911736,-56.7833146009913));
#15036=CARTESIAN_POINT('Ctrl Pts',(-26.4607405198794,24.9379618357701,-56.7766188669879));
#15037=CARTESIAN_POINT('Ctrl Pts',(-26.6065914124831,24.6051566990373,-56.7525457358707));
#15038=CARTESIAN_POINT('Ctrl Pts',(-26.6818491650357,24.3546890214273,-56.7345563629171));
#15039=CARTESIAN_POINT('Ctrl Pts',(-26.7282239770885,24.0857588423779,-56.7165615523321));
#15040=CARTESIAN_POINT('Ctrl Pts',(-26.7302490556679,24.073599100837,-56.7157508905089));
#15041=CARTESIAN_POINT('Ctrl Pts',(-26.7352113916556,24.0427096739559,-56.7136995800862));
#15042=CARTESIAN_POINT('Ctrl Pts',(-26.7380532802513,24.0239648856954,-56.7124622354357));
#15043=CARTESIAN_POINT('Ctrl Pts',(-26.748141393568,23.9532178228717,-56.7078228969454));
#15044=CARTESIAN_POINT('Ctrl Pts',(-26.7542823736696,23.9010626919744,-56.7044650186804));
#15045=CARTESIAN_POINT('Ctrl Pts',(-26.7596780965245,23.8430631179638,-56.7008167489269));
#15046=CARTESIAN_POINT('Ctrl Pts',(-26.7601944196302,23.8373475906927,-56.7004581561174));
#15047=CARTESIAN_POINT('Ctrl Pts',(-26.7608962665517,23.8293397206702,-56.6999570635484));
#15048=CARTESIAN_POINT('Ctrl Pts',(-26.7610946038527,23.8270485558136,-56.6998138454095));
#15049=CARTESIAN_POINT('Ctrl Pts',(-26.7614530022426,23.8228561646309,-56.6995520634174));
#15050=CARTESIAN_POINT('Ctrl Pts',(-26.761613827664,23.8209550059082,-56.6994334561485));
#15051=CARTESIAN_POINT('Ctrl Pts',(-26.7619189709255,23.8173092857841,-56.6992062143715));
#15052=CARTESIAN_POINT('Ctrl Pts',(-26.7620635556231,23.8155647503987,-56.6990975646541));
#15053=CARTESIAN_POINT('Ctrl Pts',(-26.7623646150963,23.8118959027206,-56.6988692544573));
#15054=CARTESIAN_POINT('Ctrl Pts',(-26.7625207822942,23.8099715648311,-56.6987496114981));
#15055=CARTESIAN_POINT('Ctrl Pts',(-26.7628866824661,23.8054120192013,-56.6984663803339));
#15056=CARTESIAN_POINT('Ctrl Pts',(-26.7630949029009,23.8027766863175,-56.6983028774209));
#15057=CARTESIAN_POINT('Ctrl Pts',(-26.7636382385536,23.7957905193735,-56.6978699590247));
#15058=CARTESIAN_POINT('Ctrl Pts',(-26.7639677614759,23.7914392370389,-56.6976008551246));
#15059=CARTESIAN_POINT('Ctrl Pts',(-26.7700530152702,23.7088574988971,-56.692503554173));
#15060=CARTESIAN_POINT('Ctrl Pts',(-26.7729599694985,23.6304366978734,-56.687832280155));
#15061=CARTESIAN_POINT('Ctrl Pts',(-26.77300206773,23.5519818324221,-56.6832588369183));
#15062=CARTESIAN_POINT('Ctrl Pts',(-26.7730021430534,23.5518352458033,-56.6857734492205));
#15063=CARTESIAN_POINT('Ctrl Pts',(-26.7730504224152,23.4535279813412,-56.679673265777));
#15064=CARTESIAN_POINT('Ctrl Pts',(-26.7685963141078,23.3550373048322,-56.6735730823334));
#15065=CARTESIAN_POINT('Ctrl Pts',(-26.7596157733965,23.2568157492181,-56.6674728988899));
#15066=CARTESIAN_POINT('Ctrl Pts',(-26.7506466024252,23.1587185461992,-56.6613804385336));
#15067=CARTESIAN_POINT('Ctrl Pts',(-26.7371624241075,23.0608902267091,-56.6552879781773));
#15068=CARTESIAN_POINT('Ctrl Pts',(-26.719191208184,22.9637840950779,-56.649195517821));
#15069=CARTESIAN_POINT('Ctrl Pts',(-26.7012377562434,22.8667739498103,-56.6431090796705));
#15070=CARTESIAN_POINT('Ctrl Pts',(-26.6788061632909,22.7704850089876,-56.6370226415201));
#15071=CARTESIAN_POINT('Ctrl Pts',(-26.6519761626021,22.6753650646633,-56.6309362033697));
#15072=CARTESIAN_POINT('Ctrl Pts',(-26.6251605514189,22.5802961352085,-56.6248530295068));
#15073=CARTESIAN_POINT('Ctrl Pts',(-26.5939513369301,22.486395384793,-56.6187698556438));
#15074=CARTESIAN_POINT('Ctrl Pts',(-26.5584790597451,22.3940991169474,-56.6126866817809));
#15075=CARTESIAN_POINT('Ctrl Pts',(-26.5230158040352,22.3018263223192,-56.6066050550192));
#15076=CARTESIAN_POINT('Ctrl Pts',(-26.4832917988825,22.2111576150075,-56.6005234282574));
#15077=CARTESIAN_POINT('Ctrl Pts',(-26.439486663886,22.122511766752,-56.5944418014957));
#15078=CARTESIAN_POINT('Ctrl Pts',(-26.3956803167897,22.0338634656421,-56.5883600064537));
#15079=CARTESIAN_POINT('Ctrl Pts',(-26.3477928138976,21.9472385333444,-56.5822782114117));
#15080=CARTESIAN_POINT('Ctrl Pts',(-26.2960503898074,21.8630324260527,-56.5761964163697));
#15081=CARTESIAN_POINT('Ctrl Pts',(-26.2442576734751,21.7787444726934,-56.5701087099867));
#15082=CARTESIAN_POINT('Ctrl Pts',(-26.1886027854569,21.6968804204321,-56.5640210036038));
#15083=CARTESIAN_POINT('Ctrl Pts',(-26.1293559639129,21.6178076945985,-56.5579332972209));
#15084=CARTESIAN_POINT('Ctrl Pts',(-26.0700813385134,21.5386978608394,-56.551842733947));
#15085=CARTESIAN_POINT('Ctrl Pts',(-26.0072117069442,21.4623823051488,-56.5457521706732));
#15086=CARTESIAN_POINT('Ctrl Pts',(-25.941056938977,21.3891944925344,-56.5396616073993));
#15087=CARTESIAN_POINT('Ctrl Pts',(-25.8747881589441,21.3158805470054,-56.5335605475623));
#15088=CARTESIAN_POINT('Ctrl Pts',(-25.8052232455941,21.2457054299825,-56.5274594877253));
#15089=CARTESIAN_POINT('Ctrl Pts',(-25.7327082825262,21.1789650210451,-56.5213584278882));
#15090=CARTESIAN_POINT('Ctrl Pts',(-25.6620236823348,21.1139092184526,-56.5154113659706));
#15091=CARTESIAN_POINT('Ctrl Pts',(-25.5885365418587,21.0521169627958,-56.5094643040529));
#15092=CARTESIAN_POINT('Ctrl Pts',(-25.5125941137661,20.9938227795259,-56.5035172421352));
#15093=CARTESIAN_POINT('Ctrl Pts',(-25.4337781190522,20.9333228171747,-56.4973451508229));
#15094=CARTESIAN_POINT('Ctrl Pts',(-25.3520228255032,20.8763646210794,-56.4911730595105));
#15095=CARTESIAN_POINT('Ctrl Pts',(-25.2676801324481,20.8232468480425,-56.4850009681982));
#15096=CARTESIAN_POINT('Ctrl Pts',(-25.1834517154039,20.7702010443367,-56.4788372394594));
#15097=CARTESIAN_POINT('Ctrl Pts',(-25.0966432310861,20.7209855508462,-56.4726735107206));
#15098=CARTESIAN_POINT('Ctrl Pts',(-25.0076387365549,20.6758581585467,-56.4665097819818));
#15099=CARTESIAN_POINT('Ctrl Pts',(-24.9187285339321,20.630778574484,-56.4603525831351));
#15100=CARTESIAN_POINT('Ctrl Pts',(-24.8276273316299,20.5897786766317,-56.4541953842885));
#15101=CARTESIAN_POINT('Ctrl Pts',(-24.7347463655899,20.5530718698116,-56.4480381854418));
#15102=CARTESIAN_POINT('Ctrl Pts',(-24.6419332899036,20.5163918934413,-56.4418854871341));
#15103=CARTESIAN_POINT('Ctrl Pts',(-24.5473434396636,20.4839989284313,-56.4357327888264));
#15104=CARTESIAN_POINT('Ctrl Pts',(-24.4514099094734,20.4560591080417,-56.4295800905187));
#15105=CARTESIAN_POINT('Ctrl Pts',(-24.3555127574146,20.4281298824719,-56.4234297253229));
#15106=CARTESIAN_POINT('Ctrl Pts',(-24.2582733544368,20.4046505675488,-56.4172793601272));
#15107=CARTESIAN_POINT('Ctrl Pts',(-24.1601410627735,20.3857377913023,-56.4111289949314));
#15108=CARTESIAN_POINT('Ctrl Pts',(-24.0620197297389,20.3668271270831,-56.4049793165592));
#15109=CARTESIAN_POINT('Ctrl Pts',(-23.9630061328096,20.3524820698902,-56.398829638187));
#15110=CARTESIAN_POINT('Ctrl Pts',(-23.8635599713673,20.3427681574929,-56.3926799598148));
#15111=CARTESIAN_POINT('Ctrl Pts',(-23.7640983107092,20.3330527311304,-56.3865293229823));
#15112=CARTESIAN_POINT('Ctrl Pts',(-23.6642043840151,20.3279699254559,-56.3803786861499));
#15113=CARTESIAN_POINT('Ctrl Pts',(-23.5643421489165,20.3275333312074,-56.3742280493174));
#15114=CARTESIAN_POINT('Ctrl Pts',(-23.4643730822042,20.3270962698947,-56.3680708325956));
#15115=CARTESIAN_POINT('Ctrl Pts',(-23.3644362100354,20.3313153474497,-56.3619136158738));
#15116=CARTESIAN_POINT('Ctrl Pts',(-23.2649945056493,20.3401520003904,-56.355756399152));
#15117=CARTESIAN_POINT('Ctrl Pts',(-23.1654973231435,20.3489935832635,-56.3495957473441));
#15118=CARTESIAN_POINT('Ctrl Pts',(-23.0664962890278,20.3624578132963,-56.3434350955363));
#15119=CARTESIAN_POINT('Ctrl Pts',(-22.9684461885151,20.3804545978289,-56.3372744437285));
#15120=CARTESIAN_POINT('Ctrl Pts',(-22.8702320153172,20.3984814973818,-56.3311034829595));
#15121=CARTESIAN_POINT('Ctrl Pts',(-22.7729723775618,20.4210560031788,-56.3249325221905));
#15122=CARTESIAN_POINT('Ctrl Pts',(-22.6771090009775,20.4480375266909,-56.3187615614214));
#15123=CARTESIAN_POINT('Ctrl Pts',(-22.6039346857091,20.4686330301902,-56.314051151201));
#15124=CARTESIAN_POINT('Ctrl Pts',(-22.5315736407393,20.4917952623318,-56.3093407409807));
#15125=CARTESIAN_POINT('Ctrl Pts',(-22.4602141034591,20.5174429782486,-56.3046303307603));
#15126=CARTESIAN_POINT('Ctrl Pts',(-22.3667110836598,20.5510494025694,-56.298458239448));
#15127=CARTESIAN_POINT('Ctrl Pts',(-22.2745989956101,20.5890431831239,-56.2922861481356));
#15128=CARTESIAN_POINT('Ctrl Pts',(-22.1843193207942,20.6312896977649,-56.2861140568233));
#15129=CARTESIAN_POINT('Ctrl Pts',(-22.0941619660126,20.6734789725551,-56.2799503280845));
#15130=CARTESIAN_POINT('Ctrl Pts',(-22.0058324797428,20.7199093462814,-56.2737865993458));
#15131=CARTESIAN_POINT('Ctrl Pts',(-21.9197553449803,20.770397052246,-56.267622870607));
#15132=CARTESIAN_POINT('Ctrl Pts',(-21.8337694008637,20.8208312712245,-56.2614656717603));
#15133=CARTESIAN_POINT('Ctrl Pts',(-21.7500314369962,20.8753140583413,-56.2553084729137));
#15134=CARTESIAN_POINT('Ctrl Pts',(-21.6689432848947,20.9336147882519,-56.249151274067));
#15135=CARTESIAN_POINT('Ctrl Pts',(-21.5879144033147,20.9918729038647,-56.2429985757593));
#15136=CARTESIAN_POINT('Ctrl Pts',(-21.5095318343514,21.0539431611003,-56.2368458774516));
#15137=CARTESIAN_POINT('Ctrl Pts',(-21.4341694546978,21.119550992272,-56.2306931791439));
#15138=CARTESIAN_POINT('Ctrl Pts',(-21.3588356525657,21.1851339448608,-56.2245428139482));
#15139=CARTESIAN_POINT('Ctrl Pts',(-21.2865200913986,21.254251521018,-56.2183924487524));
#15140=CARTESIAN_POINT('Ctrl Pts',(-21.217563791652,21.3265887071514,-56.2122420835566));
#15141=CARTESIAN_POINT('Ctrl Pts',(-21.1486151923928,21.398917815247,-56.2060924051844));
#15142=CARTESIAN_POINT('Ctrl Pts',(-21.0830254084668,21.4744655040753,-56.1999427268122));
#15143=CARTESIAN_POINT('Ctrl Pts',(-21.0210980649029,21.5528804467762,-56.19379304844));
#15144=CARTESIAN_POINT('Ctrl Pts',(-20.9591610696316,21.6313076108649,-56.1876424116076));
#15145=CARTESIAN_POINT('Ctrl Pts',(-20.9008879177549,21.7126025754948,-56.1814917747751));
#15146=CARTESIAN_POINT('Ctrl Pts',(-20.8465408321569,21.7963823516964,-56.1753411379427));
#15147=CARTESIAN_POINT('Ctrl Pts',(-20.7921356065939,21.8802517546593,-56.1691839212209));
#15148=CARTESIAN_POINT('Ctrl Pts',(-20.7416650712976,21.9666109122583,-56.163026704499));
#15149=CARTESIAN_POINT('Ctrl Pts',(-20.6953470388263,22.0550494721425,-56.1568694877772));
#15150=CARTESIAN_POINT('Ctrl Pts',(-20.6490031657144,22.1435373715371,-56.1507088359694));
#15151=CARTESIAN_POINT('Ctrl Pts',(-20.6068165924558,22.2341065897243,-56.1445481841616));
#15152=CARTESIAN_POINT('Ctrl Pts',(-20.5689573532715,22.3263258093722,-56.1383875323538));
#15153=CARTESIAN_POINT('Ctrl Pts',(-20.5310347621173,22.418699344568,-56.1322165715848));
#15154=CARTESIAN_POINT('Ctrl Pts',(-20.4974541152694,22.5127279870423,-56.1260456108157));
#15155=CARTESIAN_POINT('Ctrl Pts',(-20.4683359047219,22.6079641114683,-56.1198746500467));
#15156=CARTESIAN_POINT('Ctrl Pts',(-20.44610942789,22.680659633388,-56.1151642398263));
#15157=CARTESIAN_POINT('Ctrl Pts',(-20.4264819900035,22.7540583630027,-56.1104538296058));
#15158=CARTESIAN_POINT('Ctrl Pts',(-20.4094869886824,22.8279580167423,-56.1057434193854));
#15159=CARTESIAN_POINT('Ctrl Pts',(-20.3872182912445,22.924789373139,-56.0995713280731));
#15160=CARTESIAN_POINT('Ctrl Pts',(-20.3693926077945,23.0228220673549,-56.0933992367608));
#15161=CARTESIAN_POINT('Ctrl Pts',(-20.3561353179195,23.1216119046324,-56.0872271454484));
#15162=CARTESIAN_POINT('Ctrl Pts',(-20.3428959903615,23.2202678914471,-56.0810634167097));
#15163=CARTESIAN_POINT('Ctrl Pts',(-20.3342128109161,23.3196785555821,-56.0748996879709));
#15164=CARTESIAN_POINT('Ctrl Pts',(-20.3301606246315,23.419387438681,-56.0687359592321));
#15165=CARTESIAN_POINT('Ctrl Pts',(-20.326112731258,23.5189906895761,-56.0625787603854));
#15166=CARTESIAN_POINT('Ctrl Pts',(-20.3266860948103,23.6188910996802,-56.0564215615387));
#15167=CARTESIAN_POINT('Ctrl Pts',(-20.3319038932866,23.7186259386206,-56.0502643626921));
#15168=CARTESIAN_POINT('Ctrl Pts',(-20.3371178778686,23.8182878774419,-56.0441116643844));
#15169=CARTESIAN_POINT('Ctrl Pts',(-20.3469695253134,23.9177840532136,-56.0379589660767));
#15170=CARTESIAN_POINT('Ctrl Pts',(-20.3614299334218,24.0166515017266,-56.031806267769));
#15171=CARTESIAN_POINT('Ctrl Pts',(-20.3758848581228,24.1154814595623,-56.0256559025732));
#15172=CARTESIAN_POINT('Ctrl Pts',(-20.3949450081306,24.2136827345155,-56.0195055373775));
#15173=CARTESIAN_POINT('Ctrl Pts',(-20.4185296932377,24.3107981421542,-56.0133551721817));
#15174=CARTESIAN_POINT('Ctrl Pts',(-20.4421117445961,24.407902704722,-56.0072054938095));
#15175=CARTESIAN_POINT('Ctrl Pts',(-20.4702172240049,24.5039212189263,-56.0010558154373));
#15176=CARTESIAN_POINT('Ctrl Pts',(-20.5027146764818,24.5984083328743,-55.994906137065));
#15177=CARTESIAN_POINT('Ctrl Pts',(-20.5352171938604,24.692910173144,-55.9887555002326));
#15178=CARTESIAN_POINT('Ctrl Pts',(-20.5721129026271,24.7858797282602,-55.9826048634001));
#15179=CARTESIAN_POINT('Ctrl Pts',(-20.6132213303213,24.8768893639367,-55.9764542265677));
#15180=CARTESIAN_POINT('Ctrl Pts',(-20.6543737353976,24.967996360805,-55.9702970098458));
#15181=CARTESIAN_POINT('Ctrl Pts',(-20.6997476797155,25.0571388546636,-55.964139793124));
#15182=CARTESIAN_POINT('Ctrl Pts',(-20.7491156638787,25.1439117833112,-55.9579825764022));
#15183=CARTESIAN_POINT('Ctrl Pts',(-20.798511190238,25.2307331222204,-55.9518219245944));
#15184=CARTESIAN_POINT('Ctrl Pts',(-20.8519049618298,25.3151818960516,-55.9456612727866));
#15185=CARTESIAN_POINT('Ctrl Pts',(-20.9090260148504,25.3968819068589,-55.9395006209787));
#15186=CARTESIAN_POINT('Ctrl Pts',(-20.9662426517051,25.478718630837,-55.9333296602097));
#15187=CARTESIAN_POINT('Ctrl Pts',(-21.0271987630487,25.5577970598691,-55.9271586994407));
#15188=CARTESIAN_POINT('Ctrl Pts',(-21.0915828852142,25.6337738615533,-55.9209877386716));
#15189=CARTESIAN_POINT('Ctrl Pts',(-21.1407284945332,25.691768380812,-55.9162773284513));
#15190=CARTESIAN_POINT('Ctrl Pts',(-21.1918706150156,25.7479563985689,-55.9115669182309));
#15191=CARTESIAN_POINT('Ctrl Pts',(-21.2448571149293,25.8022004740009,-55.9068565080105));
#15192=CARTESIAN_POINT('Ctrl Pts',(-21.3142739181782,25.8732648077051,-55.900685471614));
#15193=CARTESIAN_POINT('Ctrl Pts',(-21.3871018969899,25.9412415898445,-55.8945144352176));
#15194=CARTESIAN_POINT('Ctrl Pts',(-21.4630352761606,26.0057854047592,-55.8883433988211));
#15195=CARTESIAN_POINT('Ctrl Pts',(-21.5388783893179,26.0702524930363,-55.8821796982611));
#15196=CARTESIAN_POINT('Ctrl Pts',(-21.6178192436625,26.1312944400473,-55.8760159977011));
#15197=CARTESIAN_POINT('Ctrl Pts',(-21.6995142811262,26.1886015401434,-55.8698522971412));
#15198=CARTESIAN_POINT('Ctrl Pts',(-21.7811175908716,26.2458442954555,-55.8636955172242));
#15199=CARTESIAN_POINT('Ctrl Pts',(-21.8654685800901,26.2993602956288,-55.8575387373072));
#15200=CARTESIAN_POINT('Ctrl Pts',(-21.9521905582162,26.3488799616005,-55.8513819573902));
#15201=CARTESIAN_POINT('Ctrl Pts',(-21.9926372384212,26.3719756766279,-55.8485104672123));
#15202=CARTESIAN_POINT('Ctrl Pts',(-22.0335992091366,26.3942026744379,-55.8456389770345));
#15203=CARTESIAN_POINT('Ctrl Pts',(-22.0750360153461,26.4155367745563,-55.8427674868566));
#15204=CARTESIAN_POINT('Origin',(-23.5502525316942,23.5502525316942,-77.3107734492734));
#15205=CARTESIAN_POINT('',(-22.0750359442814,26.415536737968,-54.34883718749));
#15206=CARTESIAN_POINT('',(-22.0750360179885,26.4155367759168,-54.5955012513333));
#15207=CARTESIAN_POINT('',(-22.0750360153461,26.4155367745563,-77.3107734492734));
#15208=CARTESIAN_POINT('Ctrl Pts',(-22.0750359442814,26.415536737968,-54.34883718749));
#15209=CARTESIAN_POINT('Ctrl Pts',(-21.9634080683998,26.3580641515636,-54.3561191662865));
#15210=CARTESIAN_POINT('Ctrl Pts',(-21.8551854385235,26.2940922482147,-54.3631623810082));
#15211=CARTESIAN_POINT('Ctrl Pts',(-21.6005988914945,26.1227617454723,-54.3803202095482));
#15212=CARTESIAN_POINT('Ctrl Pts',(-21.4590714163177,26.0090956425743,-54.3903947990664));
#15213=CARTESIAN_POINT('Ctrl Pts',(-21.2709694206182,25.8299796957877,-54.4054241972002));
#15214=CARTESIAN_POINT('Ctrl Pts',(-21.216088097284,25.7737548164187,-54.4100375124971));
#15215=CARTESIAN_POINT('Ctrl Pts',(-21.1365410134935,25.6860667975991,-54.4171248047951));
#15216=CARTESIAN_POINT('Ctrl Pts',(-21.1103146136579,25.6560560861961,-54.4195324404199));
#15217=CARTESIAN_POINT('Ctrl Pts',(-21.0798485180739,25.6198605189877,-54.422418471595));
#15218=CARTESIAN_POINT('Ctrl Pts',(-21.0750645639555,25.6141366695434,-54.4228743400978));
#15219=CARTESIAN_POINT('Ctrl Pts',(-21.0677310852834,25.6053002242018,-54.4235773326841));
#15220=CARTESIAN_POINT('Ctrl Pts',(-21.0651674223618,25.6021993510616,-54.4238238799014));
#15221=CARTESIAN_POINT('Ctrl Pts',(-21.060505101604,25.5965384977159,-54.4242737067586));
#15222=CARTESIAN_POINT('Ctrl Pts',(-21.0584045654735,25.593980065758,-54.4244769096891));
#15223=CARTESIAN_POINT('Ctrl Pts',(-21.0541595360249,25.5887933887831,-54.4248886665072));
#15224=CARTESIAN_POINT('Ctrl Pts',(-21.0520152433715,25.586164985643,-54.4250972281569));
#15225=CARTESIAN_POINT('Ctrl Pts',(-21.0458974877022,25.578641824525,-54.4256939015152));
#15226=CARTESIAN_POINT('Ctrl Pts',(-21.0419342490145,25.5737388058037,-54.4260824254543));
#15227=CARTESIAN_POINT('Ctrl Pts',(-21.0249478608852,25.5525979446066,-54.4277562289903));
#15228=CARTESIAN_POINT('Ctrl Pts',(-21.0120680400948,25.5362460580891,-54.4290472450986));
#15229=CARTESIAN_POINT('Ctrl Pts',(-20.7814081133303,25.2374971202017,-54.452572927402));
#15230=CARTESIAN_POINT('Ctrl Pts',(-20.6118750318638,24.9210523774672,-54.4769229566944));
#15231=CARTESIAN_POINT('Ctrl Pts',(-20.4682295873338,24.4966403678763,-54.5070118918893));
#15232=CARTESIAN_POINT('Ctrl Pts',(-20.442564008967,24.4086172455943,-54.5131005701901));
#15233=CARTESIAN_POINT('Ctrl Pts',(-20.4127760401292,24.2874472422953,-54.5211790219131));
#15234=CARTESIAN_POINT('Ctrl Pts',(-20.4053643899234,24.2551592969902,-54.523302784798));
#15235=CARTESIAN_POINT('Ctrl Pts',(-20.3960356918904,24.2114391321839,-54.5261344938964));
#15236=CARTESIAN_POINT('Ctrl Pts',(-20.3936808071156,24.2001037070915,-54.5268647058411));
#15237=CARTESIAN_POINT('Ctrl Pts',(-20.3903291676397,24.183522145934,-54.5279268240371));
#15238=CARTESIAN_POINT('Ctrl Pts',(-20.3892843172612,24.178285985677,-54.5282613433917));
#15239=CARTESIAN_POINT('Ctrl Pts',(-20.3876645171647,24.1700620746803,-54.528785334741));
#15240=CARTESIAN_POINT('Ctrl Pts',(-20.3870807830107,24.1670760945827,-54.5289752978534));
#15241=CARTESIAN_POINT('Ctrl Pts',(-20.3861029735488,24.1620364062077,-54.5292954194609));
#15242=CARTESIAN_POINT('Ctrl Pts',(-20.3857066685261,24.1599831405626,-54.529425704586));
#15243=CARTESIAN_POINT('Ctrl Pts',(-20.3849341154542,24.1559594825258,-54.5296807429276));
#15244=CARTESIAN_POINT('Ctrl Pts',(-20.3845577081447,24.1539891221694,-54.5298055052476));
#15245=CARTESIAN_POINT('Ctrl Pts',(-20.383839674244,24.1502113320759,-54.5300444654509));
#15246=CARTESIAN_POINT('Ctrl Pts',(-20.3834977563847,24.1484039665742,-54.5301586796248));
#15247=CARTESIAN_POINT('Ctrl Pts',(-20.3827074676054,24.1442068576727,-54.5304236594829));
#15248=CARTESIAN_POINT('Ctrl Pts',(-20.3822602525221,24.1418168930123,-54.5305743584375));
#15249=CARTESIAN_POINT('Ctrl Pts',(-20.3808608987448,24.1342915017538,-54.5310482833016));
#15250=CARTESIAN_POINT('Ctrl Pts',(-20.3799185329231,24.1291542320742,-54.5313709505443));
#15251=CARTESIAN_POINT('Ctrl Pts',(-20.3723412663951,24.0872736149722,-54.5339945847663));
#15252=CARTESIAN_POINT('Ctrl Pts',(-20.3663325306277,24.0504178800987,-54.5362604995031));
#15253=CARTESIAN_POINT('Ctrl Pts',(-20.3598623774903,24.0058698233629,-54.5389567647833));
#15254=CARTESIAN_POINT('Ctrl Pts',(-20.3587865005749,23.9982715345961,-54.5394151623451));
#15255=CARTESIAN_POINT('Ctrl Pts',(-20.3563798038378,23.9808257568182,-54.5404643852637));
#15256=CARTESIAN_POINT('Ctrl Pts',(-20.3550673622209,23.970975767673,-54.5410543989947));
#15257=CARTESIAN_POINT('Ctrl Pts',(-20.3533295086966,23.9574556687838,-54.5418611761408));
#15258=CARTESIAN_POINT('Ctrl Pts',(-20.3528648313952,23.9537907628808,-54.5420795602604));
#15259=CARTESIAN_POINT('Ctrl Pts',(-20.3483996903152,23.9180822978199,-54.5442044068596));
#15260=CARTESIAN_POINT('Ctrl Pts',(-20.3448746309769,23.8859801009238,-54.5460915612406));
#15261=CARTESIAN_POINT('Ctrl Pts',(-20.313684050082,23.5563354280417,-54.5652821737521));
#15262=CARTESIAN_POINT('Ctrl Pts',(-20.3270446235538,23.2563618601901,-54.5813170389239));
#15263=CARTESIAN_POINT('Ctrl Pts',(-20.3965878448685,22.8814366968608,-54.6033231574784));
#15264=CARTESIAN_POINT('Ctrl Pts',(-20.4147290828368,22.8009817787368,-54.6081543329074));
#15265=CARTESIAN_POINT('Ctrl Pts',(-20.4469014448502,22.6801101628351,-54.6156313883517));
#15266=CARTESIAN_POINT('Ctrl Pts',(-20.4586852539192,22.6391283844278,-54.6182052580888));
#15267=CARTESIAN_POINT('Ctrl Pts',(-20.4735236451243,22.5911306848696,-54.6212695649207));
#15268=CARTESIAN_POINT('Ctrl Pts',(-20.4757947286929,22.5838754963129,-54.6217341055924));
#15269=CARTESIAN_POINT('Ctrl Pts',(-20.4793161907327,22.5727639195181,-54.6224476603139));
#15270=CARTESIAN_POINT('Ctrl Pts',(-20.4805482207853,22.5689017073094,-54.6226960697375));
#15271=CARTESIAN_POINT('Ctrl Pts',(-20.4828094830234,22.561858945672,-54.6231497593548));
#15272=CARTESIAN_POINT('Ctrl Pts',(-20.4838363842109,22.5586776489706,-54.6233549624022));
#15273=CARTESIAN_POINT('Ctrl Pts',(-20.4859120022386,22.5522815316441,-54.6237680690346));
#15274=CARTESIAN_POINT('Ctrl Pts',(-20.4869608327213,22.5490667525951,-54.6239759761574));
#15275=CARTESIAN_POINT('Ctrl Pts',(-20.4899632202671,22.5399129943118,-54.6245687546988));
#15276=CARTESIAN_POINT('Ctrl Pts',(-20.4919289945143,22.5339780650848,-54.6249540297664));
#15277=CARTESIAN_POINT('Ctrl Pts',(-20.5003747544217,22.5087256417164,-54.6265973726622));
#15278=CARTESIAN_POINT('Ctrl Pts',(-20.5070204782076,22.4894644488189,-54.6278609228495));
#15279=CARTESIAN_POINT('Ctrl Pts',(-20.636204621896,22.1262599378502,-54.6518830474312));
#15280=CARTESIAN_POINT('Ctrl Pts',(-20.8161184110933,21.8056060612468,-54.6768763257385));
#15281=CARTESIAN_POINT('Ctrl Pts',(-21.127257077375,21.4214095583183,-54.7100126527375));
#15282=CARTESIAN_POINT('Ctrl Pts',(-21.2147374262675,21.3257846333039,-54.7185446932962));
#15283=CARTESIAN_POINT('Ctrl Pts',(-21.3112385772449,21.2322883971883,-54.7269739522954));
#15284=CARTESIAN_POINT('Ctrl Pts',(-21.3147392972331,21.2289120145895,-54.7272784742693));
#15285=CARTESIAN_POINT('Ctrl Pts',(-21.3203030766058,21.2235701061391,-54.7277604419814));
#15286=CARTESIAN_POINT('Ctrl Pts',(-21.3223611049412,21.2215993861215,-54.7279382851833));
#15287=CARTESIAN_POINT('Ctrl Pts',(-21.32626432619,21.2178716631422,-54.7282747509249));
#15288=CARTESIAN_POINT('Ctrl Pts',(-21.3281089925562,21.2161141155363,-54.7284334156561));
#15289=CARTESIAN_POINT('Ctrl Pts',(-21.3313110277448,21.2130705403174,-54.7287082231869));
#15290=CARTESIAN_POINT('Ctrl Pts',(-21.3326674332857,21.2117835047129,-54.7288244449558));
#15291=CARTESIAN_POINT('Ctrl Pts',(-21.3353037893955,21.2092863349823,-54.7290499701177));
#15292=CARTESIAN_POINT('Ctrl Pts',(-21.3365836096756,21.208076071885,-54.7291592837957));
#15293=CARTESIAN_POINT('Ctrl Pts',(-21.3396148324195,21.2052142974818,-54.7294177960252));
#15294=CARTESIAN_POINT('Ctrl Pts',(-21.3413670973102,21.2035636952212,-54.7295669235955));
#15295=CARTESIAN_POINT('Ctrl Pts',(-21.3474927006835,21.1978064260285,-54.7300871685351));
#15296=CARTESIAN_POINT('Ctrl Pts',(-21.3518756902447,21.1937099758455,-54.7304574983622));
#15297=CARTESIAN_POINT('Ctrl Pts',(-21.4058921103276,21.1435067519798,-54.7349983775873));
#15298=CARTESIAN_POINT('Ctrl Pts',(-21.4569603154764,21.098959778807,-54.7390524286924));
#15299=CARTESIAN_POINT('Ctrl Pts',(-21.5209131961418,21.0466310039921,-54.7439003135547));
#15300=CARTESIAN_POINT('Ctrl Pts',(-21.5324924332075,21.037289521517,-54.7447692460259));
#15301=CARTESIAN_POINT('Ctrl Pts',(-21.6955988640664,20.907558587243,-54.7568927481815));
#15302=CARTESIAN_POINT('Ctrl Pts',(-21.8576167316477,20.8009676455572,-54.7675575124803));
#15303=CARTESIAN_POINT('Ctrl Pts',(-22.1279887555187,20.6561046954278,-54.7847432974721));
#15304=CARTESIAN_POINT('Ctrl Pts',(-22.2304877550098,20.6079499299511,-54.7911290819701));
#15305=CARTESIAN_POINT('Ctrl Pts',(-22.4113832564205,20.5343212314807,-54.8024054318773));
#15306=CARTESIAN_POINT('Ctrl Pts',(-22.4886152769386,20.5062765845659,-54.8072208502105));
#15307=CARTESIAN_POINT('Ctrl Pts',(-22.6066365938036,20.4684586068987,-54.8146324315996));
#15308=CARTESIAN_POINT('Ctrl Pts',(-22.6466861380622,20.4564793733931,-54.8171562465747));
#15309=CARTESIAN_POINT('Ctrl Pts',(-22.6942402668426,20.4432575642188,-54.8201669187194));
#15310=CARTESIAN_POINT('Ctrl Pts',(-22.701531628638,20.4412579108123,-54.8206289195138));
#15311=CARTESIAN_POINT('Ctrl Pts',(-22.7127346515487,20.4382278329951,-54.8213393821206));
#15312=CARTESIAN_POINT('Ctrl Pts',(-22.7166413629431,20.4371790754502,-54.8215872474989));
#15313=CARTESIAN_POINT('Ctrl Pts',(-22.7234663050792,20.4353606866391,-54.8220204645779));
#15314=CARTESIAN_POINT('Ctrl Pts',(-22.7263836679501,20.434587792643,-54.8222057100522));
#15315=CARTESIAN_POINT('Ctrl Pts',(-22.7329579988879,20.4328559412376,-54.822623310694));
#15316=CARTESIAN_POINT('Ctrl Pts',(-22.7366155726289,20.4318993197898,-54.8228557413549));
#15317=CARTESIAN_POINT('Ctrl Pts',(-22.746427142136,20.4293515866171,-54.8234795226929));
#15318=CARTESIAN_POINT('Ctrl Pts',(-22.7525841527638,20.427772247976,-54.823871254363));
#15319=CARTESIAN_POINT('Ctrl Pts',(-22.7793516980797,20.420990425734,-54.8255756081299));
#15320=CARTESIAN_POINT('Ctrl Pts',(-22.8000083744637,20.4159738119994,-54.8268942278418));
#15321=CARTESIAN_POINT('Ctrl Pts',(-22.833501515297,20.4081898447627,-54.8290380683351));
#15322=CARTESIAN_POINT('Ctrl Pts',(-22.8463081423857,20.4052958965979,-54.8298591639152));
#15323=CARTESIAN_POINT('Ctrl Pts',(-22.8650067500868,20.4011904557137,-54.8310600734351));
#15324=CARTESIAN_POINT('Ctrl Pts',(-22.8708851226519,20.3999170476021,-54.8314379037886));
#15325=CARTESIAN_POINT('Ctrl Pts',(-22.8797380823231,20.3980251975436,-54.8320073730602));
#15326=CARTESIAN_POINT('Ctrl Pts',(-22.8827100591102,20.3973944885567,-54.8321986223099));
#15327=CARTESIAN_POINT('Ctrl Pts',(-22.8893202399611,20.3960014500662,-54.8326241628575));
#15328=CARTESIAN_POINT('Ctrl Pts',(-22.8929588759452,20.3952412115666,-54.8328585198933));
#15329=CARTESIAN_POINT('Ctrl Pts',(-22.9034154196993,20.3930753474378,-54.8335323344072));
#15330=CARTESIAN_POINT('Ctrl Pts',(-22.9102365460895,20.391685521293,-54.8339722873282));
#15331=CARTESIAN_POINT('Ctrl Pts',(-22.9231752579306,20.3890928510203,-54.8348075866252));
#15332=CARTESIAN_POINT('Ctrl Pts',(-22.9292919437922,20.3878856362517,-54.8352027945176));
#15333=CARTESIAN_POINT('Ctrl Pts',(-22.9394200686109,20.3859172246424,-54.8358577303089));
#15334=CARTESIAN_POINT('Ctrl Pts',(-22.9434295390428,20.3851458843982,-54.8361171435987));
#15335=CARTESIAN_POINT('Ctrl Pts',(-22.9529699124465,20.383329305798,-54.8367347428039));
#15336=CARTESIAN_POINT('Ctrl Pts',(-22.9585020959488,20.3822909367354,-54.8370931386916));
#15337=CARTESIAN_POINT('Ctrl Pts',(-22.9844354367949,20.3774936510289,-54.8387744604907));
#15338=CARTESIAN_POINT('Ctrl Pts',(-23.0048695065764,20.3739173440357,-54.840102910461));
#15339=CARTESIAN_POINT('Ctrl Pts',(-23.3240678213129,20.3212231781401,-54.8609117696472));
#15340=CARTESIAN_POINT('Ctrl Pts',(-23.6282327343412,20.3142601291747,-54.8817312681102));
#15341=CARTESIAN_POINT('Ctrl Pts',(-23.9965121896926,20.3578212144398,-54.9065290676153));
#15342=CARTESIAN_POINT('Ctrl Pts',(-24.0639483670755,20.3679761280843,-54.9110428536091));
#15343=CARTESIAN_POINT('Ctrl Pts',(-24.1802454107345,20.3892825100537,-54.9187275141719));
#15344=CARTESIAN_POINT('Ctrl Pts',(-24.2292620805534,20.399447996854,-54.9219352049622));
#15345=CARTESIAN_POINT('Ctrl Pts',(-24.283942889799,20.4121236430962,-54.9254635358839));
#15346=CARTESIAN_POINT('Ctrl Pts',(-24.2898567194452,20.4135121678934,-54.9258444699291));
#15347=CARTESIAN_POINT('Ctrl Pts',(-24.2990113188923,20.4156889314076,-54.9264330921904));
#15348=CARTESIAN_POINT('Ctrl Pts',(-24.3022548118121,20.4164654845921,-54.9266414352341));
#15349=CARTESIAN_POINT('Ctrl Pts',(-24.307648497744,20.4177656904545,-54.9269875428781));
#15350=CARTESIAN_POINT('Ctrl Pts',(-24.3097993576234,20.4182865230635,-54.9271254684937));
#15351=CARTESIAN_POINT('Ctrl Pts',(-24.3139819178319,20.4193038956468,-54.9273934952788));
#15352=CARTESIAN_POINT('Ctrl Pts',(-24.3160136739178,20.419800198574,-54.9275236100879));
#15353=CARTESIAN_POINT('Ctrl Pts',(-24.3198169282496,20.420733154714,-54.9277670131379));
#15354=CARTESIAN_POINT('Ctrl Pts',(-24.3215885268806,20.4211693314751,-54.9278803279453));
#15355=CARTESIAN_POINT('Ctrl Pts',(-24.3256135252938,20.4221639329359,-54.9281376274386));
#15356=CARTESIAN_POINT('Ctrl Pts',(-24.3278666884065,20.4227232871546,-54.9282815571528));
#15357=CARTESIAN_POINT('Ctrl Pts',(-24.333587522705,20.4241500651316,-54.9286467370445));
#15358=CARTESIAN_POINT('Ctrl Pts',(-24.3370543690444,20.4250208269056,-54.9288677936444));
#15359=CARTESIAN_POINT('Ctrl Pts',(-24.356094056155,20.4298366817899,-54.9300805180366));
#15360=CARTESIAN_POINT('Ctrl Pts',(-24.3716390417828,20.4338924971086,-54.9310658546786));
#15361=CARTESIAN_POINT('Ctrl Pts',(-24.6845075584583,20.5180262119252,-54.9508125533594));
#15362=CARTESIAN_POINT('Ctrl Pts',(-24.9689232365307,20.6402047948141,-54.9673273060959));
#15363=CARTESIAN_POINT('Ctrl Pts',(-25.295285764587,20.8398041747061,-54.9889391325971));
#15364=CARTESIAN_POINT('Ctrl Pts',(-25.3574912261611,20.8808783091154,-54.9931865587937));
#15365=CARTESIAN_POINT('Ctrl Pts',(-25.4823553521446,20.9696921958522,-55.0020520247273));
#15366=CARTESIAN_POINT('Ctrl Pts',(-25.5447988174219,21.0176458437683,-55.006674515143));
#15367=CARTESIAN_POINT('Ctrl Pts',(-25.6361753409885,21.0932955346298,-55.0137755930199));
#15368=CARTESIAN_POINT('Ctrl Pts',(-25.6664526318269,21.1193250195556,-55.0161875546358));
#15369=CARTESIAN_POINT('Ctrl Pts',(-25.7018058531225,21.1508793689383,-55.0190782309406));
#15370=CARTESIAN_POINT('Ctrl Pts',(-25.7073568406882,21.1558686301982,-55.0195343339643));
#15371=CARTESIAN_POINT('Ctrl Pts',(-25.715874020412,21.1635775800833,-55.020237612344));
#15372=CARTESIAN_POINT('Ctrl Pts',(-25.718852559336,21.1662836399253,-55.0204842100909));
#15373=CARTESIAN_POINT('Ctrl Pts',(-25.7242719577914,21.1712258282852,-55.0209340892659));
#15374=CARTESIAN_POINT('Ctrl Pts',(-25.7267144588198,21.173460155355,-55.02113729389));
#15375=CARTESIAN_POINT('Ctrl Pts',(-25.7316524626707,21.1779912883834,-55.0215490189667));
#15376=CARTESIAN_POINT('Ctrl Pts',(-25.7341477905415,21.180288278035,-55.0217575471256));
#15377=CARTESIAN_POINT('Ctrl Pts',(-25.7412692685266,21.1868645113543,-55.02235402115));
#15378=CARTESIAN_POINT('Ctrl Pts',(-25.7458864802154,21.1911533733365,-55.0227423788047));
#15379=CARTESIAN_POINT('Ctrl Pts',(-25.7656836733363,21.2096511676624,-55.0244146116046));
#15380=CARTESIAN_POINT('Ctrl Pts',(-25.7807382601546,21.2239930295828,-55.0257042100048));
#15381=CARTESIAN_POINT('Ctrl Pts',(-26.0444468928259,21.4801303568751,-55.0486183487306));
#15382=CARTESIAN_POINT('Ctrl Pts',(-26.2525510821041,21.7603180086611,-55.0722270704238));
#15383=CARTESIAN_POINT('Ctrl Pts',(-26.4577859842493,22.1565916928722,-55.1022570871738));
#15384=CARTESIAN_POINT('Ctrl Pts',(-26.4994772107453,22.2471338850914,-55.1088943426205));
#15385=CARTESIAN_POINT('Ctrl Pts',(-26.5498173979832,22.3713086871535,-55.1175781841747));
#15386=CARTESIAN_POINT('Ctrl Pts',(-26.5622159571699,22.4033547524672,-55.1197827489849));
#15387=CARTESIAN_POINT('Ctrl Pts',(-26.5803555802647,22.4525639721244,-55.1231061545352));
#15388=CARTESIAN_POINT('Ctrl Pts',(-26.5864681647991,22.4695863832581,-55.1242446172016));
#15389=CARTESIAN_POINT('Ctrl Pts',(-26.5937279776328,22.4903515611689,-55.125619075039));
#15390=CARTESIAN_POINT('Ctrl Pts',(-26.5950119530271,22.4940456750877,-55.1258630413849));
#15391=CARTESIAN_POINT('Ctrl Pts',(-26.597003331298,22.4998088592817,-55.1262427875031));
#15392=CARTESIAN_POINT('Ctrl Pts',(-26.597715352722,22.5018763118572,-55.1263788420695));
#15393=CARTESIAN_POINT('Ctrl Pts',(-26.5989698109654,22.5055308813404,-55.1266190329537));
#15394=CARTESIAN_POINT('Ctrl Pts',(-26.5995131101697,22.5071176889107,-55.1267232206084));
#15395=CARTESIAN_POINT('Ctrl Pts',(-26.6006708534005,22.5105077292374,-55.1269455867946));
#15396=CARTESIAN_POINT('Ctrl Pts',(-26.6012849355981,22.512311077655,-55.1270637433277));
#15397=CARTESIAN_POINT('Ctrl Pts',(-26.6030528620615,22.517517996102,-55.1274045252061));
#15398=CARTESIAN_POINT('Ctrl Pts',(-26.6042026173207,22.5209229669302,-55.1276269066011));
#15399=CARTESIAN_POINT('Ctrl Pts',(-26.6092677257412,22.5360063486839,-55.128609978525));
#15400=CARTESIAN_POINT('Ctrl Pts',(-26.6131218719575,22.5477054289738,-55.1293670772155));
#15401=CARTESIAN_POINT('Ctrl Pts',(-26.6178227146822,22.5622547741731,-55.1303022743309));
#15402=CARTESIAN_POINT('Ctrl Pts',(-26.6187325982724,22.5650842833267,-55.1304838509068));
#15403=CARTESIAN_POINT('Ctrl Pts',(-26.6222418452067,22.5760491847498,-55.1311863584215));
#15404=CARTESIAN_POINT('Ctrl Pts',(-26.6248128076308,22.5841937256383,-55.1317057458969));
#15405=CARTESIAN_POINT('Ctrl Pts',(-26.6289021989864,22.5973301787154,-55.132539719737));
#15406=CARTESIAN_POINT('Ctrl Pts',(-26.6304409147866,22.6023156613576,-55.1328553568212));
#15407=CARTESIAN_POINT('Ctrl Pts',(-26.6332670492646,22.6115519547058,-55.1334385489814));
#15408=CARTESIAN_POINT('Ctrl Pts',(-26.6345577979947,22.6158017231831,-55.1337062714734));
#15409=CARTESIAN_POINT('Ctrl Pts',(-26.7265388096929,22.9209145330444,-55.1528843487594));
#15410=CARTESIAN_POINT('Ctrl Pts',(-26.7727633327215,23.2334680455744,-55.1696604153421));
#15411=CARTESIAN_POINT('Ctrl Pts',(-26.7730574974556,23.6215446029327,-55.1917202091736));
#15412=CARTESIAN_POINT('Ctrl Pts',(-26.770582859349,23.695256143819,-55.1959563771899));
#15413=CARTESIAN_POINT('Ctrl Pts',(-26.7593379903672,23.8606823936348,-55.2056358162423));
#15414=CARTESIAN_POINT('Ctrl Pts',(-26.7491595350554,23.9522322375907,-55.2111131797558));
#15415=CARTESIAN_POINT('Ctrl Pts',(-26.7335159642199,24.0532988590675,-55.217338916616));
#15416=CARTESIAN_POINT('Ctrl Pts',(-26.731907224948,24.0633754189928,-55.2179616053503));
#15417=CARTESIAN_POINT('Ctrl Pts',(-26.7295828783929,24.0775029746968,-55.2188374467544));
#15418=CARTESIAN_POINT('Ctrl Pts',(-26.7289073175066,24.0815605736646,-55.2190893252596));
#15419=CARTESIAN_POINT('Ctrl Pts',(-26.7276551751058,24.08899340521,-55.2195513268156));
#15420=CARTESIAN_POINT('Ctrl Pts',(-26.7270809784511,24.0923690384476,-55.2197613736964));
#15421=CARTESIAN_POINT('Ctrl Pts',(-26.725907954037,24.0991992447175,-55.2201868437949));
#15422=CARTESIAN_POINT('Ctrl Pts',(-26.725308866597,24.1026537674217,-55.2204022749987));
#15423=CARTESIAN_POINT('Ctrl Pts',(-26.7238229310854,24.1111398517284,-55.2209320795149));
#15424=CARTESIAN_POINT('Ctrl Pts',(-26.722929755159,24.1161702826921,-55.2212466542327));
#15425=CARTESIAN_POINT('Ctrl Pts',(-26.7196451928627,24.1344169868981,-55.2223895806019));
#15426=CARTESIAN_POINT('Ctrl Pts',(-26.7171831812246,24.1476202607189,-55.2232201832828));
#15427=CARTESIAN_POINT('Ctrl Pts',(-26.680120228734,24.3397102156873,-55.2353575426157));
#15428=CARTESIAN_POINT('Ctrl Pts',(-26.6304990414954,24.5153307830893,-55.2471564643207));
#15429=CARTESIAN_POINT('Ctrl Pts',(-26.4957117914711,24.8733336040978,-55.2726524478074));
#15430=CARTESIAN_POINT('Ctrl Pts',(-26.4077711531711,25.0538665935108,-55.2863697394559));
#15431=CARTESIAN_POINT('Ctrl Pts',(-26.2773788723654,25.2682318598123,-55.3031468688061));
#15432=CARTESIAN_POINT('Ctrl Pts',(-26.2501053471981,25.310782636509,-55.306501069829));
#15433=CARTESIAN_POINT('Ctrl Pts',(-26.2069997537772,25.3746746237673,-55.3115561877946));
#15434=CARTESIAN_POINT('Ctrl Pts',(-26.1918865368085,25.3964896886562,-55.3132855881141));
#15435=CARTESIAN_POINT('Ctrl Pts',(-26.1499063449645,25.4555146533904,-55.3179690113146));
#15436=CARTESIAN_POINT('Ctrl Pts',(-26.122509975173,25.4923431294445,-55.3208958796263));
#15437=CARTESIAN_POINT('Ctrl Pts',(-26.0912753038264,25.532510252206,-55.3240819153644));
#15438=CARTESIAN_POINT('Ctrl Pts',(-26.0882068998961,25.5364373228806,-55.3243933414484));
#15439=CARTESIAN_POINT('Ctrl Pts',(-26.0836080880757,25.5422950153119,-55.3248577496779));
#15440=CARTESIAN_POINT('Ctrl Pts',(-26.082084574046,25.5442310022417,-55.3250112183647));
#15441=CARTESIAN_POINT('Ctrl Pts',(-26.0794588151184,25.5475597922796,-55.3252750598111));
#15442=CARTESIAN_POINT('Ctrl Pts',(-26.078357638958,25.5489534307687,-55.3253855090895));
#15443=CARTESIAN_POINT('Ctrl Pts',(-26.076077356691,25.5518344357035,-55.3256138114504));
#15444=CARTESIAN_POINT('Ctrl Pts',(-26.074898090815,25.5533216682578,-55.3257316520467));
#15445=CARTESIAN_POINT('Ctrl Pts',(-26.0721208592695,25.5568178284469,-55.3260086394904));
#15446=CARTESIAN_POINT('Ctrl Pts',(-26.0705218016787,25.5588258957119,-55.3261677076128));
#15447=CARTESIAN_POINT('Ctrl Pts',(-26.0652978370602,25.5653699947338,-55.3266860269692));
#15448=CARTESIAN_POINT('Ctrl Pts',(-26.0616630432463,25.5698981742764,-55.3270445698347));
#15449=CARTESIAN_POINT('Ctrl Pts',(-25.9723215332929,25.6805845479778,-55.3358068096169));
#15450=CARTESIAN_POINT('Ctrl Pts',(-25.8799586128539,25.7812193526092,-55.3437312782584));
#15451=CARTESIAN_POINT('Ctrl Pts',(-25.5217700317589,26.1248943015793,-55.3719311850345));
#15452=CARTESIAN_POINT('Ctrl Pts',(-25.2221814632887,26.3287992394889,-55.3913060963372));
#15453=CARTESIAN_POINT('Ctrl Pts',(-24.8765276641856,26.487518074339,-55.4143074282496));
#15454=CARTESIAN_POINT('Ctrl Pts',(-24.8578890603224,26.4958630412873,-55.4155483190382));
#15455=CARTESIAN_POINT('Ctrl Pts',(-24.8334374239143,26.5065328384396,-55.4171774224722));
#15456=CARTESIAN_POINT('Ctrl Pts',(-24.827694869945,26.5090187933722,-55.4175601088675));
#15457=CARTESIAN_POINT('Ctrl Pts',(-24.8188369662787,26.5128227903177,-55.4181505482601));
#15458=CARTESIAN_POINT('Ctrl Pts',(-24.8157266984097,26.5141526882763,-55.4183578961229));
#15459=CARTESIAN_POINT('Ctrl Pts',(-24.8096394145586,26.5167441794213,-55.4187637645624));
#15460=CARTESIAN_POINT('Ctrl Pts',(-24.8066625816164,26.5180061944998,-55.4189622704626));
#15461=CARTESIAN_POINT('Ctrl Pts',(-24.8000728106564,26.5207882067102,-55.4194017602233));
#15462=CARTESIAN_POINT('Ctrl Pts',(-24.7964589925964,26.5223060949462,-55.4196428155479));
#15463=CARTESIAN_POINT('Ctrl Pts',(-24.7889704208909,26.5254354107681,-55.4201424180721));
#15464=CARTESIAN_POINT('Ctrl Pts',(-24.7850952729389,26.5270458696803,-55.4204009976828));
#15465=CARTESIAN_POINT('Ctrl Pts',(-24.7752003043774,26.5311354379836,-55.421061393388));
#15466=CARTESIAN_POINT('Ctrl Pts',(-24.7691761181068,26.5336038747811,-55.4214635711034));
#15467=CARTESIAN_POINT('Ctrl Pts',(-24.7518354393625,26.5406480036397,-55.4226216104398));
#15468=CARTESIAN_POINT('Ctrl Pts',(-24.7405004683905,26.5451776401428,-55.4233790271196));
#15469=CARTESIAN_POINT('Ctrl Pts',(-24.6307236361333,26.5883245938208,-55.4307192045059));
#15470=CARTESIAN_POINT('Ctrl Pts',(-24.5304734175282,26.6221350960552,-55.4374625312866));
#15471=CARTESIAN_POINT('Ctrl Pts',(-24.2823213188424,26.6924421937905,-55.4542668023194));
#15472=CARTESIAN_POINT('Ctrl Pts',(-24.1331501821021,26.7235004702846,-55.4644693184428));
#15473=CARTESIAN_POINT('Ctrl Pts',(-23.7535422485739,26.7748619488649,-55.4903708273433));
#15474=CARTESIAN_POINT('Ctrl Pts',(-23.5220394199463,26.7811438036041,-55.5061351802148));
#15475=CARTESIAN_POINT('Ctrl Pts',(-23.2785771804949,26.7615586497784,-55.521553168706));
#15476=CARTESIAN_POINT('Ctrl Pts',(-23.2653254117304,26.7604100093648,-55.5223885553856));
#15477=CARTESIAN_POINT('Ctrl Pts',(-23.2484387764477,26.7588409127376,-55.5234478805438));
#15478=CARTESIAN_POINT('Ctrl Pts',(-23.2447972471421,26.7584962897772,-55.5236760106748));
#15479=CARTESIAN_POINT('Ctrl Pts',(-23.2390142378174,26.7579390684238,-55.5240377987019));
#15480=CARTESIAN_POINT('Ctrl Pts',(-23.2368723843756,26.7577305248881,-55.5241716854019));
#15481=CARTESIAN_POINT('Ctrl Pts',(-23.2328732516013,26.7573371016268,-55.5244214650139));
#15482=CARTESIAN_POINT('Ctrl Pts',(-23.2310159363426,26.757152755017,-55.5245373871528));
#15483=CARTESIAN_POINT('Ctrl Pts',(-23.2268515496233,26.7567357678768,-55.5247971173852));
#15484=CARTESIAN_POINT('Ctrl Pts',(-23.2245445735581,26.7565022514155,-55.5249408749225));
#15485=CARTESIAN_POINT('Ctrl Pts',(-23.2177326041151,26.7558053030435,-55.5253649876561));
#15486=CARTESIAN_POINT('Ctrl Pts',(-23.2132283093705,26.7553348623535,-55.5256449464931));
#15487=CARTESIAN_POINT('Ctrl Pts',(-23.1782818843785,26.7516104793563,-55.5278133898286));
#15488=CARTESIAN_POINT('Ctrl Pts',(-23.1478852001811,26.747932248123,-55.5296782664915));
#15489=CARTESIAN_POINT('Ctrl Pts',(-23.0430531268668,26.7337281666625,-55.536050570907));
#15490=CARTESIAN_POINT('Ctrl Pts',(-22.9689319669206,26.721031068864,-55.5404526587042));
#15491=CARTESIAN_POINT('Ctrl Pts',(-22.6095691825573,26.646444034771,-55.5615807370014));
#15492=CARTESIAN_POINT('Ctrl Pts',(-22.3336753044659,26.5486994933522,-55.5772652750174));
#15493=CARTESIAN_POINT('Ctrl Pts',(-22.0750357439016,26.4155366348007,-55.5940940905011));
#15494=CARTESIAN_POINT('',(-26.7730018345793,23.5523722612815,-55.4357734493122));
#15495=CARTESIAN_POINT('Ctrl Pts',(-22.0750360153461,26.4155367745563,-55.8427674868566));
#15496=CARTESIAN_POINT('Ctrl Pts',(-22.1638033690836,26.4612394187782,-55.8366160816763));
#15497=CARTESIAN_POINT('Ctrl Pts',(-22.2547513529059,26.5028413659955,-55.830464676496));
#15498=CARTESIAN_POINT('Ctrl Pts',(-22.3474633730655,26.5401381151882,-55.8243132713157));
#15499=CARTESIAN_POINT('Ctrl Pts',(-22.4401518048246,26.5774253750973,-55.8181634312162));
#15500=CARTESIAN_POINT('Ctrl Pts',(-22.5346029781623,26.6104094517274,-55.8120135911168));
#15501=CARTESIAN_POINT('Ctrl Pts',(-22.6303797647384,26.6389337478629,-55.8058637510173));
#15502=CARTESIAN_POINT('Ctrl Pts',(-22.7261578061745,26.6674584177214,-55.7997138303432));
#15503=CARTESIAN_POINT('Ctrl Pts',(-22.8232610787732,26.6915230675885,-55.793563909669));
#15504=CARTESIAN_POINT('Ctrl Pts',(-22.9212376924382,26.7110210924237,-55.7874139889948));
#15505=CARTESIAN_POINT('Ctrl Pts',(-23.0192418011187,26.7305245889574,-55.7812623424786));
#15506=CARTESIAN_POINT('Ctrl Pts',(-23.1181193118339,26.7454588295939,-55.7751106959623));
#15507=CARTESIAN_POINT('Ctrl Pts',(-23.217409555345,26.7557685768256,-55.7689590494461));
#15508=CARTESIAN_POINT('Ctrl Pts',(-23.3168125741409,26.7660900340164,-55.7628004158013));
#15509=CARTESIAN_POINT('Ctrl Pts',(-23.416628828747,26.7717764704703,-55.7566417821566));
#15510=CARTESIAN_POINT('Ctrl Pts',(-23.51639415779,26.7728246678948,-55.7504831485119));
#15511=CARTESIAN_POINT('Ctrl Pts',(-23.6162263079814,26.7738735673844,-55.7443203899173));
#15512=CARTESIAN_POINT('Ctrl Pts',(-23.7160070313591,26.7702780593493,-55.7381576313228));
#15513=CARTESIAN_POINT('Ctrl Pts',(-23.8152758372828,26.7620869312227,-55.7319948727283));
#15514=CARTESIAN_POINT('Ctrl Pts',(-23.9146972370149,26.7538832118756,-55.7258226408778));
#15515=CARTESIAN_POINT('Ctrl Pts',(-24.0136047194735,26.7410698307426,-55.7196504090274));
#15516=CARTESIAN_POINT('Ctrl Pts',(-24.1115467365093,26.7237468799074,-55.7134781771769));
#15517=CARTESIAN_POINT('Ctrl Pts',(-24.1406837651828,26.7185934296266,-55.7116419836632));
#15518=CARTESIAN_POINT('Ctrl Pts',(-24.1697354460884,26.7130412109727,-55.7098057901494));
#15519=CARTESIAN_POINT('Ctrl Pts',(-24.1986901638857,26.7070937059787,-55.7079695966356));
#15520=CARTESIAN_POINT('Ctrl Pts',(-24.2960171399522,26.6871020527961,-55.7017975053233));
#15521=CARTESIAN_POINT('Ctrl Pts',(-24.3925901342158,26.6625700144652,-55.695625414011));
#15522=CARTESIAN_POINT('Ctrl Pts',(-24.487953024853,26.6335681736014,-55.6894533226986));
#15523=CARTESIAN_POINT('Ctrl Pts',(-24.5831867082013,26.6046056273647,-55.6832895939598));
#15524=CARTESIAN_POINT('Ctrl Pts',(-24.6772131348009,26.5711854410995,-55.6771258652211));
#15525=CARTESIAN_POINT('Ctrl Pts',(-24.7695860322198,26.533429257434,-55.6709621364823));
#15526=CARTESIAN_POINT('Ctrl Pts',(-24.8618610692233,26.4957130729017,-55.6648049376356));
#15527=CARTESIAN_POINT('Ctrl Pts',(-24.9524856598126,26.4536701868769,-55.6586477387889));
#15528=CARTESIAN_POINT('Ctrl Pts',(-25.0410293012036,26.4074718417912,-55.6524905399422));
#15529=CARTESIAN_POINT('Ctrl Pts',(-25.1295082225622,26.3613072648941,-55.6463378416345));
#15530=CARTESIAN_POINT('Ctrl Pts',(-25.2159088348528,26.3109934681144,-55.6401851433268));
#15531=CARTESIAN_POINT('Ctrl Pts',(-25.299822068589,26.2567491598225,-55.6340324450191));
#15532=CARTESIAN_POINT('Ctrl Pts',(-25.3837034823076,26.2025254210495,-55.6278820798234));
#15533=CARTESIAN_POINT('Ctrl Pts',(-25.465099027226,26.1443743678503,-55.6217317146276));
#15534=CARTESIAN_POINT('Ctrl Pts',(-25.5436264153047,26.0825594093533,-55.6155813494319));
#15535=CARTESIAN_POINT('Ctrl Pts',(-25.6221450340732,26.0207513538561,-55.6094316710597));
#15536=CARTESIAN_POINT('Ctrl Pts',(-25.6977957914518,25.9552804752095,-55.6032819926875));
#15537=CARTESIAN_POINT('Ctrl Pts',(-25.7702282607602,25.886451436937,-55.5971323143153));
#15538=CARTESIAN_POINT('Ctrl Pts',(-25.8426720190566,25.8176116712906,-55.5909816774828));
#15539=CARTESIAN_POINT('Ctrl Pts',(-25.9118961780703,25.7454130057018,-55.5848310406503));
#15540=CARTESIAN_POINT('Ctrl Pts',(-25.9775867989288,25.6701973228642,-55.5786804038178));
#15541=CARTESIAN_POINT('Ctrl Pts',(-26.0433476949519,25.5949011750466,-55.572523187096));
#15542=CARTESIAN_POINT('Ctrl Pts',(-26.1055672179356,25.5165818926573,-55.5663659703742));
#15543=CARTESIAN_POINT('Ctrl Pts',(-26.1639715048073,25.4356147494361,-55.5602087536524));
#15544=CARTESIAN_POINT('Ctrl Pts',(-26.2224083751914,25.3546024349773,-55.5540481018446));
#15545=CARTESIAN_POINT('Ctrl Pts',(-26.2770255331043,25.2709396815692,-55.5478874500368));
#15546=CARTESIAN_POINT('Ctrl Pts',(-26.3275934335353,25.1850292985527,-55.541726798229));
#15547=CARTESIAN_POINT('Ctrl Pts',(-26.3782459520459,25.0989751569153,-55.53555583746));
#15548=CARTESIAN_POINT('Ctrl Pts',(-26.4248354756847,25.0106662573898,-55.5293848766909));
#15549=CARTESIAN_POINT('Ctrl Pts',(-26.4671791846668,24.9205285855162,-55.5232139159219));
#15550=CARTESIAN_POINT('Ctrl Pts',(-26.4995009327744,24.8517248081585,-55.5185035057015));
#15551=CARTESIAN_POINT('Ctrl Pts',(-26.5293497993277,24.7818559668027,-55.5137930954811));
#15552=CARTESIAN_POINT('Ctrl Pts',(-26.5566640073031,24.7111175547814,-55.5090826852607));
#15553=CARTESIAN_POINT('Ctrl Pts',(-26.5974036268661,24.6056099743735,-55.5020570259212));
#15554=CARTESIAN_POINT('Ctrl Pts',(-26.6326230710418,24.4978581799752,-55.4950313665816));
#15555=CARTESIAN_POINT('Ctrl Pts',(-26.6621013805474,24.388413795647,-55.4880057072421));
#15556=CARTESIAN_POINT('Ctrl Pts',(-26.6914692696457,24.279379370156,-55.4810063647497));
#15557=CARTESIAN_POINT('Ctrl Pts',(-26.715138833174,24.1686651889649,-55.4740070222573));
#15558=CARTESIAN_POINT('Ctrl Pts',(-26.7329381736759,24.056838819333,-55.4670076797649));
#15559=CARTESIAN_POINT('Ctrl Pts',(-26.7506182001143,23.9457620537979,-55.4600552558645));
#15560=CARTESIAN_POINT('Ctrl Pts',(-26.7625063383809,23.8335881540695,-55.4531028319641));
#15561=CARTESIAN_POINT('Ctrl Pts',(-26.7684817941327,23.7208924358339,-55.4461504080637));
#15562=CARTESIAN_POINT('Ctrl Pts',(-26.7714547168977,23.664823797694,-55.4426914218132));
#15563=CARTESIAN_POINT('Ctrl Pts',(-26.7729648340919,23.6086262739736,-55.4392324355627));
#15564=CARTESIAN_POINT('Ctrl Pts',(-26.7730018345793,23.5523722612815,-55.4357734493122));
#15565=CARTESIAN_POINT('Ctrl Pts',(-26.7730019166452,23.5522435862346,-55.438005776981));
#15566=CARTESIAN_POINT('Ctrl Pts',(-26.7730788414302,23.4277320278056,-55.4308287226616));
#15567=CARTESIAN_POINT('Ctrl Pts',(-26.7659400990873,23.3033318469675,-55.4234862517857));
#15568=CARTESIAN_POINT('Ctrl Pts',(-26.7508314924961,23.1728145698253,-55.4154867208764));
#15569=CARTESIAN_POINT('Ctrl Pts',(-26.7500166883877,23.1659682101737,-55.4150662542082));
#15570=CARTESIAN_POINT('Ctrl Pts',(-26.7486509437576,23.1547981629762,-55.4143788482534));
#15571=CARTESIAN_POINT('Ctrl Pts',(-26.7481131876054,23.1504728609894,-55.4141123253738));
#15572=CARTESIAN_POINT('Ctrl Pts',(-26.7471500005202,23.142852018815,-55.4136421228204));
#15573=CARTESIAN_POINT('Ctrl Pts',(-26.7467282432011,23.1395560139398,-55.413438559509));
#15574=CARTESIAN_POINT('Ctrl Pts',(-26.745891205554,23.1330940191292,-55.4130390655293));
#15575=CARTESIAN_POINT('Ctrl Pts',(-26.7454763158846,23.1299279817351,-55.4128431474389));
#15576=CARTESIAN_POINT('Ctrl Pts',(-26.744642350688,23.123636556246,-55.4124534527456));
#15577=CARTESIAN_POINT('Ctrl Pts',(-26.7442233919184,23.1205111558416,-55.4122596800337));
#15578=CARTESIAN_POINT('Ctrl Pts',(-26.7432253087054,23.1131476186655,-55.4118027108634));
#15579=CARTESIAN_POINT('Ctrl Pts',(-26.74264233314,23.1089100172242,-55.4115393925674));
#15580=CARTESIAN_POINT('Ctrl Pts',(-26.7408948269966,23.0963921736642,-55.4107605415615));
#15581=CARTESIAN_POINT('Ctrl Pts',(-26.7397065119313,23.0881153366979,-55.410244255322));
#15582=CARTESIAN_POINT('Ctrl Pts',(-26.7289578143729,23.0152652444207,-55.4056884032595));
#15583=CARTESIAN_POINT('Ctrl Pts',(-26.717470397897,22.9509957819651,-55.401587917036));
#15584=CARTESIAN_POINT('Ctrl Pts',(-26.6997575563654,22.8667550128291,-55.3960997077482));
#15585=CARTESIAN_POINT('Ctrl Pts',(-26.695277759821,22.8464293710084,-55.3947667477626));
#15586=CARTESIAN_POINT('Ctrl Pts',(-26.6849237527349,22.8015253070283,-55.391802443156));
#15587=CARTESIAN_POINT('Ctrl Pts',(-26.6789567359544,22.7769698737841,-55.3901684302526));
#15588=CARTESIAN_POINT('Ctrl Pts',(-26.6680249324779,22.7341828297895,-55.3872985689068));
#15589=CARTESIAN_POINT('Ctrl Pts',(-26.6631873696385,22.7159197595268,-55.3860663444757));
#15590=CARTESIAN_POINT('Ctrl Pts',(-26.5856074258991,22.4331058238264,-55.3668729393034));
#15591=CARTESIAN_POINT('Ctrl Pts',(-26.4795321946045,22.1788719186732,-55.3479602111803));
#15592=CARTESIAN_POINT('Ctrl Pts',(-26.2942602041791,21.8573546179912,-55.3232728031932));
#15593=CARTESIAN_POINT('Ctrl Pts',(-26.2421890534913,21.7757206945836,-55.3169438300984));
#15594=CARTESIAN_POINT('Ctrl Pts',(-26.1814052385875,21.689276448931,-55.3102736863033));
#15595=CARTESIAN_POINT('Ctrl Pts',(-26.1762631643443,21.6820275160331,-55.3097146123015));
#15596=CARTESIAN_POINT('Ctrl Pts',(-26.1673443991041,21.6695640483446,-55.3087539526943));
#15597=CARTESIAN_POINT('Ctrl Pts',(-26.1635819791007,21.6643394332487,-55.3083514283213));
#15598=CARTESIAN_POINT('Ctrl Pts',(-26.1582326197687,21.6569578920223,-55.307783020954));
#15599=CARTESIAN_POINT('Ctrl Pts',(-26.1566586420436,21.6547916588555,-55.3076162486798));
#15600=CARTESIAN_POINT('Ctrl Pts',(-26.1539526610715,21.6510772166947,-55.3073303497236));
#15601=CARTESIAN_POINT('Ctrl Pts',(-26.1528219740959,21.6495280544568,-55.307211131046));
#15602=CARTESIAN_POINT('Ctrl Pts',(-26.1506569128562,21.6465672426875,-55.3069833152429));
#15603=CARTESIAN_POINT('Ctrl Pts',(-26.1496227730291,21.6451554282253,-55.3068747018983));
#15604=CARTESIAN_POINT('Ctrl Pts',(-26.1471899790904,21.6418398306759,-55.3066196650804));
#15605=CARTESIAN_POINT('Ctrl Pts',(-26.1457903783541,21.6399367384976,-55.3064733080106));
#15606=CARTESIAN_POINT('Ctrl Pts',(-26.1416681916828,21.6343445324399,-55.3060433209981));
#15607=CARTESIAN_POINT('Ctrl Pts',(-26.1389398095142,21.6306596679055,-55.3057600939712));
#15608=CARTESIAN_POINT('Ctrl Pts',(-26.1157714543348,21.5995084660861,-55.3033665040913));
#15609=CARTESIAN_POINT('Ctrl Pts',(-26.09490186822,21.5723623083113,-55.3012856774986));
#15610=CARTESIAN_POINT('Ctrl Pts',(-25.8790297762686,21.3006404161083,-55.2804504389529));
#15611=CARTESIAN_POINT('Ctrl Pts',(-25.649810790791,21.0853229235165,-55.2637472765753));
#15612=CARTESIAN_POINT('Ctrl Pts',(-25.325451797575,20.8592325712338,-55.2412600523618));
#15613=CARTESIAN_POINT('Ctrl Pts',(-25.2560038534857,20.8146845938912,-55.2365120392474));
#15614=CARTESIAN_POINT('Ctrl Pts',(-25.1366330269504,20.744427393235,-55.2283898372857));
#15615=CARTESIAN_POINT('Ctrl Pts',(-25.0876083371197,20.7172692358729,-55.2250648372415));
#15616=CARTESIAN_POINT('Ctrl Pts',(-25.020036635349,20.6821071592685,-55.2204834114644));
#15617=CARTESIAN_POINT('Ctrl Pts',(-25.0020841894197,20.6729781272969,-55.2192663863316));
#15618=CARTESIAN_POINT('Ctrl Pts',(-24.9715769729359,20.6578230524914,-55.2171979544852));
#15619=CARTESIAN_POINT('Ctrl Pts',(-24.9590664202684,20.6517089530563,-55.2163496386054));
#15620=CARTESIAN_POINT('Ctrl Pts',(-24.9418555921775,20.6434355040831,-55.2151823570006));
#15621=CARTESIAN_POINT('Ctrl Pts',(-24.9371890303002,20.6412060455931,-55.2148658341642));
#15622=CARTESIAN_POINT('Ctrl Pts',(-24.9296874494974,20.6376443049841,-55.2143569707075));
#15623=CARTESIAN_POINT('Ctrl Pts',(-24.9268558061352,20.6363049001396,-55.2141648777375));
#15624=CARTESIAN_POINT('Ctrl Pts',(-24.9209575027179,20.6335254407412,-55.2137647241773));
#15625=CARTESIAN_POINT('Ctrl Pts',(-24.9178905169802,20.632086089945,-55.2135566394893));
#15626=CARTESIAN_POINT('Ctrl Pts',(-24.9108376711355,20.6287897171977,-55.2130780930953));
#15627=CARTESIAN_POINT('Ctrl Pts',(-24.9068502751516,20.6269360143984,-55.2128075169102));
#15628=CARTESIAN_POINT('Ctrl Pts',(-24.8942052560412,20.6210889071935,-55.2119493648231));
#15629=CARTESIAN_POINT('Ctrl Pts',(-24.8855337592681,20.6171257863025,-55.2113607444296));
#15630=CARTESIAN_POINT('Ctrl Pts',(-24.8527804738253,20.6023319494138,-55.2091368715181));
#15631=CARTESIAN_POINT('Ctrl Pts',(-24.8285839942945,20.5917590968131,-55.2074927910047));
#15632=CARTESIAN_POINT('Ctrl Pts',(-24.7971014803647,20.5784608727237,-55.20535157885));
#15633=CARTESIAN_POINT('Ctrl Pts',(-24.7899312013358,20.5754626635764,-55.2048637719002));
#15634=CARTESIAN_POINT('Ctrl Pts',(-24.7789259015754,20.5709075628481,-55.2041148405568));
#15635=CARTESIAN_POINT('Ctrl Pts',(-24.7750985743412,20.5693320589545,-55.2038543429142));
#15636=CARTESIAN_POINT('Ctrl Pts',(-24.7680463882286,20.5664449297232,-55.203374276119));
#15637=CARTESIAN_POINT('Ctrl Pts',(-24.7648224144842,20.5651311468491,-55.2031547794513));
#15638=CARTESIAN_POINT('Ctrl Pts',(-24.7595673307763,20.5629996007606,-55.2027969503533));
#15639=CARTESIAN_POINT('Ctrl Pts',(-24.7575374989892,20.5621786764564,-55.20265872316));
#15640=CARTESIAN_POINT('Ctrl Pts',(-24.743198041339,20.556396370184,-55.2016821518189));
#15641=CARTESIAN_POINT('Ctrl Pts',(-24.7308588531329,20.551509059811,-55.2008413634327));
#15642=CARTESIAN_POINT('Ctrl Pts',(-24.7147835250829,20.5452565343593,-55.199745390408));
#15643=CARTESIAN_POINT('Ctrl Pts',(-24.7110744237798,20.5438217719408,-55.1994924721166));
#15644=CARTESIAN_POINT('Ctrl Pts',(-24.7027207497376,20.5406081498196,-55.1989227523591));
#15645=CARTESIAN_POINT('Ctrl Pts',(-24.6980747031955,20.538833171804,-55.1986058266526));
#15646=CARTESIAN_POINT('Ctrl Pts',(-24.6791161845141,20.5316404972538,-55.1973123181178));
#15647=CARTESIAN_POINT('Ctrl Pts',(-24.6647694935682,20.5263140914803,-55.1963328369763));
#15648=CARTESIAN_POINT('Ctrl Pts',(-24.6273075325131,20.5127086333113,-55.193773561933));
#15649=CARTESIAN_POINT('Ctrl Pts',(-24.6041349315619,20.5045913150729,-55.1921888434871));
#15650=CARTESIAN_POINT('Ctrl Pts',(-24.4174790607513,20.4415913390572,-55.179411192005));
#15651=CARTESIAN_POINT('Ctrl Pts',(-24.2499410037847,20.399652636781,-55.1678420258864));
#15652=CARTESIAN_POINT('Ctrl Pts',(-24.0607885016073,20.3681392566168,-55.1548685802093));
#15653=CARTESIAN_POINT('Ctrl Pts',(-24.0416762435035,20.3651317167911,-55.1535589881339));
#15654=CARTESIAN_POINT('Ctrl Pts',(-23.9268993234158,20.3481278808895,-55.1457046768733));
#15655=CARTESIAN_POINT('Ctrl Pts',(-23.8306686681147,20.3382698197236,-55.1391606584033));
#15656=CARTESIAN_POINT('Ctrl Pts',(-23.6494306216396,20.3279117581735,-55.1270460491798));
#15657=CARTESIAN_POINT('Ctrl Pts',(-23.564557504351,20.3264172141409,-55.1214593357059));
#15658=CARTESIAN_POINT('Ctrl Pts',(-23.4467437362076,20.3289963633774,-55.1139078212282));
#15659=CARTESIAN_POINT('Ctrl Pts',(-23.4137810692429,20.3302244070553,-55.1118172578896));
#15660=CARTESIAN_POINT('Ctrl Pts',(-23.3762373694884,20.3322007075804,-55.1094659224595));
#15661=CARTESIAN_POINT('Ctrl Pts',(-23.3716337189843,20.3324529512764,-55.1091781098905));
#15662=CARTESIAN_POINT('Ctrl Pts',(-23.3646986244983,20.3328478686577,-55.1087453251952));
#15663=CARTESIAN_POINT('Ctrl Pts',(-23.3623667935396,20.3329831976648,-55.1085999411309));
#15664=CARTESIAN_POINT('Ctrl Pts',(-23.3583477335912,20.3332208302443,-55.1083495955966));
#15665=CARTESIAN_POINT('Ctrl Pts',(-23.3566604400101,20.3333219260148,-55.1082445657382));
#15666=CARTESIAN_POINT('Ctrl Pts',(-23.3531569874141,20.3335346050236,-55.1080266322967));
#15667=CARTESIAN_POINT('Ctrl Pts',(-23.3513408481613,20.3336463985887,-55.1079137410367));
#15668=CARTESIAN_POINT('Ctrl Pts',(-23.3463618634332,20.3339571159993,-55.1076044704728));
#15669=CARTESIAN_POINT('Ctrl Pts',(-23.3431992043127,20.3341591677743,-55.107408268326));
#15670=CARTESIAN_POINT('Ctrl Pts',(-23.3310706699407,20.3349519843805,-55.1066567793178));
#15671=CARTESIAN_POINT('Ctrl Pts',(-23.3221068720183,20.3355755867138,-55.1061033279163));
#15672=CARTESIAN_POINT('Ctrl Pts',(-23.3053437686649,20.3368122473116,-55.1050717762917));
#15673=CARTESIAN_POINT('Ctrl Pts',(-23.2975438939927,20.3374162285512,-55.1045931943316));
#15674=CARTESIAN_POINT('Ctrl Pts',(-23.0075361621405,20.3609355476323,-55.086848490599));
#15675=CARTESIAN_POINT('Ctrl Pts',(-22.7295198439185,20.4209168937968,-55.0715056784077));
#15676=CARTESIAN_POINT('Ctrl Pts',(-22.3450008906723,20.55873645097,-55.0485540163455));
#15677=CARTESIAN_POINT('Ctrl Pts',(-22.2296855437849,20.6078217223761,-55.0414392860695));
#15678=CARTESIAN_POINT('Ctrl Pts',(-22.0626634456669,20.6907162988059,-55.0305404699118));
#15679=CARTESIAN_POINT('Ctrl Pts',(-22.0085919303924,20.7195016364711,-55.0269150355831));
#15680=CARTESIAN_POINT('Ctrl Pts',(-21.9366758121197,20.7604584821626,-55.021942909467));
#15681=CARTESIAN_POINT('Ctrl Pts',(-21.9180833534373,20.7712950998397,-55.0206435580063));
#15682=CARTESIAN_POINT('Ctrl Pts',(-21.891112836644,20.7873788990309,-55.0187376671126));
#15683=CARTESIAN_POINT('Ctrl Pts',(-21.8826479233375,20.7924798607604,-55.0181364308397));
#15684=CARTESIAN_POINT('Ctrl Pts',(-21.867512123065,20.8016958718324,-55.0170558206725));
#15685=CARTESIAN_POINT('Ctrl Pts',(-21.8608325058726,20.8057964890609,-55.0165769776159));
#15686=CARTESIAN_POINT('Ctrl Pts',(-21.8506952527969,20.8120707813777,-55.0158472585343));
#15687=CARTESIAN_POINT('Ctrl Pts',(-21.8472266470128,20.8142267500391,-55.0155970366446));
#15688=CARTESIAN_POINT('Ctrl Pts',(-21.8409635569935,20.818136200474,-55.0151442453898));
#15689=CARTESIAN_POINT('Ctrl Pts',(-21.8381676449661,20.8198873936839,-55.0149417609927));
#15690=CARTESIAN_POINT('Ctrl Pts',(-21.8321688661262,20.8236575095015,-55.0145065577025));
#15691=CARTESIAN_POINT('Ctrl Pts',(-21.8289668608311,20.8256777876243,-55.0142737886808));
#15692=CARTESIAN_POINT('Ctrl Pts',(-21.8203784771757,20.8311177381768,-55.0136481959883));
#15693=CARTESIAN_POINT('Ctrl Pts',(-21.8149987020533,20.8345477584185,-55.0132549874915));
#15694=CARTESIAN_POINT('Ctrl Pts',(-21.7915675492942,20.8495849707157,-55.0115365259029));
#15695=CARTESIAN_POINT('Ctrl Pts',(-21.7736225171508,20.8613561227983,-55.0102051526829));
#15696=CARTESIAN_POINT('Ctrl Pts',(-21.744969228358,20.8805634727127,-55.0080542241215));
#15697=CARTESIAN_POINT('Ctrl Pts',(-21.7341859906707,20.8878870820493,-55.0072389579501));
#15698=CARTESIAN_POINT('Ctrl Pts',(-21.7185770004402,20.8986271311568,-55.0060503200258));
#15699=CARTESIAN_POINT('Ctrl Pts',(-21.7137156524232,20.9019918181511,-55.0056789133326));
#15700=CARTESIAN_POINT('Ctrl Pts',(-21.7030002596851,20.9094519620394,-55.0048575714395));
#15701=CARTESIAN_POINT('Ctrl Pts',(-21.6971505316691,20.9135535383859,-55.0044074060597));
#15702=CARTESIAN_POINT('Ctrl Pts',(-21.6856533002675,20.9216720595383,-55.0035191129067));
#15703=CARTESIAN_POINT('Ctrl Pts',(-21.6800050176504,20.9256878387504,-55.0030810307344));
#15704=CARTESIAN_POINT('Ctrl Pts',(-21.6611914792114,20.9391553366922,-55.0016161886175));
#15705=CARTESIAN_POINT('Ctrl Pts',(-21.64808473415,20.9486880261494,-55.0005863898564));
#15706=CARTESIAN_POINT('Ctrl Pts',(-21.6216822609435,20.9681970400879,-54.9984929476786));
#15707=CARTESIAN_POINT('Ctrl Pts',(-21.6083907074072,20.9781781761958,-54.9974291452662));
#15708=CARTESIAN_POINT('Ctrl Pts',(-21.3723110804667,21.1583323876443,-54.9783558075725));
#15709=CARTESIAN_POINT('Ctrl Pts',(-21.1726161808175,21.356738432022,-54.9592074660605));
#15710=CARTESIAN_POINT('Ctrl Pts',(-20.978265687732,21.6079859767994,-54.9378351084374));
#15711=CARTESIAN_POINT('Ctrl Pts',(-20.9559035422299,21.6379583238226,-54.9353285745684));
#15712=CARTESIAN_POINT('Ctrl Pts',(-20.8694592131209,21.758129256705,-54.9254651651377));
#15713=CARTESIAN_POINT('Ctrl Pts',(-20.8095104187599,21.8512241639307,-54.9182290018173));
#15714=CARTESIAN_POINT('Ctrl Pts',(-20.7514261501566,21.9525273542276,-54.9109121477205));
#15715=CARTESIAN_POINT('Ctrl Pts',(-20.7484035626668,21.9578338640952,-54.9105304383355));
#15716=CARTESIAN_POINT('Ctrl Pts',(-20.7441054943487,21.9654297546196,-54.9099863177446));
#15717=CARTESIAN_POINT('Ctrl Pts',(-20.7428177177453,21.9677121070976,-54.9098231166405));
#15718=CARTESIAN_POINT('Ctrl Pts',(-20.7405974376398,21.9716583935015,-54.9095414422922));
#15719=CARTESIAN_POINT('Ctrl Pts',(-20.73966362619,21.973321586785,-54.9094228839347));
#15720=CARTESIAN_POINT('Ctrl Pts',(-20.7378696967476,21.9765233748084,-54.909194949417));
#15721=CARTESIAN_POINT('Ctrl Pts',(-20.7370093661627,21.9780618431444,-54.9090855593253));
#15722=CARTESIAN_POINT('Ctrl Pts',(-20.7349748691037,21.9817070073866,-54.9088266895198));
#15723=CARTESIAN_POINT('Ctrl Pts',(-20.7338018024313,21.9838143206466,-54.9086772812481));
#15724=CARTESIAN_POINT('Ctrl Pts',(-20.7303118502431,21.9901003132188,-54.9082323363515));
#15725=CARTESIAN_POINT('Ctrl Pts',(-20.7280018776429,21.9942828539311,-54.9079372433761));
#15726=CARTESIAN_POINT('Ctrl Pts',(-20.7066955065813,22.0330646798854,-54.9052098029002));
#15727=CARTESIAN_POINT('Ctrl Pts',(-20.6883259044694,22.0680069855144,-54.9028168116254));
#15728=CARTESIAN_POINT('Ctrl Pts',(-20.5825806803053,22.2784527723303,-54.8887324896534));
#15729=CARTESIAN_POINT('Ctrl Pts',(-20.5107153530718,22.4613153426098,-54.8778204621623));
#15730=CARTESIAN_POINT('Ctrl Pts',(-20.4129187962472,22.7973099613299,-54.8582677154784));
#15731=CARTESIAN_POINT('Ctrl Pts',(-20.3805583395989,22.9479069034931,-54.8496707300012));
#15732=CARTESIAN_POINT('Ctrl Pts',(-20.3475600247115,23.1819031022879,-54.8360330787821));
#15733=CARTESIAN_POINT('Ctrl Pts',(-20.3391829023584,23.2639820096189,-54.8312000775601));
#15734=CARTESIAN_POINT('Ctrl Pts',(-20.3321951690406,23.3741702855651,-54.8245998753853));
#15735=CARTESIAN_POINT('Ctrl Pts',(-20.3307896423446,23.4020743386149,-54.8229189802117));
#15736=CARTESIAN_POINT('Ctrl Pts',(-20.3292992981187,23.4419850335803,-54.8204999105333));
#15737=CARTESIAN_POINT('Ctrl Pts',(-20.3289184681319,23.4539798517247,-54.8197709581643));
#15738=CARTESIAN_POINT('Ctrl Pts',(-20.3283645248389,23.4751555991665,-54.8184805507042));
#15739=CARTESIAN_POINT('Ctrl Pts',(-20.328163636515,23.4843357143486,-54.8179199693434));
#15740=CARTESIAN_POINT('Ctrl Pts',(-20.3279252395536,23.4978751629369,-54.8170914302833));
#15741=CARTESIAN_POINT('Ctrl Pts',(-20.3278573380519,23.5022339714565,-54.8168244270591));
#15742=CARTESIAN_POINT('Ctrl Pts',(-20.327754862315,23.5097975551617,-54.816360641702));
#15743=CARTESIAN_POINT('Ctrl Pts',(-20.3277162242714,23.5130022766352,-54.8161639874212));
#15744=CARTESIAN_POINT('Ctrl Pts',(-20.3276488624914,23.5193783945405,-54.8157724302156));
#15745=CARTESIAN_POINT('Ctrl Pts',(-20.3276200396307,23.5225497866913,-54.8155775306142));
#15746=CARTESIAN_POINT('Ctrl Pts',(-20.3275628006328,23.5300692189667,-54.8151150749233));
#15747=CARTESIAN_POINT('Ctrl Pts',(-20.3275385026174,23.5344172765624,-54.8148473897773));
#15748=CARTESIAN_POINT('Ctrl Pts',(-20.3274840371801,23.5496975630152,-54.8139056999258));
#15749=CARTESIAN_POINT('Ctrl Pts',(-20.3275006974699,23.5606297901022,-54.8132302267463));
#15750=CARTESIAN_POINT('Ctrl Pts',(-20.3284576747963,23.705358280467,-54.8042642712462));
#15751=CARTESIAN_POINT('Ctrl Pts',(-20.3376734622503,23.8389516442154,-54.7957129714449));
#15752=CARTESIAN_POINT('Ctrl Pts',(-20.3718405376574,24.0980590909349,-54.7785697743708));
#15753=CARTESIAN_POINT('Ctrl Pts',(-20.3960147901411,24.2234348499318,-54.7700139510418));
#15754=CARTESIAN_POINT('Ctrl Pts',(-20.4660134089959,24.4977676994828,-54.7508803302058));
#15755=CARTESIAN_POINT('Ctrl Pts',(-20.5153371595481,24.6455186445221,-54.7402921100955));
#15756=CARTESIAN_POINT('Ctrl Pts',(-20.6001468968037,24.8491851104599,-54.7256985386063));
#15757=CARTESIAN_POINT('Ctrl Pts',(-20.6269677103267,24.908470551591,-54.7214525293368));
#15758=CARTESIAN_POINT('Ctrl Pts',(-20.6680102227588,24.9923337262186,-54.7154891998209));
#15759=CARTESIAN_POINT('Ctrl Pts',(-20.6807887905279,25.0175960062414,-54.7136986383152));
#15760=CARTESIAN_POINT('Ctrl Pts',(-20.6959557888364,25.0466239396076,-54.7116507374985));
#15761=CARTESIAN_POINT('Ctrl Pts',(-20.6980206272203,25.0505559844579,-54.7113735394475));
#15762=CARTESIAN_POINT('Ctrl Pts',(-20.7011674003905,25.0565183680227,-54.710953534378));
#15763=CARTESIAN_POINT('Ctrl Pts',(-20.7022433811847,25.0585518169158,-54.7108103509092));
#15764=CARTESIAN_POINT('Ctrl Pts',(-20.7041957375733,25.0622319517613,-54.7105513245167));
#15765=CARTESIAN_POINT('Ctrl Pts',(-20.7050713627572,25.0638790239467,-54.7104354343239));
#15766=CARTESIAN_POINT('Ctrl Pts',(-20.7068339756456,25.0671876077352,-54.7102027166283));
#15767=CARTESIAN_POINT('Ctrl Pts',(-20.7077209862553,25.0688490953128,-54.7100858913388));
#15768=CARTESIAN_POINT('Ctrl Pts',(-20.7102540255229,25.0735838159427,-54.7097530862078));
#15769=CARTESIAN_POINT('Ctrl Pts',(-20.7119035916056,25.0766551690073,-54.7095373325529));
#15770=CARTESIAN_POINT('Ctrl Pts',(-20.7189650859787,25.089752048371,-54.7086178559576));
#15771=CARTESIAN_POINT('Ctrl Pts',(-20.7244252588212,25.0997516750192,-54.7079171798722));
#15772=CARTESIAN_POINT('Ctrl Pts',(-20.8201882261588,25.2729397993269,-54.6958017608508));
#15773=CARTESIAN_POINT('Ctrl Pts',(-20.9244517948233,25.4280425295136,-54.685249744017));
#15774=CARTESIAN_POINT('Ctrl Pts',(-21.2331744594496,25.8108804368285,-54.6576948031303));
#15775=CARTESIAN_POINT('Ctrl Pts',(-21.4575347825304,26.0200296116876,-54.6408473440662));
#15776=CARTESIAN_POINT('Ctrl Pts',(-21.7178504478405,26.2013967572225,-54.6216316628998));
#15777=CARTESIAN_POINT('Ctrl Pts',(-21.7277873911295,26.2082374651995,-54.6208989126937));
#15778=CARTESIAN_POINT('Ctrl Pts',(-21.7430999128358,26.2186525473302,-54.6197708305971));
#15779=CARTESIAN_POINT('Ctrl Pts',(-21.7484482851394,26.2222668818498,-54.6193770106708));
#15780=CARTESIAN_POINT('Ctrl Pts',(-21.7584021042008,26.2289500203174,-54.6186444236135));
#15781=CARTESIAN_POINT('Ctrl Pts',(-21.7630046743468,26.2320230822573,-54.6183058185895));
#15782=CARTESIAN_POINT('Ctrl Pts',(-21.7705852196155,26.2370563078044,-54.6177483443471));
#15783=CARTESIAN_POINT('Ctrl Pts',(-21.7735585853912,26.2390234207827,-54.6175297372139));
#15784=CARTESIAN_POINT('Ctrl Pts',(-21.7793642908342,26.2428505118196,-54.6171029948586));
#15785=CARTESIAN_POINT('Ctrl Pts',(-21.7821963127549,26.2447109653543,-54.6168948778723));
#15786=CARTESIAN_POINT('Ctrl Pts',(-21.788712923064,26.2489772553388,-54.6164160983547));
#15787=CARTESIAN_POINT('Ctrl Pts',(-21.7923995093482,26.2513800144884,-54.6161453209771));
#15788=CARTESIAN_POINT('Ctrl Pts',(-21.8041036336893,26.258974152679,-54.6152859009329));
#15789=CARTESIAN_POINT('Ctrl Pts',(-21.8121392797049,26.2641374065741,-54.6146962093826));
#15790=CARTESIAN_POINT('Ctrl Pts',(-21.8808987598081,26.3078877316409,-54.6096531571899));
#15791=CARTESIAN_POINT('Ctrl Pts',(-21.9428718063461,26.344464364874,-54.6051258761946));
#15792=CARTESIAN_POINT('Ctrl Pts',(-22.0288733983659,26.3914145198979,-54.5988597519354));
#15793=CARTESIAN_POINT('Ctrl Pts',(-22.0518827698974,26.4036161247636,-54.5971849162755));
#15794=CARTESIAN_POINT('Ctrl Pts',(-22.0750360179885,26.4155367759168,-54.5955012513333));
#15795=CARTESIAN_POINT('Origin',(-23.5502525316942,23.5502525316942,-77.3107734492734));
#15796=CARTESIAN_POINT('',(-22.0750356956303,26.4155366099478,-53.096872577003));
#15797=CARTESIAN_POINT('',(-22.0750361378578,26.4155368376325,-53.3407994113682));
#15798=CARTESIAN_POINT('',(-22.0750360153461,26.4155367745563,-77.3107734492734));
#15799=CARTESIAN_POINT('',(-26.7730023566686,23.5491903981972,-53.9421167188325));
#15800=CARTESIAN_POINT('Ctrl Pts',(-22.0750356956303,26.4155366099478,-53.096872577003));
#15801=CARTESIAN_POINT('Ctrl Pts',(-21.9264125543873,26.3390166718885,-53.1081849636288));
#15802=CARTESIAN_POINT('Ctrl Pts',(-21.7838852981894,26.2510064584347,-53.1194618737691));
#15803=CARTESIAN_POINT('Ctrl Pts',(-21.644761491229,26.1493381498409,-53.1304977873125));
#15804=CARTESIAN_POINT('Ctrl Pts',(-21.6407642551953,26.1464028891144,-53.130814879377));
#15805=CARTESIAN_POINT('Ctrl Pts',(-21.6326837681245,26.1404404468286,-53.1314558885018));
#15806=CARTESIAN_POINT('Ctrl Pts',(-21.6286008681162,26.1374128056937,-53.1317797777548));
#15807=CARTESIAN_POINT('Ctrl Pts',(-21.6180178841249,26.1295262063868,-53.1326192730615));
#15808=CARTESIAN_POINT('Ctrl Pts',(-21.6115289125131,26.1246522974172,-53.1331339772478));
#15809=CARTESIAN_POINT('Ctrl Pts',(-21.6016557715084,26.117178015854,-53.1339169743418));
#15810=CARTESIAN_POINT('Ctrl Pts',(-21.5982582964917,26.1145953873281,-53.1341863884835));
#15811=CARTESIAN_POINT('Ctrl Pts',(-21.585629747171,26.1049560148004,-53.1351876861482));
#15812=CARTESIAN_POINT('Ctrl Pts',(-21.5764315805592,26.0978560005917,-53.1359167442937));
#15813=CARTESIAN_POINT('Ctrl Pts',(-21.5645024581978,26.0885445855169,-53.1368617121533));
#15814=CARTESIAN_POINT('Ctrl Pts',(-21.5617365877379,26.0863783656786,-53.1370807724197));
#15815=CARTESIAN_POINT('Ctrl Pts',(-21.557489151381,26.08304056864,-53.1374171075578));
#15816=CARTESIAN_POINT('Ctrl Pts',(-21.5560050751758,26.0818722132867,-53.1375346121952));
#15817=CARTESIAN_POINT('Ctrl Pts',(-21.5530867203241,26.0795705476653,-53.1377656523878));
#15818=CARTESIAN_POINT('Ctrl Pts',(-21.5516523866666,26.0784373280153,-53.1378791929288));
#15819=CARTESIAN_POINT('Ctrl Pts',(-21.5484721537288,26.0759203332508,-53.1381309095772));
#15820=CARTESIAN_POINT('Ctrl Pts',(-21.5467267289484,26.0745359712531,-53.138269042315));
#15821=CARTESIAN_POINT('Ctrl Pts',(-21.5431004575973,26.0716537086574,-53.1385559902889));
#15822=CARTESIAN_POINT('Ctrl Pts',(-21.5412198480975,26.0701555099996,-53.1387047840066));
#15823=CARTESIAN_POINT('Ctrl Pts',(-21.5363783500534,26.0662896370802,-53.1390877979437));
#15824=CARTESIAN_POINT('Ctrl Pts',(-21.5334199490057,26.0639188319239,-53.1393217953335));
#15825=CARTESIAN_POINT('Ctrl Pts',(-21.5248120560862,26.0569956542946,-53.1400025401155));
#15826=CARTESIAN_POINT('Ctrl Pts',(-21.519173700073,26.0524293809648,-53.1404483114529));
#15827=CARTESIAN_POINT('Ctrl Pts',(-21.4609426211798,26.0049438970312,-53.1450512980499));
#15828=CARTESIAN_POINT('Ctrl Pts',(-21.409698582786,25.96038861478,-53.1490953338779));
#15829=CARTESIAN_POINT('Ctrl Pts',(-21.3276489647413,25.8843655462217,-53.1556329165519));
#15830=CARTESIAN_POINT('Ctrl Pts',(-21.2960152860911,25.8538290771929,-53.1581697852802));
#15831=CARTESIAN_POINT('Ctrl Pts',(-21.0608773142502,25.6173628954903,-53.1772424018582));
#15832=CARTESIAN_POINT('Ctrl Pts',(-20.8853333523026,25.3855054672074,-53.1928690626812));
#15833=CARTESIAN_POINT('Ctrl Pts',(-20.6933165665967,25.0450134271123,-53.2155987286319));
#15834=CARTESIAN_POINT('Ctrl Pts',(-20.6477209559888,24.9544250441392,-53.221612652192));
#15835=CARTESIAN_POINT('Ctrl Pts',(-20.6026431666172,24.8532510427292,-53.2283541414504));
#15836=CARTESIAN_POINT('Ctrl Pts',(-20.5988516485134,24.8446399978957,-53.2289280862801));
#15837=CARTESIAN_POINT('Ctrl Pts',(-20.5932865901723,24.831849424511,-53.2297808990881));
#15838=CARTESIAN_POINT('Ctrl Pts',(-20.5914840625612,24.827682498745,-53.2300587752421));
#15839=CARTESIAN_POINT('Ctrl Pts',(-20.588417214673,24.8205515128383,-53.2305343969663));
#15840=CARTESIAN_POINT('Ctrl Pts',(-20.5871485201455,24.8175893311604,-53.2307319929255));
#15841=CARTESIAN_POINT('Ctrl Pts',(-20.5846920216929,24.8118299803954,-53.2311162275239));
#15842=CARTESIAN_POINT('Ctrl Pts',(-20.583503727012,24.8090330238254,-53.2313028491362));
#15843=CARTESIAN_POINT('Ctrl Pts',(-20.5806758411265,24.8023506214307,-53.231748776472));
#15844=CARTESIAN_POINT('Ctrl Pts',(-20.5790399201579,24.7984636373417,-53.2320082068354));
#15845=CARTESIAN_POINT('Ctrl Pts',(-20.5741749926794,24.7868407071785,-53.2327841035234));
#15846=CARTESIAN_POINT('Ctrl Pts',(-20.5709685538065,24.7790954064949,-53.2333013358714));
#15847=CARTESIAN_POINT('Ctrl Pts',(-20.543896225,24.7129721410528,-53.2377188119685));
#15848=CARTESIAN_POINT('Ctrl Pts',(-20.5217199718412,24.6539213032495,-53.2416758496819));
#15849=CARTESIAN_POINT('Ctrl Pts',(-20.4700054336758,24.5028922651448,-53.2518372658197));
#15850=CARTESIAN_POINT('Ctrl Pts',(-20.4428450475918,24.4101713694486,-53.2581144346053));
#15851=CARTESIAN_POINT('Ctrl Pts',(-20.3387038807127,23.9846541524688,-53.287059718394));
#15852=CARTESIAN_POINT('Ctrl Pts',(-20.3107654224717,23.6421731156019,-53.3110069177333));
#15853=CARTESIAN_POINT('Ctrl Pts',(-20.3373648897722,23.2982956069008,-53.3328102903745));
#15854=CARTESIAN_POINT('Ctrl Pts',(-20.3376344562879,23.2948814421683,-53.333026512313));
#15855=CARTESIAN_POINT('Ctrl Pts',(-20.3388772123724,23.2794548856592,-53.3340023334152));
#15856=CARTESIAN_POINT('Ctrl Pts',(-20.3399123536812,23.2674473708176,-53.334758712591));
#15857=CARTESIAN_POINT('Ctrl Pts',(-20.3413408348653,23.2518970663943,-53.3357339068266));
#15858=CARTESIAN_POINT('Ctrl Pts',(-20.3416727088271,23.2483489339966,-53.3359561242431));
#15859=CARTESIAN_POINT('Ctrl Pts',(-20.3421904506979,23.242910941653,-53.3362962443138));
#15860=CARTESIAN_POINT('Ctrl Pts',(-20.3423721034959,23.2410206980787,-53.3364143850099));
#15861=CARTESIAN_POINT('Ctrl Pts',(-20.3427318043936,23.2373121470302,-53.3366460023423));
#15862=CARTESIAN_POINT('Ctrl Pts',(-20.3429097270817,23.2354938397536,-53.3367594851252));
#15863=CARTESIAN_POINT('Ctrl Pts',(-20.3433073192287,23.231465930234,-53.3370106962435));
#15864=CARTESIAN_POINT('Ctrl Pts',(-20.3435277255814,23.2292564087303,-53.3371483819689));
#15865=CARTESIAN_POINT('Ctrl Pts',(-20.3439897049508,23.2246731383995,-53.3374337480011));
#15866=CARTESIAN_POINT('Ctrl Pts',(-20.3442316310094,23.2222994253596,-53.3375814082492));
#15867=CARTESIAN_POINT('Ctrl Pts',(-20.3448602793852,23.2161984745238,-53.3379605894456));
#15868=CARTESIAN_POINT('Ctrl Pts',(-20.3452508680339,23.2124716255692,-53.3381918937985));
#15869=CARTESIAN_POINT('Ctrl Pts',(-20.3464045498224,23.2016458065126,-53.3388628724425));
#15870=CARTESIAN_POINT('Ctrl Pts',(-20.3471847408823,23.1945486246428,-53.3393016042207));
#15871=CARTESIAN_POINT('Ctrl Pts',(-20.3499204864417,23.1704013936626,-53.3407906016417));
#15872=CARTESIAN_POINT('Ctrl Pts',(-20.3519886820548,23.1533640535193,-53.3418348464376));
#15873=CARTESIAN_POINT('Ctrl Pts',(-20.3607321029306,23.0858504191379,-53.3459506001339));
#15874=CARTESIAN_POINT('Ctrl Pts',(-20.3684673368163,23.0355162121156,-53.3489696532923));
#15875=CARTESIAN_POINT('Ctrl Pts',(-20.3850972313087,22.9421063611589,-53.3545150781536));
#15876=CARTESIAN_POINT('Ctrl Pts',(-20.3936868526397,22.8989897321121,-53.3570517590737));
#15877=CARTESIAN_POINT('Ctrl Pts',(-20.4654737931617,22.5735458787382,-53.3761126821695));
#15878=CARTESIAN_POINT('Ctrl Pts',(-20.5655454780846,22.3007114592981,-53.3917287117786));
#15879=CARTESIAN_POINT('Ctrl Pts',(-20.7481484243374,21.9550561318075,-53.414457433548));
#15880=CARTESIAN_POINT('Ctrl Pts',(-20.799820491099,21.8675287569679,-53.4204843362831));
#15881=CARTESIAN_POINT('Ctrl Pts',(-20.8606991045604,21.7747220338233,-53.4272398258827));
#15882=CARTESIAN_POINT('Ctrl Pts',(-20.8658970600626,21.7668731875153,-53.4278140848418));
#15883=CARTESIAN_POINT('Ctrl Pts',(-20.8736533797484,21.7552719840823,-53.428667290215));
#15884=CARTESIAN_POINT('Ctrl Pts',(-20.8761854387927,21.7515020295901,-53.4289452435505));
#15885=CARTESIAN_POINT('Ctrl Pts',(-20.8805279841499,21.7450658961626,-53.4294209634691));
#15886=CARTESIAN_POINT('Ctrl Pts',(-20.8823345220245,21.7423970500725,-53.4296185803054));
#15887=CARTESIAN_POINT('Ctrl Pts',(-20.8858522327515,21.7372169987342,-53.4300028279046));
#15888=CARTESIAN_POINT('Ctrl Pts',(-20.8875629603889,21.7347054946978,-53.4301894415971));
#15889=CARTESIAN_POINT('Ctrl Pts',(-20.8916558028042,21.7287150566131,-53.4306353061616));
#15890=CARTESIAN_POINT('Ctrl Pts',(-20.8940411930921,21.725238377119,-53.4308946815753));
#15891=CARTESIAN_POINT('Ctrl Pts',(-20.9011870660204,21.7148670354655,-53.4316702551496));
#15892=CARTESIAN_POINT('Ctrl Pts',(-20.9059675926914,21.7079862858899,-53.4321872183806));
#15893=CARTESIAN_POINT('Ctrl Pts',(-20.9468778822758,21.6495902295827,-53.4365953915076));
#15894=CARTESIAN_POINT('Ctrl Pts',(-20.984480157522,21.5991277348869,-53.440543129246));
#15895=CARTESIAN_POINT('Ctrl Pts',(-21.0832386849365,21.4743883688339,-53.4506697109949));
#15896=CARTESIAN_POINT('Ctrl Pts',(-21.1462850435764,21.4016933108215,-53.4569205757691));
#15897=CARTESIAN_POINT('Ctrl Pts',(-21.241047465615,21.3018282673034,-53.4660153498107));
#15898=CARTESIAN_POINT('Ctrl Pts',(-21.2701903906715,21.2722805904828,-53.4687747355142));
#15899=CARTESIAN_POINT('Ctrl Pts',(-21.3267255778722,21.2171322341095,-53.4740534978926));
#15900=CARTESIAN_POINT('Ctrl Pts',(-21.3540102255009,21.1914303523533,-53.4765698617017));
#15901=CARTESIAN_POINT('Ctrl Pts',(-21.5759287172132,20.9895740786083,-53.4967728089937));
#15902=CARTESIAN_POINT('Ctrl Pts',(-21.7909848996853,20.8373159493884,-53.5148553221601));
#15903=CARTESIAN_POINT('Ctrl Pts',(-22.0252407489064,20.7111560143273,-53.5316767484546));
#15904=CARTESIAN_POINT('Ctrl Pts',(-22.0283450965297,20.7094907092915,-53.5318991745569));
#15905=CARTESIAN_POINT('Ctrl Pts',(-22.042112554287,20.7021343001088,-53.5328834179548));
#15906=CARTESIAN_POINT('Ctrl Pts',(-22.0528050866042,20.6964980200435,-53.5336420120053));
#15907=CARTESIAN_POINT('Ctrl Pts',(-22.066694584259,20.6892761062412,-53.5346196520834));
#15908=CARTESIAN_POINT('Ctrl Pts',(-22.0698626419416,20.6876355358304,-53.5348421212936));
#15909=CARTESIAN_POINT('Ctrl Pts',(-22.0747218628629,20.6851294249309,-53.5351825431785));
#15910=CARTESIAN_POINT('Ctrl Pts',(-22.076411064891,20.6842601202692,-53.5353007345611));
#15911=CARTESIAN_POINT('Ctrl Pts',(-22.0797264910376,20.6825576272401,-53.5355324174726));
#15912=CARTESIAN_POINT('Ctrl Pts',(-22.0813526467957,20.6817243325192,-53.5356459152116));
#15913=CARTESIAN_POINT('Ctrl Pts',(-22.084947275341,20.6798861870017,-53.5358964973556));
#15914=CARTESIAN_POINT('Ctrl Pts',(-22.0869160685292,20.6788819804275,-53.5360335403902));
#15915=CARTESIAN_POINT('Ctrl Pts',(-22.0910076325528,20.6768003302778,-53.5363179286341));
#15916=CARTESIAN_POINT('Ctrl Pts',(-22.0931305683855,20.6757232113315,-53.5364652532615));
#15917=CARTESIAN_POINT('Ctrl Pts',(-22.0985867036918,20.6729625166148,-53.5368432997671));
#15918=CARTESIAN_POINT('Ctrl Pts',(-22.1019216509747,20.6712823742681,-53.5370738068801));
#15919=CARTESIAN_POINT('Ctrl Pts',(-22.1116109496371,20.6664220144751,-53.5377418990032));
#15920=CARTESIAN_POINT('Ctrl Pts',(-22.117972957744,20.6632569865083,-53.5381785512955));
#15921=CARTESIAN_POINT('Ctrl Pts',(-22.1396363846814,20.6525689095394,-53.5396587330491));
#15922=CARTESIAN_POINT('Ctrl Pts',(-22.1549873235745,20.6451461109461,-53.540696321814));
#15923=CARTESIAN_POINT('Ctrl Pts',(-22.2172599425824,20.6156422599032,-53.5448628604659));
#15924=CARTESIAN_POINT('Ctrl Pts',(-22.2646550129647,20.5945721767084,-53.5479370047374));
#15925=CARTESIAN_POINT('Ctrl Pts',(-22.3783812312209,20.5472673143048,-53.5551329698665));
#15926=CARTESIAN_POINT('Ctrl Pts',(-22.445116130622,20.5220720286719,-53.5592135194819));
#15927=CARTESIAN_POINT('Ctrl Pts',(-22.8435373530829,20.3865789093105,-53.5830402699131));
#15928=CARTESIAN_POINT('Ctrl Pts',(-23.1905040045684,20.3286292295946,-53.6019433950894));
#15929=CARTESIAN_POINT('Ctrl Pts',(-23.5604852819765,20.3274537557524,-53.6243169797322));
#15930=CARTESIAN_POINT('Ctrl Pts',(-23.5809568112275,20.3275837810245,-53.6255609157499));
#15931=CARTESIAN_POINT('Ctrl Pts',(-23.6076881939732,20.3280082919943,-53.6271934627104));
#15932=CARTESIAN_POINT('Ctrl Pts',(-23.6139506973439,20.3281260074252,-53.6275765182799));
#15933=CARTESIAN_POINT('Ctrl Pts',(-23.6235958762808,20.3283354366992,-53.6281674022251));
#15934=CARTESIAN_POINT('Ctrl Pts',(-23.6269788414485,20.3284142231398,-53.6283748244781));
#15935=CARTESIAN_POINT('Ctrl Pts',(-23.6337034153293,20.3285814301208,-53.628787483053));
#15936=CARTESIAN_POINT('Ctrl Pts',(-23.6370450232457,20.3286697219609,-53.6289927150784));
#15937=CARTESIAN_POINT('Ctrl Pts',(-23.6444351372475,20.3288764897229,-53.6294469772071));
#15938=CARTESIAN_POINT('Ctrl Pts',(-23.6484835647494,20.328997398849,-53.6296960834212));
#15939=CARTESIAN_POINT('Ctrl Pts',(-23.6601128506016,20.3293666591382,-53.630412387059));
#15940=CARTESIAN_POINT('Ctrl Pts',(-23.667693036369,20.3296341407657,-53.6308801846923));
#15941=CARTESIAN_POINT('Ctrl Pts',(-23.7175271396097,20.3315688034118,-53.633961591426));
#15942=CARTESIAN_POINT('Ctrl Pts',(-23.7597440192034,20.3340406638312,-53.6366003744818));
#15943=CARTESIAN_POINT('Ctrl Pts',(-23.8841588440679,20.3437852520706,-53.6444653790937));
#15944=CARTESIAN_POINT('Ctrl Pts',(-23.9661348882302,20.3533844153971,-53.649762721159));
#15945=CARTESIAN_POINT('Ctrl Pts',(-24.141079906918,20.3807126067578,-53.6613164350819));
#15946=CARTESIAN_POINT('Ctrl Pts',(-24.2338189079287,20.3994121546459,-53.667594662097));
#15947=CARTESIAN_POINT('Ctrl Pts',(-24.3534955823353,20.4290757703748,-53.6758678729871));
#15948=CARTESIAN_POINT('Ctrl Pts',(-24.3813011251624,20.4363639704456,-53.6778021578916));
#15949=CARTESIAN_POINT('Ctrl Pts',(-24.4324512431185,20.4505050046481,-53.6813807688069));
#15950=CARTESIAN_POINT('Ctrl Pts',(-24.455823059852,20.45725215957,-53.6830238553027));
#15951=CARTESIAN_POINT('Ctrl Pts',(-24.499289462612,20.4703352762356,-53.6860930076009));
#15952=CARTESIAN_POINT('Ctrl Pts',(-24.5194027445228,20.4766049824001,-53.6875185943597));
#15953=CARTESIAN_POINT('Ctrl Pts',(-24.5938235606372,20.500606535501,-53.6928113428409));
#15954=CARTESIAN_POINT('Ctrl Pts',(-24.6477185820383,20.5195843617657,-53.6966802083909));
#15955=CARTESIAN_POINT('Ctrl Pts',(-24.7905314555467,20.5741818709959,-53.7069931870938));
#15956=CARTESIAN_POINT('Ctrl Pts',(-24.8784191951728,20.6123512343379,-53.713405570235));
#15957=CARTESIAN_POINT('Ctrl Pts',(-25.0244644449832,20.6836739313318,-53.7240403648126));
#15958=CARTESIAN_POINT('Ctrl Pts',(-25.0835283808606,20.7148265720418,-53.7283347501345));
#15959=CARTESIAN_POINT('Ctrl Pts',(-25.1467845617617,20.7507456523154,-53.7328926732911));
#15960=CARTESIAN_POINT('Ctrl Pts',(-25.1519741743764,20.7537116198804,-53.7332663001447));
#15961=CARTESIAN_POINT('Ctrl Pts',(-25.1592389363151,20.7578904332408,-53.7337888587177));
#15962=CARTESIAN_POINT('Ctrl Pts',(-25.161320985278,20.7590911646118,-53.7339385675561));
#15963=CARTESIAN_POINT('Ctrl Pts',(-25.1649257387841,20.7611754269837,-53.7341976692808));
#15964=CARTESIAN_POINT('Ctrl Pts',(-25.1664490623208,20.7620578763412,-53.7343071325014));
#15965=CARTESIAN_POINT('Ctrl Pts',(-25.1695893020679,20.7638804307699,-53.734532721381));
#15966=CARTESIAN_POINT('Ctrl Pts',(-25.1712061211877,20.7648206941833,-53.734648835973));
#15967=CARTESIAN_POINT('Ctrl Pts',(-25.1750239882963,20.767045430027,-53.7349229427272));
#15968=CARTESIAN_POINT('Ctrl Pts',(-25.1772243392184,20.7683311103401,-53.7350808559368));
#15969=CARTESIAN_POINT('Ctrl Pts',(-25.1818847800201,20.7710616587359,-53.7354151951705));
#15970=CARTESIAN_POINT('Ctrl Pts',(-25.1843444831164,20.7725071876143,-53.7355915781458));
#15971=CARTESIAN_POINT('Ctrl Pts',(-25.1909996745928,20.7764302382418,-53.7360686195069));
#15972=CARTESIAN_POINT('Ctrl Pts',(-25.195191490119,20.7789140236145,-53.7363688757136));
#15973=CARTESIAN_POINT('Ctrl Pts',(-25.2081620529372,20.7866392952875,-53.7372973419572));
#15974=CARTESIAN_POINT('Ctrl Pts',(-25.2169216045372,20.7919131201758,-53.7379235133485));
#15975=CARTESIAN_POINT('Ctrl Pts',(-25.2495369074405,20.8117617647422,-53.7402523541918));
#15976=CARTESIAN_POINT('Ctrl Pts',(-25.2732285651983,20.8266055692244,-53.7419387083908));
#15977=CARTESIAN_POINT('Ctrl Pts',(-25.3572506104525,20.8807840408662,-53.7479114250149));
#15978=CARTESIAN_POINT('Ctrl Pts',(-25.4164554231788,20.9218324164873,-53.7521053832842));
#15979=CARTESIAN_POINT('Ctrl Pts',(-25.7830427091458,21.1946349171485,-53.7783117506642));
#15980=CARTESIAN_POINT('Ctrl Pts',(-26.0481697824471,21.477879923486,-53.7987948838381));
#15981=CARTESIAN_POINT('Ctrl Pts',(-26.2679270647295,21.8179820977463,-53.823288773705));
#15982=CARTESIAN_POINT('Ctrl Pts',(-26.2786002779706,21.8348417146096,-53.8245014647242));
#15983=CARTESIAN_POINT('Ctrl Pts',(-26.2923840237608,21.857068875624,-53.8260986479468));
#15984=CARTESIAN_POINT('Ctrl Pts',(-26.295636757774,21.8623480725172,-53.8264778799225));
#15985=CARTESIAN_POINT('Ctrl Pts',(-26.3006343591503,21.8705118579788,-53.8270641595052));
#15986=CARTESIAN_POINT('Ctrl Pts',(-26.3023899826332,21.8733898722208,-53.8272708111726));
#15987=CARTESIAN_POINT('Ctrl Pts',(-26.3058778927084,21.8791278766723,-53.8276827591651));
#15988=CARTESIAN_POINT('Ctrl Pts',(-26.3076102506747,21.8819878187868,-53.8278880525357));
#15989=CARTESIAN_POINT('Ctrl Pts',(-26.3114417696561,21.8883355284416,-53.8283436418372));
#15990=CARTESIAN_POINT('Ctrl Pts',(-26.3135387770174,21.8918245833945,-53.8285940162184));
#15991=CARTESIAN_POINT('Ctrl Pts',(-26.3195735343807,21.9019085912587,-53.8293175262966));
#15992=CARTESIAN_POINT('Ctrl Pts',(-26.3234943044758,21.9085136273756,-53.8297912812035));
#15993=CARTESIAN_POINT('Ctrl Pts',(-26.3498570823684,21.9532889936326,-53.8330019621775));
#15994=CARTESIAN_POINT('Ctrl Pts',(-26.371533048071,21.9919027267853,-53.8357665455221));
#15995=CARTESIAN_POINT('Ctrl Pts',(-26.4162332703386,22.0755232163435,-53.8417481619889));
#15996=CARTESIAN_POINT('Ctrl Pts',(-26.4390077226515,22.1206493918931,-53.8449730416554));
#15997=CARTESIAN_POINT('Ctrl Pts',(-26.5041758098438,22.2576972187417,-53.8547596721978));
#15998=CARTESIAN_POINT('Ctrl Pts',(-26.5433071003439,22.3510931518908,-53.861421539032));
#15999=CARTESIAN_POINT('Ctrl Pts',(-26.6722433689188,22.7046744483083,-53.8865409505672));
#16000=CARTESIAN_POINT('Ctrl Pts',(-26.7330131296374,22.9741774182669,-53.9055964789788));
#16001=CARTESIAN_POINT('Ctrl Pts',(-26.7598832959582,23.2595305461044,-53.9240967512976));
#16002=CARTESIAN_POINT('Ctrl Pts',(-26.7608968990714,23.2709468391368,-53.924833956984));
#16003=CARTESIAN_POINT('Ctrl Pts',(-26.76244427627,23.2894979688374,-53.9260268554759));
#16004=CARTESIAN_POINT('Ctrl Pts',(-26.7630152225191,23.2966295035031,-53.9264842283835));
#16005=CARTESIAN_POINT('Ctrl Pts',(-26.7639816365523,23.3092279579645,-53.9272900142447));
#16006=CARTESIAN_POINT('Ctrl Pts',(-26.7643869122515,23.3146940692898,-53.9276388903131));
#16007=CARTESIAN_POINT('Ctrl Pts',(-26.7662605537946,23.3408700649972,-53.9293059945067));
#16008=CARTESIAN_POINT('Ctrl Pts',(-26.767542758271,23.3615934000929,-53.9306150855915));
#16009=CARTESIAN_POINT('Ctrl Pts',(-26.7688284710982,23.3862348875533,-53.932157775011));
#16010=CARTESIAN_POINT('Ctrl Pts',(-26.7690251912368,23.3901418453975,-53.9324019562176));
#16011=CARTESIAN_POINT('Ctrl Pts',(-26.7693323520063,23.3964716641396,-53.9327968805583));
#16012=CARTESIAN_POINT('Ctrl Pts',(-26.769447171445,23.3988942935331,-53.9329478689265));
#16013=CARTESIAN_POINT('Ctrl Pts',(-26.76964305871,23.4031284842292,-53.933211475259));
#16014=CARTESIAN_POINT('Ctrl Pts',(-26.7697253323798,23.4049399840895,-53.9333241615068));
#16015=CARTESIAN_POINT('Ctrl Pts',(-26.7698839076654,23.4084977414733,-53.9335452949049));
#16016=CARTESIAN_POINT('Ctrl Pts',(-26.7699603173148,23.4102439857482,-53.9336537479536));
#16017=CARTESIAN_POINT('Ctrl Pts',(-26.7701224129934,23.4140187899975,-53.9338880050728));
#16018=CARTESIAN_POINT('Ctrl Pts',(-26.7702076028248,23.4160473722205,-53.9340137810181));
#16019=CARTESIAN_POINT('Ctrl Pts',(-26.7704095782857,23.4209678291189,-53.9343185851533));
#16020=CARTESIAN_POINT('Ctrl Pts',(-26.7705243857482,23.4238597899097,-53.9344975023083));
#16021=CARTESIAN_POINT('Ctrl Pts',(-26.7708258853175,23.4317216455153,-53.9349832789564));
#16022=CARTESIAN_POINT('Ctrl Pts',(-26.7710049700657,23.4366918494909,-53.9352897169584));
#16023=CARTESIAN_POINT('Ctrl Pts',(-26.7723804683151,23.477490891901,-53.937799860012));
#16024=CARTESIAN_POINT('Ctrl Pts',(-26.7729905408346,23.5133385236836,-53.9399716842124));
#16025=CARTESIAN_POINT('Ctrl Pts',(-26.7730023566686,23.5491903981972,-53.9421167188325));
#16026=CARTESIAN_POINT('Ctrl Pts',(-26.7730023556334,23.5491872617795,-53.942116531179));
#16027=CARTESIAN_POINT('Ctrl Pts',(-26.7730945560227,23.8281201261137,-53.9588052287378));
#16028=CARTESIAN_POINT('Ctrl Pts',(-26.7369744698146,24.1059428445382,-53.9738720656566));
#16029=CARTESIAN_POINT('Ctrl Pts',(-26.6187707521688,24.552051586306,-53.9999189007627));
#16030=CARTESIAN_POINT('Ctrl Pts',(-26.5571558436671,24.7241023836079,-54.0104424369143));
#16031=CARTESIAN_POINT('Ctrl Pts',(-26.4738354566922,24.9063885917255,-54.0225828338893));
#16032=CARTESIAN_POINT('Ctrl Pts',(-26.4662088341052,24.9227105290593,-54.023678744104));
#16033=CARTESIAN_POINT('Ctrl Pts',(-26.4559781523645,24.9441352297471,-54.0251292783573));
#16034=CARTESIAN_POINT('Ctrl Pts',(-26.4534966669611,24.9492964369809,-54.0254796359503));
#16035=CARTESIAN_POINT('Ctrl Pts',(-26.4494155114942,24.9577271593998,-54.0260534614175));
#16036=CARTESIAN_POINT('Ctrl Pts',(-26.4478240284401,24.961000642503,-54.0262766433599));
#16037=CARTESIAN_POINT('Ctrl Pts',(-26.4447405262859,24.9673157940636,-54.0267079336213));
#16038=CARTESIAN_POINT('Ctrl Pts',(-26.443249249135,24.9703578211461,-54.0269160157792));
#16039=CARTESIAN_POINT('Ctrl Pts',(-26.4398110887038,24.9773433661698,-54.0273946023057));
#16040=CARTESIAN_POINT('Ctrl Pts',(-26.4378609275962,24.9812852552338,-54.0276652212466));
#16041=CARTESIAN_POINT('Ctrl Pts',(-26.4316554842877,24.9937640744431,-54.0285236909451));
#16042=CARTESIAN_POINT('Ctrl Pts',(-26.4273703959059,25.0022860511279,-54.0291125873443));
#16043=CARTESIAN_POINT('Ctrl Pts',(-26.4110843977381,25.0343197196009,-54.0313362557893));
#16044=CARTESIAN_POINT('Ctrl Pts',(-26.3988328610272,25.0577021741146,-54.0329798485356));
#16045=CARTESIAN_POINT('Ctrl Pts',(-26.3833746885691,25.0863430989516,-54.0350189574913));
#16046=CARTESIAN_POINT('Ctrl Pts',(-26.3804381510721,25.0917468539716,-54.0354048280166));
#16047=CARTESIAN_POINT('Ctrl Pts',(-26.3741996030749,25.1031489816459,-54.0362214649155));
#16048=CARTESIAN_POINT('Ctrl Pts',(-26.3708939116635,25.1091452960216,-54.0366523603786));
#16049=CARTESIAN_POINT('Ctrl Pts',(-26.3666905475507,25.1167127895278,-54.0371979788459));
#16050=CARTESIAN_POINT('Ctrl Pts',(-26.3658106081822,25.118293843151,-54.0373120738645));
#16051=CARTESIAN_POINT('Ctrl Pts',(-26.3636312476271,25.1222019159815,-54.0375943447815));
#16052=CARTESIAN_POINT('Ctrl Pts',(-26.3623302720827,25.1245280628413,-54.0377625755402));
#16053=CARTESIAN_POINT('Ctrl Pts',(-26.3576530459204,25.1328666551794,-54.0383664219273));
#16054=CARTESIAN_POINT('Ctrl Pts',(-26.354260404153,25.1388698427979,-54.0388026151492));
#16055=CARTESIAN_POINT('Ctrl Pts',(-26.3482420857702,25.1494397523406,-54.039573226755));
#16056=CARTESIAN_POINT('Ctrl Pts',(-26.3456244212331,25.1540110266204,-54.0399073623416));
#16057=CARTESIAN_POINT('Ctrl Pts',(-26.3409964033775,25.1620472619889,-54.0404962890854));
#16058=CARTESIAN_POINT('Ctrl Pts',(-26.3389907700402,25.1655149400047,-54.0407509144807));
#16059=CARTESIAN_POINT('Ctrl Pts',(-26.3347887704748,25.1727489127244,-54.0412831393293));
#16060=CARTESIAN_POINT('Ctrl Pts',(-26.3325912175981,25.1765145057206,-54.041560779806));
#16061=CARTESIAN_POINT('Ctrl Pts',(-26.3200151500943,25.1979639852111,-54.0431456668619));
#16062=CARTESIAN_POINT('Ctrl Pts',(-26.3094758783938,25.2155526515351,-54.0444584802907));
#16063=CARTESIAN_POINT('Ctrl Pts',(-26.1413332266607,25.4901822039067,-54.0651655423998));
#16064=CARTESIAN_POINT('Ctrl Pts',(-25.9486007724376,25.7239337604452,-54.0858881766233));
#16065=CARTESIAN_POINT('Ctrl Pts',(-25.6619031058536,25.9863692923315,-54.1118916215496));
#16066=CARTESIAN_POINT('Ctrl Pts',(-25.5951604670809,26.0426584064178,-54.1176578634111));
#16067=CARTESIAN_POINT('Ctrl Pts',(-25.505664169124,26.1121189027979,-54.1249462919421));
#16068=CARTESIAN_POINT('Ctrl Pts',(-25.4849252862279,26.1278163827829,-54.1266057840618));
#16069=CARTESIAN_POINT('Ctrl Pts',(-25.4561958483418,26.1490198674835,-54.1288620410255));
#16070=CARTESIAN_POINT('Ctrl Pts',(-25.448367725862,26.1547429438666,-54.1294725425885));
#16071=CARTESIAN_POINT('Ctrl Pts',(-25.4367182565902,26.1631793566274,-54.1303745936406));
#16072=CARTESIAN_POINT('Ctrl Pts',(-25.4329167182444,26.1659197668364,-54.1306679419268));
#16073=CARTESIAN_POINT('Ctrl Pts',(-25.4268531857238,26.1702707106203,-54.1311342059666));
#16074=CARTESIAN_POINT('Ctrl Pts',(-25.4245950823499,26.1718866166777,-54.1313074867353));
#16075=CARTESIAN_POINT('Ctrl Pts',(-25.4203032862934,26.1749494603274,-54.1316361414455));
#16076=CARTESIAN_POINT('Ctrl Pts',(-25.4182699974343,26.1763969564632,-54.1317915537984));
#16077=CARTESIAN_POINT('Ctrl Pts',(-25.4147179571499,26.1789194375477,-54.132062538667));
#16078=CARTESIAN_POINT('Ctrl Pts',(-25.4131999545484,26.1799954705384,-54.1321781841369));
#16079=CARTESIAN_POINT('Ctrl Pts',(-25.4102319034212,26.1820955077152,-54.1324039790384));
#16080=CARTESIAN_POINT('Ctrl Pts',(-25.408781944119,26.1831196261127,-54.1325141365193));
#16081=CARTESIAN_POINT('Ctrl Pts',(-25.4053208655009,26.1855599311382,-54.1327767325428));
#16082=CARTESIAN_POINT('Ctrl Pts',(-25.4033089659669,26.1869750169306,-54.1329290946841));
#16083=CARTESIAN_POINT('Ctrl Pts',(-25.3972284518379,26.1912413988257,-54.1333887275581));
#16084=CARTESIAN_POINT('Ctrl Pts',(-25.393154837788,26.1940856082853,-54.1336955126422));
#16085=CARTESIAN_POINT('Ctrl Pts',(-25.3518058090543,26.2228136207685,-54.1367981246812));
#16086=CARTESIAN_POINT('Ctrl Pts',(-25.3139918749871,26.2479183803324,-54.1395418231498));
#16087=CARTESIAN_POINT('Ctrl Pts',(-25.1961251910126,26.3226319838297,-54.1478513766108));
#16088=CARTESIAN_POINT('Ctrl Pts',(-25.1144142767542,26.3695406639125,-54.1532775352055));
#16089=CARTESIAN_POINT('Ctrl Pts',(-24.958764310648,26.4500425290349,-54.1632233292736));
#16090=CARTESIAN_POINT('Ctrl Pts',(-24.8853876011128,26.4845501442545,-54.1677602780092));
#16091=CARTESIAN_POINT('Ctrl Pts',(-24.6491029420874,26.5849697379848,-54.1821103432062));
#16092=CARTESIAN_POINT('Ctrl Pts',(-24.4820774102794,26.6403460727273,-54.191892514863));
#16093=CARTESIAN_POINT('Ctrl Pts',(-24.2353059855947,26.7003237651233,-54.2065893842924));
#16094=CARTESIAN_POINT('Ctrl Pts',(-24.1585864286003,26.7160344993569,-54.2111881145551));
#16095=CARTESIAN_POINT('Ctrl Pts',(-24.0421789256471,26.7354848961182,-54.2182535585527));
#16096=CARTESIAN_POINT('Ctrl Pts',(-24.0028664212789,26.7413083512809,-54.2206543829996));
#16097=CARTESIAN_POINT('Ctrl Pts',(-23.9560653553474,26.7473588910429,-54.223533099852));
#16098=CARTESIAN_POINT('Ctrl Pts',(-23.9486698859282,26.7482889184793,-54.2239885981075));
#16099=CARTESIAN_POINT('Ctrl Pts',(-23.9372789140357,26.7496812805819,-54.2246911394828));
#16100=CARTESIAN_POINT('Ctrl Pts',(-23.9332856271383,26.7501618096893,-54.2249376069083));
#16101=CARTESIAN_POINT('Ctrl Pts',(-23.9260042192606,26.7510241869914,-54.2253873511894));
#16102=CARTESIAN_POINT('Ctrl Pts',(-23.9227163849817,26.7514084475982,-54.2255905514854));
#16103=CARTESIAN_POINT('Ctrl Pts',(-23.9160573226146,26.752176317452,-54.2260023585802));
#16104=CARTESIAN_POINT('Ctrl Pts',(-23.9126860696489,26.7525596695694,-54.2262109732305));
#16105=CARTESIAN_POINT('Ctrl Pts',(-23.9030447207589,26.7536405872707,-54.2268079620533));
#16106=CARTESIAN_POINT('Ctrl Pts',(-23.8967731992431,26.7543250635403,-54.2271967491555));
#16107=CARTESIAN_POINT('Ctrl Pts',(-23.8697651641498,26.7571925076086,-54.2288730411456));
#16108=CARTESIAN_POINT('Ctrl Pts',(-23.8490101129141,26.7591925757223,-54.2301663035805));
#16109=CARTESIAN_POINT('Ctrl Pts',(-23.4731451342962,26.7917348749944,-54.2536824429032));
#16110=CARTESIAN_POINT('Ctrl Pts',(-23.1154739095442,26.7633479180483,-54.2780179244678));
#16111=CARTESIAN_POINT('Ctrl Pts',(-22.7078945038185,26.6616233102381,-54.3062288726731));
#16112=CARTESIAN_POINT('Ctrl Pts',(-22.6464090862336,26.6443215298324,-54.3104856719587));
#16113=CARTESIAN_POINT('Ctrl Pts',(-22.5357189712163,26.6095921115149,-54.3181074534668));
#16114=CARTESIAN_POINT('Ctrl Pts',(-22.486345273698,26.5927743535008,-54.321491678926));
#16115=CARTESIAN_POINT('Ctrl Pts',(-22.4214531628953,26.5688976294274,-54.3258995684854));
#16116=CARTESIAN_POINT('Ctrl Pts',(-22.4055539869589,26.5629044384984,-54.326976302491));
#16117=CARTESIAN_POINT('Ctrl Pts',(-22.383090840696,26.5542334534166,-54.3284922130084));
#16118=CARTESIAN_POINT('Ctrl Pts',(-22.3764874835089,26.5516594359448,-54.3289371769255));
#16119=CARTESIAN_POINT('Ctrl Pts',(-22.3664243993078,26.5476985124281,-54.3296142064318));
#16120=CARTESIAN_POINT('Ctrl Pts',(-22.3629585500161,26.5463273731909,-54.3298471901444));
#16121=CARTESIAN_POINT('Ctrl Pts',(-22.3565533634135,26.5437805305491,-54.330277395391));
#16122=CARTESIAN_POINT('Ctrl Pts',(-22.3536133701421,26.5426065049949,-54.3304747165546));
#16123=CARTESIAN_POINT('Ctrl Pts',(-22.3488160018605,26.5406825742445,-54.3307964569059));
#16124=CARTESIAN_POINT('Ctrl Pts',(-22.3469575966116,26.5399352696889,-54.3309210336652));
#16125=CARTESIAN_POINT('Ctrl Pts',(-22.3433927340596,26.5384978997172,-54.3311598863868));
#16126=CARTESIAN_POINT('Ctrl Pts',(-22.3416861760813,26.5378081068679,-54.3312741782128));
#16127=CARTESIAN_POINT('Ctrl Pts',(-22.3377198094814,26.5362009418886,-54.3315396975375));
#16128=CARTESIAN_POINT('Ctrl Pts',(-22.3354604448534,26.5352824639767,-54.3316908574796));
#16129=CARTESIAN_POINT('Ctrl Pts',(-22.328329516505,26.5323741588045,-54.3321676717003));
#16130=CARTESIAN_POINT('Ctrl Pts',(-22.3234617507009,26.5303749510802,-54.332492757533));
#16131=CARTESIAN_POINT('Ctrl Pts',(-22.2831771906318,26.5137145171572,-54.3351799488851));
#16132=CARTESIAN_POINT('Ctrl Pts',(-22.2480177698886,26.4984336323821,-54.3375050894075));
#16133=CARTESIAN_POINT('Ctrl Pts',(-22.1665638548763,26.4612907218669,-54.3428631936693));
#16134=CARTESIAN_POINT('Ctrl Pts',(-22.1205172681142,26.4389531945934,-54.3458702400929));
#16135=CARTESIAN_POINT('Ctrl Pts',(-22.0750359442814,26.415536737968,-54.34883718749));
#16136=CARTESIAN_POINT('Ctrl Pts',(-22.0750360179885,26.4155367759168,-54.5955012513333));
#16137=CARTESIAN_POINT('Ctrl Pts',(-22.1009742172714,26.4288912834129,-54.5936150694628));
#16138=CARTESIAN_POINT('Ctrl Pts',(-22.1270929863428,26.4418931842608,-54.5917178026719));
#16139=CARTESIAN_POINT('Ctrl Pts',(-22.3631894087763,26.5554478916475,-54.5745881662261));
#16140=CARTESIAN_POINT('Ctrl Pts',(-22.583295460347,26.6333174528364,-54.5586903844263));
#16141=CARTESIAN_POINT('Ctrl Pts',(-22.9444643185385,26.7185761671403,-54.533710942971));
#16142=CARTESIAN_POINT('Ctrl Pts',(-23.0810228472947,26.7416608412576,-54.5245232806531));
#16143=CARTESIAN_POINT('Ctrl Pts',(-23.2342690244468,26.7575127830412,-54.5147800949232));
#16144=CARTESIAN_POINT('Ctrl Pts',(-23.2498927320136,26.7590136495353,-54.5137933323343));
#16145=CARTESIAN_POINT('Ctrl Pts',(-23.26924961122,26.7607305158691,-54.512579441191));
#16146=CARTESIAN_POINT('Ctrl Pts',(-23.2729726611281,26.761054207585,-54.5123463605135));
#16147=CARTESIAN_POINT('Ctrl Pts',(-23.278836856725,26.76155378028,-54.5119798662717));
#16148=CARTESIAN_POINT('Ctrl Pts',(-23.2809776147187,26.7617339962119,-54.5118462081358));
#16149=CARTESIAN_POINT('Ctrl Pts',(-23.2849790632726,26.7620668219165,-54.5115966278497));
#16150=CARTESIAN_POINT('Ctrl Pts',(-23.2868396937196,26.7622199544339,-54.5114806769453));
#16151=CARTESIAN_POINT('Ctrl Pts',(-23.2910168387963,26.7625600853323,-54.511220591711));
#16152=CARTESIAN_POINT('Ctrl Pts',(-23.2933334182414,26.7627461943912,-54.5110765085364));
#16153=CARTESIAN_POINT('Ctrl Pts',(-23.2992212851966,26.7632128035431,-54.5107106956386));
#16154=CARTESIAN_POINT('Ctrl Pts',(-23.3027928534128,26.7634898561237,-54.5104891606409));
#16155=CARTESIAN_POINT('Ctrl Pts',(-23.3224780566783,26.7649838549102,-54.5092701214903));
#16156=CARTESIAN_POINT('Ctrl Pts',(-23.3386005835814,26.7660855762527,-54.5082790254939));
#16157=CARTESIAN_POINT('Ctrl Pts',(-23.6681943649612,26.7861186447997,-54.4881550361072));
#16158=CARTESIAN_POINT('Ctrl Pts',(-23.9828179903954,26.7592561360464,-54.4713535661549));
#16159=CARTESIAN_POINT('Ctrl Pts',(-24.4493290146231,26.6494516703908,-54.4442368782231));
#16160=CARTESIAN_POINT('Ctrl Pts',(-24.6068665806205,26.5993392031658,-54.4346940865865));
#16161=CARTESIAN_POINT('Ctrl Pts',(-24.7744372900431,26.5314832468387,-54.4237802596548));
#16162=CARTESIAN_POINT('Ctrl Pts',(-24.7889708301596,26.5254738449781,-54.4228273463262));
#16163=CARTESIAN_POINT('Ctrl Pts',(-24.8106793615006,26.516311057799,-54.4213942194191));
#16164=CARTESIAN_POINT('Ctrl Pts',(-24.8178879262136,26.5132374250804,-54.4209167087605));
#16165=CARTESIAN_POINT('Ctrl Pts',(-24.8294509112932,26.5082572077584,-54.4201481097848));
#16166=CARTESIAN_POINT('Ctrl Pts',(-24.8338124793116,26.5063672145977,-54.4198575875126));
#16167=CARTESIAN_POINT('Ctrl Pts',(-24.8421309194249,26.5027407139094,-54.4193023343973));
#16168=CARTESIAN_POINT('Ctrl Pts',(-24.8460885146703,26.5010058829152,-54.419037661354));
#16169=CARTESIAN_POINT('Ctrl Pts',(-24.8530782774275,26.4979251126218,-54.4185693073353));
#16170=CARTESIAN_POINT('Ctrl Pts',(-24.8561118843654,26.4965824383757,-54.4183657386683));
#16171=CARTESIAN_POINT('Ctrl Pts',(-24.8620710026045,26.4939339216791,-54.4179652632655));
#16172=CARTESIAN_POINT('Ctrl Pts',(-24.8649966513385,26.4926283958728,-54.4177683675933));
#16173=CARTESIAN_POINT('Ctrl Pts',(-24.8719997821465,26.4894908259995,-54.4172963822152));
#16174=CARTESIAN_POINT('Ctrl Pts',(-24.8760754010203,26.4876546600464,-54.4170211507328));
#16175=CARTESIAN_POINT('Ctrl Pts',(-24.8884585096692,26.4820447444417,-54.416183223067));
#16176=CARTESIAN_POINT('Ctrl Pts',(-24.8967537509843,26.4782442123375,-54.4156196032885));
#16177=CARTESIAN_POINT('Ctrl Pts',(-24.9282734109128,26.4636409527045,-54.4134691265685));
#16178=CARTESIAN_POINT('Ctrl Pts',(-24.9513843929305,26.4525969429495,-54.4118739284959));
#16179=CARTESIAN_POINT('Ctrl Pts',(-24.9797939940123,26.43860248508,-54.4098896485956));
#16180=CARTESIAN_POINT('Ctrl Pts',(-24.9852196508811,26.4359107948562,-54.4095096297131));
#16181=CARTESIAN_POINT('Ctrl Pts',(-24.9967707431323,26.4301396181388,-54.4086983040156));
#16182=CARTESIAN_POINT('Ctrl Pts',(-25.0028939959815,26.4270558516583,-54.4082668498435));
#16183=CARTESIAN_POINT('Ctrl Pts',(-25.0100883018596,26.4234038601594,-54.4077583082061));
#16184=CARTESIAN_POINT('Ctrl Pts',(-25.0111689686063,26.4228545223064,-54.4076818763637));
#16185=CARTESIAN_POINT('Ctrl Pts',(-25.0150691686775,26.420869154386,-54.4074058729279));
#16186=CARTESIAN_POINT('Ctrl Pts',(-25.0178868897647,26.4194295853725,-54.4072061788152));
#16187=CARTESIAN_POINT('Ctrl Pts',(-25.0268295150917,26.4148441928803,-54.4065714724517));
#16188=CARTESIAN_POINT('Ctrl Pts',(-25.0329464293589,26.4116829044076,-54.4061359262017));
#16189=CARTESIAN_POINT('Ctrl Pts',(-25.0438219120351,26.4060180997954,-54.4053590563451));
#16190=CARTESIAN_POINT('Ctrl Pts',(-25.0485844490868,26.4035222242766,-54.4050179971229));
#16191=CARTESIAN_POINT('Ctrl Pts',(-25.0568830071811,26.3991467398329,-54.4044222146683));
#16192=CARTESIAN_POINT('Ctrl Pts',(-25.0604218225257,26.3972724318059,-54.4041676737734));
#16193=CARTESIAN_POINT('Ctrl Pts',(-25.0678161920721,26.3933383916417,-54.40363480983));
#16194=CARTESIAN_POINT('Ctrl Pts',(-25.0716710651511,26.3912774024211,-54.403356444221));
#16195=CARTESIAN_POINT('Ctrl Pts',(-25.0918412915703,26.3804406637514,-54.4018969327223));
#16196=CARTESIAN_POINT('Ctrl Pts',(-25.1080846864529,26.3715323339636,-54.4007112912739));
#16197=CARTESIAN_POINT('Ctrl Pts',(-25.1733925527948,26.3349797233172,-54.3959025549334));
#16198=CARTESIAN_POINT('Ctrl Pts',(-25.2218031739475,26.3061928297383,-54.3922417445337));
#16199=CARTESIAN_POINT('Ctrl Pts',(-25.3760985920768,26.2088813007158,-54.3802628235232));
#16200=CARTESIAN_POINT('Ctrl Pts',(-25.4787161511149,26.1354110209033,-54.3718012654041));
#16201=CARTESIAN_POINT('Ctrl Pts',(-25.6625980719657,25.9867051271226,-54.3558168687769));
#16202=CARTESIAN_POINT('Ctrl Pts',(-25.7448147438841,25.9129209826296,-54.3483199165899));
#16203=CARTESIAN_POINT('Ctrl Pts',(-25.9185695814987,25.7400771179663,-54.3318795414821));
#16204=CARTESIAN_POINT('Ctrl Pts',(-26.0080210667679,25.6391855312603,-54.3229954344297));
#16205=CARTESIAN_POINT('Ctrl Pts',(-26.0944882661496,25.5283870092592,-54.3141920366693));
#16206=CARTESIAN_POINT('Ctrl Pts',(-26.0980590574081,25.5237857573089,-54.3138280785755));
#16207=CARTESIAN_POINT('Ctrl Pts',(-26.1031876666514,25.5171400133166,-54.3133047775727));
#16208=CARTESIAN_POINT('Ctrl Pts',(-26.1047555165223,25.5151033324617,-54.3131447250498));
#16209=CARTESIAN_POINT('Ctrl Pts',(-26.1074773118739,25.5115588797814,-54.3128667440592));
#16210=CARTESIAN_POINT('Ctrl Pts',(-26.1086323628434,25.5100519620076,-54.3127487364862));
#16211=CARTESIAN_POINT('Ctrl Pts',(-26.110864918976,25.5071339580292,-54.3125205666545));
#16212=CARTESIAN_POINT('Ctrl Pts',(-26.1119425871162,25.5057230056791,-54.3124103925851));
#16213=CARTESIAN_POINT('Ctrl Pts',(-26.1145109616175,25.5023545579807,-54.3121477321574));
#16214=CARTESIAN_POINT('Ctrl Pts',(-26.1160005959615,25.5003962410827,-54.3119953222756));
#16215=CARTESIAN_POINT('Ctrl Pts',(-26.1204930444195,25.494476279275,-54.3115354678894));
#16216=CARTESIAN_POINT('Ctrl Pts',(-26.1234889543977,25.4905093671582,-54.3112285096602));
#16217=CARTESIAN_POINT('Ctrl Pts',(-26.153790717227,25.4501928925878,-54.3081206674394));
#16218=CARTESIAN_POINT('Ctrl Pts',(-26.180335379242,25.4132740538922,-54.3053721020731));
#16219=CARTESIAN_POINT('Ctrl Pts',(-26.2081617694405,25.3727918051171,-54.3024472332834));
#16220=CARTESIAN_POINT('Ctrl Pts',(-26.2102268809981,25.3697764750768,-54.3022298981055));
#16221=CARTESIAN_POINT('Ctrl Pts',(-26.2227654635382,25.3514015542697,-54.3009086392474));
#16222=CARTESIAN_POINT('Ctrl Pts',(-26.2331112055474,25.3359547848174,-54.2998112867053));
#16223=CARTESIAN_POINT('Ctrl Pts',(-26.4171144503833,25.0560185839087,-54.2801471847028));
#16224=CARTESIAN_POINT('Ctrl Pts',(-26.5510373795378,24.7674481398338,-54.2632735533612));
#16225=CARTESIAN_POINT('Ctrl Pts',(-26.673141057891,24.3544453302687,-54.2384679291315));
#16226=CARTESIAN_POINT('Ctrl Pts',(-26.6996713705618,24.2433004487383,-54.2317531786716));
#16227=CARTESIAN_POINT('Ctrl Pts',(-26.7237305968523,24.1119716651996,-54.2236720722379));
#16228=CARTESIAN_POINT('Ctrl Pts',(-26.7270435125599,24.0929222779478,-54.2224964523209));
#16229=CARTESIAN_POINT('Ctrl Pts',(-26.7311400711194,24.0680426424433,-54.2209561776751));
#16230=CARTESIAN_POINT('Ctrl Pts',(-26.7320794992369,24.0622381615255,-54.2205964849776));
#16231=CARTESIAN_POINT('Ctrl Pts',(-26.7335801070785,24.0528026382245,-54.2200112155008));
#16232=CARTESIAN_POINT('Ctrl Pts',(-26.7341509748491,24.0491731318642,-54.2197859469785));
#16233=CARTESIAN_POINT('Ctrl Pts',(-26.7352345918202,24.0422060271325,-54.2193532626609));
#16234=CARTESIAN_POINT('Ctrl Pts',(-26.7357483048037,24.0388685817391,-54.2191458777921));
#16235=CARTESIAN_POINT('Ctrl Pts',(-26.736907822635,24.0312559758834,-54.2186725711534));
#16236=CARTESIAN_POINT('Ctrl Pts',(-26.7375502703133,24.0269803174432,-54.2184065431678));
#16237=CARTESIAN_POINT('Ctrl Pts',(-26.7395252783619,24.0136536606325,-54.2175767608807));
#16238=CARTESIAN_POINT('Ctrl Pts',(-26.7408278952094,24.0045983316087,-54.2170120578741));
#16239=CARTESIAN_POINT('Ctrl Pts',(-26.7506445087164,23.9342320601815,-54.2126169664548));
#16240=CARTESIAN_POINT('Ctrl Pts',(-26.757428561916,23.8726965365977,-54.208732104771));
#16241=CARTESIAN_POINT('Ctrl Pts',(-26.7628422223502,23.8060067312011,-54.2044730553834));
#16242=CARTESIAN_POINT('Ctrl Pts',(-26.7632364584641,23.8010054318586,-54.2041533613094));
#16243=CARTESIAN_POINT('Ctrl Pts',(-26.7652813814413,23.7742666012615,-54.2024425852595));
#16244=CARTESIAN_POINT('Ctrl Pts',(-26.7667231196907,23.7525140664367,-54.2010452825869));
#16245=CARTESIAN_POINT('Ctrl Pts',(-26.7713625741982,23.6698069936096,-54.1957113297201));
#16246=CARTESIAN_POINT('Ctrl Pts',(-26.7730489237305,23.608783393372,-54.191731846219));
#16247=CARTESIAN_POINT('Ctrl Pts',(-26.7728714384885,23.3800730712408,-54.1766626127112));
#16248=CARTESIAN_POINT('Ctrl Pts',(-26.7596550822314,23.2126720043107,-54.1653045718704));
#16249=CARTESIAN_POINT('Ctrl Pts',(-26.7044156726278,22.8632142067214,-54.1413667466472));
#16250=CARTESIAN_POINT('Ctrl Pts',(-26.6594738075372,22.6821927807123,-54.1288348467689));
#16251=CARTESIAN_POINT('Ctrl Pts',(-26.5954450045766,22.4952402911739,-54.1163823865396));
#16252=CARTESIAN_POINT('Ctrl Pts',(-26.5916866645825,22.4844540286091,-54.1156657957847));
#16253=CARTESIAN_POINT('Ctrl Pts',(-26.5867052295387,22.4703984884452,-54.1147346490989));
#16254=CARTESIAN_POINT('Ctrl Pts',(-26.5855341190207,22.4671110696124,-54.114517054414));
#16255=CARTESIAN_POINT('Ctrl Pts',(-26.5837225009203,22.46205169625,-54.1141824724128));
#16256=CARTESIAN_POINT('Ctrl Pts',(-26.5830857800475,22.4602784034766,-54.114065259137));
#16257=CARTESIAN_POINT('Ctrl Pts',(-26.5818156108227,22.456750661972,-54.1138321922));
#16258=CARTESIAN_POINT('Ctrl Pts',(-26.5811821981013,22.4549962150516,-54.1137163377503));
#16259=CARTESIAN_POINT('Ctrl Pts',(-26.5797645641339,22.4510802545368,-54.113457873606));
#16260=CARTESIAN_POINT('Ctrl Pts',(-26.5789795544314,22.4489190347964,-54.1133153122197));
#16261=CARTESIAN_POINT('Ctrl Pts',(-26.5766734977941,22.4425913146826,-54.112898158414));
#16262=CARTESIAN_POINT('Ctrl Pts',(-26.5751461537557,22.4384270905879,-54.1126239428909));
#16263=CARTESIAN_POINT('Ctrl Pts',(-26.5638572334469,22.4078438864063,-54.1106122181435));
#16264=CARTESIAN_POINT('Ctrl Pts',(-26.5537579086593,22.3815496641164,-54.108894636067));
#16265=CARTESIAN_POINT('Ctrl Pts',(-26.5194848977408,22.2956977234904,-54.1033157277895));
#16266=CARTESIAN_POINT('Ctrl Pts',(-26.4938729247173,22.2367272127551,-54.0995299467616));
#16267=CARTESIAN_POINT('Ctrl Pts',(-26.4022312468814,22.0418944696496,-54.0870528538413));
#16268=CARTESIAN_POINT('Ctrl Pts',(-26.3284184467814,21.9099090050923,-54.0786453077253));
#16269=CARTESIAN_POINT('Ctrl Pts',(-26.1904272751789,21.6993796456838,-54.0645793114023));
#16270=CARTESIAN_POINT('Ctrl Pts',(-26.1313243030524,21.6178134821019,-54.0589486018106));
#16271=CARTESIAN_POINT('Ctrl Pts',(-26.0266007056092,21.486681368543,-54.0494138811664));
#16272=CARTESIAN_POINT('Ctrl Pts',(-25.9830712178427,21.4355377110349,-54.0455622084889));
#16273=CARTESIAN_POINT('Ctrl Pts',(-25.8707981564879,21.3116836032964,-54.0358364942848));
#16274=CARTESIAN_POINT('Ctrl Pts',(-25.8002108937413,21.2407488876991,-54.0298999361944));
#16275=CARTESIAN_POINT('Ctrl Pts',(-25.7195278272604,21.1668830254051,-54.0232418543762));
#16276=CARTESIAN_POINT('Ctrl Pts',(-25.7125831670454,21.160580643764,-54.0226697747992));
#16277=CARTESIAN_POINT('Ctrl Pts',(-25.702241333459,21.1512772702684,-54.0218192855807));
#16278=CARTESIAN_POINT('Ctrl Pts',(-25.6988651344784,21.1482529499561,-54.0215418603151));
#16279=CARTESIAN_POINT('Ctrl Pts',(-25.6930792016495,21.1430920058882,-54.0210668051702));
#16280=CARTESIAN_POINT('Ctrl Pts',(-25.6906726177405,21.1409518469296,-54.0208693240994));
#16281=CARTESIAN_POINT('Ctrl Pts',(-25.6859882413396,21.1367986204205,-54.0204851456695));
#16282=CARTESIAN_POINT('Ctrl Pts',(-25.6837108003061,21.1347851609165,-54.0202984650755));
#16283=CARTESIAN_POINT('Ctrl Pts',(-25.6782628262592,21.1299823853417,-54.019852130622));
#16284=CARTESIAN_POINT('Ctrl Pts',(-25.6750896590907,21.1271960781907,-54.0195923515127));
#16285=CARTESIAN_POINT('Ctrl Pts',(-25.6655808670747,21.1188796028594,-54.018814445408));
#16286=CARTESIAN_POINT('Ctrl Pts',(-25.6592290995492,21.1133680207615,-54.0182955464928));
#16287=CARTESIAN_POINT('Ctrl Pts',(-25.6043765924501,21.0661462599866,-54.0138205947588));
#16288=CARTESIAN_POINT('Ctrl Pts',(-25.5546685121085,21.0258664172482,-54.0098060901969));
#16289=CARTESIAN_POINT('Ctrl Pts',(-25.4250785415863,20.9270976951786,-53.9994302655898));
#16290=CARTESIAN_POINT('Ctrl Pts',(-25.3436445356265,20.8707645571461,-53.9929913648597));
#16291=CARTESIAN_POINT('Ctrl Pts',(-25.0177259591958,20.6668252481455,-53.9675615037369));
#16292=CARTESIAN_POINT('Ctrl Pts',(-24.756674184183,20.5482266875432,-53.9477671583786));
#16293=CARTESIAN_POINT('Ctrl Pts',(-24.4769079329637,20.4635919133481,-53.9286710824796));
#16294=CARTESIAN_POINT('Ctrl Pts',(-24.4703786773796,20.4616392695661,-53.9282266201795));
#16295=CARTESIAN_POINT('Ctrl Pts',(-24.4632035835527,20.4595182525449,-53.9277395528156));
#16296=CARTESIAN_POINT('Ctrl Pts',(-24.4625638782925,20.4593293663158,-53.9276961395058));
#16297=CARTESIAN_POINT('Ctrl Pts',(-24.4532336303569,20.4565775662185,-53.9270631195816));
#16298=CARTESIAN_POINT('Ctrl Pts',(-24.4445322824664,20.4540510867884,-53.9264749585841));
#16299=CARTESIAN_POINT('Ctrl Pts',(-24.4345543327874,20.4511995117115,-53.9258030997667));
#16300=CARTESIAN_POINT('Ctrl Pts',(-24.4332881398974,20.4508384885672,-53.9257178892359));
#16301=CARTESIAN_POINT('Ctrl Pts',(-24.4252426810515,20.4485498581434,-53.9251767616788));
#16302=CARTESIAN_POINT('Ctrl Pts',(-24.4184572699734,20.4466437015135,-53.9247217579067));
#16303=CARTESIAN_POINT('Ctrl Pts',(-24.3731273895862,20.4340699314905,-53.9216915176154));
#16304=CARTESIAN_POINT('Ctrl Pts',(-24.3343912753339,20.424097732735,-53.9191473817995));
#16305=CARTESIAN_POINT('Ctrl Pts',(-24.2902953251472,20.4136169778787,-53.9163100795311));
#16306=CARTESIAN_POINT('Ctrl Pts',(-24.2851101449787,20.4123981337387,-53.915977362568));
#16307=CARTESIAN_POINT('Ctrl Pts',(-24.277534453801,20.4106371768667,-53.9154926168509));
#16308=CARTESIAN_POINT('Ctrl Pts',(-24.2751463429577,20.4100849353739,-53.9153400063549));
#16309=CARTESIAN_POINT('Ctrl Pts',(-24.2709622100026,20.4091223981143,-53.9150729711244));
#16310=CARTESIAN_POINT('Ctrl Pts',(-24.2691664648354,20.4087109175665,-53.9149584775118));
#16311=CARTESIAN_POINT('Ctrl Pts',(-24.2654231311523,20.4078565405154,-53.9147200445019));
#16312=CARTESIAN_POINT('Ctrl Pts',(-24.2634754872032,20.4074139154918,-53.9145961211379));
#16313=CARTESIAN_POINT('Ctrl Pts',(-24.2595002706259,20.4065143862533,-53.9143434568099));
#16314=CARTESIAN_POINT('Ctrl Pts',(-24.2574726644909,20.4060576321841,-53.9142147245971));
#16315=CARTESIAN_POINT('Ctrl Pts',(-24.2525061298565,20.4049438798658,-53.9138997455623));
#16316=CARTESIAN_POINT('Ctrl Pts',(-24.2495667123517,20.4042890372614,-53.9137136225797));
#16317=CARTESIAN_POINT('Ctrl Pts',(-24.2414884065767,20.4025012360297,-53.9132029082083));
#16318=CARTESIAN_POINT('Ctrl Pts',(-24.2363476263804,20.401376736106,-53.9128787959768));
#16319=CARTESIAN_POINT('Ctrl Pts',(-24.0503380479243,20.3611659413888,-53.9011828202846));
#16320=CARTESIAN_POINT('Ctrl Pts',(-23.866408765732,20.337710451219,-53.8906825218747));
#16321=CARTESIAN_POINT('Ctrl Pts',(-23.3713358513392,20.317538285856,-53.8628958954641));
#16322=CARTESIAN_POINT('Ctrl Pts',(-23.0610612513995,20.3497645498736,-53.8458092008685));
#16323=CARTESIAN_POINT('Ctrl Pts',(-22.7420104950499,20.4304426213078,-53.8258881001028));
#16324=CARTESIAN_POINT('Ctrl Pts',(-22.7238749286448,20.4351972993127,-53.8247481798572));
#16325=CARTESIAN_POINT('Ctrl Pts',(-22.6999441805584,20.4416950100567,-53.8232336485858));
#16326=CARTESIAN_POINT('Ctrl Pts',(-22.6941106933179,20.4432965762398,-53.8228636418414));
#16327=CARTESIAN_POINT('Ctrl Pts',(-22.6850626728558,20.4458080996332,-53.822288463435));
#16328=CARTESIAN_POINT('Ctrl Pts',(-22.68184496556,20.446706652778,-53.8220836635893));
#16329=CARTESIAN_POINT('Ctrl Pts',(-22.6754063218675,20.4485154579454,-53.8216733518423));
#16330=CARTESIAN_POINT('Ctrl Pts',(-22.672185394741,20.4494257276973,-53.8214678395778));
#16331=CARTESIAN_POINT('Ctrl Pts',(-22.6649988691765,20.451468814688,-53.821008730998));
#16332=CARTESIAN_POINT('Ctrl Pts',(-22.6610340206476,20.452604228361,-53.8207550501648));
#16333=CARTESIAN_POINT('Ctrl Pts',(-22.6494486487209,20.4559460072104,-53.8200126483842));
#16334=CARTESIAN_POINT('Ctrl Pts',(-22.6418341206175,20.4581728930602,-53.8195232570967));
#16335=CARTESIAN_POINT('Ctrl Pts',(-22.5862191318852,20.4746607855187,-53.8159381606937));
#16336=CARTESIAN_POINT('Ctrl Pts',(-22.5385509000267,20.4900100024995,-53.8128069140744));
#16337=CARTESIAN_POINT('Ctrl Pts',(-22.3844087746391,20.5436389051829,-53.8024819838771));
#16338=CARTESIAN_POINT('Ctrl Pts',(-22.2795990037145,20.5864117902428,-53.7951428469154));
#16339=CARTESIAN_POINT('Ctrl Pts',(-21.943420816368,20.7447191109677,-53.770568848282));
#16340=CARTESIAN_POINT('Ctrl Pts',(-21.7236990882241,20.8825547101724,-53.7527419670825));
#16341=CARTESIAN_POINT('Ctrl Pts',(-21.4524167307334,21.102109792908,-53.7296528279958));
#16342=CARTESIAN_POINT('Ctrl Pts',(-21.3844501649853,21.1620269118271,-53.7237720500036));
#16343=CARTESIAN_POINT('Ctrl Pts',(-21.3144569892859,21.2291801283998,-53.7176911851176));
#16344=CARTESIAN_POINT('Ctrl Pts',(-21.3098359272546,21.2336402963337,-53.7172895999336));
#16345=CARTESIAN_POINT('Ctrl Pts',(-21.3034494227692,21.2398414212685,-53.7167344699961));
#16346=CARTESIAN_POINT('Ctrl Pts',(-21.3016726499497,21.2415706079618,-53.7165800155729));
#16347=CARTESIAN_POINT('Ctrl Pts',(-21.2986233788433,21.2445450718343,-53.7163149234124));
#16348=CARTESIAN_POINT('Ctrl Pts',(-21.2973499173736,21.2457893528076,-53.7162042075203));
#16349=CARTESIAN_POINT('Ctrl Pts',(-21.2947498844039,21.2483340228526,-53.7159781474176));
#16350=CARTESIAN_POINT('Ctrl Pts',(-21.2934234087759,21.249634500981,-53.7158628112706));
#16351=CARTESIAN_POINT('Ctrl Pts',(-21.2903300971001,21.2526724367763,-53.7155938350396));
#16352=CARTESIAN_POINT('Ctrl Pts',(-21.2885641348045,21.2544107909772,-53.7154402658708));
#16353=CARTESIAN_POINT('Ctrl Pts',(-21.284841350213,21.258083839506,-53.7151165014098));
#16354=CARTESIAN_POINT('Ctrl Pts',(-21.2828849957527,21.2600190082909,-53.7149463436172));
#16355=CARTESIAN_POINT('Ctrl Pts',(-21.2776468026401,21.2652137665911,-53.7144906881227));
#16356=CARTESIAN_POINT('Ctrl Pts',(-21.2743694837242,21.2684779349518,-53.7142055472385));
#16357=CARTESIAN_POINT('Ctrl Pts',(-21.196941731958,21.3459277746352,-53.7074673264598));
#16358=CARTESIAN_POINT('Ctrl Pts',(-21.1264407299458,21.4236916997899,-53.701294987091));
#16359=CARTESIAN_POINT('Ctrl Pts',(-20.8112954570304,21.8073842075662,-53.672744741342));
#16360=CARTESIAN_POINT('Ctrl Pts',(-20.6199783799416,22.1527512741779,-53.6519673604469));
#16361=CARTESIAN_POINT('Ctrl Pts',(-20.4891070038943,22.5423442634338,-53.6270974871756));
#16362=CARTESIAN_POINT('Ctrl Pts',(-20.4831182953728,22.5607180094763,-53.6259227552702));
#16363=CARTESIAN_POINT('Ctrl Pts',(-20.4754502655289,22.584982581198,-53.6243686209678));
#16364=CARTESIAN_POINT('Ctrl Pts',(-20.473621887071,22.590826177515,-53.6239941311172));
#16365=CARTESIAN_POINT('Ctrl Pts',(-20.4708172786213,22.5998803177259,-53.6234135545696));
#16366=CARTESIAN_POINT('Ctrl Pts',(-20.4698293844633,22.6030872574051,-53.6232078513257));
#16367=CARTESIAN_POINT('Ctrl Pts',(-20.4679646195898,22.6091745038532,-53.6228172697673));
#16368=CARTESIAN_POINT('Ctrl Pts',(-20.4670867724079,22.6120545098145,-53.62263242373));
#16369=CARTESIAN_POINT('Ctrl Pts',(-20.4650656129891,22.6187189208838,-53.6222045591596));
#16370=CARTESIAN_POINT('Ctrl Pts',(-20.4639252275865,22.6225042020733,-53.6219614449882));
#16371=CARTESIAN_POINT('Ctrl Pts',(-20.4607459435362,22.6331279350019,-53.6212788549182));
#16372=CARTESIAN_POINT('Ctrl Pts',(-20.458722797967,22.6399710431983,-53.6208388639674));
#16373=CARTESIAN_POINT('Ctrl Pts',(-20.4471157125049,22.6797160134874,-53.618281517893));
#16374=CARTESIAN_POINT('Ctrl Pts',(-20.4380346299818,22.712761317348,-53.6161478099673));
#16375=CARTESIAN_POINT('Ctrl Pts',(-20.4133275438689,22.8086264552958,-53.6099338946471));
#16376=CARTESIAN_POINT('Ctrl Pts',(-20.3990657646876,22.8717773208185,-53.6058106594238));
#16377=CARTESIAN_POINT('Ctrl Pts',(-20.3491161911391,23.1287405978441,-53.5889063927086));
#16378=CARTESIAN_POINT('Ctrl Pts',(-20.3293407977036,23.3251866418383,-53.5756600584079));
#16379=CARTESIAN_POINT('Ctrl Pts',(-20.3260069066221,23.7079112193692,-53.5497530684138));
#16380=CARTESIAN_POINT('Ctrl Pts',(-20.3404482932774,23.8934516875078,-53.5371588048765));
#16381=CARTESIAN_POINT('Ctrl Pts',(-20.3763315967665,24.1101556323566,-53.5230678284819));
#16382=CARTESIAN_POINT('Ctrl Pts',(-20.3823938050241,24.1434952293927,-53.5209182514212));
#16383=CARTESIAN_POINT('Ctrl Pts',(-20.3899678458289,24.181714358312,-53.5184799692282));
#16384=CARTESIAN_POINT('Ctrl Pts',(-20.3909664742216,24.1866917998807,-53.5181629286902));
#16385=CARTESIAN_POINT('Ctrl Pts',(-20.3924552144743,24.1940222438682,-53.517696781677));
#16386=CARTESIAN_POINT('Ctrl Pts',(-20.3929361976369,24.1963770597373,-53.517547154681));
#16387=CARTESIAN_POINT('Ctrl Pts',(-20.3937866896582,24.2005173045439,-53.5172842886015));
#16388=CARTESIAN_POINT('Ctrl Pts',(-20.3941550794573,24.2023029582712,-53.5171709849542));
#16389=CARTESIAN_POINT('Ctrl Pts',(-20.3949340234267,24.2060625184211,-53.5169325774556));
#16390=CARTESIAN_POINT('Ctrl Pts',(-20.395344913707,24.2080363482531,-53.5168074935211));
#16391=CARTESIAN_POINT('Ctrl Pts',(-20.3964170680846,24.2131626358478,-53.516482849408));
#16392=CARTESIAN_POINT('Ctrl Pts',(-20.3970812086777,24.2163145000074,-53.5162834552192));
#16393=CARTESIAN_POINT('Ctrl Pts',(-20.3985411449705,24.2231919124203,-53.5158488246908));
#16394=CARTESIAN_POINT('Ctrl Pts',(-20.3993388247125,24.2269170621973,-53.5156136958505));
#16395=CARTESIAN_POINT('Ctrl Pts',(-20.4016851109997,24.2377800631558,-53.5149288502816));
#16396=CARTESIAN_POINT('Ctrl Pts',(-20.4032513922171,24.2449141325495,-53.514480123853));
#16397=CARTESIAN_POINT('Ctrl Pts',(-20.4086958305296,24.269315997934,-53.5129486150132));
#16398=CARTESIAN_POINT('Ctrl Pts',(-20.4126920462991,24.2865575007053,-53.5118722478569));
#16399=CARTESIAN_POINT('Ctrl Pts',(-20.4249737830639,24.3376300935813,-53.5086985548476));
#16400=CARTESIAN_POINT('Ctrl Pts',(-20.4336661736083,24.3713617577029,-53.5066216683911));
#16401=CARTESIAN_POINT('Ctrl Pts',(-20.4636689408993,24.4804405289553,-53.4999486693077));
#16402=CARTESIAN_POINT('Ctrl Pts',(-20.487179472856,24.5551569957334,-53.4954448115822));
#16403=CARTESIAN_POINT('Ctrl Pts',(-20.6334131949401,24.96685062181,-53.4706361289332));
#16404=CARTESIAN_POINT('Ctrl Pts',(-20.8089694298932,25.2823248171282,-53.4513217656664));
#16405=CARTESIAN_POINT('Ctrl Pts',(-21.0456445942043,25.5784230467081,-53.428399033085));
#16406=CARTESIAN_POINT('Ctrl Pts',(-21.0585768309744,25.5942898921396,-53.4271552459239));
#16407=CARTESIAN_POINT('Ctrl Pts',(-21.0756623826746,25.6148494388306,-53.425522854127));
#16408=CARTESIAN_POINT('Ctrl Pts',(-21.0796796649199,25.6196549825639,-53.4251398034008));
#16409=CARTESIAN_POINT('Ctrl Pts',(-21.085888884203,25.6270387091446,-53.4245489178817));
#16410=CARTESIAN_POINT('Ctrl Pts',(-21.0880709310687,25.6296252205906,-53.4243414891867));
#16411=CARTESIAN_POINT('Ctrl Pts',(-21.0924166666606,25.634760051124,-53.4239288120978));
#16412=CARTESIAN_POINT('Ctrl Pts',(-21.0945802548203,25.6373084500786,-53.423723567992));
#16413=CARTESIAN_POINT('Ctrl Pts',(-21.0993741784553,25.642937235037,-53.4232692709236));
#16414=CARTESIAN_POINT('Ctrl Pts',(-21.1020063610934,25.6460160340674,-53.4230201418249));
#16415=CARTESIAN_POINT('Ctrl Pts',(-21.1095847778396,25.6548465603615,-53.4223037480969));
#16416=CARTESIAN_POINT('Ctrl Pts',(-21.1145455004807,25.6605857676378,-53.4218358830612));
#16417=CARTESIAN_POINT('Ctrl Pts',(-21.1473021876072,25.6982135898575,-53.4187534375171));
#16418=CARTESIAN_POINT('Ctrl Pts',(-21.175702351635,25.7295685323623,-53.4161136640281));
#16419=CARTESIAN_POINT('Ctrl Pts',(-21.2613019078646,25.8204138387044,-53.408247043888));
#16420=CARTESIAN_POINT('Ctrl Pts',(-21.3201748464876,25.8782729101019,-53.4029490762581));
#16421=CARTESIAN_POINT('Ctrl Pts',(-21.5091359729717,26.0502291560515,-53.3862780052529));
#16422=CARTESIAN_POINT('Ctrl Pts',(-21.6462265176142,26.1561522626448,-53.3746224107306));
#16423=CARTESIAN_POINT('Ctrl Pts',(-21.8829307188597,26.3103535255527,-53.3554996505573));
#16424=CARTESIAN_POINT('Ctrl Pts',(-21.9776883720614,26.3654164988903,-53.3480832981571));
#16425=CARTESIAN_POINT('Ctrl Pts',(-22.0750361378578,26.4155368376325,-53.3407994113682));
#16426=CARTESIAN_POINT('Origin',(-23.5502525316942,23.5502525316942,-77.3107734492734));
#16427=CARTESIAN_POINT('',(-22.0750360141197,26.4155367739249,-51.843225903739));
#16428=CARTESIAN_POINT('',(-22.0750360382923,26.4155367863703,-52.0916569661403));
#16429=CARTESIAN_POINT('',(-22.0750360153461,26.4155367745563,-77.3107734492734));
#16430=CARTESIAN_POINT('Ctrl Pts',(-22.0750360141197,26.4155367739249,-51.843225903739));
#16431=CARTESIAN_POINT('Ctrl Pts',(-21.9897252008207,26.3716137595686,-51.8491828204502));
#16432=CARTESIAN_POINT('Ctrl Pts',(-21.9064243545153,26.3239056399464,-51.8552739078288));
#16433=CARTESIAN_POINT('Ctrl Pts',(-21.6581627873809,26.1666051315619,-51.8743120026963));
#16434=CARTESIAN_POINT('Ctrl Pts',(-21.5010827181033,26.0454858121205,-51.8876515832146));
#16435=CARTESIAN_POINT('Ctrl Pts',(-21.3324303570035,25.8887197230501,-51.903238253001));
#16436=CARTESIAN_POINT('Ctrl Pts',(-21.3090694962334,25.8663403152383,-51.9054276913812));
#16437=CARTESIAN_POINT('Ctrl Pts',(-21.2593355203793,25.8172386467926,-51.9101504072627));
#16438=CARTESIAN_POINT('Ctrl Pts',(-21.2330840939308,25.7903992470983,-51.9126821562577));
#16439=CARTESIAN_POINT('Ctrl Pts',(-21.1700493475658,25.7236587703121,-51.9188478690153));
#16440=CARTESIAN_POINT('Ctrl Pts',(-21.1337922148937,25.6832742995709,-51.9224696713775));
#16441=CARTESIAN_POINT('Ctrl Pts',(-21.0594741343531,25.5961677222589,-51.9300262087061));
#16442=CARTESIAN_POINT('Ctrl Pts',(-21.0216670562994,25.5492529042601,-51.9339501625412));
#16443=CARTESIAN_POINT('Ctrl Pts',(-20.9685029937478,25.4793577874751,-51.9395559324807));
#16444=CARTESIAN_POINT('Ctrl Pts',(-20.9520926830516,25.4571985955911,-51.9412993492558));
#16445=CARTESIAN_POINT('Ctrl Pts',(-20.9333886366962,25.4312523656387,-51.9432992499837));
#16446=CARTESIAN_POINT('Ctrl Pts',(-20.9308164781452,25.4276687833987,-51.9435745612431));
#16447=CARTESIAN_POINT('Ctrl Pts',(-20.9269177495744,25.4222133877612,-51.9439922856942));
#16448=CARTESIAN_POINT('Ctrl Pts',(-20.9255858204508,25.4203454386633,-51.9441350691902));
#16449=CARTESIAN_POINT('Ctrl Pts',(-20.9231748030695,25.4169564846848,-51.9443936663633));
#16450=CARTESIAN_POINT('Ctrl Pts',(-20.9220950438886,25.4154359703113,-51.9445095265595));
#16451=CARTESIAN_POINT('Ctrl Pts',(-20.9199253686315,25.4123750138554,-51.9447424354619));
#16452=CARTESIAN_POINT('Ctrl Pts',(-20.9188354900929,25.4108345579781,-51.944859481547));
#16453=CARTESIAN_POINT('Ctrl Pts',(-20.9157254645338,25.4064305876901,-51.9451936259339));
#16454=CARTESIAN_POINT('Ctrl Pts',(-20.9137086263029,25.403564722984,-51.9454104950953));
#16455=CARTESIAN_POINT('Ctrl Pts',(-20.9050673861997,25.3912431349876,-51.9463404740839));
#16456=CARTESIAN_POINT('Ctrl Pts',(-20.898489040387,25.3817549889842,-51.9470504502894));
#16457=CARTESIAN_POINT('Ctrl Pts',(-20.7860458814144,25.2176989716584,-51.9592247010205));
#16458=CARTESIAN_POINT('Ctrl Pts',(-20.6937888496416,25.054198587208,-51.9698193448342));
#16459=CARTESIAN_POINT('Ctrl Pts',(-20.5470902481273,24.7313880586405,-51.9896829837105));
#16460=CARTESIAN_POINT('Ctrl Pts',(-20.4898754918806,24.5740469823723,-51.9989449943794));
#16461=CARTESIAN_POINT('Ctrl Pts',(-20.4174652679603,24.3134282391892,-52.0144101571945));
#16462=CARTESIAN_POINT('Ctrl Pts',(-20.3946115001361,24.212611894009,-52.0204176289292));
#16463=CARTESIAN_POINT('Ctrl Pts',(-20.3711876067405,24.0800130107133,-52.0284466491232));
#16464=CARTESIAN_POINT('Ctrl Pts',(-20.3661858877997,24.0490706005728,-52.0303289482654));
#16465=CARTESIAN_POINT('Ctrl Pts',(-20.3597386947076,24.0051260647856,-52.0330165033216));
#16466=CARTESIAN_POINT('Ctrl Pts',(-20.3579197375424,23.9921798998042,-52.0338100125468));
#16467=CARTESIAN_POINT('Ctrl Pts',(-20.3552686898538,23.9724404612225,-52.0350226973708));
#16468=CARTESIAN_POINT('Ctrl Pts',(-20.3543793705177,23.9656549077074,-52.0354400675312));
#16469=CARTESIAN_POINT('Ctrl Pts',(-20.3529617851044,23.9545646066039,-52.0361230559527));
#16470=CARTESIAN_POINT('Ctrl Pts',(-20.3524205803886,23.9502615104261,-52.0363882652948));
#16471=CARTESIAN_POINT('Ctrl Pts',(-20.3513944330748,23.9419674666286,-52.0368998481531));
#16472=CARTESIAN_POINT('Ctrl Pts',(-20.3509082687275,23.9379766760756,-52.0371461825928));
#16473=CARTESIAN_POINT('Ctrl Pts',(-20.3500388952779,23.9307272475163,-52.0375939885858));
#16474=CARTESIAN_POINT('Ctrl Pts',(-20.3496531920863,23.9274689089441,-52.0377953810238));
#16475=CARTESIAN_POINT('Ctrl Pts',(-20.348885817436,23.9209003785849,-52.0382016167838));
#16476=CARTESIAN_POINT('Ctrl Pts',(-20.3485043026032,23.9175901733081,-52.0384064647653));
#16477=CARTESIAN_POINT('Ctrl Pts',(-20.3474494219307,23.9083110246299,-52.0389810492121));
#16478=CARTESIAN_POINT('Ctrl Pts',(-20.3467876120111,23.9023408045063,-52.0393511502678));
#16479=CARTESIAN_POINT('Ctrl Pts',(-20.3441639192748,23.8780524339338,-52.0408585179082));
#16480=CARTESIAN_POINT('Ctrl Pts',(-20.3423424669538,23.8597197519963,-52.0420002074042));
#16481=CARTESIAN_POINT('Ctrl Pts',(-20.3047465426246,23.4452280871383,-52.0679056645925));
#16482=CARTESIAN_POINT('Ctrl Pts',(-20.342484646457,23.0459015224298,-52.0954040832944));
#16483=CARTESIAN_POINT('Ctrl Pts',(-20.4601889674045,22.6345309650722,-52.1238185283854));
#16484=CARTESIAN_POINT('Ctrl Pts',(-20.4689505687567,22.6054683581212,-52.1258229624494));
#16485=CARTESIAN_POINT('Ctrl Pts',(-20.4921373287184,22.5323130346386,-52.1308540328354));
#16486=CARTESIAN_POINT('Ctrl Pts',(-20.5071069139545,22.4883981877375,-52.1338608174364));
#16487=CARTESIAN_POINT('Ctrl Pts',(-20.5322463792029,22.4195536727348,-52.138537026662));
#16488=CARTESIAN_POINT('Ctrl Pts',(-20.5417888464796,22.3944033125974,-52.140237295623));
#16489=CARTESIAN_POINT('Ctrl Pts',(-20.5532514083243,22.3652963983011,-52.1421931967453));
#16490=CARTESIAN_POINT('Ctrl Pts',(-20.5548656844681,22.3612216626441,-52.1424667354106));
#16491=CARTESIAN_POINT('Ctrl Pts',(-20.5573354074835,22.3550245676376,-52.1428823207265));
#16492=CARTESIAN_POINT('Ctrl Pts',(-20.5581848023828,22.3528998260356,-52.1430247319413));
#16493=CARTESIAN_POINT('Ctrl Pts',(-20.5597304440604,22.349045354493,-52.1432829369131));
#16494=CARTESIAN_POINT('Ctrl Pts',(-20.5604259266889,22.3473153299918,-52.1433987764799));
#16495=CARTESIAN_POINT('Ctrl Pts',(-20.5618296211566,22.3438323542216,-52.1436318857657));
#16496=CARTESIAN_POINT('Ctrl Pts',(-20.5625378712267,22.3420794296466,-52.1437491524705));
#16497=CARTESIAN_POINT('Ctrl Pts',(-20.564569989419,22.3370626353142,-52.1440846146279));
#16498=CARTESIAN_POINT('Ctrl Pts',(-20.5658976714384,22.3338002982404,-52.1443025780325));
#16499=CARTESIAN_POINT('Ctrl Pts',(-20.5716570002939,22.3197148436768,-52.1452428963538));
#16500=CARTESIAN_POINT('Ctrl Pts',(-20.5761422682075,22.3089135401885,-52.1459620310379));
#16501=CARTESIAN_POINT('Ctrl Pts',(-20.654939354486,22.1220353305908,-52.1583743839588));
#16502=CARTESIAN_POINT('Ctrl Pts',(-20.7447228958645,21.9528578399593,-52.1691635097813));
#16503=CARTESIAN_POINT('Ctrl Pts',(-20.9394544635006,21.6535801689934,-52.1891557525925));
#16504=CARTESIAN_POINT('Ctrl Pts',(-21.0405191250805,21.5217386785778,-52.1983528940377));
#16505=CARTESIAN_POINT('Ctrl Pts',(-21.2384687196092,21.3010698415384,-52.2153168950063));
#16506=CARTESIAN_POINT('Ctrl Pts',(-21.3314759240079,21.209271686118,-52.2229525751332));
#16507=CARTESIAN_POINT('Ctrl Pts',(-21.4402111670143,21.1142651248949,-52.2316838032351));
#16508=CARTESIAN_POINT('Ctrl Pts',(-21.450694459463,21.1052238817975,-52.2325236274529));
#16509=CARTESIAN_POINT('Ctrl Pts',(-21.4666692723492,21.0916250111101,-52.2338005809751));
#16510=CARTESIAN_POINT('Ctrl Pts',(-21.4721183045839,21.0870175416003,-52.2342356631949));
#16511=CARTESIAN_POINT('Ctrl Pts',(-21.4809978343844,21.0795598247708,-52.2349438859574));
#16512=CARTESIAN_POINT('Ctrl Pts',(-21.4844190457172,21.0766985172679,-52.2352165738291));
#16513=CARTESIAN_POINT('Ctrl Pts',(-21.491006537872,21.0712123111909,-52.235741281866));
#16514=CARTESIAN_POINT('Ctrl Pts',(-21.4941719274317,21.0685863521945,-52.2359932581151));
#16515=CARTESIAN_POINT('Ctrl Pts',(-21.4998777746368,21.063871278455,-52.2364471914248));
#16516=CARTESIAN_POINT('Ctrl Pts',(-21.5024164243122,21.0617799764888,-52.2366490591153));
#16517=CARTESIAN_POINT('Ctrl Pts',(-21.507498903764,21.0576061496168,-52.2370530156704));
#16518=CARTESIAN_POINT('Ctrl Pts',(-21.5100427275968,21.0555236234488,-52.2372551041527));
#16519=CARTESIAN_POINT('Ctrl Pts',(-21.5162902270514,21.0504249936557,-52.2377511925007));
#16520=CARTESIAN_POINT('Ctrl Pts',(-21.5199974217612,21.0474132310497,-52.2380453675553));
#16521=CARTESIAN_POINT('Ctrl Pts',(-21.5343171886579,21.0358324573817,-52.2391809264116));
#16522=CARTESIAN_POINT('Ctrl Pts',(-21.5449773086083,21.0273227094656,-52.2400246922209));
#16523=CARTESIAN_POINT('Ctrl Pts',(-21.719412853081,20.8898784734723,-52.2538070117694));
#16524=CARTESIAN_POINT('Ctrl Pts',(-21.8952302253688,20.7770892030371,-52.2673982957861));
#16525=CARTESIAN_POINT('Ctrl Pts',(-22.3317136485808,20.5534462080759,-52.3002945542933));
#16526=CARTESIAN_POINT('Ctrl Pts',(-22.5985599684848,20.4583309506143,-52.3198244506153));
#16527=CARTESIAN_POINT('Ctrl Pts',(-22.8913962245674,20.3955213901073,-52.3387921392178));
#16528=CARTESIAN_POINT('Ctrl Pts',(-22.9084358211156,20.3920106866872,-52.339886846749));
#16529=CARTESIAN_POINT('Ctrl Pts',(-22.9292935334166,20.3878891100563,-52.34121518554));
#16530=CARTESIAN_POINT('Ctrl Pts',(-22.9330849734733,20.3871469859516,-52.3414561763064));
#16531=CARTESIAN_POINT('Ctrl Pts',(-22.9390141573438,20.385997493308,-52.3418323017199));
#16532=CARTESIAN_POINT('Ctrl Pts',(-22.9411509788286,20.3855854723347,-52.3419677027523));
#16533=CARTESIAN_POINT('Ctrl Pts',(-22.9449351718859,20.3848597806119,-52.342207221219));
#16534=CARTESIAN_POINT('Ctrl Pts',(-22.946582361976,20.3845452330153,-52.3423113887773));
#16535=CARTESIAN_POINT('Ctrl Pts',(-22.9501091314918,20.3838746134338,-52.3425342267347));
#16536=CARTESIAN_POINT('Ctrl Pts',(-22.9519887773019,20.3835189302869,-52.3426528743032));
#16537=CARTESIAN_POINT('Ctrl Pts',(-22.9574394497188,20.3824925322029,-52.342996596076));
#16538=CARTESIAN_POINT('Ctrl Pts',(-22.9610113100484,20.3818261797711,-52.3432214196375));
#16539=CARTESIAN_POINT('Ctrl Pts',(-22.9770459874685,20.3788628651033,-52.3442288390815));
#16540=CARTESIAN_POINT('Ctrl Pts',(-22.9895213833982,20.3766333435147,-52.3450076217711));
#16541=CARTESIAN_POINT('Ctrl Pts',(-23.004438624141,20.3740581397258,-52.345933202787));
#16542=CARTESIAN_POINT('Ctrl Pts',(-23.0068678884837,20.3736416384814,-52.3460837548937));
#16543=CARTESIAN_POINT('Ctrl Pts',(-23.3467094626337,20.3157765020713,-52.3671205951503));
#16544=CARTESIAN_POINT('Ctrl Pts',(-23.6911834829049,20.3124289569336,-52.3852323126893));
#16545=CARTESIAN_POINT('Ctrl Pts',(-24.1691752316573,20.3843526014788,-52.4127896196593));
#16546=CARTESIAN_POINT('Ctrl Pts',(-24.307024525732,20.4144470088828,-52.4210040176603));
#16547=CARTESIAN_POINT('Ctrl Pts',(-24.4563526907502,20.4574690974191,-52.4303956750595));
#16548=CARTESIAN_POINT('Ctrl Pts',(-24.4702273715643,20.4615678354165,-52.4312729865578));
#16549=CARTESIAN_POINT('Ctrl Pts',(-24.4911277564164,20.467895366672,-52.4326018228255));
#16550=CARTESIAN_POINT('Ctrl Pts',(-24.4981743082336,20.470055105326,-52.433051093483));
#16551=CARTESIAN_POINT('Ctrl Pts',(-24.5095669990655,20.4735897139678,-52.4337795189083));
#16552=CARTESIAN_POINT('Ctrl Pts',(-24.5139177656754,20.4749496754266,-52.434058184442));
#16553=CARTESIAN_POINT('Ctrl Pts',(-24.5222525394739,20.4775743807511,-52.4345929639074));
#16554=CARTESIAN_POINT('Ctrl Pts',(-24.5262370027428,20.4788376547331,-52.4348490290793));
#16555=CARTESIAN_POINT('Ctrl Pts',(-24.5333604078968,20.4811113912041,-52.4353075634865));
#16556=CARTESIAN_POINT('Ctrl Pts',(-24.5365002833747,20.4821189282351,-52.435509936033));
#16557=CARTESIAN_POINT('Ctrl Pts',(-24.5427366890625,20.4841306559697,-52.4359124034262));
#16558=CARTESIAN_POINT('Ctrl Pts',(-24.5458332555072,20.4851347229186,-52.4361124939945));
#16559=CARTESIAN_POINT('Ctrl Pts',(-24.554275001186,20.4878861154398,-52.4366586673345));
#16560=CARTESIAN_POINT('Ctrl Pts',(-24.5596171181777,20.4896427366438,-52.4370050569881));
#16561=CARTESIAN_POINT('Ctrl Pts',(-24.5798305218702,20.4963480849113,-52.4383186182582));
#16562=CARTESIAN_POINT('Ctrl Pts',(-24.5946700478352,20.5013912285266,-52.4392889116558));
#16563=CARTESIAN_POINT('Ctrl Pts',(-24.8402609170771,20.5868575217609,-52.4554477012355));
#16564=CARTESIAN_POINT('Ctrl Pts',(-25.0611159308266,20.6931428451765,-52.4715512658913));
#16565=CARTESIAN_POINT('Ctrl Pts',(-25.3406135075725,20.8691837669334,-52.4938488210193));
#16566=CARTESIAN_POINT('Ctrl Pts',(-25.4115582344226,20.9179411652825,-52.4996864150406));
#16567=CARTESIAN_POINT('Ctrl Pts',(-25.5578974997907,21.0273913277006,-52.5120268035928));
#16568=CARTESIAN_POINT('Ctrl Pts',(-25.6326877518089,21.0887625961928,-52.5185168119012));
#16569=CARTESIAN_POINT('Ctrl Pts',(-25.7433796948718,21.1882558328908,-52.528291164311));
#16570=CARTESIAN_POINT('Ctrl Pts',(-25.7813018413411,21.2240421328298,-52.5316725871852));
#16571=CARTESIAN_POINT('Ctrl Pts',(-25.8360688989308,21.2782965947794,-52.5365841110802));
#16572=CARTESIAN_POINT('Ctrl Pts',(-25.8535926224181,21.2960642600643,-52.5381600798178));
#16573=CARTESIAN_POINT('Ctrl Pts',(-25.8738898504716,21.317127897949,-52.5399887744974));
#16574=CARTESIAN_POINT('Ctrl Pts',(-25.8768646884681,21.3202274440512,-52.5402568790687));
#16575=CARTESIAN_POINT('Ctrl Pts',(-25.8814018233075,21.3249737412854,-52.5406658999291));
#16576=CARTESIAN_POINT('Ctrl Pts',(-25.8829685783858,21.3266161944267,-52.5408071634393));
#16577=CARTESIAN_POINT('Ctrl Pts',(-25.8858065491106,21.3295975826021,-52.5410630798228));
#16578=CARTESIAN_POINT('Ctrl Pts',(-25.887078344656,21.3309359496986,-52.5411777780651));
#16579=CARTESIAN_POINT('Ctrl Pts',(-25.8896545006017,21.3336516229519,-52.5414101378102));
#16580=CARTESIAN_POINT('Ctrl Pts',(-25.8909587899795,21.3350289824253,-52.5415277938618));
#16581=CARTESIAN_POINT('Ctrl Pts',(-25.8947029085371,21.3389898561432,-52.5418655826252));
#16582=CARTESIAN_POINT('Ctrl Pts',(-25.8971396916499,21.3415762655819,-52.542085478115));
#16583=CARTESIAN_POINT('Ctrl Pts',(-25.9077619801233,21.3528882241219,-52.5430442924238));
#16584=CARTESIAN_POINT('Ctrl Pts',(-25.9159032763121,21.3616554320201,-52.5437798329132));
#16585=CARTESIAN_POINT('Ctrl Pts',(-25.9265323813206,21.3732303213727,-52.5447413505369));
#16586=CARTESIAN_POINT('Ctrl Pts',(-25.9290642424426,21.3759971480993,-52.5449704759604));
#16587=CARTESIAN_POINT('Ctrl Pts',(-25.9371213820002,21.3848329385137,-52.5456999370996));
#16588=CARTESIAN_POINT('Ctrl Pts',(-25.9426283600538,21.3909186477939,-52.5461989916147));
#16589=CARTESIAN_POINT('Ctrl Pts',(-25.9515706219715,21.4008768579321,-52.5470102665101));
#16590=CARTESIAN_POINT('Ctrl Pts',(-25.9550198898244,21.4047366702608,-52.5473234190469));
#16591=CARTESIAN_POINT('Ctrl Pts',(-25.9613889897607,21.4118984985006,-52.547902107237));
#16592=CARTESIAN_POINT('Ctrl Pts',(-25.9643113698717,21.4151982192778,-52.5481678074542));
#16593=CARTESIAN_POINT('Ctrl Pts',(-26.0355839570571,21.4960070087032,-52.5546524745252));
#16594=CARTESIAN_POINT('Ctrl Pts',(-26.1001804532907,21.5767610259256,-52.5606348081874));
#16595=CARTESIAN_POINT('Ctrl Pts',(-26.2810209898571,21.8265756214034,-52.5781747548292));
#16596=CARTESIAN_POINT('Ctrl Pts',(-26.3851290912829,22.0037603645225,-52.5894133206819));
#16597=CARTESIAN_POINT('Ctrl Pts',(-26.5233280854828,22.3004950621366,-52.6079906424235));
#16598=CARTESIAN_POINT('Ctrl Pts',(-26.568600824916,22.4141886879526,-52.615049940181));
#16599=CARTESIAN_POINT('Ctrl Pts',(-26.6239180850956,22.5799673676885,-52.6254463198742));
#16600=CARTESIAN_POINT('Ctrl Pts',(-26.6393139676713,22.6301589556454,-52.6286061686907));
#16601=CARTESIAN_POINT('Ctrl Pts',(-26.6556426107262,22.6884320949309,-52.632296163076));
#16602=CARTESIAN_POINT('Ctrl Pts',(-26.6577797374093,22.6961701749653,-52.6327865827214));
#16603=CARTESIAN_POINT('Ctrl Pts',(-26.6609761394213,22.7079144937432,-52.6335315799711));
#16604=CARTESIAN_POINT('Ctrl Pts',(-26.6620566474656,22.7119149632512,-52.6337854665638));
#16605=CARTESIAN_POINT('Ctrl Pts',(-26.6639136260692,22.7188432900237,-52.6342253755492));
#16606=CARTESIAN_POINT('Ctrl Pts',(-26.6646936917746,22.7217701854394,-52.6344112808681));
#16607=CARTESIAN_POINT('Ctrl Pts',(-26.666302875774,22.7278424172967,-52.6347971010998));
#16608=CARTESIAN_POINT('Ctrl Pts',(-26.6671313605615,22.7309879168528,-52.6349970363486));
#16609=CARTESIAN_POINT('Ctrl Pts',(-26.6691329088773,22.7386341557921,-52.6354832339393));
#16610=CARTESIAN_POINT('Ctrl Pts',(-26.670300991603,22.7431361815018,-52.635769657539));
#16611=CARTESIAN_POINT('Ctrl Pts',(-26.6746483965197,22.7600424233867,-52.6368458449617));
#16612=CARTESIAN_POINT('Ctrl Pts',(-26.6777634924159,22.7724628953724,-52.6376376859972));
#16613=CARTESIAN_POINT('Ctrl Pts',(-26.6820125117775,22.7898428615067,-52.6387474629635));
#16614=CARTESIAN_POINT('Ctrl Pts',(-26.6832088687879,22.794787093205,-52.6390633686789));
#16615=CARTESIAN_POINT('Ctrl Pts',(-26.7435070126344,23.0465902189239,-52.6551622434036));
#16616=CARTESIAN_POINT('Ctrl Pts',(-26.7732364955529,23.2995110305656,-52.6719416546303));
#16617=CARTESIAN_POINT('Ctrl Pts',(-26.7727822134999,23.7892719664017,-52.7050399444865));
#16618=CARTESIAN_POINT('Ctrl Pts',(-26.74663450226,24.0245852864968,-52.7211813837668));
#16619=CARTESIAN_POINT('Ctrl Pts',(-26.6919093968488,24.2688005347316,-52.7369922797257));
#16620=CARTESIAN_POINT('Ctrl Pts',(-26.6887136790122,24.2826327168205,-52.7378843248589));
#16621=CARTESIAN_POINT('Ctrl Pts',(-26.6845586641546,24.3000903021691,-52.7390053841722));
#16622=CARTESIAN_POINT('Ctrl Pts',(-26.683684366639,24.3037354778215,-52.7392391987727));
#16623=CARTESIAN_POINT('Ctrl Pts',(-26.682293171774,24.3094914360061,-52.7396079791744));
#16624=CARTESIAN_POINT('Ctrl Pts',(-26.6817804994965,24.3116032208455,-52.7397431888697));
#16625=CARTESIAN_POINT('Ctrl Pts',(-26.6808239338823,24.3155261661609,-52.7399941892723));
#16626=CARTESIAN_POINT('Ctrl Pts',(-26.6803806073414,24.3173374486916,-52.7401100118485));
#16627=CARTESIAN_POINT('Ctrl Pts',(-26.6793890147075,24.3213735881331,-52.740367951959));
#16628=CARTESIAN_POINT('Ctrl Pts',(-26.6788399490423,24.3235982403509,-52.7405100220968));
#16629=CARTESIAN_POINT('Ctrl Pts',(-26.6772301332399,24.3300909659134,-52.7409243656499));
#16630=CARTESIAN_POINT('Ctrl Pts',(-26.6761630132093,24.3343574775739,-52.7411962698606));
#16631=CARTESIAN_POINT('Ctrl Pts',(-26.6684199153631,24.3650485516147,-52.7431496318241));
#16632=CARTESIAN_POINT('Ctrl Pts',(-26.6614174397935,24.3913907012138,-52.7448124498148));
#16633=CARTESIAN_POINT('Ctrl Pts',(-26.6388375686339,24.4721895422076,-52.7498792864588));
#16634=CARTESIAN_POINT('Ctrl Pts',(-26.6221574882358,24.5263294480732,-52.7532272538077));
#16635=CARTESIAN_POINT('Ctrl Pts',(-26.5778971550926,24.6575866811807,-52.7612912292267));
#16636=CARTESIAN_POINT('Ctrl Pts',(-26.5487879202287,24.7341477377164,-52.7659496831208));
#16637=CARTESIAN_POINT('Ctrl Pts',(-26.4203244777721,25.0367774568539,-52.7844771973311));
#16638=CARTESIAN_POINT('Ctrl Pts',(-26.2980688754052,25.2521843940533,-52.7979958125178));
#16639=CARTESIAN_POINT('Ctrl Pts',(-26.0940359823415,25.5314334466337,-52.8181259133921));
#16640=CARTESIAN_POINT('Ctrl Pts',(-26.0320054169531,25.6086042117381,-52.824001394933));
#16641=CARTESIAN_POINT('Ctrl Pts',(-25.9603386306574,25.6898062313496,-52.8305936149293));
#16642=CARTESIAN_POINT('Ctrl Pts',(-25.9541192729382,25.6967915426531,-52.8311641608503));
#16643=CARTESIAN_POINT('Ctrl Pts',(-25.9448450461753,25.707117094005,-52.8320127249706));
#16644=CARTESIAN_POINT('Ctrl Pts',(-25.9418133662995,25.7104781737517,-52.832289764867));
#16645=CARTESIAN_POINT('Ctrl Pts',(-25.9366137460603,25.7162183849091,-52.8327643229604));
#16646=CARTESIAN_POINT('Ctrl Pts',(-25.9344492975762,25.7186006827458,-52.832961693014));
#16647=CARTESIAN_POINT('Ctrl Pts',(-25.9302334437901,25.7232269135209,-52.8333457884105));
#16648=CARTESIAN_POINT('Ctrl Pts',(-25.9281824246106,25.7254711943335,-52.8335324972004));
#16649=CARTESIAN_POINT('Ctrl Pts',(-25.9232722971412,25.730828745057,-52.8339791110253));
#16650=CARTESIAN_POINT('Ctrl Pts',(-25.9204102392042,25.7339392928263,-52.8342391417716));
#16651=CARTESIAN_POINT('Ctrl Pts',(-25.9118216983415,25.7432367322777,-52.8350185732211));
#16652=CARTESIAN_POINT('Ctrl Pts',(-25.9060770835053,25.749406758161,-52.8355387504125));
#16653=CARTESIAN_POINT('Ctrl Pts',(-25.8560379506446,25.802730419903,-52.8400599341334));
#16654=CARTESIAN_POINT('Ctrl Pts',(-25.810359853961,25.848559940563,-52.8441207453385));
#16655=CARTESIAN_POINT('Ctrl Pts',(-25.6899823962897,25.9622757817891,-52.8546693480358));
#16656=CARTESIAN_POINT('Ctrl Pts',(-25.6134213600829,26.0280804279194,-52.861238668793));
#16657=CARTESIAN_POINT('Ctrl Pts',(-25.2896809243261,26.2809178303072,-52.888431222496));
#16658=CARTESIAN_POINT('Ctrl Pts',(-25.019249989169,26.4354167404577,-52.9100221084945));
#16659=CARTESIAN_POINT('Ctrl Pts',(-24.69552290466,26.5628796624709,-52.9324049799868));
#16660=CARTESIAN_POINT('Ctrl Pts',(-24.6598587996901,26.5761971287406,-52.9348243576296));
#16661=CARTESIAN_POINT('Ctrl Pts',(-24.6190132081441,26.5906301008791,-52.9375359729122));
#16662=CARTESIAN_POINT('Ctrl Pts',(-24.614056888669,26.5923678217086,-52.9378640226648));
#16663=CARTESIAN_POINT('Ctrl Pts',(-24.6067946138255,26.5948941083061,-52.9383432348989));
#16664=CARTESIAN_POINT('Ctrl Pts',(-24.6044920093364,26.5956921756903,-52.9384949605713));
#16665=CARTESIAN_POINT('Ctrl Pts',(-24.6004485678798,26.5970884702414,-52.9387610149692));
#16666=CARTESIAN_POINT('Ctrl Pts',(-24.5987081226389,26.5976878180832,-52.938875410883));
#16667=CARTESIAN_POINT('Ctrl Pts',(-24.5953662701468,26.5988354321995,-52.9390948258316));
#16668=CARTESIAN_POINT('Ctrl Pts',(-24.5937649498605,26.5993839261605,-52.9391998584972));
#16669=CARTESIAN_POINT('Ctrl Pts',(-24.5894255088029,26.6008664790641,-52.9394842063217));
#16670=CARTESIAN_POINT('Ctrl Pts',(-24.5866865528256,26.6017981158596,-52.9396633764742));
#16671=CARTESIAN_POINT('Ctrl Pts',(-24.5807859339015,26.6037963095,-52.9400487222074));
#16672=CARTESIAN_POINT('Ctrl Pts',(-24.5776238575623,26.6048616482691,-52.9402548257505));
#16673=CARTESIAN_POINT('Ctrl Pts',(-24.5686967103348,26.6078538736223,-52.9408355854298));
#16674=CARTESIAN_POINT('Ctrl Pts',(-24.5629277967717,26.6097693759137,-52.9412095798552));
#16675=CARTESIAN_POINT('Ctrl Pts',(-24.5095554692257,26.6273235550072,-52.9446579174098));
#16676=CARTESIAN_POINT('Ctrl Pts',(-24.4615956852071,26.6418674058924,-52.9476702658952));
#16677=CARTESIAN_POINT('Ctrl Pts',(-24.34749374696,26.673582629561,-52.9546772186839));
#16678=CARTESIAN_POINT('Ctrl Pts',(-24.2811051910118,26.689781154413,-52.9586294484704));
#16679=CARTESIAN_POINT('Ctrl Pts',(-23.9179239977347,26.766249415111,-52.9798198191819));
#16680=CARTESIAN_POINT('Ctrl Pts',(-23.6142943556134,26.7865666865369,-52.9961470270256));
#16681=CARTESIAN_POINT('Ctrl Pts',(-23.2917089427677,26.7626812451586,-53.015092963649));
#16682=CARTESIAN_POINT('Ctrl Pts',(-23.2711539022192,26.7609607020362,-53.0163063600326));
#16683=CARTESIAN_POINT('Ctrl Pts',(-23.2460652795179,26.758617937616,-53.0177955641159));
#16684=CARTESIAN_POINT('Ctrl Pts',(-23.241514377516,26.7581832064688,-53.0180660245462));
#16685=CARTESIAN_POINT('Ctrl Pts',(-23.2329748418544,26.7573491156327,-53.0185741577171));
#16686=CARTESIAN_POINT('Ctrl Pts',(-23.2289859949089,26.7569519942754,-53.0188117657936));
#16687=CARTESIAN_POINT('Ctrl Pts',(-23.2199298932889,26.7560333205475,-53.0193518130592));
#16688=CARTESIAN_POINT('Ctrl Pts',(-23.2148631215906,26.7555071947111,-53.0196543839007));
#16689=CARTESIAN_POINT('Ctrl Pts',(-23.2029210869348,26.7542385258322,-53.0203685330292));
#16690=CARTESIAN_POINT('Ctrl Pts',(-23.196046942846,26.7534858642672,-53.0207804057505));
#16691=CARTESIAN_POINT('Ctrl Pts',(-23.1869868902137,26.7524643432857,-53.0213243143218));
#16692=CARTESIAN_POINT('Ctrl Pts',(-23.1847987250813,26.7522153559277,-53.0214557599027));
#16693=CARTESIAN_POINT('Ctrl Pts',(-23.1792324194128,26.7515761958789,-53.0217903440265));
#16694=CARTESIAN_POINT('Ctrl Pts',(-23.1758546436461,26.7511829195473,-53.0219935748054));
#16695=CARTESIAN_POINT('Ctrl Pts',(-23.1680403826476,26.7502605626194,-53.0224641953275));
#16696=CARTESIAN_POINT('Ctrl Pts',(-23.1636043697171,26.7497276016717,-53.0227317008958));
#16697=CARTESIAN_POINT('Ctrl Pts',(-23.1564103719225,26.7488481051033,-53.0231660850039));
#16698=CARTESIAN_POINT('Ctrl Pts',(-23.1536516920034,26.7485072218229,-53.0233327925871));
#16699=CARTESIAN_POINT('Ctrl Pts',(-23.1474122392505,26.7477280310845,-53.0237101504599));
#16700=CARTESIAN_POINT('Ctrl Pts',(-23.1439317380882,26.7472876085983,-53.0239208646709));
#16701=CARTESIAN_POINT('Ctrl Pts',(-23.1242116078043,26.7447595011469,-53.0251159826346));
#16702=CARTESIAN_POINT('Ctrl Pts',(-23.1079875783151,26.7425537929584,-53.0261039719001));
#16703=CARTESIAN_POINT('Ctrl Pts',(-23.0744713123119,26.7377367462865,-53.0281552212888));
#16704=CARTESIAN_POINT('Ctrl Pts',(-23.0571821488674,26.7351080960442,-53.0292189904562));
#16705=CARTESIAN_POINT('Ctrl Pts',(-23.034107913164,26.7314074934679,-53.0306465249964));
#16706=CARTESIAN_POINT('Ctrl Pts',(-23.0283029206094,26.7304601917093,-53.0310063253753));
#16707=CARTESIAN_POINT('Ctrl Pts',(-23.0192382585625,26.7289554653242,-53.031569210516));
#16708=CARTESIAN_POINT('Ctrl Pts',(-23.0159767781711,26.7284089025488,-53.0317719493782));
#16709=CARTESIAN_POINT('Ctrl Pts',(-23.0097414480619,26.727354109087,-53.0321599550066));
#16710=CARTESIAN_POINT('Ctrl Pts',(-23.0067674577324,26.7268467202684,-53.032345194781));
#16711=CARTESIAN_POINT('Ctrl Pts',(-22.9998185662771,26.725651134343,-53.0327784343979));
#16712=CARTESIAN_POINT('Ctrl Pts',(-22.99584424259,26.7249596496387,-53.0330265387658));
#16713=CARTESIAN_POINT('Ctrl Pts',(-22.9844755267049,26.7229596301403,-53.0337371699526));
#16714=CARTESIAN_POINT('Ctrl Pts',(-22.9770844321998,26.7216327170548,-53.0342002822185));
#16715=CARTESIAN_POINT('Ctrl Pts',(-22.9295702876154,26.7129310424172,-53.0371846699022));
#16716=CARTESIAN_POINT('Ctrl Pts',(-22.8895872167871,26.7048211084089,-53.039729335786));
#16717=CARTESIAN_POINT('Ctrl Pts',(-22.7711597115455,26.6784497737593,-53.0473701171001));
#16718=CARTESIAN_POINT('Ctrl Pts',(-22.6932390357195,26.6580056834719,-53.0525346651878));
#16719=CARTESIAN_POINT('Ctrl Pts',(-22.4835656934744,26.5945083613321,-53.0668102736648));
#16720=CARTESIAN_POINT('Ctrl Pts',(-22.3537003618806,26.5458444137825,-53.0760748887443));
#16721=CARTESIAN_POINT('Ctrl Pts',(-22.1759395151745,26.4658251380173,-53.0892395700871));
#16722=CARTESIAN_POINT('Ctrl Pts',(-22.1251412228718,26.4413338835681,-53.0930588162959));
#16723=CARTESIAN_POINT('Ctrl Pts',(-22.0750356956303,26.4155366099478,-53.096872577003));
#16724=CARTESIAN_POINT('',(-26.7730023713196,23.5492358241565,-52.9330225417352));
#16725=CARTESIAN_POINT('Ctrl Pts',(-22.0750361378578,26.4155368376325,-53.3407994113682));
#16726=CARTESIAN_POINT('Ctrl Pts',(-22.1242070858027,26.4408529252398,-53.3371202758974));
#16727=CARTESIAN_POINT('Ctrl Pts',(-22.1740388844405,26.464908014212,-53.3334755148323));
#16728=CARTESIAN_POINT('Ctrl Pts',(-22.2269649338975,26.4887955223206,-53.3297087672942));
#16729=CARTESIAN_POINT('Ctrl Pts',(-22.2294477788198,26.4899123383936,-53.3295323012437));
#16730=CARTESIAN_POINT('Ctrl Pts',(-22.2374274696282,26.4934895570924,-53.3289659225118));
#16731=CARTESIAN_POINT('Ctrl Pts',(-22.2429298310086,26.4959377132127,-53.3285765521788));
#16732=CARTESIAN_POINT('Ctrl Pts',(-22.2495689062746,26.4988693590425,-53.3281081830454));
#16733=CARTESIAN_POINT('Ctrl Pts',(-22.2506990376996,26.4993676200236,-53.3280285054649));
#16734=CARTESIAN_POINT('Ctrl Pts',(-22.2547703118536,26.5011597998254,-53.3277416501217));
#16735=CARTESIAN_POINT('Ctrl Pts',(-22.2577131132655,26.5024499741108,-53.3275346459821));
#16736=CARTESIAN_POINT('Ctrl Pts',(-22.2960583569796,26.5191928565472,-53.324841824636));
#16737=CARTESIAN_POINT('Ctrl Pts',(-22.3317359128781,26.5340131222827,-53.3223860159912));
#16738=CARTESIAN_POINT('Ctrl Pts',(-22.3720906754402,26.5499316400582,-53.319670548502));
#16739=CARTESIAN_POINT('Ctrl Pts',(-22.3765119975757,26.5516644114502,-53.3193738706306));
#16740=CARTESIAN_POINT('Ctrl Pts',(-22.3831776725568,26.5542597914343,-53.3189278635047));
#16741=CARTESIAN_POINT('Ctrl Pts',(-22.3854191626208,26.5551296615928,-53.318778099137));
#16742=CARTESIAN_POINT('Ctrl Pts',(-22.389303823817,26.5566322083863,-53.3185189235752));
#16743=CARTESIAN_POINT('Ctrl Pts',(-22.3909465396524,26.5572660467286,-53.3184094419626));
#16744=CARTESIAN_POINT('Ctrl Pts',(-22.3943355745528,26.5585705085772,-53.3181838154982));
#16745=CARTESIAN_POINT('Ctrl Pts',(-22.3960819561306,26.559240957123,-53.318067681718));
#16746=CARTESIAN_POINT('Ctrl Pts',(-22.4002116447766,26.5608222503166,-53.3177933694879));
#16747=CARTESIAN_POINT('Ctrl Pts',(-22.4025954583799,26.5617317885459,-53.3176352703644));
#16748=CARTESIAN_POINT('Ctrl Pts',(-22.4076482830864,26.5636528104836,-53.3173006696624));
#16749=CARTESIAN_POINT('Ctrl Pts',(-22.4103175652123,26.5646635822123,-53.317124210916));
#16750=CARTESIAN_POINT('Ctrl Pts',(-22.4175498291405,26.567391228943,-53.3166469160213));
#16751=CARTESIAN_POINT('Ctrl Pts',(-22.4221153923649,26.5691013067079,-53.3163464825931));
#16752=CARTESIAN_POINT('Ctrl Pts',(-22.4362753156447,26.5743684401869,-53.3154173476292));
#16753=CARTESIAN_POINT('Ctrl Pts',(-22.4458828614296,26.5778902087829,-53.314790688127));
#16754=CARTESIAN_POINT('Ctrl Pts',(-22.4818280557026,26.5908725113348,-53.3124595819443));
#16755=CARTESIAN_POINT('Ctrl Pts',(-22.5082726501679,26.6000359282977,-53.3107714852664));
#16756=CARTESIAN_POINT('Ctrl Pts',(-22.6011748115082,26.6308783095655,-53.304923630949));
#16757=CARTESIAN_POINT('Ctrl Pts',(-22.6682190529776,26.6507399100851,-53.3008499144153));
#16758=CARTESIAN_POINT('Ctrl Pts',(-23.1101907949546,26.7661730325682,-53.2746286820481));
#16759=CARTESIAN_POINT('Ctrl Pts',(-23.4990452924153,26.795743552224,-53.2540617875092));
#16760=CARTESIAN_POINT('Ctrl Pts',(-23.9038468104618,26.7536087247358,-53.229444444889));
#16761=CARTESIAN_POINT('Ctrl Pts',(-23.9237750551854,26.7513462056807,-53.228225586384));
#16762=CARTESIAN_POINT('Ctrl Pts',(-23.9498476209171,26.7481393238497,-53.2266214039715));
#16763=CARTESIAN_POINT('Ctrl Pts',(-23.9560124609934,26.7473629535743,-53.2262413978698));
#16764=CARTESIAN_POINT('Ctrl Pts',(-23.9655212291931,26.7461375194105,-53.2256541786737));
#16765=CARTESIAN_POINT('Ctrl Pts',(-23.9688667855917,26.7457010216763,-53.2254473635598));
#16766=CARTESIAN_POINT('Ctrl Pts',(-23.9755265554121,26.7448214771981,-53.2250352532907));
#16767=CARTESIAN_POINT('Ctrl Pts',(-23.9788407772145,26.7443785245904,-53.2248299613558));
#16768=CARTESIAN_POINT('Ctrl Pts',(-23.9861844897953,26.7433853867354,-53.2243746124204));
#16769=CARTESIAN_POINT('Ctrl Pts',(-23.990213635683,26.7428327309644,-53.2241244774278));
#16770=CARTESIAN_POINT('Ctrl Pts',(-24.001830915099,26.7412168430719,-53.2234023699143));
#16771=CARTESIAN_POINT('Ctrl Pts',(-24.0094162783063,26.7401341791878,-53.2229297819433));
#16772=CARTESIAN_POINT('Ctrl Pts',(-24.0604083389325,26.7326703981274,-53.2197453780736));
#16773=CARTESIAN_POINT('Ctrl Pts',(-24.1036829007203,26.7254307855831,-53.2170064200448));
#16774=CARTESIAN_POINT('Ctrl Pts',(-24.2193387200879,26.7036460381612,-53.2095834433729));
#16775=CARTESIAN_POINT('Ctrl Pts',(-24.2913868661905,26.6874942228014,-53.2048498271766));
#16776=CARTESIAN_POINT('Ctrl Pts',(-24.5290458550738,26.6255721288829,-53.1888669227109));
#16777=CARTESIAN_POINT('Ctrl Pts',(-24.6915329526469,26.569042715956,-53.1773161269921));
#16778=CARTESIAN_POINT('Ctrl Pts',(-24.9204693055348,26.4682601441986,-53.16038715081));
#16779=CARTESIAN_POINT('Ctrl Pts',(-24.9910389467116,26.4340689702133,-53.155075776131));
#16780=CARTESIAN_POINT('Ctrl Pts',(-25.1866491189176,26.3303210743683,-53.1401860839456));
#16781=CARTESIAN_POINT('Ctrl Pts',(-25.3084224856917,26.2549566596191,-53.1307119714078));
#16782=CARTESIAN_POINT('Ctrl Pts',(-25.4309513998696,26.1673399481675,-53.1212567724125));
#16783=CARTESIAN_POINT('Ctrl Pts',(-25.4370888499931,26.1629185051618,-53.1207833954757));
#16784=CARTESIAN_POINT('Ctrl Pts',(-25.4453594817836,26.1569159659023,-53.1201458661596));
#16785=CARTESIAN_POINT('Ctrl Pts',(-25.4475062955394,26.1553538286141,-53.1199804168128));
#16786=CARTESIAN_POINT('Ctrl Pts',(-25.4511283610704,26.152711366567,-53.1197013355821));
#16787=CARTESIAN_POINT('Ctrl Pts',(-25.4526046233393,26.1516324396212,-53.1195876065431));
#16788=CARTESIAN_POINT('Ctrl Pts',(-25.4555517207012,26.1494747018895,-53.1193606027074));
#16789=CARTESIAN_POINT('Ctrl Pts',(-25.4570225479631,26.1483959062484,-53.1192473286528));
#16790=CARTESIAN_POINT('Ctrl Pts',(-25.4603755945292,26.1459321937484,-53.1189891381115));
#16791=CARTESIAN_POINT('Ctrl Pts',(-25.4622572211323,26.1445464801175,-53.118844278474));
#16792=CARTESIAN_POINT('Ctrl Pts',(-25.4676461819518,26.1405687618566,-53.118429479627));
#16793=CARTESIAN_POINT('Ctrl Pts',(-25.4711497814763,26.1379716699706,-53.118159895323));
#16794=CARTESIAN_POINT('Ctrl Pts',(-25.4792297236193,26.1319568483895,-53.1175383757674));
#16795=CARTESIAN_POINT('Ctrl Pts',(-25.4838022902211,26.1285340365482,-53.117186790272));
#16796=CARTESIAN_POINT('Ctrl Pts',(-25.4985003311128,26.1174706712513,-53.1160570276572));
#16797=CARTESIAN_POINT('Ctrl Pts',(-25.5085899529218,26.1097823753797,-53.1152820619451));
#16798=CARTESIAN_POINT('Ctrl Pts',(-25.5483460986055,26.0791154674509,-53.1122295721013));
#16799=CARTESIAN_POINT('Ctrl Pts',(-25.5776569681329,26.0556780785861,-53.1099815292837));
#16800=CARTESIAN_POINT('Ctrl Pts',(-25.6580960610054,25.9890215159716,-53.1037979655626));
#16801=CARTESIAN_POINT('Ctrl Pts',(-25.7082988726084,25.944711878643,-53.0999221874937));
#16802=CARTESIAN_POINT('Ctrl Pts',(-25.9753875224474,25.6937467315603,-53.0789802995716));
#16803=CARTESIAN_POINT('Ctrl Pts',(-26.1640207033375,25.4591988905828,-53.0628291597259));
#16804=CARTESIAN_POINT('Ctrl Pts',(-26.330634000495,25.1800524022947,-53.0438306872907));
#16805=CARTESIAN_POINT('Ctrl Pts',(-26.3434514159162,25.1579865501049,-53.0423314803646));
#16806=CARTESIAN_POINT('Ctrl Pts',(-26.3593321837937,25.1298837550343,-53.0404240642853));
#16807=CARTESIAN_POINT('Ctrl Pts',(-26.3626406094728,25.1239858612637,-53.0400238660999));
#16808=CARTESIAN_POINT('Ctrl Pts',(-26.3946250702387,25.0665445437146,-53.036127103292));
#16809=CARTESIAN_POINT('Ctrl Pts',(-26.4218980096098,25.0142361947054,-53.0325851575725));
#16810=CARTESIAN_POINT('Ctrl Pts',(-26.4516682062971,24.9531017779214,-53.0284422208177));
#16811=CARTESIAN_POINT('Ctrl Pts',(-26.4555832131071,24.9449756416725,-53.0278914716006));
#16812=CARTESIAN_POINT('Ctrl Pts',(-26.4613336150686,24.9329106133996,-53.0270736368709));
#16813=CARTESIAN_POINT('Ctrl Pts',(-26.4631952647835,24.928984223625,-53.0268074645185));
#16814=CARTESIAN_POINT('Ctrl Pts',(-26.4664864968954,24.9220062917865,-53.0263343863021));
#16815=CARTESIAN_POINT('Ctrl Pts',(-26.4679192476806,24.9189562441202,-53.02612759072));
#16816=CARTESIAN_POINT('Ctrl Pts',(-26.4709147322618,24.9125533634978,-53.0256934395702));
#16817=CARTESIAN_POINT('Ctrl Pts',(-26.4724764815431,24.9092000777404,-53.0254660502804));
#16818=CARTESIAN_POINT('Ctrl Pts',(-26.4765528259633,24.9004080978849,-53.0248698077752));
#16819=CARTESIAN_POINT('Ctrl Pts',(-26.4790580241223,24.8949650853286,-53.0245006303804));
#16820=CARTESIAN_POINT('Ctrl Pts',(-26.4900061995884,24.8710023935305,-53.0228750886804));
#16821=CARTESIAN_POINT('Ctrl Pts',(-26.49828865636,24.852410280394,-53.0216132085418));
#16822=CARTESIAN_POINT('Ctrl Pts',(-26.5558032136623,24.7199422841882,-53.0126162127485));
#16823=CARTESIAN_POINT('Ctrl Pts',(-26.5985937073975,24.6033994440204,-53.0046625705489));
#16824=CARTESIAN_POINT('Ctrl Pts',(-26.7264677726202,24.1813255691787,-52.9757115417625));
#16825=CARTESIAN_POINT('Ctrl Pts',(-26.7731023432559,23.8661259127418,-52.9536327572046));
#16826=CARTESIAN_POINT('Ctrl Pts',(-26.7730023713196,23.5492358241565,-52.9330225417352));
#16827=CARTESIAN_POINT('Ctrl Pts',(-26.7730023700881,23.5492319278606,-52.9330222883241));
#16828=CARTESIAN_POINT('Ctrl Pts',(-26.7729846809421,23.4933751003751,-52.9293894185385));
#16829=CARTESIAN_POINT('Ctrl Pts',(-26.7715148199125,23.4375231614134,-52.9258125164439));
#16830=CARTESIAN_POINT('Ctrl Pts',(-26.7683879685189,23.3778073947579,-52.9220675012335));
#16831=CARTESIAN_POINT('Ctrl Pts',(-26.7681752323791,23.3738821605883,-52.9218217019452));
#16832=CARTESIAN_POINT('Ctrl Pts',(-26.7678175169938,23.3674980660912,-52.9214225373896));
#16833=CARTESIAN_POINT('Ctrl Pts',(-26.7676769006209,23.3650389801996,-52.9212689304832));
#16834=CARTESIAN_POINT('Ctrl Pts',(-26.7674249622829,23.3607199857685,-52.9209994055313));
#16835=CARTESIAN_POINT('Ctrl Pts',(-26.7673148465426,23.3588600121708,-52.9208834198018));
#16836=CARTESIAN_POINT('Ctrl Pts',(-26.7670964996327,23.3552253291779,-52.9206569330345));
#16837=CARTESIAN_POINT('Ctrl Pts',(-26.7669884126037,23.3534506101768,-52.9205464237487));
#16838=CARTESIAN_POINT('Ctrl Pts',(-26.7667702857427,23.3499172998788,-52.9203265661706));
#16839=CARTESIAN_POINT('Ctrl Pts',(-26.7666602725296,23.348158712028,-52.9202172165389));
#16840=CARTESIAN_POINT('Ctrl Pts',(-26.7663964209443,23.3439957725703,-52.9199585442965));
#16841=CARTESIAN_POINT('Ctrl Pts',(-26.7662413283009,23.3415914973977,-52.9198092928672));
#16842=CARTESIAN_POINT('Ctrl Pts',(-26.7657712726286,23.3344296345318,-52.9193651217387));
#16843=CARTESIAN_POINT('Ctrl Pts',(-26.7654484456831,23.3296725425759,-52.9190706435319));
#16844=CARTESIAN_POINT('Ctrl Pts',(-26.7623754740257,23.285830614817,-52.9163616383671));
#16845=CARTESIAN_POINT('Ctrl Pts',(-26.7589231746487,23.2467961252311,-52.913985887441));
#16846=CARTESIAN_POINT('Ctrl Pts',(-26.7536069219483,23.1970444965563,-52.9109931063958));
#16847=CARTESIAN_POINT('Ctrl Pts',(-26.7523997120542,23.1862625495263,-52.9103466444932));
#16848=CARTESIAN_POINT('Ctrl Pts',(-26.7497714237146,23.1638142608957,-52.9090047330167));
#16849=CARTESIAN_POINT('Ctrl Pts',(-26.7483409286878,23.1521491659268,-52.9083096942081));
#16850=CARTESIAN_POINT('Ctrl Pts',(-26.7100243515173,22.8532366631737,-52.8905521352205));
#16851=CARTESIAN_POINT('Ctrl Pts',(-26.6346483054277,22.5722281342401,-52.8749936966126));
#16852=CARTESIAN_POINT('Ctrl Pts',(-26.4847514209994,22.2144035730923,-52.852896990685));
#16853=CARTESIAN_POINT('Ctrl Pts',(-26.4426550919353,22.1255486306699,-52.8472156412204));
#16854=CARTESIAN_POINT('Ctrl Pts',(-26.3666885058268,21.9824947123475,-52.8376316119333));
#16855=CARTESIAN_POINT('Ctrl Pts',(-26.3351493004389,21.9271304471426,-52.8338088275422));
#16856=CARTESIAN_POINT('Ctrl Pts',(-26.2976183388697,21.8655658312983,-52.8294137365891));
#16857=CARTESIAN_POINT('Ctrl Pts',(-26.2932168809969,21.8584089416198,-52.8289005585163));
#16858=CARTESIAN_POINT('Ctrl Pts',(-26.2865621144583,21.8476823424888,-52.8281280003493));
#16859=CARTESIAN_POINT('Ctrl Pts',(-26.2843296728532,21.8440996757573,-52.8278693916304));
#16860=CARTESIAN_POINT('Ctrl Pts',(-26.2804776170884,21.8379447950353,-52.8274241165647));
#16861=CARTESIAN_POINT('Ctrl Pts',(-26.2788613870028,21.8353704609487,-52.8272375758316));
#16862=CARTESIAN_POINT('Ctrl Pts',(-26.2755249184386,21.830072786325,-52.8268530758884));
#16863=CARTESIAN_POINT('Ctrl Pts',(-26.273804234564,21.8273497311863,-52.8266551002596));
#16864=CARTESIAN_POINT('Ctrl Pts',(-26.269651257089,21.8207992365135,-52.8261780368822));
#16865=CARTESIAN_POINT('Ctrl Pts',(-26.2672149663771,21.8169743497265,-52.8258988004754));
#16866=CARTESIAN_POINT('Ctrl Pts',(-26.2597108523121,21.8052478641991,-52.8250406224921));
#16867=CARTESIAN_POINT('Ctrl Pts',(-26.2546166061976,21.7973633080732,-52.8244606948665));
#16868=CARTESIAN_POINT('Ctrl Pts',(-26.1946266885844,21.7053986387906,-52.8176620423596));
#16869=CARTESIAN_POINT('Ctrl Pts',(-26.1358703017428,21.623914635597,-52.8112976776001));
#16870=CARTESIAN_POINT('Ctrl Pts',(-25.892740352064,21.3179426178945,-52.7859931730411));
#16871=CARTESIAN_POINT('Ctrl Pts',(-25.6821743014006,21.1160551253123,-52.7660086614789));
#16872=CARTESIAN_POINT('Ctrl Pts',(-25.3924477802677,20.9050549188075,-52.7420696772945));
#16873=CARTESIAN_POINT('Ctrl Pts',(-25.3361474461298,20.8667223461637,-52.7375688992182));
#16874=CARTESIAN_POINT('Ctrl Pts',(-25.2489454289872,20.8113110484331,-52.7308681905592));
#16875=CARTESIAN_POINT('Ctrl Pts',(-25.21891015265,20.7929096106098,-52.7286070161654));
#16876=CARTESIAN_POINT('Ctrl Pts',(-25.1781502289098,20.7688476205305,-52.7256068434281));
#16877=CARTESIAN_POINT('Ctrl Pts',(-25.1676877694296,20.7627505218464,-52.7248427025274));
#16878=CARTESIAN_POINT('Ctrl Pts',(-25.1524067934221,20.75396038914,-52.7237355597798));
#16879=CARTESIAN_POINT('Ctrl Pts',(-25.14761547994,20.7512206209232,-52.7233896873278));
#16880=CARTESIAN_POINT('Ctrl Pts',(-25.1390306106827,20.7463408447419,-52.722772268801));
#16881=CARTESIAN_POINT('Ctrl Pts',(-25.135239725249,20.7441962013078,-52.7225004302937));
#16882=CARTESIAN_POINT('Ctrl Pts',(-25.1294652392343,20.7409447973587,-52.7220875799382));
#16883=CARTESIAN_POINT('Ctrl Pts',(-25.127484816265,20.7398324487818,-52.7219462078476));
#16884=CARTESIAN_POINT('Ctrl Pts',(-25.123885008566,20.7378155402523,-52.7216896370563));
#16885=CARTESIAN_POINT('Ctrl Pts',(-25.1222660228562,20.7369102868263,-52.7215743934975));
#16886=CARTESIAN_POINT('Ctrl Pts',(-25.1187700654545,20.7349594874613,-52.7213258600931));
#16887=CARTESIAN_POINT('Ctrl Pts',(-25.1168928345929,20.7339144234376,-52.721192601792));
#16888=CARTESIAN_POINT('Ctrl Pts',(-25.1118300864111,20.7311025938544,-52.7208337416046));
#16889=CARTESIAN_POINT('Ctrl Pts',(-25.1086426043639,20.729339343889,-52.7206083669186));
#16890=CARTESIAN_POINT('Ctrl Pts',(-25.0939297892302,20.7212330630903,-52.7195706369741));
#16891=CARTESIAN_POINT('Ctrl Pts',(-25.0823684602513,20.7149551179017,-52.7187624141991));
#16892=CARTESIAN_POINT('Ctrl Pts',(-25.0607716447043,20.7033984553046,-52.7172654340763));
#16893=CARTESIAN_POINT('Ctrl Pts',(-25.0507461850442,20.6981016016644,-52.7165756095101));
#16894=CARTESIAN_POINT('Ctrl Pts',(-25.037349563696,20.6911138155179,-52.7156603071847));
#16895=CARTESIAN_POINT('Ctrl Pts',(-25.034003235573,20.6893758076924,-52.7154322112815));
#16896=CARTESIAN_POINT('Ctrl Pts',(-25.025463825841,20.6849596425712,-52.7148514861295));
#16897=CARTESIAN_POINT('Ctrl Pts',(-25.0202664723663,20.6822897149665,-52.7144993059205));
#16898=CARTESIAN_POINT('Ctrl Pts',(-24.8641076946396,20.6026055552911,-52.7039548752677));
#16899=CARTESIAN_POINT('Ctrl Pts',(-24.7072922915293,20.5375939392647,-52.694397323582));
#16900=CARTESIAN_POINT('Ctrl Pts',(-24.5297422393207,20.4799085240806,-52.6839457206577));
#16901=CARTESIAN_POINT('Ctrl Pts',(-24.5133691689411,20.4747332652562,-52.6829853581581));
#16902=CARTESIAN_POINT('Ctrl Pts',(-24.4783652700363,20.4639760466004,-52.6809382450173));
#16903=CARTESIAN_POINT('Ctrl Pts',(-24.4597237072971,20.4584313888354,-52.6798516649791));
#16904=CARTESIAN_POINT('Ctrl Pts',(-24.4195497668452,20.4468770162364,-52.6775159366981));
#16905=CARTESIAN_POINT('Ctrl Pts',(-24.3980027712868,20.4409219282711,-52.6762668211985));
#16906=CARTESIAN_POINT('Ctrl Pts',(-24.3510724440081,20.4284755703248,-52.6735513610455));
#16907=CARTESIAN_POINT('Ctrl Pts',(-24.3256684571303,20.422068704251,-52.6720847049147));
#16908=CARTESIAN_POINT('Ctrl Pts',(-24.269432814875,20.4086132461758,-52.6688410125533));
#16909=CARTESIAN_POINT('Ctrl Pts',(-24.2385699781465,20.4017073542298,-52.6670627851326));
#16910=CARTESIAN_POINT('Ctrl Pts',(-24.1682199773021,20.3870495986992,-52.6630067835336));
#16911=CARTESIAN_POINT('Ctrl Pts',(-24.128679635947,20.3795809106773,-52.6607252026832));
#16912=CARTESIAN_POINT('Ctrl Pts',(-23.953491649148,20.3498761232679,-52.6505825626587));
#16913=CARTESIAN_POINT('Ctrl Pts',(-23.8166574421841,20.3355935636925,-52.6425631548651));
#16914=CARTESIAN_POINT('Ctrl Pts',(-23.6577046317934,20.3292215688205,-52.6329474442502));
#16915=CARTESIAN_POINT('Ctrl Pts',(-23.6360611788002,20.3285723399105,-52.6316319483899));
#16916=CARTESIAN_POINT('Ctrl Pts',(-23.60828701155,20.3280192832981,-52.6299353808698));
#16917=CARTESIAN_POINT('Ctrl Pts',(-23.6021604923769,20.3279147668533,-52.6295606197009));
#16918=CARTESIAN_POINT('Ctrl Pts',(-23.59230462753,20.3277747438942,-52.6289568735553));
#16919=CARTESIAN_POINT('Ctrl Pts',(-23.5885754327827,20.3277282374964,-52.6287282342494));
#16920=CARTESIAN_POINT('Ctrl Pts',(-23.5814836559181,20.3276521085517,-52.6282930532253));
#16921=CARTESIAN_POINT('Ctrl Pts',(-23.5781210894881,20.3276212754521,-52.6280865498061));
#16922=CARTESIAN_POINT('Ctrl Pts',(-23.5704704793238,20.3275630981307,-52.6276163351458));
#16923=CARTESIAN_POINT('Ctrl Pts',(-23.5661824234213,20.3275390494135,-52.6273525207771));
#16924=CARTESIAN_POINT('Ctrl Pts',(-23.5531622804205,20.3274920153239,-52.6265506670712));
#16925=CARTESIAN_POINT('Ctrl Pts',(-23.5444301897244,20.327495961545,-52.6260117832615));
#16926=CARTESIAN_POINT('Ctrl Pts',(-23.4827716447314,20.327774420141,-52.6221986595597));
#16927=CARTESIAN_POINT('Ctrl Pts',(-23.4298616568506,20.3293172096997,-52.6188848050576));
#16928=CARTESIAN_POINT('Ctrl Pts',(-23.373197642625,20.3323675506224,-52.6152881311864));
#16929=CARTESIAN_POINT('Ctrl Pts',(-23.3693795959243,20.3325798997977,-52.6150455542441));
#16930=CARTESIAN_POINT('Ctrl Pts',(-23.3615276202858,20.3330306245585,-52.614546207307));
#16931=CARTESIAN_POINT('Ctrl Pts',(-23.3574937451056,20.3332697928693,-52.6142894136466));
#16932=CARTESIAN_POINT('Ctrl Pts',(-23.3487856836105,20.3338025311705,-52.6137345040127));
#16933=CARTESIAN_POINT('Ctrl Pts',(-23.3441116708571,20.3340987042363,-52.6134363099638));
#16934=CARTESIAN_POINT('Ctrl Pts',(-23.3203134292723,20.3356587928656,-52.6119162428206));
#16935=CARTESIAN_POINT('Ctrl Pts',(-23.3012004137643,20.3370830816991,-52.6106895777369));
#16936=CARTESIAN_POINT('Ctrl Pts',(-23.1338318425769,20.3510575486446,-52.599896404522));
#16937=CARTESIAN_POINT('Ctrl Pts',(-22.9866149287709,20.3736886757336,-52.5900354302345));
#16938=CARTESIAN_POINT('Ctrl Pts',(-22.6816982268951,20.4424291117452,-52.568999678416));
#16939=CARTESIAN_POINT('Ctrl Pts',(-22.5248741610673,20.4905871048004,-52.5578215368336));
#16940=CARTESIAN_POINT('Ctrl Pts',(-22.3064547977899,20.5763489307018,-52.5421689771781));
#16941=CARTESIAN_POINT('Ctrl Pts',(-22.241385379507,20.6044073945811,-52.5374971529268));
#16942=CARTESIAN_POINT('Ctrl Pts',(-22.1497762967372,20.6475453963387,-52.5309566993903));
#16943=CARTESIAN_POINT('Ctrl Pts',(-22.1224465759216,20.6608905425067,-52.5290103704465));
#16944=CARTESIAN_POINT('Ctrl Pts',(-22.0856048948449,20.6795308223162,-52.5263973462573));
#16945=CARTESIAN_POINT('Ctrl Pts',(-22.0759257880804,20.6844897198558,-52.525711865537));
#16946=CARTESIAN_POINT('Ctrl Pts',(-22.0617456582692,20.6918454842499,-52.5247093220912));
#16947=CARTESIAN_POINT('Ctrl Pts',(-22.057225048281,20.6942041259904,-52.5243899678195));
#16948=CARTESIAN_POINT('Ctrl Pts',(-22.049092654813,20.6984718116124,-52.5238159492891));
#16949=CARTESIAN_POINT('Ctrl Pts',(-22.0454788795865,20.7003770067366,-52.5235610475396));
#16950=CARTESIAN_POINT('Ctrl Pts',(-22.0399139815044,20.7033243768008,-52.5231688006567));
#16951=CARTESIAN_POINT('Ctrl Pts',(-22.0379603094413,20.70436168876,-52.5230311475306));
#16952=CARTESIAN_POINT('Ctrl Pts',(-22.0343946316353,20.7062596117828,-52.5227800140398));
#16953=CARTESIAN_POINT('Ctrl Pts',(-22.032782296213,20.7071195790957,-52.5226664933345));
#16954=CARTESIAN_POINT('Ctrl Pts',(-22.0294951409166,20.7088764336983,-52.5224351287521));
#16955=CARTESIAN_POINT('Ctrl Pts',(-22.027820389043,20.7097734272234,-52.5223172924593));
#16956=CARTESIAN_POINT('Ctrl Pts',(-22.0230029330546,20.7123591309059,-52.5219784469385));
#16957=CARTESIAN_POINT('Ctrl Pts',(-22.0198622259353,20.714051586219,-52.5217576772823));
#16958=CARTESIAN_POINT('Ctrl Pts',(-22.0060941810934,20.7215003993676,-52.5207904592404));
#16959=CARTESIAN_POINT('Ctrl Pts',(-21.9954962825397,20.7273113961944,-52.5200474622675));
#16960=CARTESIAN_POINT('Ctrl Pts',(-21.9818484038171,20.7348949182651,-52.5190922723478));
#16961=CARTESIAN_POINT('Ctrl Pts',(-21.9787684765839,20.7366129199762,-52.5188768219932));
#16962=CARTESIAN_POINT('Ctrl Pts',(-21.7362387455544,20.8724199010594,-52.501919152427));
#16963=CARTESIAN_POINT('Ctrl Pts',(-21.5148488996317,21.036565762169,-52.486992278037));
#16964=CARTESIAN_POINT('Ctrl Pts',(-21.29123604148,21.2515069399556,-52.4695907613846));
#16965=CARTESIAN_POINT('Ctrl Pts',(-21.2659627632611,21.2766195367824,-52.4675865999366));
#16966=CARTESIAN_POINT('Ctrl Pts',(-21.2111013842029,21.3329703602861,-52.4631424840714));
#16967=CARTESIAN_POINT('Ctrl Pts',(-21.1817123168005,21.3643921930242,-52.4606988605834));
#16968=CARTESIAN_POINT('Ctrl Pts',(-21.0656658257457,21.4935543317127,-52.45076266473));
#16969=CARTESIAN_POINT('Ctrl Pts',(-20.9843673515529,21.5959225675316,-52.4431245433296));
#16970=CARTESIAN_POINT('Ctrl Pts',(-20.9015721998513,21.7142781882836,-52.4343905157874));
#16971=CARTESIAN_POINT('Ctrl Pts',(-20.8937084773239,21.7256750551589,-52.4335505110737));
#16972=CARTESIAN_POINT('Ctrl Pts',(-20.8800766596713,21.7457065513532,-52.4320756934417));
#16973=CARTESIAN_POINT('Ctrl Pts',(-20.8742763586644,21.7543190974858,-52.4314421079183));
#16974=CARTESIAN_POINT('Ctrl Pts',(-20.8659648654255,21.7667900346747,-52.4305253580512));
#16975=CARTESIAN_POINT('Ctrl Pts',(-20.8634201177541,21.7706260729648,-52.4302434597304));
#16976=CARTESIAN_POINT('Ctrl Pts',(-20.859005162701,21.7773123795494,-52.4297522590103));
#16977=CARTESIAN_POINT('Ctrl Pts',(-20.8571312381472,21.7801601944703,-52.429543096743));
#16978=CARTESIAN_POINT('Ctrl Pts',(-20.8535277130482,21.7856554628002,-52.4291395794258));
#16979=CARTESIAN_POINT('Ctrl Pts',(-20.8517974828563,21.7883025005263,-52.4289452482965));
#16980=CARTESIAN_POINT('Ctrl Pts',(-20.8477168525667,21.7945654682021,-52.4284855491162));
#16981=CARTESIAN_POINT('Ctrl Pts',(-20.8453698131854,21.7981835716638,-52.4282200556442));
#16982=CARTESIAN_POINT('Ctrl Pts',(-20.8384190908077,21.808945785676,-52.4274305450019));
#16983=CARTESIAN_POINT('Ctrl Pts',(-20.8338364251998,21.8161033659659,-52.4269057449411));
#16984=CARTESIAN_POINT('Ctrl Pts',(-20.7922609554316,21.8816084910158,-52.4221052132072));
#16985=CARTESIAN_POINT('Ctrl Pts',(-20.7571274699602,21.9411093853614,-52.4177611520951));
#16986=CARTESIAN_POINT('Ctrl Pts',(-20.7187300584901,22.0111893810128,-52.4126575085473));
#16987=CARTESIAN_POINT('Ctrl Pts',(-20.7135730811969,22.0207151543435,-52.4119640662908));
#16988=CARTESIAN_POINT('Ctrl Pts',(-20.5858623426182,22.2594850554161,-52.3945894036664));
#16989=CARTESIAN_POINT('Ctrl Pts',(-20.4914607565009,22.5026651396318,-52.3769365680758));
#16990=CARTESIAN_POINT('Ctrl Pts',(-20.4065697516636,22.8358151446688,-52.3537213810636));
#16991=CARTESIAN_POINT('Ctrl Pts',(-20.3890291622611,22.9179311394058,-52.3480838085983));
#16992=CARTESIAN_POINT('Ctrl Pts',(-20.3642192848365,23.0612775348118,-52.3384770604008));
#16993=CARTESIAN_POINT('Ctrl Pts',(-20.3554627844399,23.1222058838093,-52.3344662770859));
#16994=CARTESIAN_POINT('Ctrl Pts',(-20.3463670203406,23.2015809608084,-52.3293656008616));
#16995=CARTESIAN_POINT('Ctrl Pts',(-20.3444337465069,23.2198282789951,-52.3282015243654));
#16996=CARTESIAN_POINT('Ctrl Pts',(-20.3419298038576,23.245557432946,-52.326573052818));
#16997=CARTESIAN_POINT('Ctrl Pts',(-20.3412292932023,23.2530258730712,-52.326101883417));
#16998=CARTESIAN_POINT('Ctrl Pts',(-20.3402056436602,23.2643650975986,-52.3253889041492));
#16999=CARTESIAN_POINT('Ctrl Pts',(-20.3398634219571,23.2682340698776,-52.3251460559157));
#17000=CARTESIAN_POINT('Ctrl Pts',(-20.3393173055581,23.274537993742,-52.3247510682651));
#17001=CARTESIAN_POINT('Ctrl Pts',(-20.3391091853444,23.2769725613836,-52.3245986940545));
#17002=CARTESIAN_POINT('Ctrl Pts',(-20.338714196736,23.2816558503865,-52.324305906483));
#17003=CARTESIAN_POINT('Ctrl Pts',(-20.3385269210033,23.2839045341091,-52.3241654702888));
#17004=CARTESIAN_POINT('Ctrl Pts',(-20.3381920542471,23.2879771038951,-52.3239113941354));
#17005=CARTESIAN_POINT('Ctrl Pts',(-20.3380436552783,23.2898009140496,-52.3237977086767));
#17006=CARTESIAN_POINT('Ctrl Pts',(-20.3377465543131,23.2934911378986,-52.3235678784309));
#17007=CARTESIAN_POINT('Ctrl Pts',(-20.3375979260398,23.2953575477029,-52.3234517382075));
#17008=CARTESIAN_POINT('Ctrl Pts',(-20.3371815309458,23.300644679962,-52.3231230226498));
#17009=CARTESIAN_POINT('Ctrl Pts',(-20.3369175993968,23.3040657151614,-52.3229106646284));
#17010=CARTESIAN_POINT('Ctrl Pts',(-20.3358348848543,23.3183980914514,-52.3220223816247));
#17011=CARTESIAN_POINT('Ctrl Pts',(-20.3350661982722,23.329313310901,-52.321349253681));
#17012=CARTESIAN_POINT('Ctrl Pts',(-20.322096271135,23.5279132476972,-52.3091596615846));
#17013=CARTESIAN_POINT('Ctrl Pts',(-20.326290688331,23.7163390405978,-52.298523168509));
#17014=CARTESIAN_POINT('Ctrl Pts',(-20.3646203553982,24.0640733249256,-52.2789250280744));
#17015=CARTESIAN_POINT('Ctrl Pts',(-20.3944079082313,24.2232362328011,-52.2699634481087));
#17016=CARTESIAN_POINT('Ctrl Pts',(-20.4714891494131,24.5127199914436,-52.2528662552838));
#17017=CARTESIAN_POINT('Ctrl Pts',(-20.515474792628,24.6435249175556,-52.244823277502));
#17018=CARTESIAN_POINT('Ctrl Pts',(-20.5759133299923,24.7911773622757,-52.2351798070497));
#17019=CARTESIAN_POINT('Ctrl Pts',(-20.584333208839,24.8111691254856,-52.2338619399014));
#17020=CARTESIAN_POINT('Ctrl Pts',(-20.595390926387,24.8367003737058,-52.2321627343234));
#17021=CARTESIAN_POINT('Ctrl Pts',(-20.5978437798778,24.8423197583167,-52.2317877306516));
#17022=CARTESIAN_POINT('Ctrl Pts',(-20.6018147268672,24.8513466825338,-52.23118368707));
#17023=CARTESIAN_POINT('Ctrl Pts',(-20.6033227348869,24.8547586645989,-52.2309549934472));
#17024=CARTESIAN_POINT('Ctrl Pts',(-20.6062013011727,24.8612411743442,-52.2305197698409));
#17025=CARTESIAN_POINT('Ctrl Pts',(-20.6075707485103,24.8643121923923,-52.2303132782721));
#17026=CARTESIAN_POINT('Ctrl Pts',(-20.6106968881655,24.8712932409254,-52.2298431744942));
#17027=CARTESIAN_POINT('Ctrl Pts',(-20.6124565776214,24.8752019151794,-52.2295794593396));
#17028=CARTESIAN_POINT('Ctrl Pts',(-20.6178213201204,24.8870550085882,-52.2287781989981));
#17029=CARTESIAN_POINT('Ctrl Pts',(-20.6214508166278,24.8949882619648,-52.2282398111765));
#17030=CARTESIAN_POINT('Ctrl Pts',(-20.6472606716036,24.9508025621494,-52.2244369890565));
#17031=CARTESIAN_POINT('Ctrl Pts',(-20.6705807666726,24.9981448342399,-52.2211331809843));
#17032=CARTESIAN_POINT('Ctrl Pts',(-20.6969805598483,25.0485762345562,-52.2175255428149));
#17033=CARTESIAN_POINT('Ctrl Pts',(-20.6989167638517,25.0522575924858,-52.2172616812532));
#17034=CARTESIAN_POINT('Ctrl Pts',(-20.7027423416774,25.0594972140609,-52.2167417675745));
#17035=CARTESIAN_POINT('Ctrl Pts',(-20.704631272039,25.063055704571,-52.2164857310375));
#17036=CARTESIAN_POINT('Ctrl Pts',(-20.7088702718867,25.0710053786494,-52.2159126617132));
#17037=CARTESIAN_POINT('Ctrl Pts',(-20.7112238544829,25.075394668481,-52.2155955092694));
#17038=CARTESIAN_POINT('Ctrl Pts',(-20.7221355454589,25.0956315343891,-52.2141298458438));
#17039=CARTESIAN_POINT('Ctrl Pts',(-20.7308161055018,25.1114124107428,-52.2129771809979));
#17040=CARTESIAN_POINT('Ctrl Pts',(-20.7726327987351,25.1859469245321,-52.2074865919345));
#17041=CARTESIAN_POINT('Ctrl Pts',(-20.8074740740741,25.2437202371994,-52.2030922589324));
#17042=CARTESIAN_POINT('Ctrl Pts',(-20.9770113200173,25.5058726595033,-52.1825155827544));
#17043=CARTESIAN_POINT('Ctrl Pts',(-21.1328998420461,25.6955747959056,-52.1656974453406));
#17044=CARTESIAN_POINT('Ctrl Pts',(-21.3400442207299,25.896099281951,-52.1464586971225));
#17045=CARTESIAN_POINT('Ctrl Pts',(-21.3719773629991,25.925780962463,-52.1435696638877));
#17046=CARTESIAN_POINT('Ctrl Pts',(-21.4535301069519,25.9985560679456,-52.1364000406852));
#17047=CARTESIAN_POINT('Ctrl Pts',(-21.5038870243687,26.0407996175307,-52.1321583934052));
#17048=CARTESIAN_POINT('Ctrl Pts',(-21.5610949956279,26.0858827340856,-52.1275725973153));
#17049=CARTESIAN_POINT('Ctrl Pts',(-21.5667001824379,26.0902699148189,-52.1271256926731));
#17050=CARTESIAN_POINT('Ctrl Pts',(-21.5752718344897,26.0969332709644,-52.1264459928998));
#17051=CARTESIAN_POINT('Ctrl Pts',(-21.5782277576932,26.0992228793367,-52.1262122709998));
#17052=CARTESIAN_POINT('Ctrl Pts',(-21.5830738034972,26.1029630696163,-52.1258302066036));
#17053=CARTESIAN_POINT('Ctrl Pts',(-21.584961551617,26.1044167008118,-52.1256816500384));
#17054=CARTESIAN_POINT('Ctrl Pts',(-21.5886047667294,26.1072156718786,-52.1253954781903));
#17055=CARTESIAN_POINT('Ctrl Pts',(-21.5903600091168,26.1085613000153,-52.1252578424673));
#17056=CARTESIAN_POINT('Ctrl Pts',(-21.5935680325026,26.1110154399811,-52.1250067233921));
#17057=CARTESIAN_POINT('Ctrl Pts',(-21.595020365455,26.1121245187348,-52.1248931997333));
#17058=CARTESIAN_POINT('Ctrl Pts',(-21.5979838837376,26.1143836310927,-52.1246618837174));
#17059=CARTESIAN_POINT('Ctrl Pts',(-21.5994951364912,26.1155335599256,-52.1245440988558));
#17060=CARTESIAN_POINT('Ctrl Pts',(-21.6038452164394,26.1188375165349,-52.1242055608522));
#17061=CARTESIAN_POINT('Ctrl Pts',(-21.6066866125303,26.12098818115,-52.1239850465929));
#17062=CARTESIAN_POINT('Ctrl Pts',(-21.6191517413112,26.1303906100946,-52.1230203096895));
#17063=CARTESIAN_POINT('Ctrl Pts',(-21.628812698336,26.1375932019244,-52.1222795167671));
#17064=CARTESIAN_POINT('Ctrl Pts',(-21.776591904548,26.2464836992793,-52.1110490172245));
#17065=CARTESIAN_POINT('Ctrl Pts',(-21.9225646111997,26.3370355473912,-52.1012875088868));
#17066=CARTESIAN_POINT('Ctrl Pts',(-22.0750360382923,26.4155367863704,-52.0916569661403));
#17067=CARTESIAN_POINT('Origin',(-23.5502525316942,23.5502525316942,-77.3107734492734));
#17068=CARTESIAN_POINT('',(-22.0750357068451,26.4155366157218,-50.5964032705492));
#17069=CARTESIAN_POINT('',(-22.0750360284016,26.415536781278,-50.8458393738826));
#17070=CARTESIAN_POINT('',(-22.0750360153461,26.4155367745563,-77.3107734492734));
#17071=CARTESIAN_POINT('',(-26.7730025211998,23.5499924521692,-51.4361781865152));
#17072=CARTESIAN_POINT('Ctrl Pts',(-22.0750357068432,26.4155366157209,-50.5964032705493));
#17073=CARTESIAN_POINT('Ctrl Pts',(-21.8523485774069,26.300884179736,-50.6104004212466));
#17074=CARTESIAN_POINT('Ctrl Pts',(-21.6435050826592,26.1605201296056,-50.6245125474874));
#17075=CARTESIAN_POINT('Ctrl Pts',(-21.4370245485272,25.9835258314191,-50.6409549397257));
#17076=CARTESIAN_POINT('Ctrl Pts',(-21.4213415961363,25.9698164710839,-50.6422204904967));
#17077=CARTESIAN_POINT('Ctrl Pts',(-21.4010854162771,25.9517599837174,-50.6438774603741));
#17078=CARTESIAN_POINT('Ctrl Pts',(-21.3963902605948,25.9475498950503,-50.6442631151753));
#17079=CARTESIAN_POINT('Ctrl Pts',(-21.3891884037849,25.9410538422488,-50.6448571289976));
#17080=CARTESIAN_POINT('Ctrl Pts',(-21.3866728861307,25.9387776390878,-50.6450650749099));
#17081=CARTESIAN_POINT('Ctrl Pts',(-21.3817365449963,25.9342967215347,-50.6454740552082));
#17082=CARTESIAN_POINT('Ctrl Pts',(-21.3793154776693,25.9320922809241,-50.6456750778362));
#17083=CARTESIAN_POINT('Ctrl Pts',(-21.3739985830968,25.9272362780307,-50.6461175031256));
#17084=CARTESIAN_POINT('Ctrl Pts',(-21.3711042367558,25.9245831084216,-50.6463589741065));
#17085=CARTESIAN_POINT('Ctrl Pts',(-21.3651225139799,25.9190796727348,-50.6468593281617));
#17086=CARTESIAN_POINT('Ctrl Pts',(-21.3620358503229,25.9162286460172,-50.6471182435472));
#17087=CARTESIAN_POINT('Ctrl Pts',(-21.3541715954455,25.9089361975631,-50.6477797713994));
#17088=CARTESIAN_POINT('Ctrl Pts',(-21.3494019140452,25.9044863076776,-50.6481827472665));
#17089=CARTESIAN_POINT('Ctrl Pts',(-21.3357215758627,25.8916452837271,-50.6493436510699));
#17090=CARTESIAN_POINT('Ctrl Pts',(-21.3268452425592,25.8832178965395,-50.6501031434403));
#17091=CARTESIAN_POINT('Ctrl Pts',(-21.2414001677347,25.8011638974573,-50.6574754240567));
#17092=CARTESIAN_POINT('Ctrl Pts',(-21.1684758028635,25.7238524454953,-50.6642502535098));
#17093=CARTESIAN_POINT('Ctrl Pts',(-20.9549644604765,25.4738272077129,-50.6856760461208));
#17094=CARTESIAN_POINT('Ctrl Pts',(-20.8283594836573,25.29006164396,-50.7008133803542));
#17095=CARTESIAN_POINT('Ctrl Pts',(-20.6428144723012,24.950260983726,-50.7269526814135));
#17096=CARTESIAN_POINT('Ctrl Pts',(-20.5750932149337,24.7999170641754,-50.737949783234));
#17097=CARTESIAN_POINT('Ctrl Pts',(-20.5159184055842,24.6360815484909,-50.7489062931017));
#17098=CARTESIAN_POINT('Ctrl Pts',(-20.5127231878534,24.6271108015433,-50.7495030229306));
#17099=CARTESIAN_POINT('Ctrl Pts',(-20.5084921676235,24.6150633065856,-50.7503000203109));
#17100=CARTESIAN_POINT('Ctrl Pts',(-20.5074212254287,24.6119990836494,-50.7505023524568));
#17101=CARTESIAN_POINT('Ctrl Pts',(-20.5057521360045,24.6072001510443,-50.7508186274262));
#17102=CARTESIAN_POINT('Ctrl Pts',(-20.5051508414509,24.6054665505182,-50.750932758236));
#17103=CARTESIAN_POINT('Ctrl Pts',(-20.5039998343296,24.602138889382,-50.751151596795));
#17104=CARTESIAN_POINT('Ctrl Pts',(-20.5034498957715,24.6005449211943,-50.7512563174541));
#17105=CARTESIAN_POINT('Ctrl Pts',(-20.5021520115566,24.5967734738717,-50.7515038486648));
#17106=CARTESIAN_POINT('Ctrl Pts',(-20.5014051489639,24.5945956267435,-50.7516465938053));
#17107=CARTESIAN_POINT('Ctrl Pts',(-20.4992215740068,24.5882060280696,-50.7520648328016));
#17108=CARTESIAN_POINT('Ctrl Pts',(-20.4977912431168,24.5839920770854,-50.7523399467391));
#17109=CARTESIAN_POINT('Ctrl Pts',(-20.4872539421143,24.5527351791487,-50.7543753940437));
#17110=CARTESIAN_POINT('Ctrl Pts',(-20.4784973996368,24.5255742031726,-50.7561152636928));
#17111=CARTESIAN_POINT('Ctrl Pts',(-20.4506255884674,24.4350202791087,-50.7618316675569));
#17112=CARTESIAN_POINT('Ctrl Pts',(-20.4331019729121,24.3711513177017,-50.7657275692437));
#17113=CARTESIAN_POINT('Ctrl Pts',(-20.3743734820889,24.1279643427228,-50.7802080043999));
#17114=CARTESIAN_POINT('Ctrl Pts',(-20.3465767972757,23.9457644941269,-50.7903563699776));
#17115=CARTESIAN_POINT('Ctrl Pts',(-20.3195256562256,23.5352883572622,-50.8134044793081));
#17116=CARTESIAN_POINT('Ctrl Pts',(-20.3286280083119,23.3074920722334,-50.8263549843491));
#17117=CARTESIAN_POINT('Ctrl Pts',(-20.3636584581088,23.0686578907003,-50.8410093998726));
#17118=CARTESIAN_POINT('Ctrl Pts',(-20.3657895074648,23.0547624454579,-50.8418656753381));
#17119=CARTESIAN_POINT('Ctrl Pts',(-20.3688608738422,23.0355744096435,-50.8430533238444));
#17120=CARTESIAN_POINT('Ctrl Pts',(-20.3697236427263,23.0302694205698,-50.8433822309543));
#17121=CARTESIAN_POINT('Ctrl Pts',(-20.371122273503,23.0218032492617,-50.8439080223152));
#17122=CARTESIAN_POINT('Ctrl Pts',(-20.3716495918545,23.0186406494224,-50.8441046344678));
#17123=CARTESIAN_POINT('Ctrl Pts',(-20.3727313470763,23.0122119583332,-50.8445046994295));
#17124=CARTESIAN_POINT('Ctrl Pts',(-20.373286102112,23.0089459249933,-50.8447081621604));
#17125=CARTESIAN_POINT('Ctrl Pts',(-20.3745753363711,23.001426012113,-50.8451771218889));
#17126=CARTESIAN_POINT('Ctrl Pts',(-20.3753133274638,22.9971727484424,-50.8454427304903));
#17127=CARTESIAN_POINT('Ctrl Pts',(-20.3768799635295,22.9882502231419,-50.846000697158));
#17128=CARTESIAN_POINT('Ctrl Pts',(-20.3777103728771,22.9835812854327,-50.8462931109964));
#17129=CARTESIAN_POINT('Ctrl Pts',(-20.3799356155677,22.9712281746823,-50.8470679645034));
#17130=CARTESIAN_POINT('Ctrl Pts',(-20.3813480744009,22.9635472449331,-50.8475509661928));
#17131=CARTESIAN_POINT('Ctrl Pts',(-20.385675601702,22.940485793652,-50.8490048282376));
#17132=CARTESIAN_POINT('Ctrl Pts',(-20.388674798009,22.9251214729749,-50.849978370961));
#17133=CARTESIAN_POINT('Ctrl Pts',(-20.4242875329017,22.7494986262119,-50.8611640393299));
#17134=CARTESIAN_POINT('Ctrl Pts',(-20.468937090516,22.59194969029,-50.8717667387811));
#17135=CARTESIAN_POINT('Ctrl Pts',(-20.6342037865814,22.1422883491935,-50.903647855608));
#17136=CARTESIAN_POINT('Ctrl Pts',(-20.7859736658164,21.8636991125608,-50.925660281041));
#17137=CARTESIAN_POINT('Ctrl Pts',(-20.985644326228,21.5985430261241,-50.946669475454));
#17138=CARTESIAN_POINT('Ctrl Pts',(-20.9955858337069,21.5855481440441,-50.9476987560067));
#17139=CARTESIAN_POINT('Ctrl Pts',(-21.0078341708892,21.5697880940986,-50.9489460505656));
#17140=CARTESIAN_POINT('Ctrl Pts',(-21.0100469908302,21.5669506584499,-50.949170573052));
#17141=CARTESIAN_POINT('Ctrl Pts',(-21.0136998621713,21.5622828284069,-50.9495398576055));
#17142=CARTESIAN_POINT('Ctrl Pts',(-21.0151371456787,21.5604502887286,-50.9496848157399));
#17143=CARTESIAN_POINT('Ctrl Pts',(-21.017730332841,21.5571513397717,-50.9499457334934));
#17144=CARTESIAN_POINT('Ctrl Pts',(-21.0188855217576,21.5556843804415,-50.9500617437598));
#17145=CARTESIAN_POINT('Ctrl Pts',(-21.0213702446299,21.5525346988116,-50.9503107983834));
#17146=CARTESIAN_POINT('Ctrl Pts',(-21.0227001798117,21.5508523040752,-50.9504438128606));
#17147=CARTESIAN_POINT('Ctrl Pts',(-21.0263419279145,21.5462548599001,-50.9508072548323));
#17148=CARTESIAN_POINT('Ctrl Pts',(-21.0286571201018,21.5433424726742,-50.951037439623));
#17149=CARTESIAN_POINT('Ctrl Pts',(-21.0406354140028,21.5283278735181,-50.9522239290978));
#17150=CARTESIAN_POINT('Ctrl Pts',(-21.0503808302072,21.5162911506554,-50.9531743893107));
#17151=CARTESIAN_POINT('Ctrl Pts',(-21.1091696163747,21.4447410114492,-50.9588231579699));
#17152=CARTESIAN_POINT('Ctrl Pts',(-21.1602537452573,21.3869281243936,-50.9633830750513));
#17153=CARTESIAN_POINT('Ctrl Pts',(-21.3354527836962,21.2024426561269,-50.9781348699519));
#17154=CARTESIAN_POINT('Ctrl Pts',(-21.4679465270699,21.0841706650467,-50.9879376692314));
#17155=CARTESIAN_POINT('Ctrl Pts',(-21.6909237986502,20.9159755506486,-51.0035684909384));
#17156=CARTESIAN_POINT('Ctrl Pts',(-21.7752094530078,20.8584614589602,-51.0093036930626));
#17157=CARTESIAN_POINT('Ctrl Pts',(-21.9809378944934,20.7319481042448,-51.0231414855137));
#17158=CARTESIAN_POINT('Ctrl Pts',(-22.1044058459751,20.6666596527171,-51.0313277318296));
#17159=CARTESIAN_POINT('Ctrl Pts',(-22.241767387936,20.6050690388056,-51.0404851119107));
#17160=CARTESIAN_POINT('Ctrl Pts',(-22.2518530865624,20.600608815182,-51.0411577085419));
#17161=CARTESIAN_POINT('Ctrl Pts',(-22.2659617965919,20.5944558679757,-51.0420989672463));
#17162=CARTESIAN_POINT('Ctrl Pts',(-22.2699657355052,20.5927193824771,-51.0423661308483));
#17163=CARTESIAN_POINT('Ctrl Pts',(-22.2768891591874,20.5897334271074,-51.0428281748131));
#17164=CARTESIAN_POINT('Ctrl Pts',(-22.2798069938948,20.5884801261164,-51.0430229240539));
#17165=CARTESIAN_POINT('Ctrl Pts',(-22.2857902938033,20.5859205808457,-51.0434223265646));
#17166=CARTESIAN_POINT('Ctrl Pts',(-22.2888559407207,20.5846147746471,-51.0436269944535));
#17167=CARTESIAN_POINT('Ctrl Pts',(-22.2959923437172,20.5815881054206,-51.0441034988086));
#17168=CARTESIAN_POINT('Ctrl Pts',(-22.3000646181626,20.5798708600037,-51.0443754581047));
#17169=CARTESIAN_POINT('Ctrl Pts',(-22.3086447560199,20.5762734548074,-51.0449485766859));
#17170=CARTESIAN_POINT('Ctrl Pts',(-22.3131533835322,20.5743951568236,-51.0452497985681));
#17171=CARTESIAN_POINT('Ctrl Pts',(-22.3251977049797,20.5694095844722,-51.0460546598658));
#17172=CARTESIAN_POINT('Ctrl Pts',(-22.3327409104562,20.5663206533419,-51.0465589208699));
#17173=CARTESIAN_POINT('Ctrl Pts',(-22.3556723035424,20.5570317116574,-51.0480924866962));
#17174=CARTESIAN_POINT('Ctrl Pts',(-22.371096538562,20.5509219520077,-51.0491248334637));
#17175=CARTESIAN_POINT('Ctrl Pts',(-22.4268255253841,20.5293432200067,-51.0528581423542));
#17176=CARTESIAN_POINT('Ctrl Pts',(-22.4673915138064,20.5145659482325,-51.0555820482971));
#17177=CARTESIAN_POINT('Ctrl Pts',(-22.6046486360784,20.467667502468,-51.0648232969655));
#17178=CARTESIAN_POINT('Ctrl Pts',(-22.7025555605314,20.4393196186817,-51.071458307535));
#17179=CARTESIAN_POINT('Ctrl Pts',(-23.1063876117426,20.3428744107995,-51.098954591283));
#17180=CARTESIAN_POINT('Ctrl Pts',(-23.4200966646547,20.3149267546062,-51.1208013398413));
#17181=CARTESIAN_POINT('Ctrl Pts',(-23.7664128039007,20.3345847012311,-51.1430487047743));
#17182=CARTESIAN_POINT('Ctrl Pts',(-23.7999039736679,20.3370112961244,-51.1451784966865));
#17183=CARTESIAN_POINT('Ctrl Pts',(-23.8383957820652,20.3404057035389,-51.1475966351376));
#17184=CARTESIAN_POINT('Ctrl Pts',(-23.8434378498833,20.3408623150043,-51.1479128018672));
#17185=CARTESIAN_POINT('Ctrl Pts',(-23.850869208306,20.3415529603178,-51.1483779046328));
#17186=CARTESIAN_POINT('Ctrl Pts',(-23.8532593153964,20.3417777827319,-51.1485273578818));
#17187=CARTESIAN_POINT('Ctrl Pts',(-23.8575197968318,20.3421833427278,-51.1487935217528));
#17188=CARTESIAN_POINT('Ctrl Pts',(-23.8593902642088,20.3423630454699,-51.1489102910642));
#17189=CARTESIAN_POINT('Ctrl Pts',(-23.8633271120795,20.3427447483386,-51.1491558826757));
#17190=CARTESIAN_POINT('Ctrl Pts',(-23.8653934498348,20.3429471089222,-51.1492846839897));
#17191=CARTESIAN_POINT('Ctrl Pts',(-23.8708576454707,20.3434875600743,-51.1496250164038));
#17192=CARTESIAN_POINT('Ctrl Pts',(-23.8742551757371,20.3438290554363,-51.149836354296));
#17193=CARTESIAN_POINT('Ctrl Pts',(-23.8896688765324,20.3454030790208,-51.1507939204927));
#17194=CARTESIAN_POINT('Ctrl Pts',(-23.9016788080628,20.3466977791373,-51.1515366695742));
#17195=CARTESIAN_POINT('Ctrl Pts',(-24.1830996645291,20.3786372900485,-51.1688681407623));
#17196=CARTESIAN_POINT('Ctrl Pts',(-24.4476342174609,20.4430994449741,-51.1836520011355));
#17197=CARTESIAN_POINT('Ctrl Pts',(-24.7796606343943,20.5700236047337,-51.2035742041776));
#17198=CARTESIAN_POINT('Ctrl Pts',(-24.8571071608163,20.6031626371346,-51.2083197648294));
#17199=CARTESIAN_POINT('Ctrl Pts',(-25.063821796896,20.7013668172127,-51.2214090449272));
#17200=CARTESIAN_POINT('Ctrl Pts',(-25.1901350865688,20.7721563426756,-51.2298822940286));
#17201=CARTESIAN_POINT('Ctrl Pts',(-25.3205620314773,20.857253223562,-51.2393551503458));
#17202=CARTESIAN_POINT('Ctrl Pts',(-25.3298353183021,20.8633721660326,-51.2400327365532));
#17203=CARTESIAN_POINT('Ctrl Pts',(-25.3427185408006,20.871969063205,-51.2409798590476));
#17204=CARTESIAN_POINT('Ctrl Pts',(-25.3463554219401,20.8744066581942,-51.2412478720568));
#17205=CARTESIAN_POINT('Ctrl Pts',(-25.3526246396796,20.8786270986313,-51.2417109884189));
#17206=CARTESIAN_POINT('Ctrl Pts',(-25.3552593331547,20.8804064468412,-51.2419059592086));
#17207=CARTESIAN_POINT('Ctrl Pts',(-25.3606482592205,20.884057497316,-51.2423054500769));
#17208=CARTESIAN_POINT('Ctrl Pts',(-25.3634022312676,20.8859295748447,-51.242509984226));
#17209=CARTESIAN_POINT('Ctrl Pts',(-25.369794000597,20.8902890307971,-51.242985573136));
#17210=CARTESIAN_POINT('Ctrl Pts',(-25.3734296008231,20.8927796047472,-51.2432567493032));
#17211=CARTESIAN_POINT('Ctrl Pts',(-25.3810692196801,20.8980361942621,-51.2438279863253));
#17212=CARTESIAN_POINT('Ctrl Pts',(-25.3850721012694,20.9008038357887,-51.2441281088905));
#17213=CARTESIAN_POINT('Ctrl Pts',(-25.3957277470957,20.9082070098693,-51.2449292189247));
#17214=CARTESIAN_POINT('Ctrl Pts',(-25.4023692793907,20.9128585791288,-51.2454308203781));
#17215=CARTESIAN_POINT('Ctrl Pts',(-25.4224498126903,20.927035756903,-51.2469543730466));
#17216=CARTESIAN_POINT('Ctrl Pts',(-25.4358332418582,20.936639271146,-51.2479793197093));
#17217=CARTESIAN_POINT('Ctrl Pts',(-25.5972046479728,21.0543187514229,-51.2604549166099));
#17218=CARTESIAN_POINT('Ctrl Pts',(-25.7357621252395,21.1747050699207,-51.2723999740091));
#17219=CARTESIAN_POINT('Ctrl Pts',(-26.0688852696336,21.5180723732423,-51.3044084450203));
#17220=CARTESIAN_POINT('Ctrl Pts',(-26.2443585050461,21.7571912446087,-51.3249072531888));
#17221=CARTESIAN_POINT('Ctrl Pts',(-26.3922382351895,22.0305560530528,-51.3445658413584));
#17222=CARTESIAN_POINT('Ctrl Pts',(-26.3995493922707,22.0443084591247,-51.3455452349742));
#17223=CARTESIAN_POINT('Ctrl Pts',(-26.4083971639271,22.0612463814005,-51.3467392656973));
#17224=CARTESIAN_POINT('Ctrl Pts',(-26.4100284452235,22.0643818175785,-51.3469597856966));
#17225=CARTESIAN_POINT('Ctrl Pts',(-26.4127169242311,22.069570089161,-51.347323832487));
#17226=CARTESIAN_POINT('Ctrl Pts',(-26.4137770738864,22.0716213773827,-51.3474675459373));
#17227=CARTESIAN_POINT('Ctrl Pts',(-26.4156044220633,22.0751664573148,-51.3477155327629));
#17228=CARTESIAN_POINT('Ctrl Pts',(-26.4163726562595,22.0766597066307,-51.3478198721848));
#17229=CARTESIAN_POINT('Ctrl Pts',(-26.4180961413374,22.0800161639207,-51.3480541384553));
#17230=CARTESIAN_POINT('Ctrl Pts',(-26.4190507421148,22.0818796994603,-51.3481840235282));
#17231=CARTESIAN_POINT('Ctrl Pts',(-26.4215930542813,22.0868546474855,-51.3485302874222));
#17232=CARTESIAN_POINT('Ctrl Pts',(-26.4231775299967,22.0899677243499,-51.3487464607814));
#17233=CARTESIAN_POINT('Ctrl Pts',(-26.430579009352,22.1045683527065,-51.3497580150938));
#17234=CARTESIAN_POINT('Ctrl Pts',(-26.4363323004514,22.1160883343945,-51.3505494175845));
#17235=CARTESIAN_POINT('Ctrl Pts',(-26.5720887719039,22.3920428999539,-51.369354339184));
#17236=CARTESIAN_POINT('Ctrl Pts',(-26.6653106962469,22.6730842376335,-51.3852574007824));
#17237=CARTESIAN_POINT('Ctrl Pts',(-26.754926724025,23.1565857376758,-51.4129306387781));
#17238=CARTESIAN_POINT('Ctrl Pts',(-26.7729866310584,23.3530913192336,-51.4242445420252));
#17239=CARTESIAN_POINT('Ctrl Pts',(-26.7730025211998,23.5499924521692,-51.4361781865152));
#17240=CARTESIAN_POINT('Ctrl Pts',(-26.7730025212924,23.5499936018635,-51.436178256195));
#17241=CARTESIAN_POINT('Ctrl Pts',(-26.7730036694541,23.564284106563,-51.4370443651463));
#17242=CARTESIAN_POINT('Ctrl Pts',(-26.7729097659511,23.5785743256242,-51.4379134002376));
#17243=CARTESIAN_POINT('Ctrl Pts',(-26.772653767245,23.5979343931753,-51.4390948872342));
#17244=CARTESIAN_POINT('Ctrl Pts',(-26.7725747424517,23.6030052793834,-51.4394047328048));
#17245=CARTESIAN_POINT('Ctrl Pts',(-26.7724192226876,23.6116716775646,-51.4399349394188));
#17246=CARTESIAN_POINT('Ctrl Pts',(-26.7723486780014,23.6152672978123,-51.4401551136329));
#17247=CARTESIAN_POINT('Ctrl Pts',(-26.7722054168766,23.6219950120331,-51.4405674475457));
#17248=CARTESIAN_POINT('Ctrl Pts',(-26.7721341514057,23.6251271353701,-51.4407595614916));
#17249=CARTESIAN_POINT('Ctrl Pts',(-26.771979449176,23.6315166008643,-51.4411517772963));
#17250=CARTESIAN_POINT('Ctrl Pts',(-26.7718956393233,23.6347739296146,-51.4413518906462));
#17251=CARTESIAN_POINT('Ctrl Pts',(-26.7716885671897,23.6423736663668,-51.4418191618513));
#17252=CARTESIAN_POINT('Ctrl Pts',(-26.7715614646836,23.646715955801,-51.4420864400082));
#17253=CARTESIAN_POINT('Ctrl Pts',(-26.7712073090244,23.6580327738193,-51.4427837835971));
#17254=CARTESIAN_POINT('Ctrl Pts',(-26.770966382813,23.6650068178115,-51.4432142841619));
#17255=CARTESIAN_POINT('Ctrl Pts',(-26.7698809013161,23.6937245739015,-51.4449901683132));
#17256=CARTESIAN_POINT('Ctrl Pts',(-26.7688388009666,23.7154598414678,-51.4463417437686));
#17257=CARTESIAN_POINT('Ctrl Pts',(-26.745420974231,24.1185132049987,-51.4715484643977));
#17258=CARTESIAN_POINT('Ctrl Pts',(-26.6556390275667,24.4928170257909,-51.4978802048695));
#17259=CARTESIAN_POINT('Ctrl Pts',(-26.4702590529652,24.9163303656281,-51.5286790372521));
#17260=CARTESIAN_POINT('Ctrl Pts',(-26.4351990352113,24.9888951366271,-51.5339734477163));
#17261=CARTESIAN_POINT('Ctrl Pts',(-26.3824906048417,25.0882919125751,-51.5411778603223));
#17262=CARTESIAN_POINT('Ctrl Pts',(-26.3671083522227,25.1162860940888,-51.5432013611107));
#17263=CARTESIAN_POINT('Ctrl Pts',(-26.3490490468443,25.148024906892,-51.5454851256712));
#17264=CARTESIAN_POINT('Ctrl Pts',(-26.3467778555827,25.1519967714617,-51.5457707324011));
#17265=CARTESIAN_POINT('Ctrl Pts',(-26.3433380859656,25.1579826304651,-51.546200859667));
#17266=CARTESIAN_POINT('Ctrl Pts',(-26.3421757831382,25.1600001958026,-51.5463457846553));
#17267=CARTESIAN_POINT('Ctrl Pts',(-26.3401664370759,25.1634793653379,-51.5465956074293));
#17268=CARTESIAN_POINT('Ctrl Pts',(-26.3393204323216,25.1649415611888,-51.5467005727758));
#17269=CARTESIAN_POINT('Ctrl Pts',(-26.3375592362298,25.1679800178544,-51.5469186329217));
#17270=CARTESIAN_POINT('Ctrl Pts',(-26.3366438598279,25.1695561632495,-51.5470317150025));
#17271=CARTESIAN_POINT('Ctrl Pts',(-26.3341252902424,25.1738843158271,-51.5473421548982));
#17272=CARTESIAN_POINT('Ctrl Pts',(-26.3325193483289,25.176634733852,-51.5475393332184));
#17273=CARTESIAN_POINT('Ctrl Pts',(-26.3263129569081,25.1872280209547,-51.5482984113393));
#17274=CARTESIAN_POINT('Ctrl Pts',(-26.3216833441406,25.1950538854765,-51.5488584282042));
#17275=CARTESIAN_POINT('Ctrl Pts',(-26.2447018885549,25.3239349518066,-51.5580703769067));
#17276=CARTESIAN_POINT('Ctrl Pts',(-26.1645029373227,25.4401500692814,-51.5662224541106));
#17277=CARTESIAN_POINT('Ctrl Pts',(-25.9575071527404,25.7015914472988,-51.58510858733));
#17278=CARTESIAN_POINT('Ctrl Pts',(-25.8248110361358,25.8414356486262,-51.5956817586266));
#17279=CARTESIAN_POINT('Ctrl Pts',(-25.5642414380616,26.0709549655142,-51.6153880568697));
#17280=CARTESIAN_POINT('Ctrl Pts',(-25.4408419877386,26.1647800380138,-51.6243689863156));
#17281=CARTESIAN_POINT('Ctrl Pts',(-25.298435692277,26.2576876767086,-51.6346380324984));
#17282=CARTESIAN_POINT('Ctrl Pts',(-25.2856240598996,26.2659172890256,-51.6355609552479));
#17283=CARTESIAN_POINT('Ctrl Pts',(-25.266287114674,26.2781457538515,-51.6369527610517));
#17284=CARTESIAN_POINT('Ctrl Pts',(-25.2598049717878,26.2822127390288,-51.6374191242336));
#17285=CARTESIAN_POINT('Ctrl Pts',(-25.2493382308296,26.2887278774802,-51.6381718693823));
#17286=CARTESIAN_POINT('Ctrl Pts',(-25.2453626549264,26.2911905284825,-51.6384577162642));
#17287=CARTESIAN_POINT('Ctrl Pts',(-25.2377478016283,26.2958846082984,-51.639005107057));
#17288=CARTESIAN_POINT('Ctrl Pts',(-25.2341094205912,26.2981174780778,-51.6392665972251));
#17289=CARTESIAN_POINT('Ctrl Pts',(-25.2276431156204,26.3020681758735,-51.639731239886));
#17290=CARTESIAN_POINT('Ctrl Pts',(-25.2248169569995,26.3037888935321,-51.6399342857869));
#17291=CARTESIAN_POINT('Ctrl Pts',(-25.2192325960557,26.3071771762468,-51.6403354374103));
#17292=CARTESIAN_POINT('Ctrl Pts',(-25.2164745315431,26.3088449622772,-51.6405335347295));
#17293=CARTESIAN_POINT('Ctrl Pts',(-25.2098233058674,26.3128533068648,-51.6410111930357));
#17294=CARTESIAN_POINT('Ctrl Pts',(-25.2059276965522,26.3151897725022,-51.6412909035125));
#17295=CARTESIAN_POINT('Ctrl Pts',(-25.1916268140821,26.3237259376996,-51.6423175439621));
#17296=CARTESIAN_POINT('Ctrl Pts',(-25.1811916536026,26.3298751396929,-51.6430663138612));
#17297=CARTESIAN_POINT('Ctrl Pts',(-25.0003776997322,26.4350559497767,-51.6560352379119));
#17298=CARTESIAN_POINT('Ctrl Pts',(-24.8213368479422,26.5182943918469,-51.6688360912537));
#17299=CARTESIAN_POINT('Ctrl Pts',(-24.5405378854017,26.61875363175,-51.6887796924346));
#17300=CARTESIAN_POINT('Ctrl Pts',(-24.4436780041307,26.6483412555545,-51.6956288440029));
#17301=CARTESIAN_POINT('Ctrl Pts',(-24.2700465053489,26.692559187397,-51.7077572734322));
#17302=CARTESIAN_POINT('Ctrl Pts',(-24.1938283139689,26.709050595567,-51.7130310825922));
#17303=CARTESIAN_POINT('Ctrl Pts',(-23.9917732260967,26.7451518347319,-51.7267844979734));
#17304=CARTESIAN_POINT('Ctrl Pts',(-23.865226894629,26.7601001402267,-51.7351713682567));
#17305=CARTESIAN_POINT('Ctrl Pts',(-23.7301585549299,26.76798696434,-51.7436663171584));
#17306=CARTESIAN_POINT('Ctrl Pts',(-23.7222020128434,26.7684219547318,-51.7441650439996));
#17307=CARTESIAN_POINT('Ctrl Pts',(-23.7113305142686,26.7689758741898,-51.7448441010364));
#17308=CARTESIAN_POINT('Ctrl Pts',(-23.7084169752362,26.7691203576474,-51.7450258531578));
#17309=CARTESIAN_POINT('Ctrl Pts',(-23.7035391603307,26.769355611517,-51.7453297446951));
#17310=CARTESIAN_POINT('Ctrl Pts',(-23.7015749977616,26.7694485400722,-51.745452006065));
#17311=CARTESIAN_POINT('Ctrl Pts',(-23.6977043824371,26.7696281165326,-51.745692723252));
#17312=CARTESIAN_POINT('Ctrl Pts',(-23.6957979376536,26.7697148686969,-51.745811184782));
#17313=CARTESIAN_POINT('Ctrl Pts',(-23.6915918973804,26.7699025195815,-51.7460723142505));
#17314=CARTESIAN_POINT('Ctrl Pts',(-23.6892922645835,26.770002648326,-51.7462149385553));
#17315=CARTESIAN_POINT('Ctrl Pts',(-23.6812458298729,26.7703443630428,-51.746713474016));
#17316=CARTESIAN_POINT('Ctrl Pts',(-23.6754984460422,26.7705730295073,-51.7470686595638));
#17317=CARTESIAN_POINT('Ctrl Pts',(-23.6168146182565,26.7727504927695,-51.7506863134718));
#17318=CARTESIAN_POINT('Ctrl Pts',(-23.5638346141267,26.773409361336,-51.7538777836002));
#17319=CARTESIAN_POINT('Ctrl Pts',(-23.4924288516575,26.7725364573219,-51.7581075298641));
#17320=CARTESIAN_POINT('Ctrl Pts',(-23.4740008345274,26.772153054801,-51.7591926816894));
#17321=CARTESIAN_POINT('Ctrl Pts',(-23.4016341088597,26.7700261961374,-51.7634322605402));
#17322=CARTESIAN_POINT('Ctrl Pts',(-23.3477373517381,26.7670860678997,-51.7665422522284));
#17323=CARTESIAN_POINT('Ctrl Pts',(-23.2302324153437,26.7577108519871,-51.7732661465508));
#17324=CARTESIAN_POINT('Ctrl Pts',(-23.1666906349007,26.7507341331022,-51.7768659469478));
#17325=CARTESIAN_POINT('Ctrl Pts',(-22.9562308121514,26.721267845123,-51.7887809163077));
#17326=CARTESIAN_POINT('Ctrl Pts',(-22.8106692946528,26.6905098000263,-51.7970167334664));
#17327=CARTESIAN_POINT('Ctrl Pts',(-22.518633440772,26.6073619704652,-51.8142476960407));
#17328=CARTESIAN_POINT('Ctrl Pts',(-22.3727933997389,26.5542060149213,-51.8232399775527));
#17329=CARTESIAN_POINT('Ctrl Pts',(-22.2174526948579,26.484531718338,-51.8335220374645));
#17330=CARTESIAN_POINT('Ctrl Pts',(-22.2035940315537,26.4781973095084,-51.834445596212));
#17331=CARTESIAN_POINT('Ctrl Pts',(-22.1828403447308,26.4685328630459,-51.8358382788749));
#17332=CARTESIAN_POINT('Ctrl Pts',(-22.1759112844077,26.4652760849147,-51.8363048791042));
#17333=CARTESIAN_POINT('Ctrl Pts',(-22.1647672318393,26.45998962148,-51.8370579613755));
#17334=CARTESIAN_POINT('Ctrl Pts',(-22.1605449104506,26.4579753821192,-51.8373439076827));
#17335=CARTESIAN_POINT('Ctrl Pts',(-22.1524767292414,26.4541049048096,-51.8378914882975));
#17336=CARTESIAN_POINT('Ctrl Pts',(-22.1486301411065,26.4522502010068,-51.838153068823));
#17337=CARTESIAN_POINT('Ctrl Pts',(-22.1418095704548,26.448944812103,-51.8386178108513));
#17338=CARTESIAN_POINT('Ctrl Pts',(-22.1388341086926,26.4474971790524,-51.8388208655916));
#17339=CARTESIAN_POINT('Ctrl Pts',(-22.1329650974872,26.444630578436,-51.8392220034561));
#17340=CARTESIAN_POINT('Ctrl Pts',(-22.1300714359481,26.4432118476508,-51.8394200781282));
#17341=CARTESIAN_POINT('Ctrl Pts',(-22.1231054100691,26.4397835106682,-51.8398976305233));
#17342=CARTESIAN_POINT('Ctrl Pts',(-22.119035163781,26.4377696365212,-51.8401772575919));
#17343=CARTESIAN_POINT('Ctrl Pts',(-22.1065408601127,26.4315548040674,-51.8410374535993));
#17344=CARTESIAN_POINT('Ctrl Pts',(-22.0981309981334,26.427325562431,-51.84161901497));
#17345=CARTESIAN_POINT('Ctrl Pts',(-22.0848319909862,26.4205644510068,-51.842542785673));
#17346=CARTESIAN_POINT('Ctrl Pts',(-22.0799306944496,26.4180568426721,-51.8428841275687));
#17347=CARTESIAN_POINT('Ctrl Pts',(-22.0750360141197,26.4155367739249,-51.843225903739));
#17348=CARTESIAN_POINT('Ctrl Pts',(-22.0750360382923,26.4155367863703,-52.0916569661403));
#17349=CARTESIAN_POINT('Ctrl Pts',(-22.0944602758593,26.4255375238482,-52.0904300742972));
#17350=CARTESIAN_POINT('Ctrl Pts',(-22.1139899917392,26.435342689167,-52.0892054490706));
#17351=CARTESIAN_POINT('Ctrl Pts',(-22.2686975094169,26.5110546796618,-52.079564296515));
#17352=CARTESIAN_POINT('Ctrl Pts',(-22.4082323090169,26.567622372871,-52.0712164686481));
#17353=CARTESIAN_POINT('Ctrl Pts',(-22.6571165825054,26.648774172461,-52.0562980725477));
#17354=CARTESIAN_POINT('Ctrl Pts',(-22.7647416847825,26.6777910699522,-52.0498402380234));
#17355=CARTESIAN_POINT('Ctrl Pts',(-22.9221673782742,26.7115955183053,-52.0402484156041));
#17356=CARTESIAN_POINT('Ctrl Pts',(-22.9709206878647,26.7208920000694,-52.0372587295405));
#17357=CARTESIAN_POINT('Ctrl Pts',(-23.0276747177715,26.7303614362018,-52.0337500668831));
#17358=CARTESIAN_POINT('Ctrl Pts',(-23.0354869093704,26.7316353392866,-52.0332664837724));
#17359=CARTESIAN_POINT('Ctrl Pts',(-23.0473727921776,26.7335285970121,-52.0325297728197));
#17360=CARTESIAN_POINT('Ctrl Pts',(-23.0514431483326,26.7341689469385,-52.0322773126342));
#17361=CARTESIAN_POINT('Ctrl Pts',(-23.0588218622904,26.7353152721947,-52.0318193399827));
#17362=CARTESIAN_POINT('Ctrl Pts',(-23.0621298065346,26.7358239041175,-52.0316139122222));
#17363=CARTESIAN_POINT('Ctrl Pts',(-23.0687433907608,26.7368302703849,-52.0312029686578));
#17364=CARTESIAN_POINT('Ctrl Pts',(-23.0720490248952,26.7373280161271,-52.0309974534865));
#17365=CARTESIAN_POINT('Ctrl Pts',(-23.0813489744693,26.7387135611872,-52.0304189370871));
#17366=CARTESIAN_POINT('Ctrl Pts',(-23.0873450047798,26.7395895949876,-52.0300455629974));
#17367=CARTESIAN_POINT('Ctrl Pts',(-23.111981878885,26.7431181591284,-52.0285098220641));
#17368=CARTESIAN_POINT('Ctrl Pts',(-23.1306430290408,26.7456241722117,-52.0273428214682));
#17369=CARTESIAN_POINT('Ctrl Pts',(-23.1640333561768,26.7498106347543,-52.0252477044594));
#17370=CARTESIAN_POINT('Ctrl Pts',(-23.1787543044849,26.7515532613535,-52.024321593746));
#17371=CARTESIAN_POINT('Ctrl Pts',(-23.1986194097384,26.7537659752613,-52.0230685019021));
#17372=CARTESIAN_POINT('Ctrl Pts',(-23.2037536066594,26.7543253663877,-52.0227443346885));
#17373=CARTESIAN_POINT('Ctrl Pts',(-23.2146324125687,26.7554842016428,-52.0220568155192));
#17374=CARTESIAN_POINT('Ctrl Pts',(-23.2203773270289,26.7560805481435,-52.0216933680463));
#17375=CARTESIAN_POINT('Ctrl Pts',(-23.2310744049971,26.757161891972,-52.0210159130463));
#17376=CARTESIAN_POINT('Ctrl Pts',(-23.2360261562994,26.7576508708719,-52.0207020303228));
#17377=CARTESIAN_POINT('Ctrl Pts',(-23.2478186954159,26.7587877977416,-52.0199538420098));
#17378=CARTESIAN_POINT('Ctrl Pts',(-23.2546604415329,26.7594253369291,-52.0195192165184));
#17379=CARTESIAN_POINT('Ctrl Pts',(-23.2652194806505,26.7603752143709,-52.0188476022211));
#17380=CARTESIAN_POINT('Ctrl Pts',(-23.2689353941579,26.7607029901135,-52.0186110877008));
#17381=CARTESIAN_POINT('Ctrl Pts',(-23.283166141259,26.7619333687518,-52.0177046933082));
#17382=CARTESIAN_POINT('Ctrl Pts',(-23.2936847278869,26.7627907644519,-52.0170334397426));
#17383=CARTESIAN_POINT('Ctrl Pts',(-23.3249327906844,26.7651834242278,-52.0150354407307));
#17384=CARTESIAN_POINT('Ctrl Pts',(-23.3456728233556,26.7665697954185,-52.0137042613274));
#17385=CARTESIAN_POINT('Ctrl Pts',(-23.6686483442261,26.7850226062479,-51.9928953221564));
#17386=CARTESIAN_POINT('Ctrl Pts',(-23.9717713427006,26.759616119192,-51.9720794330503));
#17387=CARTESIAN_POINT('Ctrl Pts',(-24.3322351210805,26.6774115952042,-51.9473575928224));
#17388=CARTESIAN_POINT('Ctrl Pts',(-24.3971819737005,26.6604506227334,-51.942914114474));
#17389=CARTESIAN_POINT('Ctrl Pts',(-24.5104023337608,26.6270728565242,-51.9352378830386));
#17390=CARTESIAN_POINT('Ctrl Pts',(-24.5589045377762,26.6115157998673,-51.9319727011703));
#17391=CARTESIAN_POINT('Ctrl Pts',(-24.612817154255,26.592802717127,-51.928385115289));
#17392=CARTESIAN_POINT('Ctrl Pts',(-24.6186078045001,26.5907742337236,-51.9280003267181));
#17393=CARTESIAN_POINT('Ctrl Pts',(-24.6275597757297,26.5876095980357,-51.9274063549016));
#17394=CARTESIAN_POINT('Ctrl Pts',(-24.6307251343487,26.5864850329469,-51.9271965022155));
#17395=CARTESIAN_POINT('Ctrl Pts',(-24.6359824289321,26.5846079978574,-51.9268482538467));
#17396=CARTESIAN_POINT('Ctrl Pts',(-24.6380753453527,26.5838583121055,-51.9267096941818));
#17397=CARTESIAN_POINT('Ctrl Pts',(-24.642067767234,26.582423557765,-51.9264455290876));
#17398=CARTESIAN_POINT('Ctrl Pts',(-24.6439674066093,26.5817388688468,-51.9263199010695));
#17399=CARTESIAN_POINT('Ctrl Pts',(-24.6474441788392,26.580482038943,-51.9260900933942));
#17400=CARTESIAN_POINT('Ctrl Pts',(-24.6490215000685,26.5799104548481,-51.9259858811078));
#17401=CARTESIAN_POINT('Ctrl Pts',(-24.6524001718527,26.5786831180896,-51.925762752307));
#17402=CARTESIAN_POINT('Ctrl Pts',(-24.6542013787628,26.5780269916609,-51.9256438589628));
#17403=CARTESIAN_POINT('Ctrl Pts',(-24.6594332379648,26.5761158907409,-51.9252986852145));
#17404=CARTESIAN_POINT('Ctrl Pts',(-24.6628623574923,26.5748566847423,-51.925072658772));
#17405=CARTESIAN_POINT('Ctrl Pts',(-24.6783439831259,26.5691417901984,-51.9240531270939));
#17406=CARTESIAN_POINT('Ctrl Pts',(-24.6903721346525,26.5646197923191,-51.9232635477096));
#17407=CARTESIAN_POINT('Ctrl Pts',(-24.8975101061039,26.4853287956925,-51.9097045484926));
#17408=CARTESIAN_POINT('Ctrl Pts',(-25.0849546137523,26.3918179824922,-51.8980072591855));
#17409=CARTESIAN_POINT('Ctrl Pts',(-25.3341159196798,26.235617349404,-51.8815686660606));
#17410=CARTESIAN_POINT('Ctrl Pts',(-25.4043674513326,26.187601656175,-51.8768256195252));
#17411=CARTESIAN_POINT('Ctrl Pts',(-25.5528892293528,26.0772194463773,-51.8664119769963));
#17412=CARTESIAN_POINT('Ctrl Pts',(-25.6303186225467,26.0138756113528,-51.8607297364876));
#17413=CARTESIAN_POINT('Ctrl Pts',(-25.7538376891319,25.9028468228143,-51.8510898653242));
#17414=CARTESIAN_POINT('Ctrl Pts',(-25.8016265927918,25.8571555253527,-51.8472031435511));
#17415=CARTESIAN_POINT('Ctrl Pts',(-25.8788917065523,25.7785930042181,-51.8406209434621));
#17416=CARTESIAN_POINT('Ctrl Pts',(-25.9091591729469,25.7465268389901,-51.8379605244546));
#17417=CARTESIAN_POINT('Ctrl Pts',(-25.9439092182099,25.7081645083122,-51.8348035436568));
#17418=CARTESIAN_POINT('Ctrl Pts',(-25.9490398907663,25.7024596862411,-51.8343347286017));
#17419=CARTESIAN_POINT('Ctrl Pts',(-25.95686028813,25.6937014409633,-51.8336159640884));
#17420=CARTESIAN_POINT('Ctrl Pts',(-25.9595647079522,25.6906611275184,-51.8333666331414));
#17421=CARTESIAN_POINT('Ctrl Pts',(-25.9644810015687,25.6851130982854,-51.8329119701966));
#17422=CARTESIAN_POINT('Ctrl Pts',(-25.966694747484,25.6826070428281,-51.832706717055));
#17423=CARTESIAN_POINT('Ctrl Pts',(-25.9711334454713,25.6775664573033,-51.8322941148941));
#17424=CARTESIAN_POINT('Ctrl Pts',(-25.9733583271021,25.6750318710384,-51.8320867633065));
#17425=CARTESIAN_POINT('Ctrl Pts',(-25.9796665791009,25.6678227133804,-51.8314973260264));
#17426=CARTESIAN_POINT('Ctrl Pts',(-25.9837404126964,25.6631398500943,-51.8311148440127));
#17427=CARTESIAN_POINT('Ctrl Pts',(-26.0008849845853,25.6433168431819,-51.8294974149155));
#17428=CARTESIAN_POINT('Ctrl Pts',(-26.0138279312494,25.6280672137208,-51.8282571969842));
#17429=CARTESIAN_POINT('Ctrl Pts',(-26.2733492822518,25.3164603535922,-51.8029923768085));
#17430=CARTESIAN_POINT('Ctrl Pts',(-26.4648703881453,24.9783886693485,-51.7764301520398));
#17431=CARTESIAN_POINT('Ctrl Pts',(-26.6190031122065,24.5379295180845,-51.7453319152465));
#17432=CARTESIAN_POINT('Ctrl Pts',(-26.6429590267875,24.4601452085407,-51.7399831899107));
#17433=CARTESIAN_POINT('Ctrl Pts',(-26.6722356842628,24.3504846098654,-51.7327141226101));
#17434=CARTESIAN_POINT('Ctrl Pts',(-26.680060041981,24.3193138607931,-51.7306780417303));
#17435=CARTESIAN_POINT('Ctrl Pts',(-26.688466199439,24.2835693354726,-51.7283815803464));
#17436=CARTESIAN_POINT('Ctrl Pts',(-26.6895056878486,24.2791065509039,-51.728095542567));
#17437=CARTESIAN_POINT('Ctrl Pts',(-26.6910593632357,24.2723712462426,-51.7276648919206));
#17438=CARTESIAN_POINT('Ctrl Pts',(-26.6915806042266,24.2701003848977,-51.7275198731515));
#17439=CARTESIAN_POINT('Ctrl Pts',(-26.6925151718729,24.2660084605588,-51.727258884052));
#17440=CARTESIAN_POINT('Ctrl Pts',(-26.692929377438,24.2641876077711,-51.7271428629701));
#17441=CARTESIAN_POINT('Ctrl Pts',(-26.6938157710736,24.2602752916347,-51.7268938268155));
#17442=CARTESIAN_POINT('Ctrl Pts',(-26.6942874533587,24.2581837225802,-51.7267608415514));
#17443=CARTESIAN_POINT('Ctrl Pts',(-26.6955507053046,24.2525559510441,-51.726403424794));
#17444=CARTESIAN_POINT('Ctrl Pts',(-26.6963384015977,24.2490188683528,-51.7261792174017));
#17445=CARTESIAN_POINT('Ctrl Pts',(-26.6999194962568,24.2328094633972,-51.725153682713));
#17446=CARTESIAN_POINT('Ctrl Pts',(-26.7026423576825,24.2201214376259,-51.7243563710701));
#17447=CARTESIAN_POINT('Ctrl Pts',(-26.7501016854109,23.9922699899402,-51.7101299256025));
#17448=CARTESIAN_POINT('Ctrl Pts',(-26.7727983690918,23.7730645285911,-51.6978852062535));
#17449=CARTESIAN_POINT('Ctrl Pts',(-26.77325117555,23.2821927916021,-51.6704564854239));
#17450=CARTESIAN_POINT('Ctrl Pts',(-26.7393135786712,23.0122566572046,-51.6552875631999));
#17451=CARTESIAN_POINT('Ctrl Pts',(-26.6677793148311,22.7332863647463,-51.6378359715757));
#17452=CARTESIAN_POINT('Ctrl Pts',(-26.6634234847531,22.7168417318907,-51.6368009779229));
#17453=CARTESIAN_POINT('Ctrl Pts',(-26.6574041616154,22.6948227370646,-51.6354064742231));
#17454=CARTESIAN_POINT('Ctrl Pts',(-26.6558554220354,22.6892170668814,-51.6350507001506));
#17455=CARTESIAN_POINT('Ctrl Pts',(-26.6534057783083,22.6804431619201,-51.6344926518395));
#17456=CARTESIAN_POINT('Ctrl Pts',(-26.6525151705972,22.6772720445952,-51.6342907134743));
#17457=CARTESIAN_POINT('Ctrl Pts',(-26.6507987944088,22.671196473737,-51.6339033456216));
#17458=CARTESIAN_POINT('Ctrl Pts',(-26.6499738019086,22.6682918028937,-51.6337179416275));
#17459=CARTESIAN_POINT('Ctrl Pts',(-26.6480302146227,22.6614851456829,-51.6332829873689));
#17460=CARTESIAN_POINT('Ctrl Pts',(-26.6469083295029,22.6575841112009,-51.6330333298396));
#17461=CARTESIAN_POINT('Ctrl Pts',(-26.6436575214771,22.6463602327161,-51.6323139367552));
#17462=CARTESIAN_POINT('Ctrl Pts',(-26.6415099832622,22.6390428491901,-51.6318435929266));
#17463=CARTESIAN_POINT('Ctrl Pts',(-26.6270473214732,22.590403288121,-51.6287081686714));
#17464=CARTESIAN_POINT('Ctrl Pts',(-26.6139304365051,22.5493258845263,-51.6260168919555));
#17465=CARTESIAN_POINT('Ctrl Pts',(-26.573637201482,22.4313641277324,-51.6181576116182));
#17466=CARTESIAN_POINT('Ctrl Pts',(-26.5443637019809,22.3552368254296,-51.6129218756975));
#17467=CARTESIAN_POINT('Ctrl Pts',(-26.395053584253,22.006990328839,-51.5881987289899));
#17468=CARTESIAN_POINT('Ctrl Pts',(-26.2406305830803,21.7512598188643,-51.5676242281987));
#17469=CARTESIAN_POINT('Ctrl Pts',(-25.9961280271729,21.4497600773205,-51.54193942183));
#17470=CARTESIAN_POINT('Ctrl Pts',(-25.9359235346717,21.3816232468663,-51.5360373107027));
#17471=CARTESIAN_POINT('Ctrl Pts',(-25.8684572218001,21.3114836986007,-51.5299361951867));
#17472=CARTESIAN_POINT('Ctrl Pts',(-25.863987641658,21.3068647551684,-51.5295342947188));
#17473=CARTESIAN_POINT('Ctrl Pts',(-25.8577742388518,21.3004820357207,-51.5289787992825));
#17474=CARTESIAN_POINT('Ctrl Pts',(-25.8560421921495,21.298706894716,-51.5288242930903));
#17475=CARTESIAN_POINT('Ctrl Pts',(-25.85306307765,21.2956607010867,-51.5285591354109));
#17476=CARTESIAN_POINT('Ctrl Pts',(-25.8518170059294,21.2943886829256,-51.5284484056825));
#17477=CARTESIAN_POINT('Ctrl Pts',(-25.8492422924765,21.2917647111907,-51.5282199763358));
#17478=CARTESIAN_POINT('Ctrl Pts',(-25.847913514779,21.2904128996919,-51.5281022885555));
#17479=CARTESIAN_POINT('Ctrl Pts',(-25.8447934200369,21.2872443161379,-51.5278264175924));
#17480=CARTESIAN_POINT('Ctrl Pts',(-25.8430011321461,21.2854284927928,-51.5276683112942));
#17481=CARTESIAN_POINT('Ctrl Pts',(-25.8371834296547,21.2795483781905,-51.5271562726114));
#17482=CARTESIAN_POINT('Ctrl Pts',(-25.8331493207149,21.2754926461995,-51.5268030248629));
#17483=CARTESIAN_POINT('Ctrl Pts',(-25.7258047875243,21.16814590025,-51.5174505632922));
#17484=CARTESIAN_POINT('Ctrl Pts',(-25.6155843810992,21.0719715418063,-51.5090014812559));
#17485=CARTESIAN_POINT('Ctrl Pts',(-25.2203742665292,20.7718748525581,-51.4808987789746));
#17486=CARTESIAN_POINT('Ctrl Pts',(-24.908944561337,20.607015498601,-51.4619701653074));
#17487=CARTESIAN_POINT('Ctrl Pts',(-24.5575474500855,20.4888966916738,-51.4395540331151));
#17488=CARTESIAN_POINT('Ctrl Pts',(-24.5379425440212,20.4825154111626,-51.4383013293991));
#17489=CARTESIAN_POINT('Ctrl Pts',(-24.5122869261745,20.4744360806918,-51.4366588584812));
#17490=CARTESIAN_POINT('Ctrl Pts',(-24.5062902764446,20.4725669002253,-51.436274730895));
#17491=CARTESIAN_POINT('Ctrl Pts',(-24.4970512119608,20.4697166534585,-51.4356825486539));
#17492=CARTESIAN_POINT('Ctrl Pts',(-24.4938126273699,20.4687231413165,-51.4354749029845));
#17493=CARTESIAN_POINT('Ctrl Pts',(-24.4876838619079,20.4668535655714,-51.4350818208016));
#17494=CARTESIAN_POINT('Ctrl Pts',(-24.484794002366,20.465976454128,-51.4348964189028));
#17495=CARTESIAN_POINT('Ctrl Pts',(-24.4782974285923,20.4640146249744,-51.4344795007577));
#17496=CARTESIAN_POINT('Ctrl Pts',(-24.4746900414402,20.4629321664071,-51.4342479107452));
#17497=CARTESIAN_POINT('Ctrl Pts',(-24.4672039506104,20.4607001330859,-51.4337671315724));
#17498=CARTESIAN_POINT('Ctrl Pts',(-24.4633249652806,20.4595515336705,-51.4335179109159));
#17499=CARTESIAN_POINT('Ctrl Pts',(-24.4535417070031,20.4566746555556,-51.4328890886992));
#17500=CARTESIAN_POINT('Ctrl Pts',(-24.4476346479032,20.4549559794022,-51.432509173585));
#17501=CARTESIAN_POINT('Ctrl Pts',(-24.3649360431675,20.4311512061691,-51.4271869749393));
#17502=CARTESIAN_POINT('Ctrl Pts',(-24.2873600528845,20.4119133270749,-51.422152382408));
#17503=CARTESIAN_POINT('Ctrl Pts',(-24.1383073133034,20.3807813694407,-51.4123861213722));
#17504=CARTESIAN_POINT('Ctrl Pts',(-24.0669861380849,20.368375565872,-51.4076734799077));
#17505=CARTESIAN_POINT('Ctrl Pts',(-23.8282706697898,20.3350902151898,-51.3917824677408));
#17506=CARTESIAN_POINT('Ctrl Pts',(-23.6596700038075,20.3249490776832,-51.3803517546932));
#17507=CARTESIAN_POINT('Ctrl Pts',(-23.3070572731419,20.3314260116111,-51.3564940687527));
#17508=CARTESIAN_POINT('Ctrl Pts',(-23.1236511305305,20.3505623782717,-51.3441156252281));
#17509=CARTESIAN_POINT('Ctrl Pts',(-22.9323261645463,20.3872792991368,-51.3318475428132));
#17510=CARTESIAN_POINT('Ctrl Pts',(-22.9217998279379,20.3893539455351,-51.3311747363232));
#17511=CARTESIAN_POINT('Ctrl Pts',(-22.9079472280528,20.3921561037545,-51.3302923524473));
#17512=CARTESIAN_POINT('Ctrl Pts',(-22.9046116369511,20.3928363433303,-51.3300801132109));
#17513=CARTESIAN_POINT('Ctrl Pts',(-22.8994484827568,20.3938978086633,-51.3297519537983));
#17514=CARTESIAN_POINT('Ctrl Pts',(-22.8976201753688,20.3942753367144,-51.3296358213192));
#17515=CARTESIAN_POINT('Ctrl Pts',(-22.8939636944171,20.3950336784642,-51.3294037082599));
#17516=CARTESIAN_POINT('Ctrl Pts',(-22.8921355353989,20.3954144900626,-51.3292877288838));
#17517=CARTESIAN_POINT('Ctrl Pts',(-22.8880267482298,20.3962740909557,-51.3290272262007));
#17518=CARTESIAN_POINT('Ctrl Pts',(-22.8857463126106,20.3967537640061,-51.3288827547734));
#17519=CARTESIAN_POINT('Ctrl Pts',(-22.8789813305356,20.3981843927773,-51.3284545007411));
#17520=CARTESIAN_POINT('Ctrl Pts',(-22.8744982664322,20.3991424492825,-51.3281711262704));
#17521=CARTESIAN_POINT('Ctrl Pts',(-22.8385478174045,20.4069055155296,-51.3259019889037));
#17522=CARTESIAN_POINT('Ctrl Pts',(-22.8071805313547,20.4141724530473,-51.323942369801));
#17523=CARTESIAN_POINT('Ctrl Pts',(-22.6967159199258,20.4415146134322,-51.3170960638365));
#17524=CARTESIAN_POINT('Ctrl Pts',(-22.6182723452372,20.4641236746936,-51.312333990133));
#17525=CARTESIAN_POINT('Ctrl Pts',(-22.1750010442751,20.610330876928,-51.2855623696668));
#17526=CARTESIAN_POINT('Ctrl Pts',(-21.8338395819266,20.7955446747904,-51.2650698896105));
#17527=CARTESIAN_POINT('Ctrl Pts',(-21.5178240766507,21.049102579892,-51.240561750116));
#17528=CARTESIAN_POINT('Ctrl Pts',(-21.5023620992083,21.0617467039201,-51.2393478768252));
#17529=CARTESIAN_POINT('Ctrl Pts',(-21.4822534188262,21.0785050295087,-51.2377493411908));
#17530=CARTESIAN_POINT('Ctrl Pts',(-21.4774994217515,21.0824902680724,-51.2373699500574));
#17531=CARTESIAN_POINT('Ctrl Pts',(-21.4701792119187,21.0886628184276,-51.2367834714108));
#17532=CARTESIAN_POINT('Ctrl Pts',(-21.4676048577017,21.0908404885469,-51.236576780247));
#17533=CARTESIAN_POINT('Ctrl Pts',(-21.4625353397269,21.0951425081735,-51.2361688853135));
#17534=CARTESIAN_POINT('Ctrl Pts',(-21.4600399886969,21.0972666315719,-51.2359676910047));
#17535=CARTESIAN_POINT('Ctrl Pts',(-21.4545368872986,21.1019655435187,-51.235523062998));
#17536=CARTESIAN_POINT('Ctrl Pts',(-21.4515306367522,21.1045420733403,-51.2352795574505));
#17537=CARTESIAN_POINT('Ctrl Pts',(-21.4453094796805,21.109893880163,-51.234774369141));
#17538=CARTESIAN_POINT('Ctrl Pts',(-21.4420952975684,21.1126699841176,-51.2345126522897));
#17539=CARTESIAN_POINT('Ctrl Pts',(-21.4338775382209,21.1197961119896,-51.2338416898385));
#17540=CARTESIAN_POINT('Ctrl Pts',(-21.4288818982841,21.1241552220767,-51.2334320658743));
#17541=CARTESIAN_POINT('Ctrl Pts',(-21.3222126570088,21.2178143441682,-51.2246480449216));
#17542=CARTESIAN_POINT('Ctrl Pts',(-21.2262640280818,21.3134024529221,-51.2160055639916));
#17543=CARTESIAN_POINT('Ctrl Pts',(-20.9027265161788,21.6790743524155,-51.1839878552845));
#17544=CARTESIAN_POINT('Ctrl Pts',(-20.7138886881856,21.9799995816138,-51.1592019920556));
#17545=CARTESIAN_POINT('Ctrl Pts',(-20.5680105986171,22.3283829022343,-51.1351328512517));
#17546=CARTESIAN_POINT('Ctrl Pts',(-20.5586979092823,22.3513641417916,-51.1335664065855));
#17547=CARTESIAN_POINT('Ctrl Pts',(-20.5481370860205,22.3783149768094,-51.1317560411249));
#17548=CARTESIAN_POINT('Ctrl Pts',(-20.5466305816187,22.3821814879705,-51.1314969529947));
#17549=CARTESIAN_POINT('Ctrl Pts',(-20.5442392615321,22.3883541355109,-51.1310843619695));
#17550=CARTESIAN_POINT('Ctrl Pts',(-20.5433496282864,22.3906583815624,-51.1309305699409));
#17551=CARTESIAN_POINT('Ctrl Pts',(-20.5417841498454,22.3947270547631,-51.1306594200765));
#17552=CARTESIAN_POINT('Ctrl Pts',(-20.5411072066387,22.3964910549615,-51.1305419955694));
#17553=CARTESIAN_POINT('Ctrl Pts',(-20.5397017037959,22.4001632104066,-51.1302978311048));
#17554=CARTESIAN_POINT('Ctrl Pts',(-20.5389734081932,22.4020714594231,-51.1301711073665));
#17555=CARTESIAN_POINT('Ctrl Pts',(-20.5370860831278,22.40703069515,-51.1298421776322));
#17556=CARTESIAN_POINT('Ctrl Pts',(-20.5359298696236,22.4100827621117,-51.1296401421094));
#17557=CARTESIAN_POINT('Ctrl Pts',(-20.5310128279783,22.4231220767256,-51.12877866488));
#17558=CARTESIAN_POINT('Ctrl Pts',(-20.5272969273411,22.4331263648332,-51.1281219018149));
#17559=CARTESIAN_POINT('Ctrl Pts',(-20.4684252477398,22.5940709547398,-51.1176206487024));
#17560=CARTESIAN_POINT('Ctrl Pts',(-20.4245769699635,22.7489346392783,-51.1084199970133));
#17561=CARTESIAN_POINT('Ctrl Pts',(-20.3525187137542,23.1023701891515,-51.0881096158864));
#17562=CARTESIAN_POINT('Ctrl Pts',(-20.3308950044511,23.3015828607029,-51.077106659923));
#17563=CARTESIAN_POINT('Ctrl Pts',(-20.3257385774263,23.6425092801541,-51.0575808891623));
#17564=CARTESIAN_POINT('Ctrl Pts',(-20.3328620788933,23.7834740185373,-51.0493118804113));
#17565=CARTESIAN_POINT('Ctrl Pts',(-20.3504706059953,23.934485994549,-51.0400635701361));
#17566=CARTESIAN_POINT('Ctrl Pts',(-20.3518071796368,23.9454576064803,-51.0393894681638));
#17567=CARTESIAN_POINT('Ctrl Pts',(-20.3537507391579,23.9607558053156,-51.0384464327214));
#17568=CARTESIAN_POINT('Ctrl Pts',(-20.3543101342112,23.9650884498677,-51.0381790051741));
#17569=CARTESIAN_POINT('Ctrl Pts',(-20.3552915346554,23.9725698086195,-51.0377166209411));
#17570=CARTESIAN_POINT('Ctrl Pts',(-20.355709390599,23.9757190692285,-51.0375217958141));
#17571=CARTESIAN_POINT('Ctrl Pts',(-20.3565749810297,23.982169611503,-51.0371223586216));
#17572=CARTESIAN_POINT('Ctrl Pts',(-20.3570231791587,23.985470825685,-51.0369177321179));
#17573=CARTESIAN_POINT('Ctrl Pts',(-20.3580764422194,23.9931394434956,-51.0364419113638));
#17574=CARTESIAN_POINT('Ctrl Pts',(-20.3586853515575,23.9975063044286,-51.0361705955634));
#17575=CARTESIAN_POINT('Ctrl Pts',(-20.3599864640104,24.0066994088877,-51.0355986548238));
#17576=CARTESIAN_POINT('Ctrl Pts',(-20.3606806612871,24.0115253548728,-51.0352979671656));
#17577=CARTESIAN_POINT('Ctrl Pts',(-20.3625616564966,24.0243944380355,-51.0344949417278));
#17578=CARTESIAN_POINT('Ctrl Pts',(-20.3637679382625,24.0324346518951,-51.0339919861131));
#17579=CARTESIAN_POINT('Ctrl Pts',(-20.3917246614464,24.2140868194161,-51.0226001475537));
#17580=CARTESIAN_POINT('Ctrl Pts',(-20.4325895427568,24.3851975183107,-51.0112534193078));
#17581=CARTESIAN_POINT('Ctrl Pts',(-20.5861665038666,24.8547452705939,-50.9784029695819));
#17582=CARTESIAN_POINT('Ctrl Pts',(-20.7294484550355,25.1410279188329,-50.9561787758156));
#17583=CARTESIAN_POINT('Ctrl Pts',(-20.9217725394888,25.4150523901588,-50.9349888361478));
#17584=CARTESIAN_POINT('Ctrl Pts',(-20.9312796977172,25.4283810958436,-50.933958896492));
#17585=CARTESIAN_POINT('Ctrl Pts',(-20.943000574052,25.4445512795666,-50.9327108913504));
#17586=CARTESIAN_POINT('Ctrl Pts',(-20.94511779121,25.4474619300092,-50.932486308949));
#17587=CARTESIAN_POINT('Ctrl Pts',(-20.9486132370446,25.4522504204135,-50.9321169417382));
#17588=CARTESIAN_POINT('Ctrl Pts',(-20.9499886256495,25.4541303132627,-50.9319719607284));
#17589=CARTESIAN_POINT('Ctrl Pts',(-20.9524702875869,25.4575145644505,-50.9317110123444));
#17590=CARTESIAN_POINT('Ctrl Pts',(-20.9535758277237,25.4590194489759,-50.9315949942891));
#17591=CARTESIAN_POINT('Ctrl Pts',(-20.9559538384064,25.4622505577044,-50.9313459344992));
#17592=CARTESIAN_POINT('Ctrl Pts',(-20.9572267206693,25.4639764681293,-50.9312129226274));
#17593=CARTESIAN_POINT('Ctrl Pts',(-20.9607122858286,25.4686927094224,-50.9308495160471));
#17594=CARTESIAN_POINT('Ctrl Pts',(-20.9629284337504,25.4716804936564,-50.9306193639441));
#17595=CARTESIAN_POINT('Ctrl Pts',(-20.9743923525576,25.4870802154808,-50.9294334281529));
#17596=CARTESIAN_POINT('Ctrl Pts',(-20.9837244865469,25.4994295260389,-50.928483482292));
#17597=CARTESIAN_POINT('Ctrl Pts',(-21.0406759791349,25.573675826263,-50.9227755513642));
#17598=CARTESIAN_POINT('Ctrl Pts',(-21.0904475099349,25.6338978377655,-50.9181596634146));
#17599=CARTESIAN_POINT('Ctrl Pts',(-21.1774997288823,25.7317557951212,-50.9105693189738));
#17600=CARTESIAN_POINT('Ctrl Pts',(-21.2136049266329,25.7703855749308,-50.9075477171387));
#17601=CARTESIAN_POINT('Ctrl Pts',(-21.2766902698847,25.8346373928394,-50.9024437090867));
#17602=CARTESIAN_POINT('Ctrl Pts',(-21.3031925922703,25.8607116341073,-50.9003491874576));
#17603=CARTESIAN_POINT('Ctrl Pts',(-21.3534595798391,25.908483480218,-50.8964552259784));
#17604=CARTESIAN_POINT('Ctrl Pts',(-21.3771093710663,25.9302948234613,-50.8946542630287));
#17605=CARTESIAN_POINT('Ctrl Pts',(-21.5477037864088,26.0829648691416,-50.8818523335301));
#17606=CARTESIAN_POINT('Ctrl Pts',(-21.7060229119617,26.2004683146711,-50.8709206884809));
#17607=CARTESIAN_POINT('Ctrl Pts',(-21.9396995371645,26.3427679374918,-50.8550034730067));
#17608=CARTESIAN_POINT('Ctrl Pts',(-22.0067333528666,26.3803705550361,-50.850464096738));
#17609=CARTESIAN_POINT('Ctrl Pts',(-22.0750360284016,26.415536781278,-50.8458393738826));
#17610=CARTESIAN_POINT('Origin',(-23.5502525316942,23.5502525316942,-77.3107734492734));
#17611=CARTESIAN_POINT('',(-22.0750360150599,26.4155367744089,-49.3491334787091));
#17612=CARTESIAN_POINT('',(-22.0750360207194,26.4155367773228,-49.5934531403533));
#17613=CARTESIAN_POINT('',(-22.0750360153461,26.4155367745563,-77.3107734492734));
#17614=CARTESIAN_POINT('Ctrl Pts',(-22.0750360150599,26.4155367744089,-49.3491334787091));
#17615=CARTESIAN_POINT('Ctrl Pts',(-22.0691259159558,26.412493908475,-49.3495623158237));
#17616=CARTESIAN_POINT('Ctrl Pts',(-22.0632250938881,26.4094326859608,-49.3499902916244));
#17617=CARTESIAN_POINT('Ctrl Pts',(-22.0356084854432,26.3949971452919,-49.351992246194));
#17618=CARTESIAN_POINT('Ctrl Pts',(-22.0140128525966,26.3833932332581,-49.3535547529389));
#17619=CARTESIAN_POINT('Ctrl Pts',(-21.9844229622205,26.3670559551105,-49.3556893679477));
#17620=CARTESIAN_POINT('Ctrl Pts',(-21.9763142381812,26.3625331044573,-49.3562736714923));
#17621=CARTESIAN_POINT('Ctrl Pts',(-21.9624531224613,26.3547229791749,-49.3572712021989));
#17622=CARTESIAN_POINT('Ctrl Pts',(-21.9566911673401,26.3514529234272,-49.3576854858052));
#17623=CARTESIAN_POINT('Ctrl Pts',(-21.9485948326466,26.3468249820133,-49.3582670276047));
#17624=CARTESIAN_POINT('Ctrl Pts',(-21.9462520637019,26.3454819236423,-49.3584352345438));
#17625=CARTESIAN_POINT('Ctrl Pts',(-21.9423936544358,26.3432635335765,-49.3587121446412));
#17626=CARTESIAN_POINT('Ctrl Pts',(-21.9408770400775,26.3423899124177,-49.3588209590127));
#17627=CARTESIAN_POINT('Ctrl Pts',(-21.9377093778048,26.3405617934692,-49.3590481693375));
#17628=CARTESIAN_POINT('Ctrl Pts',(-21.9360584649653,26.3396070653584,-49.3591665497985));
#17629=CARTESIAN_POINT('Ctrl Pts',(-21.9324212021028,26.337499314187,-49.3594272856177));
#17630=CARTESIAN_POINT('Ctrl Pts',(-21.9304352317322,26.3363456299852,-49.3595695978266));
#17631=CARTESIAN_POINT('Ctrl Pts',(-21.923506627991,26.3323107729891,-49.3600659198906));
#17632=CARTESIAN_POINT('Ctrl Pts',(-21.9185703970297,26.32941854073,-49.3604192127122));
#17633=CARTESIAN_POINT('Ctrl Pts',(-21.8689354191354,26.3001586310397,-49.3639688206033));
#17634=CARTESIAN_POINT('Ctrl Pts',(-21.8248689323501,26.2727262191741,-49.3670970123069));
#17635=CARTESIAN_POINT('Ctrl Pts',(-21.778063033863,26.2419952139568,-49.3704159454854));
#17636=CARTESIAN_POINT('Ctrl Pts',(-21.7746490484246,26.2397444082848,-49.3706580039756));
#17637=CARTESIAN_POINT('Ctrl Pts',(-21.5389753898331,26.0837228416099,-49.3873669026408));
#17638=CARTESIAN_POINT('Ctrl Pts',(-21.3276013259104,25.9004796844223,-49.4023852707713));
#17639=CARTESIAN_POINT('Ctrl Pts',(-21.0590572699968,25.5986155227901,-49.4252893958585));
#17640=CARTESIAN_POINT('Ctrl Pts',(-20.981250299577,25.5001416371026,-49.4325201041075));
#17641=CARTESIAN_POINT('Ctrl Pts',(-20.8788210679617,25.353697762684,-49.4431469877096));
#17642=CARTESIAN_POINT('Ctrl Pts',(-20.8493499999454,25.3092538869737,-49.4463558825097));
#17643=CARTESIAN_POINT('Ctrl Pts',(-20.8167105517051,25.2572764774925,-49.4500981094948));
#17644=CARTESIAN_POINT('Ctrl Pts',(-20.8124505142066,25.250435645089,-49.4505904184373));
#17645=CARTESIAN_POINT('Ctrl Pts',(-20.8060355151092,25.2400477126223,-49.4513377065188));
#17646=CARTESIAN_POINT('Ctrl Pts',(-20.8038616514365,25.2365122744931,-49.451591988131));
#17647=CARTESIAN_POINT('Ctrl Pts',(-20.7999620691484,25.2301426901958,-49.4520500243231));
#17648=CARTESIAN_POINT('Ctrl Pts',(-20.798233883955,25.2273100546687,-49.4522536878041));
#17649=CARTESIAN_POINT('Ctrl Pts',(-20.7945335911162,25.2212238534026,-49.4526912150723));
#17650=CARTESIAN_POINT('Ctrl Pts',(-20.7925628656177,25.2179694569693,-49.4529251291864));
#17651=CARTESIAN_POINT('Ctrl Pts',(-20.7872596075099,25.2091767139723,-49.4535570181752));
#17652=CARTESIAN_POINT('Ctrl Pts',(-20.7839379793887,25.2036318403731,-49.4539553914731));
#17653=CARTESIAN_POINT('Ctrl Pts',(-20.7692837035791,25.1790013247308,-49.4557245354168));
#17654=CARTESIAN_POINT('Ctrl Pts',(-20.7581319476875,25.1598092590007,-49.4571018780437));
#17655=CARTESIAN_POINT('Ctrl Pts',(-20.740927583315,25.1294838088069,-49.4592768128805));
#17656=CARTESIAN_POINT('Ctrl Pts',(-20.7347407287,25.1184270666214,-49.4600695080851));
#17657=CARTESIAN_POINT('Ctrl Pts',(-20.7259364637163,25.1024726011364,-49.4612129744289));
#17658=CARTESIAN_POINT('Ctrl Pts',(-20.7232662058473,25.0976040459501,-49.4615618583171));
#17659=CARTESIAN_POINT('Ctrl Pts',(-20.7172802257783,25.0866228758949,-49.4623486734307));
#17660=CARTESIAN_POINT('Ctrl Pts',(-20.7139716866925,25.080506395497,-49.4627868557418));
#17661=CARTESIAN_POINT('Ctrl Pts',(-20.709806592617,25.0727464935172,-49.4633426877643));
#17662=CARTESIAN_POINT('Ctrl Pts',(-20.708931604492,25.0711129412083,-49.463459692335));
#17663=CARTESIAN_POINT('Ctrl Pts',(-20.7047821567747,25.0633500825722,-49.4640156916099));
#17664=CARTESIAN_POINT('Ctrl Pts',(-20.7015261378426,25.0572109865896,-49.4644553268903));
#17665=CARTESIAN_POINT('Ctrl Pts',(-20.6960291968827,25.0467652400348,-49.4652032674357));
#17666=CARTESIAN_POINT('Ctrl Pts',(-20.6937780938749,25.0424639499864,-49.4655112202199));
#17667=CARTESIAN_POINT('Ctrl Pts',(-20.6896841454133,25.0345982364084,-49.4660743168653));
#17668=CARTESIAN_POINT('Ctrl Pts',(-20.687838218511,25.0310354202859,-49.4663293547703));
#17669=CARTESIAN_POINT('Ctrl Pts',(-20.6839786244681,25.0235518490328,-49.4668650128491));
#17670=CARTESIAN_POINT('Ctrl Pts',(-20.6819663384318,25.0196303942432,-49.4671456791547));
#17671=CARTESIAN_POINT('Ctrl Pts',(-20.6706729617978,24.9975107588224,-49.4687286986706));
#17672=CARTESIAN_POINT('Ctrl Pts',(-20.6615571851455,24.9792291026326,-49.4700365702729));
#17673=CARTESIAN_POINT('Ctrl Pts',(-20.5205315224112,24.6895379978154,-49.4907539376423));
#17674=CARTESIAN_POINT('Ctrl Pts',(-20.4272256431046,24.4010296392564,-49.5114947818016));
#17675=CARTESIAN_POINT('Ctrl Pts',(-20.360349998304,24.0175019709703,-49.5375402399015));
#17676=CARTESIAN_POINT('Ctrl Pts',(-20.3488211924274,23.9305683473128,-49.5433312635735));
#17677=CARTESIAN_POINT('Ctrl Pts',(-20.3385161720901,23.8176966828114,-49.5506207813762));
#17678=CARTESIAN_POINT('Ctrl Pts',(-20.3364872747463,23.7920991476344,-49.5522587060306));
#17679=CARTESIAN_POINT('Ctrl Pts',(-20.3341199585045,23.7568949923583,-49.554487959778));
#17680=CARTESIAN_POINT('Ctrl Pts',(-20.333518309329,23.7473078106942,-49.5550926754608));
#17681=CARTESIAN_POINT('Ctrl Pts',(-20.332688810562,23.7330719013884,-49.5559869380209));
#17682=CARTESIAN_POINT('Ctrl Pts',(-20.3324281570223,23.7284252453407,-49.5562782480867));
#17683=CARTESIAN_POINT('Ctrl Pts',(-20.3320287756304,23.7210186137934,-49.5567416447074));
#17684=CARTESIAN_POINT('Ctrl Pts',(-20.3318835317959,23.718259018232,-49.5569140905009));
#17685=CARTESIAN_POINT('Ctrl Pts',(-20.3316143492816,23.7130161490807,-49.5572413142629));
#17686=CARTESIAN_POINT('Ctrl Pts',(-20.331489734678,23.7105329143801,-49.5573961299677));
#17687=CARTESIAN_POINT('Ctrl Pts',(-20.3312769728162,23.7061928072554,-49.557666409968));
#17688=CARTESIAN_POINT('Ctrl Pts',(-20.3311875583144,23.70433600072,-49.5577819461307));
#17689=CARTESIAN_POINT('Ctrl Pts',(-20.3310157728409,23.7007032336661,-49.5580077982845));
#17690=CARTESIAN_POINT('Ctrl Pts',(-20.3309332650555,23.6989272866583,-49.5581181218911));
#17691=CARTESIAN_POINT('Ctrl Pts',(-20.3307396446026,23.694683943484,-49.5583815131137));
#17692=CARTESIAN_POINT('Ctrl Pts',(-20.330629898545,23.6922164815876,-49.5585345032649));
#17693=CARTESIAN_POINT('Ctrl Pts',(-20.3302474336868,23.6833887713138,-49.5590812505616));
#17694=CARTESIAN_POINT('Ctrl Pts',(-20.329990721671,23.6770277896843,-49.5594741104517));
#17695=CARTESIAN_POINT('Ctrl Pts',(-20.326499272205,23.5836477907786,-49.565225600634));
#17696=CARTESIAN_POINT('Ctrl Pts',(-20.3267735471633,23.4965240630276,-49.570391329925));
#17697=CARTESIAN_POINT('Ctrl Pts',(-20.3324562768539,23.36652413677,-49.5779407758143));
#17698=CARTESIAN_POINT('Ctrl Pts',(-20.3351960448085,23.323579019144,-49.5804087560653));
#17699=CARTESIAN_POINT('Ctrl Pts',(-20.3564168650059,23.0707531555806,-49.5948492969427));
#17700=CARTESIAN_POINT('Ctrl Pts',(-20.3945835070007,22.8630377654017,-49.6063854087763));
#17701=CARTESIAN_POINT('Ctrl Pts',(-20.4815895007542,22.5601335951613,-49.6242894523401));
#17702=CARTESIAN_POINT('Ctrl Pts',(-20.5152885023191,22.4612076004466,-49.6303124967231));
#17703=CARTESIAN_POINT('Ctrl Pts',(-20.5780311409963,22.302703984273,-49.6403883408207));
#17704=CARTESIAN_POINT('Ctrl Pts',(-20.6042130674933,22.2420752151218,-49.6443478812584));
#17705=CARTESIAN_POINT('Ctrl Pts',(-20.6358315936319,22.174629085286,-49.6488882532704));
#17706=CARTESIAN_POINT('Ctrl Pts',(-20.6394561971918,22.1669759984534,-49.6494054449437));
#17707=CARTESIAN_POINT('Ctrl Pts',(-20.6449385287891,22.1555174173792,-49.6501828435674));
#17708=CARTESIAN_POINT('Ctrl Pts',(-20.6467736835842,22.151701112229,-49.6504422645194));
#17709=CARTESIAN_POINT('Ctrl Pts',(-20.6499398124872,22.1451500643923,-49.6508884607435));
#17710=CARTESIAN_POINT('Ctrl Pts',(-20.6512671492896,22.1424135617437,-49.651075108912));
#17711=CARTESIAN_POINT('Ctrl Pts',(-20.6540059009508,22.1367875133794,-49.651459387439));
#17712=CARTESIAN_POINT('Ctrl Pts',(-20.6554177707774,22.1338981936299,-49.6516570335606));
#17713=CARTESIAN_POINT('Ctrl Pts',(-20.6588225695653,22.1269568042779,-49.6521325782717));
#17714=CARTESIAN_POINT('Ctrl Pts',(-20.6608196912004,22.1229068084962,-49.6524106234732));
#17715=CARTESIAN_POINT('Ctrl Pts',(-20.6669600030131,22.1105204672533,-49.6532627890281));
#17716=CARTESIAN_POINT('Ctrl Pts',(-20.6711307795822,22.1021979205268,-49.6538378767057));
#17717=CARTESIAN_POINT('Ctrl Pts',(-20.7192343972942,22.0072393134792,-49.6604284871116));
#17718=CARTESIAN_POINT('Ctrl Pts',(-20.7670222776059,21.922622495287,-49.6665801843234));
#17719=CARTESIAN_POINT('Ctrl Pts',(-20.8906306081776,21.7251546950487,-49.6816438569462));
#17720=CARTESIAN_POINT('Ctrl Pts',(-20.9699079564834,21.6146942467331,-49.6906677397866));
#17721=CARTESIAN_POINT('Ctrl Pts',(-21.1787037325698,21.3594808978904,-49.7128666434198));
#17722=CARTESIAN_POINT('Ctrl Pts',(-21.3147957074456,21.220776250317,-49.7261356604317));
#17723=CARTESIAN_POINT('Ctrl Pts',(-21.5196051820531,21.046614907131,-49.7438540995113));
#17724=CARTESIAN_POINT('Ctrl Pts',(-21.578357124272,21.000083796899,-49.748709720288));
#17725=CARTESIAN_POINT('Ctrl Pts',(-21.6448726637571,20.9510787720001,-49.7539157078703));
#17726=CARTESIAN_POINT('Ctrl Pts',(-21.6510789261483,20.9465405097836,-49.7543987423098));
#17727=CARTESIAN_POINT('Ctrl Pts',(-21.6605017494822,20.9397017889718,-49.7551279502848));
#17728=CARTESIAN_POINT('Ctrl Pts',(-21.6637063477573,20.9373850081739,-49.7553752190289));
#17729=CARTESIAN_POINT('Ctrl Pts',(-21.6689218576993,20.9336290256352,-49.7557764601246));
#17730=CARTESIAN_POINT('Ctrl Pts',(-21.6709301639283,20.9321862385135,-49.7559306775886));
#17731=CARTESIAN_POINT('Ctrl Pts',(-21.6747885974224,20.9294210290101,-49.756226413994));
#17732=CARTESIAN_POINT('Ctrl Pts',(-21.6766384664507,20.9280982515625,-49.7563679574608));
#17733=CARTESIAN_POINT('Ctrl Pts',(-21.6799806553775,20.9257137102094,-49.7566232456918));
#17734=CARTESIAN_POINT('Ctrl Pts',(-21.6814724770791,20.9246512625842,-49.7567370379822));
#17735=CARTESIAN_POINT('Ctrl Pts',(-21.6844808404255,20.9225126251233,-49.7569661888592));
#17736=CARTESIAN_POINT('Ctrl Pts',(-21.685997402147,20.9214364802132,-49.7570815443175));
#17737=CARTESIAN_POINT('Ctrl Pts',(-21.6902636479221,20.9184147211751,-49.7574055958832));
#17738=CARTESIAN_POINT('Ctrl Pts',(-21.6930154623841,20.9164720971741,-49.7576140845964));
#17739=CARTESIAN_POINT('Ctrl Pts',(-21.7043152333803,20.9085216190895,-49.7584680480524));
#17740=CARTESIAN_POINT('Ctrl Pts',(-21.7128894594236,20.9025509488741,-49.7591109872184));
#17741=CARTESIAN_POINT('Ctrl Pts',(-21.8607810069994,20.8006309130596,-49.7701170341141));
#17742=CARTESIAN_POINT('Ctrl Pts',(-22.0074337458379,20.7157400745456,-49.7797662405502));
#17743=CARTESIAN_POINT('Ctrl Pts',(-22.3525485525572,20.5507311621223,-49.801266138834));
#17744=CARTESIAN_POINT('Ctrl Pts',(-22.5536536195101,20.478052816462,-49.813007878494));
#17745=CARTESIAN_POINT('Ctrl Pts',(-22.8404728745875,20.4055520668102,-49.8300824343979));
#17746=CARTESIAN_POINT('Ctrl Pts',(-22.9212246442353,20.3884096405883,-49.8349186477814));
#17747=CARTESIAN_POINT('Ctrl Pts',(-23.0442790305731,20.3671876139351,-49.8423842776353));
#17748=CARTESIAN_POINT('Ctrl Pts',(-23.0861534703752,20.3608131992344,-49.8449411316729));
#17749=CARTESIAN_POINT('Ctrl Pts',(-23.1356628229357,20.3542721628591,-49.8479872100228));
#17750=CARTESIAN_POINT('Ctrl Pts',(-23.1431891727396,20.3533048366527,-49.848450893938));
#17751=CARTESIAN_POINT('Ctrl Pts',(-23.1547385284602,20.3518618979489,-49.8491634057405));
#17752=CARTESIAN_POINT('Ctrl Pts',(-23.1587591672811,20.3513672698933,-49.8494116317708));
#17753=CARTESIAN_POINT('Ctrl Pts',(-23.1660992764346,20.3504783188219,-49.849865130603));
#17754=CARTESIAN_POINT('Ctrl Pts',(-23.169418452664,20.3500815767288,-49.8500703266021));
#17755=CARTESIAN_POINT('Ctrl Pts',(-23.1760983761141,20.3492936631634,-49.8504835426966));
#17756=CARTESIAN_POINT('Ctrl Pts',(-23.1794591337816,20.3489026185968,-49.8506915665279));
#17757=CARTESIAN_POINT('Ctrl Pts',(-23.1890410559834,20.3478029946427,-49.8512850394249));
#17758=CARTESIAN_POINT('Ctrl Pts',(-23.1952636529138,20.3471072551569,-49.8516708936641));
#17759=CARTESIAN_POINT('Ctrl Pts',(-23.2218212977175,20.3442162216857,-49.8533196316222));
#17760=CARTESIAN_POINT('Ctrl Pts',(-23.2421746142569,20.3421964439256,-49.8545880422652));
#17761=CARTESIAN_POINT('Ctrl Pts',(-23.623560302085,20.3080122024984,-49.8784504722928));
#17762=CARTESIAN_POINT('Ctrl Pts',(-23.9873870202627,20.3368021084894,-49.9032415357527));
#17763=CARTESIAN_POINT('Ctrl Pts',(-24.4665956615241,20.4577054378386,-49.9363884148461));
#17764=CARTESIAN_POINT('Ctrl Pts',(-24.5924652140133,20.4978216552833,-49.9450929520787));
#17765=CARTESIAN_POINT('Ctrl Pts',(-24.7200889308477,20.5473165969402,-49.9536806207586));
#17766=CARTESIAN_POINT('Ctrl Pts',(-24.7246397445941,20.5490934049673,-49.9539865129444));
#17767=CARTESIAN_POINT('Ctrl Pts',(-24.731846715071,20.5519261788487,-49.9544704045179));
#17768=CARTESIAN_POINT('Ctrl Pts',(-24.7345055146659,20.5529753331637,-49.9546488054395));
#17769=CARTESIAN_POINT('Ctrl Pts',(-24.7395417216747,20.554970352711,-49.9549865003513));
#17770=CARTESIAN_POINT('Ctrl Pts',(-24.7419194030628,20.5559155137667,-49.9551458364193));
#17771=CARTESIAN_POINT('Ctrl Pts',(-24.7460330501115,20.5575564208503,-49.9554213363765));
#17772=CARTESIAN_POINT('Ctrl Pts',(-24.7477695380206,20.5582508472503,-49.9555375806456));
#17773=CARTESIAN_POINT('Ctrl Pts',(-24.7511395163107,20.5596019148371,-49.9557630718101));
#17774=CARTESIAN_POINT('Ctrl Pts',(-24.7527730702585,20.5602583818175,-49.9558723291145));
#17775=CARTESIAN_POINT('Ctrl Pts',(-24.7566356988388,20.561814311769,-49.9561305655069));
#17776=CARTESIAN_POINT('Ctrl Pts',(-24.7588643105157,20.5627149321883,-49.9562794739778));
#17777=CARTESIAN_POINT('Ctrl Pts',(-24.7654905943,20.5654013558052,-49.9567219716669));
#17778=CARTESIAN_POINT('Ctrl Pts',(-24.7698853558342,20.5671943918027,-49.9570151240182));
#17779=CARTESIAN_POINT('Ctrl Pts',(-24.8099544235803,20.5836456782026,-49.9596850907256));
#17780=CARTESIAN_POINT('Ctrl Pts',(-24.845368789658,20.5989343038941,-49.9620243426277));
#17781=CARTESIAN_POINT('Ctrl Pts',(-25.0133085586637,20.6750404726049,-49.9730578589526));
#17782=CARTESIAN_POINT('Ctrl Pts',(-25.1418932780101,20.7441758041256,-49.9813305777251));
#17783=CARTESIAN_POINT('Ctrl Pts',(-25.3440782575088,20.8712693727745,-49.99473253995));
#17784=CARTESIAN_POINT('Ctrl Pts',(-25.420613634216,20.9241316253425,-49.999906843828));
#17785=CARTESIAN_POINT('Ctrl Pts',(-25.5770310612405,21.0424785320367,-50.0108964125547));
#17786=CARTESIAN_POINT('Ctrl Pts',(-25.6562653236546,21.1086403413865,-50.0167139084268));
#17787=CARTESIAN_POINT('Ctrl Pts',(-25.8275432788986,21.266209454202,-50.0301014258739));
#17788=CARTESIAN_POINT('Ctrl Pts',(-25.9175114863494,21.3595940509773,-50.037729175639));
#17789=CARTESIAN_POINT('Ctrl Pts',(-26.0083381314482,21.4660164117986,-50.0462453674974));
#17790=CARTESIAN_POINT('Ctrl Pts',(-26.0150293952991,21.4739336669997,-50.0468778893076));
#17791=CARTESIAN_POINT('Ctrl Pts',(-26.0246346015815,21.4854106261046,-50.0477933672426));
#17792=CARTESIAN_POINT('Ctrl Pts',(-26.0275793504165,21.4889445596168,-50.0480750622075));
#17793=CARTESIAN_POINT('Ctrl Pts',(-26.0326927827819,21.4951078703413,-50.0485660156373));
#17794=CARTESIAN_POINT('Ctrl Pts',(-26.0348648853371,21.4977344120937,-50.048775134348));
#17795=CARTESIAN_POINT('Ctrl Pts',(-26.0390446612811,21.5028050226104,-50.0491786443299));
#17796=CARTESIAN_POINT('Ctrl Pts',(-26.0410529122718,21.5052486122011,-50.0493730118053));
#17797=CARTESIAN_POINT('Ctrl Pts',(-26.0457926434958,21.5110331379632,-50.0498329155719));
#17798=CARTESIAN_POINT('Ctrl Pts',(-26.0485210122141,21.5143766061185,-50.0500985775737));
#17799=CARTESIAN_POINT('Ctrl Pts',(-26.056609808026,21.5243297326302,-50.0508889457516));
#17800=CARTESIAN_POINT('Ctrl Pts',(-26.0619507473045,21.5309551152992,-50.0514144372414));
#17801=CARTESIAN_POINT('Ctrl Pts',(-26.1106123824566,21.5918111497292,-50.0562356908908));
#17802=CARTESIAN_POINT('Ctrl Pts',(-26.1521938400078,21.647403239183,-50.0606004305876));
#17803=CARTESIAN_POINT('Ctrl Pts',(-26.1977801256834,21.7126402357766,-50.0656841701246));
#17804=CARTESIAN_POINT('Ctrl Pts',(-26.20357473441,21.7210170094307,-50.0663362337197));
#17805=CARTESIAN_POINT('Ctrl Pts',(-26.3559778343107,21.9435810257917,-50.0836422213472));
#17806=CARTESIAN_POINT('Ctrl Pts',(-26.4761966022829,22.1746451062456,-50.1012653627369));
#17807=CARTESIAN_POINT('Ctrl Pts',(-26.5969500618658,22.4962962127341,-50.1244673141327));
#17808=CARTESIAN_POINT('Ctrl Pts',(-26.6234155195122,22.5761579045349,-50.1301168416261));
#17809=CARTESIAN_POINT('Ctrl Pts',(-26.6639125476698,22.7165363219465,-50.1397670341973));
#17810=CARTESIAN_POINT('Ctrl Pts',(-26.6793761391667,22.7765937253411,-50.1438086556587));
#17811=CARTESIAN_POINT('Ctrl Pts',(-26.6992497716561,22.86417190174,-50.1495422905182));
#17812=CARTESIAN_POINT('Ctrl Pts',(-26.7050505240801,22.891359518013,-50.1513001436345));
#17813=CARTESIAN_POINT('Ctrl Pts',(-26.7113653586342,22.9229545184331,-50.1533147485235));
#17814=CARTESIAN_POINT('Ctrl Pts',(-26.7122228002378,22.9272909570457,-50.1535906406513));
#17815=CARTESIAN_POINT('Ctrl Pts',(-26.7135120748713,22.9338825963787,-50.1540090658486));
#17816=CARTESIAN_POINT('Ctrl Pts',(-26.7139504199097,22.9361364947424,-50.1541519711122));
#17817=CARTESIAN_POINT('Ctrl Pts',(-26.7147404418734,22.9402219528891,-50.1544106969069));
#17818=CARTESIAN_POINT('Ctrl Pts',(-26.7150929365947,22.9420533436724,-50.1545265641887));
#17819=CARTESIAN_POINT('Ctrl Pts',(-26.7157986723795,22.9457372298634,-50.1547594088259));
#17820=CARTESIAN_POINT('Ctrl Pts',(-26.7161518757414,22.9475897218564,-50.1548763836876));
#17821=CARTESIAN_POINT('Ctrl Pts',(-26.7171556987238,22.952879839244,-50.1552101027301));
#17822=CARTESIAN_POINT('Ctrl Pts',(-26.717802349375,22.9563182290865,-50.155426618705));
#17823=CARTESIAN_POINT('Ctrl Pts',(-26.7205499963181,22.971060220494,-50.156353281195));
#17824=CARTESIAN_POINT('Ctrl Pts',(-26.72259612913,22.9823741496658,-50.1570603216025));
#17825=CARTESIAN_POINT('Ctrl Pts',(-26.7566303065972,23.1764896729262,-50.1691240477111));
#17826=CARTESIAN_POINT('Ctrl Pts',(-26.7728355587225,23.3617380754516,-50.1796271695459));
#17827=CARTESIAN_POINT('Ctrl Pts',(-26.7732738217376,23.8527672334791,-50.2071415556081));
#17828=CARTESIAN_POINT('Ctrl Pts',(-26.7301425946833,24.1566006082652,-50.2239916669425));
#17829=CARTESIAN_POINT('Ctrl Pts',(-26.6397864473579,24.4674409269653,-50.2435913330446));
#17830=CARTESIAN_POINT('Ctrl Pts',(-26.6345134267056,24.4850193893926,-50.2447073275911));
#17831=CARTESIAN_POINT('Ctrl Pts',(-26.6273184089501,24.5082812995509,-50.2461945707037));
#17832=CARTESIAN_POINT('Ctrl Pts',(-26.6255301975547,24.5140060323908,-50.2465614209946));
#17833=CARTESIAN_POINT('Ctrl Pts',(-26.6227242115075,24.522901712989,-50.2471327917352));
#17834=CARTESIAN_POINT('Ctrl Pts',(-26.6217174778103,24.5260761519119,-50.2473369484592));
#17835=CARTESIAN_POINT('Ctrl Pts',(-26.6196983835967,24.5324086920071,-50.2477447369298));
#17836=CARTESIAN_POINT('Ctrl Pts',(-26.6186860650631,24.5355668024578,-50.2479483670876));
#17837=CARTESIAN_POINT('Ctrl Pts',(-26.6164026788373,24.5426525921482,-50.2484058376068));
#17838=CARTESIAN_POINT('Ctrl Pts',(-26.6151289371629,24.5465793976186,-50.2486597659605));
#17839=CARTESIAN_POINT('Ctrl Pts',(-26.6113791913829,24.5580642155471,-50.2494036346368));
#17840=CARTESIAN_POINT('Ctrl Pts',(-26.6088827632978,24.5656154822051,-50.249894249397));
#17841=CARTESIAN_POINT('Ctrl Pts',(-26.5903056432636,24.6211178550001,-50.2535116176539));
#17842=CARTESIAN_POINT('Ctrl Pts',(-26.5731268917951,24.6686914415021,-50.2566746412048));
#17843=CARTESIAN_POINT('Ctrl Pts',(-26.5132237490912,24.823106432757,-50.2671553438891));
#17844=CARTESIAN_POINT('Ctrl Pts',(-26.4659009576916,24.9280568257782,-50.2746239359925));
#17845=CARTESIAN_POINT('Ctrl Pts',(-26.2723798936959,25.3023943562076,-50.3025135354043));
#17846=CARTESIAN_POINT('Ctrl Pts',(-26.0936161196279,25.5530659161506,-50.3238439952972));
#17847=CARTESIAN_POINT('Ctrl Pts',(-25.8807558965519,25.7762075686282,-50.3437362181018));
#17848=CARTESIAN_POINT('Ctrl Pts',(-25.8793403175193,25.7776886915042,-50.3438682918727));
#17849=CARTESIAN_POINT('Ctrl Pts',(-25.8501560844299,25.8081659678576,-50.3465867440912));
#17850=CARTESIAN_POINT('Ctrl Pts',(-25.8218477741054,25.8366437630058,-50.3491409006351));
#17851=CARTESIAN_POINT('Ctrl Pts',(-25.7891840009625,25.8682973693923,-50.3519882691086));
#17852=CARTESIAN_POINT('Ctrl Pts',(-25.7853456647844,25.8719985731562,-50.3523213396173));
#17853=CARTESIAN_POINT('Ctrl Pts',(-25.7797287683693,25.8773879565007,-50.3528064986618));
#17854=CARTESIAN_POINT('Ctrl Pts',(-25.7779574648793,25.8790836346399,-50.3529591703685));
#17855=CARTESIAN_POINT('Ctrl Pts',(-25.7748199802351,25.8820803101524,-50.3532290191686));
#17856=CARTESIAN_POINT('Ctrl Pts',(-25.7734545911583,25.8833821304019,-50.3533462608763));
#17857=CARTESIAN_POINT('Ctrl Pts',(-25.7706027724896,25.8860963995772,-50.3535907348077));
#17858=CARTESIAN_POINT('Ctrl Pts',(-25.7691161409313,25.8875086260464,-50.3537179496442));
#17859=CARTESIAN_POINT('Ctrl Pts',(-25.7652336482612,25.8911897593421,-50.3540495943589));
#17860=CARTESIAN_POINT('Ctrl Pts',(-25.7628356407964,25.8934564144334,-50.3542538484359));
#17861=CARTESIAN_POINT('Ctrl Pts',(-25.752432847631,25.9032591801555,-50.3551374144098));
#17862=CARTESIAN_POINT('Ctrl Pts',(-25.7443928857226,25.9107581018392,-50.3558138734789));
#17863=CARTESIAN_POINT('Ctrl Pts',(-25.6860587048758,25.9646111901403,-50.3606771931072));
#17864=CARTESIAN_POINT('Ctrl Pts',(-25.6343342714735,26.0093988512965,-50.3647508343422));
#17865=CARTESIAN_POINT('Ctrl Pts',(-25.5191354080867,26.1029004521583,-50.3734196444774));
#17866=CARTESIAN_POINT('Ctrl Pts',(-25.4551939900038,26.1509660253299,-50.377983831344));
#17867=CARTESIAN_POINT('Ctrl Pts',(-25.1092319277721,26.39141743402,-50.4017789993747));
#17868=CARTESIAN_POINT('Ctrl Pts',(-24.7998031977697,26.5404449754087,-50.4203103113212));
#17869=CARTESIAN_POINT('Ctrl Pts',(-24.4534209982649,26.6439253073304,-50.4421752659924));
#17870=CARTESIAN_POINT('Ctrl Pts',(-24.4340384490717,26.6495180810118,-50.4434011861833));
#17871=CARTESIAN_POINT('Ctrl Pts',(-24.40860558306,26.6565986786266,-50.4450133511992));
#17872=CARTESIAN_POINT('Ctrl Pts',(-24.4026013644391,26.6582515361678,-50.4453942118229));
#17873=CARTESIAN_POINT('Ctrl Pts',(-24.3933343153643,26.660773721166,-50.4459824526326));
#17874=CARTESIAN_POINT('Ctrl Pts',(-24.3900748231625,26.6616553475836,-50.4461894325555));
#17875=CARTESIAN_POINT('Ctrl Pts',(-24.3836499279953,26.6633823196646,-50.4465975746036));
#17876=CARTESIAN_POINT('Ctrl Pts',(-24.3804846090037,26.6642279642547,-50.4467987267362));
#17877=CARTESIAN_POINT('Ctrl Pts',(-24.3734989781126,26.666082832643,-50.4472428227357));
#17878=CARTESIAN_POINT('Ctrl Pts',(-24.3696780929086,26.6670898590595,-50.4474858375984));
#17879=CARTESIAN_POINT('Ctrl Pts',(-24.3617571884742,26.669161908222,-50.4479898535839));
#17880=CARTESIAN_POINT('Ctrl Pts',(-24.3576569040913,26.6702258787162,-50.4482508883521));
#17881=CARTESIAN_POINT('Ctrl Pts',(-24.347158771125,26.6729279269138,-50.4489195626694));
#17882=CARTESIAN_POINT('Ctrl Pts',(-24.3407579863139,26.6745544222816,-50.4493275769424));
#17883=CARTESIAN_POINT('Ctrl Pts',(-24.3222768308405,26.6791902165059,-50.4505065894271));
#17884=CARTESIAN_POINT('Ctrl Pts',(-24.3101840653041,26.682149179274,-50.4512792120296));
#17885=CARTESIAN_POINT('Ctrl Pts',(-24.1917834116107,26.7103943727069,-50.4588557694568));
#17886=CARTESIAN_POINT('Ctrl Pts',(-24.0842831083798,26.7303256531529,-50.4658312976475));
#17887=CARTESIAN_POINT('Ctrl Pts',(-23.6808163275798,26.7840961245158,-50.4923907813779));
#17888=CARTESIAN_POINT('Ctrl Pts',(-23.3816742706496,26.7823308358957,-50.512995451743));
#17889=CARTESIAN_POINT('Ctrl Pts',(-22.9976072689334,26.7265507694895,-50.5386695975442));
#17890=CARTESIAN_POINT('Ctrl Pts',(-22.9087351143983,26.7098009572123,-50.5445389936143));
#17891=CARTESIAN_POINT('Ctrl Pts',(-22.8144232653694,26.6878812639749,-50.5506090339629));
#17892=CARTESIAN_POINT('Ctrl Pts',(-22.8081748452796,26.6864093325922,-50.5510104332862));
#17893=CARTESIAN_POINT('Ctrl Pts',(-22.799519813761,26.6843431642154,-50.5515653426784));
#17894=CARTESIAN_POINT('Ctrl Pts',(-22.7971094811021,26.6837648185823,-50.5517197615124));
#17895=CARTESIAN_POINT('Ctrl Pts',(-22.7929692117749,26.6827663313488,-50.5519848046707));
#17896=CARTESIAN_POINT('Ctrl Pts',(-22.7912389564238,26.6823475373166,-50.5520955070968));
#17897=CARTESIAN_POINT('Ctrl Pts',(-22.7876669963338,26.6814798401352,-50.5523239143032));
#17898=CARTESIAN_POINT('Ctrl Pts',(-22.7858253441804,26.6810307465909,-50.5524416071977));
#17899=CARTESIAN_POINT('Ctrl Pts',(-22.7815048873509,26.6799731480659,-50.5527175471227));
#17900=CARTESIAN_POINT('Ctrl Pts',(-22.7790264008944,26.6793633211207,-50.5528757171403));
#17901=CARTESIAN_POINT('Ctrl Pts',(-22.7709896441648,26.6773757635143,-50.5533881975562));
#17902=CARTESIAN_POINT('Ctrl Pts',(-22.7654342805864,26.675986152589,-50.5537418216334));
#17903=CARTESIAN_POINT('Ctrl Pts',(-22.6155969661923,26.6380814055283,-50.5632634913327));
#17904=CARTESIAN_POINT('Ctrl Pts',(-22.4739902523969,26.5916240966747,-50.5718605016207));
#17905=CARTESIAN_POINT('Ctrl Pts',(-22.2472101780383,26.4993885800572,-50.5857134494194));
#17906=CARTESIAN_POINT('Ctrl Pts',(-22.160112839272,26.4593393289906,-50.5910556896339));
#17907=CARTESIAN_POINT('Ctrl Pts',(-22.0750357068432,26.4155366157209,-50.5964032705493));
#17908=CARTESIAN_POINT('',(-26.7730025135596,23.5499106452406,-50.4388495108445));
#17909=CARTESIAN_POINT('Ctrl Pts',(-22.0750360284016,26.415536781278,-50.8458393738826));
#17910=CARTESIAN_POINT('Ctrl Pts',(-22.0956768960379,26.4261639114079,-50.8444417962392));
#17911=CARTESIAN_POINT('Ctrl Pts',(-22.1164336446989,26.4365685430621,-50.8430364980611));
#17912=CARTESIAN_POINT('Ctrl Pts',(-22.1464834693602,26.4512272514963,-50.8410014702696));
#17913=CARTESIAN_POINT('Ctrl Pts',(-22.1556853635674,26.4556620235051,-50.8403782280499));
#17914=CARTESIAN_POINT('Ctrl Pts',(-22.1687212408711,26.4618683529765,-50.8394951535349));
#17915=CARTESIAN_POINT('Ctrl Pts',(-22.1725379286027,26.4636762685401,-50.839236585064));
#17916=CARTESIAN_POINT('Ctrl Pts',(-22.1791982204146,26.4668151481272,-50.8387853340284));
#17917=CARTESIAN_POINT('Ctrl Pts',(-22.1820402429718,26.4681494717756,-50.8385927682097));
#17918=CARTESIAN_POINT('Ctrl Pts',(-22.1879248129586,26.4709017775051,-50.8381940231165));
#17919=CARTESIAN_POINT('Ctrl Pts',(-22.1909676335063,26.4723191626449,-50.837987823499));
#17920=CARTESIAN_POINT('Ctrl Pts',(-22.1981517685009,26.475651975884,-50.8375009464129));
#17921=CARTESIAN_POINT('Ctrl Pts',(-22.2022949391999,26.4775633642484,-50.8372201297208));
#17922=CARTESIAN_POINT('Ctrl Pts',(-22.2110622710138,26.4815854787121,-50.8366258278653));
#17923=CARTESIAN_POINT('Ctrl Pts',(-22.2156873906137,26.4836940743727,-50.8363122700022));
#17924=CARTESIAN_POINT('Ctrl Pts',(-22.2507945630995,26.4995992479001,-50.8339318657707));
#17925=CARTESIAN_POINT('Ctrl Pts',(-22.2814838740098,26.5129308844117,-50.8318490961091));
#17926=CARTESIAN_POINT('Ctrl Pts',(-22.3702613471033,26.5498640446792,-50.8258162338943));
#17927=CARTESIAN_POINT('Ctrl Pts',(-22.4288353212862,26.5722503786448,-50.8218260035584));
#17928=CARTESIAN_POINT('Ctrl Pts',(-22.5620731542152,26.618765368079,-50.8127237181772));
#17929=CARTESIAN_POINT('Ctrl Pts',(-22.637038721028,26.6419039598359,-50.8075842972956));
#17930=CARTESIAN_POINT('Ctrl Pts',(-22.9971138315956,26.7388042961162,-50.7828496390657));
#17931=CARTESIAN_POINT('Ctrl Pts',(-23.290578276944,26.7759897482668,-50.7623901779033));
#17932=CARTESIAN_POINT('Ctrl Pts',(-23.5882462737214,26.7727802015371,-50.7431377838111));
#17933=CARTESIAN_POINT('Ctrl Pts',(-23.591493324781,26.772740282562,-50.7429279716931));
#17934=CARTESIAN_POINT('Ctrl Pts',(-23.5960766206183,26.7726770073656,-50.7426321020325));
#17935=CARTESIAN_POINT('Ctrl Pts',(-23.5974129088404,26.7726577277195,-50.7425458736657));
#17936=CARTESIAN_POINT('Ctrl Pts',(-23.6013447125728,26.7725985543666,-50.7422922627132));
#17937=CARTESIAN_POINT('Ctrl Pts',(-23.6039401986983,26.7725563558673,-50.7421249777092));
#17938=CARTESIAN_POINT('Ctrl Pts',(-23.6459391657969,26.7718227609664,-50.7394201848066));
#17939=CARTESIAN_POINT('Ctrl Pts',(-23.6853290275148,26.7704117460691,-50.7369138269154));
#17940=CARTESIAN_POINT('Ctrl Pts',(-23.7294541178396,26.7680199507212,-50.7341476208134));
#17941=CARTESIAN_POINT('Ctrl Pts',(-23.7342224425952,26.7677508524412,-50.7338492377378));
#17942=CARTESIAN_POINT('Ctrl Pts',(-23.7413973147941,26.7673299396213,-50.7334010985473));
#17943=CARTESIAN_POINT('Ctrl Pts',(-23.7438042921338,26.7671860238301,-50.7332509015141));
#17944=CARTESIAN_POINT('Ctrl Pts',(-23.7479703925729,26.7669322354467,-50.7329911818766));
#17945=CARTESIAN_POINT('Ctrl Pts',(-23.7497295867082,26.7668236211622,-50.7328815881482));
#17946=CARTESIAN_POINT('Ctrl Pts',(-23.7533924879916,26.7665944537024,-50.7326535584582));
#17947=CARTESIAN_POINT('Ctrl Pts',(-23.7552961751057,26.7664736536673,-50.7325351371265));
#17948=CARTESIAN_POINT('Ctrl Pts',(-23.7598155160419,26.7661828463333,-50.7322542183688));
#17949=CARTESIAN_POINT('Ctrl Pts',(-23.7624310794692,26.7660113374825,-50.732091806101));
#17950=CARTESIAN_POINT('Ctrl Pts',(-23.7711431118365,26.7654293929783,-50.7315513911076));
#17951=CARTESIAN_POINT('Ctrl Pts',(-23.7772386704085,26.7650048070667,-50.7311741834696));
#17952=CARTESIAN_POINT('Ctrl Pts',(-23.9311374103601,26.7538450890673,-50.7216725978437));
#17953=CARTESIAN_POINT('Ctrl Pts',(-24.0780497708452,26.7329434927783,-50.713112765683));
#17954=CARTESIAN_POINT('Ctrl Pts',(-24.2969529822255,26.6862166691887,-50.7004469260784));
#17955=CARTESIAN_POINT('Ctrl Pts',(-24.370308865288,26.6678382513418,-50.6962185083487));
#17956=CARTESIAN_POINT('Ctrl Pts',(-24.5361296049185,26.6200355178534,-50.6865743014601));
#17957=CARTESIAN_POINT('Ctrl Pts',(-24.6280462335212,26.5889827557182,-50.6811649761854));
#17958=CARTESIAN_POINT('Ctrl Pts',(-24.8918154783562,26.4863962337935,-50.6651745219889));
#17959=CARTESIAN_POINT('Ctrl Pts',(-25.0590178775955,26.4040819624656,-50.6544159768157));
#17960=CARTESIAN_POINT('Ctrl Pts',(-25.2280973206403,26.3018137124546,-50.6424003194625));
#17961=CARTESIAN_POINT('Ctrl Pts',(-25.2379883096228,26.2957579506732,-50.6416931616399));
#17962=CARTESIAN_POINT('Ctrl Pts',(-25.2516369872835,26.2872999160644,-50.6407113615871));
#17963=CARTESIAN_POINT('Ctrl Pts',(-25.2554227838812,26.2849429823193,-50.6404383938511));
#17964=CARTESIAN_POINT('Ctrl Pts',(-25.2619174534283,26.2808808483826,-50.6399689997531));
#17965=CARTESIAN_POINT('Ctrl Pts',(-25.2646287079938,26.2791794516062,-50.6397727144357));
#17966=CARTESIAN_POINT('Ctrl Pts',(-25.2701458810268,26.2757057863946,-50.6393726098349));
#17967=CARTESIAN_POINT('Ctrl Pts',(-25.2729516046243,26.2739332179408,-50.6391687795936));
#17968=CARTESIAN_POINT('Ctrl Pts',(-25.2794166703331,26.2698348055958,-50.6386982726403));
#17969=CARTESIAN_POINT('Ctrl Pts',(-25.2830740604103,26.2675059082123,-50.638431482486));
#17970=CARTESIAN_POINT('Ctrl Pts',(-25.2907438706796,26.2626002602529,-50.637870702135));
#17971=CARTESIAN_POINT('Ctrl Pts',(-25.2947552910684,26.2600219727802,-50.6375766549293));
#17972=CARTESIAN_POINT('Ctrl Pts',(-25.3053742358064,26.2531634340918,-50.6367962574583));
#17973=CARTESIAN_POINT('Ctrl Pts',(-25.3119717930802,26.2488678775412,-50.636309334412));
#17974=CARTESIAN_POINT('Ctrl Pts',(-25.4471803020444,26.1601287914516,-50.6262877503444));
#17975=CARTESIAN_POINT('Ctrl Pts',(-25.5695766385052,26.0666202562459,-50.616404789033));
#17976=CARTESIAN_POINT('Ctrl Pts',(-25.9416694005638,25.7376667219318,-50.5836004305717));
#17977=CARTESIAN_POINT('Ctrl Pts',(-26.1606189150832,25.4710904597472,-50.5595541428315));
#17978=CARTESIAN_POINT('Ctrl Pts',(-26.3345797123176,25.1731033444322,-50.537745502929));
#17979=CARTESIAN_POINT('Ctrl Pts',(-26.335710276104,25.1711620798558,-50.5376036350083));
#17980=CARTESIAN_POINT('Ctrl Pts',(-26.3432850657636,25.158124257781,-50.5366522222086));
#17981=CARTESIAN_POINT('Ctrl Pts',(-26.3496651229148,25.1469902625698,-50.535846506356));
#17982=CARTESIAN_POINT('Ctrl Pts',(-26.3577749224714,25.1326396265604,-50.5348169772922));
#17983=CARTESIAN_POINT('Ctrl Pts',(-26.3595658191417,25.1294579477183,-50.5345892832113));
#17984=CARTESIAN_POINT('Ctrl Pts',(-26.3622885884199,25.1246014293397,-50.5342425962013));
#17985=CARTESIAN_POINT('Ctrl Pts',(-26.3632243725285,25.1229288043453,-50.5341233505836));
#17986=CARTESIAN_POINT('Ctrl Pts',(-26.3649761414641,25.1197911184493,-50.5338999513798));
#17987=CARTESIAN_POINT('Ctrl Pts',(-26.3657924719637,25.1183262606664,-50.5337957756199));
#17988=CARTESIAN_POINT('Ctrl Pts',(-26.3676634252024,25.1149627721575,-50.5335568513913));
#17989=CARTESIAN_POINT('Ctrl Pts',(-26.3687172703442,25.1130637155943,-50.5334221537534));
#17990=CARTESIAN_POINT('Ctrl Pts',(-26.3716307350508,25.1078010439874,-50.5330494320366));
#17991=CARTESIAN_POINT('Ctrl Pts',(-26.3734862661872,25.1044351513719,-50.5328116718754));
#17992=CARTESIAN_POINT('Ctrl Pts',(-26.3835712364906,25.0860635788879,-50.5315172979406));
#17993=CARTESIAN_POINT('Ctrl Pts',(-26.3916872706754,25.0709954784822,-50.5304678709575));
#17994=CARTESIAN_POINT('Ctrl Pts',(-26.4833367007158,24.8975451180664,-50.5185187838262));
#17995=CARTESIAN_POINT('Ctrl Pts',(-26.5536634684481,24.7325054650257,-50.5083857883047));
#17996=CARTESIAN_POINT('Ctrl Pts',(-26.6733032548985,24.3708607447798,-50.4870404757371));
#17997=CARTESIAN_POINT('Ctrl Pts',(-26.7185475392238,24.1737473751388,-50.4758838170986));
#17998=CARTESIAN_POINT('Ctrl Pts',(-26.7593915971981,23.8655895963788,-50.4579020537943));
#17999=CARTESIAN_POINT('Ctrl Pts',(-26.768222768076,23.7568309416626,-50.4514617962942));
#18000=CARTESIAN_POINT('Ctrl Pts',(-26.771950602867,23.6337809247315,-50.4439882212096));
#18001=CARTESIAN_POINT('Ctrl Pts',(-26.7722845086353,23.6197175156082,-50.4431313724413));
#18002=CARTESIAN_POINT('Ctrl Pts',(-26.7726187430012,23.6002771832538,-50.4419430587074));
#18003=CARTESIAN_POINT('Ctrl Pts',(-26.7726977094018,23.5949016263272,-50.4416140633374));
#18004=CARTESIAN_POINT('Ctrl Pts',(-26.7728023016572,23.5863194883079,-50.4410881588143));
#18005=CARTESIAN_POINT('Ctrl Pts',(-26.77283659333,23.5831130067104,-50.4408915219491));
#18006=CARTESIAN_POINT('Ctrl Pts',(-26.7728958080148,23.5766779111493,-50.4404965938168));
#18007=CARTESIAN_POINT('Ctrl Pts',(-26.7729206649192,23.5734493002506,-50.4402983006936));
#18008=CARTESIAN_POINT('Ctrl Pts',(-26.7729609906621,23.5669410663189,-50.439898276714));
#18009=CARTESIAN_POINT('Ctrl Pts',(-26.7729763050827,23.5636614466582,-50.4396965412549));
#18010=CARTESIAN_POINT('Ctrl Pts',(-26.772997583751,23.5568914254722,-50.4392797806001));
#18011=CARTESIAN_POINT('Ctrl Pts',(-26.7730028838382,23.5534010296548,-50.4390647349235));
#18012=CARTESIAN_POINT('Ctrl Pts',(-26.7730025135596,23.5499106452406,-50.4388495108445));
#18013=CARTESIAN_POINT('Ctrl Pts',(-26.7730025136018,23.5499110428036,-50.4388495353591));
#18014=CARTESIAN_POINT('Ctrl Pts',(-26.7730020002086,23.5450659720061,-50.438550778629));
#18015=CARTESIAN_POINT('Ctrl Pts',(-26.7729905607256,23.540220929427,-50.4382516785179));
#18016=CARTESIAN_POINT('Ctrl Pts',(-26.7728798798832,23.5162441225703,-50.4367697892271));
#18017=CARTESIAN_POINT('Ctrl Pts',(-26.7726212019504,23.4971138010535,-50.4355820031528));
#18018=CARTESIAN_POINT('Ctrl Pts',(-26.7679256386955,23.2877626462575,-50.422522228925));
#18019=CARTESIAN_POINT('Ctrl Pts',(-26.7468224487095,23.0983244634533,-50.4101158335791));
#18020=CARTESIAN_POINT('Ctrl Pts',(-26.650632902803,22.6223437056152,-50.3775986227797));
#18021=CARTESIAN_POINT('Ctrl Pts',(-26.5525937045061,22.3422243301948,-50.3570929796435));
#18022=CARTESIAN_POINT('Ctrl Pts',(-26.4120233109153,22.068178321527,-50.3376681968354));
#18023=CARTESIAN_POINT('Ctrl Pts',(-26.4062135782473,22.0570136123423,-50.3368782619577));
#18024=CARTESIAN_POINT('Ctrl Pts',(-26.398720963306,22.0428185650594,-50.3358760358632));
#18025=CARTESIAN_POINT('Ctrl Pts',(-26.3970984993017,22.0397567168573,-50.3356599833889));
#18026=CARTESIAN_POINT('Ctrl Pts',(-26.3944906508888,22.0348544183463,-50.3353142731019));
#18027=CARTESIAN_POINT('Ctrl Pts',(-26.3935084167594,22.0330123092114,-50.3351844149724));
#18028=CARTESIAN_POINT('Ctrl Pts',(-26.3916398712976,22.0295161738203,-50.3349380495827));
#18029=CARTESIAN_POINT('Ctrl Pts',(-26.3907539118305,22.0278619795431,-50.3348215214092));
#18030=CARTESIAN_POINT('Ctrl Pts',(-26.3887220668953,22.0240762257711,-50.3345549265203));
#18031=CARTESIAN_POINT('Ctrl Pts',(-26.3875752265068,22.0219451854384,-50.334404921986));
#18032=CARTESIAN_POINT('Ctrl Pts',(-26.3840379300535,22.0153899429654,-50.3339436890125));
#18033=CARTESIAN_POINT('Ctrl Pts',(-26.3816395038037,22.0109700153203,-50.333632968857));
#18034=CARTESIAN_POINT('Ctrl Pts',(-26.3635086965006,21.9777435055112,-50.3312990484874));
#18035=CARTESIAN_POINT('Ctrl Pts',(-26.3473466800712,21.9491718295774,-50.3293028488182));
#18036=CARTESIAN_POINT('Ctrl Pts',(-26.3264923106088,21.9135848269859,-50.3268237435692));
#18037=CARTESIAN_POINT('Ctrl Pts',(-26.3222058991371,21.9063355576893,-50.3263191182778));
#18038=CARTESIAN_POINT('Ctrl Pts',(-26.1901947753866,21.6850599623424,-50.3109251116409));
#18039=CARTESIAN_POINT('Ctrl Pts',(-26.0380820088197,21.486523530566,-50.2973245438593));
#18040=CARTESIAN_POINT('Ctrl Pts',(-25.7133344992387,21.1514133043372,-50.2711313247174));
#18041=CARTESIAN_POINT('Ctrl Pts',(-25.5467122623584,21.0110636318964,-50.2586960517792));
#18042=CARTESIAN_POINT('Ctrl Pts',(-25.3569658949198,20.8815338321716,-50.2447317633018));
#18043=CARTESIAN_POINT('Ctrl Pts',(-25.3466392148444,20.8745717675132,-50.2439725241306));
#18044=CARTESIAN_POINT('Ctrl Pts',(-25.3331143765499,20.8655671497709,-50.2429790297503));
#18045=CARTESIAN_POINT('Ctrl Pts',(-25.3299525016519,20.8634700740895,-50.2427468302474));
#18046=CARTESIAN_POINT('Ctrl Pts',(-25.3237524759972,20.859373727748,-50.2422916357075));
#18047=CARTESIAN_POINT('Ctrl Pts',(-25.3207146287371,20.8573740062624,-50.2420686580513));
#18048=CARTESIAN_POINT('Ctrl Pts',(-25.3176684801766,20.8553762028834,-50.2418451250709));
#18049=CARTESIAN_POINT('Ctrl Pts',(-25.3176635475717,20.8553729678751,-50.2418447631059));
#18050=CARTESIAN_POINT('Ctrl Pts',(-25.3176536763093,20.8553664939278,-50.2418440387318));
#18051=CARTESIAN_POINT('Ctrl Pts',(-25.317648736119,20.8553632539835,-50.2418436762104));
#18052=CARTESIAN_POINT('Ctrl Pts',(-25.3176388439939,20.8553567664315,-50.2418429503059));
#18053=CARTESIAN_POINT('Ctrl Pts',(-25.3176338935312,20.8553535197893,-50.241842587031));
#18054=CARTESIAN_POINT('Ctrl Pts',(-25.3176239887374,20.8553470240067,-50.2418418601974));
#18055=CARTESIAN_POINT('Ctrl Pts',(-25.3176190310386,20.8553437726579,-50.2418414963918));
#18056=CARTESIAN_POINT('Ctrl Pts',(-25.3176091048279,20.8553372629081,-50.2418407679872));
#18057=CARTESIAN_POINT('Ctrl Pts',(-25.317604137428,20.8553340052364,-50.2418404034699));
#18058=CARTESIAN_POINT('Ctrl Pts',(-25.3175941967233,20.8553274860598,-50.2418396740023));
#18059=CARTESIAN_POINT('Ctrl Pts',(-25.3175892218346,20.8553242235162,-50.2418393089358));
#18060=CARTESIAN_POINT('Ctrl Pts',(-25.3175792602737,20.8553176907409,-50.2418385779383));
#18061=CARTESIAN_POINT('Ctrl Pts',(-25.3175742761751,20.855314422197,-50.2418382121963));
#18062=CARTESIAN_POINT('Ctrl Pts',(-25.3175642957918,20.8553078771571,-50.2418374798182));
#18063=CARTESIAN_POINT('Ctrl Pts',(-25.3175593012948,20.8553046018337,-50.2418371133133));
#18064=CARTESIAN_POINT('Ctrl Pts',(-25.3175493070174,20.8552980477617,-50.2418363799162));
#18065=CARTESIAN_POINT('Ctrl Pts',(-25.3175443048984,20.8552947674796,-50.2418360128523));
#18066=CARTESIAN_POINT('Ctrl Pts',(-25.3175342884258,20.8552881989321,-50.2418352778271));
#18067=CARTESIAN_POINT('Ctrl Pts',(-25.3175292761578,20.8552849120346,-50.2418349100187));
#18068=CARTESIAN_POINT('Ctrl Pts',(-25.3175192435097,20.8552783329597,-50.2418341738071));
#18069=CARTESIAN_POINT('Ctrl Pts',(-25.3175142222856,20.855275040229,-50.2418338053418));
#18070=CARTESIAN_POINT('Ctrl Pts',(-25.3175041704501,20.855268448652,-50.2418330677228));
#18071=CARTESIAN_POINT('Ctrl Pts',(-25.317499139872,20.8552651498276,-50.2418326985714));
#18072=CARTESIAN_POINT('Ctrl Pts',(-25.3174890689219,20.8552585457967,-50.2418319595503));
#18073=CARTESIAN_POINT('Ctrl Pts',(-25.3174840284966,20.8552552405553,-50.2418315896766));
#18074=CARTESIAN_POINT('Ctrl Pts',(-25.3174739400269,20.8552486251169,-50.2418308493705));
#18075=CARTESIAN_POINT('Ctrl Pts',(-25.3174688905957,20.8552453140105,-50.2418304788362));
#18076=CARTESIAN_POINT('Ctrl Pts',(-25.3174587822177,20.8552386855986,-50.2418297370698));
#18077=CARTESIAN_POINT('Ctrl Pts',(-25.3174537233094,20.8552353683184,-50.2418293658404));
#18078=CARTESIAN_POINT('Ctrl Pts',(-25.3174435949174,20.8552287268641,-50.2418286226059));
#18079=CARTESIAN_POINT('Ctrl Pts',(-25.3174385257194,20.8552254028775,-50.2418282506217));
#18080=CARTESIAN_POINT('Ctrl Pts',(-25.3174283800736,20.8552187501914,-50.2418275061217));
#18081=CARTESIAN_POINT('Ctrl Pts',(-25.3174233019599,20.8552154203995,-50.2418271334836));
#18082=CARTESIAN_POINT('Ctrl Pts',(-25.3174131352233,20.855208753966,-50.2418263874365));
#18083=CARTESIAN_POINT('Ctrl Pts',(-25.3174080473457,20.855205417813,-50.2418260140822));
#18084=CARTESIAN_POINT('Ctrl Pts',(-25.317397859896,20.8551987378801,-50.2418252665157));
#18085=CARTESIAN_POINT('Ctrl Pts',(-25.3173927611784,20.8551953946606,-50.2418248923663));
#18086=CARTESIAN_POINT('Ctrl Pts',(-25.3173825573834,20.8551887040929,-50.241824143601));
#18087=CARTESIAN_POINT('Ctrl Pts',(-25.3173774502884,20.8551853554218,-50.2418237688371));
#18088=CARTESIAN_POINT('Ctrl Pts',(-25.3173672216869,20.8551786486718,-50.2418230182522));
#18089=CARTESIAN_POINT('Ctrl Pts',(-25.3173621029243,20.8551752923921,-50.2418226426324));
#18090=CARTESIAN_POINT('Ctrl Pts',(-25.317351858965,20.8551685756556,-50.241821890921));
#18091=CARTESIAN_POINT('Ctrl Pts',(-25.317346731654,20.8551652138127,-50.2418215146743));
#18092=CARTESIAN_POINT('Ctrl Pts',(-25.3173364624011,20.8551584805755,-50.2418207611075));
#18093=CARTESIAN_POINT('Ctrl Pts',(-25.3173313230958,20.8551551109102,-50.2418203839809));
#18094=CARTESIAN_POINT('Ctrl Pts',(-25.3173210376342,20.8551483671297,-50.2418196292253));
#18095=CARTESIAN_POINT('Ctrl Pts',(-25.3173158887848,20.8551449912488,-50.2418192513987));
#18096=CARTESIAN_POINT('Ctrl Pts',(-25.3173055818222,20.8551382334554,-50.2418184950659));
#18097=CARTESIAN_POINT('Ctrl Pts',(-25.3173004232899,20.8551348512681,-50.2418181165291));
#18098=CARTESIAN_POINT('Ctrl Pts',(-25.3172900935528,20.8551280786274,-50.2418173585257));
#18099=CARTESIAN_POINT('Ctrl Pts',(-25.3172849240483,20.8551246892886,-50.241816979184));
#18100=CARTESIAN_POINT('Ctrl Pts',(-25.3172745746714,20.8551179038563,-50.2418162197401));
#18101=CARTESIAN_POINT('Ctrl Pts',(-25.3172693950126,20.8551145079027,-50.2418158396536));
#18102=CARTESIAN_POINT('Ctrl Pts',(-25.3172590230613,20.8551077077552,-50.2418150785538));
#18103=CARTESIAN_POINT('Ctrl Pts',(-25.3172538322125,20.855104304508,-50.2418146976465));
#18104=CARTESIAN_POINT('Ctrl Pts',(-25.3172434404056,20.8550974914284,-50.2418139350903));
#18105=CARTESIAN_POINT('Ctrl Pts',(-25.3172382392833,20.8550940814886,-50.2418135534294));
#18106=CARTESIAN_POINT('Ctrl Pts',(-25.3172278240575,20.8550872531414,-50.2418127891554));
#18107=CARTESIAN_POINT('Ctrl Pts',(-25.317222611199,20.8550838355504,-50.2418124066336));
#18108=CARTESIAN_POINT('Ctrl Pts',(-25.3172121760735,20.8550769942432,-50.2418116408999));
#18109=CARTESIAN_POINT('Ctrl Pts',(-25.3172069523462,20.8550735695699,-50.2418112575809));
#18110=CARTESIAN_POINT('Ctrl Pts',(-25.3171964960468,20.855066714468,-50.2418104902941));
#18111=CARTESIAN_POINT('Ctrl Pts',(-25.3171912621843,20.8550632831936,-50.2418101062317));
#18112=CARTESIAN_POINT('Ctrl Pts',(-25.3171807803602,20.8550564114452,-50.2418093370725));
#18113=CARTESIAN_POINT('Ctrl Pts',(-25.317175533757,20.8550529718618,-50.2418089520755));
#18114=CARTESIAN_POINT('Ctrl Pts',(-25.3171650344398,20.8550460887328,-50.2418081816333));
#18115=CARTESIAN_POINT('Ctrl Pts',(-25.3171597781994,20.8550426428753,-50.2418077959294));
#18116=CARTESIAN_POINT('Ctrl Pts',(-25.3171492537723,20.8550357433728,-50.2418070236453));
#18117=CARTESIAN_POINT('Ctrl Pts',(-25.3171439867632,20.8550322904998,-50.2418066371516));
#18118=CARTESIAN_POINT('Ctrl Pts',(-25.3171334365432,20.8550253741767,-50.2418058629754));
#18119=CARTESIAN_POINT('Ctrl Pts',(-25.3171281561072,20.8550219125458,-50.2418054754967));
#18120=CARTESIAN_POINT('Ctrl Pts',(-25.3171175889064,20.8550149851795,-50.2418047000752));
#18121=CARTESIAN_POINT('Ctrl Pts',(-25.3171122988296,20.855011517273,-50.2418043118893));
#18122=CARTESIAN_POINT('Ctrl Pts',(-25.317101704821,20.8550045724219,-50.2418035345013));
#18123=CARTESIAN_POINT('Ctrl Pts',(-25.317096403136,20.8550010969503,-50.241803145464));
#18124=CARTESIAN_POINT('Ctrl Pts',(-25.3170857835668,20.8549941354328,-50.241802366201));
#18125=CARTESIAN_POINT('Ctrl Pts',(-25.3170804678823,20.8549906508289,-50.2418019761367));
#18126=CARTESIAN_POINT('Ctrl Pts',(-25.3170673903863,20.8549820781606,-50.241801016512));
#18127=CARTESIAN_POINT('Ctrl Pts',(-25.3170596238428,20.8549769870198,-50.2418004466046));
#18128=CARTESIAN_POINT('Ctrl Pts',(-25.3170440162035,20.854966755964,-50.2417993013198));
#18129=CARTESIAN_POINT('Ctrl Pts',(-25.3170361764729,20.8549616169449,-50.2417987260427));
#18130=CARTESIAN_POINT('Ctrl Pts',(-25.3170204225301,20.8549512901813,-50.2417975700236));
#18131=CARTESIAN_POINT('Ctrl Pts',(-25.3170125083478,20.8549461024575,-50.2417969892839));
#18132=CARTESIAN_POINT('Ctrl Pts',(-25.3169966059355,20.854935678572,-50.2417958223717));
#18133=CARTESIAN_POINT('Ctrl Pts',(-25.3169886165374,20.8549304416456,-50.2417952361134));
#18134=CARTESIAN_POINT('Ctrl Pts',(-25.3169725626485,20.8549199186726,-50.2417940580874));
#18135=CARTESIAN_POINT('Ctrl Pts',(-25.3169644975312,20.8549146322164,-50.2417934662736));
#18136=CARTESIAN_POINT('Ctrl Pts',(-25.3169482859129,20.8549040060633,-50.241792276675));
#18137=CARTESIAN_POINT('Ctrl Pts',(-25.316940141956,20.8548986680351,-50.2417916790769));
#18138=CARTESIAN_POINT('Ctrl Pts',(-25.3169237726923,20.8548879387631,-50.2417904779119));
#18139=CARTESIAN_POINT('Ctrl Pts',(-25.3169155479906,20.854882547917,-50.2417898743894));
#18140=CARTESIAN_POINT('Ctrl Pts',(-25.3168990215729,20.8548717158543,-50.2417886616942));
#18141=CARTESIAN_POINT('Ctrl Pts',(-25.316890717171,20.8548662728782,-50.2417880523242));
#18142=CARTESIAN_POINT('Ctrl Pts',(-25.3168740235799,20.8548553314641,-50.2417868273635));
#18143=CARTESIAN_POINT('Ctrl Pts',(-25.3168656360262,20.8548498340991,-50.2417862118928));
#18144=CARTESIAN_POINT('Ctrl Pts',(-25.3168487761526,20.8548387839241,-50.2417849747321));
#18145=CARTESIAN_POINT('Ctrl Pts',(-25.3168403040439,20.8548332312537,-50.2417843530576));
#18146=CARTESIAN_POINT('Ctrl Pts',(-25.3168232747434,20.8548220702637,-50.2417831034662));
#18147=CARTESIAN_POINT('Ctrl Pts',(-25.316814716858,20.8548164614907,-50.2417824754983));
#18148=CARTESIAN_POINT('Ctrl Pts',(-25.3167975138016,20.8548051868555,-50.2417812131586));
#18149=CARTESIAN_POINT('Ctrl Pts',(-25.3167888682306,20.8547995207323,-50.2417805787573));
#18150=CARTESIAN_POINT('Ctrl Pts',(-25.3167714892016,20.8547881310063,-50.2417793035067));
#18151=CARTESIAN_POINT('Ctrl Pts',(-25.3167627549109,20.8547824068589,-50.2417786625962));
#18152=CARTESIAN_POINT('Ctrl Pts',(-25.3167451948876,20.8547708987582,-50.2417773740662));
#18153=CARTESIAN_POINT('Ctrl Pts',(-25.3167363699281,20.8547651153129,-50.2417767265034));
#18154=CARTESIAN_POINT('Ctrl Pts',(-25.3167186243574,20.8547534858615,-50.2417754243601));
#18155=CARTESIAN_POINT('Ctrl Pts',(-25.3167097055671,20.85474764105,-50.241774769913));
#18156=CARTESIAN_POINT('Ctrl Pts',(-25.3166917750511,20.8547358906503,-50.2417734542005));
#18157=CARTESIAN_POINT('Ctrl Pts',(-25.3166827621516,20.8547299842941,-50.2417727928488));
#18158=CARTESIAN_POINT('Ctrl Pts',(-25.3166646385515,20.8547181076204,-50.24177146297));
#18159=CARTESIAN_POINT('Ctrl Pts',(-25.3166555284443,20.8547121376933,-50.2417707944863));
#18160=CARTESIAN_POINT('Ctrl Pts',(-25.3166372117029,20.8547001347166,-50.241769450437));
#18161=CARTESIAN_POINT('Ctrl Pts',(-25.3166280039023,20.8546941009042,-50.2417687747858));
#18162=CARTESIAN_POINT('Ctrl Pts',(-25.3166094849838,20.8546819657121,-50.2417674159031));
#18163=CARTESIAN_POINT('Ctrl Pts',(-25.3166001754163,20.8546758653497,-50.2417667327854));
#18164=CARTESIAN_POINT('Ctrl Pts',(-25.3165814563936,20.8546635993091,-50.2417653592214));
#18165=CARTESIAN_POINT('Ctrl Pts',(-25.3165720451032,20.85465743243,-50.2417646686406));
#18166=CARTESIAN_POINT('Ctrl Pts',(-25.3165531156774,20.8546450288018,-50.2417632796397));
#18167=CARTESIAN_POINT('Ctrl Pts',(-25.3165435987515,20.8546387928468,-50.2417625813085));
#18168=CARTESIAN_POINT('Ctrl Pts',(-25.3165244594839,20.8546262520081,-50.2417611769121));
#18169=CARTESIAN_POINT('Ctrl Pts',(-25.3165148361539,20.8546199464784,-50.2417604707743));
#18170=CARTESIAN_POINT('Ctrl Pts',(-25.3164954783713,20.854607262756,-50.2417590503458));
#18171=CARTESIAN_POINT('Ctrl Pts',(-25.3164857451203,20.8546008853522,-50.2417583361434));
#18172=CARTESIAN_POINT('Ctrl Pts',(-25.3164661668358,20.8545880574544,-50.2417568995372));
#18173=CARTESIAN_POINT('Ctrl Pts',(-25.3164563215481,20.8545816067955,-50.2417561771149));
#18174=CARTESIAN_POINT('Ctrl Pts',(-25.3164365182896,20.8545686318024,-50.241754724003));
#18175=CARTESIAN_POINT('Ctrl Pts',(-25.3164265593842,20.8545621068577,-50.2417539932448));
#18176=CARTESIAN_POINT('Ctrl Pts',(-25.3164065228835,20.854548979363,-50.2417525230205));
#18177=CARTESIAN_POINT('Ctrl Pts',(-25.3163964462786,20.8545423774637,-50.241751783627));
#18178=CARTESIAN_POINT('Ctrl Pts',(-25.3163761763708,20.8545290973704,-50.2417502962783));
#18179=CARTESIAN_POINT('Ctrl Pts',(-25.3163659813274,20.8545224180379,-50.2417495481953));
#18180=CARTESIAN_POINT('Ctrl Pts',(-25.3163454674766,20.8545089784548,-50.2417480429491));
#18181=CARTESIAN_POINT('Ctrl Pts',(-25.316335149813,20.8545022189555,-50.2417472858699));
#18182=CARTESIAN_POINT('Ctrl Pts',(-25.3163143900167,20.8544886185827,-50.2417457625794));
#18183=CARTESIAN_POINT('Ctrl Pts',(-25.3163039474617,20.8544817774346,-50.2417449963373));
#18184=CARTESIAN_POINT('Ctrl Pts',(-25.3162829355784,20.8544680122609,-50.241743454552));
#18185=CARTESIAN_POINT('Ctrl Pts',(-25.3162723658106,20.8544610879495,-50.2417426789766));
#18186=CARTESIAN_POINT('Ctrl Pts',(-25.3162510940008,20.854447152852,-50.2417411181214));
#18187=CARTESIAN_POINT('Ctrl Pts',(-25.3162403931832,20.8544401428702,-50.2417403329313));
#18188=CARTESIAN_POINT('Ctrl Pts',(-25.3162130384493,20.8544222233332,-50.2417383257346));
#18189=CARTESIAN_POINT('Ctrl Pts',(-25.3161963847925,20.8544113140776,-50.2417371037478));
#18190=CARTESIAN_POINT('Ctrl Pts',(-25.3161621888355,20.8543889138985,-50.2417345945721));
#18191=CARTESIAN_POINT('Ctrl Pts',(-25.3161446457126,20.8543774224602,-50.2417333073229));
#18192=CARTESIAN_POINT('Ctrl Pts',(-25.3161086033742,20.8543538138081,-50.2417306626737));
#18193=CARTESIAN_POINT('Ctrl Pts',(-25.3160901048937,20.8543416971031,-50.2417293053278));
#18194=CARTESIAN_POINT('Ctrl Pts',(-25.3160520663688,20.8543167820168,-50.2417265142142));
#18195=CARTESIAN_POINT('Ctrl Pts',(-25.3160325260867,20.8543039835123,-50.2417250804291));
#18196=CARTESIAN_POINT('Ctrl Pts',(-25.3132022331559,20.8524502404983,-50.241517405584));
#18197=CARTESIAN_POINT('Ctrl Pts',(-25.3103885668257,20.8506136688153,-50.2413109964285));
#18198=CARTESIAN_POINT('Ctrl Pts',(-25.3037494041122,20.8462948624852,-50.2408240555912));
#18199=CARTESIAN_POINT('Ctrl Pts',(-25.2999215087333,20.8438163456926,-50.240543385359));
#18200=CARTESIAN_POINT('Ctrl Pts',(-25.2876680888495,20.8359192627766,-50.2396451881001));
#18201=CARTESIAN_POINT('Ctrl Pts',(-25.2792226172716,20.830531893,-50.2390265000034));
#18202=CARTESIAN_POINT('Ctrl Pts',(-25.1923656756222,20.7756938795585,-50.232667237762));
#18203=CARTESIAN_POINT('Ctrl Pts',(-25.1118876241331,20.7296135494006,-50.2268030202967));
#18204=CARTESIAN_POINT('Ctrl Pts',(-24.7705435170173,20.5532550727604,-50.2020061750991));
#18205=CARTESIAN_POINT('Ctrl Pts',(-24.4946061995773,20.4552166954043,-50.1819770665401));
#18206=CARTESIAN_POINT('Ctrl Pts',(-24.1619521466171,20.3857171687362,-50.159233896628));
#18207=CARTESIAN_POINT('Ctrl Pts',(-24.1143525715086,20.3768864974977,-50.1560163074523));
#18208=CARTESIAN_POINT('Ctrl Pts',(-23.9972707340411,20.3578833096796,-50.1482174639488));
#18209=CARTESIAN_POINT('Ctrl Pts',(-23.9276156883753,20.348901988529,-50.1436764124958));
#18210=CARTESIAN_POINT('Ctrl Pts',(-23.8465975529191,20.3411370817139,-50.1385500225014));
#18211=CARTESIAN_POINT('Ctrl Pts',(-23.8354723295114,20.3401291666838,-50.1378494680136));
#18212=CARTESIAN_POINT('Ctrl Pts',(-23.8210347256364,20.3388968081694,-50.1369449250092));
#18213=CARTESIAN_POINT('Ctrl Pts',(-23.8177271022499,20.3386196239797,-50.1367380085852));
#18214=CARTESIAN_POINT('Ctrl Pts',(-23.8123710462274,20.3381791095128,-50.1364034597079));
#18215=CARTESIAN_POINT('Ctrl Pts',(-23.8103228861163,20.3380126284564,-50.1362756491896));
#18216=CARTESIAN_POINT('Ctrl Pts',(-23.8063953621675,20.3376971676469,-50.1360307957626));
#18217=CARTESIAN_POINT('Ctrl Pts',(-23.8045160325539,20.3375478784749,-50.135913735879));
#18218=CARTESIAN_POINT('Ctrl Pts',(-23.8002009847008,20.3372089120075,-50.1356451946692));
#18219=CARTESIAN_POINT('Ctrl Pts',(-23.7977651753108,20.3370203548177,-50.1354937770644));
#18220=CARTESIAN_POINT('Ctrl Pts',(-23.7900605607506,20.3364327497014,-50.1350153703267));
#18221=CARTESIAN_POINT('Ctrl Pts',(-23.7847909527081,20.3360438869517,-50.1346889550394));
#18222=CARTESIAN_POINT('Ctrl Pts',(-23.7407378759118,20.3329019712742,-50.1319666276001));
#18223=CARTESIAN_POINT('Ctrl Pts',(-23.701906368189,20.3308378736766,-50.1296087597192));
#18224=CARTESIAN_POINT('Ctrl Pts',(-23.6545350688029,20.3291789185289,-50.1267729262057));
#18225=CARTESIAN_POINT('Ctrl Pts',(-23.646023975837,20.3289146260291,-50.1262650135649));
#18226=CARTESIAN_POINT('Ctrl Pts',(-23.6307030236759,20.328499643136,-50.1253534237588));
#18227=CARTESIAN_POINT('Ctrl Pts',(-23.6238935784234,20.3283368043207,-50.1249492286689));
#18228=CARTESIAN_POINT('Ctrl Pts',(-23.2898947997024,20.321409086965,-50.1051687871448));
#18229=CARTESIAN_POINT('Ctrl Pts',(-22.9635481752055,20.3644945939467,-50.0877812691631));
#18230=CARTESIAN_POINT('Ctrl Pts',(-22.5240788380082,20.4924621811883,-50.0614472605143));
#18231=CARTESIAN_POINT('Ctrl Pts',(-22.4012478275343,20.5364682089086,-50.053769557474));
#18232=CARTESIAN_POINT('Ctrl Pts',(-22.2726711430846,20.5915375871081,-50.0452505704415));
#18233=CARTESIAN_POINT('Ctrl Pts',(-22.263930260567,20.5953272636757,-50.0446690122715));
#18234=CARTESIAN_POINT('Ctrl Pts',(-22.2511889896193,20.6009185859215,-50.043817707755));
#18235=CARTESIAN_POINT('Ctrl Pts',(-22.2471752156891,20.6026897557305,-50.0435490065917));
#18236=CARTESIAN_POINT('Ctrl Pts',(-22.2401247505953,20.6058181508242,-50.0430760914124));
#18237=CARTESIAN_POINT('Ctrl Pts',(-22.2370865140661,20.6071718946628,-50.042871997264));
#18238=CARTESIAN_POINT('Ctrl Pts',(-22.2311430464702,20.6098311548748,-50.0424721493944));
#18239=CARTESIAN_POINT('Ctrl Pts',(-22.2282376433837,20.6111362797852,-50.0422764093245));
#18240=CARTESIAN_POINT('Ctrl Pts',(-22.2207061464996,20.6145329014726,-50.0417682788296));
#18241=CARTESIAN_POINT('Ctrl Pts',(-22.2160830648774,20.6166310204909,-50.0414556603345));
#18242=CARTESIAN_POINT('Ctrl Pts',(-22.1997527663674,20.6240888772935,-50.0403488540552));
#18243=CARTESIAN_POINT('Ctrl Pts',(-22.1880728508341,20.6295077880025,-50.039552623334));
#18244=CARTESIAN_POINT('Ctrl Pts',(-21.9873743675207,20.7240877924514,-50.0257901834959));
#18245=CARTESIAN_POINT('Ctrl Pts',(-21.8074753929521,20.831338691536,-50.012167152358));
#18246=CARTESIAN_POINT('Ctrl Pts',(-21.4117530127917,21.122752107863,-49.9792070801838));
#18247=CARTESIAN_POINT('Ctrl Pts',(-21.2072704939656,21.3194710233723,-49.9596439535045));
#18248=CARTESIAN_POINT('Ctrl Pts',(-21.0201796111594,21.5539678151568,-49.9406445867811));
#18249=CARTESIAN_POINT('Ctrl Pts',(-21.009414551862,21.567687514963,-49.9395472483268));
#18250=CARTESIAN_POINT('Ctrl Pts',(-20.9963991267586,21.5845553785613,-49.9382161227806));
#18251=CARTESIAN_POINT('Ctrl Pts',(-20.9940426477454,21.5876207421544,-49.9379749401167));
#18252=CARTESIAN_POINT('Ctrl Pts',(-20.9903680187879,21.5924186311604,-49.9375985764283));
#18253=CARTESIAN_POINT('Ctrl Pts',(-20.9890461080359,21.5941482509935,-49.9374631284888));
#18254=CARTESIAN_POINT('Ctrl Pts',(-20.9867089210746,21.5972127134853,-49.9372235562282));
#18255=CARTESIAN_POINT('Ctrl Pts',(-20.9856929398078,21.598547001972,-49.9371193817052));
#18256=CARTESIAN_POINT('Ctrl Pts',(-20.9835204976667,21.6014046961486,-49.9368965599921));
#18257=CARTESIAN_POINT('Ctrl Pts',(-20.9823643545868,21.6029283341004,-49.9367779355847));
#18258=CARTESIAN_POINT('Ctrl Pts',(-20.9790171240451,21.6073476892115,-49.9364343734598));
#18259=CARTESIAN_POINT('Ctrl Pts',(-20.9768295644485,21.6102460934441,-49.9362096860037));
#18260=CARTESIAN_POINT('Ctrl Pts',(-20.9670424276813,21.623259230776,-49.9352037082689));
#18261=CARTESIAN_POINT('Ctrl Pts',(-20.9594974165506,21.6334151444595,-49.934426217781));
#18262=CARTESIAN_POINT('Ctrl Pts',(-20.9505359937039,21.6456271850315,-49.9335000420566));
#18263=CARTESIAN_POINT('Ctrl Pts',(-20.949062057381,21.6476406675715,-49.9333476193017));
#18264=CARTESIAN_POINT('Ctrl Pts',(-20.7458123518565,21.9259692109315,-49.9123164835966));
#18265=CARTESIAN_POINT('Ctrl Pts',(-20.5892825295412,22.2327034267842,-49.8942103961434));
#18266=CARTESIAN_POINT('Ctrl Pts',(-20.4499226741283,22.6635252302605,-49.8683969487487));
#18267=CARTESIAN_POINT('Ctrl Pts',(-20.4213438088466,22.770344059194,-49.8619885794897));
#18268=CARTESIAN_POINT('Ctrl Pts',(-20.388010474822,22.9267277684508,-49.852462266578));
#18269=CARTESIAN_POINT('Ctrl Pts',(-20.3788248170785,22.9752709685916,-49.8494860659408));
#18270=CARTESIAN_POINT('Ctrl Pts',(-20.3694678225881,23.0318041701198,-49.8459917853832));
#18271=CARTESIAN_POINT('Ctrl Pts',(-20.3682055342755,23.0396088459752,-49.845508766755));
#18272=CARTESIAN_POINT('Ctrl Pts',(-20.366338220827,23.0514301959241,-49.8447762037539));
#18273=CARTESIAN_POINT('Ctrl Pts',(-20.3657120433869,23.0554435385461,-49.8445273318617));
#18274=CARTESIAN_POINT('Ctrl Pts',(-20.3645935109586,23.0627025925342,-49.8440768836937));
#18275=CARTESIAN_POINT('Ctrl Pts',(-20.3640985239652,23.0659478977344,-49.8438753913066));
#18276=CARTESIAN_POINT('Ctrl Pts',(-20.3630417931978,23.0729479282544,-49.8434405372689));
#18277=CARTESIAN_POINT('Ctrl Pts',(-20.3624817243261,23.076702898027,-49.843207122772));
#18278=CARTESIAN_POINT('Ctrl Pts',(-20.3610302424024,23.0865535942789,-49.8425943931043));
#18279=CARTESIAN_POINT('Ctrl Pts',(-20.36014967387,23.0926508809827,-49.8422147344845));
#18280=CARTESIAN_POINT('Ctrl Pts',(-20.3563922652732,23.1192061680272,-49.840559463026));
#18281=CARTESIAN_POINT('Ctrl Pts',(-20.3536947489173,23.1396886774523,-49.8392781814762));
#18282=CARTESIAN_POINT('Ctrl Pts',(-20.3095087415122,23.5020806693544,-49.8165247135761));
#18283=CARTESIAN_POINT('Ctrl Pts',(-20.3229102067689,23.8483743413689,-49.7930996990299));
#18284=CARTESIAN_POINT('Ctrl Pts',(-20.4182598044101,24.3223432656205,-49.7605507383427));
#18285=CARTESIAN_POINT('Ctrl Pts',(-20.4545391319408,24.4569336796419,-49.7513007592741));
#18286=CARTESIAN_POINT('Ctrl Pts',(-20.5044837763894,24.6036553632162,-49.7414987900895));
#18287=CARTESIAN_POINT('Ctrl Pts',(-20.5096600760049,24.6185045519117,-49.740510132091));
#18288=CARTESIAN_POINT('Ctrl Pts',(-20.5162016786626,24.6368375338564,-49.7392942222472));
#18289=CARTESIAN_POINT('Ctrl Pts',(-20.5174645119276,24.6403572850109,-49.739060994819));
#18290=CARTESIAN_POINT('Ctrl Pts',(-20.5194626737804,24.6458961859858,-49.7386943216765));
#18291=CARTESIAN_POINT('Ctrl Pts',(-20.5201938954758,24.6479167978367,-49.7385606309943));
#18292=CARTESIAN_POINT('Ctrl Pts',(-20.5215641657706,24.651691513139,-49.738311021361));
#18293=CARTESIAN_POINT('Ctrl Pts',(-20.5222027132966,24.6534457808833,-49.7381950735894));
#18294=CARTESIAN_POINT('Ctrl Pts',(-20.5236393598822,24.6573820040369,-49.737935035595));
#18295=CARTESIAN_POINT('Ctrl Pts',(-20.5244382925804,24.6595636471099,-49.7377909964453));
#18296=CARTESIAN_POINT('Ctrl Pts',(-20.5264742844153,24.6651047595953,-49.7374253691098));
#18297=CARTESIAN_POINT('Ctrl Pts',(-20.5277145870833,24.6684630451683,-49.737203975308));
#18298=CARTESIAN_POINT('Ctrl Pts',(-20.5345743312589,24.686941919117,-49.7359868322829));
#18299=CARTESIAN_POINT('Ctrl Pts',(-20.5403017725884,24.7020225718351,-49.7349974680043));
#18300=CARTESIAN_POINT('Ctrl Pts',(-20.6622212337014,25.0159214111125,-49.7144742219785));
#18301=CARTESIAN_POINT('Ctrl Pts',(-20.8222680473139,25.2958447536944,-49.6973660628039));
#18302=CARTESIAN_POINT('Ctrl Pts',(-21.0991314900078,25.6464388991739,-49.6720461834813));
#18303=CARTESIAN_POINT('Ctrl Pts',(-21.1829393425262,25.7406440667304,-49.664783428253));
#18304=CARTESIAN_POINT('Ctrl Pts',(-21.3098639827515,25.8675001418701,-49.6541133903177));
#18305=CARTESIAN_POINT('Ctrl Pts',(-21.3486212761428,25.9043546183876,-49.6508952996255));
#18306=CARTESIAN_POINT('Ctrl Pts',(-21.3942567741854,25.9456366135999,-49.6471432601842));
#18307=CARTESIAN_POINT('Ctrl Pts',(-21.4002579565977,25.9510244765975,-49.6466505802782));
#18308=CARTESIAN_POINT('Ctrl Pts',(-21.4093366251953,25.9591139666523,-49.6459063058606));
#18309=CARTESIAN_POINT('Ctrl Pts',(-21.4123991715399,25.9618323752324,-49.645655416949));
#18310=CARTESIAN_POINT('Ctrl Pts',(-21.4179289871208,25.9667219946389,-49.6452027257308));
#18311=CARTESIAN_POINT('Ctrl Pts',(-21.4203944162299,25.9688952857916,-49.6450010108997));
#18312=CARTESIAN_POINT('Ctrl Pts',(-21.4253391362841,25.9732406640172,-49.6445966735427));
#18313=CARTESIAN_POINT('Ctrl Pts',(-21.4278184437906,25.9754127263514,-49.6443940503254));
#18314=CARTESIAN_POINT('Ctrl Pts',(-21.434521208968,25.9812667082719,-49.6438465651668));
#18315=CARTESIAN_POINT('Ctrl Pts',(-21.4387509292319,25.9849414109663,-49.6435014036081));
#18316=CARTESIAN_POINT('Ctrl Pts',(-21.4553368811333,25.9992752497532,-49.6421491704837));
#18317=CARTESIAN_POINT('Ctrl Pts',(-21.4677642507908,26.0098513609089,-49.6411386727369));
#18318=CARTESIAN_POINT('Ctrl Pts',(-21.6633696427828,26.1737729801621,-49.6252736036894));
#18319=CARTESIAN_POINT('Ctrl Pts',(-21.8628644390159,26.3062983933942,-49.6095527808294));
#18320=CARTESIAN_POINT('Ctrl Pts',(-22.0750360207194,26.4155367773228,-49.5934531403533));
#18321=CARTESIAN_POINT('Origin',(-23.5502525316942,23.5502525316942,-77.3107734492734));
#18322=CARTESIAN_POINT('',(-22.0750360039475,26.4155367686876,-48.0944001480293));
#18323=CARTESIAN_POINT('',(-22.0750360153631,26.415536774565,-48.3398410585546));
#18324=CARTESIAN_POINT('',(-22.0750360153461,26.4155367745563,-77.3107734492734));
#18325=CARTESIAN_POINT('',(-26.7730021298787,23.5518618488042,-48.9415966136197));
#18326=CARTESIAN_POINT('Ctrl Pts',(-22.0750360039475,26.4155367686876,-48.0944001480293));
#18327=CARTESIAN_POINT('Ctrl Pts',(-22.0625887732288,26.4091282036162,-48.09532660084));
#18328=CARTESIAN_POINT('Ctrl Pts',(-22.0501825072825,26.4026381203314,-48.0962551212754));
#18329=CARTESIAN_POINT('Ctrl Pts',(-21.7725163997001,26.2550698835405,-48.1171500683835));
#18330=CARTESIAN_POINT('Ctrl Pts',(-21.5282523406975,26.0776798282403,-48.1380504180745));
#18331=CARTESIAN_POINT('Ctrl Pts',(-21.2870403498004,25.8448550398867,-48.1595706989458));
#18332=CARTESIAN_POINT('Ctrl Pts',(-21.262378884575,25.8202667324444,-48.1617807350983));
#18333=CARTESIAN_POINT('Ctrl Pts',(-21.2349097336589,25.7919765382236,-48.1642485383034));
#18334=CARTESIAN_POINT('Ctrl Pts',(-21.2317069554985,25.7886638445665,-48.1645363694615));
#18335=CARTESIAN_POINT('Ctrl Pts',(-21.22686887767,25.783638205244,-48.164971293972));
#18336=CARTESIAN_POINT('Ctrl Pts',(-21.2252283603404,25.7819303250401,-48.1651187929188));
#18337=CARTESIAN_POINT('Ctrl Pts',(-21.2223778179862,25.7789561789583,-48.165375122372));
#18338=CARTESIAN_POINT('Ctrl Pts',(-21.2211669428764,25.777690735112,-48.1654840196397));
#18339=CARTESIAN_POINT('Ctrl Pts',(-21.2187446984804,25.7751551962392,-48.1657018808578));
#18340=CARTESIAN_POINT('Ctrl Pts',(-21.2175333362632,25.7738850998876,-48.1658108441033));
#18341=CARTESIAN_POINT('Ctrl Pts',(-21.2145903253526,25.7707943425504,-48.1660755995659));
#18342=CARTESIAN_POINT('Ctrl Pts',(-21.2128597630664,25.7689726404851,-48.1662313064656));
#18343=CARTESIAN_POINT('Ctrl Pts',(-21.2092051600506,25.7651165471217,-48.1665601845476));
#18344=CARTESIAN_POINT('Ctrl Pts',(-21.2072816344027,25.7630816660154,-48.1667333158049));
#18345=CARTESIAN_POINT('Ctrl Pts',(-21.2021069081029,25.7575930562424,-48.1671991762352));
#18346=CARTESIAN_POINT('Ctrl Pts',(-21.1988606605349,25.7541346360319,-48.1674915272791));
#18347=CARTESIAN_POINT('Ctrl Pts',(-21.1161145471454,25.6655893439804,-48.1749465463505));
#18348=CARTESIAN_POINT('Ctrl Pts',(-21.0412662040387,25.5762515719009,-48.1817631982991));
#18349=CARTESIAN_POINT('Ctrl Pts',(-20.8000529502861,25.2544113876788,-48.2047711065651));
#18350=CARTESIAN_POINT('Ctrl Pts',(-20.6598605958874,25.0040072646886,-48.220201212852));
#18351=CARTESIAN_POINT('Ctrl Pts',(-20.5156234243607,24.6403312462466,-48.2429112139811));
#18352=CARTESIAN_POINT('Ctrl Pts',(-20.4815743555706,24.540432334521,-48.2491621203294));
#18353=CARTESIAN_POINT('Ctrl Pts',(-20.4496334201428,24.4291073033612,-48.256210759028));
#18354=CARTESIAN_POINT('Ctrl Pts',(-20.446828266588,24.4191497703988,-48.256841913022));
#18355=CARTESIAN_POINT('Ctrl Pts',(-20.4429394427688,24.4050864102072,-48.2577343328712));
#18356=CARTESIAN_POINT('Ctrl Pts',(-20.4418158484235,24.4009916093653,-48.2579942986));
#18357=CARTESIAN_POINT('Ctrl Pts',(-20.4398740573298,24.3938597872687,-48.258447291053));
#18358=CARTESIAN_POINT('Ctrl Pts',(-20.4390522059858,24.3908237592847,-48.2586401987118));
#18359=CARTESIAN_POINT('Ctrl Pts',(-20.4373456507233,24.3844827269534,-48.2590432487689));
#18360=CARTESIAN_POINT('Ctrl Pts',(-20.4364617631893,24.3811775091202,-48.2592534173823));
#18361=CARTESIAN_POINT('Ctrl Pts',(-20.4343826351071,24.3733528923157,-48.2597511567321));
#18362=CARTESIAN_POINT('Ctrl Pts',(-20.4331919638677,24.3688322970479,-48.2600388753806));
#18363=CARTESIAN_POINT('Ctrl Pts',(-20.4292874430094,24.3538760417347,-48.2609913051552));
#18364=CARTESIAN_POINT('Ctrl Pts',(-20.4266161535181,24.343429436979,-48.2616573941101));
#18365=CARTESIAN_POINT('Ctrl Pts',(-20.384303960178,24.1744300662099,-48.2724470963648));
#18366=CARTESIAN_POINT('Ctrl Pts',(-20.3567341204745,24.0131272109517,-48.2829643848882));
#18367=CARTESIAN_POINT('Ctrl Pts',(-20.3104686642528,23.5186082854301,-48.3158572334247));
#18368=CARTESIAN_POINT('Ctrl Pts',(-20.3310855188014,23.1839900232791,-48.3391900229575));
#18369=CARTESIAN_POINT('Ctrl Pts',(-20.4059707817135,22.8432494438367,-48.3612573309848));
#18370=CARTESIAN_POINT('Ctrl Pts',(-20.409431204229,22.8280319961916,-48.3622386839533));
#18371=CARTESIAN_POINT('Ctrl Pts',(-20.4138114167834,22.8093968067229,-48.3634348108927));
#18372=CARTESIAN_POINT('Ctrl Pts',(-20.4146263957595,22.8059550048508,-48.363655491745));
#18373=CARTESIAN_POINT('Ctrl Pts',(-20.415982969897,22.8002677239412,-48.3640197491373));
#18374=CARTESIAN_POINT('Ctrl Pts',(-20.4165213130549,22.7980214852302,-48.3641635127119));
#18375=CARTESIAN_POINT('Ctrl Pts',(-20.4174723178158,22.7940721532068,-48.3644160941215));
#18376=CARTESIAN_POINT('Ctrl Pts',(-20.4178839526641,22.7923688213315,-48.3645249713726));
#18377=CARTESIAN_POINT('Ctrl Pts',(-20.4187860226274,22.7886493736889,-48.3647625872896));
#18378=CARTESIAN_POINT('Ctrl Pts',(-20.4192770144226,22.7866334001925,-48.3648912928893));
#18379=CARTESIAN_POINT('Ctrl Pts',(-20.4205950058017,22.7812444733419,-48.3652351155361));
#18380=CARTESIAN_POINT('Ctrl Pts',(-20.4214255140287,22.7778723681848,-48.3654500288049));
#18381=CARTESIAN_POINT('Ctrl Pts',(-20.423267937923,22.7704433272696,-48.365923001553));
#18382=CARTESIAN_POINT('Ctrl Pts',(-20.4242823032629,22.7663869970449,-48.3661809204885));
#18383=CARTESIAN_POINT('Ctrl Pts',(-20.4273336801604,22.7542850131336,-48.3669494659465));
#18384=CARTESIAN_POINT('Ctrl Pts',(-20.4293938990702,22.7462451669669,-48.3674587867714));
#18385=CARTESIAN_POINT('Ctrl Pts',(-20.4367885328502,22.7178448870333,-48.3692537795239));
#18386=CARTESIAN_POINT('Ctrl Pts',(-20.4422914520189,22.6975283449827,-48.3705302927805));
#18387=CARTESIAN_POINT('Ctrl Pts',(-20.4735865563069,22.5863174720065,-48.3774835663004));
#18388=CARTESIAN_POINT('Ctrl Pts',(-20.5031695499096,22.4965291778998,-48.3829719226044));
#18389=CARTESIAN_POINT('Ctrl Pts',(-20.6436884877099,22.1257463939698,-48.4055988094271));
#18390=CARTESIAN_POINT('Ctrl Pts',(-20.7898794208234,21.8597838920622,-48.4218895392893));
#18391=CARTESIAN_POINT('Ctrl Pts',(-20.9831712292851,21.6017593739134,-48.4407770982359));
#18392=CARTESIAN_POINT('Ctrl Pts',(-20.9955306148411,21.5855826099918,-48.4419748928928));
#18393=CARTESIAN_POINT('Ctrl Pts',(-21.0108214617046,21.5659572282934,-48.4434454501685));
#18394=CARTESIAN_POINT('Ctrl Pts',(-21.0136081694865,21.5623960505268,-48.4437130021893));
#18395=CARTESIAN_POINT('Ctrl Pts',(-21.0188889274124,21.5556768728978,-48.4442191654296));
#18396=CARTESIAN_POINT('Ctrl Pts',(-21.0213814172274,21.5525176539001,-48.4444577196151));
#18397=CARTESIAN_POINT('Ctrl Pts',(-21.0265627685202,21.545975550922,-48.4449529013298));
#18398=CARTESIAN_POINT('Ctrl Pts',(-21.0292525288564,21.5425933918409,-48.4452095616096));
#18399=CARTESIAN_POINT('Ctrl Pts',(-21.0648210393213,21.4980530112639,-48.4485983461633));
#18400=CARTESIAN_POINT('Ctrl Pts',(-21.0986957539248,21.4577035008415,-48.4517674378346));
#18401=CARTESIAN_POINT('Ctrl Pts',(-21.1393109565201,21.4116655430357,-48.4555088065573));
#18402=CARTESIAN_POINT('Ctrl Pts',(-21.1451057131952,21.4051505839833,-48.4560412666273));
#18403=CARTESIAN_POINT('Ctrl Pts',(-21.1537878382799,21.395468806964,-48.4568370851176));
#18404=CARTESIAN_POINT('Ctrl Pts',(-21.1566552339007,21.39228406509,-48.457099600796));
#18405=CARTESIAN_POINT('Ctrl Pts',(-21.1617836452282,21.3866108687821,-48.4575685611331));
#18406=CARTESIAN_POINT('Ctrl Pts',(-21.1640422232325,21.384120210999,-48.4577749023314));
#18407=CARTESIAN_POINT('Ctrl Pts',(-21.1688150903041,21.3788734323361,-48.458210545946));
#18408=CARTESIAN_POINT('Ctrl Pts',(-21.1713302741994,21.376118135436,-48.4584398862504));
#18409=CARTESIAN_POINT('Ctrl Pts',(-21.1779930961137,21.3688446491991,-48.4590468066445));
#18410=CARTESIAN_POINT('Ctrl Pts',(-21.1821488428739,21.3643339381333,-48.4594247325239));
#18411=CARTESIAN_POINT('Ctrl Pts',(-21.2010751421603,21.3439083591188,-48.4611431088836));
#18412=CARTESIAN_POINT('Ctrl Pts',(-21.2159931471152,21.3281314495534,-48.4624898828902));
#18413=CARTESIAN_POINT('Ctrl Pts',(-21.3269650247111,21.2131210039306,-48.4724542191031));
#18414=CARTESIAN_POINT('Ctrl Pts',(-21.4291368776997,21.1200158376521,-48.4813439936919));
#18415=CARTESIAN_POINT('Ctrl Pts',(-21.6481939454459,20.9447610228789,-48.4998574208491));
#18416=CARTESIAN_POINT('Ctrl Pts',(-21.7652069971699,20.8632430439146,-48.5094755387822));
#18417=CARTESIAN_POINT('Ctrl Pts',(-22.0563389884322,20.6878546586753,-48.5324827293605));
#18418=CARTESIAN_POINT('Ctrl Pts',(-22.2344827127081,20.6017162144219,-48.5458572541248));
#18419=CARTESIAN_POINT('Ctrl Pts',(-22.4249222868872,20.5303545062692,-48.5587596223211));
#18420=CARTESIAN_POINT('Ctrl Pts',(-22.4304426190029,20.5283031600954,-48.5591324440799));
#18421=CARTESIAN_POINT('Ctrl Pts',(-22.449146118309,20.521411259232,-48.5603915302762));
#18422=CARTESIAN_POINT('Ctrl Pts',(-22.4623555328882,20.5166416593952,-48.5612739246607));
#18423=CARTESIAN_POINT('Ctrl Pts',(-22.479115737028,20.5107135093853,-48.562384493903));
#18424=CARTESIAN_POINT('Ctrl Pts',(-22.4826376673603,20.5094746702226,-48.562617362655));
#18425=CARTESIAN_POINT('Ctrl Pts',(-22.4882096922287,20.5075255842298,-48.5629849800685));
#18426=CARTESIAN_POINT('Ctrl Pts',(-22.4902583509053,20.5068112875683,-48.563119970085));
#18427=CARTESIAN_POINT('Ctrl Pts',(-22.4938945406286,20.5055475904437,-48.563359259596));
#18428=CARTESIAN_POINT('Ctrl Pts',(-22.4954817712766,20.5049973654464,-48.5634636081955));
#18429=CARTESIAN_POINT('Ctrl Pts',(-22.4991197230587,20.5037394285934,-48.5637025396719));
#18430=CARTESIAN_POINT('Ctrl Pts',(-22.5011707251942,20.5030325474968,-48.5638370722662));
#18431=CARTESIAN_POINT('Ctrl Pts',(-22.5069079002291,20.5010617000299,-48.5642129173741));
#18432=CARTESIAN_POINT('Ctrl Pts',(-22.5105956699819,20.4998023422652,-48.5644539549664));
#18433=CARTESIAN_POINT('Ctrl Pts',(-22.5188404542173,20.4970034712504,-48.5649916360898));
#18434=CARTESIAN_POINT('Ctrl Pts',(-22.5233986607553,20.4954674611691,-48.5652880742313));
#18435=CARTESIAN_POINT('Ctrl Pts',(-22.5374883148152,20.49075467372,-48.5662018864853));
#18436=CARTESIAN_POINT('Ctrl Pts',(-22.5470313014161,20.4876122212475,-48.5668172963515));
#18437=CARTESIAN_POINT('Ctrl Pts',(-22.5825547126252,20.4760984135653,-48.5690956188059));
#18438=CARTESIAN_POINT('Ctrl Pts',(-22.6086272902514,20.4680123356921,-48.5707429860009));
#18439=CARTESIAN_POINT('Ctrl Pts',(-22.7018437899409,20.4403957016421,-48.5765551328132));
#18440=CARTESIAN_POINT('Ctrl Pts',(-22.7695206058325,20.4227190136458,-48.5806325251765));
#18441=CARTESIAN_POINT('Ctrl Pts',(-23.2166397810928,20.3213553717628,-48.6069611290282));
#18442=CARTESIAN_POINT('Ctrl Pts',(-23.6079464127548,20.3046736333209,-48.6276040647128));
#18443=CARTESIAN_POINT('Ctrl Pts',(-24.0121987978122,20.360721994616,-48.6522972937338));
#18444=CARTESIAN_POINT('Ctrl Pts',(-24.031529155098,20.3635815123814,-48.6534850407414));
#18445=CARTESIAN_POINT('Ctrl Pts',(-24.0569071133381,20.3675718193061,-48.6550539394472));
#18446=CARTESIAN_POINT('Ctrl Pts',(-24.062979459188,20.3685444245444,-48.6554300607141));
#18447=CARTESIAN_POINT('Ctrl Pts',(-24.0723660559536,20.3700754413111,-48.6560125943732));
#18448=CARTESIAN_POINT('Ctrl Pts',(-24.0756823025816,20.3706216703927,-48.6562186190283));
#18449=CARTESIAN_POINT('Ctrl Pts',(-24.0822969828859,20.3717218253803,-48.6566299989592));
#18450=CARTESIAN_POINT('Ctrl Pts',(-24.0855954209009,20.3722757004591,-48.6568353523844));
#18451=CARTESIAN_POINT('Ctrl Pts',(-24.0929235467024,20.3735179749072,-48.6572920704274));
#18452=CARTESIAN_POINT('Ctrl Pts',(-24.0969527938465,20.374208908264,-48.6575435154686));
#18453=CARTESIAN_POINT('Ctrl Pts',(-24.108629193469,20.3762340495094,-48.6582731329766));
#18454=CARTESIAN_POINT('Ctrl Pts',(-24.1162728141645,20.3775882160427,-48.6587519409795));
#18455=CARTESIAN_POINT('Ctrl Pts',(-24.1692344630231,20.387168541915,-48.6620778511232));
#18456=CARTESIAN_POINT('Ctrl Pts',(-24.2143745220704,20.3963374116326,-48.664954927293));
#18457=CARTESIAN_POINT('Ctrl Pts',(-24.3503745488949,20.4270108386525,-48.6737576984558));
#18458=CARTESIAN_POINT('Ctrl Pts',(-24.4405045843798,20.4514975542336,-48.679776584192));
#18459=CARTESIAN_POINT('Ctrl Pts',(-24.6692783356723,20.5244562754472,-48.6955300152039));
#18460=CARTESIAN_POINT('Ctrl Pts',(-24.8058973144251,20.5785507954279,-48.705408106444));
#18461=CARTESIAN_POINT('Ctrl Pts',(-25.0003587387974,20.6713583912824,-48.7199892998986));
#18462=CARTESIAN_POINT('Ctrl Pts',(-25.0614122450346,20.7029316945391,-48.7246454100565));
#18463=CARTESIAN_POINT('Ctrl Pts',(-25.2065567813154,20.7839763093766,-48.7358506145005));
#18464=CARTESIAN_POINT('Ctrl Pts',(-25.289507715626,20.8353635974676,-48.7423704001027));
#18465=CARTESIAN_POINT('Ctrl Pts',(-25.3734414090793,20.8927880985035,-48.7490032681743));
#18466=CARTESIAN_POINT('Ctrl Pts',(-25.3768730131422,20.8951456575032,-48.7492745127282));
#18467=CARTESIAN_POINT('Ctrl Pts',(-25.3888199373307,20.9033874818409,-48.7502190243816));
#18468=CARTESIAN_POINT('Ctrl Pts',(-25.3973115601326,20.9093061770784,-48.7508907008086));
#18469=CARTESIAN_POINT('Ctrl Pts',(-25.4118141828719,20.9195187280865,-48.7520382250619));
#18470=CARTESIAN_POINT('Ctrl Pts',(-25.4178391578042,20.9237924953388,-48.7525150678665));
#18471=CARTESIAN_POINT('Ctrl Pts',(-25.4561739757982,20.951183594443,-48.7555495205143));
#18472=CARTESIAN_POINT('Ctrl Pts',(-25.4880705438722,20.9748772962822,-48.7580764957407));
#18473=CARTESIAN_POINT('Ctrl Pts',(-25.5237307965886,21.0024045452112,-48.7608965171035));
#18474=CARTESIAN_POINT('Ctrl Pts',(-25.5279310202789,21.0056634448298,-48.7612285892539));
#18475=CARTESIAN_POINT('Ctrl Pts',(-25.5340544512918,21.0104388565594,-48.7617125664865));
#18476=CARTESIAN_POINT('Ctrl Pts',(-25.5359839964076,21.0119471696969,-48.7618650507402));
#18477=CARTESIAN_POINT('Ctrl Pts',(-25.5393964527488,21.0146209375752,-48.7621346833478));
#18478=CARTESIAN_POINT('Ctrl Pts',(-25.5408800611607,21.0157854952609,-48.7622518959708));
#18479=CARTESIAN_POINT('Ctrl Pts',(-25.5437358951059,21.0180312352415,-48.7624774943016));
#18480=CARTESIAN_POINT('Ctrl Pts',(-25.5451082591138,21.0191122271626,-48.762585893148));
#18481=CARTESIAN_POINT('Ctrl Pts',(-25.5488029996504,21.0220273939485,-48.7628776994782));
#18482=CARTESIAN_POINT('Ctrl Pts',(-25.5511237370934,21.0238636582883,-48.7630609567088));
#18483=CARTESIAN_POINT('Ctrl Pts',(-25.5599125367578,21.0308374297148,-48.7637548580096));
#18484=CARTESIAN_POINT('Ctrl Pts',(-25.566363441161,21.0359966584179,-48.7642639555229));
#18485=CARTESIAN_POINT('Ctrl Pts',(-25.5823665541918,21.0488966350769,-48.7655265542763));
#18486=CARTESIAN_POINT('Ctrl Pts',(-25.5918945289732,21.0566674242728,-48.7662779733475));
#18487=CARTESIAN_POINT('Ctrl Pts',(-25.6291144126728,21.0873794219178,-48.7692131290252));
#18488=CARTESIAN_POINT('Ctrl Pts',(-25.6564671443365,21.110729848832,-48.7713697897656));
#18489=CARTESIAN_POINT('Ctrl Pts',(-25.7326571568299,21.178008556507,-48.7773948749799));
#18490=CARTESIAN_POINT('Ctrl Pts',(-25.780552275895,21.2229804138201,-48.781203831528));
#18491=CARTESIAN_POINT('Ctrl Pts',(-26.0239842128392,21.4659773572458,-48.8008858703337));
#18492=CARTESIAN_POINT('Ctrl Pts',(-26.1946361767158,21.6872443632114,-48.8159300031509));
#18493=CARTESIAN_POINT('Ctrl Pts',(-26.3553867082756,21.9631103889067,-48.8344043131287));
#18494=CARTESIAN_POINT('Ctrl Pts',(-26.3753468596096,21.998917694892,-48.8367947850814));
#18495=CARTESIAN_POINT('Ctrl Pts',(-26.3978515975773,22.0411652491172,-48.8396118650846));
#18496=CARTESIAN_POINT('Ctrl Pts',(-26.4010656923614,22.0472458156652,-48.8400172375522));
#18497=CARTESIAN_POINT('Ctrl Pts',(-26.4101184150067,22.0645056630013,-48.84116772132));
#18498=CARTESIAN_POINT('Ctrl Pts',(-26.4159108747056,22.0757089130765,-48.8419142837949));
#18499=CARTESIAN_POINT('Ctrl Pts',(-26.4231847823085,22.0899821936172,-48.8428653050112));
#18500=CARTESIAN_POINT('Ctrl Pts',(-26.42472737604,22.0930210655285,-48.8430677764194));
#18501=CARTESIAN_POINT('Ctrl Pts',(-26.4294217000084,22.1023052260808,-48.8436863386655));
#18502=CARTESIAN_POINT('Ctrl Pts',(-26.4325579044372,22.1085583072656,-48.8441029329401));
#18503=CARTESIAN_POINT('Ctrl Pts',(-26.4364017761514,22.1162850379191,-48.844617701473));
#18504=CARTESIAN_POINT('Ctrl Pts',(-26.4371287308447,22.1177491127632,-48.844715240581));
#18505=CARTESIAN_POINT('Ctrl Pts',(-26.4431758367006,22.1299511825295,-48.8455281633168));
#18506=CARTESIAN_POINT('Ctrl Pts',(-26.4484371175296,22.1407181150175,-48.8462454784779));
#18507=CARTESIAN_POINT('Ctrl Pts',(-26.4588291086963,22.1622889504617,-48.8476827455507));
#18508=CARTESIAN_POINT('Ctrl Pts',(-26.4639599695666,22.1730925672083,-48.8484026780558));
#18509=CARTESIAN_POINT('Ctrl Pts',(-26.4789994741936,22.2052202630491,-48.8505440886882));
#18510=CARTESIAN_POINT('Ctrl Pts',(-26.4887348483143,22.2266241524303,-48.8519713567779));
#18511=CARTESIAN_POINT('Ctrl Pts',(-26.5008732996909,22.2541054388927,-48.8538053349721));
#18512=CARTESIAN_POINT('Ctrl Pts',(-26.5034934843897,22.2600866210292,-48.8542045790501));
#18513=CARTESIAN_POINT('Ctrl Pts',(-26.5076325470082,22.269613672577,-48.8548406629974));
#18514=CARTESIAN_POINT('Ctrl Pts',(-26.5091632775615,22.2731543991117,-48.8550770969578));
#18515=CARTESIAN_POINT('Ctrl Pts',(-26.5118772925569,22.2794632489935,-48.8554984368283));
#18516=CARTESIAN_POINT('Ctrl Pts',(-26.5130630643143,22.2822303028363,-48.8556832574976));
#18517=CARTESIAN_POINT('Ctrl Pts',(-26.5157954745657,22.2886312676377,-48.8561108507973));
#18518=CARTESIAN_POINT('Ctrl Pts',(-26.517339311495,22.2922663629126,-48.8563537186633));
#18519=CARTESIAN_POINT('Ctrl Pts',(-26.5216470289197,22.3024612931751,-48.8570349750167));
#18520=CARTESIAN_POINT('Ctrl Pts',(-26.5243958505806,22.3090274310425,-48.8574738753375));
#18521=CARTESIAN_POINT('Ctrl Pts',(-26.5401471669495,22.3470055045489,-48.8600132587494));
#18522=CARTESIAN_POINT('Ctrl Pts',(-26.5526733159221,22.3786115329793,-48.8621298278362));
#18523=CARTESIAN_POINT('Ctrl Pts',(-26.5873490281897,22.4703153366671,-48.868282806512));
#18524=CARTESIAN_POINT('Ctrl Pts',(-26.6082090823643,22.5308800413996,-48.872361260698));
#18525=CARTESIAN_POINT('Ctrl Pts',(-26.7240475078328,22.9028518982277,-48.8975094081118));
#18526=CARTESIAN_POINT('Ctrl Pts',(-26.7731646259633,23.226454141433,-48.9200696560392));
#18527=CARTESIAN_POINT('Ctrl Pts',(-26.7730021298787,23.5518618488042,-48.9415966136197));
#18528=CARTESIAN_POINT('Ctrl Pts',(-26.7730021275415,23.5518665225018,-48.9415969228025));
#18529=CARTESIAN_POINT('Ctrl Pts',(-26.7729567465358,23.6424814237964,-48.9475914394289));
#18530=CARTESIAN_POINT('Ctrl Pts',(-26.7690895901357,23.7330660802197,-48.9534754575283));
#18531=CARTESIAN_POINT('Ctrl Pts',(-26.7610384286827,23.82772417437,-48.9594298922931));
#18532=CARTESIAN_POINT('Ctrl Pts',(-26.7606599341482,23.8320696702523,-48.9597028119813));
#18533=CARTESIAN_POINT('Ctrl Pts',(-26.7600379551602,23.8390467177372,-48.9601402979653));
#18534=CARTESIAN_POINT('Ctrl Pts',(-26.75980005591,23.8416787427777,-48.9603051733615));
#18535=CARTESIAN_POINT('Ctrl Pts',(-26.7593827892507,23.84623273136,-48.9605901605202));
#18536=CARTESIAN_POINT('Ctrl Pts',(-26.759204932593,23.8481548267028,-48.9607103570862));
#18537=CARTESIAN_POINT('Ctrl Pts',(-26.7588624974538,23.8518196290644,-48.9609393638615));
#18538=CARTESIAN_POINT('Ctrl Pts',(-26.7586982259238,23.8535623630601,-48.9610481914545));
#18539=CARTESIAN_POINT('Ctrl Pts',(-26.7583519296886,23.8572044099883,-48.9612754713449));
#18540=CARTESIAN_POINT('Ctrl Pts',(-26.7581696380846,23.8591036957877,-48.9613939080884));
#18541=CARTESIAN_POINT('Ctrl Pts',(-26.7577638594909,23.8632923626147,-48.9616549173684));
#18542=CARTESIAN_POINT('Ctrl Pts',(-26.7575396075129,23.8655816725151,-48.961797446419));
#18543=CARTESIAN_POINT('Ctrl Pts',(-26.7567469557411,23.8735852502377,-48.9622953056613));
#18544=CARTESIAN_POINT('Ctrl Pts',(-26.7561657298866,23.8792982810752,-48.9626499128697));
#18545=CARTESIAN_POINT('Ctrl Pts',(-26.7501011337481,23.9373670798313,-48.9662466883265));
#18546=CARTESIAN_POINT('Ctrl Pts',(-26.7433506170332,23.989586292889,-48.9694187468367));
#18547=CARTESIAN_POINT('Ctrl Pts',(-26.734702399696,24.0456444778887,-48.972779159396));
#18548=CARTESIAN_POINT('Ctrl Pts',(-26.734073947508,24.0496675241411,-48.9730200712531));
#18549=CARTESIAN_POINT('Ctrl Pts',(-26.7327533780536,24.0580173644067,-48.9735195850712));
#18550=CARTESIAN_POINT('Ctrl Pts',(-26.7320600572377,24.0623439621837,-48.9737781372859));
#18551=CARTESIAN_POINT('Ctrl Pts',(-26.727678888223,24.0893317850814,-48.9753892327602));
#18552=CARTESIAN_POINT('Ctrl Pts',(-26.7237577079695,24.1119549767869,-48.9767324504512));
#18553=CARTESIAN_POINT('Ctrl Pts',(-26.7172868662011,24.1470549849147,-48.9788077094251));
#18554=CARTESIAN_POINT('Ctrl Pts',(-26.7149045271264,24.1595614837528,-48.9795454113565));
#18555=CARTESIAN_POINT('Ctrl Pts',(-26.6560804733714,24.4587136573785,-48.9971563453131));
#18556=CARTESIAN_POINT('Ctrl Pts',(-26.5609967222382,24.7363857581216,-49.0128667683592));
#18557=CARTESIAN_POINT('Ctrl Pts',(-26.3927833667704,25.0710831774834,-49.0344844041002));
#18558=CARTESIAN_POINT('Ctrl Pts',(-26.3529731138757,25.1432569650069,-49.0393126003399));
#18559=CARTESIAN_POINT('Ctrl Pts',(-26.2884028590074,25.2503917818587,-49.0467899573306));
#18560=CARTESIAN_POINT('Ctrl Pts',(-26.2656385910068,25.2865183429035,-49.0493673024379));
#18561=CARTESIAN_POINT('Ctrl Pts',(-26.2379826302175,25.3285332518099,-49.0524353318259));
#18562=CARTESIAN_POINT('Ctrl Pts',(-26.2337786869781,25.3348709150991,-49.0529000466538));
#18563=CARTESIAN_POINT('Ctrl Pts',(-26.2272991732058,25.344564455887,-49.0536138133581));
#18564=CARTESIAN_POINT('Ctrl Pts',(-26.2250396171451,25.3479310483918,-49.053862260045));
#18565=CARTESIAN_POINT('Ctrl Pts',(-26.2209054998537,25.3540655656761,-49.0543159884572));
#18566=CARTESIAN_POINT('Ctrl Pts',(-26.2190329710048,25.3568348587752,-49.0545211929664));
#18567=CARTESIAN_POINT('Ctrl Pts',(-26.2152578508239,25.3623992265932,-49.0549342774717));
#18568=CARTESIAN_POINT('Ctrl Pts',(-26.2133551629919,25.3651942304437,-49.0551421609653));
#18569=CARTESIAN_POINT('Ctrl Pts',(-26.2079228080447,25.3731472979787,-49.0557347989312));
#18570=CARTESIAN_POINT('Ctrl Pts',(-26.2043825437837,25.3782980740122,-49.0561199567438));
#18571=CARTESIAN_POINT('Ctrl Pts',(-26.1892462226009,25.4001834432565,-49.0577622092377));
#18572=CARTESIAN_POINT('Ctrl Pts',(-26.1775069087434,25.4168179567027,-49.0590247772945));
#18573=CARTESIAN_POINT('Ctrl Pts',(-25.9521505927985,25.7298079857328,-49.0830581709015));
#18574=CARTESIAN_POINT('Ctrl Pts',(-25.6898642055569,25.9877693983333,-49.1080665703639));
#18575=CARTESIAN_POINT('Ctrl Pts',(-25.3309421236721,26.2373426121892,-49.1373663979367));
#18576=CARTESIAN_POINT('Ctrl Pts',(-25.2704222479836,26.2764817802581,-49.1421502015224));
#18577=CARTESIAN_POINT('Ctrl Pts',(-25.1787967277514,26.3314703565341,-49.1491132973499));
#18578=CARTESIAN_POINT('Ctrl Pts',(-25.1486661158156,26.3488955983873,-49.1513599344601));
#18579=CARTESIAN_POINT('Ctrl Pts',(-25.1029056874575,26.374379746724,-49.154701072346));
#18580=CARTESIAN_POINT('Ctrl Pts',(-25.0874834453558,26.3828039431672,-49.1558152027539));
#18581=CARTESIAN_POINT('Ctrl Pts',(-25.06558813087,26.394532470835,-49.1573793834898));
#18582=CARTESIAN_POINT('Ctrl Pts',(-25.0591719272884,26.3979415263556,-49.1578356347659));
#18583=CARTESIAN_POINT('Ctrl Pts',(-25.0479339989977,26.4038638136734,-49.1586309887028));
#18584=CARTESIAN_POINT('Ctrl Pts',(-25.0431173708502,26.4063865795262,-49.158970676795));
#18585=CARTESIAN_POINT('Ctrl Pts',(-25.0360837231905,26.4100478816885,-49.1594649384184));
#18586=CARTESIAN_POINT('Ctrl Pts',(-25.0338717639853,26.411196038153,-49.1596201190301));
#18587=CARTESIAN_POINT('Ctrl Pts',(-25.0300801006743,26.4131585880015,-49.1598856829612));
#18588=CARTESIAN_POINT('Ctrl Pts',(-25.028501053168,26.4139742412838,-49.1599961467792));
#18589=CARTESIAN_POINT('Ctrl Pts',(-25.0253561188513,26.4155954554208,-49.1602158921002));
#18590=CARTESIAN_POINT('Ctrl Pts',(-25.0237902488112,26.4164010379067,-49.1603251749774));
#18591=CARTESIAN_POINT('Ctrl Pts',(-25.0200839518579,26.4183039510962,-49.1605835365493));
#18592=CARTESIAN_POINT('Ctrl Pts',(-25.0179429515142,26.4194001716199,-49.160732544462));
#18593=CARTESIAN_POINT('Ctrl Pts',(-25.0115678307858,26.4226553146899,-49.1611755319071));
#18594=CARTESIAN_POINT('Ctrl Pts',(-25.0073301358853,26.4248072810717,-49.1614690732155));
#18595=CARTESIAN_POINT('Ctrl Pts',(-24.968499562134,26.444418110747,-49.1641505346628));
#18596=CARTESIAN_POINT('Ctrl Pts',(-24.9335973293514,26.4612620708883,-49.1665005369411));
#18597=CARTESIAN_POINT('Ctrl Pts',(-24.8649818034231,26.4928632757829,-49.1710205080573));
#18598=CARTESIAN_POINT('Ctrl Pts',(-24.8313032308686,26.5076805320263,-49.1731932180098));
#18599=CARTESIAN_POINT('Ctrl Pts',(-24.661626097081,26.5788892440546,-49.1839475645431));
#18600=CARTESIAN_POINT('Ctrl Pts',(-24.5221197254395,26.626495791773,-49.1921850125021));
#18601=CARTESIAN_POINT('Ctrl Pts',(-24.3634380166207,26.6687673956451,-49.2013629226141));
#18602=CARTESIAN_POINT('Ctrl Pts',(-24.3470043168155,26.6730064737956,-49.2023110958707));
#18603=CARTESIAN_POINT('Ctrl Pts',(-24.3116216291841,26.6818359598224,-49.2043487884643));
#18604=CARTESIAN_POINT('Ctrl Pts',(-24.2926629426245,26.6863846159111,-49.2054383061194));
#18605=CARTESIAN_POINT('Ctrl Pts',(-24.2514988423938,26.6958667078181,-49.2078007051296));
#18606=CARTESIAN_POINT('Ctrl Pts',(-24.2292801607809,26.7007376378881,-49.2090738141181));
#18607=CARTESIAN_POINT('Ctrl Pts',(-24.1804381771634,26.7109044222156,-49.2118707400491));
#18608=CARTESIAN_POINT('Ctrl Pts',(-24.153795872133,26.7160999277049,-49.2133953263303));
#18609=CARTESIAN_POINT('Ctrl Pts',(-24.0940075435168,26.7269770731785,-49.2168187295836));
#18610=CARTESIAN_POINT('Ctrl Pts',(-24.0608320531575,26.7324776677728,-49.2187197355504));
#18611=CARTESIAN_POINT('Ctrl Pts',(-23.9096143433815,26.755124439188,-49.2274070574949));
#18612=CARTESIAN_POINT('Ctrl Pts',(-23.7907726261889,26.7662268315229,-49.2343005819276));
#18613=CARTESIAN_POINT('Ctrl Pts',(-23.6199393809664,26.7726636754038,-49.244474280415));
#18614=CARTESIAN_POINT('Ctrl Pts',(-23.5682450903625,26.773366807634,-49.2475866494336));
#18615=CARTESIAN_POINT('Ctrl Pts',(-23.5085617023303,26.7727427786152,-49.2512260637711));
#18616=CARTESIAN_POINT('Ctrl Pts',(-23.5005653954728,26.7726294034196,-49.2517146182971));
#18617=CARTESIAN_POINT('Ctrl Pts',(-23.4884328885317,26.7724122131031,-49.2524573533995));
#18618=CARTESIAN_POINT('Ctrl Pts',(-23.4842962890748,26.7723301928601,-49.2527108493687));
#18619=CARTESIAN_POINT('Ctrl Pts',(-23.4768127957714,26.7721673933757,-49.2531699202211));
#18620=CARTESIAN_POINT('Ctrl Pts',(-23.4734658428679,26.7720893641579,-49.2533754084496));
#18621=CARTESIAN_POINT('Ctrl Pts',(-23.4667866720461,26.7719232355739,-49.2537858243134));
#18622=CARTESIAN_POINT('Ctrl Pts',(-23.4634544569821,26.7718351812716,-49.2539907502867));
#18623=CARTESIAN_POINT('Ctrl Pts',(-23.4541116813719,26.7715737911078,-49.2545657987274));
#18624=CARTESIAN_POINT('Ctrl Pts',(-23.4481014836733,26.7713888035794,-49.254936286761));
#18625=CARTESIAN_POINT('Ctrl Pts',(-23.4236315623909,26.7705670908518,-49.2564469980195));
#18626=CARTESIAN_POINT('Ctrl Pts',(-23.4051772417756,26.769788502479,-49.257591668744));
#18627=CARTESIAN_POINT('Ctrl Pts',(-23.0828687255674,26.753413550024,-49.2776798272868));
#18628=CARTESIAN_POINT('Ctrl Pts',(-22.7827898024326,26.6950260697744,-49.2981007390121));
#18629=CARTESIAN_POINT('Ctrl Pts',(-22.4002677386943,26.5625266408897,-49.3254915867263));
#18630=CARTESIAN_POINT('Ctrl Pts',(-22.3066967989176,26.5251191299678,-49.3322869313917));
#18631=CARTESIAN_POINT('Ctrl Pts',(-22.1678264692362,26.4619024759629,-49.3423892443644));
#18632=CARTESIAN_POINT('Ctrl Pts',(-22.1211488588169,26.4392783731394,-49.345787528242));
#18633=CARTESIAN_POINT('Ctrl Pts',(-22.0750360150599,26.4155367744089,-49.3491334787091));
#18634=CARTESIAN_POINT('Ctrl Pts',(-22.0750360207194,26.4155367773228,-49.5934531403533));
#18635=CARTESIAN_POINT('Ctrl Pts',(-22.0975079081856,26.427106624005,-49.5917479670868));
#18636=CARTESIAN_POINT('Ctrl Pts',(-22.1201220559539,26.4384152736554,-49.5900394829616));
#18637=CARTESIAN_POINT('Ctrl Pts',(-22.2880781858102,26.5199471563108,-49.5774121407802));
#18638=CARTESIAN_POINT('Ctrl Pts',(-22.4383791123868,26.5794294445297,-49.5664362692498));
#18639=CARTESIAN_POINT('Ctrl Pts',(-22.642195859053,26.6428660639966,-49.5524125383963));
#18640=CARTESIAN_POINT('Ctrl Pts',(-22.6922520479763,26.657125755106,-49.5490355965523));
#18641=CARTESIAN_POINT('Ctrl Pts',(-22.7675842448179,26.676626167679,-49.5440748684636));
#18642=CARTESIAN_POINT('Ctrl Pts',(-22.792611447065,26.6827853485506,-49.5424465948504));
#18643=CARTESIAN_POINT('Ctrl Pts',(-22.8219311134469,26.6896289436143,-49.5405642764711));
#18644=CARTESIAN_POINT('Ctrl Pts',(-22.8261534477659,26.690605515226,-49.5402938120567));
#18645=CARTESIAN_POINT('Ctrl Pts',(-22.8325981505533,26.6920824030801,-49.5398819344156));
#18646=CARTESIAN_POINT('Ctrl Pts',(-22.8348190797115,26.6925888802357,-49.5397401664924));
#18647=CARTESIAN_POINT('Ctrl Pts',(-22.8386824455193,26.6934656026781,-49.5394938561264));
#18648=CARTESIAN_POINT('Ctrl Pts',(-22.8403246311321,26.6938369147179,-49.5393892518762));
#18649=CARTESIAN_POINT('Ctrl Pts',(-22.843769508272,26.6946129934734,-49.5391700166708));
#18650=CARTESIAN_POINT('Ctrl Pts',(-22.8455722517542,26.69501749574,-49.5390554013944));
#18651=CARTESIAN_POINT('Ctrl Pts',(-22.8500327404483,26.6960143187445,-49.5387720885838));
#18652=CARTESIAN_POINT('Ctrl Pts',(-22.8526908965577,26.6966048231953,-49.538603496288));
#18653=CARTESIAN_POINT('Ctrl Pts',(-22.8631944171482,26.6989241957844,-49.5379382651893));
#18654=CARTESIAN_POINT('Ctrl Pts',(-22.8710455734795,26.7006271145302,-49.5374431113115));
#18655=CARTESIAN_POINT('Ctrl Pts',(-23.0129226856056,26.7308452812935,-49.5285316544743));
#18656=CARTESIAN_POINT('Ctrl Pts',(-23.1486460554971,26.750817537752,-49.5205906024215));
#18657=CARTESIAN_POINT('Ctrl Pts',(-23.3341350994132,26.7661221248341,-49.5100312447018));
#18658=CARTESIAN_POINT('Ctrl Pts',(-23.3831109539556,26.7690392380872,-49.5072709721861));
#18659=CARTESIAN_POINT('Ctrl Pts',(-23.6010741383817,26.7770332020473,-49.4950424786369));
#18660=CARTESIAN_POINT('Ctrl Pts',(-23.7702332011132,26.7699269078915,-49.4856859237203));
#18661=CARTESIAN_POINT('Ctrl Pts',(-24.0436685827172,26.7367830690584,-49.4699576292959));
#18662=CARTESIAN_POINT('Ctrl Pts',(-24.1485773604565,26.7187601420243,-49.4637787988912));
#18663=CARTESIAN_POINT('Ctrl Pts',(-24.2996215711956,26.6850419921105,-49.4545538159176));
#18664=CARTESIAN_POINT('Ctrl Pts',(-24.346601238612,26.6734379680743,-49.451637794015));
#18665=CARTESIAN_POINT('Ctrl Pts',(-24.4008902413153,26.6587240037998,-49.4482077133876));
#18666=CARTESIAN_POINT('Ctrl Pts',(-24.4084728522287,26.6566390636018,-49.4477272534286));
#18667=CARTESIAN_POINT('Ctrl Pts',(-24.4199514200567,26.6534376422684,-49.4469978189516));
#18668=CARTESIAN_POINT('Ctrl Pts',(-24.4238530652423,26.6523415204976,-49.446749508314));
#18669=CARTESIAN_POINT('Ctrl Pts',(-24.4309112744391,26.6503442266845,-49.4462996304829));
#18670=CARTESIAN_POINT('Ctrl Pts',(-24.4340685536346,26.64944558437,-49.4460981461018));
#18671=CARTESIAN_POINT('Ctrl Pts',(-24.4404137991494,26.6476290806542,-49.4456927240257));
#18672=CARTESIAN_POINT('Ctrl Pts',(-24.4436017320988,26.6467111175841,-49.445488783212));
#18673=CARTESIAN_POINT('Ctrl Pts',(-24.4522649111747,26.6442020690492,-49.4449338886527));
#18674=CARTESIAN_POINT('Ctrl Pts',(-24.4577373422873,26.6426013784949,-49.44458262105));
#18675=CARTESIAN_POINT('Ctrl Pts',(-24.4795365833807,26.636162233802,-49.4431803565251));
#18676=CARTESIAN_POINT('Ctrl Pts',(-24.4958289491037,26.6312089999372,-49.4421256045996));
#18677=CARTESIAN_POINT('Ctrl Pts',(-24.7763606749729,26.5434864936577,-49.4238457264704));
#18678=CARTESIAN_POINT('Ctrl Pts',(-25.0288285932198,26.4271494220938,-49.4054204557959));
#18679=CARTESIAN_POINT('Ctrl Pts',(-25.329317273431,26.2385841062258,-49.3814106331462));
#18680=CARTESIAN_POINT('Ctrl Pts',(-25.3938414146064,26.194752173251,-49.3761274987378));
#18681=CARTESIAN_POINT('Ctrl Pts',(-25.5407256476909,26.0869811624334,-49.3638774327463));
#18682=CARTESIAN_POINT('Ctrl Pts',(-25.6217070904627,26.0212958606118,-49.3569477740287));
#18683=CARTESIAN_POINT('Ctrl Pts',(-25.7207034237206,25.9327050749023,-49.3483803895977));
#18684=CARTESIAN_POINT('Ctrl Pts',(-25.7417829977435,25.9133292424876,-49.3465503087621));
#18685=CARTESIAN_POINT('Ctrl Pts',(-25.774103771486,25.8828162298911,-49.3437390337215));
#18686=CARTESIAN_POINT('Ctrl Pts',(-25.7855253558886,25.871873338103,-49.3427445342516));
#18687=CARTESIAN_POINT('Ctrl Pts',(-25.7995523653758,25.8582347365101,-49.3415224050741));
#18688=CARTESIAN_POINT('Ctrl Pts',(-25.8022340037898,25.8556182400417,-49.3412887272013));
#18689=CARTESIAN_POINT('Ctrl Pts',(-25.8064476373062,25.8514925957241,-49.3409215049628));
#18690=CARTESIAN_POINT('Ctrl Pts',(-25.8079826843344,25.8499865912776,-49.3407877144075));
#18691=CARTESIAN_POINT('Ctrl Pts',(-25.8108474325151,25.8471704103993,-49.3405380145509));
#18692=CARTESIAN_POINT('Ctrl Pts',(-25.8121774938252,25.8458606238669,-49.340422076228));
#18693=CARTESIAN_POINT('Ctrl Pts',(-25.8151588621376,25.8429195952922,-49.3401621824195));
#18694=CARTESIAN_POINT('Ctrl Pts',(-25.8168095416713,25.8412877280205,-49.340018277756));
#18695=CARTESIAN_POINT('Ctrl Pts',(-25.8209966632281,25.837139371436,-49.3396532171404));
#18696=CARTESIAN_POINT('Ctrl Pts',(-25.8235306934871,25.8346204372816,-49.3394322545307));
#18697=CARTESIAN_POINT('Ctrl Pts',(-25.8374205879948,25.8207672891992,-49.3382208850104));
#18698=CARTESIAN_POINT('Ctrl Pts',(-25.8486961430384,25.8093523463161,-49.3372367926405));
#18699=CARTESIAN_POINT('Ctrl Pts',(-26.0754332320842,25.5763574069595,-49.3174210730235));
#18700=CARTESIAN_POINT('Ctrl Pts',(-26.2580384844972,25.3249660200484,-49.3008524065526));
#18701=CARTESIAN_POINT('Ctrl Pts',(-26.4897473261149,24.8847689247677,-49.2727421470666));
#18702=CARTESIAN_POINT('Ctrl Pts',(-26.5626610031226,24.7108310567506,-49.2618486030793));
#18703=CARTESIAN_POINT('Ctrl Pts',(-26.6229904198606,24.5221051770588,-49.2497845587341));
#18704=CARTESIAN_POINT('Ctrl Pts',(-26.6259631645772,24.5126556660406,-49.2491799745773));
#18705=CARTESIAN_POINT('Ctrl Pts',(-26.630227447683,24.4988791540285,-49.2482977158869));
#18706=CARTESIAN_POINT('Ctrl Pts',(-26.6315535536646,24.4945628426601,-49.2480211775141));
#18707=CARTESIAN_POINT('Ctrl Pts',(-26.6338606809879,24.486996822905,-49.2475362235022));
#18708=CARTESIAN_POINT('Ctrl Pts',(-26.6348456496207,24.4837483175464,-49.2473279377194));
#18709=CARTESIAN_POINT('Ctrl Pts',(-26.6367450352745,24.4774481618576,-49.2469238527489));
#18710=CARTESIAN_POINT('Ctrl Pts',(-26.6376600638998,24.474396698591,-49.2467280738751));
#18711=CARTESIAN_POINT('Ctrl Pts',(-26.6398287843243,24.4671252175234,-49.2462613942141));
#18712=CARTESIAN_POINT('Ctrl Pts',(-26.6410783544322,24.4629039854447,-49.2459903587622));
#18713=CARTESIAN_POINT('Ctrl Pts',(-26.6454910646547,24.4478841939649,-49.2450255407615));
#18714=CARTESIAN_POINT('Ctrl Pts',(-26.6486062662182,24.4370717396631,-49.2443301930727));
#18715=CARTESIAN_POINT('Ctrl Pts',(-26.6936083217375,24.2777436628749,-49.2340715857434));
#18716=CARTESIAN_POINT('Ctrl Pts',(-26.7248259381615,24.1264468228135,-49.2241588555701));
#18717=CARTESIAN_POINT('Ctrl Pts',(-26.7500987126622,23.9356850347559,-49.2114473536258));
#18718=CARTESIAN_POINT('Ctrl Pts',(-26.754438131268,23.8977698691747,-49.208911385436));
#18719=CARTESIAN_POINT('Ctrl Pts',(-26.7681229096629,23.755948325642,-49.1993965020762));
#18720=CARTESIAN_POINT('Ctrl Pts',(-26.7730944442293,23.6516874405683,-49.1923409029875));
#18721=CARTESIAN_POINT('Ctrl Pts',(-26.7728465732488,23.3742538390487,-49.1735607967991));
#18722=CARTESIAN_POINT('Ctrl Pts',(-26.7587427175285,23.2014123261941,-49.1618456192302));
#18723=CARTESIAN_POINT('Ctrl Pts',(-26.7245902886662,22.9924091793172,-49.1482161848915));
#18724=CARTESIAN_POINT('Ctrl Pts',(-26.7176763179749,22.9544033133532,-49.1457606099963));
#18725=CARTESIAN_POINT('Ctrl Pts',(-26.7091465976908,22.9118730275633,-49.1430453772746));
#18726=CARTESIAN_POINT('Ctrl Pts',(-26.7082025381722,22.9072191976012,-49.1427487073633));
#18727=CARTESIAN_POINT('Ctrl Pts',(-26.7067649862634,22.900212173412,-49.1423027101931));
#18728=CARTESIAN_POINT('Ctrl Pts',(-26.7062791461965,22.897857442893,-49.1421529478476));
#18729=CARTESIAN_POINT('Ctrl Pts',(-26.7054329484205,22.893779226352,-49.1418937748276));
#18730=CARTESIAN_POINT('Ctrl Pts',(-26.7050738134907,22.8920554922917,-49.1417842937381));
#18731=CARTESIAN_POINT('Ctrl Pts',(-26.7043223835432,22.8884636106587,-49.1415562922983));
#18732=CARTESIAN_POINT('Ctrl Pts',(-26.7039298417775,22.8865955192,-49.1414377868705));
#18733=CARTESIAN_POINT('Ctrl Pts',(-26.702992768437,22.8821556279684,-49.1411563117007));
#18734=CARTESIAN_POINT('Ctrl Pts',(-26.7024467478438,22.8795841360348,-49.140993428033));
#18735=CARTESIAN_POINT('Ctrl Pts',(-26.7006120045458,22.8709951242968,-49.14044984406));
#18736=CARTESIAN_POINT('Ctrl Pts',(-26.6993091821647,22.8649805803513,-49.140069951718));
#18737=CARTESIAN_POINT('Ctrl Pts',(-26.662882204658,22.6991113693642,-49.1296132755312));
#18738=CARTESIAN_POINT('Ctrl Pts',(-26.6156426434075,22.5421329476644,-49.1202253442559));
#18739=CARTESIAN_POINT('Ctrl Pts',(-26.4668300842655,22.1567317040386,-49.0969464905421));
#18740=CARTESIAN_POINT('Ctrl Pts',(-26.3502907431995,21.9352887576804,-49.0832904496715));
#18741=CARTESIAN_POINT('Ctrl Pts',(-26.1551382330422,21.6502770974722,-49.0631597745355));
#18742=CARTESIAN_POINT('Ctrl Pts',(-26.0973851441392,21.5735257343748,-49.0574548132892));
#18743=CARTESIAN_POINT('Ctrl Pts',(-26.0298197343569,21.4916200614403,-49.0509917225545));
#18744=CARTESIAN_POINT('Ctrl Pts',(-26.023305729356,21.4837992808552,-49.0503706669106));
#18745=CARTESIAN_POINT('Ctrl Pts',(-26.0140654140519,21.4728115328613,-49.0494925069135));
#18746=CARTESIAN_POINT('Ctrl Pts',(-26.0113697775207,21.4696187520656,-49.0492366610302));
#18747=CARTESIAN_POINT('Ctrl Pts',(-26.0066449951567,21.4640446283018,-49.0487888083604));
#18748=CARTESIAN_POINT('Ctrl Pts',(-26.0046185722838,21.4616609753031,-49.0485969138496));
#18749=CARTESIAN_POINT('Ctrl Pts',(-26.0003592561216,21.4566655598788,-49.0481939605298));
#18750=CARTESIAN_POINT('Ctrl Pts',(-25.9981256517518,21.4540544118602,-49.0479828724923));
#18751=CARTESIAN_POINT('Ctrl Pts',(-25.9927911105632,21.4478383325835,-49.0474792550143));
#18752=CARTESIAN_POINT('Ctrl Pts',(-25.9896863693835,21.4442366901025,-49.0471865680764));
#18753=CARTESIAN_POINT('Ctrl Pts',(-25.9792148496023,21.4321434700043,-49.0462008131347));
#18754=CARTESIAN_POINT('Ctrl Pts',(-25.9718116768996,21.4236836425772,-49.0455062308958));
#18755=CARTESIAN_POINT('Ctrl Pts',(-25.954237683648,21.403812077674,-49.043862769157));
#18756=CARTESIAN_POINT('Ctrl Pts',(-25.9440297011954,21.3924337062935,-49.0429123343568));
#18757=CARTESIAN_POINT('Ctrl Pts',(-25.828747511873,21.2657586962357,-49.0322243092749));
#18758=CARTESIAN_POINT('Ctrl Pts',(-25.7155322675603,21.158181840617,-49.0221323626888));
#18759=CARTESIAN_POINT('Ctrl Pts',(-25.3442072907263,20.853381890382,-48.9902367271506));
#18760=CARTESIAN_POINT('Ctrl Pts',(-25.0637981232711,20.6865913387992,-48.9675634603602));
#18761=CARTESIAN_POINT('Ctrl Pts',(-24.7628766840616,20.5643422241424,-48.9470143995007));
#18762=CARTESIAN_POINT('Ctrl Pts',(-24.7625335605392,20.5642028993626,-48.9469909734531));
#18763=CARTESIAN_POINT('Ctrl Pts',(-24.7478156332019,20.5582296624775,-48.9459863466688));
#18764=CARTESIAN_POINT('Ctrl Pts',(-24.7333985690961,20.5524994215711,-48.9450108147615));
#18765=CARTESIAN_POINT('Ctrl Pts',(-24.7156503350406,20.5455931523956,-48.9438208531043));
#18766=CARTESIAN_POINT('Ctrl Pts',(-24.7123582021844,20.5443183280629,-48.9436005878669));
#18767=CARTESIAN_POINT('Ctrl Pts',(-24.7069104785225,20.5422190739908,-48.9432368703767));
#18768=CARTESIAN_POINT('Ctrl Pts',(-24.7047560966887,20.5413915500088,-48.9430932320644));
#18769=CARTESIAN_POINT('Ctrl Pts',(-24.7009722156792,20.5399427781028,-48.9428413024894));
#18770=CARTESIAN_POINT('Ctrl Pts',(-24.6993431046424,20.5393205399532,-48.9427329512655));
#18771=CARTESIAN_POINT('Ctrl Pts',(-24.6960077625151,20.5380497089426,-48.9425113541662));
#18772=CARTESIAN_POINT('Ctrl Pts',(-24.6943014910657,20.5374012454627,-48.942398116341));
#18773=CARTESIAN_POINT('Ctrl Pts',(-24.6895891676365,20.5356149210458,-48.9420857233108));
#18774=CARTESIAN_POINT('Ctrl Pts',(-24.6865819524212,20.5344801030549,-48.9418867521956));
#18775=CARTESIAN_POINT('Ctrl Pts',(-24.6800165066005,20.5320137476784,-48.9414531826345));
#18776=CARTESIAN_POINT('Ctrl Pts',(-24.6764576031618,20.5306839973368,-48.9412186907904));
#18777=CARTESIAN_POINT('Ctrl Pts',(-24.6660756237772,20.5268257776988,-48.9405361597888));
#18778=CARTESIAN_POINT('Ctrl Pts',(-24.6592462709372,20.5243140990271,-48.9400891028638));
#18779=CARTESIAN_POINT('Ctrl Pts',(-24.5883057218364,20.4984962264614,-48.9354645519725));
#18780=CARTESIAN_POINT('Ctrl Pts',(-24.5234730010526,20.4772060860717,-48.9314013395652));
#18781=CARTESIAN_POINT('Ctrl Pts',(-24.4157737530889,20.4455902263549,-48.9248424599982));
#18782=CARTESIAN_POINT('Ctrl Pts',(-24.3732883040271,20.434058151931,-48.9223029286349));
#18783=CARTESIAN_POINT('Ctrl Pts',(-24.0470997403555,20.3526557288685,-48.9030783291185));
#18784=CARTESIAN_POINT('Ctrl Pts',(-23.755322356125,20.3207878374269,-48.8873132788591));
#18785=CARTESIAN_POINT('Ctrl Pts',(-23.3648675914253,20.3313345686431,-48.8645729784289));
#18786=CARTESIAN_POINT('Ctrl Pts',(-23.2666840494428,20.3384950137551,-48.8587301292027));
#18787=CARTESIAN_POINT('Ctrl Pts',(-23.1597143991977,20.3512394398913,-48.852173053691));
#18788=CARTESIAN_POINT('Ctrl Pts',(-23.1504451083214,20.3523846770462,-48.8516032989546));
#18789=CARTESIAN_POINT('Ctrl Pts',(-23.1366942888761,20.3541443353795,-48.8507557163725));
#18790=CARTESIAN_POINT('Ctrl Pts',(-23.1322088070671,20.3547279320841,-48.8504788636787));
#18791=CARTESIAN_POINT('Ctrl Pts',(-23.1245343506585,20.3557428747286,-48.8500045366332));
#18792=CARTESIAN_POINT('Ctrl Pts',(-23.121344756971,20.356169558636,-48.8498072100856));
#18793=CARTESIAN_POINT('Ctrl Pts',(-23.1151424394857,20.3570087237739,-48.8494231261229));
#18794=CARTESIAN_POINT('Ctrl Pts',(-23.1121296494338,20.3574206931681,-48.849236385148));
#18795=CARTESIAN_POINT('Ctrl Pts',(-23.10492770969,20.3584158731929,-48.8487895774475));
#18796=CARTESIAN_POINT('Ctrl Pts',(-23.1007391244065,20.3590030666663,-48.8485293847339));
#18797=CARTESIAN_POINT('Ctrl Pts',(-23.088193334579,20.3607870378944,-48.8477490412913));
#18798=CARTESIAN_POINT('Ctrl Pts',(-23.0798397131253,20.362008404321,-48.8472281114063));
#18799=CARTESIAN_POINT('Ctrl Pts',(-23.0071060890651,20.3729347197549,-48.8426806507235));
#18800=CARTESIAN_POINT('Ctrl Pts',(-22.9430331663998,20.3845551079751,-48.8385935403762));
#18801=CARTESIAN_POINT('Ctrl Pts',(-22.7795942385087,20.4193409439302,-48.8279471217776));
#18802=CARTESIAN_POINT('Ctrl Pts',(-22.680902384818,20.4452970665587,-48.8213040210221));
#18803=CARTESIAN_POINT('Ctrl Pts',(-22.2927887270105,20.5673271822396,-48.7943588920547));
#18804=CARTESIAN_POINT('Ctrl Pts',(-22.0164366043374,20.6995595218724,-48.7731376931124));
#18805=CARTESIAN_POINT('Ctrl Pts',(-21.7590763505427,20.8711061508532,-48.7531965094375));
#18806=CARTESIAN_POINT('Ctrl Pts',(-21.7553714803239,20.8735867972799,-48.7529094398673));
#18807=CARTESIAN_POINT('Ctrl Pts',(-21.7208600317703,20.8967982821713,-48.7502353989753));
#18808=CARTESIAN_POINT('Ctrl Pts',(-21.6904070868979,20.9180535288288,-48.7478762290566));
#18809=CARTESIAN_POINT('Ctrl Pts',(-21.6561563794648,20.9428507911263,-48.7452295622994));
#18810=CARTESIAN_POINT('Ctrl Pts',(-21.6519932286792,20.945880114009,-48.7449079767908));
#18811=CARTESIAN_POINT('Ctrl Pts',(-21.6458566494886,20.9503679366434,-48.7444341446921));
#18812=CARTESIAN_POINT('Ctrl Pts',(-21.6438776249272,20.9518187152021,-48.744281365186));
#18813=CARTESIAN_POINT('Ctrl Pts',(-21.6403797496466,20.9543890762678,-48.7440113866434));
#18814=CARTESIAN_POINT('Ctrl Pts',(-21.6388602241925,20.9555077331211,-48.7438941228026));
#18815=CARTESIAN_POINT('Ctrl Pts',(-21.6357252400114,20.9578199200212,-48.7436522312593));
#18816=CARTESIAN_POINT('Ctrl Pts',(-21.6341099180439,20.9590136232046,-48.7435276163908));
#18817=CARTESIAN_POINT('Ctrl Pts',(-21.629933555164,20.9621059449428,-48.7432054810465));
#18818=CARTESIAN_POINT('Ctrl Pts',(-21.6273742057868,20.9640068608231,-48.743008121826));
#18819=CARTESIAN_POINT('Ctrl Pts',(-21.6218016326251,20.9681586453014,-48.7425785049554));
#18820=CARTESIAN_POINT('Ctrl Pts',(-21.6187895150299,20.9704110009285,-48.7423463507975));
#18821=CARTESIAN_POINT('Ctrl Pts',(-21.6100418219927,20.9769761258533,-48.7416723023923));
#18822=CARTESIAN_POINT('Ctrl Pts',(-21.60431665445,20.9813028196859,-48.7412313611109));
#18823=CARTESIAN_POINT('Ctrl Pts',(-21.5455872353762,21.0259955195116,-48.7367097339907));
#18824=CARTESIAN_POINT('Ctrl Pts',(-21.4938279911415,21.0679801873633,-48.7327381148028));
#18825=CARTESIAN_POINT('Ctrl Pts',(-21.3627479563389,21.1812227873413,-48.7226056379018));
#18826=CARTESIAN_POINT('Ctrl Pts',(-21.2855929496266,21.2548662223083,-48.7165652180958));
#18827=CARTESIAN_POINT('Ctrl Pts',(-21.0731017897852,21.4788513419078,-48.6992272074093));
#18828=CARTESIAN_POINT('Ctrl Pts',(-20.9480900870268,21.6382570778448,-48.6880825141914));
#18829=CARTESIAN_POINT('Ctrl Pts',(-20.8077338175771,21.85672976859,-48.6731335150186));
#18830=CARTESIAN_POINT('Ctrl Pts',(-20.7779369415227,21.9059611960316,-48.6697866944855));
#18831=CARTESIAN_POINT('Ctrl Pts',(-20.740665065862,21.9714387434569,-48.6653467193498));
#18832=CARTESIAN_POINT('Ctrl Pts',(-20.731983770707,21.9869880373438,-48.6642931713985));
#18833=CARTESIAN_POINT('Ctrl Pts',(-20.7196249112983,22.0095618803614,-48.6627644163005));
#18834=CARTESIAN_POINT('Ctrl Pts',(-20.715843603709,22.0165294680999,-48.6622926563766));
#18835=CARTESIAN_POINT('Ctrl Pts',(-20.7112096620727,22.0251438191769,-48.6617094911271));
#18836=CARTESIAN_POINT('Ctrl Pts',(-20.7103326680423,22.0267775011935,-48.6615988999826));
#18837=CARTESIAN_POINT('Ctrl Pts',(-20.6880236897193,22.0684213134511,-48.6587799436781));
#18838=CARTESIAN_POINT('Ctrl Pts',(-20.6674387997649,22.108877364906,-48.6560435618705));
#18839=CARTESIAN_POINT('Ctrl Pts',(-20.6444612748875,22.1564983122312,-48.6528203313566));
#18840=CARTESIAN_POINT('Ctrl Pts',(-20.6412302114293,22.1632547699389,-48.6523629709846));
#18841=CARTESIAN_POINT('Ctrl Pts',(-20.6361170882535,22.1740432530182,-48.6516325725699));
#18842=CARTESIAN_POINT('Ctrl Pts',(-20.6342197637046,22.1780680480595,-48.6513600649143));
#18843=CARTESIAN_POINT('Ctrl Pts',(-20.6308888814549,22.1851719567128,-48.6508790346522));
#18844=CARTESIAN_POINT('Ctrl Pts',(-20.6294518416437,22.1882494379421,-48.6506706330818));
#18845=CARTESIAN_POINT('Ctrl Pts',(-20.626493778627,22.1946104655199,-48.6502398427367));
#18846=CARTESIAN_POINT('Ctrl Pts',(-20.6249734161483,22.1978943122497,-48.650017431471));
#18847=CARTESIAN_POINT('Ctrl Pts',(-20.6211014698528,22.2062944498116,-48.649448449743));
#18848=CARTESIAN_POINT('Ctrl Pts',(-20.6187577653232,22.2114143401864,-48.6491016077772));
#18849=CARTESIAN_POINT('Ctrl Pts',(-20.6092979203606,22.2322235745123,-48.6476916940024));
#18850=CARTESIAN_POINT('Ctrl Pts',(-20.6022943229896,22.2479634934697,-48.646624756197));
#18851=CARTESIAN_POINT('Ctrl Pts',(-20.557509296215,22.350826293858,-48.6396481040668));
#18852=CARTESIAN_POINT('Ctrl Pts',(-20.5234716410309,22.4395186480559,-48.6336116327341));
#18853=CARTESIAN_POINT('Ctrl Pts',(-20.448169579379,22.6650430433396,-48.6181940329165));
#18854=CARTESIAN_POINT('Ctrl Pts',(-20.4119972063323,22.8033520262698,-48.6086721098018));
#18855=CARTESIAN_POINT('Ctrl Pts',(-20.3377497671372,23.1907227166895,-48.5820633003659));
#18856=CARTESIAN_POINT('Ctrl Pts',(-20.3194846789699,23.4425699382387,-48.5647823129555));
#18857=CARTESIAN_POINT('Ctrl Pts',(-20.3313394823289,23.7080998643683,-48.5479918722126));
#18858=CARTESIAN_POINT('Ctrl Pts',(-20.3320620944576,23.7222040567293,-48.5471045035409));
#18859=CARTESIAN_POINT('Ctrl Pts',(-20.3330934036003,23.7400384765182,-48.5459885177985));
#18860=CARTESIAN_POINT('Ctrl Pts',(-20.333315899882,23.7437732478306,-48.5457551521051));
#18861=CARTESIAN_POINT('Ctrl Pts',(-20.3336778134725,23.7496750984065,-48.5453869190254));
#18862=CARTESIAN_POINT('Ctrl Pts',(-20.3338129172378,23.7518424238998,-48.5452518089594));
#18863=CARTESIAN_POINT('Ctrl Pts',(-20.334065783101,23.7558339074541,-48.5450031964936));
#18864=CARTESIAN_POINT('Ctrl Pts',(-20.3341829058967,23.7576580907777,-48.5448896587522));
#18865=CARTESIAN_POINT('Ctrl Pts',(-20.3344464202711,23.7617084214813,-48.5446377482922));
#18866=CARTESIAN_POINT('Ctrl Pts',(-20.3345935710591,23.7639345116348,-48.544499419321));
#18867=CARTESIAN_POINT('Ctrl Pts',(-20.3349043507566,23.7685629432944,-48.5442120611435));
#18868=CARTESIAN_POINT('Ctrl Pts',(-20.3350683608361,23.7709652590692,-48.5440630535227));
#18869=CARTESIAN_POINT('Ctrl Pts',(-20.3354980941764,23.7771575859987,-48.5436793229908));
#18870=CARTESIAN_POINT('Ctrl Pts',(-20.3357678283208,23.7809473286343,-48.5434448240731));
#18871=CARTESIAN_POINT('Ctrl Pts',(-20.3365737164673,23.7919941015368,-48.5427622673769));
#18872=CARTESIAN_POINT('Ctrl Pts',(-20.3371277526264,23.7992498620811,-48.5423151919203));
#18873=CARTESIAN_POINT('Ctrl Pts',(-20.3391065050481,23.8240568978418,-48.5407907270635));
#18874=CARTESIAN_POINT('Ctrl Pts',(-20.3406505198908,23.8415987047001,-48.5397196866321));
#18875=CARTESIAN_POINT('Ctrl Pts',(-20.3456832336404,23.8938674875193,-48.5365467506839));
#18876=CARTESIAN_POINT('Ctrl Pts',(-20.3495924405204,23.9285524298016,-48.5344654922422));
#18877=CARTESIAN_POINT('Ctrl Pts',(-20.3652006573589,24.049368293463,-48.5272795874743));
#18878=CARTESIAN_POINT('Ctrl Pts',(-20.3798202344228,24.1350885065831,-48.5222938628633));
#18879=CARTESIAN_POINT('Ctrl Pts',(-20.4706944076417,24.5627391530154,-48.4975367452816));
#18880=CARTESIAN_POINT('Ctrl Pts',(-20.5988529322427,24.8911651671507,-48.4785968961045));
#18881=CARTESIAN_POINT('Ctrl Pts',(-20.7876612272928,25.209956255913,-48.4561885134168));
#18882=CARTESIAN_POINT('Ctrl Pts',(-20.7981383384728,25.2272720920309,-48.4549586436408));
#18883=CARTESIAN_POINT('Ctrl Pts',(-20.8120558656314,25.249792312028,-48.4533419952281));
#18884=CARTESIAN_POINT('Ctrl Pts',(-20.8153494342785,25.2550872726168,-48.4529606380494));
#18885=CARTESIAN_POINT('Ctrl Pts',(-20.8204510410486,25.2632361269736,-48.4523717918824));
#18886=CARTESIAN_POINT('Ctrl Pts',(-20.8222482467243,25.2660968128208,-48.4521647044679));
#18887=CARTESIAN_POINT('Ctrl Pts',(-20.8258329671119,25.2717828906178,-48.4517523436892));
#18888=CARTESIAN_POINT('Ctrl Pts',(-20.8276203870326,25.274608337581,-48.4515470740206));
#18889=CARTESIAN_POINT('Ctrl Pts',(-20.8315878686558,25.2808583483926,-48.4510921969015));
#18890=CARTESIAN_POINT('Ctrl Pts',(-20.8337700082759,25.2842815806338,-48.4508425122894));
#18891=CARTESIAN_POINT('Ctrl Pts',(-20.8400710570237,25.2941252692056,-48.4501229653665));
#18892=CARTESIAN_POINT('Ctrl Pts',(-20.8442062802706,25.3005352042462,-48.4496524943695));
#18893=CARTESIAN_POINT('Ctrl Pts',(-20.8718904811528,25.3431153624163,-48.4465143207082));
#18894=CARTESIAN_POINT('Ctrl Pts',(-20.8961403222089,25.3788225989339,-48.443820369126));
#18895=CARTESIAN_POINT('Ctrl Pts',(-20.9681639066834,25.4804232403466,-48.4359681182858));
#18896=CARTESIAN_POINT('Ctrl Pts',(-21.0177230796161,25.5450039781833,-48.4307425078457));
#18897=CARTESIAN_POINT('Ctrl Pts',(-21.1004073196492,25.6446961986292,-48.422291871813));
#18898=CARTESIAN_POINT('Ctrl Pts',(-21.1319705186023,25.681061677452,-48.4191224527582));
#18899=CARTESIAN_POINT('Ctrl Pts',(-21.1889691182188,25.7438343083818,-48.4134997066853));
#18900=CARTESIAN_POINT('Ctrl Pts',(-21.2140631719153,25.7705406954405,-48.4110566128114));
#18901=CARTESIAN_POINT('Ctrl Pts',(-21.4358619832459,25.998666563722,-48.3897529547349));
#18902=CARTESIAN_POINT('Ctrl Pts',(-21.6577186481136,26.173933440987,-48.3702486348577));
#18903=CARTESIAN_POINT('Ctrl Pts',(-21.9053380276005,26.3216095283544,-48.3518747842697));
#18904=CARTESIAN_POINT('Ctrl Pts',(-21.9111592331467,26.3250563966818,-48.3514446649301));
#18905=CARTESIAN_POINT('Ctrl Pts',(-21.9278492457012,26.3348680849572,-48.3502167771492));
#18906=CARTESIAN_POINT('Ctrl Pts',(-21.9387447201346,26.3411876415089,-48.3494216139709));
#18907=CARTESIAN_POINT('Ctrl Pts',(-21.9568727300183,26.3515606366444,-48.348109579425));
#18908=CARTESIAN_POINT('Ctrl Pts',(-21.9640842467949,26.3556502694197,-48.3475904934599));
#18909=CARTESIAN_POINT('Ctrl Pts',(-21.9739852532848,26.3612147221348,-48.3468818062777));
#18910=CARTESIAN_POINT('Ctrl Pts',(-21.9766611051454,26.3627135521442,-48.3466906736602));
#18911=CARTESIAN_POINT('Ctrl Pts',(-21.980910151939,26.3650856164445,-48.3463878051533));
#18912=CARTESIAN_POINT('Ctrl Pts',(-21.9824819369371,26.3659613522498,-48.3462759073395));
#18913=CARTESIAN_POINT('Ctrl Pts',(-21.9856304259121,26.3677121108605,-48.3460520383965));
#18914=CARTESIAN_POINT('Ctrl Pts',(-21.9872071265352,26.3685871242438,-48.3459400683186));
#18915=CARTESIAN_POINT('Ctrl Pts',(-21.9908787648564,26.3706207255406,-48.3456796473428));
#18916=CARTESIAN_POINT('Ctrl Pts',(-21.9929742645306,26.3717783055037,-48.3455312619089));
#18917=CARTESIAN_POINT('Ctrl Pts',(-21.9994071743167,26.375322574951,-48.3450764789039));
#18918=CARTESIAN_POINT('Ctrl Pts',(-22.0037488217754,26.3777016201463,-48.3447705724961));
#18919=CARTESIAN_POINT('Ctrl Pts',(-22.0137691854714,26.3831623843668,-48.3440668874065));
#18920=CARTESIAN_POINT('Ctrl Pts',(-22.0194517439059,26.386237062041,-48.3436695505007));
#18921=CARTESIAN_POINT('Ctrl Pts',(-22.0383482932117,26.3963881254767,-48.342353846686));
#18922=CARTESIAN_POINT('Ctrl Pts',(-22.051602636388,26.4033895342728,-48.3414400290071));
#18923=CARTESIAN_POINT('Ctrl Pts',(-22.0682793503257,26.4120504812494,-48.3403009377785));
#18924=CARTESIAN_POINT('Ctrl Pts',(-22.0716561491687,26.4137966210548,-48.3400708338911));
#18925=CARTESIAN_POINT('Ctrl Pts',(-22.0750360153631,26.415536774565,-48.3398410585546));
#18926=CARTESIAN_POINT('Origin',(-23.5502525316942,23.5502525316942,-77.3107734492734));
#18927=CARTESIAN_POINT('',(-22.0750360041347,26.415536768784,-46.8440307128639));
#18928=CARTESIAN_POINT('',(-22.075036119826,26.4155368283487,-47.0942077761624));
#18929=CARTESIAN_POINT('',(-22.0750360153461,26.4155367745563,-77.3107734492734));
#18930=CARTESIAN_POINT('Ctrl Pts',(-22.0750360041347,26.415536768784,-46.8440307128639));
#18931=CARTESIAN_POINT('Ctrl Pts',(-22.0617973538971,26.4087207344862,-46.8448939685705));
#18932=CARTESIAN_POINT('Ctrl Pts',(-22.0486049166737,26.4018124210467,-46.845759825945));
#18933=CARTESIAN_POINT('Ctrl Pts',(-21.9782325485303,26.364337531751,-46.8504099569758));
#18934=CARTESIAN_POINT('Ctrl Pts',(-21.9219412593692,26.3321444734535,-46.8542415819791));
#18935=CARTESIAN_POINT('Ctrl Pts',(-21.8475121248935,26.2865451003208,-46.8594816902241));
#18936=CARTESIAN_POINT('Ctrl Pts',(-21.8284860184323,26.2746133648144,-46.8608369379362));
#18937=CARTESIAN_POINT('Ctrl Pts',(-21.7968069472908,26.2542822525078,-46.8631208245042));
#18938=CARTESIAN_POINT('Ctrl Pts',(-21.784085668844,26.2459904174565,-46.8640454691496));
#18939=CARTESIAN_POINT('Ctrl Pts',(-21.7669628396108,26.2346563861459,-46.8653004175424));
#18940=CARTESIAN_POINT('Ctrl Pts',(-21.7625094261512,26.2316925865386,-46.8656277691874));
#18941=CARTESIAN_POINT('Ctrl Pts',(-21.7554580687743,26.2269744495097,-46.8661476128196));
#18942=CARTESIAN_POINT('Ctrl Pts',(-21.7528552560251,26.2252273769495,-46.8663398300661));
#18943=CARTESIAN_POINT('Ctrl Pts',(-21.7474601347964,26.2215946080767,-46.8667389491385));
#18944=CARTESIAN_POINT('Ctrl Pts',(-21.744668227357,26.2197083255139,-46.8669458730176));
#18945=CARTESIAN_POINT('Ctrl Pts',(-21.7382840745544,26.2153804345445,-46.8674199227538));
#18946=CARTESIAN_POINT('Ctrl Pts',(-21.7346938025153,26.2129359392415,-46.8676871580563));
#18947=CARTESIAN_POINT('Ctrl Pts',(-21.7236702483595,26.2053977112748,-46.8685096626089));
#18948=CARTESIAN_POINT('Ctrl Pts',(-21.7162534270643,26.2002800870252,-46.8690658416));
#18949=CARTESIAN_POINT('Ctrl Pts',(-21.6606080051764,26.1615391217311,-46.8732597979878));
#18950=CARTESIAN_POINT('Ctrl Pts',(-21.6132888367138,26.1266346848498,-46.8769466360745));
#18951=CARTESIAN_POINT('Ctrl Pts',(-21.5553188563046,26.081373836786,-46.8816212885295));
#18952=CARTESIAN_POINT('Ctrl Pts',(-21.5437472971752,26.0722105334717,-46.8825625199561));
#18953=CARTESIAN_POINT('Ctrl Pts',(-21.4904405882721,26.029398826164,-46.8869363410957));
#18954=CARTESIAN_POINT('Ctrl Pts',(-21.4494880835879,25.9947933490911,-46.8904050929509));
#18955=CARTESIAN_POINT('Ctrl Pts',(-21.2132317707212,25.7848308368318,-46.9110648058796));
#18956=CARTESIAN_POINT('Ctrl Pts',(-21.0390894741094,25.587170814896,-46.9290988687397));
#18957=CARTESIAN_POINT('Ctrl Pts',(-20.8672048519715,25.33606538398,-46.9494424758253));
#18958=CARTESIAN_POINT('Ctrl Pts',(-20.8442181698907,25.3010382588787,-46.9522259833028));
#18959=CARTESIAN_POINT('Ctrl Pts',(-20.7858165773178,25.2081465426222,-46.9594495812359));
#18960=CARTESIAN_POINT('Ctrl Pts',(-20.7515318668456,25.1495907884584,-46.9638467998252));
#18961=CARTESIAN_POINT('Ctrl Pts',(-20.7116783729464,25.0763117731561,-46.9691215314157));
#18962=CARTESIAN_POINT('Ctrl Pts',(-20.7043373737445,25.0625775629877,-46.9701005227528));
#18963=CARTESIAN_POINT('Ctrl Pts',(-20.6953629075255,25.0454905357816,-46.9713061247124));
#18964=CARTESIAN_POINT('Ctrl Pts',(-20.6936354890233,25.0421876934592,-46.9715385917781));
#18965=CARTESIAN_POINT('Ctrl Pts',(-20.690922496168,25.0369784365136,-46.9719043332558));
#18966=CARTESIAN_POINT('Ctrl Pts',(-20.6899330963325,25.0350740347311,-46.97203785059));
#18967=CARTESIAN_POINT('Ctrl Pts',(-20.6880864950052,25.031510992184,-46.9722872968151));
#18968=CARTESIAN_POINT('Ctrl Pts',(-20.687228838393,25.029852606029,-46.9724032541889));
#18969=CARTESIAN_POINT('Ctrl Pts',(-20.6853055385183,25.0261257318557,-46.9726635190122));
#18970=CARTESIAN_POINT('Ctrl Pts',(-20.6842406962814,25.0240568389309,-46.9728077749742));
#18971=CARTESIAN_POINT('Ctrl Pts',(-20.6815379590678,25.0187916568753,-46.9731743301255));
#18972=CARTESIAN_POINT('Ctrl Pts',(-20.6799031598458,25.0155937701784,-46.9733964332031));
#18973=CARTESIAN_POINT('Ctrl Pts',(-20.6708892976152,24.9978884815273,-46.9746232294401));
#18974=CARTESIAN_POINT('Ctrl Pts',(-20.6636146991916,24.9833277311196,-46.9756214188908));
#18975=CARTESIAN_POINT('Ctrl Pts',(-20.5203407810084,24.6910343531535,-46.9954579244464));
#18976=CARTESIAN_POINT('Ctrl Pts',(-20.4248799514166,24.3951600816855,-47.0120341698549));
#18977=CARTESIAN_POINT('Ctrl Pts',(-20.3555298369252,23.9870622586498,-47.0354281403252));
#18978=CARTESIAN_POINT('Ctrl Pts',(-20.3430388509584,23.8831695340491,-47.041413946819));
#18979=CARTESIAN_POINT('Ctrl Pts',(-20.3315873573965,23.7221400975372,-47.0508755450341));
#18980=CARTESIAN_POINT('Ctrl Pts',(-20.3290558537634,23.6653273840794,-47.0542481709916));
#18981=CARTESIAN_POINT('Ctrl Pts',(-20.3276607328868,23.588123216149,-47.0588915530379));
#18982=CARTESIAN_POINT('Ctrl Pts',(-20.3274857990944,23.5677639183115,-47.0601217008978));
#18983=CARTESIAN_POINT('Ctrl Pts',(-20.3275162039612,23.5333564938741,-47.0622108183582));
#18984=CARTESIAN_POINT('Ctrl Pts',(-20.3276204731539,23.5193087169935,-47.0630666177642));
#18985=CARTESIAN_POINT('Ctrl Pts',(-20.3278890102855,23.5000747061631,-47.0642424210385));
#18986=CARTESIAN_POINT('Ctrl Pts',(-20.3279739625217,23.4948873762799,-47.0645599339599));
#18987=CARTESIAN_POINT('Ctrl Pts',(-20.3281302932074,23.486568512563,-47.065069781156));
#18988=CARTESIAN_POINT('Ctrl Pts',(-20.3281937123897,23.4834368233929,-47.0652618653115));
#18989=CARTESIAN_POINT('Ctrl Pts',(-20.3283351824986,23.4769202680563,-47.0656618743923));
#18990=CARTESIAN_POINT('Ctrl Pts',(-20.3284140020381,23.4735354239389,-47.0658698232106));
#18991=CARTESIAN_POINT('Ctrl Pts',(-20.3286071295908,23.4657676902345,-47.0663474408824));
#18992=CARTESIAN_POINT('Ctrl Pts',(-20.3287250477481,23.461384904256,-47.0666172227831));
#18993=CARTESIAN_POINT('Ctrl Pts',(-20.3291258365591,23.4475393347061,-47.0674704279294));
#18994=CARTESIAN_POINT('Ctrl Pts',(-20.3294414580854,23.4380776147196,-47.0680548786724));
#18995=CARTESIAN_POINT('Ctrl Pts',(-20.3324296689895,23.3589606434352,-47.0729537726236));
#18996=CARTESIAN_POINT('Ctrl Pts',(-20.3373196481172,23.2894123079943,-47.0773375420822));
#18997=CARTESIAN_POINT('Ctrl Pts',(-20.3454350314713,23.2106161187651,-47.0823981301487));
#18998=CARTESIAN_POINT('Ctrl Pts',(-20.3464517779048,23.2011553679717,-47.08300726854));
#18999=CARTESIAN_POINT('Ctrl Pts',(-20.3801025034337,22.9005734793209,-47.1024093181714));
#19000=CARTESIAN_POINT('Ctrl Pts',(-20.4522358843225,22.6152834436127,-47.1224670611751));
#19001=CARTESIAN_POINT('Ctrl Pts',(-20.5855505006402,22.2850802587583,-47.1463780076429));
#19002=CARTESIAN_POINT('Ctrl Pts',(-20.6109553438996,22.2271305394117,-47.1505943250702));
#19003=CARTESIAN_POINT('Ctrl Pts',(-20.667485763366,22.1078598540245,-47.1592659405423));
#19004=CARTESIAN_POINT('Ctrl Pts',(-20.6989026482498,22.0467079358772,-47.1637083577696));
#19005=CARTESIAN_POINT('Ctrl Pts',(-20.7376036926109,21.9769611889129,-47.1687317206941));
#19006=CARTESIAN_POINT('Ctrl Pts',(-20.743003083187,21.9673470754087,-47.1694231705848));
#19007=CARTESIAN_POINT('Ctrl Pts',(-20.7500840792734,21.9548889016379,-47.170317690645));
#19008=CARTESIAN_POINT('Ctrl Pts',(-20.7517207784185,21.9520196011798,-47.1705236095619));
#19009=CARTESIAN_POINT('Ctrl Pts',(-20.7543809879693,21.9473725982048,-47.1708569353029));
#19010=CARTESIAN_POINT('Ctrl Pts',(-20.7554017838038,21.9455933568952,-47.1709845178313));
#19011=CARTESIAN_POINT('Ctrl Pts',(-20.7573645294233,21.9421798569341,-47.1712292061707));
#19012=CARTESIAN_POINT('Ctrl Pts',(-20.758306212477,21.9405454554959,-47.1713463284693));
#19013=CARTESIAN_POINT('Ctrl Pts',(-20.7604745034774,21.9367897585847,-47.1716153836962));
#19014=CARTESIAN_POINT('Ctrl Pts',(-20.7617020992184,21.9346690294988,-47.1717672520724));
#19015=CARTESIAN_POINT('Ctrl Pts',(-20.7656040860108,21.9279458618129,-47.172248526888));
#19016=CARTESIAN_POINT('Ctrl Pts',(-20.7682874794295,21.9233486174671,-47.1725773496111));
#19017=CARTESIAN_POINT('Ctrl Pts',(-20.7911857822933,21.8843410872419,-47.1753653008139));
#19018=CARTESIAN_POINT('Ctrl Pts',(-20.8120279862677,21.8503004840158,-47.177784325062));
#19019=CARTESIAN_POINT('Ctrl Pts',(-20.9790454331558,21.588564369038,-47.1963456171584));
#19020=CARTESIAN_POINT('Ctrl Pts',(-21.1527569379827,21.3796803058727,-47.2110006121102));
#19021=CARTESIAN_POINT('Ctrl Pts',(-21.431746132,21.1191233576879,-47.232510879437));
#19022=CARTESIAN_POINT('Ctrl Pts',(-21.5167955263189,21.0475523447392,-47.2388446238688));
#19023=CARTESIAN_POINT('Ctrl Pts',(-21.670306456883,20.9313685222524,-47.2500983564281));
#19024=CARTESIAN_POINT('Ctrl Pts',(-21.7370828018914,20.8847010850375,-47.2549396878769));
#19025=CARTESIAN_POINT('Ctrl Pts',(-21.8143395975489,20.8349563942568,-47.2605134405143));
#19026=CARTESIAN_POINT('Ctrl Pts',(-21.8231557614661,20.8293402635072,-47.2611490808039));
#19027=CARTESIAN_POINT('Ctrl Pts',(-21.8389422485114,20.8193914893992,-47.2622866271828));
#19028=CARTESIAN_POINT('Ctrl Pts',(-21.8459021231342,20.8150423751377,-47.2627879195581));
#19029=CARTESIAN_POINT('Ctrl Pts',(-21.8564154209942,20.8085284906532,-47.2635448435893));
#19030=CARTESIAN_POINT('Ctrl Pts',(-21.8599565853941,20.8063439165117,-47.263799743835));
#19031=CARTESIAN_POINT('Ctrl Pts',(-21.8660949718367,20.8025734862848,-47.2642415110466));
#19032=CARTESIAN_POINT('Ctrl Pts',(-21.8686902337131,20.8009844361986,-47.2644282601176));
#19033=CARTESIAN_POINT('Ctrl Pts',(-21.8740290866806,20.7977259034166,-47.2648123787922));
#19034=CARTESIAN_POINT('Ctrl Pts',(-21.8767729299815,20.7960568415651,-47.2650097636152));
#19035=CARTESIAN_POINT('Ctrl Pts',(-21.8841387732989,20.7915913184023,-47.2655395688877));
#19036=CARTESIAN_POINT('Ctrl Pts',(-21.888765302435,20.7888023814877,-47.2658722646943));
#19037=CARTESIAN_POINT('Ctrl Pts',(-21.9056040913213,20.7787093587756,-47.2670828836337));
#19038=CARTESIAN_POINT('Ctrl Pts',(-21.9178575418911,20.7714746279035,-47.2679633350704));
#19039=CARTESIAN_POINT('Ctrl Pts',(-22.1292828481976,20.6485251040233,-47.2831475946921));
#19040=CARTESIAN_POINT('Ctrl Pts',(-22.340205051915,20.5544351795862,-47.2982583267488));
#19041=CARTESIAN_POINT('Ctrl Pts',(-22.6701077160021,20.4478307199388,-47.3216100270666));
#19042=CARTESIAN_POINT('Ctrl Pts',(-22.7827648297599,20.4180586934479,-47.3295234546108));
#19043=CARTESIAN_POINT('Ctrl Pts',(-22.9885197852767,20.3754533312228,-47.3436829744536));
#19044=CARTESIAN_POINT('Ctrl Pts',(-23.0810454723112,20.3604655964995,-47.3499450596661));
#19045=CARTESIAN_POINT('Ctrl Pts',(-23.2129113175266,20.344968498332,-47.3586153603607));
#19046=CARTESIAN_POINT('Ctrl Pts',(-23.2518061617596,20.3411132559289,-47.3611414874403));
#19047=CARTESIAN_POINT('Ctrl Pts',(-23.3170911307728,20.3358395215527,-47.3653189617976));
#19048=CARTESIAN_POINT('Ctrl Pts',(-23.3434451365479,20.334036424161,-47.3669882602258));
#19049=CARTESIAN_POINT('Ctrl Pts',(-23.3741744678156,20.3323132680365,-47.3689125308422));
#19050=CARTESIAN_POINT('Ctrl Pts',(-23.3785301049849,20.3320778941289,-47.3691847623406));
#19051=CARTESIAN_POINT('Ctrl Pts',(-23.3851669774262,20.3317327573079,-47.3695987695002));
#19052=CARTESIAN_POINT('Ctrl Pts',(-23.3874478516876,20.3316165761085,-47.3697409055185));
#19053=CARTESIAN_POINT('Ctrl Pts',(-23.3914109224923,20.3314189320698,-47.3699876165936));
#19054=CARTESIAN_POINT('Ctrl Pts',(-23.3930930553839,20.3313363634886,-47.3700922541369));
#19055=CARTESIAN_POINT('Ctrl Pts',(-23.3966173999533,20.3311661379833,-47.3703113202413));
#19056=CARTESIAN_POINT('Ctrl Pts',(-23.3984596169259,20.3310787440668,-47.3704257334943));
#19057=CARTESIAN_POINT('Ctrl Pts',(-23.403010497229,20.330866767588,-47.3707081388022));
#19058=CARTESIAN_POINT('Ctrl Pts',(-23.4057192509209,20.3307440217318,-47.3708760269253));
#19059=CARTESIAN_POINT('Ctrl Pts',(-23.4163741443601,20.3302746744788,-47.3715356250808));
#19060=CARTESIAN_POINT('Ctrl Pts',(-23.4243214884951,20.3299540674094,-47.3720258816204));
#19061=CARTESIAN_POINT('Ctrl Pts',(-23.5690192845518,20.3246532347125,-47.380921861269));
#19062=CARTESIAN_POINT('Ctrl Pts',(-23.7059688843849,20.3283577597362,-47.3888533519137));
#19063=CARTESIAN_POINT('Ctrl Pts',(-23.954186105668,20.3509431142435,-47.4029953352529));
#19064=CARTESIAN_POINT('Ctrl Pts',(-24.0654810817681,20.3669705773545,-47.4092500934105));
#19065=CARTESIAN_POINT('Ctrl Pts',(-24.320680828745,20.4174589333123,-47.423793069435));
#19066=CARTESIAN_POINT('Ctrl Pts',(-24.4634959094615,20.4560745035243,-47.4320889013825));
#19067=CARTESIAN_POINT('Ctrl Pts',(-24.6969895379359,20.5367877465825,-47.4464103239032));
#19068=CARTESIAN_POINT('Ctrl Pts',(-24.7892721830987,20.5735424195685,-47.4522774769329));
#19069=CARTESIAN_POINT('Ctrl Pts',(-24.890412640943,20.6193436956108,-47.4590039587461));
#19070=CARTESIAN_POINT('Ctrl Pts',(-24.9010933914153,20.6242510467542,-47.4597180504822));
#19071=CARTESIAN_POINT('Ctrl Pts',(-24.917488408652,20.6318927620447,-47.4608200733898));
#19072=CARTESIAN_POINT('Ctrl Pts',(-24.9232219342466,20.6345857628224,-47.4612065773598));
#19073=CARTESIAN_POINT('Ctrl Pts',(-24.9338710309585,20.6396259525855,-47.4619265374849));
#19074=CARTESIAN_POINT('Ctrl Pts',(-24.9387886707921,20.6419687380518,-47.4622598401406));
#19075=CARTESIAN_POINT('Ctrl Pts',(-24.9468984305534,20.6458575214774,-47.4628108805329));
#19076=CARTESIAN_POINT('Ctrl Pts',(-24.9500939935174,20.6473963479032,-47.4630283682338));
#19077=CARTESIAN_POINT('Ctrl Pts',(-24.9563440862442,20.6504188064498,-47.4634544456392));
#19078=CARTESIAN_POINT('Ctrl Pts',(-24.959398825031,20.6519019977394,-47.463663019745));
#19079=CARTESIAN_POINT('Ctrl Pts',(-24.9664479487446,20.6553383924866,-47.46414508766));
#19080=CARTESIAN_POINT('Ctrl Pts',(-24.9704406402646,20.6572950365662,-47.4644187015173));
#19081=CARTESIAN_POINT('Ctrl Pts',(-24.9811381219992,20.6625648890244,-47.4651533122397));
#19082=CARTESIAN_POINT('Ctrl Pts',(-24.9878354197033,20.6658931690694,-47.4656148367683));
#19083=CARTESIAN_POINT('Ctrl Pts',(-25.0349227904443,20.6894983830256,-47.468871179256));
#19084=CARTESIAN_POINT('Ctrl Pts',(-25.0748922761995,20.7105987868947,-47.4716948896382));
#19085=CARTESIAN_POINT('Ctrl Pts',(-25.1155887923938,20.7331899140132,-47.4746338884125));
#19086=CARTESIAN_POINT('Ctrl Pts',(-25.1167738788161,20.7338487484984,-47.4747195287587));
#19087=CARTESIAN_POINT('Ctrl Pts',(-25.1288947920409,20.740597240982,-47.4755960251268));
#19088=CARTESIAN_POINT('Ctrl Pts',(-25.1397953446281,20.7467497445412,-47.476389088828));
#19089=CARTESIAN_POINT('Ctrl Pts',(-25.1541113297589,20.7549403251158,-47.4774370316322));
#19090=CARTESIAN_POINT('Ctrl Pts',(-25.1575593317277,20.7569215046375,-47.4776899195798));
#19091=CARTESIAN_POINT('Ctrl Pts',(-25.1653284791891,20.7614047088825,-47.4782608447964));
#19092=CARTESIAN_POINT('Ctrl Pts',(-25.1696474873995,20.7639104005177,-47.4785790090972));
#19093=CARTESIAN_POINT('Ctrl Pts',(-25.1924850528609,20.7772307497336,-47.4802654846703));
#19094=CARTESIAN_POINT('Ctrl Pts',(-25.2109008049985,20.7882198138015,-47.4816398100409));
#19095=CARTESIAN_POINT('Ctrl Pts',(-25.3124456267901,20.85019639283,-47.4892982316818));
#19096=CARTESIAN_POINT('Ctrl Pts',(-25.3933303455758,20.9047489883541,-47.4957021716166));
#19097=CARTESIAN_POINT('Ctrl Pts',(-25.5231927479517,21.0011836452817,-47.5064756413385));
#19098=CARTESIAN_POINT('Ctrl Pts',(-25.5736149346995,21.0410197048902,-47.5107910864128));
#19099=CARTESIAN_POINT('Ctrl Pts',(-25.7129364982711,21.1580220425904,-47.5230666806483));
#19100=CARTESIAN_POINT('Ctrl Pts',(-25.7988478514112,21.2385890884365,-47.531066307469));
#19101=CARTESIAN_POINT('Ctrl Pts',(-25.9457457208314,21.3923041016103,-47.5453575933093));
#19102=CARTESIAN_POINT('Ctrl Pts',(-26.0082724415354,21.4638034066355,-47.5516724899737));
#19103=CARTESIAN_POINT('Ctrl Pts',(-26.0985950253867,21.5767938145125,-47.5610426117928));
#19104=CARTESIAN_POINT('Ctrl Pts',(-26.1287344254795,21.6163392492569,-47.5642160608358));
#19105=CARTESIAN_POINT('Ctrl Pts',(-26.1608998024438,21.6606325665487,-47.5676415001442));
#19106=CARTESIAN_POINT('Ctrl Pts',(-26.1638413587519,21.6647032141632,-47.5679551291323));
#19107=CARTESIAN_POINT('Ctrl Pts',(-26.1681854499258,21.6707444449664,-47.5684188246096));
#19108=CARTESIAN_POINT('Ctrl Pts',(-26.1695952832584,21.6727097326198,-47.5685693954869));
#19109=CARTESIAN_POINT('Ctrl Pts',(-26.1719936168834,21.6760609346103,-47.5688256775558));
#19110=CARTESIAN_POINT('Ctrl Pts',(-26.172983231632,21.6774460451591,-47.5689314665877));
#19111=CARTESIAN_POINT('Ctrl Pts',(-26.1750096448848,21.6802870630739,-47.5691481706702));
#19112=CARTESIAN_POINT('Ctrl Pts',(-26.1760463275236,21.6817430457938,-47.5692590776212));
#19113=CARTESIAN_POINT('Ctrl Pts',(-26.1785332334019,21.685241970796,-47.5695252418675));
#19114=CARTESIAN_POINT('Ctrl Pts',(-26.1799822894141,21.6872857470487,-47.5696804179622));
#19115=CARTESIAN_POINT('Ctrl Pts',(-26.1852308605211,21.6947067575552,-47.5702428072437));
#19116=CARTESIAN_POINT('Ctrl Pts',(-26.1890163117902,21.7000939903794,-47.5706490545481));
#19117=CARTESIAN_POINT('Ctrl Pts',(-26.2509271634519,21.7887784153394,-47.5773043215657));
#19118=CARTESIAN_POINT('Ctrl Pts',(-26.3051061569114,21.8747762208373,-47.5832906013368));
#19119=CARTESIAN_POINT('Ctrl Pts',(-26.4037624409338,22.0491368207772,-47.5948283147031));
#19120=CARTESIAN_POINT('Ctrl Pts',(-26.4484145684482,22.1372677985473,-47.6003814547682));
#19121=CARTESIAN_POINT('Ctrl Pts',(-26.5566916300025,22.3777881095969,-47.6151460053493));
#19122=CARTESIAN_POINT('Ctrl Pts',(-26.6127733276649,22.5332408745153,-47.6243002187779));
#19123=CARTESIAN_POINT('Ctrl Pts',(-26.6910432130484,22.81663740077,-47.6411347831165));
#19124=CARTESIAN_POINT('Ctrl Pts',(-26.7178841376198,22.9429130446096,-47.6486821127377));
#19125=CARTESIAN_POINT('Ctrl Pts',(-26.7391319047749,23.0840392384923,-47.6573126872796));
#19126=CARTESIAN_POINT('Ctrl Pts',(-26.7410912866878,23.0976439575544,-47.6581465939898));
#19127=CARTESIAN_POINT('Ctrl Pts',(-26.7443696239255,23.1214867288704,-47.6596115664574));
#19128=CARTESIAN_POINT('Ctrl Pts',(-26.745726541553,23.1317194255068,-47.6602414271434));
#19129=CARTESIAN_POINT('Ctrl Pts',(-26.7476160382063,23.1465134367289,-47.6611537458396));
#19130=CARTESIAN_POINT('Ctrl Pts',(-26.7481880740367,23.1510697211231,-47.6614349548675));
#19131=CARTESIAN_POINT('Ctrl Pts',(-26.7491675531493,23.159008546947,-47.6619253396636));
#19132=CARTESIAN_POINT('Ctrl Pts',(-26.7495793753157,23.1623905489854,-47.6621343766136));
#19133=CARTESIAN_POINT('Ctrl Pts',(-26.7503634161464,23.1689155329448,-47.662537928585));
#19134=CARTESIAN_POINT('Ctrl Pts',(-26.7507363695441,23.1720584241957,-47.6627324201304));
#19135=CARTESIAN_POINT('Ctrl Pts',(-26.7516078060431,23.1794956574521,-47.6631929269654));
#19136=CARTESIAN_POINT('Ctrl Pts',(-26.752102278165,23.1837904557012,-47.6634590687595));
#19137=CARTESIAN_POINT('Ctrl Pts',(-26.7535478709375,23.196572630649,-47.6642517967511));
#19138=CARTESIAN_POINT('Ctrl Pts',(-26.7544738910744,23.2050627568472,-47.6647791748513));
#19139=CARTESIAN_POINT('Ctrl Pts',(-26.7627072088433,23.2834382303695,-47.6696554605864));
#19140=CARTESIAN_POINT('Ctrl Pts',(-26.7677603403508,23.3535365684622,-47.6740750797761));
#19141=CARTESIAN_POINT('Ctrl Pts',(-26.7707203924583,23.4288820121909,-47.6788935395248));
#19142=CARTESIAN_POINT('Ctrl Pts',(-26.7709100919968,23.4340246348451,-47.6792227543725));
#19143=CARTESIAN_POINT('Ctrl Pts',(-26.7723884515744,23.4768887296141,-47.6819695853973));
#19144=CARTESIAN_POINT('Ctrl Pts',(-26.7730266283869,23.5146284689443,-47.6844061844595));
#19145=CARTESIAN_POINT('Ctrl Pts',(-26.7729035704247,23.7019621054397,-47.6965900601896));
#19146=CARTESIAN_POINT('Ctrl Pts',(-26.7623899232043,23.8513515124925,-47.7065999799563));
#19147=CARTESIAN_POINT('Ctrl Pts',(-26.708452900686,24.2345376627611,-47.7327486043081));
#19148=CARTESIAN_POINT('Ctrl Pts',(-26.6494864425825,24.4652642392901,-47.7489886335974));
#19149=CARTESIAN_POINT('Ctrl Pts',(-26.5607912290871,24.7004559809181,-47.764864332236));
#19150=CARTESIAN_POINT('Ctrl Pts',(-26.5557963518902,24.7134453724226,-47.765738655074));
#19151=CARTESIAN_POINT('Ctrl Pts',(-26.54935950927,24.7298663427011,-47.7668404430173));
#19152=CARTESIAN_POINT('Ctrl Pts',(-26.5479956277592,24.7333280729802,-47.7670725138135));
#19153=CARTESIAN_POINT('Ctrl Pts',(-26.5458280437455,24.7388019031685,-47.7674391499264));
#19154=CARTESIAN_POINT('Ctrl Pts',(-26.5450283073043,24.7408155542676,-47.7675739544661));
#19155=CARTESIAN_POINT('Ctrl Pts',(-26.5435363206126,24.7445612022171,-47.7678245767746));
#19156=CARTESIAN_POINT('Ctrl Pts',(-26.5428446018212,24.7462933935928,-47.7679404256059));
#19157=CARTESIAN_POINT('Ctrl Pts',(-26.5412967289456,24.7501598032785,-47.7681988941076));
#19158=CARTESIAN_POINT('Ctrl Pts',(-26.5404397962093,24.7522937013399,-47.7683414654413));
#19159=CARTESIAN_POINT('Ctrl Pts',(-26.5379228525427,24.7585419423017,-47.7687586998311));
#19160=CARTESIAN_POINT('Ctrl Pts',(-26.5362566201195,24.7626537979144,-47.7690329857462));
#19161=CARTESIAN_POINT('Ctrl Pts',(-26.5239379169787,24.7928739166099,-47.7710468205445));
#19162=CARTESIAN_POINT('Ctrl Pts',(-26.5129512615402,24.8188458646461,-47.7727663945632));
#19163=CARTESIAN_POINT('Ctrl Pts',(-26.4757334853176,24.9037051921803,-47.7783585491426));
#19164=CARTESIAN_POINT('Ctrl Pts',(-26.4480750278351,24.9619532350114,-47.782155089418));
#19165=CARTESIAN_POINT('Ctrl Pts',(-26.3490773334306,25.1552494267479,-47.7947387234217));
#19166=CARTESIAN_POINT('Ctrl Pts',(-26.2698921510799,25.2860526028011,-47.8032352822164));
#19167=CARTESIAN_POINT('Ctrl Pts',(-26.0915808545907,25.5382540526202,-47.8204954181967));
#19168=CARTESIAN_POINT('Ctrl Pts',(-25.9922935529425,25.6590272083428,-47.8292411117475));
#19169=CARTESIAN_POINT('Ctrl Pts',(-25.8671920430915,25.7904646014397,-47.8397567218835));
#19170=CARTESIAN_POINT('Ctrl Pts',(-25.8495182670465,25.8086005673556,-47.8412314554028));
#19171=CARTESIAN_POINT('Ctrl Pts',(-25.8169167073545,25.8412752690036,-47.8439342187483));
#19172=CARTESIAN_POINT('Ctrl Pts',(-25.8020580644704,25.8558811842682,-47.8451595914002));
#19173=CARTESIAN_POINT('Ctrl Pts',(-25.7835649888661,25.873710426203,-47.8466774849437));
#19174=CARTESIAN_POINT('Ctrl Pts',(-25.78006331817,25.8770711698944,-47.846964584204));
#19175=CARTESIAN_POINT('Ctrl Pts',(-25.7736611541424,25.8831879505817,-47.8474889320059));
#19176=CARTESIAN_POINT('Ctrl Pts',(-25.770763090615,25.8859465246214,-47.8477260797917));
#19177=CARTESIAN_POINT('Ctrl Pts',(-25.7637781398705,25.892570526475,-47.8482971644642));
#19178=CARTESIAN_POINT('Ctrl Pts',(-25.7596862637958,25.8964306557096,-47.8486313098547));
#19179=CARTESIAN_POINT('Ctrl Pts',(-25.7505759676133,25.9049800134306,-47.8493743900267));
#19180=CARTESIAN_POINT('Ctrl Pts',(-25.7455526309979,25.9096639432213,-47.8497835334456));
#19181=CARTESIAN_POINT('Ctrl Pts',(-25.7362751132598,25.9182593375862,-47.8505381315842));
#19182=CARTESIAN_POINT('Ctrl Pts',(-25.7320253025991,25.9221754932104,-47.8508833955851));
#19183=CARTESIAN_POINT('Ctrl Pts',(-25.7268084285273,25.9269569041691,-47.851306749717));
#19184=CARTESIAN_POINT('Ctrl Pts',(-25.7258513270892,25.9278330513925,-47.8513843998196));
#19185=CARTESIAN_POINT('Ctrl Pts',(-25.7226911365864,25.930722438502,-47.8516407234415));
#19186=CARTESIAN_POINT('Ctrl Pts',(-25.720485784604,25.9327331920815,-47.8518194971427));
#19187=CARTESIAN_POINT('Ctrl Pts',(-25.712621801844,25.9398832845496,-47.8524566185536));
#19188=CARTESIAN_POINT('Ctrl Pts',(-25.7069477140139,25.9450055219908,-47.8529156555452));
#19189=CARTESIAN_POINT('Ctrl Pts',(-25.6793105875979,25.969776827654,-47.855148400613));
#19190=CARTESIAN_POINT('Ctrl Pts',(-25.6570975093795,25.9891437091238,-47.856933463041));
#19191=CARTESIAN_POINT('Ctrl Pts',(-25.6295800765584,26.0124788077354,-47.8591345835247));
#19192=CARTESIAN_POINT('Ctrl Pts',(-25.6245245212276,26.0167393015084,-47.859538561997));
#19193=CARTESIAN_POINT('Ctrl Pts',(-25.6162118135022,26.0237010785946,-47.8602021491472));
#19194=CARTESIAN_POINT('Ctrl Pts',(-25.6129623704095,26.0264115712651,-47.8604613805459));
#19195=CARTESIAN_POINT('Ctrl Pts',(-25.6071260294127,26.0312604401029,-47.8609266959869));
#19196=CARTESIAN_POINT('Ctrl Pts',(-25.6045411070135,26.0334011934501,-47.8611326826912));
#19197=CARTESIAN_POINT('Ctrl Pts',(-25.5990516558421,26.0379329501982,-47.8615699111964));
#19198=CARTESIAN_POINT('Ctrl Pts',(-25.5961462770467,26.0403229118749,-47.8618011949061));
#19199=CARTESIAN_POINT('Ctrl Pts',(-25.5883848308079,26.0466847159949,-47.8624187152953));
#19200=CARTESIAN_POINT('Ctrl Pts',(-25.5835213573027,26.0506474607845,-47.862805319733));
#19201=CARTESIAN_POINT('Ctrl Pts',(-25.5606622593701,26.0691621952075,-47.8646208378062));
#19202=CARTESIAN_POINT('Ctrl Pts',(-25.5425221560978,26.0835339737648,-47.8660569834112));
#19203=CARTESIAN_POINT('Ctrl Pts',(-25.4020079338285,26.1924158405113,-47.8771489000386));
#19204=CARTESIAN_POINT('Ctrl Pts',(-25.2731483245337,26.2781899388207,-47.8871481763896));
#19205=CARTESIAN_POINT('Ctrl Pts',(-24.8854611873628,26.4977951803487,-47.9167179495369));
#19206=CARTESIAN_POINT('Ctrl Pts',(-24.6140398443489,26.6062521831323,-47.9369236556562));
#19207=CARTESIAN_POINT('Ctrl Pts',(-24.3305363976869,26.6771161750845,-47.9558434141988));
#19208=CARTESIAN_POINT('Ctrl Pts',(-24.3293115995256,26.6774215589014,-47.9559251096147));
#19209=CARTESIAN_POINT('Ctrl Pts',(-24.3207618144074,26.6795479762501,-47.9564950942162));
#19210=CARTESIAN_POINT('Ctrl Pts',(-24.313430561039,26.6813440078023,-47.9569823290274));
#19211=CARTESIAN_POINT('Ctrl Pts',(-24.3034231065928,26.6837584261897,-47.9576452993145));
#19212=CARTESIAN_POINT('Ctrl Pts',(-24.3007523849871,26.6843991581375,-47.9578220222424));
#19213=CARTESIAN_POINT('Ctrl Pts',(-24.2620775509646,26.693625355581,-47.9603781405919));
#19214=CARTESIAN_POINT('Ctrl Pts',(-24.2259270052012,26.7015938123652,-47.9627296414857));
#19215=CARTESIAN_POINT('Ctrl Pts',(-24.1846039363556,26.7099585805031,-47.9653685461465));
#19216=CARTESIAN_POINT('Ctrl Pts',(-24.1795600736413,26.7109670138955,-47.9656898199352));
#19217=CARTESIAN_POINT('Ctrl Pts',(-24.172107495715,26.7124384816562,-47.966163273564));
#19218=CARTESIAN_POINT('Ctrl Pts',(-24.169700663438,26.7129108424495,-47.9663159851364));
#19219=CARTESIAN_POINT('Ctrl Pts',(-24.165441559326,26.7137416785302,-47.9665858799373));
#19220=CARTESIAN_POINT('Ctrl Pts',(-24.1635895107506,26.7141012752443,-47.966703127854));
#19221=CARTESIAN_POINT('Ctrl Pts',(-24.1597648750936,26.7148403880855,-47.9669450174277));
#19222=CARTESIAN_POINT('Ctrl Pts',(-24.1577922531819,26.7152196854642,-47.9670696462005));
#19223=CARTESIAN_POINT('Ctrl Pts',(-24.1526872904146,26.7161963234113,-47.9673918407488));
#19224=CARTESIAN_POINT('Ctrl Pts',(-24.149554405679,26.7167908616176,-47.9675892451703));
#19225=CARTESIAN_POINT('Ctrl Pts',(-24.1427227292941,26.7180768302361,-47.9680190151754));
#19226=CARTESIAN_POINT('Ctrl Pts',(-24.1390235927064,26.7187664356449,-47.9682512770475));
#19227=CARTESIAN_POINT('Ctrl Pts',(-24.1282616904498,26.7207532082102,-47.9689257253198));
#19228=CARTESIAN_POINT('Ctrl Pts',(-24.1211957306731,26.7220332607507,-47.9693669573613));
#19229=CARTESIAN_POINT('Ctrl Pts',(-23.9555121915603,26.751476491219,-47.9796769983529));
#19230=CARTESIAN_POINT('Ctrl Pts',(-23.7949834760435,26.7677348606644,-47.9888978287936));
#19231=CARTESIAN_POINT('Ctrl Pts',(-23.3757520520354,26.7786186633544,-48.0125083363321));
#19232=CARTESIAN_POINT('Ctrl Pts',(-23.1177613781264,26.7542726599896,-48.0266500808854));
#19233=CARTESIAN_POINT('Ctrl Pts',(-22.8454455323168,26.6950551324025,-48.0429752627857));
#19234=CARTESIAN_POINT('Ctrl Pts',(-22.8254918737524,26.6905165757998,-48.0441791865166));
#19235=CARTESIAN_POINT('Ctrl Pts',(-22.8013250602391,26.6847771142227,-48.0456473207597));
#19236=CARTESIAN_POINT('Ctrl Pts',(-22.7970691068637,26.683757190104,-48.0459062476904));
#19237=CARTESIAN_POINT('Ctrl Pts',(-22.7889185141786,26.6817863649306,-48.0464028527255));
#19238=CARTESIAN_POINT('Ctrl Pts',(-22.7850235437187,26.6808368590505,-48.0466404894344));
#19239=CARTESIAN_POINT('Ctrl Pts',(-22.7762118795118,26.6786713469832,-48.0471788347376));
#19240=CARTESIAN_POINT('Ctrl Pts',(-22.7712962679749,26.6774510149827,-48.0474796709734));
#19241=CARTESIAN_POINT('Ctrl Pts',(-22.7596723898274,26.6745362054221,-48.0481922989133));
#19242=CARTESIAN_POINT('Ctrl Pts',(-22.7529666812628,26.6728317070337,-48.0486043897545));
#19243=CARTESIAN_POINT('Ctrl Pts',(-22.7441876507059,26.6705700762383,-48.0491452045463));
#19244=CARTESIAN_POINT('Ctrl Pts',(-22.7421092896663,26.6700324392332,-48.0492733342308));
#19245=CARTESIAN_POINT('Ctrl Pts',(-22.7363855522159,26.6685457013298,-48.0496264660401));
#19246=CARTESIAN_POINT('Ctrl Pts',(-22.7327413079909,26.6675922871627,-48.0498515997971));
#19247=CARTESIAN_POINT('Ctrl Pts',(-22.7264096959591,26.6659239324678,-48.0502432770014));
#19248=CARTESIAN_POINT('Ctrl Pts',(-22.723721561379,26.6652118975012,-48.050409730781));
#19249=CARTESIAN_POINT('Ctrl Pts',(-22.7156619097791,26.6630658839282,-48.0509092936543));
#19250=CARTESIAN_POINT('Ctrl Pts',(-22.7102931975177,26.6616214889843,-48.0512427245238));
#19251=CARTESIAN_POINT('Ctrl Pts',(-22.6926947473034,26.6568379442574,-48.0523378954151));
#19252=CARTESIAN_POINT('Ctrl Pts',(-22.6804810822102,26.6534405533648,-48.0531014495013));
#19253=CARTESIAN_POINT('Ctrl Pts',(-22.6469525549751,26.6439006635392,-48.0552073754439));
#19254=CARTESIAN_POINT('Ctrl Pts',(-22.6256808709784,26.6376101102117,-48.0565544327209));
#19255=CARTESIAN_POINT('Ctrl Pts',(-22.5982987011248,26.629204175539,-48.0583032151905));
#19256=CARTESIAN_POINT('Ctrl Pts',(-22.5921269314877,26.6272891993241,-48.0586983531868));
#19257=CARTESIAN_POINT('Ctrl Pts',(-22.5823310537688,26.6242174058018,-48.0593270815939));
#19258=CARTESIAN_POINT('Ctrl Pts',(-22.578703139882,26.6230727043937,-48.0595602730121));
#19259=CARTESIAN_POINT('Ctrl Pts',(-22.5719145793246,26.6209175124845,-48.0599972637917));
#19260=CARTESIAN_POINT('Ctrl Pts',(-22.568753447111,26.619908558048,-48.0602010122901));
#19261=CARTESIAN_POINT('Ctrl Pts',(-22.5616415380342,26.6176265054982,-48.0606599961497));
#19262=CARTESIAN_POINT('Ctrl Pts',(-22.5576916565996,26.6163506548679,-48.0609153220629));
#19263=CARTESIAN_POINT('Ctrl Pts',(-22.5460779384951,26.6125745158803,-48.0616672654709));
#19264=CARTESIAN_POINT('Ctrl Pts',(-22.5384210474532,26.6100531124611,-48.0621645799476));
#19265=CARTESIAN_POINT('Ctrl Pts',(-22.4801258946871,26.5906138577146,-48.0659628676603));
#19266=CARTESIAN_POINT('Ctrl Pts',(-22.4299081919831,26.5724696019742,-48.0693043348848));
#19267=CARTESIAN_POINT('Ctrl Pts',(-22.276123752642,26.5125458903103,-48.0797624180011));
#19268=CARTESIAN_POINT('Ctrl Pts',(-22.1742777374574,26.466632238947,-48.0870135425246));
#19269=CARTESIAN_POINT('Ctrl Pts',(-22.0750360039475,26.4155367686876,-48.0944001480293));
#19270=CARTESIAN_POINT('',(-26.773002855424,23.551903308829,-47.9332000262529));
#19271=CARTESIAN_POINT('Ctrl Pts',(-22.0750360153631,26.415536774565,-48.3398410585546));
#19272=CARTESIAN_POINT('Ctrl Pts',(-22.1133942443118,26.4352858424012,-48.3372333295926));
#19273=CARTESIAN_POINT('Ctrl Pts',(-22.1521475496805,26.4542638705128,-48.3346679043009));
#19274=CARTESIAN_POINT('Ctrl Pts',(-22.2912003786824,26.5189307592828,-48.3256653736361));
#19275=CARTESIAN_POINT('Ctrl Pts',(-22.3934539284286,26.5602497666329,-48.3194121678932));
#19276=CARTESIAN_POINT('Ctrl Pts',(-22.7224336130672,26.6739370652559,-48.2998564456631));
#19277=CARTESIAN_POINT('Ctrl Pts',(-22.9551302316336,26.7264945517448,-48.2867810556429));
#19278=CARTESIAN_POINT('Ctrl Pts',(-23.2852817073651,26.7634776295853,-48.2674063904904));
#19279=CARTESIAN_POINT('Ctrl Pts',(-23.379482822315,26.76985811539,-48.261795893775));
#19280=CARTESIAN_POINT('Ctrl Pts',(-23.4840874515198,26.7723396174469,-48.2554265425794));
#19281=CARTESIAN_POINT('Ctrl Pts',(-23.4943541427971,26.7725340793388,-48.2547999453092));
#19282=CARTESIAN_POINT('Ctrl Pts',(-23.5087452916319,26.7727378645741,-48.253919522527));
#19283=CARTESIAN_POINT('Ctrl Pts',(-23.5128691806755,26.7727883431962,-48.2536669891383));
#19284=CARTESIAN_POINT('Ctrl Pts',(-23.5204200254212,26.772866273498,-48.2532041532776));
#19285=CARTESIAN_POINT('Ctrl Pts',(-23.5238469547929,26.7728961751435,-48.2529939279742));
#19286=CARTESIAN_POINT('Ctrl Pts',(-23.5307768025355,26.7729455870931,-48.2525684723367));
#19287=CARTESIAN_POINT('Ctrl Pts',(-23.5342797170267,26.7729648524544,-48.2523532346309));
#19288=CARTESIAN_POINT('Ctrl Pts',(-23.5428760226446,26.7729981146558,-48.2518245930969));
#19289=CARTESIAN_POINT('Ctrl Pts',(-23.5479694163242,26.7730057478577,-48.2515109898842));
#19290=CARTESIAN_POINT('Ctrl Pts',(-23.5663893694442,26.772989685574,-48.250375481382));
#19291=CARTESIAN_POINT('Ctrl Pts',(-23.5797155911597,26.7728954036369,-48.2495513634195));
#19292=CARTESIAN_POINT('Ctrl Pts',(-23.7695191525022,26.7703751771359,-48.2377754074615));
#19293=CARTESIAN_POINT('Ctrl Pts',(-23.9454755922586,26.7535395313318,-48.2263629673671));
#19294=CARTESIAN_POINT('Ctrl Pts',(-24.1512149335226,26.7166421605112,-48.2124535675206));
#19295=CARTESIAN_POINT('Ctrl Pts',(-24.1831947318097,26.7104049308991,-48.2102758769589));
#19296=CARTESIAN_POINT('Ctrl Pts',(-24.2411755921231,26.698181131087,-48.2063014122114));
#19297=CARTESIAN_POINT('Ctrl Pts',(-24.2672076602134,26.6923544484336,-48.204507284416));
#19298=CARTESIAN_POINT('Ctrl Pts',(-24.3151279530915,26.681002064407,-48.2011882960618));
#19299=CARTESIAN_POINT('Ctrl Pts',(-24.3370363844787,26.675568228242,-48.1996645572802));
#19300=CARTESIAN_POINT('Ctrl Pts',(-24.3777623792751,26.6650117970623,-48.1968213261261));
#19301=CARTESIAN_POINT('Ctrl Pts',(-24.3965941155757,26.6599476530509,-48.1955023086766));
#19302=CARTESIAN_POINT('Ctrl Pts',(-24.4318514204217,26.6501224299345,-48.1930255314741));
#19303=CARTESIAN_POINT('Ctrl Pts',(-24.4482873601915,26.6454009017314,-48.1918679414845));
#19304=CARTESIAN_POINT('Ctrl Pts',(-24.6150317997973,26.5960604809965,-48.180096883176));
#19305=CARTESIAN_POINT('Ctrl Pts',(-24.7619432714318,26.5406561780747,-48.1694888837999));
#19306=CARTESIAN_POINT('Ctrl Pts',(-24.9096095988687,26.472289638636,-48.1589184976846));
#19307=CARTESIAN_POINT('Ctrl Pts',(-24.9149658794914,26.469791873744,-48.1585352252729));
#19308=CARTESIAN_POINT('Ctrl Pts',(-24.9217285067946,26.4666156177921,-48.1580515320269));
#19309=CARTESIAN_POINT('Ctrl Pts',(-24.9231412371491,26.4659508361634,-48.157950498936));
#19310=CARTESIAN_POINT('Ctrl Pts',(-24.9288541317922,26.4632574745711,-48.157541983339));
#19311=CARTESIAN_POINT('Ctrl Pts',(-24.9331503104697,26.4612203953117,-48.157234885785));
#19312=CARTESIAN_POINT('Ctrl Pts',(-24.9398048549327,26.4580470148486,-48.1567593997401));
#19313=CARTESIAN_POINT('Ctrl Pts',(-24.9421663533241,26.4569173435582,-48.156590701407));
#19314=CARTESIAN_POINT('Ctrl Pts',(-24.9800311540979,26.4387472113551,-48.1538863846729));
#19315=CARTESIAN_POINT('Ctrl Pts',(-25.0152226025531,26.4210592938839,-48.1513818747014));
#19316=CARTESIAN_POINT('Ctrl Pts',(-25.054309184869,26.400507598537,-48.1486175224203));
#19317=CARTESIAN_POINT('Ctrl Pts',(-25.0585305551473,26.3982760159177,-48.1483192011688));
#19318=CARTESIAN_POINT('Ctrl Pts',(-25.0648759791946,26.3949035098945,-48.1478711392579));
#19319=CARTESIAN_POINT('Ctrl Pts',(-25.0670037141435,26.3937695838896,-48.1477209578917));
#19320=CARTESIAN_POINT('Ctrl Pts',(-25.0706846385711,26.3918026152214,-48.147461257962));
#19321=CARTESIAN_POINT('Ctrl Pts',(-25.0722384168639,26.3909706863505,-48.1473516683002));
#19322=CARTESIAN_POINT('Ctrl Pts',(-25.0753585539365,26.3892967979527,-48.1471316710419));
#19323=CARTESIAN_POINT('Ctrl Pts',(-25.0769248960658,26.3884548177782,-48.1470212653897));
#19324=CARTESIAN_POINT('Ctrl Pts',(-25.0806810019198,26.386431730913,-48.1467565944215));
#19325=CARTESIAN_POINT('Ctrl Pts',(-25.0828701024732,26.3852493807927,-48.146602408932));
#19326=CARTESIAN_POINT('Ctrl Pts',(-25.0898268162673,26.3814815932993,-48.1461126333047));
#19327=CARTESIAN_POINT('Ctrl Pts',(-25.0945893055481,26.3788866379254,-48.1457776499571));
#19328=CARTESIAN_POINT('Ctrl Pts',(-25.1056920959117,26.3728006199492,-48.1449973781955));
#19329=CARTESIAN_POINT('Ctrl Pts',(-25.1120272619395,26.3693001798807,-48.1445526767075));
#19330=CARTESIAN_POINT('Ctrl Pts',(-25.1336229717801,26.3572725183588,-48.1430383278276));
#19331=CARTESIAN_POINT('Ctrl Pts',(-25.1488262148281,26.348642312683,-48.1419749348479));
#19332=CARTESIAN_POINT('Ctrl Pts',(-25.194326439302,26.3223220335867,-48.1387982552431));
#19333=CARTESIAN_POINT('Ctrl Pts',(-25.224406470546,26.3042600004006,-48.136706017134));
#19334=CARTESIAN_POINT('Ctrl Pts',(-25.3103737040802,26.2507104426311,-48.1307315603854));
#19335=CARTESIAN_POINT('Ctrl Pts',(-25.3654721946375,26.2139863849008,-48.1269085437208));
#19336=CARTESIAN_POINT('Ctrl Pts',(-25.6618849634079,26.0029505404372,-48.1061550237849));
#19337=CARTESIAN_POINT('Ctrl Pts',(-25.8792748305835,25.7975586816019,-48.0900853051901));
#19338=CARTESIAN_POINT('Ctrl Pts',(-26.0788632534354,25.5484290540982,-48.0714083003768));
#19339=CARTESIAN_POINT('Ctrl Pts',(-26.0921626853434,25.5314830426917,-48.070142252939));
#19340=CARTESIAN_POINT('Ctrl Pts',(-26.108322415936,25.5104619003947,-48.0685763492666));
#19341=CARTESIAN_POINT('Ctrl Pts',(-26.1113446651781,25.5065115598479,-48.0682822790734));
#19342=CARTESIAN_POINT('Ctrl Pts',(-26.1167668782265,25.4993901581752,-48.0677524926499));
#19343=CARTESIAN_POINT('Ctrl Pts',(-26.1191701443562,25.4962216160007,-48.0675168951757));
#19344=CARTESIAN_POINT('Ctrl Pts',(-26.1294738546591,25.482584526293,-48.0665034143078));
#19345=CARTESIAN_POINT('Ctrl Pts',(-26.1373161421172,25.4720723563789,-48.0657234521109));
#19346=CARTESIAN_POINT('Ctrl Pts',(-26.1461884690007,25.4600267534124,-48.0648310339839));
#19347=CARTESIAN_POINT('Ctrl Pts',(-26.1472816963462,25.4585398492817,-48.0647208970747));
#19348=CARTESIAN_POINT('Ctrl Pts',(-26.1525565411491,25.4513525777255,-48.0641886351589));
#19349=CARTESIAN_POINT('Ctrl Pts',(-26.1567206480046,25.4456394315469,-48.0637658708803));
#19350=CARTESIAN_POINT('Ctrl Pts',(-26.1642500206985,25.4352374123322,-48.0629967026498));
#19351=CARTESIAN_POINT('Ctrl Pts',(-26.1676215613572,25.4305531019943,-48.0626505324834));
#19352=CARTESIAN_POINT('Ctrl Pts',(-26.1784869921047,25.4153711719485,-48.06152922832));
#19353=CARTESIAN_POINT('Ctrl Pts',(-26.1859303821194,25.4048377097258,-48.0607522343565));
#19354=CARTESIAN_POINT('Ctrl Pts',(-26.2057522503595,25.3764265758463,-48.058658884286));
#19355=CARTESIAN_POINT('Ctrl Pts',(-26.2180131885803,25.3584680711016,-48.0573381933167));
#19356=CARTESIAN_POINT('Ctrl Pts',(-26.2336533160652,25.3350547382627,-48.0556190503393));
#19357=CARTESIAN_POINT('Ctrl Pts',(-26.2371994610022,25.3297116866843,-48.0552269132274));
#19358=CARTESIAN_POINT('Ctrl Pts',(-26.2428178371051,25.3211912737644,-48.05460185606));
#19359=CARTESIAN_POINT('Ctrl Pts',(-26.2449004592589,25.3180207569838,-48.0543693269339));
#19360=CARTESIAN_POINT('Ctrl Pts',(-26.2486291864632,25.3123223632662,-48.0539515047257));
#19361=CARTESIAN_POINT('Ctrl Pts',(-26.2502773517209,25.309795834224,-48.0537662891761));
#19362=CARTESIAN_POINT('Ctrl Pts',(-26.2541181731114,25.3038900036703,-48.0533334262539));
#19363=CARTESIAN_POINT('Ctrl Pts',(-26.2563080418871,25.3005089030515,-48.053085674987));
#19364=CARTESIAN_POINT('Ctrl Pts',(-26.2625471595148,25.2908361681732,-48.0523770781844));
#19365=CARTESIAN_POINT('Ctrl Pts',(-26.2665808251406,25.2845345573154,-48.0519156524887));
#19366=CARTESIAN_POINT('Ctrl Pts',(-26.2921831911561,25.2442287178093,-48.0489655946774));
#19367=CARTESIAN_POINT('Ctrl Pts',(-26.3131341121019,25.209838081078,-48.0464541871503));
#19368=CARTESIAN_POINT('Ctrl Pts',(-26.3734950587642,25.1064443151658,-48.0389164477733));
#19369=CARTESIAN_POINT('Ctrl Pts',(-26.4110010984762,25.0363706689073,-48.03382348974));
#19370=CARTESIAN_POINT('Ctrl Pts',(-26.5847859626775,24.6806745161146,-48.0080431472434));
#19371=CARTESIAN_POINT('Ctrl Pts',(-26.681040065905,24.3775157549382,-47.9860698081352));
#19372=CARTESIAN_POINT('Ctrl Pts',(-26.7335359402297,24.0532161792036,-47.9644604240851));
#19373=CARTESIAN_POINT('Ctrl Pts',(-26.7354127113856,24.0411907425774,-47.9636620766814));
#19374=CARTESIAN_POINT('Ctrl Pts',(-26.7394487850028,24.0143317335835,-47.9618859432923));
#19375=CARTESIAN_POINT('Ctrl Pts',(-26.741572827519,23.9994930379943,-47.9609094352365));
#19376=CARTESIAN_POINT('Ctrl Pts',(-26.74395815269,23.981957634892,-47.9597614617846));
#19377=CARTESIAN_POINT('Ctrl Pts',(-26.7443196289926,23.9792749877021,-47.9595860050774));
#19378=CARTESIAN_POINT('Ctrl Pts',(-26.7455076698001,23.9703733756249,-47.9590043572596));
#19379=CARTESIAN_POINT('Ctrl Pts',(-26.7463194600648,23.9641524129433,-47.9585987681337));
#19380=CARTESIAN_POINT('Ctrl Pts',(-26.7472810592437,23.9566118797392,-47.9581082679169));
#19381=CARTESIAN_POINT('Ctrl Pts',(-26.7474482190151,23.9552945822239,-47.9580226211536));
#19382=CARTESIAN_POINT('Ctrl Pts',(-26.7481713292853,23.9495677945834,-47.9576504636398));
#19383=CARTESIAN_POINT('Ctrl Pts',(-26.7487189750331,23.9451572372253,-47.9573643087123));
#19384=CARTESIAN_POINT('Ctrl Pts',(-26.7537587620555,23.9038701884394,-47.9546900778334));
#19385=CARTESIAN_POINT('Ctrl Pts',(-26.7576223344678,23.8669177490666,-47.9523298281324));
#19386=CARTESIAN_POINT('Ctrl Pts',(-26.761293094546,23.8247749920161,-47.9496820704458));
#19387=CARTESIAN_POINT('Ctrl Pts',(-26.7617276281419,23.8196440372644,-47.949360442931));
#19388=CARTESIAN_POINT('Ctrl Pts',(-26.7623510857833,23.8120663266482,-47.9488865605085));
#19389=CARTESIAN_POINT('Ctrl Pts',(-26.762549513094,23.8096203936125,-47.9487337725244));
#19390=CARTESIAN_POINT('Ctrl Pts',(-26.7628955735838,23.8052933290219,-47.9484637841957));
#19391=CARTESIAN_POINT('Ctrl Pts',(-26.7630443485005,23.8034122931889,-47.9483465190307));
#19392=CARTESIAN_POINT('Ctrl Pts',(-26.7633276815207,23.7997894946098,-47.9481208695808));
#19393=CARTESIAN_POINT('Ctrl Pts',(-26.76346247498,23.7980477590446,-47.9480124720665));
#19394=CARTESIAN_POINT('Ctrl Pts',(-26.7637497412047,23.7942961950074,-47.9477791803535));
#19395=CARTESIAN_POINT('Ctrl Pts',(-26.7639017449384,23.7922863297547,-47.9476543128028));
#19396=CARTESIAN_POINT('Ctrl Pts',(-26.7642646995405,23.7874265478035,-47.9473526658659));
#19397=CARTESIAN_POINT('Ctrl Pts',(-26.7644737459934,23.7845764841183,-47.9471759936231));
#19398=CARTESIAN_POINT('Ctrl Pts',(-26.7650297785464,23.7768549739956,-47.9466979635083));
#19399=CARTESIAN_POINT('Ctrl Pts',(-26.7653694844485,23.7719829864772,-47.9463970099636));
#19400=CARTESIAN_POINT('Ctrl Pts',(-26.7705290319652,23.6954800720143,-47.9416814422417));
#19401=CARTESIAN_POINT('Ctrl Pts',(-26.7729654280244,23.6237028739272,-47.9373972869849));
#19402=CARTESIAN_POINT('Ctrl Pts',(-26.7730021111297,23.5518989666397,-47.9331984791512));
#19403=CARTESIAN_POINT('Ctrl Pts',(-26.7730021088701,23.5519033837932,-47.9331987374489));
#19404=CARTESIAN_POINT('Ctrl Pts',(-26.773147384322,23.2683005089752,-47.9166147515683));
#19405=CARTESIAN_POINT('Ctrl Pts',(-26.7358584101289,22.9858792144759,-47.9013537634378));
#19406=CARTESIAN_POINT('Ctrl Pts',(-26.6262836614549,22.5791349749879,-47.8773094696323));
#19407=CARTESIAN_POINT('Ctrl Pts',(-26.582043218141,22.448764920814,-47.8692848252479));
#19408=CARTESIAN_POINT('Ctrl Pts',(-26.5213570636572,22.3016033990152,-47.859662947226));
#19409=CARTESIAN_POINT('Ctrl Pts',(-26.5128973020304,22.2816616892274,-47.8583469239738));
#19410=CARTESIAN_POINT('Ctrl Pts',(-26.5017872252828,22.2561899090499,-47.8566497696991));
#19411=CARTESIAN_POINT('Ctrl Pts',(-26.4993211388889,22.2505797005474,-47.8562749545605));
#19412=CARTESIAN_POINT('Ctrl Pts',(-26.4953284812921,22.241566502041,-47.8556711422199));
#19413=CARTESIAN_POINT('Ctrl Pts',(-26.4938119701412,22.2381590497909,-47.8554424908258));
#19414=CARTESIAN_POINT('Ctrl Pts',(-26.4909169383517,22.2316844760013,-47.8550073003305));
#19415=CARTESIAN_POINT('Ctrl Pts',(-26.489539524762,22.228616862411,-47.8548007995544));
#19416=CARTESIAN_POINT('Ctrl Pts',(-26.4863948391397,22.2216426198048,-47.8543306095999));
#19417=CARTESIAN_POINT('Ctrl Pts',(-26.4846245693555,22.2177373566026,-47.8540668173341));
#19418=CARTESIAN_POINT('Ctrl Pts',(-26.4792262008718,22.2058913351981,-47.8532650958377));
#19419=CARTESIAN_POINT('Ctrl Pts',(-26.4755736461966,22.1979618247744,-47.8527263225446));
#19420=CARTESIAN_POINT('Ctrl Pts',(-26.4495652081416,22.1420973134583,-47.8489154970363));
#19421=CARTESIAN_POINT('Ctrl Pts',(-26.4260655786542,22.0947066216884,-47.8456038840066));
#19422=CARTESIAN_POINT('Ctrl Pts',(-26.3998480786388,22.0449505585624,-47.8420392979006));
#19423=CARTESIAN_POINT('Ctrl Pts',(-26.3982799565857,22.0419857786257,-47.8418265623427));
#19424=CARTESIAN_POINT('Ctrl Pts',(-26.3947903095413,22.035412902044,-47.8413541857304));
#19425=CARTESIAN_POINT('Ctrl Pts',(-26.3928665442558,22.0318060069521,-47.8410944679094));
#19426=CARTESIAN_POINT('Ctrl Pts',(-26.3885465894806,22.0237434426945,-47.840512796437));
#19427=CARTESIAN_POINT('Ctrl Pts',(-26.3861467639681,22.0192897430682,-47.8401907187037));
#19428=CARTESIAN_POINT('Ctrl Pts',(-26.3743889621559,21.9975916133996,-47.8386178278566));
#19429=CARTESIAN_POINT('Ctrl Pts',(-26.364884285639,21.9804275197131,-47.8373620292444));
#19430=CARTESIAN_POINT('Ctrl Pts',(-26.2277658042201,21.7380599185687,-47.8194639378452));
#19431=CARTESIAN_POINT('Ctrl Pts',(-26.0736448719002,21.5289735842125,-47.8018702336454));
#19432=CARTESIAN_POINT('Ctrl Pts',(-25.8391703467169,21.2800328928449,-47.7787862027967));
#19433=CARTESIAN_POINT('Ctrl Pts',(-25.779788600825,21.2216881169396,-47.7732008949706));
#19434=CARTESIAN_POINT('Ctrl Pts',(-25.6741105274969,21.125608754104,-47.7637780041608));
#19435=CARTESIAN_POINT('Ctrl Pts',(-25.6289016523962,21.0867410047727,-47.7598961886213));
#19436=CARTESIAN_POINT('Ctrl Pts',(-25.5685190694999,21.0376744324307,-47.7549297632581));
#19437=CARTESIAN_POINT('Ctrl Pts',(-25.5543031504199,21.0263211389551,-47.7537757475303));
#19438=CARTESIAN_POINT('Ctrl Pts',(-25.53412788755,21.0104864606184,-47.7521602082924));
#19439=CARTESIAN_POINT('Ctrl Pts',(-25.5282482763929,21.005904686,-47.7516920278819));
#19440=CARTESIAN_POINT('Ctrl Pts',(-25.5179666463049,20.9979497518961,-47.7508779790647));
#19441=CARTESIAN_POINT('Ctrl Pts',(-25.5135717475837,20.9945675013716,-47.7505314859176));
#19442=CARTESIAN_POINT('Ctrl Pts',(-25.5071705319801,20.9896674752845,-47.7500289795794));
#19443=CARTESIAN_POINT('Ctrl Pts',(-25.505171164584,20.9881407016143,-47.749872331625));
#19444=CARTESIAN_POINT('Ctrl Pts',(-25.5017598987094,20.9855420799565,-47.7496055869691));
#19445=CARTESIAN_POINT('Ctrl Pts',(-25.5003489022511,20.984469054788,-47.74949540625));
#19446=CARTESIAN_POINT('Ctrl Pts',(-25.4975402522987,20.9823368066288,-47.7492763909243));
#19447=CARTESIAN_POINT('Ctrl Pts',(-25.4961426210979,20.9812775614284,-47.7491675546778));
#19448=CARTESIAN_POINT('Ctrl Pts',(-25.4928488015731,20.9787854517268,-47.7489114085107));
#19449=CARTESIAN_POINT('Ctrl Pts',(-25.4909518882989,20.9773535405826,-47.748764166452));
#19450=CARTESIAN_POINT('Ctrl Pts',(-25.4853464607215,20.9731319323172,-47.7483298612345));
#19451=CARTESIAN_POINT('Ctrl Pts',(-25.4816334826611,20.9703481302152,-47.7480432125426));
#19452=CARTESIAN_POINT('Ctrl Pts',(-25.4493301613815,20.9462375634959,-47.7455581500931));
#19453=CARTESIAN_POINT('Ctrl Pts',(-25.4203921673918,20.9253777156906,-47.7433918184966));
#19454=CARTESIAN_POINT('Ctrl Pts',(-25.2997221307899,20.8414020829198,-47.7345750696422));
#19455=CARTESIAN_POINT('Ctrl Pts',(-25.2050879245994,20.7825749230887,-47.7281658391023));
#19456=CARTESIAN_POINT('Ctrl Pts',(-25.0461163003156,20.6948297287179,-47.7178829268279));
#19457=CARTESIAN_POINT('Ctrl Pts',(-24.9835492510793,20.6629166089733,-47.7139505090426));
#19458=CARTESIAN_POINT('Ctrl Pts',(-24.7898331283247,20.5719589317981,-47.7019862929217));
#19459=CARTESIAN_POINT('Ctrl Pts',(-24.6557365507812,20.519626234304,-47.6939829554487));
#19460=CARTESIAN_POINT('Ctrl Pts',(-24.4183861315362,20.4448538564775,-47.6797652406158));
#19461=CARTESIAN_POINT('Ctrl Pts',(-24.3166975432183,20.4182059424897,-47.6736601753268));
#19462=CARTESIAN_POINT('Ctrl Pts',(-24.1668448498245,20.3866717629485,-47.6645308130075));
#19463=CARTESIAN_POINT('Ctrl Pts',(-24.1195804874036,20.3778252799413,-47.6616329994601));
#19464=CARTESIAN_POINT('Ctrl Pts',(-24.0643902763561,20.3687683525638,-47.6582223505244));
#19465=CARTESIAN_POINT('Ctrl Pts',(-24.056638220856,20.3675252837769,-47.6577426777728));
#19466=CARTESIAN_POINT('Ctrl Pts',(-24.0448243097055,20.3656751365731,-47.6570107150606));
#19467=CARTESIAN_POINT('Ctrl Pts',(-24.0407656693459,20.3650474691173,-47.6567590795747));
#19468=CARTESIAN_POINT('Ctrl Pts',(-24.0333982579434,20.3639225166175,-47.6563019852268));
#19469=CARTESIAN_POINT('Ctrl Pts',(-24.0300898862017,20.3634226223867,-47.6560966095309));
#19470=CARTESIAN_POINT('Ctrl Pts',(-24.0229757090799,20.3623590011573,-47.6556547283608));
#19471=CARTESIAN_POINT('Ctrl Pts',(-24.0191696638895,20.3617969357347,-47.6554181704878));
#19472=CARTESIAN_POINT('Ctrl Pts',(-24.0089444579914,20.3603056123116,-47.654782223324));
#19473=CARTESIAN_POINT('Ctrl Pts',(-24.0025235081615,20.3593889190355,-47.6543824361515));
#19474=CARTESIAN_POINT('Ctrl Pts',(-23.9732237069118,20.3552961192214,-47.6525560925661));
#19475=CARTESIAN_POINT('Ctrl Pts',(-23.9503143445909,20.3523467179206,-47.6511223738493));
#19476=CARTESIAN_POINT('Ctrl Pts',(-23.9152659260728,20.3482170122614,-47.6489197979172));
#19477=CARTESIAN_POINT('Ctrl Pts',(-23.9031482605978,20.3468588868687,-47.6481566090561));
#19478=CARTESIAN_POINT('Ctrl Pts',(-23.8788217511065,20.3442721212665,-47.6466210754421));
#19479=CARTESIAN_POINT('Ctrl Pts',(-23.8666130175699,20.3430443750156,-47.6458487160998));
#19480=CARTESIAN_POINT('Ctrl Pts',(-23.8510702808225,20.3415709620217,-47.644863214139));
#19481=CARTESIAN_POINT('Ctrl Pts',(-23.8477423783294,20.341260707965,-47.6446520757404));
#19482=CARTESIAN_POINT('Ctrl Pts',(-23.8335008782966,20.3399553439481,-47.6437479690377));
#19483=CARTESIAN_POINT('Ctrl Pts',(-23.8225828253953,20.3390107367021,-47.6430534499218));
#19484=CARTESIAN_POINT('Ctrl Pts',(-23.8076952315126,20.3377991632403,-47.6421044980782));
#19485=CARTESIAN_POINT('Ctrl Pts',(-23.8037296096592,20.3374838255932,-47.6418515391843));
#19486=CARTESIAN_POINT('Ctrl Pts',(-23.7946895221739,20.3367818192163,-47.6412744661729));
#19487=CARTESIAN_POINT('Ctrl Pts',(-23.7896147131363,20.3363998269343,-47.6409502116259));
#19488=CARTESIAN_POINT('Ctrl Pts',(-23.7632589618185,20.3344787412873,-47.6392646270525));
#19489=CARTESIAN_POINT('Ctrl Pts',(-23.7419644096619,20.3331390223145,-47.6378973594693));
#19490=CARTESIAN_POINT('Ctrl Pts',(-23.4642851162601,20.3184358962199,-47.6199980997976));
#19491=CARTESIAN_POINT('Ctrl Pts',(-23.2072392968542,20.3355471056643,-47.6025395323643));
#19492=CARTESIAN_POINT('Ctrl Pts',(-22.8736050059555,20.3982492060126,-47.5796290440575));
#19493=CARTESIAN_POINT('Ctrl Pts',(-22.7928249908994,20.4166792186849,-47.5740721003254));
#19494=CARTESIAN_POINT('Ctrl Pts',(-22.6635282575336,20.4514712437436,-47.5652424360716));
#19495=CARTESIAN_POINT('Ctrl Pts',(-22.6145347271709,20.4659117267404,-47.5619122901724));
#19496=CARTESIAN_POINT('Ctrl Pts',(-22.5578451162316,20.4840958683256,-47.5580930847178));
#19497=CARTESIAN_POINT('Ctrl Pts',(-22.5497979164179,20.4867121404687,-47.5575517513844));
#19498=CARTESIAN_POINT('Ctrl Pts',(-22.5250865709336,20.4948539431376,-47.5558921163806));
#19499=CARTESIAN_POINT('Ctrl Pts',(-22.5084568578154,20.5004840834936,-47.5547790230891));
#19500=CARTESIAN_POINT('Ctrl Pts',(-22.4850155692696,20.5086344599768,-47.5532161728546));
#19501=CARTESIAN_POINT('Ctrl Pts',(-22.4781655754629,20.5110421340786,-47.5527602266676));
#19502=CARTESIAN_POINT('Ctrl Pts',(-22.4677493800631,20.5147428747101,-47.5520681130539));
#19503=CARTESIAN_POINT('Ctrl Pts',(-22.4641772832026,20.5160191019961,-47.5518309780003));
#19504=CARTESIAN_POINT('Ctrl Pts',(-22.4575852424116,20.5183874176202,-47.5513937732603));
#19505=CARTESIAN_POINT('Ctrl Pts',(-22.4545646672882,20.519477716731,-47.5511935986982));
#19506=CARTESIAN_POINT('Ctrl Pts',(-22.4496529605139,20.5212589364434,-47.5508683636008));
#19507=CARTESIAN_POINT('Ctrl Pts',(-22.4477608472288,20.521947114156,-47.5507431390005));
#19508=CARTESIAN_POINT('Ctrl Pts',(-22.4440982350716,20.523283125029,-47.5505008645502));
#19509=CARTESIAN_POINT('Ctrl Pts',(-22.4423276650325,20.5239307367307,-47.5503838022071));
#19510=CARTESIAN_POINT('Ctrl Pts',(-22.4382637215367,20.5254212275451,-47.5501152420184));
#19511=CARTESIAN_POINT('Ctrl Pts',(-22.4359707322665,20.5262651633285,-47.5499638079247));
#19512=CARTESIAN_POINT('Ctrl Pts',(-22.4287207571431,20.5289428859385,-47.5494852974449));
#19513=CARTESIAN_POINT('Ctrl Pts',(-22.4237672888319,20.5307862716709,-47.5491587952589));
#19514=CARTESIAN_POINT('Ctrl Pts',(-22.3823780507819,20.5463049068447,-47.546434134649));
#19515=CARTESIAN_POINT('Ctrl Pts',(-22.3461862368394,20.5606276679563,-47.5440740927625));
#19516=CARTESIAN_POINT('Ctrl Pts',(-22.3075094257139,20.5767502161452,-47.5415672390349));
#19517=CARTESIAN_POINT('Ctrl Pts',(-22.3047596255157,20.5779009594828,-47.5413890932151));
#19518=CARTESIAN_POINT('Ctrl Pts',(-22.3003102247923,20.5797702145015,-47.5411009681085));
#19519=CARTESIAN_POINT('Ctrl Pts',(-22.2986096441706,20.5804863709535,-47.5409908760492));
#19520=CARTESIAN_POINT('Ctrl Pts',(-22.2942984664424,20.5823062751178,-47.5407118547799));
#19521=CARTESIAN_POINT('Ctrl Pts',(-22.2916887035257,20.5834120091039,-47.5405430200048));
#19522=CARTESIAN_POINT('Ctrl Pts',(-22.2879081636193,20.5850196771776,-47.5402985406211));
#19523=CARTESIAN_POINT('Ctrl Pts',(-22.2867362272803,20.5855188617662,-47.5402227675557));
#19524=CARTESIAN_POINT('Ctrl Pts',(-22.2829853165945,20.5871191847731,-47.5399802899592));
#19525=CARTESIAN_POINT('Ctrl Pts',(-22.2804074766501,20.58822299734,-47.5398137097176));
#19526=CARTESIAN_POINT('Ctrl Pts',(-22.2714029370305,20.5920925920377,-47.5392320491054));
#19527=CARTESIAN_POINT('Ctrl Pts',(-22.2649837635269,20.5948759550989,-47.5388177742811));
#19528=CARTESIAN_POINT('Ctrl Pts',(-22.25411481255,20.5996308579175,-47.5381168871319));
#19529=CARTESIAN_POINT('Ctrl Pts',(-22.2496603713128,20.6015916014402,-47.5378298023229));
#19530=CARTESIAN_POINT('Ctrl Pts',(-22.1133485377821,20.661961944064,-47.5290490600604));
#19531=CARTESIAN_POINT('Ctrl Pts',(-21.9855429453391,20.7291522116693,-47.5209385986133));
#19532=CARTESIAN_POINT('Ctrl Pts',(-21.7396013084066,20.8803229213432,-47.5047864451248));
#19533=CARTESIAN_POINT('Ctrl Pts',(-21.6217699271547,20.9641482832484,-47.4967608580446));
#19534=CARTESIAN_POINT('Ctrl Pts',(-21.4339337403402,21.1177724859014,-47.4829393962682));
#19535=CARTESIAN_POINT('Ctrl Pts',(-21.3607929085943,21.1833920442899,-47.4772613696336));
#19536=CARTESIAN_POINT('Ctrl Pts',(-21.2453553155002,21.2968945635193,-47.4676821147604));
#19537=CARTESIAN_POINT('Ctrl Pts',(-21.2012805010894,21.3428778811891,-47.4638606566956));
#19538=CARTESIAN_POINT('Ctrl Pts',(-21.152967734335,21.3963691211557,-47.4594669750718));
#19539=CARTESIAN_POINT('Ctrl Pts',(-21.1473609649096,21.4026258737268,-47.4589538371114));
#19540=CARTESIAN_POINT('Ctrl Pts',(-21.1389740218879,21.4120590584778,-47.4581813274228));
#19541=CARTESIAN_POINT('Ctrl Pts',(-21.1361754887756,21.4152191803518,-47.4579227269247));
#19542=CARTESIAN_POINT('Ctrl Pts',(-21.1313724533557,21.4206643159967,-47.4574774612566));
#19543=CARTESIAN_POINT('Ctrl Pts',(-21.1293649554274,21.4229466898387,-47.4572909216856));
#19544=CARTESIAN_POINT('Ctrl Pts',(-21.1252366930217,21.4276536244933,-47.4569064197081));
#19545=CARTESIAN_POINT('Ctrl Pts',(-21.1231163291163,21.4300785311292,-47.4567084408764));
#19546=CARTESIAN_POINT('Ctrl Pts',(-21.1180194887726,21.435925084362,-47.4562313625064));
#19547=CARTESIAN_POINT('Ctrl Pts',(-21.1150465981124,21.4393498360819,-47.4559521142895));
#19548=CARTESIAN_POINT('Ctrl Pts',(-21.1059418664999,21.4498832624002,-47.4550938762961));
#19549=CARTESIAN_POINT('Ctrl Pts',(-21.0998338913293,21.4570124166249,-47.4545139002819));
#19550=CARTESIAN_POINT('Ctrl Pts',(-21.0774218033451,21.4834040566216,-47.4523700556633));
#19551=CARTESIAN_POINT('Ctrl Pts',(-21.0613132995523,21.5028307700093,-47.4507981972706));
#19552=CARTESIAN_POINT('Ctrl Pts',(-21.0416350287371,21.5271380372149,-47.4488386269224));
#19553=CARTESIAN_POINT('Ctrl Pts',(-21.0378483123344,21.5318424961323,-47.4484596986602));
#19554=CARTESIAN_POINT('Ctrl Pts',(-21.0297848657579,21.5419180360483,-47.4476488423562));
#19555=CARTESIAN_POINT('Ctrl Pts',(-21.0255120372625,21.5472921885936,-47.4472167619492));
#19556=CARTESIAN_POINT('Ctrl Pts',(-21.0203333791398,21.553848549086,-47.4466901351038));
#19557=CARTESIAN_POINT('Ctrl Pts',(-21.0194111286095,21.5550178155127,-47.4465962354542));
#19558=CARTESIAN_POINT('Ctrl Pts',(-21.0145738899807,21.5611594117836,-47.4461031270948));
#19559=CARTESIAN_POINT('Ctrl Pts',(-21.0106727655152,21.5661425992519,-47.4457033762698));
#19560=CARTESIAN_POINT('Ctrl Pts',(-21.000985667636,21.5785920030382,-47.4447055463073));
#19561=CARTESIAN_POINT('Ctrl Pts',(-20.9952178211088,21.5860721914201,-47.4441067698283));
#19562=CARTESIAN_POINT('Ctrl Pts',(-20.9841192101113,21.600597335083,-47.4429455194635));
#19563=CARTESIAN_POINT('Ctrl Pts',(-20.9787843591245,21.6076390743095,-47.4423832083823));
#19564=CARTESIAN_POINT('Ctrl Pts',(-20.9608138784568,21.6315629555823,-47.4404749998625));
#19565=CARTESIAN_POINT('Ctrl Pts',(-20.9483152122752,21.6485468811345,-47.4391240342816));
#19566=CARTESIAN_POINT('Ctrl Pts',(-20.7611197931617,21.9082194234163,-47.4185241752362));
#19567=CARTESIAN_POINT('Ctrl Pts',(-20.6208849357184,22.1739241579009,-47.3979763336342));
#19568=CARTESIAN_POINT('Ctrl Pts',(-20.4903647942636,22.5351394379514,-47.372275639186));
#19569=CARTESIAN_POINT('Ctrl Pts',(-20.4646117882576,22.6163408430149,-47.3666459920126));
#19570=CARTESIAN_POINT('Ctrl Pts',(-20.4347231242829,22.7254047427757,-47.359357760525));
#19571=CARTESIAN_POINT('Ctrl Pts',(-20.4276925770921,22.7524324932346,-47.3575735649393));
#19572=CARTESIAN_POINT('Ctrl Pts',(-20.4185707794457,22.7894691595945,-47.3551616717672));
#19573=CARTESIAN_POINT('Ctrl Pts',(-20.4161747365096,22.7994008040699,-47.3545181316066));
#19574=CARTESIAN_POINT('Ctrl Pts',(-20.4127063995809,22.8140830235846,-47.3535716978841));
#19575=CARTESIAN_POINT('Ctrl Pts',(-20.4115976079334,22.8188247867374,-47.3532667955687));
#19576=CARTESIAN_POINT('Ctrl Pts',(-20.409612478466,22.8274018585581,-47.3527166688546));
#19577=CARTESIAN_POINT('Ctrl Pts',(-20.4087324105224,22.8312362813486,-47.3524712340588));
#19578=CARTESIAN_POINT('Ctrl Pts',(-20.407401470553,22.8370842294088,-47.3520976922816));
#19579=CARTESIAN_POINT('Ctrl Pts',(-20.4069455112797,22.8390965745571,-47.35196929216));
#19580=CARTESIAN_POINT('Ctrl Pts',(-20.4060892632535,22.8428924782776,-47.3517273553989));
#19581=CARTESIAN_POINT('Ctrl Pts',(-20.4056885605524,22.8446759339904,-47.351613795194));
#19582=CARTESIAN_POINT('Ctrl Pts',(-20.404814728027,22.8485807354448,-47.3513654020984));
#19583=CARTESIAN_POINT('Ctrl Pts',(-20.4043422279676,22.8507022137297,-47.3512306062464));
#19584=CARTESIAN_POINT('Ctrl Pts',(-20.4030604171187,22.8564849795576,-47.3508635984211));
#19585=CARTESIAN_POINT('Ctrl Pts',(-20.4022553462217,22.8601472186875,-47.3506316314891));
#19586=CARTESIAN_POINT('Ctrl Pts',(-20.3984307754859,22.87769101493,-47.3495225695694));
#19587=CARTESIAN_POINT('Ctrl Pts',(-20.3954966313154,22.891591311234,-47.3486503263737));
#19588=CARTESIAN_POINT('Ctrl Pts',(-20.3908096691602,22.9145455320387,-47.3472199539967));
#19589=CARTESIAN_POINT('Ctrl Pts',(-20.3890036621952,22.92358820317,-47.3466590200307));
#19590=CARTESIAN_POINT('Ctrl Pts',(-20.3862706125908,22.9375851026141,-47.3457945352758));
#19591=CARTESIAN_POINT('Ctrl Pts',(-20.3853163552575,22.9425338773559,-47.3454896135562));
#19592=CARTESIAN_POINT('Ctrl Pts',(-20.3836140037037,22.9514750322665,-47.3449399787979));
#19593=CARTESIAN_POINT('Ctrl Pts',(-20.3828618429396,22.9554666156502,-47.3446950664567));
#19594=CARTESIAN_POINT('Ctrl Pts',(-20.3707705677244,23.0203062505158,-47.3407240009115));
#19595=CARTESIAN_POINT('Ctrl Pts',(-20.3611784005086,23.0814713064166,-47.3370824303284));
#19596=CARTESIAN_POINT('Ctrl Pts',(-20.315695004104,23.4384058732049,-47.316240379338));
#19597=CARTESIAN_POINT('Ctrl Pts',(-20.3191924537592,23.7377371569682,-47.300249038256));
#19598=CARTESIAN_POINT('Ctrl Pts',(-20.3761110827618,24.1139501367766,-47.278288685536));
#19599=CARTESIAN_POINT('Ctrl Pts',(-20.3915861853837,24.195042587439,-47.2734522083116));
#19600=CARTESIAN_POINT('Ctrl Pts',(-20.4196857768931,24.3167139577483,-47.265986394354));
#19601=CARTESIAN_POINT('Ctrl Pts',(-20.4300283421045,24.3577870945927,-47.2634296329413));
#19602=CARTESIAN_POINT('Ctrl Pts',(-20.4431746155306,24.4059639147094,-47.2603836350048));
#19603=CARTESIAN_POINT('Ctrl Pts',(-20.4451981345848,24.413277640003,-47.2599199368838));
#19604=CARTESIAN_POINT('Ctrl Pts',(-20.4483415004261,24.4244847253398,-47.2592073993224));
#19605=CARTESIAN_POINT('Ctrl Pts',(-20.4494428983012,24.4283832688448,-47.2589591617686));
#19606=CARTESIAN_POINT('Ctrl Pts',(-20.4514665783504,24.4354950710643,-47.2585056398136));
#19607=CARTESIAN_POINT('Ctrl Pts',(-20.4523865162567,24.4387089956891,-47.2583004322183));
#19608=CARTESIAN_POINT('Ctrl Pts',(-20.454247639724,24.4451730424365,-47.2578871909914));
#19609=CARTESIAN_POINT('Ctrl Pts',(-20.4551889464292,24.4484231249994,-47.2576791536209));
#19610=CARTESIAN_POINT('Ctrl Pts',(-20.4578868470618,24.4576836564633,-47.2570856368946));
#19611=CARTESIAN_POINT('Ctrl Pts',(-20.4596558354621,24.4636904518863,-47.2566997522975));
#19612=CARTESIAN_POINT('Ctrl Pts',(-20.4672781945341,24.489297379722,-47.2550508420696));
#19613=CARTESIAN_POINT('Ctrl Pts',(-20.4733004950927,24.5088463578669,-47.2537822882406));
#19614=CARTESIAN_POINT('Ctrl Pts',(-20.5895740044897,24.8738929946832,-47.2299072153831));
#19615=CARTESIAN_POINT('Ctrl Pts',(-20.7571665682539,25.1983319541831,-47.2051008477312));
#19616=CARTESIAN_POINT('Ctrl Pts',(-21.0100123558617,25.5343566747527,-47.1768981366939));
#19617=CARTESIAN_POINT('Ctrl Pts',(-21.046175207795,25.57980587069,-47.1730320685999));
#19618=CARTESIAN_POINT('Ctrl Pts',(-21.127815212177,25.6769040113041,-47.164697268809));
#19619=CARTESIAN_POINT('Ctrl Pts',(-21.1737607447188,25.7281270701512,-47.160250876277));
#19620=CARTESIAN_POINT('Ctrl Pts',(-21.2263687238229,25.7831284974839,-47.1554576277512));
#19621=CARTESIAN_POINT('Ctrl Pts',(-21.2314410200714,25.7883955581977,-47.154998419822));
#19622=CARTESIAN_POINT('Ctrl Pts',(-21.2391853412541,25.7963826571953,-47.1543018317876));
#19623=CARTESIAN_POINT('Ctrl Pts',(-21.2418442977628,25.7991152498885,-47.1540634691045));
#19624=CARTESIAN_POINT('Ctrl Pts',(-21.2467611019674,25.8041503099204,-47.1536241969889));
#19625=CARTESIAN_POINT('Ctrl Pts',(-21.2490175638551,25.8064541150039,-47.1534231811015));
#19626=CARTESIAN_POINT('Ctrl Pts',(-21.2526906202971,25.8101929937142,-47.1530969135354));
#19627=CARTESIAN_POINT('Ctrl Pts',(-21.2541051033683,25.8116301242302,-47.1529714958614));
#19628=CARTESIAN_POINT('Ctrl Pts',(-21.2568439845844,25.8144076388309,-47.1527290884919));
#19629=CARTESIAN_POINT('Ctrl Pts',(-21.2581682054392,25.8157481848528,-47.1526120858858));
#19630=CARTESIAN_POINT('Ctrl Pts',(-21.261207624226,25.8188196812746,-47.1523439895658));
#19631=CARTESIAN_POINT('Ctrl Pts',(-21.2629236140808,25.820549852158,-47.1521929588693));
#19632=CARTESIAN_POINT('Ctrl Pts',(-21.2683433549751,25.8260019999951,-47.1517169825856));
#19633=CARTESIAN_POINT('Ctrl Pts',(-21.2720542649503,25.8297168967579,-47.1513926025711));
#19634=CARTESIAN_POINT('Ctrl Pts',(-21.3027145482172,25.8602604574713,-47.1487248529345));
#19635=CARTESIAN_POINT('Ctrl Pts',(-21.330129180086,25.8866207002085,-47.1464178565613));
#19636=CARTESIAN_POINT('Ctrl Pts',(-21.3607216682144,25.9150116933644,-47.1439192738293));
#19637=CARTESIAN_POINT('Ctrl Pts',(-21.3634422737156,25.9175277988921,-47.143697718868));
#19638=CARTESIAN_POINT('Ctrl Pts',(-21.3699530437738,25.9235283715593,-47.143169030346));
#19639=CARTESIAN_POINT('Ctrl Pts',(-21.3737472412924,25.9270084700771,-47.142862160856));
#19640=CARTESIAN_POINT('Ctrl Pts',(-21.3851203782429,25.9373900204001,-47.1419459221601));
#19641=CARTESIAN_POINT('Ctrl Pts',(-21.3927239866929,25.9442644811945,-47.1413381300067));
#19642=CARTESIAN_POINT('Ctrl Pts',(-21.4605294885784,26.0049823570778,-47.1359589016551));
#19643=CARTESIAN_POINT('Ctrl Pts',(-21.5227070276251,26.0565848910482,-47.1313097251169));
#19644=CARTESIAN_POINT('Ctrl Pts',(-21.672070481874,26.1713445675928,-47.1206116268679));
#19645=CARTESIAN_POINT('Ctrl Pts',(-21.7606101883463,26.2325785548331,-47.114615818604));
#19646=CARTESIAN_POINT('Ctrl Pts',(-21.9246983669837,26.3343139626544,-47.1038264355563));
#19647=CARTESIAN_POINT('Ctrl Pts',(-21.9990874090174,26.3764339774463,-47.0990452192217));
#19648=CARTESIAN_POINT('Ctrl Pts',(-22.075036119826,26.4155368283487,-47.0942077761624));
#19649=CARTESIAN_POINT('Origin',(-23.5502525316942,23.5502525316942,-77.3107734492734));
#19650=CARTESIAN_POINT('',(-22.075035968613,26.4155367504953,-45.5987738960335));
#19651=CARTESIAN_POINT('',(-22.0750360214967,26.415536777723,-45.8455485119974));
#19652=CARTESIAN_POINT('',(-22.0750360153461,26.4155367745563,-77.3107734492734));
#19653=CARTESIAN_POINT('',(-26.7730016394076,23.5478543589546,-46.4374510733466));
#19654=CARTESIAN_POINT('Ctrl Pts',(-22.075035968613,26.4155367504953,-45.5987738960335));
#19655=CARTESIAN_POINT('Ctrl Pts',(-22.0165580353436,26.3854288766699,-45.6025778778048));
#19656=CARTESIAN_POINT('Ctrl Pts',(-21.9589923427003,26.3535259016668,-45.6063198601432));
#19657=CARTESIAN_POINT('Ctrl Pts',(-21.6136990603566,26.1480877521114,-45.6289827267317));
#19658=CARTESIAN_POINT('Ctrl Pts',(-21.3536432859975,25.9322443973274,-45.6472608830081));
#19659=CARTESIAN_POINT('Ctrl Pts',(-21.1180092056232,25.6646636061829,-45.6688201462336));
#19660=CARTESIAN_POINT('Ctrl Pts',(-21.1045458555812,25.6490761576661,-45.6700716168196));
#19661=CARTESIAN_POINT('Ctrl Pts',(-21.087174758204,25.6285703285659,-45.6717126809756));
#19662=CARTESIAN_POINT('Ctrl Pts',(-21.0831304663481,25.6237678310967,-45.6720966467837));
#19663=CARTESIAN_POINT('Ctrl Pts',(-21.07692618545,25.6163565509976,-45.6726886268114));
#19664=CARTESIAN_POINT('Ctrl Pts',(-21.0747562160286,25.6137561116753,-45.6728962324679));
#19665=CARTESIAN_POINT('Ctrl Pts',(-21.0704732909849,25.6086070783613,-45.6733070981949));
#19666=CARTESIAN_POINT('Ctrl Pts',(-21.0683601548949,25.6060586393545,-45.6735103505449));
#19667=CARTESIAN_POINT('Ctrl Pts',(-21.0637344427058,25.6004625104821,-45.6739564575553));
#19668=CARTESIAN_POINT('Ctrl Pts',(-21.0612235379373,25.5974134516035,-45.6741993797395));
#19669=CARTESIAN_POINT('Ctrl Pts',(-21.0541502303927,25.5887918941537,-45.6748858806032));
#19670=CARTESIAN_POINT('Ctrl Pts',(-21.0496009139492,25.5832087329391,-45.6753299885735));
#19671=CARTESIAN_POINT('Ctrl Pts',(-21.0394558104914,25.570672548558,-45.676326171888));
#19672=CARTESIAN_POINT('Ctrl Pts',(-21.0338701320247,25.5637114549905,-45.6768786506533));
#19673=CARTESIAN_POINT('Ctrl Pts',(-20.9214489946373,25.4224092767963,-45.6880799576363));
#19674=CARTESIAN_POINT('Ctrl Pts',(-20.8255040282504,25.2797921036104,-45.6991648826075));
#19675=CARTESIAN_POINT('Ctrl Pts',(-20.5839922915552,24.8504358265447,-45.7319009234585));
#19676=CARTESIAN_POINT('Ctrl Pts',(-20.4693026896633,24.5487101236792,-45.7543193423022));
#19677=CARTESIAN_POINT('Ctrl Pts',(-20.3976736607389,24.2192988513585,-45.7756515485088));
#19678=CARTESIAN_POINT('Ctrl Pts',(-20.3943721622441,24.2035485096867,-45.7766637686151));
#19679=CARTESIAN_POINT('Ctrl Pts',(-20.3904811574243,24.1842676874093,-45.7778928697495));
#19680=CARTESIAN_POINT('Ctrl Pts',(-20.3897794497448,24.1807604649602,-45.7781160418671));
#19681=CARTESIAN_POINT('Ctrl Pts',(-20.3886317780269,24.1749742019226,-45.778483559913));
#19682=CARTESIAN_POINT('Ctrl Pts',(-20.3881824385008,24.1726958472464,-45.7786280987122));
#19683=CARTESIAN_POINT('Ctrl Pts',(-20.3873763461655,24.1685851946369,-45.7788885652633));
#19684=CARTESIAN_POINT('Ctrl Pts',(-20.3870187235814,24.1667530769632,-45.7790045428694));
#19685=CARTESIAN_POINT('Ctrl Pts',(-20.3862527367308,24.1628106758395,-45.7792538647139));
#19686=CARTESIAN_POINT('Ctrl Pts',(-20.3858448928842,24.1607003001344,-45.7793871784667));
#19687=CARTESIAN_POINT('Ctrl Pts',(-20.3847327436159,24.1549144528182,-45.7797522702867));
#19688=CARTESIAN_POINT('Ctrl Pts',(-20.3840327256504,24.1512381452704,-45.7799838019323));
#19689=CARTESIAN_POINT('Ctrl Pts',(-20.3804173632127,24.1320695782407,-45.7811887398416));
#19690=CARTESIAN_POINT('Ctrl Pts',(-20.3776092487336,24.1165569498306,-45.782156082503));
#19691=CARTESIAN_POINT('Ctrl Pts',(-20.3509120974131,23.9626410773502,-45.7916826035666));
#19692=CARTESIAN_POINT('Ctrl Pts',(-20.3359777592654,23.8228176379373,-45.7997681901704));
#19693=CARTESIAN_POINT('Ctrl Pts',(-20.3189810922899,23.408814198073,-45.8231853555543));
#19694=CARTESIAN_POINT('Ctrl Pts',(-20.342670188454,23.1348797720613,-45.8381075215888));
#19695=CARTESIAN_POINT('Ctrl Pts',(-20.4049382015424,22.8477477104668,-45.855324449209));
#19696=CARTESIAN_POINT('Ctrl Pts',(-20.4093454358813,22.828298342796,-45.856497997509));
#19697=CARTESIAN_POINT('Ctrl Pts',(-20.4151240283008,22.8038520737236,-45.8579829026203));
#19698=CARTESIAN_POINT('Ctrl Pts',(-20.4163273642619,22.7988156275238,-45.8582893525236));
#19699=CARTESIAN_POINT('Ctrl Pts',(-20.4185064964472,22.7897913636945,-45.8588394084121));
#19700=CARTESIAN_POINT('Ctrl Pts',(-20.4194777860636,22.7858024618903,-45.8590828811931));
#19701=CARTESIAN_POINT('Ctrl Pts',(-20.4212551693743,22.7785632916962,-45.8595253619068));
#19702=CARTESIAN_POINT('Ctrl Pts',(-20.4220587130763,22.775312398797,-45.8597242937678));
#19703=CARTESIAN_POINT('Ctrl Pts',(-20.435604053182,22.7208764519669,-45.8630592318811));
#19704=CARTESIAN_POINT('Ctrl Pts',(-20.4495949062555,22.6700130072156,-45.8662323980992));
#19705=CARTESIAN_POINT('Ctrl Pts',(-20.4673461278434,22.611166937673,-45.8699781604755));
#19706=CARTESIAN_POINT('Ctrl Pts',(-20.469899126371,22.602826258172,-45.8705108325926));
#19707=CARTESIAN_POINT('Ctrl Pts',(-20.4737570437703,22.59040283204,-45.8713069065935));
#19708=CARTESIAN_POINT('Ctrl Pts',(-20.4750363123559,22.5863121096867,-45.8715694649342));
#19709=CARTESIAN_POINT('Ctrl Pts',(-20.4773336827149,22.5790169190626,-45.8720384729108));
#19710=CARTESIAN_POINT('Ctrl Pts',(-20.4783486478458,22.5758114632265,-45.872244819006));
#19711=CARTESIAN_POINT('Ctrl Pts',(-20.4804774019647,22.5691248261565,-45.8726758211716));
#19712=CARTESIAN_POINT('Ctrl Pts',(-20.4815920999582,22.5656439413388,-45.8729005069672));
#19713=CARTESIAN_POINT('Ctrl Pts',(-20.4845313154655,22.5565190813885,-45.8734903400546));
#19714=CARTESIAN_POINT('Ctrl Pts',(-20.486365491299,22.5508782530394,-45.8738558057817));
#19715=CARTESIAN_POINT('Ctrl Pts',(-20.4944327139779,22.5262992565031,-45.8754519623203));
#19716=CARTESIAN_POINT('Ctrl Pts',(-20.5008257475127,22.5074144199652,-45.8766879354915));
#19717=CARTESIAN_POINT('Ctrl Pts',(-20.5178676367267,22.4585701898914,-45.8799101756262));
#19718=CARTESIAN_POINT('Ctrl Pts',(-20.5287851614256,22.4287074812179,-45.8819052893778));
#19719=CARTESIAN_POINT('Ctrl Pts',(-20.5781164904373,22.2997225022952,-45.8906345613972));
#19720=CARTESIAN_POINT('Ctrl Pts',(-20.6209760372579,22.20238266801,-45.897514785925));
#19721=CARTESIAN_POINT('Ctrl Pts',(-20.7269662233711,21.9907051172541,-45.9131270333222));
#19722=CARTESIAN_POINT('Ctrl Pts',(-20.7923942729529,21.8777253439123,-45.9219125899876));
#19723=CARTESIAN_POINT('Ctrl Pts',(-20.9855454231276,21.5864877227647,-45.9455603035558));
#19724=CARTESIAN_POINT('Ctrl Pts',(-21.124915775929,21.4167441857732,-45.9604612288683));
#19725=CARTESIAN_POINT('Ctrl Pts',(-21.2894446790957,21.253510016613,-45.9750829089385));
#19726=CARTESIAN_POINT('Ctrl Pts',(-21.2984984398579,21.2446329079144,-45.9758789637071));
#19727=CARTESIAN_POINT('Ctrl Pts',(-21.3102144537941,21.2332803308726,-45.9768978714395));
#19728=CARTESIAN_POINT('Ctrl Pts',(-21.3128286656943,21.2307557729151,-45.977124509184));
#19729=CARTESIAN_POINT('Ctrl Pts',(-21.3168255920612,21.2269089652074,-45.9774699265147));
#19730=CARTESIAN_POINT('Ctrl Pts',(-21.3182052115899,21.225583526551,-45.9775889559404));
#19731=CARTESIAN_POINT('Ctrl Pts',(-21.3207963418269,21.2230985891858,-45.977812137595));
#19732=CARTESIAN_POINT('Ctrl Pts',(-21.3220075728037,21.2219388118779,-45.9779163116334));
#19733=CARTESIAN_POINT('Ctrl Pts',(-21.3247925669511,21.2192762892711,-45.9781554891084));
#19734=CARTESIAN_POINT('Ctrl Pts',(-21.3263669443155,21.2177741948747,-45.9782904412377));
#19735=CARTESIAN_POINT('Ctrl Pts',(-21.3307401528241,21.2136102224128,-45.978664595588));
#19736=CARTESIAN_POINT('Ctrl Pts',(-21.3335422616741,21.2109517685088,-45.978903530524));
#19737=CARTESIAN_POINT('Ctrl Pts',(-21.3489824989436,21.1963557557022,-45.9802157540737));
#19738=CARTESIAN_POINT('Ctrl Pts',(-21.3617125979305,21.1845152725435,-45.9812816193898));
#19739=CARTESIAN_POINT('Ctrl Pts',(-21.5174295384143,21.0420129738234,-45.9941354918279));
#19740=CARTESIAN_POINT('Ctrl Pts',(-21.6718424580248,20.9243748027023,-46.0050273612869));
#19741=CARTESIAN_POINT('Ctrl Pts',(-21.994619412911,20.7216039196989,-46.0263509412829));
#19742=CARTESIAN_POINT('Ctrl Pts',(-22.1617149513185,20.635942027308,-46.0367538669091));
#19743=CARTESIAN_POINT('Ctrl Pts',(-22.3734063939086,20.5497787115827,-46.0499778769603));
#19744=CARTESIAN_POINT('Ctrl Pts',(-22.4118022945988,20.5350011590443,-46.0523768650431));
#19745=CARTESIAN_POINT('Ctrl Pts',(-22.4593732506605,20.5177305312903,-46.0553553279665));
#19746=CARTESIAN_POINT('Ctrl Pts',(-22.4682911618978,20.5145373144202,-46.0559139492672));
#19747=CARTESIAN_POINT('Ctrl Pts',(-22.4816988408589,20.509803041301,-46.0567542790278));
#19748=CARTESIAN_POINT('Ctrl Pts',(-22.4861781939927,20.5082324960368,-46.0570351017341));
#19749=CARTESIAN_POINT('Ctrl Pts',(-22.4944535683765,20.505351508906,-46.0575540623688));
#19750=CARTESIAN_POINT('Ctrl Pts',(-22.4982486052393,20.5040382536044,-46.0577921146944));
#19751=CARTESIAN_POINT('Ctrl Pts',(-22.5064763972298,20.5012082726801,-46.0583083595162));
#19752=CARTESIAN_POINT('Ctrl Pts',(-22.5109100205617,20.4996941145305,-46.0585866294469));
#19753=CARTESIAN_POINT('Ctrl Pts',(-22.521954953952,20.4959489546148,-46.0592800776259));
#19754=CARTESIAN_POINT('Ctrl Pts',(-22.5285702163325,20.4937297533191,-46.0596956160141));
#19755=CARTESIAN_POINT('Ctrl Pts',(-22.5368071427109,20.4909962658855,-46.0602132946096));
#19756=CARTESIAN_POINT('Ctrl Pts',(-22.5384221107824,20.4904617454406,-46.0603148060901));
#19757=CARTESIAN_POINT('Ctrl Pts',(-22.5496166216751,20.4867664298182,-46.061018548245));
#19758=CARTESIAN_POINT('Ctrl Pts',(-22.5592104565531,20.4836493746648,-46.0616221346211));
#19759=CARTESIAN_POINT('Ctrl Pts',(-22.5781465875493,20.4775951313769,-46.0628145064408));
#19760=CARTESIAN_POINT('Ctrl Pts',(-22.5874879536924,20.474655381459,-46.0634032034695));
#19761=CARTESIAN_POINT('Ctrl Pts',(-22.608202369643,20.468240124388,-46.064709811335));
#19762=CARTESIAN_POINT('Ctrl Pts',(-22.6195815100508,20.4647849123068,-46.0654283583065));
#19763=CARTESIAN_POINT('Ctrl Pts',(-22.6371832277268,20.4595464788583,-46.0665411515939));
#19764=CARTESIAN_POINT('Ctrl Pts',(-22.6433925699015,20.4577188669407,-46.0669339625419));
#19765=CARTESIAN_POINT('Ctrl Pts',(-22.661352148811,20.4524915179566,-46.0680708664624));
#19766=CARTESIAN_POINT('Ctrl Pts',(-22.6731161948093,20.4491399847251,-46.0688165078664));
#19767=CARTESIAN_POINT('Ctrl Pts',(-22.6892931252701,20.444630649933,-46.0698432260492));
#19768=CARTESIAN_POINT('Ctrl Pts',(-22.6936899179442,20.4434150946271,-46.0701224208528));
#19769=CARTESIAN_POINT('Ctrl Pts',(-22.7012026739291,20.4413552475152,-46.0705997208565));
#19770=CARTESIAN_POINT('Ctrl Pts',(-22.7043173614008,20.4405062925143,-46.070797674122));
#19771=CARTESIAN_POINT('Ctrl Pts',(-22.7103644309178,20.4388678298487,-46.0711821343374));
#19772=CARTESIAN_POINT('Ctrl Pts',(-22.7132966641218,20.4380777839747,-46.0713686235187));
#19773=CARTESIAN_POINT('Ctrl Pts',(-22.7193553506811,20.4364545443433,-46.0717540878499));
#19774=CARTESIAN_POINT('Ctrl Pts',(-22.7224819495484,20.435621912398,-46.0719530810012));
#19775=CARTESIAN_POINT('Ctrl Pts',(-22.7321693670575,20.433057712472,-46.0725698695383));
#19776=CARTESIAN_POINT('Ctrl Pts',(-22.7387343728662,20.4313421639516,-46.0729881843282));
#19777=CARTESIAN_POINT('Ctrl Pts',(-22.7737857426186,20.4223008010219,-46.0752234103511));
#19778=CARTESIAN_POINT('Ctrl Pts',(-22.8023652241135,20.4153446882904,-46.0770522501172));
#19779=CARTESIAN_POINT('Ctrl Pts',(-22.8826486484254,20.3969643749896,-46.0822089927264));
#19780=CARTESIAN_POINT('Ctrl Pts',(-22.9345428623239,20.3864222242885,-46.0855646568667));
#19781=CARTESIAN_POINT('Ctrl Pts',(-23.1145095619368,20.3544578077146,-46.0972839549419));
#19782=CARTESIAN_POINT('Ctrl Pts',(-23.2435896173721,20.3395007323407,-46.105838033096));
#19783=CARTESIAN_POINT('Ctrl Pts',(-23.6628375659541,20.3164341110151,-46.1339607275463));
#19784=CARTESIAN_POINT('Ctrl Pts',(-23.9532932906882,20.3396722613074,-46.1540792125754));
#19785=CARTESIAN_POINT('Ctrl Pts',(-24.2523256931709,20.4048644980893,-46.1734443658615));
#19786=CARTESIAN_POINT('Ctrl Pts',(-24.2679041569044,20.4083822644858,-46.1744488508876));
#19787=CARTESIAN_POINT('Ctrl Pts',(-24.2869294799187,20.4128272563152,-46.1756696941076));
#19788=CARTESIAN_POINT('Ctrl Pts',(-24.2904014250837,20.4136445070041,-46.1758922460162));
#19789=CARTESIAN_POINT('Ctrl Pts',(-24.2961285957211,20.4150026472226,-46.1762589525115));
#19790=CARTESIAN_POINT('Ctrl Pts',(-24.2983845943666,20.4155402071196,-46.1764032985086));
#19791=CARTESIAN_POINT('Ctrl Pts',(-24.3024551908386,20.4165147944557,-46.1766635581792));
#19792=CARTESIAN_POINT('Ctrl Pts',(-24.3042699846525,20.4169509619584,-46.1767795213428));
#19793=CARTESIAN_POINT('Ctrl Pts',(-24.3081760822386,20.4178933435161,-46.177028968745));
#19794=CARTESIAN_POINT('Ctrl Pts',(-24.3102672524509,20.4184000740372,-46.1771624222164));
#19795=CARTESIAN_POINT('Ctrl Pts',(-24.3160040379381,20.4197962910135,-46.177528284821));
#19796=CARTESIAN_POINT('Ctrl Pts',(-24.3196486242385,20.4206900547257,-46.1777604457879));
#19797=CARTESIAN_POINT('Ctrl Pts',(-24.3387231373438,20.4254030417539,-46.1789741118318));
#19798=CARTESIAN_POINT('Ctrl Pts',(-24.354126565583,20.429330105086,-46.179949448137));
#19799=CARTESIAN_POINT('Ctrl Pts',(-24.5460263904108,20.4797694875027,-46.1920482889384));
#19800=CARTESIAN_POINT('Ctrl Pts',(-24.7183199660161,20.5410881113918,-46.2023685455189));
#19801=CARTESIAN_POINT('Ctrl Pts',(-24.9559136318388,20.6491515694645,-46.2169906174701));
#19802=CARTESIAN_POINT('Ctrl Pts',(-25.0261032001551,20.6842213438887,-46.2213609389931));
#19803=CARTESIAN_POINT('Ctrl Pts',(-25.1816447476865,20.76916710313,-46.2312868364782));
#19804=CARTESIAN_POINT('Ctrl Pts',(-25.2661197870087,20.8204769209934,-46.2368512206316));
#19805=CARTESIAN_POINT('Ctrl Pts',(-25.3916137472444,20.9048309859256,-46.2455263522853));
#19806=CARTESIAN_POINT('Ctrl Pts',(-25.4344039128285,20.935135042783,-46.2485614447882));
#19807=CARTESIAN_POINT('Ctrl Pts',(-25.4931223726926,20.9789089921159,-46.2528501432773));
#19808=CARTESIAN_POINT('Ctrl Pts',(-25.5096890776061,20.9915108071235,-46.2540743473389));
#19809=CARTESIAN_POINT('Ctrl Pts',(-25.5358770730943,21.0118347373889,-46.2560331637053));
#19810=CARTESIAN_POINT('Ctrl Pts',(-25.5455782576202,21.0194532588561,-46.256764047246));
#19811=CARTESIAN_POINT('Ctrl Pts',(-25.5973460143364,21.0605901231864,-46.2606930433605));
#19812=CARTESIAN_POINT('Ctrl Pts',(-25.6386102531276,21.095100369918,-46.2639278050148));
#19813=CARTESIAN_POINT('Ctrl Pts',(-25.6855782360978,21.136421820434,-46.2677399912346));
#19814=CARTESIAN_POINT('Ctrl Pts',(-25.69214286011,21.14224497665,-46.2682758550324));
#19815=CARTESIAN_POINT('Ctrl Pts',(-25.7018861595441,21.1509591451082,-46.2690757739128));
#19816=CARTESIAN_POINT('Ctrl Pts',(-25.7050830066274,21.153829854572,-46.2693389733487));
#19817=CARTESIAN_POINT('Ctrl Pts',(-25.7107722153232,21.1589592471565,-46.2698086980577));
#19818=CARTESIAN_POINT('Ctrl Pts',(-25.713266804345,21.1612154595256,-46.2700151185932));
#19819=CARTESIAN_POINT('Ctrl Pts',(-25.7180810199725,21.1655833622212,-46.2704143685858));
#19820=CARTESIAN_POINT('Ctrl Pts',(-25.7204011055336,21.1676945429397,-46.270607176271));
#19821=CARTESIAN_POINT('Ctrl Pts',(-25.7254160516534,21.1722713363335,-46.2710248048688));
#19822=CARTESIAN_POINT('Ctrl Pts',(-25.7281098079192,21.174738147762,-46.2712496767344));
#19823=CARTESIAN_POINT('Ctrl Pts',(-25.7386709937686,21.1844426327633,-46.272133460234));
#19824=CARTESIAN_POINT('Ctrl Pts',(-25.7465065161628,21.1917147909929,-46.2727938455169));
#19825=CARTESIAN_POINT('Ctrl Pts',(-25.8312572755242,21.2711606250431,-46.2799882969201));
#19826=CARTESIAN_POINT('Ctrl Pts',(-25.9046130369542,21.3470219535522,-46.2866829151918));
#19827=CARTESIAN_POINT('Ctrl Pts',(-26.0179198385658,21.4763301188398,-46.29783967667));
#19828=CARTESIAN_POINT('Ctrl Pts',(-26.0601679719696,21.5276651500236,-46.3022087778334));
#19829=CARTESIAN_POINT('Ctrl Pts',(-26.299050875577,21.8369473528616,-46.3281555348715));
#19830=CARTESIAN_POINT('Ctrl Pts',(-26.4574111655566,22.1220626151391,-46.3508198618096));
#19831=CARTESIAN_POINT('Ctrl Pts',(-26.5755924763332,22.4395568428949,-46.3722538042032));
#19832=CARTESIAN_POINT('Ctrl Pts',(-26.580546123074,22.453143848663,-46.3731638405641));
#19833=CARTESIAN_POINT('Ctrl Pts',(-26.5870050880402,22.4712372244287,-46.3743657043706));
#19834=CARTESIAN_POINT('Ctrl Pts',(-26.5885920457054,22.4757139702297,-46.3746622648242));
#19835=CARTESIAN_POINT('Ctrl Pts',(-26.5909649691406,22.4824551817748,-46.375107598245));
#19836=CARTESIAN_POINT('Ctrl Pts',(-26.5917583061088,22.4847170174911,-46.3752568091337));
#19837=CARTESIAN_POINT('Ctrl Pts',(-26.5931673079274,22.488748533657,-46.3755223890342));
#19838=CARTESIAN_POINT('Ctrl Pts',(-26.5937839523025,22.4905178643814,-46.3756388167044));
#19839=CARTESIAN_POINT('Ctrl Pts',(-26.5950886137476,22.4942718462325,-46.3758855673337));
#19840=CARTESIAN_POINT('Ctrl Pts',(-26.5957762318597,22.4962566273221,-46.3760158660535));
#19841=CARTESIAN_POINT('Ctrl Pts',(-26.5976119500857,22.5015721468608,-46.3763643949824));
#19842=CARTESIAN_POINT('Ctrl Pts',(-26.5987565340152,22.5049041101099,-46.3765824149693));
#19843=CARTESIAN_POINT('Ctrl Pts',(-26.6041616364888,22.5207231150396,-46.3776153903402));
#19844=CARTESIAN_POINT('Ctrl Pts',(-26.6083509903354,22.5332346009201,-46.3784261592266));
#19845=CARTESIAN_POINT('Ctrl Pts',(-26.6414664383251,22.6341887311959,-46.3849208107518));
#19846=CARTESIAN_POINT('Ctrl Pts',(-26.6666295296635,22.7238299216021,-46.3903960046259));
#19847=CARTESIAN_POINT('Ctrl Pts',(-26.7442560136724,23.0548436791869,-46.4099802088258));
#19848=CARTESIAN_POINT('Ctrl Pts',(-26.77281788917,23.3009243090713,-46.4233912076773));
#19849=CARTESIAN_POINT('Ctrl Pts',(-26.7730016394076,23.5478543589546,-46.4374510733466));
#19850=CARTESIAN_POINT('Ctrl Pts',(-26.7730016423177,23.5478582728161,-46.4374512961967));
#19851=CARTESIAN_POINT('Ctrl Pts',(-26.7731184949075,23.7051456001714,-46.4464070291098));
#19852=CARTESIAN_POINT('Ctrl Pts',(-26.7617209856594,23.8622143069203,-46.4555805427443));
#19853=CARTESIAN_POINT('Ctrl Pts',(-26.7376925346768,24.0260819106865,-46.4656481510428));
#19854=CARTESIAN_POINT('Ctrl Pts',(-26.7364482240046,24.0343438234673,-46.4661570432107));
#19855=CARTESIAN_POINT('Ctrl Pts',(-26.7344127238532,24.0475111378039,-46.4669701939533));
#19856=CARTESIAN_POINT('Ctrl Pts',(-26.7336422874599,24.0524197479978,-46.4672737947172));
#19857=CARTESIAN_POINT('Ctrl Pts',(-26.7323011605808,24.0608372197463,-46.4677952318725));
#19858=CARTESIAN_POINT('Ctrl Pts',(-26.7317360085714,24.0643469651105,-46.4680128921738));
#19859=CARTESIAN_POINT('Ctrl Pts',(-26.7306619783229,24.0709473804426,-46.4684226817433));
#19860=CARTESIAN_POINT('Ctrl Pts',(-26.7301543987995,24.0740382600113,-46.4686147695162));
#19861=CARTESIAN_POINT('Ctrl Pts',(-26.7290875719744,24.0804759403122,-46.4690152460477));
#19862=CARTESIAN_POINT('Ctrl Pts',(-26.7285275436922,24.0838226061254,-46.4692236594402));
#19863=CARTESIAN_POINT('Ctrl Pts',(-26.7272240568216,24.0915372283624,-46.4697046049134));
#19864=CARTESIAN_POINT('Ctrl Pts',(-26.7264768749336,24.0959045411449,-46.469977255277));
#19865=CARTESIAN_POINT('Ctrl Pts',(-26.7241236099639,24.1094908626452,-46.470826646969));
#19866=CARTESIAN_POINT('Ctrl Pts',(-26.7224863886345,24.1187043644816,-46.4714043798367));
#19867=CARTESIAN_POINT('Ctrl Pts',(-26.7082586366505,24.1967953672538,-46.4763158875254));
#19868=CARTESIAN_POINT('Ctrl Pts',(-26.6934674928553,24.2652481002497,-46.4807196536279));
#19869=CARTESIAN_POINT('Ctrl Pts',(-26.6746212359348,24.3405025200152,-46.4856765265498));
#19870=CARTESIAN_POINT('Ctrl Pts',(-26.6727567724568,24.3478377051879,-46.4861609027556));
#19871=CARTESIAN_POINT('Ctrl Pts',(-26.6576835994587,24.4062757162355,-46.4900295875302));
#19872=CARTESIAN_POINT('Ctrl Pts',(-26.6432477028271,24.4570512501088,-46.4934507474262));
#19873=CARTESIAN_POINT('Ctrl Pts',(-26.6225758173727,24.5235100343554,-46.4980065634005));
#19874=CARTESIAN_POINT('Ctrl Pts',(-26.6174538962157,24.5395332367675,-46.4991110010633));
#19875=CARTESIAN_POINT('Ctrl Pts',(-26.6060956329998,24.5741296430884,-46.5015085427888));
#19876=CARTESIAN_POINT('Ctrl Pts',(-26.5998149102964,24.5926875067223,-46.5028027149303));
#19877=CARTESIAN_POINT('Ctrl Pts',(-26.5055103472674,24.8631844356457,-46.5217826651902));
#19878=CARTESIAN_POINT('Ctrl Pts',(-26.3867048588624,25.1032696751286,-46.540226619876));
#19879=CARTESIAN_POINT('Ctrl Pts',(-26.201012114542,25.3845140138018,-46.5623849775488));
#19880=CARTESIAN_POINT('Ctrl Pts',(-26.1604427523329,25.4417995942538,-46.5669236662633));
#19881=CARTESIAN_POINT('Ctrl Pts',(-26.1112837936525,25.5066167965359,-46.5720475767282));
#19882=CARTESIAN_POINT('Ctrl Pts',(-26.1044894786437,25.5154792079462,-46.5727479009901));
#19883=CARTESIAN_POINT('Ctrl Pts',(-26.0956163030252,25.5269295027079,-46.5736521834068));
#19884=CARTESIAN_POINT('Ctrl Pts',(-26.0935794266073,25.5295495993394,-46.5738590674778));
#19885=CARTESIAN_POINT('Ctrl Pts',(-26.0902748938611,25.5337867976081,-46.574193572185));
#19886=CARTESIAN_POINT('Ctrl Pts',(-26.0890097385519,25.5354058328394,-46.5743213708168));
#19887=CARTESIAN_POINT('Ctrl Pts',(-26.086580858206,25.5385079822049,-46.5745662070783));
#19888=CARTESIAN_POINT('Ctrl Pts',(-26.0854173837576,25.5399912806832,-46.5746832616708));
#19889=CARTESIAN_POINT('Ctrl Pts',(-26.0827431036422,25.5433945322093,-46.5749517982425));
#19890=CARTESIAN_POINT('Ctrl Pts',(-26.0812314122539,25.5453137932795,-46.5751032164912));
#19891=CARTESIAN_POINT('Ctrl Pts',(-26.0764430676977,25.5513789302333,-46.5755816542551));
#19892=CARTESIAN_POINT('Ctrl Pts',(-26.0731583776459,25.5555184942358,-46.5759080997903));
#19893=CARTESIAN_POINT('Ctrl Pts',(-26.0456097165686,25.5900621371338,-46.5786315746146));
#19894=CARTESIAN_POINT('Ctrl Pts',(-26.0208059720214,25.6200343406938,-46.5809905236041));
#19895=CARTESIAN_POINT('Ctrl Pts',(-25.9935136519419,25.6518237600829,-46.5834971307362));
#19896=CARTESIAN_POINT('Ctrl Pts',(-25.9915598427492,25.6540931014208,-46.5836760949816));
#19897=CARTESIAN_POINT('Ctrl Pts',(-25.8141781590945,25.8595413667278,-46.599880802174));
#19898=CARTESIAN_POINT('Ctrl Pts',(-25.6140322967345,26.0400373000633,-46.6144265851439));
#19899=CARTESIAN_POINT('Ctrl Pts',(-25.3443717270565,26.2281032386562,-46.6329509681757));
#19900=CARTESIAN_POINT('Ctrl Pts',(-25.2939944147815,26.2611770880131,-46.6363675788085));
#19901=CARTESIAN_POINT('Ctrl Pts',(-25.1600263545218,26.3438502925547,-46.6453906473557));
#19902=CARTESIAN_POINT('Ctrl Pts',(-25.0750724138897,26.3911119128342,-46.6510525841636));
#19903=CARTESIAN_POINT('Ctrl Pts',(-24.9465053806826,26.4552065017461,-46.6596234300786));
#19904=CARTESIAN_POINT('Ctrl Pts',(-24.9044499331921,26.4750480188053,-46.6624269787629));
#19905=CARTESIAN_POINT('Ctrl Pts',(-24.8548962124833,26.4971292849785,-46.6657354070103));
#19906=CARTESIAN_POINT('Ctrl Pts',(-24.8477995385892,26.5002609208534,-46.666209328047));
#19907=CARTESIAN_POINT('Ctrl Pts',(-24.8376361491402,26.5047020748432,-46.6668882344434));
#19908=CARTESIAN_POINT('Ctrl Pts',(-24.834578560702,26.5060325188655,-46.667092503166));
#19909=CARTESIAN_POINT('Ctrl Pts',(-24.8284004338454,26.5087094019919,-46.6675052974828));
#19910=CARTESIAN_POINT('Ctrl Pts',(-24.8252798197861,26.5100556548196,-46.6677138291186));
#19911=CARTESIAN_POINT('Ctrl Pts',(-24.819236918863,26.5126512706072,-46.6681176928903));
#19912=CARTESIAN_POINT('Ctrl Pts',(-24.8163149006211,26.5139012526221,-46.6683130036056));
#19913=CARTESIAN_POINT('Ctrl Pts',(-24.8093670192176,26.5168612692332,-46.6687774669044));
#19914=CARTESIAN_POINT('Ctrl Pts',(-24.805339521502,26.5185674311037,-46.6690467512245));
#19915=CARTESIAN_POINT('Ctrl Pts',(-24.7910927341977,26.5245685934888,-46.6699994888805));
#19916=CARTESIAN_POINT('Ctrl Pts',(-24.7808548599474,26.5288190238772,-46.6706844565143));
#19917=CARTESIAN_POINT('Ctrl Pts',(-24.6383167925666,26.5871358434497,-46.6802259763764));
#19918=CARTESIAN_POINT('Ctrl Pts',(-24.5026041036304,26.6323882093989,-46.6893810592387));
#19919=CARTESIAN_POINT('Ctrl Pts',(-24.2081147414089,26.7092727874002,-46.7094099572248));
#19920=CARTESIAN_POINT('Ctrl Pts',(-24.049043628112,26.7382599382118,-46.7203276045688));
#19921=CARTESIAN_POINT('Ctrl Pts',(-23.8687860598017,26.7572832955246,-46.732596188559));
#19922=CARTESIAN_POINT('Ctrl Pts',(-23.8490684234534,26.7591805451026,-46.7339365784371));
#19923=CARTESIAN_POINT('Ctrl Pts',(-23.654390093876,26.7761027648933,-46.747149233727));
#19924=CARTESIAN_POINT('Ctrl Pts',(-23.4784713051421,26.7769873987355,-46.7589346424501));
#19925=CARTESIAN_POINT('Ctrl Pts',(-23.2912282831935,26.7625992603705,-46.7707738080367));
#19926=CARTESIAN_POINT('Ctrl Pts',(-23.2791239829174,26.7616002842415,-46.7715359130555));
#19927=CARTESIAN_POINT('Ctrl Pts',(-23.2636173294508,26.7602322089864,-46.7725078353246));
#19928=CARTESIAN_POINT('Ctrl Pts',(-23.2602097293672,26.7599261040177,-46.7727211435077));
#19929=CARTESIAN_POINT('Ctrl Pts',(-23.2547335247202,26.759425383988,-46.7730634965432));
#19930=CARTESIAN_POINT('Ctrl Pts',(-23.2526646214662,26.7592341949524,-46.7731927349279));
#19931=CARTESIAN_POINT('Ctrl Pts',(-23.2487253259274,26.7588663190229,-46.7734386148563));
#19932=CARTESIAN_POINT('Ctrl Pts',(-23.2468549171314,26.7586899986782,-46.7735552760045));
#19933=CARTESIAN_POINT('Ctrl Pts',(-23.242597558466,26.7582849083609,-46.7738206248765));
#19934=CARTESIAN_POINT('Ctrl Pts',(-23.2402107122097,26.7580551101822,-46.7739692534737));
#19935=CARTESIAN_POINT('Ctrl Pts',(-23.2327995505412,26.7573332374187,-46.7744303273297));
#19936=CARTESIAN_POINT('Ctrl Pts',(-23.2277761021706,26.756832017922,-46.7747422563615));
#19937=CARTESIAN_POINT('Ctrl Pts',(-23.1896680133286,26.7529392881662,-46.7771041727925));
#19938=CARTESIAN_POINT('Ctrl Pts',(-23.1566349287742,26.7490474686763,-46.7791264286368));
#19939=CARTESIAN_POINT('Ctrl Pts',(-22.8758242412108,26.7115474000657,-46.7961482088612));
#19940=CARTESIAN_POINT('Ctrl Pts',(-22.6326387363219,26.6497139524358,-46.809812340871));
#19941=CARTESIAN_POINT('Ctrl Pts',(-22.2884334891064,26.5180715099323,-46.8304749790125));
#19942=CARTESIAN_POINT('Ctrl Pts',(-22.1802744908533,26.4697197196176,-46.8371684026907));
#19943=CARTESIAN_POINT('Ctrl Pts',(-22.0750360041347,26.415536768784,-46.8440307128639));
#19944=CARTESIAN_POINT('Ctrl Pts',(-22.075036119826,26.4155368283487,-47.0942077761624));
#19945=CARTESIAN_POINT('Ctrl Pts',(-22.1330124871448,26.4453864627005,-47.0905150554735));
#19946=CARTESIAN_POINT('Ctrl Pts',(-22.1918977163122,26.473477944352,-47.0867898262114));
#19947=CARTESIAN_POINT('Ctrl Pts',(-22.319582456183,26.5296961542186,-47.0787173477208));
#19948=CARTESIAN_POINT('Ctrl Pts',(-22.3885628141297,26.5572624976775,-47.0743591562471));
#19949=CARTESIAN_POINT('Ctrl Pts',(-22.4996906902738,26.5972773982751,-47.0673028948009));
#19950=CARTESIAN_POINT('Ctrl Pts',(-22.5412484516954,26.6112901332707,-47.0646566665043));
#19951=CARTESIAN_POINT('Ctrl Pts',(-22.5903858961391,26.6267492894881,-47.0615148705455));
#19952=CARTESIAN_POINT('Ctrl Pts',(-22.5977022209877,26.6290224423473,-47.0610467417006));
#19953=CARTESIAN_POINT('Ctrl Pts',(-22.6089143713249,26.6324622209073,-47.0603288120002));
#19954=CARTESIAN_POINT('Ctrl Pts',(-22.6128044501931,26.6336476076934,-47.0600796274143));
#19955=CARTESIAN_POINT('Ctrl Pts',(-22.6198970762396,26.6357942133557,-47.0596251176888));
#19956=CARTESIAN_POINT('Ctrl Pts',(-22.6230989000773,26.6367578185858,-47.0594198711317));
#19957=CARTESIAN_POINT('Ctrl Pts',(-22.6295346098767,26.6386837605029,-47.0590071853025));
#19958=CARTESIAN_POINT('Ctrl Pts',(-22.6327685188655,26.6396460049674,-47.058799743306));
#19959=CARTESIAN_POINT('Ctrl Pts',(-22.6419627763121,26.6423660319385,-47.058209768298));
#19960=CARTESIAN_POINT('Ctrl Pts',(-22.6479266819802,26.6441116490745,-47.0578268377941));
#19961=CARTESIAN_POINT('Ctrl Pts',(-22.6731650542139,26.6514196612096,-47.0562052888221));
#19962=CARTESIAN_POINT('Ctrl Pts',(-22.69248585988,26.6568191760392,-47.0549613662014));
#19963=CARTESIAN_POINT('Ctrl Pts',(-23.0854136996775,26.762684301952,-47.0296075216957));
#19964=CARTESIAN_POINT('Ctrl Pts',(-23.4739950965551,26.7952178787711,-47.0029391143135));
#19965=CARTESIAN_POINT('Ctrl Pts',(-23.9173639981117,26.7525642337943,-46.9732697255462));
#19966=CARTESIAN_POINT('Ctrl Pts',(-23.9756989674553,26.7453373769415,-46.9693937319517));
#19967=CARTESIAN_POINT('Ctrl Pts',(-24.0806142091689,26.7294152292454,-46.9625085289852));
#19968=CARTESIAN_POINT('Ctrl Pts',(-24.1272626093662,26.7212805853694,-46.9594781666081));
#19969=CARTESIAN_POINT('Ctrl Pts',(-24.1794910982479,26.7109820387632,-46.9561329232489));
#19970=CARTESIAN_POINT('Ctrl Pts',(-24.1852614114,26.7098278060737,-46.9557639913551));
#19971=CARTESIAN_POINT('Ctrl Pts',(-24.1942237084996,26.7080095386474,-46.9551920331907));
#19972=CARTESIAN_POINT('Ctrl Pts',(-24.1974178644855,26.7073564615284,-46.9549883966249));
#19973=CARTESIAN_POINT('Ctrl Pts',(-24.2027478694714,26.7062582599145,-46.9546489487162));
#19974=CARTESIAN_POINT('Ctrl Pts',(-24.2048842581659,26.7058158134465,-46.9545129854842));
#19975=CARTESIAN_POINT('Ctrl Pts',(-24.2089962855683,26.7049598562067,-46.9542514751177));
#19976=CARTESIAN_POINT('Ctrl Pts',(-24.2109719873206,26.7045466583748,-46.9541259100718));
#19977=CARTESIAN_POINT('Ctrl Pts',(-24.2147334684804,26.7037562939214,-46.953887009438));
#19978=CARTESIAN_POINT('Ctrl Pts',(-24.2165193036891,26.7033794689252,-46.9537736553027));
#19979=CARTESIAN_POINT('Ctrl Pts',(-24.2205830006119,26.7025183910443,-46.9535158711941));
#19980=CARTESIAN_POINT('Ctrl Pts',(-24.2228606539795,26.702033187056,-46.9533714970115));
#19981=CARTESIAN_POINT('Ctrl Pts',(-24.2286554661443,26.7007921620787,-46.9530044569959));
#19982=CARTESIAN_POINT('Ctrl Pts',(-24.2321718995174,26.7000329177162,-46.952781988154));
#19983=CARTESIAN_POINT('Ctrl Pts',(-24.2516620614176,26.6957905660183,-46.951550338644));
#19984=CARTESIAN_POINT('Ctrl Pts',(-24.2676107550675,26.6921917513006,-46.9505477216402));
#19985=CARTESIAN_POINT('Ctrl Pts',(-24.5914431899217,26.6165247593142,-46.9302838092796));
#19986=CARTESIAN_POINT('Ctrl Pts',(-24.8871475521932,26.499641204892,-46.9133817943598));
#19987=CARTESIAN_POINT('Ctrl Pts',(-25.2124729907998,26.3118925201923,-46.8921162567716));
#19988=CARTESIAN_POINT('Ctrl Pts',(-25.2629915425828,26.2808489738545,-46.8887341087877));
#19989=CARTESIAN_POINT('Ctrl Pts',(-25.3816958190136,26.2033148115728,-46.880551710371));
#19990=CARTESIAN_POINT('Ctrl Pts',(-25.4490054378459,26.1555662854329,-46.8757174453742));
#19991=CARTESIAN_POINT('Ctrl Pts',(-25.5481521782361,26.0793484979839,-46.8682414954455));
#19992=CARTESIAN_POINT('Ctrl Pts',(-25.5813802629199,26.0527411489711,-46.8656720388585));
#19993=CARTESIAN_POINT('Ctrl Pts',(-25.6199069149128,26.0206181001692,-46.8626124404476));
#19994=CARTESIAN_POINT('Ctrl Pts',(-25.6257260834494,26.0157311550627,-46.8621481024007));
#19995=CARTESIAN_POINT('Ctrl Pts',(-25.6346226448806,26.0082059941872,-46.8614347858529));
#19996=CARTESIAN_POINT('Ctrl Pts',(-25.6377124626503,26.0055824543198,-46.8611864113062));
#19997=CARTESIAN_POINT('Ctrl Pts',(-25.6433416006531,26.0007844919388,-46.8607327468616));
#19998=CARTESIAN_POINT('Ctrl Pts',(-25.6458825062066,25.9986119310812,-46.8605275340269));
#19999=CARTESIAN_POINT('Ctrl Pts',(-25.6509872677555,25.9942334176294,-46.8601143746657));
#20000=CARTESIAN_POINT('Ctrl Pts',(-25.6535510405158,25.9920273748689,-46.8599064245482));
#20001=CARTESIAN_POINT('Ctrl Pts',(-25.6608461668602,25.9857301426175,-46.8593134269374));
#20002=CARTESIAN_POINT('Ctrl Pts',(-25.6655690698663,25.9816292257842,-46.8589279753431));
#20003=CARTESIAN_POINT('Ctrl Pts',(-25.6856425014342,25.964096621346,-46.8572831001916));
#20004=CARTESIAN_POINT('Ctrl Pts',(-25.7008769990905,25.950533344733,-46.8560181817894));
#20005=CARTESIAN_POINT('Ctrl Pts',(-25.9828337876292,25.6946678455981,-46.8322917193505));
#20006=CARTESIAN_POINT('Ctrl Pts',(-26.2071317354619,25.4095044703714,-46.8076625732223));
#20007=CARTESIAN_POINT('Ctrl Pts',(-26.4447442181116,24.9738261989016,-46.7743616586402));
#20008=CARTESIAN_POINT('Ctrl Pts',(-26.5022890901235,24.8503042221108,-46.7653788345486));
#20009=CARTESIAN_POINT('Ctrl Pts',(-26.5539703217729,24.7180841893289,-46.7564868321669));
#20010=CARTESIAN_POINT('Ctrl Pts',(-26.5560715938307,24.7126651563515,-46.7561236337535));
#20011=CARTESIAN_POINT('Ctrl Pts',(-26.5590801625802,24.7048435610338,-46.7556012260144));
#20012=CARTESIAN_POINT('Ctrl Pts',(-26.5599992499383,24.7024455925758,-46.7554413104187));
#20013=CARTESIAN_POINT('Ctrl Pts',(-26.5615927357418,24.6982731506303,-46.7551634892879));
#20014=CARTESIAN_POINT('Ctrl Pts',(-26.5622684334703,24.6964991777259,-46.7550455049079));
#20015=CARTESIAN_POINT('Ctrl Pts',(-26.5635732720719,24.6930643413765,-46.7548173217338));
#20016=CARTESIAN_POINT('Ctrl Pts',(-26.56420260586,24.6914035590408,-46.7547071112235));
#20017=CARTESIAN_POINT('Ctrl Pts',(-26.5657013281483,24.6874386129672,-46.7544442761747));
#20018=CARTESIAN_POINT('Ctrl Pts',(-26.5665694505736,24.6851339671112,-46.7542917283461));
#20019=CARTESIAN_POINT('Ctrl Pts',(-26.5691850651587,24.6781659686935,-46.7538311840202));
#20020=CARTESIAN_POINT('Ctrl Pts',(-26.5709244011678,24.6734995306799,-46.75352367582));
#20021=CARTESIAN_POINT('Ctrl Pts',(-26.5885369767576,24.6259102465299,-46.7503967922341));
#20022=CARTESIAN_POINT('Ctrl Pts',(-26.6035060472169,24.5826552569206,-46.7476304343677));
#20023=CARTESIAN_POINT('Ctrl Pts',(-26.6194177587917,24.5332985336971,-46.7445434031147));
#20024=CARTESIAN_POINT('Ctrl Pts',(-26.6212695132344,24.527498321365,-46.7441817060314));
#20025=CARTESIAN_POINT('Ctrl Pts',(-26.7222290461342,24.2081439302195,-46.7243245233967));
#20026=CARTESIAN_POINT('Ctrl Pts',(-26.7727927939184,23.8812388493818,-46.7068622091694));
#20027=CARTESIAN_POINT('Ctrl Pts',(-26.773035153289,23.4999560933854,-46.6849291560942));
#20028=CARTESIAN_POINT('Ctrl Pts',(-26.7717931189852,23.4476200877005,-46.6818898520361));
#20029=CARTESIAN_POINT('Ctrl Pts',(-26.7688702821422,23.3868849057655,-46.678317954044));
#20030=CARTESIAN_POINT('Ctrl Pts',(-26.7684301183913,23.3784322088236,-46.6778198368517));
#20031=CARTESIAN_POINT('Ctrl Pts',(-26.7640409680229,23.3000891765746,-46.673193425053));
#20032=CARTESIAN_POINT('Ctrl Pts',(-26.7578493740784,23.2303475714157,-46.6690030614743));
#20033=CARTESIAN_POINT('Ctrl Pts',(-26.7482618182816,23.1515775638346,-46.6641700045108));
#20034=CARTESIAN_POINT('Ctrl Pts',(-26.7470907523437,23.14229356907,-46.6635987952765));
#20035=CARTESIAN_POINT('Ctrl Pts',(-26.745305630228,23.1286213034153,-46.6627552272422));
#20036=CARTESIAN_POINT('Ctrl Pts',(-26.744722923658,23.1242289294534,-46.6624838611846));
#20037=CARTESIAN_POINT('Ctrl Pts',(-26.7436779604442,23.1164748138436,-46.6620041617089));
#20038=CARTESIAN_POINT('Ctrl Pts',(-26.7432194480526,23.1131125673906,-46.6617959472037));
#20039=CARTESIAN_POINT('Ctrl Pts',(-26.7422599654973,23.1061587857662,-46.6613648757264));
#20040=CARTESIAN_POINT('Ctrl Pts',(-26.7417582422151,23.1025673608797,-46.6611419951535));
#20041=CARTESIAN_POINT('Ctrl Pts',(-26.7404571869492,23.0933675205467,-46.6605704303623));
#20042=CARTESIAN_POINT('Ctrl Pts',(-26.739649128997,23.0877603692963,-46.6602214697937));
#20043=CARTESIAN_POINT('Ctrl Pts',(-26.7362837278989,23.064836003685,-46.6587922921019));
#20044=CARTESIAN_POINT('Ctrl Pts',(-26.733600133626,23.0475378863215,-46.6577080743013));
#20045=CARTESIAN_POINT('Ctrl Pts',(-26.7150573729905,22.9341208833049,-46.6505602643618));
#20046=CARTESIAN_POINT('Ctrl Pts',(-26.6949893351046,22.8387505728653,-46.6443631592467));
#20047=CARTESIAN_POINT('Ctrl Pts',(-26.6340935951159,22.6029404839351,-46.6285531923041));
#20048=CARTESIAN_POINT('Ctrl Pts',(-26.5879727769467,22.4641017445517,-46.6187946602675));
#20049=CARTESIAN_POINT('Ctrl Pts',(-26.4395708032775,22.1017329182192,-46.5923575114094));
#20050=CARTESIAN_POINT('Ctrl Pts',(-26.3208909208857,21.8859348797931,-46.575527966804));
#20051=CARTESIAN_POINT('Ctrl Pts',(-26.1706697959829,21.6741579505544,-46.5591256829535));
#20052=CARTESIAN_POINT('Ctrl Pts',(-26.1624126350708,21.6626781283301,-46.5582371568628));
#20053=CARTESIAN_POINT('Ctrl Pts',(-26.1518743416585,21.6482284698605,-46.5571199131279));
#20054=CARTESIAN_POINT('Ctrl Pts',(-26.1496634003198,21.6452079888327,-46.5568864340756));
#20055=CARTESIAN_POINT('Ctrl Pts',(-26.146161266654,21.6404409913575,-46.5565180616147));
#20056=CARTESIAN_POINT('Ctrl Pts',(-26.1448735714259,21.638691928393,-46.5563829252218));
#20057=CARTESIAN_POINT('Ctrl Pts',(-26.1424769080871,21.6354434490548,-46.5561319863809));
#20058=CARTESIAN_POINT('Ctrl Pts',(-26.1413684135299,21.6339437028636,-46.556016152221));
#20059=CARTESIAN_POINT('Ctrl Pts',(-26.1388939971074,21.6306019946083,-46.5557580929059));
#20060=CARTESIAN_POINT('Ctrl Pts',(-26.1375274140051,21.6287605321186,-46.5556159153389));
#20061=CARTESIAN_POINT('Ctrl Pts',(-26.1335294800728,21.6233853381248,-46.5552009759156));
#20062=CARTESIAN_POINT('Ctrl Pts',(-26.1308928334417,21.6198555240237,-46.5549285848699));
#20063=CARTESIAN_POINT('Ctrl Pts',(-26.1117827121665,21.5943809503201,-46.5529633361353));
#20064=CARTESIAN_POINT('Ctrl Pts',(-26.0950361539813,21.5726411074351,-46.5512893765287));
#20065=CARTESIAN_POINT('Ctrl Pts',(-26.0414444605985,21.5048783298875,-46.5460723807065));
#20066=CARTESIAN_POINT('Ctrl Pts',(-26.0036113124238,21.4596486788763,-46.5425911882753));
#20067=CARTESIAN_POINT('Ctrl Pts',(-25.9096322750607,21.3533638718184,-46.5343430910105));
#20068=CARTESIAN_POINT('Ctrl Pts',(-25.8523286069484,21.2933875014658,-46.529631358699));
#20069=CARTESIAN_POINT('Ctrl Pts',(-25.6313768652727,21.0793134772969,-46.5123087205326));
#20070=CARTESIAN_POINT('Ctrl Pts',(-25.4540760963841,20.9402578623714,-46.4999710028688));
#20071=CARTESIAN_POINT('Ctrl Pts',(-25.1647515816971,20.7586268058148,-46.480232414632));
#20072=CARTESIAN_POINT('Ctrl Pts',(-25.0624533198982,20.7019152393474,-46.4733286565222));
#20073=CARTESIAN_POINT('Ctrl Pts',(-24.9477683123053,20.6462587868321,-46.46557181216));
#20074=CARTESIAN_POINT('Ctrl Pts',(-24.9382048182414,20.641675822494,-46.4649248879337));
#20075=CARTESIAN_POINT('Ctrl Pts',(-24.9247395316761,20.6353045958309,-46.4640138443326));
#20076=CARTESIAN_POINT('Ctrl Pts',(-24.920856448475,20.6334767629851,-46.4637510989049));
#20077=CARTESIAN_POINT('Ctrl Pts',(-24.9141106898126,20.6303178656993,-46.4632946118325));
#20078=CARTESIAN_POINT('Ctrl Pts',(-24.9112496810858,20.6289832376397,-46.4631009938652));
#20079=CARTESIAN_POINT('Ctrl Pts',(-24.9053541469863,20.6262435786964,-46.4627019867332));
#20080=CARTESIAN_POINT('Ctrl Pts',(-24.9023193879799,20.624839063314,-46.4624965800683));
#20081=CARTESIAN_POINT('Ctrl Pts',(-24.895211877587,20.6215630619481,-46.4620154715268));
#20082=CARTESIAN_POINT('Ctrl Pts',(-24.8911374046532,20.6196953475649,-46.461739639836));
#20083=CARTESIAN_POINT('Ctrl Pts',(-24.8825295161465,20.6157712521831,-46.4611568383128));
#20084=CARTESIAN_POINT('Ctrl Pts',(-24.8779952095606,20.6137168646149,-46.460849800539));
#20085=CARTESIAN_POINT('Ctrl Pts',(-24.8658174851728,20.6082333957536,-46.4600250762262));
#20086=CARTESIAN_POINT('Ctrl Pts',(-24.8581654648535,20.6048236155251,-46.4595067270423));
#20087=CARTESIAN_POINT('Ctrl Pts',(-24.6668382433594,20.5204597897077,-46.4465427181176));
#20088=CARTESIAN_POINT('Ctrl Pts',(-24.4760485194764,20.4568268983653,-46.4334923567176));
#20089=CARTESIAN_POINT('Ctrl Pts',(-23.994870006502,20.3448660316377,-46.400426477945));
#20090=CARTESIAN_POINT('Ctrl Pts',(-23.7013880696028,20.3177063706888,-46.3800632280934));
#20091=CARTESIAN_POINT('Ctrl Pts',(-23.4048492154817,20.3307825077523,-46.3612846846083));
#20092=CARTESIAN_POINT('Ctrl Pts',(-23.4014181101811,20.3309393014148,-46.3610676700417));
#20093=CARTESIAN_POINT('Ctrl Pts',(-23.3851072172945,20.3317108038475,-46.3600372895401));
#20094=CARTESIAN_POINT('Ctrl Pts',(-23.3722307023733,20.3323973344564,-46.3592276280347));
#20095=CARTESIAN_POINT('Ctrl Pts',(-23.3557498050453,20.3333752695618,-46.3581964475166));
#20096=CARTESIAN_POINT('Ctrl Pts',(-23.3521415529839,20.3335954671754,-46.3579710000214));
#20097=CARTESIAN_POINT('Ctrl Pts',(-23.3463958206743,20.333955811521,-46.3576125095075));
#20098=CARTESIAN_POINT('Ctrl Pts',(-23.3442581100167,20.3340920181118,-46.3574792446728));
#20099=CARTESIAN_POINT('Ctrl Pts',(-23.3402568265992,20.3343509700358,-46.3572300168982));
#20100=CARTESIAN_POINT('Ctrl Pts',(-23.3383932374804,20.3344732031463,-46.3571140259975));
#20101=CARTESIAN_POINT('Ctrl Pts',(-23.3342020895015,20.3347517603026,-46.3568533598662));
#20102=CARTESIAN_POINT('Ctrl Pts',(-23.3318745983783,20.3349089913061,-46.356708736798));
#20103=CARTESIAN_POINT('Ctrl Pts',(-23.3249618985641,20.33538351137,-46.3562795955888));
#20104=CARTESIAN_POINT('Ctrl Pts',(-23.3203771708225,20.3357080839843,-46.3559954881318));
#20105=CARTESIAN_POINT('Ctrl Pts',(-23.2833307072301,20.3384104251202,-46.3537038177598));
#20106=CARTESIAN_POINT('Ctrl Pts',(-23.2509045004983,20.3412701488556,-46.3517229846406));
#20107=CARTESIAN_POINT('Ctrl Pts',(-23.1371835504187,20.3530382792884,-46.3448466603966));
#20108=CARTESIAN_POINT('Ctrl Pts',(-23.0561843632333,20.3645494995546,-46.3400756755157));
#20109=CARTESIAN_POINT('Ctrl Pts',(-22.5970652321221,20.4477332922677,-46.3133200499539));
#20110=CARTESIAN_POINT('Ctrl Pts',(-22.2337909285373,20.5835788628724,-46.2928407818915));
#20111=CARTESIAN_POINT('Ctrl Pts',(-21.8859916640033,20.7904073239977,-46.2683612263381));
#20112=CARTESIAN_POINT('Ctrl Pts',(-21.8690630352994,20.8006868103224,-46.2671575171404));
#20113=CARTESIAN_POINT('Ctrl Pts',(-21.8469755647055,20.81437911306,-46.2655705002012));
#20114=CARTESIAN_POINT('Ctrl Pts',(-21.8417300264633,20.8176518222342,-46.2651923693094));
#20115=CARTESIAN_POINT('Ctrl Pts',(-21.8336418869733,20.822730433082,-46.2646074082557));
#20116=CARTESIAN_POINT('Ctrl Pts',(-21.830792624352,20.8245257422136,-46.2644009711096));
#20117=CARTESIAN_POINT('Ctrl Pts',(-21.8251195999338,20.8281127274198,-46.263989205737));
#20118=CARTESIAN_POINT('Ctrl Pts',(-21.822295802351,20.8299043393402,-46.2637838800683));
#20119=CARTESIAN_POINT('Ctrl Pts',(-21.8161052162796,20.833845602083,-46.2633329402335));
#20120=CARTESIAN_POINT('Ctrl Pts',(-21.8127396292087,20.8359971214083,-46.2630872566405));
#20121=CARTESIAN_POINT('Ctrl Pts',(-21.8031235571604,20.8421696035595,-46.2623837873306));
#20122=CARTESIAN_POINT('Ctrl Pts',(-21.7968830003237,20.8462059188769,-46.2619254283299));
#20123=CARTESIAN_POINT('Ctrl Pts',(-21.7829011138335,20.855317983409,-46.2608943419191));
#20124=CARTESIAN_POINT('Ctrl Pts',(-21.7751676031434,20.8604055569928,-46.2603211724284));
#20125=CARTESIAN_POINT('Ctrl Pts',(-21.6320767873944,20.9554252220369,-46.2496622784904));
#20126=CARTESIAN_POINT('Ctrl Pts',(-21.5037131776303,21.0554201105109,-46.2391872215998));
#20127=CARTESIAN_POINT('Ctrl Pts',(-21.152563576092,21.3743634760058,-46.2077409502529));
#20128=CARTESIAN_POINT('Ctrl Pts',(-20.9533618697632,21.6164609730973,-46.1859974222693));
#20129=CARTESIAN_POINT('Ctrl Pts',(-20.7890506496034,21.8883514133137,-46.165646234025));
#20130=CARTESIAN_POINT('Ctrl Pts',(-20.7860660085806,21.8933204185877,-46.1652756175016));
#20131=CARTESIAN_POINT('Ctrl Pts',(-20.7810807664614,21.9016711007082,-46.1646550171362));
#20132=CARTESIAN_POINT('Ctrl Pts',(-20.7790729256724,21.9050484132058,-46.1644046369155));
#20133=CARTESIAN_POINT('Ctrl Pts',(-20.7654705597469,21.9280239858796,-46.1627055238305));
#20134=CARTESIAN_POINT('Ctrl Pts',(-20.7540774627416,21.9477416452648,-46.1612680897028));
#20135=CARTESIAN_POINT('Ctrl Pts',(-20.740854581943,21.9711964949647,-46.1595841013725));
#20136=CARTESIAN_POINT('Ctrl Pts',(-20.7388222086184,21.9748178786069,-46.1593248206375));
#20137=CARTESIAN_POINT('Ctrl Pts',(-20.735591706771,21.9806003063442,-46.1589119810952));
#20138=CARTESIAN_POINT('Ctrl Pts',(-20.734389062758,21.9827588021015,-46.1587581326101));
#20139=CARTESIAN_POINT('Ctrl Pts',(-20.7322711086601,21.9865703925111,-46.158486917287));
#20140=CARTESIAN_POINT('Ctrl Pts',(-20.7313547692201,21.9882229104134,-46.1583694836743));
#20141=CARTESIAN_POINT('Ctrl Pts',(-20.7294511441487,21.9916630204107,-46.1581253348545));
#20142=CARTESIAN_POINT('Ctrl Pts',(-20.7284641060033,21.9934507416918,-46.1579986358084));
#20143=CARTESIAN_POINT('Ctrl Pts',(-20.7259048522426,21.9980964866438,-46.1576698416296));
#20144=CARTESIAN_POINT('Ctrl Pts',(-20.7243352703738,22.000955970346,-46.1574679167065));
#20145=CARTESIAN_POINT('Ctrl Pts',(-20.7176567159525,22.013166958621,-46.1566075237079));
#20146=CARTESIAN_POINT('Ctrl Pts',(-20.7125897236506,22.0225415283679,-46.1559517258786));
#20147=CARTESIAN_POINT('Ctrl Pts',(-20.6320264091037,22.173377516649,-46.1454730549811));
#20148=CARTESIAN_POINT('Ctrl Pts',(-20.5671326875692,22.3202769682032,-46.1362912286893));
#20149=CARTESIAN_POINT('Ctrl Pts',(-20.4105962454914,22.7609113210053,-46.1099589024377));
#20150=CARTESIAN_POINT('Ctrl Pts',(-20.3496821334957,23.0635901017848,-46.0931842016818));
#20151=CARTESIAN_POINT('Ctrl Pts',(-20.3324041733085,23.3725601936962,-46.0746639114791));
#20152=CARTESIAN_POINT('Ctrl Pts',(-20.332280905291,23.374806710498,-46.074529188141));
#20153=CARTESIAN_POINT('Ctrl Pts',(-20.3316531963427,23.3864697303183,-46.0738294305091));
#20154=CARTESIAN_POINT('Ctrl Pts',(-20.3311877386212,23.3958882135158,-46.073263231291));
#20155=CARTESIAN_POINT('Ctrl Pts',(-20.3294508462794,23.4344679791359,-46.0709392789465));
#20156=CARTESIAN_POINT('Ctrl Pts',(-20.3285343119595,23.4636431461924,-46.0691708247247));
#20157=CARTESIAN_POINT('Ctrl Pts',(-20.3278993798856,23.4992695901027,-46.066996668511));
#20158=CARTESIAN_POINT('Ctrl Pts',(-20.327803871908,23.5057134545317,-46.0666028378809));
#20159=CARTESIAN_POINT('Ctrl Pts',(-20.3276782847574,23.5163370966136,-46.0659525726295));
#20160=CARTESIAN_POINT('Ctrl Pts',(-20.3276370075518,23.5205167442933,-46.0656964898248));
#20161=CARTESIAN_POINT('Ctrl Pts',(-20.3275772848037,23.5280478438802,-46.0652346127475));
#20162=CARTESIAN_POINT('Ctrl Pts',(-20.3275559357436,23.5313992721643,-46.0650289099322));
#20163=CARTESIAN_POINT('Ctrl Pts',(-20.3275219270339,23.5384694318735,-46.0645946156991));
#20164=CARTESIAN_POINT('Ctrl Pts',(-20.3275104760203,23.5421881618024,-46.0643659866316));
#20165=CARTESIAN_POINT('Ctrl Pts',(-20.3274971164855,23.5520956537011,-46.0637563302126));
#20166=CARTESIAN_POINT('Ctrl Pts',(-20.3275065982229,23.5582843928995,-46.0633749457714));
#20167=CARTESIAN_POINT('Ctrl Pts',(-20.3275666074314,23.5718839702037,-46.0625356163095));
#20168=CARTESIAN_POINT('Ctrl Pts',(-20.3276248716612,23.5792947232415,-46.0620774300091));
#20169=CARTESIAN_POINT('Ctrl Pts',(-20.3278735737933,23.6012808888444,-46.0607156373471));
#20170=CARTESIAN_POINT('Ctrl Pts',(-20.3281373368476,23.6158551340316,-46.0598097342772));
#20171=CARTESIAN_POINT('Ctrl Pts',(-20.3294024548483,23.6666930435857,-46.0566383627491));
#20172=CARTESIAN_POINT('Ctrl Pts',(-20.3309172057724,23.7029401094892,-46.0543569176981));
#20173=CARTESIAN_POINT('Ctrl Pts',(-20.3407692351601,23.8707326214571,-46.0436984142799));
#20174=CARTESIAN_POINT('Ctrl Pts',(-20.356558828979,24.0016986909128,-46.0350940231204));
#20175=CARTESIAN_POINT('Ctrl Pts',(-20.4368313216917,24.4396162249895,-46.0054450394432));
#20176=CARTESIAN_POINT('Ctrl Pts',(-20.5380114740334,24.7380074249844,-45.9835919345037));
#20177=CARTESIAN_POINT('Ctrl Pts',(-20.687931905263,25.0312969865993,-45.9627509634836));
#20178=CARTESIAN_POINT('Ctrl Pts',(-20.6952982755937,25.0454475913818,-45.9617475911628));
#20179=CARTESIAN_POINT('Ctrl Pts',(-20.7044394368102,25.0626936395594,-45.9605279244867));
#20180=CARTESIAN_POINT('Ctrl Pts',(-20.7061145143444,25.0658412669197,-45.9603054504141));
#20181=CARTESIAN_POINT('Ctrl Pts',(-20.7088875809531,25.0710313309255,-45.9599388414944));
#20182=CARTESIAN_POINT('Ctrl Pts',(-20.7099825507154,25.0730753627264,-45.9597945154271));
#20183=CARTESIAN_POINT('Ctrl Pts',(-20.7119628986108,25.0767626054331,-45.9595342710988));
#20184=CARTESIAN_POINT('Ctrl Pts',(-20.7128474959311,25.0784062247432,-45.9594183033958));
#20185=CARTESIAN_POINT('Ctrl Pts',(-20.7147551199263,25.0819433040308,-45.9591688231514));
#20186=CARTESIAN_POINT('Ctrl Pts',(-20.7157786126209,25.0838365027771,-45.9590353414224));
#20187=CARTESIAN_POINT('Ctrl Pts',(-20.7185927253908,25.089029448095,-45.9586693439844));
#20188=CARTESIAN_POINT('Ctrl Pts',(-20.7203872233828,25.0923271064922,-45.9584370767283));
#20189=CARTESIAN_POINT('Ctrl Pts',(-20.7298195061279,25.1095884254356,-45.9572220442659));
#20190=CARTESIAN_POINT('Ctrl Pts',(-20.7375550676699,25.1234988193722,-45.9562454642447));
#20191=CARTESIAN_POINT('Ctrl Pts',(-20.8352549962929,25.296162590281,-45.9441486338051));
#20192=CARTESIAN_POINT('Ctrl Pts',(-20.9384566120151,25.4470803951999,-45.9338310820955));
#20193=CARTESIAN_POINT('Ctrl Pts',(-21.194929451784,25.7612022840765,-45.9111133885398));
#20194=CARTESIAN_POINT('Ctrl Pts',(-21.3534990623299,25.9188201340518,-45.8987894029577));
#20195=CARTESIAN_POINT('Ctrl Pts',(-21.5984024774316,26.1163386873029,-45.8804187559971));
#20196=CARTESIAN_POINT('Ctrl Pts',(-21.6721554302956,26.1707993491951,-45.8749664249813));
#20197=CARTESIAN_POINT('Ctrl Pts',(-21.7557289257133,26.2271699278189,-45.8688296711048));
#20198=CARTESIAN_POINT('Ctrl Pts',(-21.7633560397364,26.2322671928011,-45.8682700022821));
#20199=CARTESIAN_POINT('Ctrl Pts',(-21.7747420577831,26.2398064372527,-45.8674350409187));
#20200=CARTESIAN_POINT('Ctrl Pts',(-21.7784845075419,26.2422732823821,-45.8671606840082));
#20201=CARTESIAN_POINT('Ctrl Pts',(-21.7849133788009,26.2464916758612,-45.8666895275101));
#20202=CARTESIAN_POINT('Ctrl Pts',(-21.7875972983359,26.2482470415996,-45.8664928713735));
#20203=CARTESIAN_POINT('Ctrl Pts',(-21.7929887513667,26.2517617385734,-45.8660979106451));
#20204=CARTESIAN_POINT('Ctrl Pts',(-21.7956963171346,26.2535210123184,-45.8658996042491));
#20205=CARTESIAN_POINT('Ctrl Pts',(-21.801990469728,26.2575972746609,-45.86543870387));
#20206=CARTESIAN_POINT('Ctrl Pts',(-21.8055790202991,26.2599112063128,-45.8651759961366));
#20207=CARTESIAN_POINT('Ctrl Pts',(-21.8165165246988,26.2669330783378,-45.8643754982902));
#20208=CARTESIAN_POINT('Ctrl Pts',(-21.8238799689431,26.2716182745962,-45.8638368625392));
#20209=CARTESIAN_POINT('Ctrl Pts',(-21.8408017527841,26.2822889120907,-45.8625996375618));
#20210=CARTESIAN_POINT('Ctrl Pts',(-21.8503726200641,26.2882541807357,-45.8619003079741));
#20211=CARTESIAN_POINT('Ctrl Pts',(-21.8818567176964,26.307648677063,-45.8596011239976));
#20212=CARTESIAN_POINT('Ctrl Pts',(-21.9038988640269,26.3208657551258,-45.8579935210221));
#20213=CARTESIAN_POINT('Ctrl Pts',(-21.975021736893,26.3623645755398,-45.8528118381749));
#20214=CARTESIAN_POINT('Ctrl Pts',(-22.0246856347003,26.3896134432406,-45.8492016664255));
#20215=CARTESIAN_POINT('Ctrl Pts',(-22.0750360214967,26.415536777723,-45.8455485119974));
#20216=CARTESIAN_POINT('Origin',(-23.5502525316942,23.5502525316942,-77.3107734492734));
#20217=CARTESIAN_POINT('',(-22.0750358850059,26.4155367074495,-44.3469709746179));
#20218=CARTESIAN_POINT('',(-22.0750360439056,26.4155367892604,-44.590879968079));
#20219=CARTESIAN_POINT('',(-22.0750360153461,26.4155367745563,-77.3107734492734));
#20220=CARTESIAN_POINT('Ctrl Pts',(-22.0750358850059,26.4155367074495,-44.3469709746179));
#20221=CARTESIAN_POINT('Ctrl Pts',(-22.0169725835823,26.3856423083017,-44.3513892165499));
#20222=CARTESIAN_POINT('Ctrl Pts',(-21.9598136445485,26.3539807650537,-44.3557997793458));
#20223=CARTESIAN_POINT('Ctrl Pts',(-21.8457511816202,26.2861852140145,-44.3646822062245));
#20224=CARTESIAN_POINT('Ctrl Pts',(-21.7889519536985,26.2499698889702,-44.3691484126009));
#20225=CARTESIAN_POINT('Ctrl Pts',(-21.7045223056156,26.1923376455813,-44.3758098838951));
#20226=CARTESIAN_POINT('Ctrl Pts',(-21.6760380971063,26.1722087258025,-44.378061292946));
#20227=CARTESIAN_POINT('Ctrl Pts',(-21.6336792693039,26.1412319255837,-44.3814088395849));
#20228=CARTESIAN_POINT('Ctrl Pts',(-21.619558463127,26.1307268553778,-44.3825246902981));
#20229=CARTESIAN_POINT('Ctrl Pts',(-21.5968111644351,26.1135129116554,-44.3843211214563));
#20230=CARTESIAN_POINT('Ctrl Pts',(-21.5881317034422,26.1068750721422,-44.3850063044345));
#20231=CARTESIAN_POINT('Ctrl Pts',(-21.5775463190195,26.0986939712461,-44.3858414490104));
#20232=CARTESIAN_POINT('Ctrl Pts',(-21.5756083192604,26.0971926186904,-44.3859943289051));
#20233=CARTESIAN_POINT('Ctrl Pts',(-21.5718604427551,26.0942823203659,-44.386289938722));
#20234=CARTESIAN_POINT('Ctrl Pts',(-21.5700503541546,26.0928736515963,-44.3864326881218));
#20235=CARTESIAN_POINT('Ctrl Pts',(-21.5667712732047,26.0903161406334,-44.3866912493087));
#20236=CARTESIAN_POINT('Ctrl Pts',(-21.5653017789302,26.0891679594687,-44.3868071075507));
#20237=CARTESIAN_POINT('Ctrl Pts',(-21.5623470792556,26.0868551881438,-44.3870400345603));
#20238=CARTESIAN_POINT('Ctrl Pts',(-21.5608619062647,26.0856905735403,-44.3871571006709));
#20239=CARTESIAN_POINT('Ctrl Pts',(-21.5566207499223,26.0823588037863,-44.3874913646555));
#20240=CARTESIAN_POINT('Ctrl Pts',(-21.5538672678695,26.0801884465189,-44.3877083331261));
#20241=CARTESIAN_POINT('Ctrl Pts',(-21.542051182748,26.0708434367121,-44.3886392464672));
#20242=CARTESIAN_POINT('Ctrl Pts',(-21.5330235263869,26.0636244337569,-44.3893500499413));
#20243=CARTESIAN_POINT('Ctrl Pts',(-21.3807514102762,25.9405104582887,-44.4013358768773));
#20244=CARTESIAN_POINT('Ctrl Pts',(-21.2476429511839,25.8125696518064,-44.4117698133184));
#20245=CARTESIAN_POINT('Ctrl Pts',(-21.0203755581141,25.5531561303944,-44.4310985593496));
#20246=CARTESIAN_POINT('Ctrl Pts',(-20.9237427157361,25.4246444288825,-44.4399938590089));
#20247=CARTESIAN_POINT('Ctrl Pts',(-20.7771734304109,25.1959975505793,-44.4554736952566));
#20248=CARTESIAN_POINT('Ctrl Pts',(-20.7221314649247,25.0995013974687,-44.4619106121795));
#20249=CARTESIAN_POINT('Ctrl Pts',(-20.6499203943485,24.9561823371162,-44.4714712458676));
#20250=CARTESIAN_POINT('Ctrl Pts',(-20.6286808613619,24.9114959663492,-44.4744516673446));
#20251=CARTESIAN_POINT('Ctrl Pts',(-20.6052686809462,24.8591640967576,-44.4779475402239));
#20252=CARTESIAN_POINT('Ctrl Pts',(-20.6020845226447,24.8519762946386,-44.4784278149744));
#20253=CARTESIAN_POINT('Ctrl Pts',(-20.5972582622911,24.8409731289868,-44.4791632265973));
#20254=CARTESIAN_POINT('Ctrl Pts',(-20.5955971681179,24.837166086536,-44.4794177122683));
#20255=CARTESIAN_POINT('Ctrl Pts',(-20.5927369571064,24.8305760733751,-44.4798582961328));
#20256=CARTESIAN_POINT('Ctrl Pts',(-20.5915343940823,24.8277945965112,-44.4800442761707));
#20257=CARTESIAN_POINT('Ctrl Pts',(-20.5890508247112,24.8220278914376,-44.4804299047371));
#20258=CARTESIAN_POINT('Ctrl Pts',(-20.5877704057644,24.8190424152076,-44.4806295730832));
#20259=CARTESIAN_POINT('Ctrl Pts',(-20.5846738382919,24.8117920923489,-44.4811145368752));
#20260=CARTESIAN_POINT('Ctrl Pts',(-20.5828623768827,24.8075252621059,-44.4813999918641));
#20261=CARTESIAN_POINT('Ctrl Pts',(-20.5761212339426,24.791551025848,-44.4824688916757));
#20262=CARTESIAN_POINT('Ctrl Pts',(-20.5712516310859,24.7798185342348,-44.4832543778021));
#20263=CARTESIAN_POINT('Ctrl Pts',(-20.4912583821253,24.5838233616141,-44.4963840561369));
#20264=CARTESIAN_POINT('Ctrl Pts',(-20.4333040942262,24.3930571740781,-44.5093206099543));
#20265=CARTESIAN_POINT('Ctrl Pts',(-20.3524421671249,23.9990788085523,-44.5362338522077));
#20266=CARTESIAN_POINT('Ctrl Pts',(-20.3305052907613,23.7965474741878,-44.5501644929574));
#20267=CARTESIAN_POINT('Ctrl Pts',(-20.3267885178811,23.518331513674,-44.5686561212443));
#20268=CARTESIAN_POINT('Ctrl Pts',(-20.328403499623,23.4433422847134,-44.5735718142303));
#20269=CARTESIAN_POINT('Ctrl Pts',(-20.3343556287385,23.337986095886,-44.5803225269693));
#20270=CARTESIAN_POINT('Ctrl Pts',(-20.3365112127802,23.3075246309403,-44.5822559232885));
#20271=CARTESIAN_POINT('Ctrl Pts',(-20.3394819250748,23.272601618811,-44.5844478065109));
#20272=CARTESIAN_POINT('Ctrl Pts',(-20.3398737707547,23.2681069493158,-44.5847294365413));
#20273=CARTESIAN_POINT('Ctrl Pts',(-20.340482678102,23.2612880034529,-44.5851559737254));
#20274=CARTESIAN_POINT('Ctrl Pts',(-20.3406928264419,23.2589631393118,-44.5853012694923));
#20275=CARTESIAN_POINT('Ctrl Pts',(-20.3410594766465,23.2549554707227,-44.5855515104033));
#20276=CARTESIAN_POINT('Ctrl Pts',(-20.3412147760544,23.2532725631549,-44.5856565237815));
#20277=CARTESIAN_POINT('Ctrl Pts',(-20.3415400683596,23.2497775699289,-44.5858744689852));
#20278=CARTESIAN_POINT('Ctrl Pts',(-20.3417102720206,23.2479655109107,-44.585987388419));
#20279=CARTESIAN_POINT('Ctrl Pts',(-20.3421812947833,23.2429960245115,-44.5862968496949));
#20280=CARTESIAN_POINT('Ctrl Pts',(-20.3424852411559,23.2398388846685,-44.5864932139865));
#20281=CARTESIAN_POINT('Ctrl Pts',(-20.3436698665765,23.2277215492746,-44.5872459784305));
#20282=CARTESIAN_POINT('Ctrl Pts',(-20.3445834420388,23.2187645001618,-44.5878005351652));
#20283=CARTESIAN_POINT('Ctrl Pts',(-20.3604344347574,23.0695523827211,-44.5970090696813));
#20284=CARTESIAN_POINT('Ctrl Pts',(-20.3845284698873,22.9304021272233,-44.6051627393486));
#20285=CARTESIAN_POINT('Ctrl Pts',(-20.4611659485258,22.6132605091413,-44.6236419392076));
#20286=CARTESIAN_POINT('Ctrl Pts',(-20.5200967300328,22.4373427113619,-44.6338291931138));
#20287=CARTESIAN_POINT('Ctrl Pts',(-20.6447837179472,22.1499782549216,-44.6515709118009));
#20288=CARTESIAN_POINT('Ctrl Pts',(-20.7027093526818,22.035653608662,-44.6589470228328));
#20289=CARTESIAN_POINT('Ctrl Pts',(-20.7944915476084,21.8784836360213,-44.6697662252125));
#20290=CARTESIAN_POINT('Ctrl Pts',(-20.8228701544828,21.8325754143647,-44.6730131888152));
#20291=CARTESIAN_POINT('Ctrl Pts',(-20.8567293212722,21.7807573199098,-44.6767871793769));
#20292=CARTESIAN_POINT('Ctrl Pts',(-20.8610964573364,21.7741274810356,-44.6772721269792));
#20293=CARTESIAN_POINT('Ctrl Pts',(-20.8678233221934,21.7639969730188,-44.6780163655331));
#20294=CARTESIAN_POINT('Ctrl Pts',(-20.870165528338,21.7604846587409,-44.6782749957575));
#20295=CARTESIAN_POINT('Ctrl Pts',(-20.8742059589771,21.7544514452565,-44.6787202868754));
#20296=CARTESIAN_POINT('Ctrl Pts',(-20.8759008651161,21.7519283215563,-44.6789068221031));
#20297=CARTESIAN_POINT('Ctrl Pts',(-20.8793990565683,21.7467366182383,-44.6792912911707));
#20298=CARTESIAN_POINT('Ctrl Pts',(-20.8812027774441,21.7440683370753,-44.679489241399));
#20299=CARTESIAN_POINT('Ctrl Pts',(-20.8855552043637,21.737650459634,-44.6799662115031));
#20300=CARTESIAN_POINT('Ctrl Pts',(-20.8881078239687,21.7339035363958,-44.68024537993));
#20301=CARTESIAN_POINT('Ctrl Pts',(-20.8959675968225,21.7224185428511,-44.6811032444338));
#20302=CARTESIAN_POINT('Ctrl Pts',(-20.901300609268,21.7146983058699,-44.6816829256186));
#20303=CARTESIAN_POINT('Ctrl Pts',(-20.9211038172643,21.686296601531,-44.6838267653367));
#20304=CARTESIAN_POINT('Ctrl Pts',(-20.9357828222693,21.6657624807298,-44.6853989184963));
#20305=CARTESIAN_POINT('Ctrl Pts',(-20.9542715158919,21.6405309247524,-44.6873588722853));
#20306=CARTESIAN_POINT('Ctrl Pts',(-20.9578555196447,21.6356685608166,-44.6877378858872));
#20307=CARTESIAN_POINT('Ctrl Pts',(-20.9655423139584,21.6253011579772,-44.6885488247335));
#20308=CARTESIAN_POINT('Ctrl Pts',(-20.969649063141,21.6197991036727,-44.6889809020956));
#20309=CARTESIAN_POINT('Ctrl Pts',(-20.9746559402539,21.6131356226268,-44.6895062687476));
#20310=CARTESIAN_POINT('Ctrl Pts',(-20.9755393451414,21.6119616019797,-44.6895989104087));
#20311=CARTESIAN_POINT('Ctrl Pts',(-20.9803379865793,21.6055934094242,-44.6901018505671));
#20312=CARTESIAN_POINT('Ctrl Pts',(-20.9842681165415,21.6004105249615,-44.6905127243629));
#20313=CARTESIAN_POINT('Ctrl Pts',(-20.9938355216162,21.5878724689794,-44.6915104445947));
#20314=CARTESIAN_POINT('Ctrl Pts',(-20.9994888587572,21.5805296776051,-44.6920979084727));
#20315=CARTESIAN_POINT('Ctrl Pts',(-21.0115392127134,21.5650170510399,-44.6933457380659));
#20316=CARTESIAN_POINT('Ctrl Pts',(-21.0179441632385,21.5568535368391,-44.6940064042516));
#20317=CARTESIAN_POINT('Ctrl Pts',(-21.1655203930636,21.370617378989,-44.7091703636432));
#20318=CARTESIAN_POINT('Ctrl Pts',(-21.325072060825,21.2079681044509,-44.7244178380066));
#20319=CARTESIAN_POINT('Ctrl Pts',(-21.6011512445853,20.9803922731512,-44.7486365336156));
#20320=CARTESIAN_POINT('Ctrl Pts',(-21.7068996069316,20.9035128708808,-44.7574831994809));
#20321=CARTESIAN_POINT('Ctrl Pts',(-21.8826383657212,20.7914054261341,-44.77124045892));
#20322=CARTESIAN_POINT('Ctrl Pts',(-21.9497514008328,20.7519364721087,-44.7762909336431));
#20323=CARTESIAN_POINT('Ctrl Pts',(-22.0251503160503,20.7111958925188,-44.7816925579985));
#20324=CARTESIAN_POINT('Ctrl Pts',(-22.032080627332,20.7074839093075,-44.7821865720227));
#20325=CARTESIAN_POINT('Ctrl Pts',(-22.0441484950789,20.7010768879566,-44.7830424173952));
#20326=CARTESIAN_POINT('Ctrl Pts',(-22.0492798375856,20.6983703127437,-44.7834049562671));
#20327=CARTESIAN_POINT('Ctrl Pts',(-22.0567103316646,20.6944766381837,-44.7839279215447));
#20328=CARTESIAN_POINT('Ctrl Pts',(-22.0590036104428,20.6932784484719,-44.7840890481928));
#20329=CARTESIAN_POINT('Ctrl Pts',(-22.062984728058,20.6912044980877,-44.7843682803339));
#20330=CARTESIAN_POINT('Ctrl Pts',(-22.0646719011601,20.6903274682601,-44.7844864669854));
#20331=CARTESIAN_POINT('Ctrl Pts',(-22.067931737407,20.6886365964423,-44.7847145276506));
#20332=CARTESIAN_POINT('Ctrl Pts',(-22.0695042914533,20.6878225592538,-44.7848244142156));
#20333=CARTESIAN_POINT('Ctrl Pts',(-22.0732479999372,20.6858885283004,-44.7850857076161));
#20334=CARTESIAN_POINT('Ctrl Pts',(-22.0754197623772,20.6847697044188,-44.785237039787));
#20335=CARTESIAN_POINT('Ctrl Pts',(-22.0831141387008,20.6808168678289,-44.7857723315915));
#20336=CARTESIAN_POINT('Ctrl Pts',(-22.0886437118507,20.6779963187962,-44.7861554423007));
#20337=CARTESIAN_POINT('Ctrl Pts',(-22.1638078244865,20.6399295444725,-44.791342197598));
#20338=CARTESIAN_POINT('Ctrl Pts',(-22.2346990471095,20.6072047560611,-44.7959910189264));
#20339=CARTESIAN_POINT('Ctrl Pts',(-22.5189449489731,20.4883180115178,-44.8139564299608));
#20340=CARTESIAN_POINT('Ctrl Pts',(-22.7400850737778,20.4225240380272,-44.8265131305272));
#20341=CARTESIAN_POINT('Ctrl Pts',(-23.1511896439697,20.346787719161,-44.8500639281638));
#20342=CARTESIAN_POINT('Ctrl Pts',(-23.3386130698037,20.3289745934403,-44.86087323742));
#20343=CARTESIAN_POINT('Ctrl Pts',(-23.5397374249775,20.3274925182272,-44.8730418676754));
#20344=CARTESIAN_POINT('Ctrl Pts',(-23.5529702745348,20.3274765112967,-44.8738449734727));
#20345=CARTESIAN_POINT('Ctrl Pts',(-23.5761381853061,20.3275911762619,-44.8752555394141));
#20346=CARTESIAN_POINT('Ctrl Pts',(-23.5860733049993,20.3276862953566,-44.8758618821446));
#20347=CARTESIAN_POINT('Ctrl Pts',(-23.6005710137762,20.32789214829,-44.8767488451523));
#20348=CARTESIAN_POINT('Ctrl Pts',(-23.6051341267267,20.3279666349496,-44.8770283271636));
#20349=CARTESIAN_POINT('Ctrl Pts',(-23.6130987171833,20.328113569023,-44.8775166949268));
#20350=CARTESIAN_POINT('Ctrl Pts',(-23.616500274885,20.3281817109063,-44.8777254451794));
#20351=CARTESIAN_POINT('Ctrl Pts',(-23.6230732227454,20.3283237968118,-44.8781291624373));
#20352=CARTESIAN_POINT('Ctrl Pts',(-23.6262446256737,20.3283970372255,-44.8783241071151));
#20353=CARTESIAN_POINT('Ctrl Pts',(-23.6337659677475,20.3285818466368,-44.8787868077373));
#20354=CARTESIAN_POINT('Ctrl Pts',(-23.6381157915674,20.3286975431467,-44.8790546930827));
#20355=CARTESIAN_POINT('Ctrl Pts',(-23.6511131829695,20.3290695909416,-44.8798560196478));
#20356=CARTESIAN_POINT('Ctrl Pts',(-23.6597599143415,20.3293519527296,-44.8803902770197));
#20357=CARTESIAN_POINT('Ctrl Pts',(-23.7419484046763,20.3323671830337,-44.8854796878124));
#20358=CARTESIAN_POINT('Ctrl Pts',(-23.8153720750082,20.3375832969437,-44.8901124887298));
#20359=CARTESIAN_POINT('Ctrl Pts',(-23.9282473178351,20.3494977651845,-44.8973765586769));
#20360=CARTESIAN_POINT('Ctrl Pts',(-23.9678636276213,20.3544252694393,-44.8999530840359));
#20361=CARTESIAN_POINT('Ctrl Pts',(-24.3032778109199,20.4024873528457,-44.9219952892521));
#20362=CARTESIAN_POINT('Ctrl Pts',(-24.591830282267,20.4858535029736,-44.9426587130554));
#20363=CARTESIAN_POINT('Ctrl Pts',(-24.9293705036529,20.6366345390483,-44.967181020467));
#20364=CARTESIAN_POINT('Ctrl Pts',(-24.9930874681241,20.6676555986252,-44.971816987828));
#20365=CARTESIAN_POINT('Ctrl Pts',(-25.0818483779472,20.7145508534923,-44.9782345107791));
#20366=CARTESIAN_POINT('Ctrl Pts',(-25.1077724517435,20.7287065555354,-44.9801037353328));
#20367=CARTESIAN_POINT('Ctrl Pts',(-25.1373969822194,20.7454156237942,-44.9822306440995));
#20368=CARTESIAN_POINT('Ctrl Pts',(-25.1412900464867,20.7476221219093,-44.9825099651054));
#20369=CARTESIAN_POINT('Ctrl Pts',(-25.1472002051788,20.7509881455452,-44.9829337150519));
#20370=CARTESIAN_POINT('Ctrl Pts',(-25.1492206403128,20.7521417470552,-44.9830785249679));
#20371=CARTESIAN_POINT('Ctrl Pts',(-25.1528601753934,20.7542250302901,-44.9833392830459));
#20372=CARTESIAN_POINT('Ctrl Pts',(-25.1544797128154,20.7551539288429,-44.9834552815724));
#20373=CARTESIAN_POINT('Ctrl Pts',(-25.1577186438274,20.7570153858573,-44.9836871982694));
#20374=CARTESIAN_POINT('Ctrl Pts',(-25.1593380270245,20.7579479417004,-44.9838031158737));
#20375=CARTESIAN_POINT('Ctrl Pts',(-25.1639132901304,20.7605880049193,-44.9841305233886));
#20376=CARTESIAN_POINT('Ctrl Pts',(-25.166867280788,20.7622988074491,-44.9843417987758));
#20377=CARTESIAN_POINT('Ctrl Pts',(-25.1791574988787,20.7694427837216,-44.9852203717435));
#20378=CARTESIAN_POINT('Ctrl Pts',(-25.1884692386814,20.7749182679858,-44.9858849476514));
#20379=CARTESIAN_POINT('Ctrl Pts',(-25.31484519532,20.8500874505381,-44.9948921019625));
#20380=CARTESIAN_POINT('Ctrl Pts',(-25.4274194536192,20.9270992391841,-45.0027740407067));
#20381=CARTESIAN_POINT('Ctrl Pts',(-25.5948174109338,21.0579291798846,-45.0148168165361));
#20382=CARTESIAN_POINT('Ctrl Pts',(-25.6531609486468,21.1069559954136,-45.0190814707401));
#20383=CARTESIAN_POINT('Ctrl Pts',(-25.8296936744641,21.2663105592593,-45.0323746359616));
#20384=CARTESIAN_POINT('Ctrl Pts',(-25.941352421998,21.3834852286414,-45.0413739313162));
#20385=CARTESIAN_POINT('Ctrl Pts',(-26.1243003304545,21.6069143806605,-45.0579921632987));
#20386=CARTESIAN_POINT('Ctrl Pts',(-26.1989534783728,21.709963835474,-45.0654782918616));
#20387=CARTESIAN_POINT('Ctrl Pts',(-26.273361661736,21.8266167067517,-45.0738952107026));
#20388=CARTESIAN_POINT('Ctrl Pts',(-26.2793539880419,21.8361203818638,-45.0745804866644));
#20389=CARTESIAN_POINT('Ctrl Pts',(-26.2878108739276,21.8496895412562,-45.0755583473319));
#20390=CARTESIAN_POINT('Ctrl Pts',(-26.2903163693343,21.8537295206943,-45.0758494175754));
#20391=CARTESIAN_POINT('Ctrl Pts',(-26.2946172525071,21.8606988491651,-45.0763514246348));
#20392=CARTESIAN_POINT('Ctrl Pts',(-26.2964169164785,21.8636255609076,-45.0765622034144));
#20393=CARTESIAN_POINT('Ctrl Pts',(-26.2998464221396,21.86922285066,-45.076965250311));
#20394=CARTESIAN_POINT('Ctrl Pts',(-26.3014770628597,21.8718929367649,-45.0771574887376));
#20395=CARTESIAN_POINT('Ctrl Pts',(-26.3052767833891,21.8781351911929,-45.077606850173));
#20396=CARTESIAN_POINT('Ctrl Pts',(-26.3074428045839,21.881709206917,-45.0778640851357));
#20397=CARTESIAN_POINT('Ctrl Pts',(-26.314862400078,21.894005714278,-45.0787489529087));
#20398=CARTESIAN_POINT('Ctrl Pts',(-26.3200815427048,21.9027488168243,-45.0793778442057));
#20399=CARTESIAN_POINT('Ctrl Pts',(-26.3741684089553,21.9943385544905,-45.0859633831031));
#20400=CARTESIAN_POINT('Ctrl Pts',(-26.4193406353654,22.0793006466735,-45.0920532553449));
#20401=CARTESIAN_POINT('Ctrl Pts',(-26.5610097665651,22.3771918997081,-45.113373878517));
#20402=CARTESIAN_POINT('Ctrl Pts',(-26.6381112326239,22.5985017357892,-45.1292230096892));
#20403=CARTESIAN_POINT('Ctrl Pts',(-26.7295860685309,22.995222832459,-45.1567407211548));
#20404=CARTESIAN_POINT('Ctrl Pts',(-26.754857500866,23.1671823410113,-45.1683685278468));
#20405=CARTESIAN_POINT('Ctrl Pts',(-26.7668434730624,23.3508275649975,-45.1799527221918));
#20406=CARTESIAN_POINT('Ctrl Pts',(-26.7674755659971,23.3612986848333,-45.180610329277));
#20407=CARTESIAN_POINT('Ctrl Pts',(-26.7682361194059,23.3750106778657,-45.1814675057145));
#20408=CARTESIAN_POINT('Ctrl Pts',(-26.768410822246,23.3782487663602,-45.1816696387536));
#20409=CARTESIAN_POINT('Ctrl Pts',(-26.7686873488845,23.3835220833069,-45.1819983409278));
#20410=CARTESIAN_POINT('Ctrl Pts',(-26.7687921297576,23.3855571441588,-45.1821250768914));
#20411=CARTESIAN_POINT('Ctrl Pts',(-26.7689904254819,23.3894809248369,-45.1823692104319));
#20412=CARTESIAN_POINT('Ctrl Pts',(-26.7690842078933,23.3913696226442,-45.1824866226049));
#20413=CARTESIAN_POINT('Ctrl Pts',(-26.7692971605752,23.3957358908377,-45.18275782381));
#20414=CARTESIAN_POINT('Ctrl Pts',(-26.7694151332441,23.398213523834,-45.1829115448948));
#20415=CARTESIAN_POINT('Ctrl Pts',(-26.7697753407421,23.4059669233087,-45.1833920628319));
#20416=CARTESIAN_POINT('Ctrl Pts',(-26.7700074691429,23.4112431849558,-45.1837182916079));
#20417=CARTESIAN_POINT('Ctrl Pts',(-26.7719120699812,23.4571016385121,-45.1865472069361));
#20418=CARTESIAN_POINT('Ctrl Pts',(-26.7728302773295,23.4977137980555,-45.1890083205923));
#20419=CARTESIAN_POINT('Ctrl Pts',(-26.7729937518526,23.5419194276276,-45.1916496469392));
#20420=CARTESIAN_POINT('Ctrl Pts',(-26.7730010272996,23.5455041604006,-45.1918635692455));
#20421=CARTESIAN_POINT('Ctrl Pts',(-26.7730321986284,23.6318360839317,-45.1970091952331));
#20422=CARTESIAN_POINT('Ctrl Pts',(-26.7698751374493,23.7145601871732,-45.2018004724637));
#20423=CARTESIAN_POINT('Ctrl Pts',(-26.7412431602374,24.0873058694652,-45.2231168771338));
#20424=CARTESIAN_POINT('Ctrl Pts',(-26.6797358568846,24.3731690499141,-45.2388484144448));
#20425=CARTESIAN_POINT('Ctrl Pts',(-26.5492046359256,24.733873763714,-45.2612377452138));
#20426=CARTESIAN_POINT('Ctrl Pts',(-26.5140030105104,24.8194465797843,-45.2667391947205));
#20427=CARTESIAN_POINT('Ctrl Pts',(-26.4708835928088,24.9126534019564,-45.2729909010341));
#20428=CARTESIAN_POINT('Ctrl Pts',(-26.4665502562231,24.9219046393978,-45.2736142978734));
#20429=CARTESIAN_POINT('Ctrl Pts',(-26.4604096853497,24.9348534994649,-45.2744909679228));
#20430=CARTESIAN_POINT('Ctrl Pts',(-26.4586392109606,24.9385685701141,-45.2747429637209));
#20431=CARTESIAN_POINT('Ctrl Pts',(-26.455382404655,24.9453689110046,-45.2752051131632));
#20432=CARTESIAN_POINT('Ctrl Pts',(-26.4538982594631,24.9484552273224,-45.2754151904567));
#20433=CARTESIAN_POINT('Ctrl Pts',(-26.450884980503,24.9546959260041,-45.2758406531165));
#20434=CARTESIAN_POINT('Ctrl Pts',(-26.4493556142839,24.9578501898577,-45.2760560463556));
#20435=CARTESIAN_POINT('Ctrl Pts',(-26.4455858950721,24.965592897282,-45.2765856309788));
#20436=CARTESIAN_POINT('Ctrl Pts',(-26.4433397831903,24.9701785122659,-45.2769000233911));
#20437=CARTESIAN_POINT('Ctrl Pts',(-26.4351547041232,24.9867889517107,-45.2780415681139));
#20438=CARTESIAN_POINT('Ctrl Pts',(-26.4291516508244,24.99878188371,-45.2788709642983));
#20439=CARTESIAN_POINT('Ctrl Pts',(-26.3409887841099,25.17220118813,-45.2909405528309));
#20440=CARTESIAN_POINT('Ctrl Pts',(-26.2454526735476,25.3264288107428,-45.3026669017893));
#20441=CARTESIAN_POINT('Ctrl Pts',(-25.966591284306,25.7018975621877,-45.3338298404498));
#20442=CARTESIAN_POINT('Ctrl Pts',(-25.765773544799,25.9081609206969,-45.353719126118));
#20443=CARTESIAN_POINT('Ctrl Pts',(-25.5100472888222,26.1089249714982,-45.3746414491687));
#20444=CARTESIAN_POINT('Ctrl Pts',(-25.4793358311925,26.1321584356106,-45.3770892641025));
#20445=CARTESIAN_POINT('Ctrl Pts',(-25.4443795213895,26.1576311034743,-45.3797966903431));
#20446=CARTESIAN_POINT('Ctrl Pts',(-25.4405391491752,26.1604166211963,-45.3800930837598));
#20447=CARTESIAN_POINT('Ctrl Pts',(-25.4347442032644,26.1646003427752,-45.380538730874));
#20448=CARTESIAN_POINT('Ctrl Pts',(-25.4327942150391,26.1660048418496,-45.3806884187287));
#20449=CARTESIAN_POINT('Ctrl Pts',(-25.4294130743251,26.168434403992,-45.380947494078));
#20450=CARTESIAN_POINT('Ctrl Pts',(-25.4279826531968,26.169460475376,-45.3810569518733));
#20451=CARTESIAN_POINT('Ctrl Pts',(-25.4249992995014,26.1715967981597,-45.3812849361929));
#20452=CARTESIAN_POINT('Ctrl Pts',(-25.4234462227242,26.172706840665,-45.3814034477518));
#20453=CARTESIAN_POINT('Ctrl Pts',(-25.4197512798437,26.175342798552,-45.3816849917962));
#20454=CARTESIAN_POINT('Ctrl Pts',(-25.4176085242473,26.1768674779089,-45.381847938076));
#20455=CARTESIAN_POINT('Ctrl Pts',(-25.4104402114887,26.181954890924,-45.3823919754168));
#20456=CARTESIAN_POINT('Ctrl Pts',(-25.4054062658167,26.185505865985,-45.3827722566296));
#20457=CARTESIAN_POINT('Ctrl Pts',(-25.2571892209753,26.2894238691042,-45.3939181881737));
#20458=CARTESIAN_POINT('Ctrl Pts',(-25.1060592960262,26.3780038839481,-45.4038974436268));
#20459=CARTESIAN_POINT('Ctrl Pts',(-24.7383053689803,26.5550913930487,-45.426839197013));
#20460=CARTESIAN_POINT('Ctrl Pts',(-24.517793410645,26.6331710177218,-45.4396595269493));
#20461=CARTESIAN_POINT('Ctrl Pts',(-24.1927260648965,26.7099198296471,-45.4590857302529));
#20462=CARTESIAN_POINT('Ctrl Pts',(-24.0936416790154,26.7284587416941,-45.465064435559));
#20463=CARTESIAN_POINT('Ctrl Pts',(-23.9845534767991,26.7436188609489,-45.4717679415841));
#20464=CARTESIAN_POINT('Ctrl Pts',(-23.9752426270166,26.7448713258039,-45.4723410307475));
#20465=CARTESIAN_POINT('Ctrl Pts',(-23.9614277581929,26.746668192521,-45.473192774146));
#20466=CARTESIAN_POINT('Ctrl Pts',(-23.9569277935016,26.7472438320822,-45.4734704399695));
#20467=CARTESIAN_POINT('Ctrl Pts',(-23.9492303195171,26.748211985072,-45.4739457941239));
#20468=CARTESIAN_POINT('Ctrl Pts',(-23.946033400301,26.7486092104523,-45.4741433332132));
#20469=CARTESIAN_POINT('Ctrl Pts',(-23.9398192647578,26.7493718730358,-45.4745275325132));
#20470=CARTESIAN_POINT('Ctrl Pts',(-23.9368021160454,26.7497378369264,-45.4747141758154));
#20471=CARTESIAN_POINT('Ctrl Pts',(-23.9296790025828,26.7505916094527,-45.4751550627587));
#20472=CARTESIAN_POINT('Ctrl Pts',(-23.925572615267,26.7510757842419,-45.4754094209627));
#20473=CARTESIAN_POINT('Ctrl Pts',(-23.9134349872087,26.7524832260508,-45.4761618254598));
#20474=CARTESIAN_POINT('Ctrl Pts',(-23.9054012356492,26.7533841730794,-45.4766605760629));
#20475=CARTESIAN_POINT('Ctrl Pts',(-23.8871626850371,26.7553600812507,-45.4777945794142));
#20476=CARTESIAN_POINT('Ctrl Pts',(-23.8769560087251,26.7564165464982,-45.4784304118783));
#20477=CARTESIAN_POINT('Ctrl Pts',(-23.7882252624795,26.7651727267044,-45.4839687965563));
#20478=CARTESIAN_POINT('Ctrl Pts',(-23.7094540852722,26.7700345088245,-45.4889602488078));
#20479=CARTESIAN_POINT('Ctrl Pts',(-23.5553034239995,26.7738783643619,-45.4988844937393));
#20480=CARTESIAN_POINT('Ctrl Pts',(-23.4799799534304,26.7731160778694,-45.5038065085097));
#20481=CARTESIAN_POINT('Ctrl Pts',(-23.1046353526768,26.7561532812966,-45.5286669960293));
#20482=CARTESIAN_POINT('Ctrl Pts',(-22.8079168428669,26.7006958470769,-45.5495584711883));
#20483=CARTESIAN_POINT('Ctrl Pts',(-22.5191689055393,26.603611675694,-45.5692877037621));
#20484=CARTESIAN_POINT('Ctrl Pts',(-22.5151564042361,26.6022537626356,-45.5695617087534));
#20485=CARTESIAN_POINT('Ctrl Pts',(-22.5054210655288,26.5989377162579,-45.5702261145347));
#20486=CARTESIAN_POINT('Ctrl Pts',(-22.499701017421,26.5969713674669,-45.5706161539965));
#20487=CARTESIAN_POINT('Ctrl Pts',(-22.4574010109084,26.5822968424369,-45.5734978561477));
#20488=CARTESIAN_POINT('Ctrl Pts',(-22.4210451807522,26.5689456664167,-45.5759599067181));
#20489=CARTESIAN_POINT('Ctrl Pts',(-22.3805065096659,26.5532234584556,-45.5786816308035));
#20490=CARTESIAN_POINT('Ctrl Pts',(-22.3760799120296,26.551495408061,-45.5789785090993));
#20491=CARTESIAN_POINT('Ctrl Pts',(-22.3694186275566,26.5488779897712,-45.5794247626371));
#20492=CARTESIAN_POINT('Ctrl Pts',(-22.3671811123695,26.5479959102805,-45.5795745736815));
#20493=CARTESIAN_POINT('Ctrl Pts',(-22.3633071232243,26.5464636825496,-45.5798338038848));
#20494=CARTESIAN_POINT('Ctrl Pts',(-22.3616701949922,26.5458146979849,-45.5799432935444));
#20495=CARTESIAN_POINT('Ctrl Pts',(-22.3582601318707,26.5444594924763,-45.5801712855241));
#20496=CARTESIAN_POINT('Ctrl Pts',(-22.3564870942583,26.5437530387319,-45.5802897729619));
#20497=CARTESIAN_POINT('Ctrl Pts',(-22.3522745330482,26.5420702369977,-45.5805711579638));
#20498=CARTESIAN_POINT('Ctrl Pts',(-22.3498355668013,26.5410924768471,-45.5807339695857));
#20499=CARTESIAN_POINT('Ctrl Pts',(-22.3416942815873,26.5378171441703,-45.5812770998512));
#20500=CARTESIAN_POINT('Ctrl Pts',(-22.3359972963003,26.5355062198109,-45.5816566123466));
#20501=CARTESIAN_POINT('Ctrl Pts',(-22.2435254400753,26.4976874406595,-45.5878083317032));
#20502=CARTESIAN_POINT('Ctrl Pts',(-22.158354761156,26.4584341573107,-45.5933540196748));
#20503=CARTESIAN_POINT('Ctrl Pts',(-22.075035968613,26.4155367504953,-45.5987738960335));
#20504=CARTESIAN_POINT('',(-26.7730015954251,23.5477959646253,-45.4377814573121));
#20505=CARTESIAN_POINT('Ctrl Pts',(-22.0750360214967,26.415536777723,-45.8455485119974));
#20506=CARTESIAN_POINT('Ctrl Pts',(-22.0932331211949,26.4249057127422,-45.844228227893));
#20507=CARTESIAN_POINT('Ctrl Pts',(-22.1115198899388,26.4341015112559,-45.842902360652));
#20508=CARTESIAN_POINT('Ctrl Pts',(-22.2339163535886,26.4941964530481,-45.8340345953022));
#20509=CARTESIAN_POINT('Ctrl Pts',(-22.3406090816023,26.5396179041769,-45.8263310922209));
#20510=CARTESIAN_POINT('Ctrl Pts',(-22.6831170533065,26.6640884797216,-45.8018196283623));
#20511=CARTESIAN_POINT('Ctrl Pts',(-22.9257694193826,26.721676500522,-45.7847079721004));
#20512=CARTESIAN_POINT('Ctrl Pts',(-23.2067875505152,26.7548323662921,-45.766549079901));
#20513=CARTESIAN_POINT('Ctrl Pts',(-23.2410029016038,26.7583150331222,-45.7643669235498));
#20514=CARTESIAN_POINT('Ctrl Pts',(-23.2798433131508,26.7616412490265,-45.7619273093996));
#20515=CARTESIAN_POINT('Ctrl Pts',(-23.2844183817378,26.7620232029315,-45.7616405328371));
#20516=CARTESIAN_POINT('Ctrl Pts',(-23.2913503768492,26.7625870137509,-45.7612069266999));
#20517=CARTESIAN_POINT('Ctrl Pts',(-23.2937066886552,26.7627760539274,-45.7610596949936));
#20518=CARTESIAN_POINT('Ctrl Pts',(-23.2978081927628,26.7631005645538,-45.7608036958914));
#20519=CARTESIAN_POINT('Ctrl Pts',(-23.2995532872719,26.7632372056989,-45.7606948621655));
#20520=CARTESIAN_POINT('Ctrl Pts',(-23.303210314001,26.7635205538429,-45.7604669752774));
#20521=CARTESIAN_POINT('Ctrl Pts',(-23.3051222650122,26.7636669761543,-45.7603479387869));
#20522=CARTESIAN_POINT('Ctrl Pts',(-23.3097025030671,26.7640136314109,-45.7600630293673));
#20523=CARTESIAN_POINT('Ctrl Pts',(-23.3123709190455,26.7642122484319,-45.759897248194));
#20524=CARTESIAN_POINT('Ctrl Pts',(-23.3214496065645,26.7648766298269,-45.7593339033445));
#20525=CARTESIAN_POINT('Ctrl Pts',(-23.3278610764336,26.7653265453296,-45.7589372303916));
#20526=CARTESIAN_POINT('Ctrl Pts',(-23.3431220310402,26.7663515912021,-45.7579957329688));
#20527=CARTESIAN_POINT('Ctrl Pts',(-23.3519726821841,26.766909384762,-45.7574518565877));
#20528=CARTESIAN_POINT('Ctrl Pts',(-23.4570304964405,26.7730951706566,-45.7510203094309));
#20529=CARTESIAN_POINT('Ctrl Pts',(-23.5534516378947,26.774442160417,-45.7453588402578));
#20530=CARTESIAN_POINT('Ctrl Pts',(-23.7338978176656,26.7688658280046,-45.7349773740592));
#20531=CARTESIAN_POINT('Ctrl Pts',(-23.8178675640792,26.7629742023149,-45.7302331595992));
#20532=CARTESIAN_POINT('Ctrl Pts',(-23.922031018559,26.7515529463684,-45.7243589640467));
#20533=CARTESIAN_POINT('Ctrl Pts',(-23.9425264350419,26.7491061981499,-45.7232037150364));
#20534=CARTESIAN_POINT('Ctrl Pts',(-23.9808183542393,26.7441613487728,-45.7210444092883));
#20535=CARTESIAN_POINT('Ctrl Pts',(-23.9986201701884,26.7417109634887,-45.7200401745927));
#20536=CARTESIAN_POINT('Ctrl Pts',(-24.1716457302892,26.7164180545362,-45.7102691335204));
#20537=CARTESIAN_POINT('Ctrl Pts',(-24.3250206543941,26.6824185730999,-45.7015139056533));
#20538=CARTESIAN_POINT('Ctrl Pts',(-24.5123817935236,26.626276464297,-45.6902377880939));
#20539=CARTESIAN_POINT('Ctrl Pts',(-24.5492576995849,26.614498681982,-45.6879902703741));
#20540=CARTESIAN_POINT('Ctrl Pts',(-24.6056888843577,26.5953482370758,-45.684501095138));
#20541=CARTESIAN_POINT('Ctrl Pts',(-24.6254001475624,26.5884446464585,-45.683272872589));
#20542=CARTESIAN_POINT('Ctrl Pts',(-24.7066383600016,26.5591025390506,-45.6781693273891));
#20543=CARTESIAN_POINT('Ctrl Pts',(-24.7675379578507,26.5349839785283,-45.6742439646287));
#20544=CARTESIAN_POINT('Ctrl Pts',(-24.8353415429127,26.5057108457034,-45.6697452134095));
#20545=CARTESIAN_POINT('Ctrl Pts',(-24.8430125762614,26.5023634845028,-45.6692343661572));
#20546=CARTESIAN_POINT('Ctrl Pts',(-24.8545861024484,26.4972594562234,-45.6684607635568));
#20547=CARTESIAN_POINT('Ctrl Pts',(-24.8584983195285,26.4955248171282,-45.6681987638727));
#20548=CARTESIAN_POINT('Ctrl Pts',(-24.8652876788679,26.4924982847094,-45.6677432134642));
#20549=CARTESIAN_POINT('Ctrl Pts',(-24.8681664084323,26.4912099477123,-45.667549785173));
#20550=CARTESIAN_POINT('Ctrl Pts',(-24.8739561675086,26.4886086103741,-45.6671602081692));
#20551=CARTESIAN_POINT('Ctrl Pts',(-24.8768671452372,26.487295505095,-45.6669640560323));
#20552=CARTESIAN_POINT('Ctrl Pts',(-24.8828026564844,26.4846074464491,-45.6665635253163));
#20553=CARTESIAN_POINT('Ctrl Pts',(-24.8858270242565,26.4832321387678,-45.666359134698));
#20554=CARTESIAN_POINT('Ctrl Pts',(-24.8957997353745,26.4786785025035,-45.6656841552503));
#20555=CARTESIAN_POINT('Ctrl Pts',(-24.90273886281,26.475480158115,-45.6652128751468));
#20556=CARTESIAN_POINT('Ctrl Pts',(-24.9494907823421,26.4537296066758,-45.6620266090919));
#20557=CARTESIAN_POINT('Ctrl Pts',(-24.9889304379036,26.4343905972579,-45.6592844124577));
#20558=CARTESIAN_POINT('Ctrl Pts',(-25.0907383523097,26.3818618156891,-45.6520583963383));
#20559=CARTESIAN_POINT('Ctrl Pts',(-25.1524294724456,26.3474181539741,-45.647531596187));
#20560=CARTESIAN_POINT('Ctrl Pts',(-25.2732667424991,26.2746423150326,-45.6383623908322));
#20561=CARTESIAN_POINT('Ctrl Pts',(-25.3323872803082,26.2363412085222,-45.6337228315378));
#20562=CARTESIAN_POINT('Ctrl Pts',(-25.6491876305378,26.0160379113047,-45.608043033346));
#20563=CARTESIAN_POINT('Ctrl Pts',(-25.8803149713862,25.7989036534411,-45.5860397343649));
#20564=CARTESIAN_POINT('Ctrl Pts',(-26.0863683622212,25.5388453539497,-45.5650390869338));
#20565=CARTESIAN_POINT('Ctrl Pts',(-26.0964253369512,25.525952152405,-45.5640104329362));
#20566=CARTESIAN_POINT('Ctrl Pts',(-26.1085750182408,25.5101292012963,-45.5627637979426));
#20567=CARTESIAN_POINT('Ctrl Pts',(-26.1107612739811,25.5072720732943,-45.5625393165491));
#20568=CARTESIAN_POINT('Ctrl Pts',(-26.1143548544824,25.5025594399686,-45.5621700814502));
#20569=CARTESIAN_POINT('Ctrl Pts',(-26.1157649524785,25.5007060698993,-45.5620251317832));
#20570=CARTESIAN_POINT('Ctrl Pts',(-26.1183020772094,25.4973638744345,-45.5617642171858));
#20571=CARTESIAN_POINT('Ctrl Pts',(-26.119429816298,25.4958756014545,-45.5616482016347));
#20572=CARTESIAN_POINT('Ctrl Pts',(-26.1218501747177,25.4926756898648,-45.5613991221658));
#20573=CARTESIAN_POINT('Ctrl Pts',(-26.1231423753933,25.4909637454651,-45.5612660881557));
#20574=CARTESIAN_POINT('Ctrl Pts',(-26.126671982098,25.4862779003522,-45.5609025595889));
#20575=CARTESIAN_POINT('Ctrl Pts',(-26.1289059563282,25.4833014003113,-45.5606723079115));
#20576=CARTESIAN_POINT('Ctrl Pts',(-26.1404167126564,25.4679092487397,-45.5594850196444));
#20577=CARTESIAN_POINT('Ctrl Pts',(-26.1496092068731,25.455430388674,-45.5585338367919));
#20578=CARTESIAN_POINT('Ctrl Pts',(-26.203298951527,25.3814342640725,-45.5529572330896));
#20579=CARTESIAN_POINT('Ctrl Pts',(-26.2457049345611,25.3184211395376,-45.5484657394944));
#20580=CARTESIAN_POINT('Ctrl Pts',(-26.4308887957867,25.0210771098771,-45.528142400024));
#20581=CARTESIAN_POINT('Ctrl Pts',(-26.5456049614685,24.7706123587006,-45.5133402523503));
#20582=CARTESIAN_POINT('Ctrl Pts',(-26.6329142654349,24.4902965054614,-45.4965542690082));
#20583=CARTESIAN_POINT('Ctrl Pts',(-26.6384586989395,24.4719187889303,-45.4954533287968));
#20584=CARTESIAN_POINT('Ctrl Pts',(-26.6495809833839,24.4338251126536,-45.4931692212223));
#20585=CARTESIAN_POINT('Ctrl Pts',(-26.6551356407016,24.414103337585,-45.4919855662485));
#20586=CARTESIAN_POINT('Ctrl Pts',(-26.6698105997036,24.3600291893616,-45.4887353545723));
#20587=CARTESIAN_POINT('Ctrl Pts',(-26.6785510956958,24.3255774583779,-45.4866592760994));
#20588=CARTESIAN_POINT('Ctrl Pts',(-26.6900987965241,24.2766815496717,-45.4837012043833));
#20589=CARTESIAN_POINT('Ctrl Pts',(-26.6933798102469,24.2623512509855,-45.4828328691964));
#20590=CARTESIAN_POINT('Ctrl Pts',(-26.6974694769903,24.243909944142,-45.4817134125032));
#20591=CARTESIAN_POINT('Ctrl Pts',(-26.6983683536607,24.239818973637,-45.4814649480156));
#20592=CARTESIAN_POINT('Ctrl Pts',(-26.7000677915748,24.2320119037782,-45.4809905366412));
#20593=CARTESIAN_POINT('Ctrl Pts',(-26.7008697587294,24.2282961153476,-45.4807646317626));
#20594=CARTESIAN_POINT('Ctrl Pts',(-26.7031012567801,24.2178673806173,-45.4801302959796));
#20595=CARTESIAN_POINT('Ctrl Pts',(-26.7045159141957,24.2111513004468,-45.4797214240073));
#20596=CARTESIAN_POINT('Ctrl Pts',(-26.7076882272467,24.1958485440645,-45.478788939057));
#20597=CARTESIAN_POINT('Ctrl Pts',(-26.7094323243651,24.1872591392677,-45.4782649216822));
#20598=CARTESIAN_POINT('Ctrl Pts',(-26.7126900963205,24.1708726229237,-45.4772639872759));
#20599=CARTESIAN_POINT('Ctrl Pts',(-26.714210029584,24.1630768112884,-45.4767872654356));
#20600=CARTESIAN_POINT('Ctrl Pts',(-26.7200551394064,24.1324955024424,-45.474915012691));
#20601=CARTESIAN_POINT('Ctrl Pts',(-26.7241630405492,24.1096696279425,-45.4735128309974));
#20602=CARTESIAN_POINT('Ctrl Pts',(-26.7299914343831,24.0751503325694,-45.47138441366));
#20603=CARTESIAN_POINT('Ctrl Pts',(-26.7318946120283,24.0634882060678,-45.4706639840158));
#20604=CARTESIAN_POINT('Ctrl Pts',(-26.734433217846,24.0473753826809,-45.4696666576261));
#20605=CARTESIAN_POINT('Ctrl Pts',(-26.7351235502036,24.0429333270995,-45.4693915055423));
#20606=CARTESIAN_POINT('Ctrl Pts',(-26.7362909637467,24.0353164236135,-45.4689193394605));
#20607=CARTESIAN_POINT('Ctrl Pts',(-26.736772600416,24.0321422714484,-45.4687224702966));
#20608=CARTESIAN_POINT('Ctrl Pts',(-26.737729484473,24.0257719105155,-45.4683271494224));
#20609=CARTESIAN_POINT('Ctrl Pts',(-26.7382046693119,24.0225756967735,-45.4681286960091));
#20610=CARTESIAN_POINT('Ctrl Pts',(-26.7391520762268,24.0161366336653,-45.4677286733704));
#20611=CARTESIAN_POINT('Ctrl Pts',(-26.7396241606454,24.0128937684043,-45.4675271000424));
#20612=CARTESIAN_POINT('Ctrl Pts',(-26.7406935169153,24.0054686673828,-45.4670653033087));
#20613=CARTESIAN_POINT('Ctrl Pts',(-26.7412875119866,24.0012859724142,-45.4668049762491));
#20614=CARTESIAN_POINT('Ctrl Pts',(-26.7427852061509,23.9905887004333,-45.4661387004403));
#20615=CARTESIAN_POINT('Ctrl Pts',(-26.7436771871845,23.9840725262204,-45.4657323808035));
#20616=CARTESIAN_POINT('Ctrl Pts',(-26.7455910060445,23.9697657430924,-45.4648392427615));
#20617=CARTESIAN_POINT('Ctrl Pts',(-26.746604309516,23.9619740526951,-45.4643521562291));
#20618=CARTESIAN_POINT('Ctrl Pts',(-26.7646199230559,23.8193688646117,-45.4554249193446));
#20619=CARTESIAN_POINT('Ctrl Pts',(-26.7731051425797,23.683638580119,-45.446715141092));
#20620=CARTESIAN_POINT('Ctrl Pts',(-26.7730015954251,23.5477959646253,-45.4377814573121));
#20621=CARTESIAN_POINT('Ctrl Pts',(-26.7730015985351,23.5478000480778,-45.4377817258601));
#20622=CARTESIAN_POINT('Ctrl Pts',(-26.7728034974816,23.2874802721333,-45.4206618149297));
#20623=CARTESIAN_POINT('Ctrl Pts',(-26.7410675662046,23.0281666471294,-45.4027352975828));
#20624=CARTESIAN_POINT('Ctrl Pts',(-26.6551711849931,22.6813409747046,-45.3789621655378));
#20625=CARTESIAN_POINT('Ctrl Pts',(-26.6276096000244,22.5882729779119,-45.3726171768751));
#20626=CARTESIAN_POINT('Ctrl Pts',(-26.592978418147,22.488171587896,-45.3659313184682));
#20627=CARTESIAN_POINT('Ctrl Pts',(-26.5900341125884,22.4797738088478,-45.3653715175065));
#20628=CARTESIAN_POINT('Ctrl Pts',(-26.5848975046335,22.4653152123082,-45.3644097197638));
#20629=CARTESIAN_POINT('Ctrl Pts',(-26.5827217540219,22.4592486288017,-45.3640067812941));
#20630=CARTESIAN_POINT('Ctrl Pts',(-26.5796159063412,22.4506697550354,-45.3634378921017));
#20631=CARTESIAN_POINT('Ctrl Pts',(-26.5787008714247,22.4481520861421,-45.3632710500649));
#20632=CARTESIAN_POINT('Ctrl Pts',(-26.5771252521819,22.4438336347131,-45.3629850682525));
#20633=CARTESIAN_POINT('Ctrl Pts',(-26.5764661984156,22.4420322985958,-45.3628658363443));
#20634=CARTESIAN_POINT('Ctrl Pts',(-26.5752028406082,22.4385887997385,-45.3626380214458));
#20635=CARTESIAN_POINT('Ctrl Pts',(-26.574598808126,22.4369465429322,-45.3625294221929));
#20636=CARTESIAN_POINT('Ctrl Pts',(-26.5731764772806,22.4330891783799,-45.362274455812));
#20637=CARTESIAN_POINT('Ctrl Pts',(-26.5723570798476,22.4308744727247,-45.3621281549943));
#20638=CARTESIAN_POINT('Ctrl Pts',(-26.5699407981392,22.424365625477,-45.3616984419026));
#20639=CARTESIAN_POINT('Ctrl Pts',(-26.5683371818847,22.4200739630624,-45.3614154318165));
#20640=CARTESIAN_POINT('Ctrl Pts',(-26.5547035375743,22.3838230092142,-45.3590275238853));
#20641=CARTESIAN_POINT('Ctrl Pts',(-26.542174819467,22.3520518266533,-45.356952007745));
#20642=CARTESIAN_POINT('Ctrl Pts',(-26.4113695088488,22.0351997138116,-45.3363702189845));
#20643=CARTESIAN_POINT('Ctrl Pts',(-26.2532097011805,21.7682703403302,-45.31986470917));
#20644=CARTESIAN_POINT('Ctrl Pts',(-26.0298486387752,21.4911390425142,-45.2996459172125));
#20645=CARTESIAN_POINT('Ctrl Pts',(-25.9994276656126,21.4550470164918,-45.2969468322258));
#20646=CARTESIAN_POINT('Ctrl Pts',(-25.9137067431168,21.3577648475905,-45.2894640793166));
#20647=CARTESIAN_POINT('Ctrl Pts',(-25.8568366435307,21.2980122757972,-45.2846320174133));
#20648=CARTESIAN_POINT('Ctrl Pts',(-25.7672344770345,21.2108251615749,-45.277158474638));
#20649=CARTESIAN_POINT('Ctrl Pts',(-25.7361440480881,21.1817493376022,-45.2745891283966));
#20650=CARTESIAN_POINT('Ctrl Pts',(-25.6988529112685,21.1482343439667,-45.271531034162));
#20651=CARTESIAN_POINT('Ctrl Pts',(-25.6932000355061,21.1431898072018,-45.271068093199));
#20652=CARTESIAN_POINT('Ctrl Pts',(-25.6850478405084,21.1359663958933,-45.2704013497791));
#20653=CARTESIAN_POINT('Ctrl Pts',(-25.6825628348166,21.1337713446945,-45.270198225376));
#20654=CARTESIAN_POINT('Ctrl Pts',(-25.6776742471662,21.1294665776766,-45.26979885875));
#20655=CARTESIAN_POINT('Ctrl Pts',(-25.6752709029983,21.127356596634,-45.2696026279345));
#20656=CARTESIAN_POINT('Ctrl Pts',(-25.670485784601,21.1231681679802,-45.2692121382054));
#20657=CARTESIAN_POINT('Ctrl Pts',(-25.6681040848658,21.1210896400942,-45.2690178829367));
#20658=CARTESIAN_POINT('Ctrl Pts',(-25.6624694320859,21.116186820468,-45.2685585532779));
#20659=CARTESIAN_POINT('Ctrl Pts',(-25.6592138722089,21.1133655452292,-45.2682933539526));
#20660=CARTESIAN_POINT('Ctrl Pts',(-25.6478538876781,21.1035607724016,-45.2673686161135));
#20661=CARTESIAN_POINT('Ctrl Pts',(-25.6397204216473,21.0966111671023,-45.2667076779282));
#20662=CARTESIAN_POINT('Ctrl Pts',(-25.5389136325498,21.0113419583673,-45.2585296908099));
#20663=CARTESIAN_POINT('Ctrl Pts',(-25.4419348617774,20.9382855523003,-45.2507990142347));
#20664=CARTESIAN_POINT('Ctrl Pts',(-25.2307021859127,20.7971030656318,-45.2342103919956));
#20665=CARTESIAN_POINT('Ctrl Pts',(-25.1158819005871,20.7302273458819,-45.2253295179925));
#20666=CARTESIAN_POINT('Ctrl Pts',(-24.8981456314014,20.6208140689927,-45.2088743000523));
#20667=CARTESIAN_POINT('Ctrl Pts',(-24.7965100460048,20.5761530071109,-45.2013374879993));
#20668=CARTESIAN_POINT('Ctrl Pts',(-24.6144293087517,20.507118381267,-45.1882488061272));
#20669=CARTESIAN_POINT('Ctrl Pts',(-24.5349512615989,20.4804792651584,-45.182668313399));
#20670=CARTESIAN_POINT('Ctrl Pts',(-24.4146005061842,20.445296825031,-45.1744957101365));
#20671=CARTESIAN_POINT('Ctrl Pts',(-24.3744560912716,20.4344001245433,-45.171814989321));
#20672=CARTESIAN_POINT('Ctrl Pts',(-24.3139391802099,20.4192251113258,-45.1678527717216));
#20673=CARTESIAN_POINT('Ctrl Pts',(-24.2937193084048,20.4143623533056,-45.1665420095325));
#20674=CARTESIAN_POINT('Ctrl Pts',(-24.2694769449185,20.4087798747163,-45.1649872770877));
#20675=CARTESIAN_POINT('Ctrl Pts',(-24.2654989748122,20.4078717881873,-45.1647326975547));
#20676=CARTESIAN_POINT('Ctrl Pts',(-24.259350457191,20.406480491751,-45.1643400528222));
#20677=CARTESIAN_POINT('Ctrl Pts',(-24.2571811344344,20.4059919735069,-45.164201681918));
#20678=CARTESIAN_POINT('Ctrl Pts',(-24.2533728059519,20.405138501659,-45.1639590532566));
#20679=CARTESIAN_POINT('Ctrl Pts',(-24.251734027114,20.4047725852287,-45.1638547398956));
#20680=CARTESIAN_POINT('Ctrl Pts',(-24.2479857761102,20.403938728063,-45.1636163653293));
#20681=CARTESIAN_POINT('Ctrl Pts',(-24.2458761228079,20.4034716287975,-45.1634823534853));
#20682=CARTESIAN_POINT('Ctrl Pts',(-24.2401575380812,20.4022115062517,-45.1631195045512));
#20683=CARTESIAN_POINT('Ctrl Pts',(-24.2365476959867,20.4014225643095,-45.1628909033215));
#20684=CARTESIAN_POINT('Ctrl Pts',(-24.219585424991,20.3977459629985,-45.1618187911798));
#20685=CARTESIAN_POINT('Ctrl Pts',(-24.2062158208505,20.3949369584659,-45.1609797517779));
#20686=CARTESIAN_POINT('Ctrl Pts',(-24.1917101658824,20.3919854485543,-45.160075507181));
#20687=CARTESIAN_POINT('Ctrl Pts',(-24.1905917293686,20.3917584954748,-45.1600058259435));
#20688=CARTESIAN_POINT('Ctrl Pts',(-24.1881021061363,20.3912546779936,-45.1598508032302));
#20689=CARTESIAN_POINT('Ctrl Pts',(-24.1867308582596,20.3909781119691,-45.1597654775152));
#20690=CARTESIAN_POINT('Ctrl Pts',(-23.8979647845241,20.3329327196181,-45.1418092839725));
#20691=CARTESIAN_POINT('Ctrl Pts',(-23.6039780835636,20.3146337129784,-45.12599133174));
#20692=CARTESIAN_POINT('Ctrl Pts',(-23.1965119478916,20.3448996337368,-45.1029867512282));
#20693=CARTESIAN_POINT('Ctrl Pts',(-23.0820432226493,20.3596105028491,-45.09641683267));
#20694=CARTESIAN_POINT('Ctrl Pts',(-22.9087625693298,20.3914060299975,-45.086116877009));
#20695=CARTESIAN_POINT('Ctrl Pts',(-22.8492354849055,20.4040810502791,-45.0825141454747));
#20696=CARTESIAN_POINT('Ctrl Pts',(-22.7692935234882,20.4234843524806,-45.0775715287664));
#20697=CARTESIAN_POINT('Ctrl Pts',(-22.7485327837924,20.4287430200786,-45.0762783570718));
#20698=CARTESIAN_POINT('Ctrl Pts',(-22.718304718016,20.4367211964937,-45.0743808356975));
#20699=CARTESIAN_POINT('Ctrl Pts',(-22.7087947158741,20.4392778804321,-45.0737817348839));
#20700=CARTESIAN_POINT('Ctrl Pts',(-22.6917731054205,20.4439377563845,-45.0727055492494));
#20701=CARTESIAN_POINT('Ctrl Pts',(-22.6842571034399,20.4460247170519,-45.0722289936075));
#20702=CARTESIAN_POINT('Ctrl Pts',(-22.6728177865572,20.4492458389132,-45.0715015807294));
#20703=CARTESIAN_POINT('Ctrl Pts',(-22.6688888911746,20.4503602152463,-45.0712513690741));
#20704=CARTESIAN_POINT('Ctrl Pts',(-22.6617898821309,20.4523883372215,-45.0707985814163));
#20705=CARTESIAN_POINT('Ctrl Pts',(-22.6586190283564,20.4532994899673,-45.0705960903513));
#20706=CARTESIAN_POINT('Ctrl Pts',(-22.6518121759099,20.45526677639,-45.0701608681467));
#20707=CARTESIAN_POINT('Ctrl Pts',(-22.648176631097,20.4563244511137,-45.0699280868675));
#20708=CARTESIAN_POINT('Ctrl Pts',(-22.6384190335322,20.4591818510478,-45.0693024272133));
#20709=CARTESIAN_POINT('Ctrl Pts',(-22.632300471429,20.4609933494242,-45.0689091638688));
#20710=CARTESIAN_POINT('Ctrl Pts',(-22.6056200170591,20.4689787878761,-45.0671901720207));
#20711=CARTESIAN_POINT('Ctrl Pts',(-22.585115107875,20.4753398192319,-45.0658583187525));
#20712=CARTESIAN_POINT('Ctrl Pts',(-22.552268549486,20.4858903871596,-45.0637071298217));
#20713=CARTESIAN_POINT('Ctrl Pts',(-22.5398858600029,20.4899508207054,-45.0628920895583));
#20714=CARTESIAN_POINT('Ctrl Pts',(-22.5219253408943,20.4959611802209,-45.0617039196904));
#20715=CARTESIAN_POINT('Ctrl Pts',(-22.5163275962682,20.497851558988,-45.0613327544074));
#20716=CARTESIAN_POINT('Ctrl Pts',(-22.503974508117,20.5020611214996,-45.060511783333));
#20717=CARTESIAN_POINT('Ctrl Pts',(-22.4972216262323,20.5043873858569,-45.0600617471255));
#20718=CARTESIAN_POINT('Ctrl Pts',(-22.4839316283652,20.5090150658228,-45.0591735824255));
#20719=CARTESIAN_POINT('Ctrl Pts',(-22.4773940898212,20.5113151589937,-45.0587354991087));
#20720=CARTESIAN_POINT('Ctrl Pts',(-22.4652019844564,20.5156489361261,-45.0579162832414));
#20721=CARTESIAN_POINT('Ctrl Pts',(-22.4595455780171,20.5176773862581,-45.0575353221834));
#20722=CARTESIAN_POINT('Ctrl Pts',(-22.4500721710333,20.521104588394,-45.0568957809913));
#20723=CARTESIAN_POINT('Ctrl Pts',(-22.4462520679164,20.5224947698972,-45.0566374783523));
#20724=CARTESIAN_POINT('Ctrl Pts',(-22.4292181472484,20.528730141824,-45.0554838642378));
#20725=CARTESIAN_POINT('Ctrl Pts',(-22.4160336771917,20.5336545764127,-45.0545860128434));
#20726=CARTESIAN_POINT('Ctrl Pts',(-22.2398166444256,20.6007906733022,-45.042519248083));
#20727=CARTESIAN_POINT('Ctrl Pts',(-22.0820887129767,20.6760487840267,-45.0309291086369));
#20728=CARTESIAN_POINT('Ctrl Pts',(-21.8293093166297,20.8229148899508,-45.011207636818));
#20729=CARTESIAN_POINT('Ctrl Pts',(-21.7307001781605,20.887688829786,-45.0031940605351));
#20730=CARTESIAN_POINT('Ctrl Pts',(-21.5586145166671,21.0147611735799,-44.9888114403302));
#20731=CARTESIAN_POINT('Ctrl Pts',(-21.4839489874093,21.0752311321703,-44.9824211301116));
#20732=CARTESIAN_POINT('Ctrl Pts',(-21.386717035229,21.1614491172433,-44.9740021201736));
#20733=CARTESIAN_POINT('Ctrl Pts',(-21.3616990588191,21.1843485812641,-44.9718267292021));
#20734=CARTESIAN_POINT('Ctrl Pts',(-21.3240241870501,21.2199422853436,-44.9685428527679));
#20735=CARTESIAN_POINT('Ctrl Pts',(-21.3111047078489,21.2323535811299,-44.9674152789667));
#20736=CARTESIAN_POINT('Ctrl Pts',(-21.2954996388782,21.2475970733138,-44.9660522747915));
#20737=CARTESIAN_POINT('Ctrl Pts',(-21.2927151636425,21.2503269242224,-44.9658090277211));
#20738=CARTESIAN_POINT('Ctrl Pts',(-21.2883787446777,21.2545937363338,-44.9654301518959));
#20739=CARTESIAN_POINT('Ctrl Pts',(-21.2868234091344,21.2561272211838,-44.9652942503991));
#20740=CARTESIAN_POINT('Ctrl Pts',(-21.2840764647279,21.2588410869277,-44.965054211899));
#20741=CARTESIAN_POINT('Ctrl Pts',(-21.2828842245792,21.2600208107505,-44.9649500238509));
#20742=CARTESIAN_POINT('Ctrl Pts',(-21.2803383456023,21.262543899199,-44.9647275312949));
#20743=CARTESIAN_POINT('Ctrl Pts',(-21.2789849819542,21.2638875308775,-44.9646092489906));
#20744=CARTESIAN_POINT('Ctrl Pts',(-21.2750777284315,21.2677735803586,-44.964267735299));
#20745=CARTESIAN_POINT('Ctrl Pts',(-21.2725268987723,21.2703190918492,-44.964044749505));
#20746=CARTESIAN_POINT('Ctrl Pts',(-21.2612154229078,21.2816449148349,-44.963055769378));
#20747=CARTESIAN_POINT('Ctrl Pts',(-21.2525010858741,21.2904716330932,-44.9622934198514));
#20748=CARTESIAN_POINT('Ctrl Pts',(-21.2418492262579,21.3013861844153,-44.9613606875415));
#20749=CARTESIAN_POINT('Ctrl Pts',(-21.2398633854212,21.3034264010395,-44.9611867588706));
#20750=CARTESIAN_POINT('Ctrl Pts',(-21.0631292209979,21.4854819200006,-44.945703906993));
#20751=CARTESIAN_POINT('Ctrl Pts',(-20.9099639989115,21.6853179177608,-44.9319210444006));
#20752=CARTESIAN_POINT('Ctrl Pts',(-20.6991602642798,22.0391963654348,-44.9088777128871));
#20753=CARTESIAN_POINT('Ctrl Pts',(-20.6272754008357,22.1834255272332,-44.8998099401317));
#20754=CARTESIAN_POINT('Ctrl Pts',(-20.5440571046845,22.3873150978992,-44.8869226753958));
#20755=CARTESIAN_POINT('Ctrl Pts',(-20.5231680039762,22.4428262230988,-44.8834091944686));
#20756=CARTESIAN_POINT('Ctrl Pts',(-20.496969542046,22.5187381681002,-44.8785826031711));
#20757=CARTESIAN_POINT('Ctrl Pts',(-20.4903104819024,22.5386629324985,-44.8773137846334));
#20758=CARTESIAN_POINT('Ctrl Pts',(-20.480859788145,22.5678880407044,-44.8754492659968));
#20759=CARTESIAN_POINT('Ctrl Pts',(-20.4779145387035,22.5771384269165,-44.8748586036238));
#20760=CARTESIAN_POINT('Ctrl Pts',(-20.4727015074216,22.5937710139456,-44.8737956069141));
#20761=CARTESIAN_POINT('Ctrl Pts',(-20.4704183708487,22.6011483536146,-44.8733237794919));
#20762=CARTESIAN_POINT('Ctrl Pts',(-20.4669754016512,22.6124166260711,-44.87260256269));
#20763=CARTESIAN_POINT('Ctrl Pts',(-20.46579635802,22.6163016984241,-44.8723538040856));
#20764=CARTESIAN_POINT('Ctrl Pts',(-20.4636692427214,22.6233587282291,-44.8719017659872));
#20765=CARTESIAN_POINT('Ctrl Pts',(-20.4627187097627,22.626529942945,-44.8716985674912));
#20766=CARTESIAN_POINT('Ctrl Pts',(-20.4608245385674,22.6328849582267,-44.8712912289732));
#20767=CARTESIAN_POINT('Ctrl Pts',(-20.4598809313744,22.6360687638598,-44.8710870882142));
#20768=CARTESIAN_POINT('Ctrl Pts',(-20.4572604662097,22.6449608429802,-44.8705167492959));
#20769=CARTESIAN_POINT('Ctrl Pts',(-20.4555944982706,22.6506722883516,-44.8701501954468));
#20770=CARTESIAN_POINT('Ctrl Pts',(-20.4489552411344,22.6736703958866,-44.8686732901961));
#20771=CARTESIAN_POINT('Ctrl Pts',(-20.4441109798194,22.6909936860314,-44.8675587366589));
#20772=CARTESIAN_POINT('Ctrl Pts',(-20.4352859533609,22.7236025156855,-44.8654565659501));
#20773=CARTESIAN_POINT('Ctrl Pts',(-20.4312720338651,22.7388785902106,-44.8644700665219));
#20774=CARTESIAN_POINT('Ctrl Pts',(-20.4260742069639,22.7592690282358,-44.8631509158559));
#20775=CARTESIAN_POINT('Ctrl Pts',(-20.4247902197799,22.7643578544405,-44.8628215000721));
#20776=CARTESIAN_POINT('Ctrl Pts',(-20.4226914948034,22.7727622233332,-44.8622771308827));
#20777=CARTESIAN_POINT('Ctrl Pts',(-20.4218695814428,22.7760759785073,-44.8620624077709));
#20778=CARTESIAN_POINT('Ctrl Pts',(-20.4206782507937,22.7809120111051,-44.8617489214697));
#20779=CARTESIAN_POINT('Ctrl Pts',(-20.4203046731385,22.782433269756,-44.8616502910719));
#20780=CARTESIAN_POINT('Ctrl Pts',(-20.4189846294926,22.787825637859,-44.8613006150651));
#20781=CARTESIAN_POINT('Ctrl Pts',(-20.4180442377539,22.7916982179214,-44.861049376423));
#20782=CARTESIAN_POINT('Ctrl Pts',(-20.4154813042982,22.802338533051,-44.8603587527368));
#20783=CARTESIAN_POINT('Ctrl Pts',(-20.4138735052767,22.8091097661576,-44.8599189022605));
#20784=CARTESIAN_POINT('Ctrl Pts',(-20.4093289806717,22.8285286259707,-44.8586564514283));
#20785=CARTESIAN_POINT('Ctrl Pts',(-20.4064467644044,22.8411887551764,-44.8578321493275));
#20786=CARTESIAN_POINT('Ctrl Pts',(-20.4010661933736,22.8655007723999,-44.8562467672213));
#20787=CARTESIAN_POINT('Ctrl Pts',(-20.3985558021515,22.8771498022945,-44.8554860727357));
#20788=CARTESIAN_POINT('Ctrl Pts',(-20.3270481729637,23.2181409589842,-44.8331876894662));
#20789=CARTESIAN_POINT('Ctrl Pts',(-20.3100026497799,23.5562321470106,-44.8099080844745));
#20790=CARTESIAN_POINT('Ctrl Pts',(-20.3532325366874,23.9631548564351,-44.7827384640491));
#20791=CARTESIAN_POINT('Ctrl Pts',(-20.3633838722017,24.0353246763728,-44.7779665758087));
#20792=CARTESIAN_POINT('Ctrl Pts',(-20.3811660052329,24.1366919355419,-44.7713851975304));
#20793=CARTESIAN_POINT('Ctrl Pts',(-20.3867722033162,24.1662175951536,-44.76948292917));
#20794=CARTESIAN_POINT('Ctrl Pts',(-20.3936936770142,24.2000787267925,-44.7673216673449));
#20795=CARTESIAN_POINT('Ctrl Pts',(-20.3946058044604,24.2044937871827,-44.7670402654172));
#20796=CARTESIAN_POINT('Ctrl Pts',(-20.3960002440421,24.2111726672493,-44.7666151942605));
#20797=CARTESIAN_POINT('Ctrl Pts',(-20.39647573059,24.2134378818333,-44.7664711347015));
#20798=CARTESIAN_POINT('Ctrl Pts',(-20.3973390118192,24.2175286226634,-44.7662111756556));
#20799=CARTESIAN_POINT('Ctrl Pts',(-20.3977259508137,24.2193543193829,-44.7660952272359));
#20800=CARTESIAN_POINT('Ctrl Pts',(-20.3985049166878,24.2230140429887,-44.7658629444919));
#20801=CARTESIAN_POINT('Ctrl Pts',(-20.3988969570447,24.2248480563953,-44.7657466114873));
#20802=CARTESIAN_POINT('Ctrl Pts',(-20.4000140301585,24.2300516384619,-44.7654167452201));
#20803=CARTESIAN_POINT('Ctrl Pts',(-20.4007428706314,24.2334204007105,-44.765203431752));
#20804=CARTESIAN_POINT('Ctrl Pts',(-20.4038348006572,24.2476014497764,-44.7643064578189));
#20805=CARTESIAN_POINT('Ctrl Pts',(-20.4062482108974,24.258402862455,-44.7636256628503));
#20806=CARTESIAN_POINT('Ctrl Pts',(-20.4500295747269,24.4497134534795,-44.751607025997));
#20807=CARTESIAN_POINT('Ctrl Pts',(-20.5068321490864,24.6263689912586,-44.741121579045));
#20808=CARTESIAN_POINT('Ctrl Pts',(-20.6480721669903,24.9629775227874,-44.7206642480205));
#20809=CARTESIAN_POINT('Ctrl Pts',(-20.7313850065157,25.1226475079508,-44.7107148208347));
#20810=CARTESIAN_POINT('Ctrl Pts',(-20.8966685795722,25.3836335752822,-44.6929930723686));
#20811=CARTESIAN_POINT('Ctrl Pts',(-20.9722480863356,25.4884684021089,-44.6854184352356));
#20812=CARTESIAN_POINT('Ctrl Pts',(-21.0607872971317,25.5969080500766,-44.6769300379716));
#20813=CARTESIAN_POINT('Ctrl Pts',(-21.067711742607,25.6053017259999,-44.6762685646686));
#20814=CARTESIAN_POINT('Ctrl Pts',(-21.0801029305507,25.6201680586037,-44.6750889957753));
#20815=CARTESIAN_POINT('Ctrl Pts',(-21.0855529633116,25.6266545582839,-44.6745715827647));
#20816=CARTESIAN_POINT('Ctrl Pts',(-21.093756083571,25.6363399158125,-44.6737948512717));
#20817=CARTESIAN_POINT('Ctrl Pts',(-21.0964900108697,25.6395550145692,-44.6735363215207));
#20818=CARTESIAN_POINT('Ctrl Pts',(-21.1013369479442,25.6452323773558,-44.6730785711106));
#20819=CARTESIAN_POINT('Ctrl Pts',(-21.1034473797392,25.6476968428271,-44.6728794571511));
#20820=CARTESIAN_POINT('Ctrl Pts',(-21.1076658383732,25.6526079340681,-44.672481847716));
#20821=CARTESIAN_POINT('Ctrl Pts',(-21.1097738284339,25.6550545867801,-44.6722833538897));
#20822=CARTESIAN_POINT('Ctrl Pts',(-21.1154770028903,25.6616539281768,-44.6717468486042));
#20823=CARTESIAN_POINT('Ctrl Pts',(-21.1190791200695,25.6658005871027,-44.6714085490555));
#20824=CARTESIAN_POINT('Ctrl Pts',(-21.1324312436267,25.6810920496013,-44.670156591904));
#20825=CARTESIAN_POINT('Ctrl Pts',(-21.1422473104427,25.6921786916639,-44.6692401757693));
#20826=CARTESIAN_POINT('Ctrl Pts',(-21.3122523665041,25.8815432351422,-44.6534351708116));
#20827=CARTESIAN_POINT('Ctrl Pts',(-21.4917252325096,26.0414332269614,-44.6376683242449));
#20828=CARTESIAN_POINT('Ctrl Pts',(-21.7030871302608,26.1911758316436,-44.6201957948438));
#20829=CARTESIAN_POINT('Ctrl Pts',(-21.7190598699247,26.2022761598967,-44.6188820847764));
#20830=CARTESIAN_POINT('Ctrl Pts',(-21.8441975835271,26.2875716355257,-44.6086448226165));
#20831=CARTESIAN_POINT('Ctrl Pts',(-21.9577136023082,26.3551323111444,-44.5996747431003));
#20832=CARTESIAN_POINT('Ctrl Pts',(-22.0750360439056,26.4155367892604,-44.590879968079));
#20833=CARTESIAN_POINT('Origin',(-23.5502525316942,23.5502525316942,-77.3107734492734));
#20834=CARTESIAN_POINT('',(-22.0750360145756,26.4155367741596,-43.0932330566435));
#20835=CARTESIAN_POINT('',(-22.0750361136176,26.4155368251522,-43.341564988124));
#20836=CARTESIAN_POINT('',(-22.0750360153461,26.4155367745563,-77.3107734492734));
#20837=CARTESIAN_POINT('',(-26.7730011356003,23.5532335332771,-43.9391856912327));
#20838=CARTESIAN_POINT('Ctrl Pts',(-22.0750360145756,26.4155367741596,-43.0932330566435));
#20839=CARTESIAN_POINT('Ctrl Pts',(-22.0509411675559,26.4031313325723,-43.0949199058338));
#20840=CARTESIAN_POINT('Ctrl Pts',(-22.0270038178035,26.3904224862259,-43.09661747516));
#20841=CARTESIAN_POINT('Ctrl Pts',(-21.930883109556,26.337825215561,-43.103524041299));
#20842=CARTESIAN_POINT('Ctrl Pts',(-21.8600885552139,26.2954779462133,-43.1088193988789));
#20843=CARTESIAN_POINT('Ctrl Pts',(-21.5833383513035,26.1151687011008,-43.1303745886662));
#20844=CARTESIAN_POINT('Ctrl Pts',(-21.3919924743565,25.9563764069618,-43.1473357358126));
#20845=CARTESIAN_POINT('Ctrl Pts',(-21.1258009127753,25.6779357062376,-43.1732132722146));
#20846=CARTESIAN_POINT('Ctrl Pts',(-21.0372778885744,25.5726199210681,-43.1823014093251));
#20847=CARTESIAN_POINT('Ctrl Pts',(-20.950887762283,25.4553738640371,-43.1914490342169));
#20848=CARTESIAN_POINT('Ctrl Pts',(-20.9460597476488,25.4487689109754,-43.1919612533885));
#20849=CARTESIAN_POINT('Ctrl Pts',(-20.9394677329414,25.4396782607697,-43.192661909344));
#20850=CARTESIAN_POINT('Ctrl Pts',(-20.9376820826013,25.4372084134788,-43.1928518345535));
#20851=CARTESIAN_POINT('Ctrl Pts',(-20.9348500783737,25.4332795610114,-43.1931532555518));
#20852=CARTESIAN_POINT('Ctrl Pts',(-20.9338014411278,25.4318222159437,-43.1932649105526));
#20853=CARTESIAN_POINT('Ctrl Pts',(-20.9317630011989,25.4289842919179,-43.1934820416224));
#20854=CARTESIAN_POINT('Ctrl Pts',(-20.9307730750831,25.4276038106479,-43.1935875260526));
#20855=CARTESIAN_POINT('Ctrl Pts',(-20.9283896780335,25.4242745376001,-43.193841591688));
#20856=CARTESIAN_POINT('Ctrl Pts',(-20.9269972849552,25.4223249695479,-43.1939900974984));
#20857=CARTESIAN_POINT('Ctrl Pts',(-20.9228169131104,25.4164579736698,-43.1944362003183));
#20858=CARTESIAN_POINT('Ctrl Pts',(-20.9200355100866,25.4125358349052,-43.1947333425803));
#20859=CARTESIAN_POINT('Ctrl Pts',(-20.8966778283354,25.3794417613896,-43.1972315970212));
#20860=CARTESIAN_POINT('Ctrl Pts',(-20.8765777541089,25.3499345558076,-43.1994005413393));
#20861=CARTESIAN_POINT('Ctrl Pts',(-20.8033881603989,25.2385575013189,-43.2073957699233));
#20862=CARTESIAN_POINT('Ctrl Pts',(-20.7535308021796,25.1546180052873,-43.2130428969139));
#20863=CARTESIAN_POINT('Ctrl Pts',(-20.61283514177,24.8911925405185,-43.2300363220955));
#20864=CARTESIAN_POINT('Ctrl Pts',(-20.5349167902404,24.7053699118333,-43.241063335693));
#20865=CARTESIAN_POINT('Ctrl Pts',(-20.4226323126586,24.3468683586313,-43.2623523678401));
#20866=CARTESIAN_POINT('Ctrl Pts',(-20.3840793568824,24.1763027509273,-43.2724862112721));
#20867=CARTESIAN_POINT('Ctrl Pts',(-20.3579134738227,23.9920907363947,-43.2838008872555));
#20868=CARTESIAN_POINT('Ctrl Pts',(-20.3563580576937,23.9807031597127,-43.2845017201422));
#20869=CARTESIAN_POINT('Ctrl Pts',(-20.354285982917,23.9649031253491,-43.2854761062605));
#20870=CARTESIAN_POINT('Ctrl Pts',(-20.3537174708215,23.9604974585504,-43.2857480178683));
#20871=CARTESIAN_POINT('Ctrl Pts',(-20.3527555823451,23.9529199339334,-43.2862160662392));
#20872=CARTESIAN_POINT('Ctrl Pts',(-20.3523578111157,23.9497486316861,-43.2864120637698));
#20873=CARTESIAN_POINT('Ctrl Pts',(-20.3515480318244,23.9432138122725,-43.2868161725079));
#20874=CARTESIAN_POINT('Ctrl Pts',(-20.3511366100199,23.9398502281367,-43.2870243019567));
#20875=CARTESIAN_POINT('Ctrl Pts',(-20.350193734576,23.9320395361099,-43.2875079056571));
#20876=CARTESIAN_POINT('Ctrl Pts',(-20.3496662457684,23.927591964797,-43.2877835048707));
#20877=CARTESIAN_POINT('Ctrl Pts',(-20.3480544367186,23.9137552885425,-43.2886416200268));
#20878=CARTESIAN_POINT('Ctrl Pts',(-20.3470021553277,23.9043625667906,-43.2892251469476));
#20879=CARTESIAN_POINT('Ctrl Pts',(-20.337285020128,23.8140374283075,-43.2948466070312));
#20880=CARTESIAN_POINT('Ctrl Pts',(-20.3316485479049,23.732815267769,-43.2999795957716));
#20881=CARTESIAN_POINT('Ctrl Pts',(-20.3281365440153,23.6210513809252,-43.3071594480434));
#20882=CARTESIAN_POINT('Ctrl Pts',(-20.3276116339609,23.5906191540321,-43.3091261755423));
#20883=CARTESIAN_POINT('Ctrl Pts',(-20.3268423603734,23.3410125783794,-43.3253524121541));
#20884=CARTESIAN_POINT('Ctrl Pts',(-20.348527276048,23.1223654367842,-43.3402244465518));
#20885=CARTESIAN_POINT('Ctrl Pts',(-20.4223257031285,22.7596908600062,-43.3652397117691));
#20886=CARTESIAN_POINT('Ctrl Pts',(-20.4627952842113,22.6140199553117,-43.3753689358388));
#20887=CARTESIAN_POINT('Ctrl Pts',(-20.514100827385,22.4695557091456,-43.3851768718604));
#20888=CARTESIAN_POINT('Ctrl Pts',(-20.5148685743261,22.4674011913597,-43.385323089076));
#20889=CARTESIAN_POINT('Ctrl Pts',(-20.5250485645522,22.438929121007,-43.3872545889702));
#20890=CARTESIAN_POINT('Ctrl Pts',(-20.5348008887788,22.4127331758003,-43.3890230008916));
#20891=CARTESIAN_POINT('Ctrl Pts',(-20.5466000703984,22.3822577527964,-43.391067360424));
#20892=CARTESIAN_POINT('Ctrl Pts',(-20.5483166647578,22.3778528714839,-43.3913625312122));
#20893=CARTESIAN_POINT('Ctrl Pts',(-20.5509164751562,22.3712247521225,-43.3918061835212));
#20894=CARTESIAN_POINT('Ctrl Pts',(-20.5517924744881,22.3689987187988,-43.3919550981166));
#20895=CARTESIAN_POINT('Ctrl Pts',(-20.5533588347952,22.3650313536954,-43.3922203486137));
#20896=CARTESIAN_POINT('Ctrl Pts',(-20.5540482347313,22.363289650127,-43.3923367426168));
#20897=CARTESIAN_POINT('Ctrl Pts',(-20.5555149565223,22.3595935367529,-43.3925836320781));
#20898=CARTESIAN_POINT('Ctrl Pts',(-20.5562926711997,22.3576392917081,-43.3927141029301));
#20899=CARTESIAN_POINT('Ctrl Pts',(-20.5578820544281,22.3536568348538,-43.3929798490574));
#20900=CARTESIAN_POINT('Ctrl Pts',(-20.5586938733969,22.3516286837144,-43.3931151151122));
#20901=CARTESIAN_POINT('Ctrl Pts',(-20.5622993115452,22.3426477694502,-43.3937137833543));
#20902=CARTESIAN_POINT('Ctrl Pts',(-20.5651151416482,22.3357038612845,-43.3941758483552));
#20903=CARTESIAN_POINT('Ctrl Pts',(-20.5920069388273,22.2700465007535,-43.3985376866179));
#20904=CARTESIAN_POINT('Ctrl Pts',(-20.6177898714931,22.2120415877526,-43.4023368314478));
#20905=CARTESIAN_POINT('Ctrl Pts',(-20.6729204209858,22.0972710564713,-43.4098170670278));
#20906=CARTESIAN_POINT('Ctrl Pts',(-20.7022759620202,22.0405421107163,-43.4134956255235));
#20907=CARTESIAN_POINT('Ctrl Pts',(-20.8121204999002,21.8428924562843,-43.4263720995039));
#20908=CARTESIAN_POINT('Ctrl Pts',(-20.9015424225747,21.7072159658174,-43.4353327702715));
#20909=CARTESIAN_POINT('Ctrl Pts',(-21.13121880199,21.4101953444886,-43.4564178222973));
#20910=CARTESIAN_POINT('Ctrl Pts',(-21.2780226763631,21.2549268810314,-43.4686259340821));
#20911=CARTESIAN_POINT('Ctrl Pts',(-21.4489751884401,21.1067052865176,-43.4823703505936));
#20912=CARTESIAN_POINT('Ctrl Pts',(-21.4589378525004,21.0981733084019,-43.4831696123388));
#20913=CARTESIAN_POINT('Ctrl Pts',(-21.4725393929948,21.0866682017941,-43.4842585847397));
#20914=CARTESIAN_POINT('Ctrl Pts',(-21.4761331918699,21.0836417798647,-43.4845461042142));
#20915=CARTESIAN_POINT('Ctrl Pts',(-21.4822362324827,21.0785250357067,-43.485034026552));
#20916=CARTESIAN_POINT('Ctrl Pts',(-21.4847420649467,21.0764306424176,-43.4852342625583));
#20917=CARTESIAN_POINT('Ctrl Pts',(-21.4895754972568,21.0724032876278,-43.4856203044036));
#20918=CARTESIAN_POINT('Ctrl Pts',(-21.4919026446797,21.0704697873581,-43.4858060879171));
#20919=CARTESIAN_POINT('Ctrl Pts',(-21.4974014018514,21.0659142424378,-43.4862448759366));
#20920=CARTESIAN_POINT('Ctrl Pts',(-21.5005753122253,21.0632949943601,-43.4864979938534));
#20921=CARTESIAN_POINT('Ctrl Pts',(-21.5071413582922,21.0578975166931,-43.4870213224489));
#20922=CARTESIAN_POINT('Ctrl Pts',(-21.5105341628678,21.0551201177233,-43.4872915661259));
#20923=CARTESIAN_POINT('Ctrl Pts',(-21.5290512781828,21.0400247466253,-43.4887655775794));
#20924=CARTESIAN_POINT('Ctrl Pts',(-21.5442812535625,21.0278375689044,-43.4899746138252));
#20925=CARTESIAN_POINT('Ctrl Pts',(-21.5839344893001,20.9966929053899,-43.4931144886326));
#20926=CARTESIAN_POINT('Ctrl Pts',(-21.608521147046,20.9779476253101,-43.4950536277252));
#20927=CARTESIAN_POINT('Ctrl Pts',(-21.7138836280822,20.8999888790961,-43.5033333371192));
#20928=CARTESIAN_POINT('Ctrl Pts',(-21.7971196442831,20.8442093240221,-43.5098027894704));
#20929=CARTESIAN_POINT('Ctrl Pts',(-22.020984040137,20.7088573407347,-43.5270118794189));
#20930=CARTESIAN_POINT('Ctrl Pts',(-22.1652303784352,20.6358238695582,-43.5379265022705));
#20931=CARTESIAN_POINT('Ctrl Pts',(-22.4957677786971,20.4985683293647,-43.5621518756575));
#20932=CARTESIAN_POINT('Ctrl Pts',(-22.6837406905633,20.4399645917796,-43.5754235621738));
#20933=CARTESIAN_POINT('Ctrl Pts',(-22.8875641391993,20.3963495654122,-43.5885643782032));
#20934=CARTESIAN_POINT('Ctrl Pts',(-22.8992415203174,20.3939185031191,-43.5893129023727));
#20935=CARTESIAN_POINT('Ctrl Pts',(-22.9144110619574,20.3908481914616,-43.5902794170298));
#20936=CARTESIAN_POINT('Ctrl Pts',(-22.9178909598769,20.3901498430943,-43.5905007365136));
#20937=CARTESIAN_POINT('Ctrl Pts',(-22.9232316319113,20.3890872483263,-43.5908397802094));
#20938=CARTESIAN_POINT('Ctrl Pts',(-22.9250915712984,20.3887188957549,-43.5909577400968));
#20939=CARTESIAN_POINT('Ctrl Pts',(-22.9287633078862,20.3879950918075,-43.5911903776596));
#20940=CARTESIAN_POINT('Ctrl Pts',(-22.9305750757971,20.3876395578835,-43.5913050592661));
#20941=CARTESIAN_POINT('Ctrl Pts',(-22.9346162498314,20.3868501403777,-43.5915606130374));
#20942=CARTESIAN_POINT('Ctrl Pts',(-22.9368458042925,20.3864170574972,-43.5917014384353));
#20943=CARTESIAN_POINT('Ctrl Pts',(-22.9414522046534,20.3855273331717,-43.5919920531183));
#20944=CARTESIAN_POINT('Ctrl Pts',(-22.943829111907,20.3850710114029,-43.5921418239974));
#20945=CARTESIAN_POINT('Ctrl Pts',(-22.9565032161387,20.3826526209519,-43.5929394460822));
#20946=CARTESIAN_POINT('Ctrl Pts',(-22.9668095846618,20.3807380927009,-43.5935845986867));
#20947=CARTESIAN_POINT('Ctrl Pts',(-23.0707428243228,20.3619554186031,-43.6000573956181));
#20948=CARTESIAN_POINT('Ctrl Pts',(-23.1650740556054,20.3491887229214,-43.6056617280261));
#20949=CARTESIAN_POINT('Ctrl Pts',(-23.4158465504955,20.3264986019552,-43.6201733701816));
#20950=CARTESIAN_POINT('Ctrl Pts',(-23.5726820099204,20.3237750440163,-43.6288620410276));
#20951=CARTESIAN_POINT('Ctrl Pts',(-23.9731936088545,20.346035988815,-43.6512946120207));
#20952=CARTESIAN_POINT('Ctrl Pts',(-24.2149080607951,20.3873281251913,-43.6651257297402));
#20953=CARTESIAN_POINT('Ctrl Pts',(-24.4641986666611,20.45977511806,-43.6808746572005));
#20954=CARTESIAN_POINT('Ctrl Pts',(-24.4787511637168,20.4641160376623,-43.6817992341494));
#20955=CARTESIAN_POINT('Ctrl Pts',(-24.4985797232819,20.4701837163419,-43.683066344267));
#20956=CARTESIAN_POINT('Ctrl Pts',(-24.5038829705225,20.4718215425147,-43.6834059571441));
#20957=CARTESIAN_POINT('Ctrl Pts',(-24.5122759306501,20.4744373478704,-43.6839445783091));
#20958=CARTESIAN_POINT('Ctrl Pts',(-24.5153684618371,20.4754063068497,-43.6841432897073));
#20959=CARTESIAN_POINT('Ctrl Pts',(-24.5213520814412,20.477291024612,-43.6845282494803));
#20960=CARTESIAN_POINT('Ctrl Pts',(-24.5242433503916,20.4782062031824,-43.6847144785845));
#20961=CARTESIAN_POINT('Ctrl Pts',(-24.5311087193042,20.4803899770237,-43.6851572020395));
#20962=CARTESIAN_POINT('Ctrl Pts',(-24.5350816490168,20.4816622079864,-43.6854138160133));
#20963=CARTESIAN_POINT('Ctrl Pts',(-24.543299760506,20.4843114556736,-43.6859454903174));
#20964=CARTESIAN_POINT('Ctrl Pts',(-24.5475445723407,20.4856895831446,-43.6862205869046));
#20965=CARTESIAN_POINT('Ctrl Pts',(-24.5714508312109,20.4935059573867,-43.6877725995387));
#20966=CARTESIAN_POINT('Ctrl Pts',(-24.5910524237005,20.5001244787869,-43.6890554664467));
#20967=CARTESIAN_POINT('Ctrl Pts',(-24.6420907740677,20.517906959013,-43.6924233899346));
#20968=CARTESIAN_POINT('Ctrl Pts',(-24.6734196569644,20.5293708899276,-43.6945183180815));
#20969=CARTESIAN_POINT('Ctrl Pts',(-24.8123832170093,20.5826812133356,-43.7039371486519));
#20970=CARTESIAN_POINT('Ctrl Pts',(-24.9178895854968,20.629804422128,-43.711434387635));
#20971=CARTESIAN_POINT('Ctrl Pts',(-25.1273611009064,20.7372057591243,-43.7270165065939));
#20972=CARTESIAN_POINT('Ctrl Pts',(-25.2309472919627,20.7978416674148,-43.7351011477651));
#20973=CARTESIAN_POINT('Ctrl Pts',(-25.5127154675556,20.9846266102452,-43.7579778811962));
#20974=CARTESIAN_POINT('Ctrl Pts',(-25.6818387317231,21.1233081791136,-43.7728120429735));
#20975=CARTESIAN_POINT('Ctrl Pts',(-25.8444607642891,21.2868741387223,-43.7873606536753));
#20976=CARTESIAN_POINT('Ctrl Pts',(-25.8532044227488,21.2957712689919,-43.7881437297337));
#20977=CARTESIAN_POINT('Ctrl Pts',(-25.8644127238423,21.3073095520401,-43.7891483607205));
#20978=CARTESIAN_POINT('Ctrl Pts',(-25.8669247363571,21.3099042325787,-43.7893735731497));
#20979=CARTESIAN_POINT('Ctrl Pts',(-25.8707576310827,21.313876604251,-43.7897172826972));
#20980=CARTESIAN_POINT('Ctrl Pts',(-25.8720816491104,21.3152512442902,-43.7898360258242));
#20981=CARTESIAN_POINT('Ctrl Pts',(-25.8745668155211,21.3178360192205,-43.7900589294994));
#20982=CARTESIAN_POINT('Ctrl Pts',(-25.8757282358848,21.319045879584,-43.7901631113578));
#20983=CARTESIAN_POINT('Ctrl Pts',(-25.8783985118063,21.3218318760326,-43.7904026634742));
#20984=CARTESIAN_POINT('Ctrl Pts',(-25.879906708732,21.3234086353311,-43.790537981753));
#20985=CARTESIAN_POINT('Ctrl Pts',(-25.8829983585549,21.3266474095249,-43.7908154083975));
#20986=CARTESIAN_POINT('Ctrl Pts',(-25.8845816398346,21.3283095875483,-43.7909575033429));
#20987=CARTESIAN_POINT('Ctrl Pts',(-25.8885964035542,21.3325334391033,-43.7913178733926));
#20988=CARTESIAN_POINT('Ctrl Pts',(-25.8910254611662,21.335097428854,-43.7915359613267));
#20989=CARTESIAN_POINT('Ctrl Pts',(-25.9246373957772,21.3706935010755,-43.7945545605907));
#20990=CARTESIAN_POINT('Ctrl Pts',(-25.9551246576252,21.4043793695039,-43.7973023613202));
#20991=CARTESIAN_POINT('Ctrl Pts',(-26.0588020540511,21.5239203662249,-43.8067287131811));
#20992=CARTESIAN_POINT('Ctrl Pts',(-26.1281944655074,21.6129702010591,-43.813187838189));
#20993=CARTESIAN_POINT('Ctrl Pts',(-26.2176084750917,21.7410506752079,-43.8220053197226));
#20994=CARTESIAN_POINT('Ctrl Pts',(-26.2417178399554,21.7771158531775,-43.8244393960341));
#20995=CARTESIAN_POINT('Ctrl Pts',(-26.2895124925356,21.8518337850288,-43.8294048548734));
#20996=CARTESIAN_POINT('Ctrl Pts',(-26.313124936592,21.8905213876216,-43.8319351524646));
#20997=CARTESIAN_POINT('Ctrl Pts',(-26.4229062984415,22.0792302191516,-43.8441361506689));
#20998=CARTESIAN_POINT('Ctrl Pts',(-26.497711834573,22.2355194720664,-43.8538380577828));
#20999=CARTESIAN_POINT('Ctrl Pts',(-26.5700302623551,22.4242382821998,-43.8656427933311));
#21000=CARTESIAN_POINT('Ctrl Pts',(-26.5800816549773,22.4515710297423,-43.8673540510259));
#21001=CARTESIAN_POINT('Ctrl Pts',(-26.5931986717294,22.4887897154795,-43.8696883603576));
#21002=CARTESIAN_POINT('Ctrl Pts',(-26.5965893012321,22.4985601791344,-43.8703015302585));
#21003=CARTESIAN_POINT('Ctrl Pts',(-26.6172178335677,22.5589403280299,-43.8740935436191));
#21004=CARTESIAN_POINT('Ctrl Pts',(-26.6332403294934,22.6099537648394,-43.8773092123728));
#21005=CARTESIAN_POINT('Ctrl Pts',(-26.650401775007,22.6697589496453,-43.8811007974053));
#21006=CARTESIAN_POINT('Ctrl Pts',(-26.6527833098899,22.6781877136872,-43.8816356638887));
#21007=CARTESIAN_POINT('Ctrl Pts',(-26.6562809560341,22.6907623209282,-43.8824343815505));
#21008=CARTESIAN_POINT('Ctrl Pts',(-26.6574232042868,22.6949009044045,-43.8826973808729));
#21009=CARTESIAN_POINT('Ctrl Pts',(-26.6594454733324,22.7022854774641,-43.8831668816874));
#21010=CARTESIAN_POINT('Ctrl Pts',(-26.6603286910237,22.7055305913927,-43.8833732788157));
#21011=CARTESIAN_POINT('Ctrl Pts',(-26.6621797728984,22.7123740840218,-43.8838087070617));
#21012=CARTESIAN_POINT('Ctrl Pts',(-26.6631464785182,22.7159727685076,-43.8840377754976));
#21013=CARTESIAN_POINT('Ctrl Pts',(-26.6650967834387,22.7232836099785,-43.8845033340359));
#21014=CARTESIAN_POINT('Ctrl Pts',(-26.666079993025,22.726995863867,-43.8847398363881));
#21015=CARTESIAN_POINT('Ctrl Pts',(-26.6684967646987,22.7361870919654,-43.8853256574845));
#21016=CARTESIAN_POINT('Ctrl Pts',(-26.6699225198927,22.7416680890393,-43.8856752291155));
#21017=CARTESIAN_POINT('Ctrl Pts',(-26.6738405014706,22.7568945152182,-43.8866470035722));
#21018=CARTESIAN_POINT('Ctrl Pts',(-26.6763015432764,22.7666478349685,-43.8872702148627));
#21019=CARTESIAN_POINT('Ctrl Pts',(-26.7415982445304,23.0306279515672,-43.9041585040978));
#21020=CARTESIAN_POINT('Ctrl Pts',(-26.7732432702996,23.2914917503899,-43.9214885813748));
#21021=CARTESIAN_POINT('Ctrl Pts',(-26.7730011528923,23.5532336498954,-43.9391856718898));
#21022=CARTESIAN_POINT('Ctrl Pts',(-26.7730011529985,23.5532335351257,-43.9391856641299));
#21023=CARTESIAN_POINT('Ctrl Pts',(-26.7728064224409,23.7637558140599,-43.9534196550246));
#21024=CARTESIAN_POINT('Ctrl Pts',(-26.7519842051116,23.9737757280023,-43.9677792446346));
#21025=CARTESIAN_POINT('Ctrl Pts',(-26.7047525355364,24.2107145975974,-43.9832586569748));
#21026=CARTESIAN_POINT('Ctrl Pts',(-26.698246890775,24.2410579347819,-43.9852263806559));
#21027=CARTESIAN_POINT('Ctrl Pts',(-26.6904240561525,24.2751358443274,-43.9874161333868));
#21028=CARTESIAN_POINT('Ctrl Pts',(-26.68953739194,24.2789661836675,-43.9876619722946));
#21029=CARTESIAN_POINT('Ctrl Pts',(-26.6880837960387,24.2851937449196,-43.9880611900244));
#21030=CARTESIAN_POINT('Ctrl Pts',(-26.6875211247066,24.2875919418643,-43.9882148105837));
#21031=CARTESIAN_POINT('Ctrl Pts',(-26.6864272837871,24.2922301503398,-43.9885116915697));
#21032=CARTESIAN_POINT('Ctrl Pts',(-26.6858964628286,24.2944702414108,-43.9886549719671));
#21033=CARTESIAN_POINT('Ctrl Pts',(-26.6849311846578,24.2985243971933,-43.9889140950309));
#21034=CARTESIAN_POINT('Ctrl Pts',(-26.6844975540301,24.3003386481243,-43.9890299851679));
#21035=CARTESIAN_POINT('Ctrl Pts',(-26.6835573191463,24.3042574103085,-43.9892801584192));
#21036=CARTESIAN_POINT('Ctrl Pts',(-26.6830501711172,24.3063617820915,-43.9894144091693));
#21037=CARTESIAN_POINT('Ctrl Pts',(-26.6816675884769,24.3120734315302,-43.9897785441984));
#21038=CARTESIAN_POINT('Ctrl Pts',(-26.6807880377044,24.31567972432,-43.9900081897754));
#21039=CARTESIAN_POINT('Ctrl Pts',(-26.676602161561,24.3327145505152,-43.9910917272369));
#21040=CARTESIAN_POINT('Ctrl Pts',(-26.6732155873367,24.3461234938437,-43.9919410316794));
#21041=CARTESIAN_POINT('Ctrl Pts',(-26.6125353569683,24.5800308387846,-44.0067000471658));
#21042=CARTESIAN_POINT('Ctrl Pts',(-26.532095525908,24.793903359641,-44.0193446485638));
#21043=CARTESIAN_POINT('Ctrl Pts',(-26.4095802799876,25.037659597885,-44.0345883897453));
#21044=CARTESIAN_POINT('Ctrl Pts',(-26.3885729915567,25.077364798808,-44.0370985389698));
#21045=CARTESIAN_POINT('Ctrl Pts',(-26.3452575063813,25.1552506237087,-44.0420962992416));
#21046=CARTESIAN_POINT('Ctrl Pts',(-26.322979885118,25.1934368176919,-44.0445830912485));
#21047=CARTESIAN_POINT('Ctrl Pts',(-26.2341824592457,25.3386946082248,-44.0542170830922));
#21048=CARTESIAN_POINT('Ctrl Pts',(-26.1621944183185,25.4422778503158,-44.0614652258796));
#21049=CARTESIAN_POINT('Ctrl Pts',(-26.0499242335088,25.5851629186638,-44.0722407816024));
#21050=CARTESIAN_POINT('Ctrl Pts',(-26.0143898338377,25.628050808158,-44.0755842125731));
#21051=CARTESIAN_POINT('Ctrl Pts',(-25.9730248206347,25.6754216798197,-44.0794118503892));
#21052=CARTESIAN_POINT('Ctrl Pts',(-25.9682677311354,25.6808327264182,-44.0798511089894));
#21053=CARTESIAN_POINT('Ctrl Pts',(-25.9605173452598,25.689589167691,-44.080565279666));
#21054=CARTESIAN_POINT('Ctrl Pts',(-25.9575351157197,25.6929443606694,-44.0808397284495));
#21055=CARTESIAN_POINT('Ctrl Pts',(-25.9517554211544,25.6994195784357,-44.0813709473472));
#21056=CARTESIAN_POINT('Ctrl Pts',(-25.9489588602203,25.7025404009419,-44.0816276791472));
#21057=CARTESIAN_POINT('Ctrl Pts',(-25.9441262661089,25.7079122172302,-44.0820708061248));
#21058=CARTESIAN_POINT('Ctrl Pts',(-25.9420931202541,25.7101658109076,-44.0822570790823));
#21059=CARTESIAN_POINT('Ctrl Pts',(-25.9378877511288,25.7148139361769,-44.0826420445012));
#21060=CARTESIAN_POINT('Ctrl Pts',(-25.9357151027817,25.7172080773116,-44.082840754887));
#21061=CARTESIAN_POINT('Ctrl Pts',(-25.9298291560608,25.7236744933328,-44.0833786086417));
#21062=CARTESIAN_POINT('Ctrl Pts',(-25.926109020974,25.7277405055549,-44.0837180427182));
#21063=CARTESIAN_POINT('Ctrl Pts',(-25.9122732346699,25.7427849978114,-44.0849785879073));
#21064=CARTESIAN_POINT('Ctrl Pts',(-25.9020918902868,25.7537025618919,-44.0859025068547));
#21065=CARTESIAN_POINT('Ctrl Pts',(-25.7249126951009,25.9410667050012,-44.10191929494));
#21066=CARTESIAN_POINT('Ctrl Pts',(-25.5386029604331,26.0981055208699,-44.1179163434642));
#21067=CARTESIAN_POINT('Ctrl Pts',(-25.2694125362097,26.2773566600447,-44.139741262783));
#21068=CARTESIAN_POINT('Ctrl Pts',(-25.2007050358146,26.3194788565966,-44.1452046211406));
#21069=CARTESIAN_POINT('Ctrl Pts',(-25.0563156160717,26.4007148344623,-44.156401997556));
#21070=CARTESIAN_POINT('Ctrl Pts',(-24.9805117191027,26.4394948642049,-44.1621297489368));
#21071=CARTESIAN_POINT('Ctrl Pts',(-24.8420217959087,26.5035561143908,-44.1722350791115));
#21072=CARTESIAN_POINT('Ctrl Pts',(-24.7799058072096,26.5299545412802,-44.1766437670589));
#21073=CARTESIAN_POINT('Ctrl Pts',(-24.6992215948731,26.5612908082457,-44.1821740004241));
#21074=CARTESIAN_POINT('Ctrl Pts',(-24.6813792770177,26.568038762912,-44.1833848449165));
#21075=CARTESIAN_POINT('Ctrl Pts',(-24.6525719671542,26.5786422806434,-44.1853192115192));
#21076=CARTESIAN_POINT('Ctrl Pts',(-24.6416444914597,26.582597533392,-44.1860482387957));
#21077=CARTESIAN_POINT('Ctrl Pts',(-24.6283427683745,26.5873309372046,-44.1869297137504));
#21078=CARTESIAN_POINT('Ctrl Pts',(-24.6259888917026,26.5881654803317,-44.1870854740507));
#21079=CARTESIAN_POINT('Ctrl Pts',(-24.6214402312325,26.5897722121947,-44.1873860279881));
#21080=CARTESIAN_POINT('Ctrl Pts',(-24.6192455777557,26.5905447616199,-44.1875308430383));
#21081=CARTESIAN_POINT('Ctrl Pts',(-24.6152883148327,26.5919329601594,-44.1877916066426));
#21082=CARTESIAN_POINT('Ctrl Pts',(-24.6135260111995,26.5925494527908,-44.1879076055729));
#21083=CARTESIAN_POINT('Ctrl Pts',(-24.6097367155983,26.5938713371232,-44.1881567504995));
#21084=CARTESIAN_POINT('Ctrl Pts',(-24.6077095600623,26.5945762335898,-44.1882898664103));
#21085=CARTESIAN_POINT('Ctrl Pts',(-24.6022489584266,26.5964689192764,-44.1886479933995));
#21086=CARTESIAN_POINT('Ctrl Pts',(-24.5988141924936,26.5976529329612,-44.1888727788367));
#21087=CARTESIAN_POINT('Ctrl Pts',(-24.5830174690146,26.6030684235343,-44.1899044112115));
#21088=CARTESIAN_POINT('Ctrl Pts',(-24.5706316231403,26.6072305834148,-44.190707184202));
#21089=CARTESIAN_POINT('Ctrl Pts',(-24.3529866087256,26.6788981979001,-44.2047123418067));
#21090=CARTESIAN_POINT('Ctrl Pts',(-24.1414395626157,26.7256792846855,-44.2167701713485));
#21091=CARTESIAN_POINT('Ctrl Pts',(-23.7642556063533,26.7700502779302,-44.2379933954064));
#21092=CARTESIAN_POINT('Ctrl Pts',(-23.6005244821389,26.7767619929972,-44.2471175930084));
#21093=CARTESIAN_POINT('Ctrl Pts',(-23.3318620279809,26.7673150131332,-44.2626357384577));
#21094=CARTESIAN_POINT('Ctrl Pts',(-23.2269768729407,26.7584724148352,-44.2688281660583));
#21095=CARTESIAN_POINT('Ctrl Pts',(-23.1011371574599,26.741629517725,-44.2765016065565));
#21096=CARTESIAN_POINT('Ctrl Pts',(-23.0795854805883,26.7385223096761,-44.277824364355));
#21097=CARTESIAN_POINT('Ctrl Pts',(-23.053590284159,26.7345051437122,-44.2794307099017));
#21098=CARTESIAN_POINT('Ctrl Pts',(-23.049114702704,26.7338038445044,-44.279707663284));
#21099=CARTESIAN_POINT('Ctrl Pts',(-23.0404725949796,26.7324309977076,-44.2802432043376));
#21100=CARTESIAN_POINT('Ctrl Pts',(-23.0363058776558,26.7317606976387,-44.2805017519178));
#21101=CARTESIAN_POINT('Ctrl Pts',(-23.0291406774643,26.7305935881853,-44.2809469485592));
#21102=CARTESIAN_POINT('Ctrl Pts',(-23.0261415513006,26.7301007168043,-44.2811334721052));
#21103=CARTESIAN_POINT('Ctrl Pts',(-23.0199652520881,26.7290767388683,-44.2815179616249));
#21104=CARTESIAN_POINT('Ctrl Pts',(-23.0167881698206,26.7285451100312,-44.2817159440528));
#21105=CARTESIAN_POINT('Ctrl Pts',(-23.0091394957951,26.727253447292,-44.2821930648784));
#21106=CARTESIAN_POINT('Ctrl Pts',(-23.0046687097978,26.726488736432,-44.2824723520327));
#21107=CARTESIAN_POINT('Ctrl Pts',(-22.9909463680264,26.7241117548851,-44.2833308198402));
#21108=CARTESIAN_POINT('Ctrl Pts',(-22.9817002951605,26.7224684929247,-44.2839109874938));
#21109=CARTESIAN_POINT('Ctrl Pts',(-22.947640556665,26.7162615202366,-44.2860546331614));
#21110=CARTESIAN_POINT('Ctrl Pts',(-22.9228740627714,26.711446974669,-44.2876260954237));
#21111=CARTESIAN_POINT('Ctrl Pts',(-22.8922636534636,26.7051225033921,-44.2895845807344));
#21112=CARTESIAN_POINT('Ctrl Pts',(-22.8863635684173,26.7038862050682,-44.2899628229004));
#21113=CARTESIAN_POINT('Ctrl Pts',(-22.8737533468999,26.7012069146758,-44.2907728478956));
#21114=CARTESIAN_POINT('Ctrl Pts',(-22.8670442910972,26.6997590278718,-44.2912047845563));
#21115=CARTESIAN_POINT('Ctrl Pts',(-22.8587964581718,26.6979514622926,-44.2917369974765));
#21116=CARTESIAN_POINT('Ctrl Pts',(-22.8572532143058,26.6976120607894,-44.2918366313904));
#21117=CARTESIAN_POINT('Ctrl Pts',(-22.8529687294189,26.6966664814866,-44.2921133883212));
#21118=CARTESIAN_POINT('Ctrl Pts',(-22.8502280347373,26.6960578575121,-44.2922905885265));
#21119=CARTESIAN_POINT('Ctrl Pts',(-22.8343836352574,26.692517572628,-44.2933159655243));
#21120=CARTESIAN_POINT('Ctrl Pts',(-22.8212977139485,26.689507655021,-44.2941666019462));
#21121=CARTESIAN_POINT('Ctrl Pts',(-22.8043610757859,26.685500418919,-44.2952724825394));
#21122=CARTESIAN_POINT('Ctrl Pts',(-22.8004927226181,26.6845775956935,-44.2955254015406));
#21123=CARTESIAN_POINT('Ctrl Pts',(-22.7917864137743,26.6824836036253,-44.2960953876416));
#21124=CARTESIAN_POINT('Ctrl Pts',(-22.7869494512413,26.6813083834694,-44.2964125795543));
#21125=CARTESIAN_POINT('Ctrl Pts',(-22.7672935746408,26.676484408575,-44.2977036846719));
#21126=CARTESIAN_POINT('Ctrl Pts',(-22.7524981257123,26.6727416624544,-44.2986804777368));
#21127=CARTESIAN_POINT('Ctrl Pts',(-22.5923816023055,26.6310253314078,-44.3093051795325));
#21128=CARTESIAN_POINT('Ctrl Pts',(-22.4498757888398,26.5830464593163,-44.3192564266551));
#21129=CARTESIAN_POINT('Ctrl Pts',(-22.2310392747397,26.4919091114387,-44.3352088536775));
#21130=CARTESIAN_POINT('Ctrl Pts',(-22.1522381483177,26.4552849687086,-44.3410963813956));
#21131=CARTESIAN_POINT('Ctrl Pts',(-22.0750358850059,26.4155367074495,-44.3469709746179));
#21132=CARTESIAN_POINT('Ctrl Pts',(-22.0750360439056,26.4155367892604,-44.590879968079));
#21133=CARTESIAN_POINT('Ctrl Pts',(-22.0939080709219,26.4252532162916,-44.5894652751221));
#21134=CARTESIAN_POINT('Ctrl Pts',(-22.1128785974627,26.4347844837046,-44.588055277812));
#21135=CARTESIAN_POINT('Ctrl Pts',(-22.2024727047585,26.4786951348385,-44.5814568536133));
#21136=CARTESIAN_POINT('Ctrl Pts',(-22.2742473122324,26.5106747138146,-44.5763462405824));
#21137=CARTESIAN_POINT('Ctrl Pts',(-22.3614803433788,26.5457788114761,-44.5704007074401));
#21138=CARTESIAN_POINT('Ctrl Pts',(-22.3758774018533,26.5514523061039,-44.5694279513745));
#21139=CARTESIAN_POINT('Ctrl Pts',(-22.393785436603,26.5583607837284,-44.5682289883443));
#21140=CARTESIAN_POINT('Ctrl Pts',(-22.397258102119,26.5596935501703,-44.5679970012262));
#21141=CARTESIAN_POINT('Ctrl Pts',(-22.4027364778163,26.5617852091252,-44.5676318402594));
#21142=CARTESIAN_POINT('Ctrl Pts',(-22.4047406375414,26.5625481117396,-44.5674984247915));
#21143=CARTESIAN_POINT('Ctrl Pts',(-22.4084913993002,26.5639715905979,-44.5672490624772));
#21144=CARTESIAN_POINT('Ctrl Pts',(-22.4102378021263,26.5646326447256,-44.5671330873654));
#21145=CARTESIAN_POINT('Ctrl Pts',(-22.4141640654205,26.5661149266703,-44.5668726459375));
#21146=CARTESIAN_POINT('Ctrl Pts',(-22.4163442376663,26.5669353074364,-44.5667282313953));
#21147=CARTESIAN_POINT('Ctrl Pts',(-22.4218956069895,26.569017373432,-44.5663610211165));
#21148=CARTESIAN_POINT('Ctrl Pts',(-22.4252680419937,26.5702757795291,-44.566138422687));
#21149=CARTESIAN_POINT('Ctrl Pts',(-22.4439943671323,26.5772276873519,-44.5649050136516));
#21150=CARTESIAN_POINT('Ctrl Pts',(-22.4593897344955,26.5828098854831,-44.5639007885651));
#21151=CARTESIAN_POINT('Ctrl Pts',(-22.7748517307943,26.6944798336812,-44.543510098824));
#21152=CARTESIAN_POINT('Ctrl Pts',(-23.0890093136093,26.7556770305349,-44.5265119161997));
#21153=CARTESIAN_POINT('Ctrl Pts',(-23.5826415731307,26.7776274072564,-44.4985216854913));
#21154=CARTESIAN_POINT('Ctrl Pts',(-23.7585134945245,26.7710616324607,-44.4883279238951));
#21155=CARTESIAN_POINT('Ctrl Pts',(-23.9410319873616,26.7492328525504,-44.4771513848425));
#21156=CARTESIAN_POINT('Ctrl Pts',(-23.9491017435406,26.7482367374884,-44.4766560501961));
#21157=CARTESIAN_POINT('Ctrl Pts',(-23.962004530246,26.74659444539,-44.4758621326672));
#21158=CARTESIAN_POINT('Ctrl Pts',(-23.9668400497666,26.7459678157792,-44.4755641671165));
#21159=CARTESIAN_POINT('Ctrl Pts',(-23.9760452796345,26.7447536723811,-44.4749961075253));
#21160=CARTESIAN_POINT('Ctrl Pts',(-23.9804152464805,26.7441681599708,-44.4747260773252));
#21161=CARTESIAN_POINT('Ctrl Pts',(-23.9880851899923,26.7431244717508,-44.4742515017066));
#21162=CARTESIAN_POINT('Ctrl Pts',(-23.9913856906121,26.7426701419453,-44.4740470784323));
#21163=CARTESIAN_POINT('Ctrl Pts',(-23.9978318735311,26.741772606366,-44.4736474166093));
#21164=CARTESIAN_POINT('Ctrl Pts',(-24.0009776177882,26.741329865592,-44.4734521930138));
#21165=CARTESIAN_POINT('Ctrl Pts',(-24.0084473419851,26.7402672901807,-44.4729881755901));
#21166=CARTESIAN_POINT('Ctrl Pts',(-24.0127707187578,26.7396433151954,-44.4727192506367));
#21167=CARTESIAN_POINT('Ctrl Pts',(-24.0280263114848,26.7374098672805,-44.4717690420173));
#21168=CARTESIAN_POINT('Ctrl Pts',(-24.0389514098522,26.7357529740163,-44.4710862546508));
#21169=CARTESIAN_POINT('Ctrl Pts',(-24.1890481373595,26.7121990784579,-44.461673380567));
#21170=CARTESIAN_POINT('Ctrl Pts',(-24.3266266071022,26.6812586436298,-44.4526534228665));
#21171=CARTESIAN_POINT('Ctrl Pts',(-24.6115447361728,26.5972467807794,-44.4331197079007));
#21172=CARTESIAN_POINT('Ctrl Pts',(-24.7579434283226,26.5422402306996,-44.4225734931525));
#21173=CARTESIAN_POINT('Ctrl Pts',(-24.9714475392082,26.4437889976112,-44.4066583802809));
#21174=CARTESIAN_POINT('Ctrl Pts',(-25.0418928578784,26.4081115497507,-44.4013164795713));
#21175=CARTESIAN_POINT('Ctrl Pts',(-25.2237970862564,26.3074249545266,-44.3873790050684));
#21176=CARTESIAN_POINT('Ctrl Pts',(-25.3328005342051,26.2382410863217,-44.3788766457892));
#21177=CARTESIAN_POINT('Ctrl Pts',(-25.4438555731693,26.1580195816999,-44.370274693111));
#21178=CARTESIAN_POINT('Ctrl Pts',(-25.4503183301819,26.1533144653481,-44.3697743516584));
#21179=CARTESIAN_POINT('Ctrl Pts',(-25.4591185747322,26.1468573387428,-44.3690934514519));
#21180=CARTESIAN_POINT('Ctrl Pts',(-25.4614712158099,26.1451261771537,-44.3689114608231));
#21181=CARTESIAN_POINT('Ctrl Pts',(-25.4654044235199,26.1422237243919,-44.3686072755992));
#21182=CARTESIAN_POINT('Ctrl Pts',(-25.4669862710729,26.1410541846417,-44.3684849585616));
#21183=CARTESIAN_POINT('Ctrl Pts',(-25.4701001646737,26.1387475131164,-44.3682442153143));
#21184=CARTESIAN_POINT('Ctrl Pts',(-25.4716322718291,26.1376104692315,-44.3681257832574));
#21185=CARTESIAN_POINT('Ctrl Pts',(-25.4750088352727,26.1350999203895,-44.3678648146011));
#21186=CARTESIAN_POINT('Ctrl Pts',(-25.4768528361952,26.133725798013,-44.3677223214244));
#21187=CARTESIAN_POINT('Ctrl Pts',(-25.4832930663349,26.1289159032263,-44.3672247458874));
#21188=CARTESIAN_POINT('Ctrl Pts',(-25.487881623635,26.1254698032097,-44.3668703853822));
#21189=CARTESIAN_POINT('Ctrl Pts',(-25.5343508780332,26.0903759306731,-44.3632829921509));
#21190=CARTESIAN_POINT('Ctrl Pts',(-25.5754645642451,26.0577194076122,-44.3601196709919));
#21191=CARTESIAN_POINT('Ctrl Pts',(-25.623976105572,26.0172147386756,-44.3563751719887));
#21192=CARTESIAN_POINT('Ctrl Pts',(-25.6321532660555,26.010317841633,-44.3557435742859));
#21193=CARTESIAN_POINT('Ctrl Pts',(-25.7773001512882,25.8866539581371,-44.3445219058685));
#21194=CARTESIAN_POINT('Ctrl Pts',(-25.9042986776505,25.7586438255213,-44.3345205643541));
#21195=CARTESIAN_POINT('Ctrl Pts',(-26.1171650045232,25.5047280966557,-44.3160049273764));
#21196=CARTESIAN_POINT('Ctrl Pts',(-26.2060855198365,25.3820716587437,-44.3075312779911));
#21197=CARTESIAN_POINT('Ctrl Pts',(-26.3279667414487,25.1863175570599,-44.2941939611924));
#21198=CARTESIAN_POINT('Ctrl Pts',(-26.367375799719,25.117485771569,-44.2895385493286));
#21199=CARTESIAN_POINT('Ctrl Pts',(-26.422874155559,25.0116826216806,-44.2823876951746));
#21200=CARTESIAN_POINT('Ctrl Pts',(-26.440875565869,24.9757458333644,-44.2799598988517));
#21201=CARTESIAN_POINT('Ctrl Pts',(-26.4614231750913,24.932735431567,-44.2770522040719));
#21202=CARTESIAN_POINT('Ctrl Pts',(-26.4646232113001,24.9259767132744,-44.2765952283441));
#21203=CARTESIAN_POINT('Ctrl Pts',(-26.469510454303,24.9155609086803,-44.2758908781075));
#21204=CARTESIAN_POINT('Ctrl Pts',(-26.4712143923038,24.9119116636408,-44.27564408396));
#21205=CARTESIAN_POINT('Ctrl Pts',(-26.4743065046176,24.9052569176684,-44.27519399018));
#21206=CARTESIAN_POINT('Ctrl Pts',(-26.4756968988445,24.902252449282,-44.2749907677016));
#21207=CARTESIAN_POINT('Ctrl Pts',(-26.4785015903821,24.8961672778013,-44.2745791330657));
#21208=CARTESIAN_POINT('Ctrl Pts',(-26.4799156612509,24.8930864755126,-44.2743707134046));
#21209=CARTESIAN_POINT('Ctrl Pts',(-26.4839407810036,24.8842804228967,-44.2737749218644));
#21210=CARTESIAN_POINT('Ctrl Pts',(-26.4865399152792,24.8785497720521,-44.2733871397327));
#21211=CARTESIAN_POINT('Ctrl Pts',(-26.4976221638633,24.8539238132396,-44.2717204464071));
#21212=CARTESIAN_POINT('Ctrl Pts',(-26.5059396468539,24.8349549112277,-44.2704358587337));
#21213=CARTESIAN_POINT('Ctrl Pts',(-26.6537554979134,24.4888102377743,-44.2469768269609));
#21214=CARTESIAN_POINT('Ctrl Pts',(-26.7382953999085,24.140901122623,-44.2226997416912));
#21215=CARTESIAN_POINT('Ctrl Pts',(-26.770140375584,23.7074329332471,-44.1935053817704));
#21216=CARTESIAN_POINT('Ctrl Pts',(-26.7730299190195,23.6282965878572,-44.1882362982356));
#21217=CARTESIAN_POINT('Ctrl Pts',(-26.7730005616036,23.5440366669574,-44.1827398891842));
#21218=CARTESIAN_POINT('Ctrl Pts',(-26.7729867141529,23.5389436382277,-44.1824081078875));
#21219=CARTESIAN_POINT('Ctrl Pts',(-26.7729169771423,23.525241440422,-44.1815167226417));
#21220=CARTESIAN_POINT('Ctrl Pts',(-26.7728386624681,23.5166323677089,-44.1809579765281));
#21221=CARTESIAN_POINT('Ctrl Pts',(-26.7727004529541,23.5060856473388,-44.1802751583279));
#21222=CARTESIAN_POINT('Ctrl Pts',(-26.7726733084472,23.504147689381,-44.1801497603201));
#21223=CARTESIAN_POINT('Ctrl Pts',(-26.7719593807288,23.4562621398112,-44.1770530067836));
#21224=CARTESIAN_POINT('Ctrl Pts',(-26.7702916363931,23.4103313920859,-44.1741222338254));
#21225=CARTESIAN_POINT('Ctrl Pts',(-26.7673545128391,23.3594718680321,-44.1709323058993));
#21226=CARTESIAN_POINT('Ctrl Pts',(-26.76705552291,23.3544951941257,-44.1706207557786));
#21227=CARTESIAN_POINT('Ctrl Pts',(-26.7665915023988,23.3470598647845,-44.1701561887559));
#21228=CARTESIAN_POINT('Ctrl Pts',(-26.7664352005285,23.3446007017767,-44.170002684877));
#21229=CARTESIAN_POINT('Ctrl Pts',(-26.7661613664911,23.3403690298846,-44.1697387949705));
#21230=CARTESIAN_POINT('Ctrl Pts',(-26.7660451892934,23.3385964393573,-44.1696283323728));
#21231=CARTESIAN_POINT('Ctrl Pts',(-26.7658018452044,23.3349300350442,-44.1694000141655));
#21232=CARTESIAN_POINT('Ctrl Pts',(-26.765674471066,23.3330362408672,-44.1692821710267));
#21233=CARTESIAN_POINT('Ctrl Pts',(-26.76537091793,23.3285818008578,-44.1690051971424));
#21234=CARTESIAN_POINT('Ctrl Pts',(-26.7651933523251,23.3260212440186,-44.168846145083));
#21235=CARTESIAN_POINT('Ctrl Pts',(-26.7646042467549,23.317670701931,-44.1683279600743));
#21236=CARTESIAN_POINT('Ctrl Pts',(-26.7641801200287,23.311881573237,-44.1679695349507));
#21237=CARTESIAN_POINT('Ctrl Pts',(-26.7534026977402,23.1700349876353,-44.1592065764107));
#21238=CARTESIAN_POINT('Ctrl Pts',(-26.734432811212,23.0347499129251,-44.1512813715373));
#21239=CARTESIAN_POINT('Ctrl Pts',(-26.634435542464,22.5485165809761,-44.1230809506669));
#21240=CARTESIAN_POINT('Ctrl Pts',(-26.5034047872842,22.2106413311036,-44.1037060853067));
#21241=CARTESIAN_POINT('Ctrl Pts',(-26.3088087132513,21.8838485870156,-44.0807052283262));
#21242=CARTESIAN_POINT('Ctrl Pts',(-26.2981977652514,21.8664083354568,-44.079464753495));
#21243=CARTESIAN_POINT('Ctrl Pts',(-26.2841191877998,21.8437561740551,-44.0778361073457));
#21244=CARTESIAN_POINT('Ctrl Pts',(-26.2808008987597,21.8384516302325,-44.0774534582676));
#21245=CARTESIAN_POINT('Ctrl Pts',(-26.275664901501,21.8302942707367,-44.0768630564061));
#21246=CARTESIAN_POINT('Ctrl Pts',(-26.2738581012997,21.8274345767124,-44.0766557086453));
#21247=CARTESIAN_POINT('Ctrl Pts',(-26.2702567076883,21.8217543334991,-44.0762431068013));
#21248=CARTESIAN_POINT('Ctrl Pts',(-26.268462221066,21.8189337213476,-44.0760378568659));
#21249=CARTESIAN_POINT('Ctrl Pts',(-26.2644826113276,21.8126999247376,-44.0755834233583));
#21250=CARTESIAN_POINT('Ctrl Pts',(-26.262295434747,21.8092880636795,-44.0753341634085));
#21251=CARTESIAN_POINT('Ctrl Pts',(-26.2559904048339,21.7994933185549,-44.0746170274513));
#21252=CARTESIAN_POINT('Ctrl Pts',(-26.2518564337723,21.7931208874432,-44.0741485490933));
#21253=CARTESIAN_POINT('Ctrl Pts',(-26.2244425678996,21.7511884182704,-44.0710531028079));
#21254=CARTESIAN_POINT('Ctrl Pts',(-26.2004846114187,21.716078690838,-44.068400697592));
#21255=CARTESIAN_POINT('Ctrl Pts',(-26.127985994073,21.6142209958959,-44.0605204588349));
#21256=CARTESIAN_POINT('Ctrl Pts',(-26.0775707774778,21.5488559088993,-44.0552217598652));
#21257=CARTESIAN_POINT('Ctrl Pts',(-25.8333490901618,21.2561739553779,-44.0303464685409));
#21258=CARTESIAN_POINT('Ctrl Pts',(-25.6110809087874,21.0546022860257,-44.0096746401498));
#21259=CARTESIAN_POINT('Ctrl Pts',(-25.2904641200018,20.8362601068329,-43.9840249187697));
#21260=CARTESIAN_POINT('Ctrl Pts',(-25.2145923435694,20.7890810955855,-43.9782288179988));
#21261=CARTESIAN_POINT('Ctrl Pts',(-25.1312783365336,20.7419583953759,-43.9722283849153));
#21262=CARTESIAN_POINT('Ctrl Pts',(-25.1256962377857,20.7388230585876,-43.971828059682));
#21263=CARTESIAN_POINT('Ctrl Pts',(-25.1179424014397,20.7344982516968,-43.9712743909393));
#21264=CARTESIAN_POINT('Ctrl Pts',(-25.1157786286348,20.7332946454408,-43.9711201439557));
#21265=CARTESIAN_POINT('Ctrl Pts',(-25.1120573262834,20.731230269832,-43.9708553142887));
#21266=CARTESIAN_POINT('Ctrl Pts',(-25.1105004712808,20.7303682971328,-43.9707446537968));
#21267=CARTESIAN_POINT('Ctrl Pts',(-25.1072832510673,20.7285905220069,-43.9705162541773));
#21268=CARTESIAN_POINT('Ctrl Pts',(-25.105622794694,20.7276748971597,-43.9703985270504));
#21269=CARTESIAN_POINT('Ctrl Pts',(-25.1017228159079,20.7255288196915,-43.9701223747253));
#21270=CARTESIAN_POINT('Ctrl Pts',(-25.0994826305223,20.7242995609351,-43.9699640268711));
#21271=CARTESIAN_POINT('Ctrl Pts',(-25.0923242656936,20.7203826156539,-43.9694589121017));
#21272=CARTESIAN_POINT('Ctrl Pts',(-25.0874005016209,20.7177050750432,-43.9691127950465));
#21273=CARTESIAN_POINT('Ctrl Pts',(-25.0758334850618,20.7114539796289,-43.968302716921));
#21274=CARTESIAN_POINT('Ctrl Pts',(-25.0691845881576,20.7078908596037,-43.9678394063338));
#21275=CARTESIAN_POINT('Ctrl Pts',(-24.998481256975,20.6703201379484,-43.9629367112537));
#21276=CARTESIAN_POINT('Ctrl Pts',(-24.9333031374764,20.6384575685772,-43.9586263181298));
#21277=CARTESIAN_POINT('Ctrl Pts',(-24.7944778716177,20.5763070307247,-43.9497624106067));
#21278=CARTESIAN_POINT('Ctrl Pts',(-24.7206727173662,20.5464938034426,-43.9452287928722));
#21279=CARTESIAN_POINT('Ctrl Pts',(-24.383733114627,20.4246962089417,-43.9250168060919));
#21280=CARTESIAN_POINT('Ctrl Pts',(-24.1104678493923,20.3643543338467,-43.9098104778768));
#21281=CARTESIAN_POINT('Ctrl Pts',(-23.7604754597425,20.3335458310424,-43.8891203309641));
#21282=CARTESIAN_POINT('Ctrl Pts',(-23.6879147657029,20.3296247159069,-43.8847746886013));
#21283=CARTESIAN_POINT('Ctrl Pts',(-23.6058349411253,20.3279680086924,-43.8797747874892));
#21284=CARTESIAN_POINT('Ctrl Pts',(-23.5963815818106,20.3278188148966,-43.8791976867926));
#21285=CARTESIAN_POINT('Ctrl Pts',(-23.5824777448033,20.3276605774545,-43.8783470173325));
#21286=CARTESIAN_POINT('Ctrl Pts',(-23.5780276258794,20.3276191501693,-43.8780744654394));
#21287=CARTESIAN_POINT('Ctrl Pts',(-23.5701809476437,20.327562357695,-43.8775933835428));
#21288=CARTESIAN_POINT('Ctrl Pts',(-23.5667844159003,20.327543144235,-43.8773849746575));
#21289=CARTESIAN_POINT('Ctrl Pts',(-23.5597694582857,20.3275145523151,-43.8769541948769));
#21290=CARTESIAN_POINT('Ctrl Pts',(-23.5561510356956,20.3275058982921,-43.8767318015334));
#21291=CARTESIAN_POINT('Ctrl Pts',(-23.5469030809893,20.3274993553895,-43.8761629185265));
#21292=CARTESIAN_POINT('Ctrl Pts',(-23.541273572088,20.3275101231479,-43.8758161575446));
#21293=CARTESIAN_POINT('Ctrl Pts',(-23.5187936219518,20.3276120234177,-43.8744295827964));
#21294=CARTESIAN_POINT('Ctrl Pts',(-23.5019442172992,20.3278205622038,-43.8733860900485));
#21295=CARTESIAN_POINT('Ctrl Pts',(-23.2847025608547,20.3322134830783,-43.8598762763329));
#21296=CARTESIAN_POINT('Ctrl Pts',(-23.0851615594973,20.3549504286628,-43.8468109571785));
#21297=CARTESIAN_POINT('Ctrl Pts',(-22.655950357664,20.4449237468844,-43.8174216336159));
#21298=CARTESIAN_POINT('Ctrl Pts',(-22.428984400246,20.5194766173101,-43.8010244730725));
#21299=CARTESIAN_POINT('Ctrl Pts',(-22.2072485861976,20.6206640189016,-43.7851176388257));
#21300=CARTESIAN_POINT('Ctrl Pts',(-22.2021983029271,20.6229844795703,-43.7847554412038));
#21301=CARTESIAN_POINT('Ctrl Pts',(-22.1944923495493,20.626549316318,-43.7842029606378));
#21302=CARTESIAN_POINT('Ctrl Pts',(-22.1918323557627,20.6277842617501,-43.7840122839371));
#21303=CARTESIAN_POINT('Ctrl Pts',(-22.1858146767193,20.6305880582221,-43.7835809968639));
#21304=CARTESIAN_POINT('Ctrl Pts',(-22.1824579987125,20.6321590764513,-43.7833404795384));
#21305=CARTESIAN_POINT('Ctrl Pts',(-22.176432228506,20.634991985308,-43.7829088224254));
#21306=CARTESIAN_POINT('Ctrl Pts',(-22.1737621512612,20.636251757592,-43.7827175897463));
#21307=CARTESIAN_POINT('Ctrl Pts',(-22.1700524036658,20.6380082945575,-43.7824519528234));
#21308=CARTESIAN_POINT('Ctrl Pts',(-22.1690112710182,20.638501946572,-43.7823774087126));
#21309=CARTESIAN_POINT('Ctrl Pts',(-22.1651796896409,20.6403212045782,-43.7821030949611));
#21310=CARTESIAN_POINT('Ctrl Pts',(-22.1623908733598,20.6416502687856,-43.7819034822858));
#21311=CARTESIAN_POINT('Ctrl Pts',(-22.1582726146511,20.6436201760141,-43.7816087866479));
#21312=CARTESIAN_POINT('Ctrl Pts',(-22.1569417026505,20.6442579215438,-43.7815135601734));
#21313=CARTESIAN_POINT('Ctrl Pts',(-22.1532783696489,20.6460164102133,-43.7812514816206));
#21314=CARTESIAN_POINT('Ctrl Pts',(-22.1509468544462,20.6471390512311,-43.7810847185771));
#21315=CARTESIAN_POINT('Ctrl Pts',(-22.1131200866666,20.6654090623793,-43.7783797486821));
#21316=CARTESIAN_POINT('Ctrl Pts',(-22.0779389891969,20.6832044519755,-43.7758727072152));
#21317=CARTESIAN_POINT('Ctrl Pts',(-22.038869602058,20.7038755336643,-43.7731058153627));
#21318=CARTESIAN_POINT('Ctrl Pts',(-22.0346527949085,20.7061186013979,-43.7728074094154));
#21319=CARTESIAN_POINT('Ctrl Pts',(-22.0283145769239,20.7095082209585,-43.7723592416358));
#21320=CARTESIAN_POINT('Ctrl Pts',(-22.0261894644702,20.7106477802604,-43.7722090388073));
#21321=CARTESIAN_POINT('Ctrl Pts',(-22.0225132335267,20.7126244189981,-43.7719493118801));
#21322=CARTESIAN_POINT('Ctrl Pts',(-22.0209615230498,20.7134603856175,-43.7718397166471));
#21323=CARTESIAN_POINT('Ctrl Pts',(-22.0177319364094,20.7152037091745,-43.7716116865637));
#21324=CARTESIAN_POINT('Ctrl Pts',(-22.0160541818713,20.7161112817807,-43.7714932663394));
#21325=CARTESIAN_POINT('Ctrl Pts',(-22.0120729590632,20.7182694747473,-43.7712123549382));
#21326=CARTESIAN_POINT('Ctrl Pts',(-22.0097702021025,20.7195214203333,-43.7710499489061));
#21327=CARTESIAN_POINT('Ctrl Pts',(-22.0022314375228,20.7236319625877,-43.7705184994234));
#21328=CARTESIAN_POINT('Ctrl Pts',(-21.9970017996363,20.7265023100199,-43.770150205448));
#21329=CARTESIAN_POINT('Ctrl Pts',(-21.9846454581716,20.7333289447707,-43.7692808278358));
#21330=CARTESIAN_POINT('Ctrl Pts',(-21.9775256951463,20.7372978032738,-43.7687805297236));
#21331=CARTESIAN_POINT('Ctrl Pts',(-21.7124954253981,20.8863577236959,-43.7501781515924));
#21332=CARTESIAN_POINT('Ctrl Pts',(-21.4757280177946,21.0662832075499,-43.7342133350316));
#21333=CARTESIAN_POINT('Ctrl Pts',(-21.1243805163157,21.4190542105313,-43.7061904398073));
#21334=CARTESIAN_POINT('Ctrl Pts',(-20.9957130527506,21.5751143587977,-43.6945846522785));
#21335=CARTESIAN_POINT('Ctrl Pts',(-20.8754233831136,21.7525970129527,-43.6815560320951));
#21336=CARTESIAN_POINT('Ctrl Pts',(-20.8684152671212,21.7630689324418,-43.6807880545692));
#21337=CARTESIAN_POINT('Ctrl Pts',(-20.8589219557502,21.7774359488874,-43.6797353354369));
#21338=CARTESIAN_POINT('Ctrl Pts',(-20.8563833920705,21.7812957873085,-43.6794526017103));
#21339=CARTESIAN_POINT('Ctrl Pts',(-20.8520762541478,21.7878754825785,-43.6789707845249));
#21340=CARTESIAN_POINT('Ctrl Pts',(-20.850303466007,21.7905925842772,-43.67877185928));
#21341=CARTESIAN_POINT('Ctrl Pts',(-20.8468819488609,21.7958539891234,-43.6783867395101));
#21342=CARTESIAN_POINT('Ctrl Pts',(-20.8452327010549,21.798397951527,-43.6782005647097));
#21343=CARTESIAN_POINT('Ctrl Pts',(-20.8413268106732,21.804441448071,-43.6777583666986));
#21344=CARTESIAN_POINT('Ctrl Pts',(-20.8390733601025,21.8079430296312,-43.6775022247182));
#21345=CARTESIAN_POINT('Ctrl Pts',(-20.8325370248106,21.8181430667149,-43.6767562738232));
#21346=CARTESIAN_POINT('Ctrl Pts',(-20.8282721567674,21.8248529803659,-43.6762657954194));
#21347=CARTESIAN_POINT('Ctrl Pts',(-20.796666312334,21.8749872683819,-43.6726027207023));
#21348=CARTESIAN_POINT('Ctrl Pts',(-20.7703424755866,21.9190412151846,-43.6693927598346));
#21349=CARTESIAN_POINT('Ctrl Pts',(-20.6869628712055,22.0664642372666,-43.6586712095719));
#21350=CARTESIAN_POINT('Ctrl Pts',(-20.6345399322387,22.1723301948385,-43.6509999157526));
#21351=CARTESIAN_POINT('Ctrl Pts',(-20.5083899639432,22.466700413827,-43.6297791058253));
#21352=CARTESIAN_POINT('Ctrl Pts',(-20.4464093208745,22.6596568674107,-43.6159596054851));
#21353=CARTESIAN_POINT('Ctrl Pts',(-20.3732962817598,22.991647275081,-43.5931202175534));
#21354=CARTESIAN_POINT('Ctrl Pts',(-20.3523220606205,23.1279473593706,-43.5840087097376));
#21355=CARTESIAN_POINT('Ctrl Pts',(-20.3393984633464,23.2734800224228,-43.5748301915731));
#21356=CARTESIAN_POINT('Ctrl Pts',(-20.3386941987595,23.2817754415655,-43.5743089118939));
#21357=CARTESIAN_POINT('Ctrl Pts',(-20.3377740416975,23.2931359178994,-43.5735977115822));
#21358=CARTESIAN_POINT('Ctrl Pts',(-20.3375303835385,23.2961985989969,-43.573406245548));
#21359=CARTESIAN_POINT('Ctrl Pts',(-20.3371508927334,23.3010565016326,-43.573102978379));
#21360=CARTESIAN_POINT('Ctrl Pts',(-20.3370121848354,23.3028514867321,-43.5729910145659));
#21361=CARTESIAN_POINT('Ctrl Pts',(-20.3367456615726,23.3063385354253,-43.5727736882371));
#21362=CARTESIAN_POINT('Ctrl Pts',(-20.3366176793313,23.3080305723596,-43.5726683171305));
#21363=CARTESIAN_POINT('Ctrl Pts',(-20.3363131865703,23.3120989541871,-43.5724151585849));
#21364=CARTESIAN_POINT('Ctrl Pts',(-20.3361379752792,23.3144753933964,-43.5722674454976));
#21365=CARTESIAN_POINT('Ctrl Pts',(-20.3356432879058,23.3212880063699,-43.5718444530216));
#21366=CARTESIAN_POINT('Ctrl Pts',(-20.3353303576651,23.3257246723819,-43.5715695427246));
#21367=CARTESIAN_POINT('Ctrl Pts',(-20.3328454158035,23.362026323137,-43.5693246557309));
#21368=CARTESIAN_POINT('Ctrl Pts',(-20.3311379246294,23.3939227837029,-43.5673804288136));
#21369=CARTESIAN_POINT('Ctrl Pts',(-20.3267900776463,23.5064650668968,-43.5606034597468));
#21370=CARTESIAN_POINT('Ctrl Pts',(-20.3267039146096,23.5871846694168,-43.5558925417804));
#21371=CARTESIAN_POINT('Ctrl Pts',(-20.3363866708493,23.8524115641234,-43.5406623171468));
#21372=CARTESIAN_POINT('Ctrl Pts',(-20.3589814887923,24.036081615633,-43.5304950981702));
#21373=CARTESIAN_POINT('Ctrl Pts',(-20.4406325420954,24.4223202881182,-43.5083122289569));
#21374=CARTESIAN_POINT('Ctrl Pts',(-20.5040560283541,24.6230551518152,-43.496269887367));
#21375=CARTESIAN_POINT('Ctrl Pts',(-20.591615667434,24.828044369122,-43.4827274064666));
#21376=CARTESIAN_POINT('Ctrl Pts',(-20.5967556209701,24.8398804102354,-43.4819410435605));
#21377=CARTESIAN_POINT('Ctrl Pts',(-20.603850841636,24.8559540357782,-43.4808670002361));
#21378=CARTESIAN_POINT('Ctrl Pts',(-20.6057444836715,24.8602188258035,-43.4805814344464));
#21379=CARTESIAN_POINT('Ctrl Pts',(-20.6089756032406,24.8674534280129,-43.4800960019841));
#21380=CARTESIAN_POINT('Ctrl Pts',(-20.6103083368397,24.8704253620999,-43.479896298616));
#21381=CARTESIAN_POINT('Ctrl Pts',(-20.6128887940042,24.8761563760043,-43.4795106319443));
#21382=CARTESIAN_POINT('Ctrl Pts',(-20.6141359056584,24.8789157283209,-43.479324689909));
#21383=CARTESIAN_POINT('Ctrl Pts',(-20.6170951367739,24.885438794376,-43.4788845264711));
#21384=CARTESIAN_POINT('Ctrl Pts',(-20.6188106112326,24.8892009721269,-43.4786301895062));
#21385=CARTESIAN_POINT('Ctrl Pts',(-20.6237716985429,24.9000258130365,-43.4778970219368));
#21386=CARTESIAN_POINT('Ctrl Pts',(-20.6270356115475,24.9070800129527,-43.4774175591392));
#21387=CARTESIAN_POINT('Ctrl Pts',(-20.6496400968237,24.9554742667882,-43.4741166150031));
#21388=CARTESIAN_POINT('Ctrl Pts',(-20.6698306064827,24.9964094420536,-43.4712657185882));
#21389=CARTESIAN_POINT('Ctrl Pts',(-20.7328014883289,25.1175255684658,-43.4626475897631));
#21390=CARTESIAN_POINT('Ctrl Pts',(-20.7781078372217,25.1963346588691,-43.4567931385375));
#21391=CARTESIAN_POINT('Ctrl Pts',(-20.9295259028893,25.4357021377593,-43.4382293650395));
#21392=CARTESIAN_POINT('Ctrl Pts',(-21.0467155028626,25.5887365569703,-43.4251802510341));
#21393=CARTESIAN_POINT('Ctrl Pts',(-21.2778015911528,25.8403094039,-43.4020821930794));
#21394=CARTESIAN_POINT('Ctrl Pts',(-21.3862926052458,25.9430918478627,-43.3920532200363));
#21395=CARTESIAN_POINT('Ctrl Pts',(-21.5293854483496,26.0609329528217,-43.3801435272218));
#21396=CARTESIAN_POINT('Ctrl Pts',(-21.5576281680185,26.0834063690238,-43.3778517341946));
#21397=CARTESIAN_POINT('Ctrl Pts',(-21.5899358095286,26.1082395517465,-43.3753013482047));
#21398=CARTESIAN_POINT('Ctrl Pts',(-21.5936339172394,26.1110693631318,-43.3750104544027));
#21399=CARTESIAN_POINT('Ctrl Pts',(-21.599232033722,26.1153338651161,-43.3745716872008));
#21400=CARTESIAN_POINT('Ctrl Pts',(-21.6011275002128,26.1167744665936,-43.3744233981051));
#21401=CARTESIAN_POINT('Ctrl Pts',(-21.6044227614518,26.1192731907677,-43.3741660746582));
#21402=CARTESIAN_POINT('Ctrl Pts',(-21.605821823781,26.1203322704701,-43.3740569722799));
#21403=CARTESIAN_POINT('Ctrl Pts',(-21.6087485878461,26.1225440511554,-43.373829048276));
#21404=CARTESIAN_POINT('Ctrl Pts',(-21.6102764503374,26.1236965331939,-43.3737102425814));
#21405=CARTESIAN_POINT('Ctrl Pts',(-21.6139268696478,26.1264449828392,-43.373426810005));
#21406=CARTESIAN_POINT('Ctrl Pts',(-21.616050380609,26.1280396939121,-43.3732622724333));
#21407=CARTESIAN_POINT('Ctrl Pts',(-21.6231001782321,26.1333203246849,-43.3727171454003));
#21408=CARTESIAN_POINT('Ctrl Pts',(-21.6280350876932,26.1369947910035,-43.3723373595259));
#21409=CARTESIAN_POINT('Ctrl Pts',(-21.6397926060123,26.1456970523951,-43.3714367195191));
#21410=CARTESIAN_POINT('Ctrl Pts',(-21.6466246241101,26.1507121412347,-43.3709167292385));
#21411=CARTESIAN_POINT('Ctrl Pts',(-21.6709824950554,26.1684447660121,-43.3690743976062));
#21412=CARTESIAN_POINT('Ctrl Pts',(-21.6886170889714,26.1810128745784,-43.3677617624746));
#21413=CARTESIAN_POINT('Ctrl Pts',(-21.7302331169343,26.2100444274727,-43.3647099031045));
#21414=CARTESIAN_POINT('Ctrl Pts',(-21.7543137278452,26.2263630543977,-43.3629790235023));
#21415=CARTESIAN_POINT('Ctrl Pts',(-21.8104356227183,26.263296201581,-43.3590171334029));
#21416=CARTESIAN_POINT('Ctrl Pts',(-21.842628448613,26.2836732881986,-43.3567975297631));
#21417=CARTESIAN_POINT('Ctrl Pts',(-21.9404679187915,26.3431993746108,-43.3501860564257));
#21418=CARTESIAN_POINT('Ctrl Pts',(-22.0071309136415,26.3805752452119,-43.3458587578018));
#21419=CARTESIAN_POINT('Ctrl Pts',(-22.0750361136176,26.4155368251522,-43.341564988124));
#21420=CARTESIAN_POINT('Origin',(-23.5502525316942,23.5502525316942,-77.3107734492734));
#21421=CARTESIAN_POINT('',(-22.0750357700609,26.4155366482691,-41.8463063580885));
#21422=CARTESIAN_POINT('',(-22.0750360182176,26.4155367760347,-42.0958126606468));
#21423=CARTESIAN_POINT('',(-22.0750360153461,26.4155367745563,-77.3107734492734));
#21424=CARTESIAN_POINT('Ctrl Pts',(-22.0750357700609,26.4155366482691,-41.8463063580885));
#21425=CARTESIAN_POINT('Ctrl Pts',(-21.9772531459235,26.3651924030721,-41.8524539240125));
#21426=CARTESIAN_POINT('Ctrl Pts',(-21.8820641779325,26.3098512670906,-41.8586200916589));
#21427=CARTESIAN_POINT('Ctrl Pts',(-21.7018797839775,26.1923474161378,-41.8709105408599));
#21428=CARTESIAN_POINT('Ctrl Pts',(-21.6167745270493,26.1307189459993,-41.8770130351582));
#21429=CARTESIAN_POINT('Ctrl Pts',(-21.4973713426764,26.0350264255765,-41.8861354317059));
#21430=CARTESIAN_POINT('Ctrl Pts',(-21.4605854268994,26.0041705202263,-41.8890288970496));
#21431=CARTESIAN_POINT('Ctrl Pts',(-21.4185764649339,25.9673038142383,-41.8924372254398));
#21432=CARTESIAN_POINT('Ctrl Pts',(-21.4126682026131,25.9620802598644,-41.8929190375543));
#21433=CARTESIAN_POINT('Ctrl Pts',(-21.4037069666418,25.9540987468317,-41.8936535898197));
#21434=CARTESIAN_POINT('Ctrl Pts',(-21.4006399735063,25.9513565149293,-41.8939056682826));
#21435=CARTESIAN_POINT('Ctrl Pts',(-21.3953267190542,25.946587537054,-41.8943435496765));
#21436=CARTESIAN_POINT('Ctrl Pts',(-21.3930780400227,25.944563482318,-41.8945292387955));
#21437=CARTESIAN_POINT('Ctrl Pts',(-21.3884076157069,25.9403476742309,-41.8949156778006));
#21438=CARTESIAN_POINT('Ctrl Pts',(-21.3859863465828,25.938155400535,-41.8951164496235));
#21439=CARTESIAN_POINT('Ctrl Pts',(-21.3793646061916,25.9321415773189,-41.8956667119782));
#21440=CARTESIAN_POINT('Ctrl Pts',(-21.3751709111567,25.9283126137988,-41.8960165174593));
#21441=CARTESIAN_POINT('Ctrl Pts',(-21.3591627440885,25.9136189293234,-41.8973568478698));
#21442=CARTESIAN_POINT('Ctrl Pts',(-21.3474195336887,25.9026772286176,-41.8983506600611));
#21443=CARTESIAN_POINT('Ctrl Pts',(-21.1563529310658,25.7219663065232,-41.9146966355623));
#21444=CARTESIAN_POINT('Ctrl Pts',(-20.9970827748512,25.5322644302741,-41.9309845116944));
#21445=CARTESIAN_POINT('Ctrl Pts',(-20.769825700203,25.1881616169025,-41.9588311178608));
#21446=CARTESIAN_POINT('Ctrl Pts',(-20.6893758193029,25.0432050835991,-41.970113442863));
#21447=CARTESIAN_POINT('Ctrl Pts',(-20.5941299169304,24.8353357931206,-41.9852240713513));
#21448=CARTESIAN_POINT('Ctrl Pts',(-20.5695316750797,24.7772016815339,-41.9893397432001));
#21449=CARTESIAN_POINT('Ctrl Pts',(-20.539947288755,24.7011314864607,-41.9945514894867));
#21450=CARTESIAN_POINT('Ctrl Pts',(-20.5333881561239,24.6838262613359,-41.9957256797153));
#21451=CARTESIAN_POINT('Ctrl Pts',(-20.5230460552348,24.6558145635857,-41.9976068413836));
#21452=CARTESIAN_POINT('Ctrl Pts',(-20.5191700679046,24.6451431948922,-41.9983189611952));
#21453=CARTESIAN_POINT('Ctrl Pts',(-20.5142285853146,24.631310939241,-41.9992359572336));
#21454=CARTESIAN_POINT('Ctrl Pts',(-20.5131115532476,24.6281687440217,-41.999443862976));
#21455=CARTESIAN_POINT('Ctrl Pts',(-20.5113078476957,24.6230698833658,-41.9997805730516));
#21456=CARTESIAN_POINT('Ctrl Pts',(-20.5106181855329,24.6211142894133,-41.9999095560698));
#21457=CARTESIAN_POINT('Ctrl Pts',(-20.5093069448188,24.6173846854606,-42.000155244019));
#21458=CARTESIAN_POINT('Ctrl Pts',(-20.5086850354972,24.615610810412,-42.0002719680059));
#21459=CARTESIAN_POINT('Ctrl Pts',(-20.5072708046455,24.6115656606711,-42.0005378505535));
#21460=CARTESIAN_POINT('Ctrl Pts',(-20.5064794748299,24.6092940451811,-42.0006869491311));
#21461=CARTESIAN_POINT('Ctrl Pts',(-20.5040223867026,24.6022151502412,-42.0011509224828));
#21462=CARTESIAN_POINT('Ctrl Pts',(-20.5023654577852,24.5974047807082,-42.001465271605));
#21463=CARTESIAN_POINT('Ctrl Pts',(-20.4896787706626,24.5602877720829,-42.0038837237919));
#21464=CARTESIAN_POINT('Ctrl Pts',(-20.4791510409752,24.5278100977849,-42.0059585890049));
#21465=CARTESIAN_POINT('Ctrl Pts',(-20.4393291266002,24.3979619287134,-42.0141133862875));
#21466=CARTESIAN_POINT('Ctrl Pts',(-20.4141314820632,24.2993882418838,-42.0199927732055));
#21467=CARTESIAN_POINT('Ctrl Pts',(-20.3513205921513,23.9941354409259,-42.0377076206906));
#21468=CARTESIAN_POINT('Ctrl Pts',(-20.3292018707765,23.7848474238674,-42.0492072795638));
#21469=CARTESIAN_POINT('Ctrl Pts',(-20.3268140389264,23.4725158351821,-42.0669666502198));
#21470=CARTESIAN_POINT('Ctrl Pts',(-20.3309100057908,23.3701698817405,-42.0728749776811));
#21471=CARTESIAN_POINT('Ctrl Pts',(-20.3455751930156,23.2032486111865,-42.0827826772659));
#21472=CARTESIAN_POINT('Ctrl Pts',(-20.3532507868973,23.1384910873882,-42.0866933019996));
#21473=CARTESIAN_POINT('Ctrl Pts',(-20.3641371763042,23.0656306614346,-42.091183635963));
#21474=CARTESIAN_POINT('Ctrl Pts',(-20.365422855797,23.0572521784007,-42.0917013459963));
#21475=CARTESIAN_POINT('Ctrl Pts',(-20.3674006303901,23.0446941437229,-42.0924793706786));
#21476=CARTESIAN_POINT('Ctrl Pts',(-20.3680679435657,23.0405106792913,-42.0927388974333));
#21477=CARTESIAN_POINT('Ctrl Pts',(-20.369228551177,23.0333257963348,-42.0931852149236));
#21478=CARTESIAN_POINT('Ctrl Pts',(-20.3697178508434,23.0303237306508,-42.0933718783629));
#21479=CARTESIAN_POINT('Ctrl Pts',(-20.370733101384,23.0241497924835,-42.0937561320919));
#21480=CARTESIAN_POINT('Ctrl Pts',(-20.3712595502285,23.02097800596,-42.0939537380618));
#21481=CARTESIAN_POINT('Ctrl Pts',(-20.3725363974964,23.0133557982813,-42.0944290943114));
#21482=CARTESIAN_POINT('Ctrl Pts',(-20.3732913985376,23.0089061638473,-42.0947069909473));
#21483=CARTESIAN_POINT('Ctrl Pts',(-20.3756306592494,22.9952930659829,-42.0955584039115));
#21484=CARTESIAN_POINT('Ctrl Pts',(-20.3772452260908,22.9861349222681,-42.0961328852279));
#21485=CARTESIAN_POINT('Ctrl Pts',(-20.3961066341779,22.8817925776158,-42.1026977986869));
#21486=CARTESIAN_POINT('Ctrl Pts',(-20.4175892926568,22.7874335243588,-42.1088232591418));
#21487=CARTESIAN_POINT('Ctrl Pts',(-20.4595390820231,22.635181862189,-42.1190330845082));
#21488=CARTESIAN_POINT('Ctrl Pts',(-20.4774747040188,22.5766511419825,-42.1230384878416));
#21489=CARTESIAN_POINT('Ctrl Pts',(-20.5520754098858,22.3558546782773,-42.138443849064));
#21490=CARTESIAN_POINT('Ctrl Pts',(-20.6200179521351,22.1977105702668,-42.1501147494433));
#21491=CARTESIAN_POINT('Ctrl Pts',(-20.7812055735126,21.8923688109779,-42.1734514990341));
#21492=CARTESIAN_POINT('Ctrl Pts',(-20.8744360382992,21.7457521434629,-42.1850750385602));
#21493=CARTESIAN_POINT('Ctrl Pts',(-20.9853026803273,21.599032870359,-42.1966501638791));
#21494=CARTESIAN_POINT('Ctrl Pts',(-20.9916182186336,21.5907586261338,-42.1973026909872));
#21495=CARTESIAN_POINT('Ctrl Pts',(-20.9999481600588,21.5799541709706,-42.1981542628992));
#21496=CARTESIAN_POINT('Ctrl Pts',(-21.0019263463784,21.5773963099422,-42.1983558286606));
#21497=CARTESIAN_POINT('Ctrl Pts',(-21.0051652400162,21.573221311745,-42.1986847630483));
#21498=CARTESIAN_POINT('Ctrl Pts',(-21.0064236407612,21.571602400765,-42.1988122955204));
#21499=CARTESIAN_POINT('Ctrl Pts',(-21.0088428028075,21.568496312718,-42.1990569499474));
#21500=CARTESIAN_POINT('Ctrl Pts',(-21.010003321482,21.5670089582617,-42.1991740882795));
#21501=CARTESIAN_POINT('Ctrl Pts',(-21.0126752770312,21.5635906953627,-42.1994432652668));
#21502=CARTESIAN_POINT('Ctrl Pts',(-21.014187615828,21.5616604875767,-42.199595239177));
#21503=CARTESIAN_POINT('Ctrl Pts',(-21.0188771863956,21.5556892088956,-42.2000653180862));
#21504=CARTESIAN_POINT('Ctrl Pts',(-21.0220619049011,21.5516539869881,-42.2003828895237));
#21505=CARTESIAN_POINT('Ctrl Pts',(-21.048208529133,21.518687211093,-42.2029767545228));
#21506=CARTESIAN_POINT('Ctrl Pts',(-21.0716577896036,21.490143254738,-42.20521873646));
#21507=CARTESIAN_POINT('Ctrl Pts',(-21.0985907105131,21.4584845550575,-42.2077090886249));
#21508=CARTESIAN_POINT('Ctrl Pts',(-21.1015951965244,21.4549682529067,-42.20798574228));
#21509=CARTESIAN_POINT('Ctrl Pts',(-21.108136588268,21.4473458169412,-42.2085856012056));
#21510=CARTESIAN_POINT('Ctrl Pts',(-21.1116763086222,21.443242105251,-42.2089086408403));
#21511=CARTESIAN_POINT('Ctrl Pts',(-21.1219216727674,21.4314247266792,-42.2098392234232));
#21512=CARTESIAN_POINT('Ctrl Pts',(-21.1286537374724,21.423733941964,-42.2104452589701));
#21513=CARTESIAN_POINT('Ctrl Pts',(-21.1417117784353,21.4089587162792,-42.2116106374164));
#21514=CARTESIAN_POINT('Ctrl Pts',(-21.1480326944234,21.4018699723854,-42.2121702424001));
#21515=CARTESIAN_POINT('Ctrl Pts',(-21.1763833872309,21.3703569626046,-42.214660698649));
#21516=CARTESIAN_POINT('Ctrl Pts',(-21.1987555846416,21.3462421763196,-42.2165738573126));
#21517=CARTESIAN_POINT('Ctrl Pts',(-21.4028245425305,21.132923277902,-42.2336095192303));
#21518=CARTESIAN_POINT('Ctrl Pts',(-21.6066250754386,20.9662134490909,-42.247807610266));
#21519=CARTESIAN_POINT('Ctrl Pts',(-21.9418568106877,20.7543272299207,-42.2704712334115));
#21520=CARTESIAN_POINT('Ctrl Pts',(-22.0596781889589,20.6897776502195,-42.2783110418898));
#21521=CARTESIAN_POINT('Ctrl Pts',(-22.1939061139439,20.6267888557906,-42.2872750033166));
#21522=CARTESIAN_POINT('Ctrl Pts',(-22.2066803525832,20.6208960735144,-42.2881283122233));
#21523=CARTESIAN_POINT('Ctrl Pts',(-22.2290709151561,20.610744528428,-42.2896245671747));
#21524=CARTESIAN_POINT('Ctrl Pts',(-22.2386703302467,20.6064488205291,-42.2902662362333));
#21525=CARTESIAN_POINT('Ctrl Pts',(-22.2525233778769,20.6003308348388,-42.2911925643565));
#21526=CARTESIAN_POINT('Ctrl Pts',(-22.2567602483382,20.5984705806026,-42.2914759199633));
#21527=CARTESIAN_POINT('Ctrl Pts',(-22.2641291083669,20.5952540966387,-42.2919688201161));
#21528=CARTESIAN_POINT('Ctrl Pts',(-22.2672592810342,20.5938937020141,-42.2921782217));
#21529=CARTESIAN_POINT('Ctrl Pts',(-22.2732883196702,20.5912848188119,-42.292581602588));
#21530=CARTESIAN_POINT('Ctrl Pts',(-22.2761868718267,20.5900356107747,-42.2927755570157));
#21531=CARTESIAN_POINT('Ctrl Pts',(-22.2830289397769,20.5870987506503,-42.2932334451609));
#21532=CARTESIAN_POINT('Ctrl Pts',(-22.2869739923337,20.5854147125646,-42.2934975019409));
#21533=CARTESIAN_POINT('Ctrl Pts',(-22.3006726082262,20.5795994424533,-42.2944145613369));
#21534=CARTESIAN_POINT('Ctrl Pts',(-22.3104430882525,20.5755084584332,-42.2950689330862));
#21535=CARTESIAN_POINT('Ctrl Pts',(-22.4277489051545,20.5270698147462,-42.3029291912258));
#21536=CARTESIAN_POINT('Ctrl Pts',(-22.5375762724683,20.4885325361548,-42.3103311111154));
#21537=CARTESIAN_POINT('Ctrl Pts',(-22.663020889403,20.4520040386413,-42.3188452461836));
#21538=CARTESIAN_POINT('Ctrl Pts',(-22.6768327436961,20.4480820695106,-42.3197834027166));
#21539=CARTESIAN_POINT('Ctrl Pts',(-22.9133305712872,20.3826315354656,-42.3358589201773));
#21540=CARTESIAN_POINT('Ctrl Pts',(-23.1419572090988,20.3451369001051,-42.3516458422299));
#21541=CARTESIAN_POINT('Ctrl Pts',(-23.4456335415051,20.328370469413,-42.3721039806439));
#21542=CARTESIAN_POINT('Ctrl Pts',(-23.5187969997473,20.326825656299,-42.376987993387));
#21543=CARTESIAN_POINT('Ctrl Pts',(-23.6591955041478,20.3286424852505,-42.386205683276));
#21544=CARTESIAN_POINT('Ctrl Pts',(-23.7264001447948,20.331617196725,-42.3905497023721));
#21545=CARTESIAN_POINT('Ctrl Pts',(-23.804275611836,20.3375111299206,-42.3954674478925));
#21546=CARTESIAN_POINT('Ctrl Pts',(-23.8150793914783,20.3383836392505,-42.3961470879095));
#21547=CARTESIAN_POINT('Ctrl Pts',(-23.829141937261,20.3395907636404,-42.3970281532736));
#21548=CARTESIAN_POINT('Ctrl Pts',(-23.832404717011,20.3398758506911,-42.3972323264589));
#21549=CARTESIAN_POINT('Ctrl Pts',(-23.8377189687975,20.3403483503212,-42.3975644585424));
#21550=CARTESIAN_POINT('Ctrl Pts',(-23.8397706953569,20.3405327559157,-42.3976925873288));
#21551=CARTESIAN_POINT('Ctrl Pts',(-23.8436980708678,20.3408895379243,-42.3979376541969));
#21552=CARTESIAN_POINT('Ctrl Pts',(-23.8455737395852,20.3410615909078,-42.3980546099619));
#21553=CARTESIAN_POINT('Ctrl Pts',(-23.8498711169182,20.3414595839368,-42.3983223754822));
#21554=CARTESIAN_POINT('Ctrl Pts',(-23.852292726685,20.3416866216819,-42.3984731227273));
#21555=CARTESIAN_POINT('Ctrl Pts',(-23.8599177562962,20.34241021431,-42.3989473497799));
#21556=CARTESIAN_POINT('Ctrl Pts',(-23.8651202601746,20.3429166903765,-42.3992702699017));
#21557=CARTESIAN_POINT('Ctrl Pts',(-23.9075757440468,20.3471541278045,-42.4019004166495));
#21558=CARTESIAN_POINT('Ctrl Pts',(-23.944764296926,20.3515215290251,-42.40417239754));
#21559=CARTESIAN_POINT('Ctrl Pts',(-24.3039480142052,20.4000637401541,-42.4258801344396));
#21560=CARTESIAN_POINT('Ctrl Pts',(-24.617633056031,20.492064434711,-42.4431593496046));
#21561=CARTESIAN_POINT('Ctrl Pts',(-25.033682016491,20.6860777768977,-42.4693963282932));
#21562=CARTESIAN_POINT('Ctrl Pts',(-25.1514194910646,20.7501957829155,-42.4772205318204));
#21563=CARTESIAN_POINT('Ctrl Pts',(-25.2828093379547,20.8327507463927,-42.486601805105));
#21564=CARTESIAN_POINT('Ctrl Pts',(-25.3006881220055,20.8442325298096,-42.4878928141654));
#21565=CARTESIAN_POINT('Ctrl Pts',(-25.3235783791506,20.8592544635153,-42.4895649186859));
#21566=CARTESIAN_POINT('Ctrl Pts',(-25.3286953819097,20.8626334753739,-42.489939959418));
#21567=CARTESIAN_POINT('Ctrl Pts',(-25.3369097189948,20.8680915422372,-42.4905440402268));
#21568=CARTESIAN_POINT('Ctrl Pts',(-25.3400131587495,20.8701614183261,-42.4907727339081));
#21569=CARTESIAN_POINT('Ctrl Pts',(-25.3459069578501,20.8741071602081,-42.4912079429805));
#21570=CARTESIAN_POINT('Ctrl Pts',(-25.3486979909341,20.875982014805,-42.4914144199335));
#21571=CARTESIAN_POINT('Ctrl Pts',(-25.3550400611338,20.8802566693332,-42.491884470234));
#21572=CARTESIAN_POINT('Ctrl Pts',(-25.3585892499257,20.8826591884993,-42.4921481464711));
#21573=CARTESIAN_POINT('Ctrl Pts',(-25.3693463877062,20.8899722506675,-42.4929492183142));
#21574=CARTESIAN_POINT('Ctrl Pts',(-25.3765391607579,20.8949049505468,-42.4934874560171));
#21575=CARTESIAN_POINT('Ctrl Pts',(-25.4270751002638,20.9298642329007,-42.4972875788717));
#21576=CARTESIAN_POINT('Ctrl Pts',(-25.469693482917,20.9609198584305,-42.5005887754197));
#21577=CARTESIAN_POINT('Ctrl Pts',(-25.5148876366285,20.9955814407048,-42.5041983783339));
#21578=CARTESIAN_POINT('Ctrl Pts',(-25.5182412265592,20.9981639800784,-42.5044668860547));
#21579=CARTESIAN_POINT('Ctrl Pts',(-25.5247750204387,21.0032160740899,-42.504991311349));
#21580=CARTESIAN_POINT('Ctrl Pts',(-25.5279557044425,21.0056849976737,-42.5052472043932));
#21581=CARTESIAN_POINT('Ctrl Pts',(-25.5350326513094,21.0111995790706,-42.5058179007252));
#21582=CARTESIAN_POINT('Ctrl Pts',(-25.5389265415828,21.0142482530289,-42.506132819046));
#21583=CARTESIAN_POINT('Ctrl Pts',(-25.5569838986532,21.028453203817,-42.5075974406308));
#21584=CARTESIAN_POINT('Ctrl Pts',(-25.5710603904479,21.0397190810876,-42.5087513120912));
#21585=CARTESIAN_POINT('Ctrl Pts',(-25.6027457622187,21.065517066641,-42.5113763314517));
#21586=CARTESIAN_POINT('Ctrl Pts',(-25.6202961055793,21.0801192651444,-42.5128500655626));
#21587=CARTESIAN_POINT('Ctrl Pts',(-25.8682073367593,21.2908834682366,-42.5339509385485));
#21588=CARTESIAN_POINT('Ctrl Pts',(-26.0699644106634,21.5183414982037,-42.554851459151));
#21589=CARTESIAN_POINT('Ctrl Pts',(-26.2780933961966,21.8325396938435,-42.5798920261439));
#21590=CARTESIAN_POINT('Ctrl Pts',(-26.3170242708538,21.8959765357849,-42.5847687082337));
#21591=CARTESIAN_POINT('Ctrl Pts',(-26.3687342173936,21.9871772482324,-42.5914749978725));
#21592=CARTESIAN_POINT('Ctrl Pts',(-26.3833666073867,22.0138580005604,-42.5934014212401));
#21593=CARTESIAN_POINT('Ctrl Pts',(-26.3997375880703,22.0447383591887,-42.5955871226326));
#21594=CARTESIAN_POINT('Ctrl Pts',(-26.4018472153906,22.0487380393782,-42.595869380028));
#21595=CARTESIAN_POINT('Ctrl Pts',(-26.4050252235891,22.054794137042,-42.5962954764623));
#21596=CARTESIAN_POINT('Ctrl Pts',(-26.4060998049847,22.0568472671244,-42.5964397086933));
#21597=CARTESIAN_POINT('Ctrl Pts',(-26.408035838937,22.0605560476472,-42.5966998464624));
#21598=CARTESIAN_POINT('Ctrl Pts',(-26.4088980655487,22.0622112830827,-42.5968158012749));
#21599=CARTESIAN_POINT('Ctrl Pts',(-26.4107518733939,22.065777636598,-42.5970653235902));
#21600=CARTESIAN_POINT('Ctrl Pts',(-26.4117429747484,22.0676889943004,-42.5971988601585));
#21601=CARTESIAN_POINT('Ctrl Pts',(-26.4144147587184,22.0728542400324,-42.5975592121155));
#21602=CARTESIAN_POINT('Ctrl Pts',(-26.4160918178819,22.0761100145078,-42.5977857970638));
#21603=CARTESIAN_POINT('Ctrl Pts',(-26.4238538358473,22.0912421882877,-42.5988363833944));
#21604=CARTESIAN_POINT('Ctrl Pts',(-26.4298706572446,22.1031536743205,-42.5996561270869));
#21605=CARTESIAN_POINT('Ctrl Pts',(-26.4365067778225,22.1164964808641,-42.6005666974657));
#21606=CARTESIAN_POINT('Ctrl Pts',(-26.4371991066031,22.1178910339406,-42.6006617744745));
#21607=CARTESIAN_POINT('Ctrl Pts',(-26.5905687020566,22.4273852639512,-42.6217417220802));
#21608=CARTESIAN_POINT('Ctrl Pts',(-26.6929862897288,22.7579917088256,-42.6399262684548));
#21609=CARTESIAN_POINT('Ctrl Pts',(-26.7623689865021,23.2481784002927,-42.668163738631));
#21610=CARTESIAN_POINT('Ctrl Pts',(-26.7729948114299,23.3990451833679,-42.6769881055619));
#21611=CARTESIAN_POINT('Ctrl Pts',(-26.7730031690222,23.5626459800112,-42.686929797715));
#21612=CARTESIAN_POINT('Ctrl Pts',(-26.7729304079758,23.5752038179512,-42.6876951967023));
#21613=CARTESIAN_POINT('Ctrl Pts',(-26.7727305631484,23.5923735461849,-42.6887449119696));
#21614=CARTESIAN_POINT('Ctrl Pts',(-26.7726669694687,23.5969861804832,-42.6890272351));
#21615=CARTESIAN_POINT('Ctrl Pts',(-26.7725418143981,23.6048405690312,-42.6895085216415));
#21616=CARTESIAN_POINT('Ctrl Pts',(-26.7724852639444,23.608082405886,-42.6897073275621));
#21617=CARTESIAN_POINT('Ctrl Pts',(-26.7723663613252,23.6143557724717,-42.6900923515634));
#21618=CARTESIAN_POINT('Ctrl Pts',(-26.7723046228136,23.6173873109976,-42.6902785501383));
#21619=CARTESIAN_POINT('Ctrl Pts',(-26.7721478602195,23.6245857450682,-42.6907210154545));
#21620=CARTESIAN_POINT('Ctrl Pts',(-26.7720490308998,23.6287525446252,-42.6909774014118));
#21621=CARTESIAN_POINT('Ctrl Pts',(-26.7717332217499,23.6410602859584,-42.6917354965202));
#21622=CARTESIAN_POINT('Ctrl Pts',(-26.7714934679459,23.6492005650299,-42.6922379200724));
#21623=CARTESIAN_POINT('Ctrl Pts',(-26.7693729358582,23.7129819256551,-42.6961826877747));
#21624=CARTESIAN_POINT('Ctrl Pts',(-26.7660816035998,23.7685637455731,-42.6996691237189));
#21625=CARTESIAN_POINT('Ctrl Pts',(-26.749929619662,23.9580084090001,-42.7117297819845));
#21626=CARTESIAN_POINT('Ctrl Pts',(-26.7301343182387,24.0911243350592,-42.7205154458314));
#21627=CARTESIAN_POINT('Ctrl Pts',(-26.6373933776506,24.5258748386025,-42.7501456410641));
#21628=CARTESIAN_POINT('Ctrl Pts',(-26.5292722417456,24.8182113858969,-42.7717503436998));
#21629=CARTESIAN_POINT('Ctrl Pts',(-26.3737817774825,25.103968056285,-42.7923333706462));
#21630=CARTESIAN_POINT('Ctrl Pts',(-26.3664104822633,25.1172891465686,-42.7932911428775));
#21631=CARTESIAN_POINT('Ctrl Pts',(-26.3570222227504,25.1339749940236,-42.794488153266));
#21632=CARTESIAN_POINT('Ctrl Pts',(-26.3550933037446,25.1373886884717,-42.7947329029303));
#21633=CARTESIAN_POINT('Ctrl Pts',(-26.3519726255543,25.1428880355719,-42.7951269462766));
#21634=CARTESIAN_POINT('Ctrl Pts',(-26.3507847637066,25.1449758776391,-42.7952764899572));
#21635=CARTESIAN_POINT('Ctrl Pts',(-26.3486634220908,25.1486947679565,-42.7955427565334));
#21636=CARTESIAN_POINT('Ctrl Pts',(-26.3477308500097,25.1503263277374,-42.795659538285));
#21637=CARTESIAN_POINT('Ctrl Pts',(-26.345765351748,25.153758048638,-42.7959050944951));
#21638=CARTESIAN_POINT('Ctrl Pts',(-26.3447321161026,25.1555580235983,-42.7960338480734));
#21639=CARTESIAN_POINT('Ctrl Pts',(-26.3419960725353,25.1603137730059,-42.7963739192489));
#21640=CARTESIAN_POINT('Ctrl Pts',(-26.3402903034429,25.1632678543349,-42.7965850441716));
#21641=CARTESIAN_POINT('Ctrl Pts',(-26.3325400871556,25.1766407410522,-42.7975402998714));
#21642=CARTESIAN_POINT('Ctrl Pts',(-26.3264418450237,25.1870284956511,-42.7982809719925));
#21643=CARTESIAN_POINT('Ctrl Pts',(-26.1816643495727,25.4305056634149,-42.8156155831094));
#21644=CARTESIAN_POINT('Ctrl Pts',(-26.0141419164698,25.6452428918902,-42.8304032814843));
#21645=CARTESIAN_POINT('Ctrl Pts',(-25.7149858650322,25.9424607360275,-42.8540382761423));
#21646=CARTESIAN_POINT('Ctrl Pts',(-25.6010294874988,26.0408424941152,-42.8625526899209));
#21647=CARTESIAN_POINT('Ctrl Pts',(-25.4691774011028,26.1394704584868,-42.87221390628));
#21648=CARTESIAN_POINT('Ctrl Pts',(-25.4576676665194,26.1479610645109,-42.8730556642666));
#21649=CARTESIAN_POINT('Ctrl Pts',(-25.4405888475054,26.1603852206541,-42.8743026268573));
#21650=CARTESIAN_POINT('Ctrl Pts',(-25.4350630948944,26.1643782327105,-42.8747057545563));
#21651=CARTESIAN_POINT('Ctrl Pts',(-25.4262668707534,26.1706921597827,-42.8753469991283));
#21652=CARTESIAN_POINT('Ctrl Pts',(-25.4230046468484,26.173024569023,-42.8755847112169));
#21653=CARTESIAN_POINT('Ctrl Pts',(-25.4156735084646,26.1782455000225,-42.8761186923344));
#21654=CARTESIAN_POINT('Ctrl Pts',(-25.4116022276421,26.1811306685822,-42.8764150788139));
#21655=CARTESIAN_POINT('Ctrl Pts',(-25.4018615973445,26.1879995707798,-42.8771238362133));
#21656=CARTESIAN_POINT('Ctrl Pts',(-25.3961860845648,26.1919744874478,-42.8775365183289));
#21657=CARTESIAN_POINT('Ctrl Pts',(-25.3888365929864,26.197086547447,-42.8780705746595));
#21658=CARTESIAN_POINT('Ctrl Pts',(-25.3871742721678,26.1982404804455,-42.8781913456986));
#21659=CARTESIAN_POINT('Ctrl Pts',(-25.3815445806098,26.2021405903462,-42.8786002788691));
#21660=CARTESIAN_POINT('Ctrl Pts',(-25.3775721428924,26.2048794136122,-42.878888704554));
#21661=CARTESIAN_POINT('Ctrl Pts',(-25.3719468599377,26.2087391924316,-42.8792969667268));
#21662=CARTESIAN_POINT('Ctrl Pts',(-25.3702990875168,26.2098675574987,-42.8794165352257));
#21663=CARTESIAN_POINT('Ctrl Pts',(-25.3638707123897,26.2142608220175,-42.8798829228463));
#21664=CARTESIAN_POINT('Ctrl Pts',(-25.35908238543,26.2175143553336,-42.880230152109));
#21665=CARTESIAN_POINT('Ctrl Pts',(-25.3435836421814,26.2279843856537,-42.8813535349786));
#21666=CARTESIAN_POINT('Ctrl Pts',(-25.3328387034576,26.2351493428293,-42.8821315518111));
#21667=CARTESIAN_POINT('Ctrl Pts',(-25.3039186834693,26.2541837072214,-42.8842237045303));
#21668=CARTESIAN_POINT('Ctrl Pts',(-25.2856665019268,26.2659342306405,-42.8855421463071));
#21669=CARTESIAN_POINT('Ctrl Pts',(-25.2618743443805,26.2809135137602,-42.8872587441196));
#21670=CARTESIAN_POINT('Ctrl Pts',(-25.256441202096,26.2843115743443,-42.8876506081753));
#21671=CARTESIAN_POINT('Ctrl Pts',(-25.2477768349266,26.2896946616509,-42.8882753222793));
#21672=CARTESIAN_POINT('Ctrl Pts',(-25.2445521592834,26.2916902412186,-42.8885077821123));
#21673=CARTESIAN_POINT('Ctrl Pts',(-25.2387560977432,26.2952629814768,-42.8889255314625));
#21674=CARTESIAN_POINT('Ctrl Pts',(-25.2361860015664,26.2968422347697,-42.8891107435676));
#21675=CARTESIAN_POINT('Ctrl Pts',(-25.2301777337006,26.3005225391007,-42.8895436645211));
#21676=CARTESIAN_POINT('Ctrl Pts',(-25.2267378368535,26.3026207518507,-42.889791477387));
#21677=CARTESIAN_POINT('Ctrl Pts',(-25.2170224969143,26.3085217876392,-42.8904912536433));
#21678=CARTESIAN_POINT('Ctrl Pts',(-25.2107380178703,26.3123096190881,-42.8909437658583));
#21679=CARTESIAN_POINT('Ctrl Pts',(-25.1718189249581,26.335586413627,-42.8937452936679));
#21680=CARTESIAN_POINT('Ctrl Pts',(-25.1388557176521,26.3545175190888,-42.8961145495043));
#21681=CARTESIAN_POINT('Ctrl Pts',(-25.0404811514895,26.4087238895446,-42.9031784018418));
#21682=CARTESIAN_POINT('Ctrl Pts',(-24.9741795382192,26.442322772762,-42.9079310053756));
#21683=CARTESIAN_POINT('Ctrl Pts',(-24.7737068257992,26.5353486382798,-42.9222813716412));
#21684=CARTESIAN_POINT('Ctrl Pts',(-24.6365858724406,26.5879343773074,-42.9320801662562));
#21685=CARTESIAN_POINT('Ctrl Pts',(-24.3190657090242,26.6854474529186,-42.9545085646638));
#21686=CARTESIAN_POINT('Ctrl Pts',(-24.1373812674653,26.724493635316,-42.9671674935667));
#21687=CARTESIAN_POINT('Ctrl Pts',(-23.944443624342,26.7488164850273,-42.9799066384287));
#21688=CARTESIAN_POINT('Ctrl Pts',(-23.935541674287,26.749900990639,-42.9804928060862));
#21689=CARTESIAN_POINT('Ctrl Pts',(-23.9214534223858,26.7515576848575,-42.9814178267836));
#21690=CARTESIAN_POINT('Ctrl Pts',(-23.9162701145603,26.7521544531446,-42.9817575908504));
#21691=CARTESIAN_POINT('Ctrl Pts',(-23.9085947836463,26.7530192535508,-42.9822598460023));
#21692=CARTESIAN_POINT('Ctrl Pts',(-23.9061038837766,26.7532969677676,-42.9824227104421));
#21693=CARTESIAN_POINT('Ctrl Pts',(-23.8510150238207,26.7593738539185,-42.9860216288555));
#21694=CARTESIAN_POINT('Ctrl Pts',(-23.7982785290693,26.7638800237957,-42.9894065051399));
#21695=CARTESIAN_POINT('Ctrl Pts',(-23.7397115768795,26.7674338909795,-42.9930814223604));
#21696=CARTESIAN_POINT('Ctrl Pts',(-23.7339708694857,26.7677668210038,-42.993440740328));
#21697=CARTESIAN_POINT('Ctrl Pts',(-23.7259312181542,26.7682114902152,-42.9939426686887));
#21698=CARTESIAN_POINT('Ctrl Pts',(-23.7236330428516,26.7683361319187,-42.9940860006708));
#21699=CARTESIAN_POINT('Ctrl Pts',(-23.7194290760997,26.7685596178955,-42.9943479215933));
#21700=CARTESIAN_POINT('Ctrl Pts',(-23.7175233278509,26.7686592314575,-42.9944665541269));
#21701=CARTESIAN_POINT('Ctrl Pts',(-23.7136536332149,26.7688580541859,-42.9947072337291));
#21702=CARTESIAN_POINT('Ctrl Pts',(-23.7116896838639,26.7689571586119,-42.9948292747261));
#21703=CARTESIAN_POINT('Ctrl Pts',(-23.7068116924114,26.7691988350085,-42.9951321284785));
#21704=CARTESIAN_POINT('Ctrl Pts',(-23.7038975376462,26.7693392479435,-42.995312818822));
#21705=CARTESIAN_POINT('Ctrl Pts',(-23.6932050600677,26.7698398917377,-42.9959749423367));
#21706=CARTESIAN_POINT('Ctrl Pts',(-23.6854255479992,26.7701758930425,-42.9964550192184));
#21707=CARTESIAN_POINT('Ctrl Pts',(-23.4902013778715,26.7778989565271,-43.0084623570223));
#21708=CARTESIAN_POINT('Ctrl Pts',(-23.3024352674284,26.7689351101779,-43.0190948824889));
#21709=CARTESIAN_POINT('Ctrl Pts',(-22.8604541181004,26.7089009432671,-43.0440987794798));
#21710=CARTESIAN_POINT('Ctrl Pts',(-22.6095554302573,26.6434643067658,-43.0583441782979));
#21711=CARTESIAN_POINT('Ctrl Pts',(-22.3581892156027,26.5444538945471,-43.0743291516297));
#21712=CARTESIAN_POINT('Ctrl Pts',(-22.3472361732084,26.540069982122,-43.0750290372827));
#21713=CARTESIAN_POINT('Ctrl Pts',(-22.3299544988236,26.5330427201627,-43.0761387735316));
#21714=CARTESIAN_POINT('Ctrl Pts',(-22.3236097450076,26.530439114825,-43.0765473686224));
#21715=CARTESIAN_POINT('Ctrl Pts',(-22.3055903922116,26.5229774799171,-43.0777111710808));
#21716=CARTESIAN_POINT('Ctrl Pts',(-22.2939360981708,26.5180710017822,-43.0784679200922));
#21717=CARTESIAN_POINT('Ctrl Pts',(-22.2713968250993,26.5084253767869,-43.0799395096063));
#21718=CARTESIAN_POINT('Ctrl Pts',(-22.2605085518176,26.5036944153984,-43.080654072008));
#21719=CARTESIAN_POINT('Ctrl Pts',(-22.2452342047817,26.4969571296919,-43.0816617519892));
#21720=CARTESIAN_POINT('Ctrl Pts',(-22.2408260269479,26.4950009164835,-43.08195318887));
#21721=CARTESIAN_POINT('Ctrl Pts',(-22.218431093261,26.4850025073071,-43.0834369619699));
#21722=CARTESIAN_POINT('Ctrl Pts',(-22.2005142701219,26.4768055145826,-43.0846344956677));
#21723=CARTESIAN_POINT('Ctrl Pts',(-22.1770872020643,26.4658266788861,-43.0862144973648));
#21724=CARTESIAN_POINT('Ctrl Pts',(-22.171507926024,26.4631924455562,-43.0865918453896));
#21725=CARTESIAN_POINT('Ctrl Pts',(-22.162897531423,26.4590968020099,-43.0871758563069));
#21726=CARTESIAN_POINT('Ctrl Pts',(-22.159861058266,26.4576466288553,-43.0873821282361));
#21727=CARTESIAN_POINT('Ctrl Pts',(-22.1538113793065,26.4547457498651,-43.0877937310732));
#21728=CARTESIAN_POINT('Ctrl Pts',(-22.1507981491557,26.453295104159,-43.0879990596938));
#21729=CARTESIAN_POINT('Ctrl Pts',(-22.1441127285459,26.4500637449395,-43.0884553271919));
#21730=CARTESIAN_POINT('Ctrl Pts',(-22.1404416562234,26.4482807430166,-43.0887063457074));
#21731=CARTESIAN_POINT('Ctrl Pts',(-22.1299658720555,26.4431681470142,-43.089424015885));
#21732=CARTESIAN_POINT('Ctrl Pts',(-22.1231695339633,26.4398215426241,-43.0898912620281));
#21733=CARTESIAN_POINT('Ctrl Pts',(-22.1025516172965,26.4295785329546,-43.0913137850912));
#21734=CARTESIAN_POINT('Ctrl Pts',(-22.088768237422,26.4226069285476,-43.0922716814179));
#21735=CARTESIAN_POINT('Ctrl Pts',(-22.0750360145756,26.4155367741596,-43.0932330566435));
#21736=CARTESIAN_POINT('',(-26.7730012459478,23.5532182425584,-42.9355038191065));
#21737=CARTESIAN_POINT('Ctrl Pts',(-22.0750361136176,26.4155368251522,-43.341564988124));
#21738=CARTESIAN_POINT('Ctrl Pts',(-22.1509427032916,26.4546179898321,-43.3367652759782));
#21739=CARTESIAN_POINT('Ctrl Pts',(-22.2284014654945,26.4906823867973,-43.3320071409988));
#21740=CARTESIAN_POINT('Ctrl Pts',(-22.5314253727972,26.6173611431577,-43.3136374046661));
#21741=CARTESIAN_POINT('Ctrl Pts',(-22.7654593675607,26.6854142183436,-43.2998809977801));
#21742=CARTESIAN_POINT('Ctrl Pts',(-23.019686662624,26.729064029028,-43.2842307957217));
#21743=CARTESIAN_POINT('Ctrl Pts',(-23.0344914490408,26.7314996410399,-43.2833172542116));
#21744=CARTESIAN_POINT('Ctrl Pts',(-23.0547682160038,26.7346902147219,-43.2820629360421));
#21745=CARTESIAN_POINT('Ctrl Pts',(-23.0602260924065,26.7355346467322,-43.2817250036414));
#21746=CARTESIAN_POINT('Ctrl Pts',(-23.0688847564448,26.7368515173849,-43.2811883911328));
#21747=CARTESIAN_POINT('Ctrl Pts',(-23.0720841486359,26.737333175163,-43.2809900039576));
#21748=CARTESIAN_POINT('Ctrl Pts',(-23.0782857274384,26.7382572536265,-43.2806052467567));
#21749=CARTESIAN_POINT('Ctrl Pts',(-23.0812878255569,26.7387002536557,-43.2804188953232));
#21750=CARTESIAN_POINT('Ctrl Pts',(-23.0884317713322,26.7397441312741,-43.2799752139371));
#21751=CARTESIAN_POINT('Ctrl Pts',(-23.0925741648609,26.7403411810519,-43.2797177628843));
#21752=CARTESIAN_POINT('Ctrl Pts',(-23.1011546879221,26.7415608486552,-43.2791840954712));
#21753=CARTESIAN_POINT('Ctrl Pts',(-23.1055929744104,26.742182281074,-43.2789078420717));
#21754=CARTESIAN_POINT('Ctrl Pts',(-23.1308289876758,26.7456620781179,-43.2773358438323));
#21755=CARTESIAN_POINT('Ctrl Pts',(-23.1516525654624,26.7483263757426,-43.2760339657362));
#21756=CARTESIAN_POINT('Ctrl Pts',(-23.2842769950932,26.7639797533935,-43.2677107947191));
#21757=CARTESIAN_POINT('Ctrl Pts',(-23.3966554147684,26.771306482326,-43.2605115909895));
#21758=CARTESIAN_POINT('Ctrl Pts',(-23.6819401472285,26.7749429109132,-43.2418534081711));
#21759=CARTESIAN_POINT('Ctrl Pts',(-23.8545854562671,26.7632480547429,-43.230194448169));
#21760=CARTESIAN_POINT('Ctrl Pts',(-24.2245240346053,26.7080982289457,-43.204875831523));
#21761=CARTESIAN_POINT('Ctrl Pts',(-24.420411636503,26.6598303796107,-43.1912559840728));
#21762=CARTESIAN_POINT('Ctrl Pts',(-24.6222829617328,26.5894996631098,-43.1777724204905));
#21763=CARTESIAN_POINT('Ctrl Pts',(-24.6340088545185,26.5853381340295,-43.1769913630384));
#21764=CARTESIAN_POINT('Ctrl Pts',(-24.6491037292234,26.579882315304,-43.1759889466229));
#21765=CARTESIAN_POINT('Ctrl Pts',(-24.6524948389542,26.5786502064451,-43.1757639497925));
#21766=CARTESIAN_POINT('Ctrl Pts',(-24.6576760423978,26.5767578382635,-43.1754204944025));
#21767=CARTESIAN_POINT('Ctrl Pts',(-24.6594676164031,26.5761016850145,-43.1753017904183));
#21768=CARTESIAN_POINT('Ctrl Pts',(-24.6628330205577,26.5748657352924,-43.1750789183773));
#21769=CARTESIAN_POINT('Ctrl Pts',(-24.664406974584,26.5742863034969,-43.1749747290874));
#21770=CARTESIAN_POINT('Ctrl Pts',(-24.6680285047044,26.5729498705327,-43.1747351020247));
#21771=CARTESIAN_POINT('Ctrl Pts',(-24.670075760727,26.5721920188194,-43.1745997163465));
#21772=CARTESIAN_POINT('Ctrl Pts',(-24.6742756255496,26.5706324619997,-43.174322130593));
#21773=CARTESIAN_POINT('Ctrl Pts',(-24.6764281511334,26.5698305341925,-43.1741799439913));
#21774=CARTESIAN_POINT('Ctrl Pts',(-24.6868494873043,26.5659353506076,-43.1734919458912));
#21775=CARTESIAN_POINT('Ctrl Pts',(-24.6951065275419,26.5628103877854,-43.1729480226252));
#21776=CARTESIAN_POINT('Ctrl Pts',(-24.7158331253518,26.5548686681785,-43.1715854331672));
#21777=CARTESIAN_POINT('Ctrl Pts',(-24.7282858826642,26.5500081360755,-43.1707692883313));
#21778=CARTESIAN_POINT('Ctrl Pts',(-24.7781563947916,26.5301843454133,-43.1675095434055));
#21779=CARTESIAN_POINT('Ctrl Pts',(-24.8153239242216,26.5145966770975,-43.1650999266536));
#21780=CARTESIAN_POINT('Ctrl Pts',(-24.9438703527657,26.4578273417474,-43.1568030173911));
#21781=CARTESIAN_POINT('Ctrl Pts',(-25.0336183545985,26.4130816950656,-43.1510754175367));
#21782=CARTESIAN_POINT('Ctrl Pts',(-25.1941080437709,26.3234889160769,-43.1407025997512));
#21783=CARTESIAN_POINT('Ctrl Pts',(-25.2654644298278,26.2799319288187,-43.1360398852771));
#21784=CARTESIAN_POINT('Ctrl Pts',(-25.431619193957,26.1694181901096,-43.1248890819668));
#21785=CARTESIAN_POINT('Ctrl Pts',(-25.5246495743898,26.1000219310312,-43.1184006538264));
#21786=CARTESIAN_POINT('Ctrl Pts',(-25.6539676115307,25.9922279432827,-43.1087895065271));
#21787=CARTESIAN_POINT('Ctrl Pts',(-25.6933763416155,25.9577161424069,-43.1057743619891));
#21788=CARTESIAN_POINT('Ctrl Pts',(-25.8049385677268,25.8551059089662,-43.0969527498797));
#21789=CARTESIAN_POINT('Ctrl Pts',(-25.8748056359993,25.7846222454367,-43.0910638382995));
#21790=CARTESIAN_POINT('Ctrl Pts',(-25.9475815132422,25.7040907109088,-43.0844571203788));
#21791=CARTESIAN_POINT('Ctrl Pts',(-25.9538259928983,25.6971199616267,-43.0838862180708));
#21792=CARTESIAN_POINT('Ctrl Pts',(-25.9630464721434,25.6867364342051,-43.0830372006146));
#21793=CARTESIAN_POINT('Ctrl Pts',(-25.9660458234296,25.6833443806362,-43.0827600651662));
#21794=CARTESIAN_POINT('Ctrl Pts',(-25.9711653965373,25.6775298589418,-43.0822853785946));
#21795=CARTESIAN_POINT('Ctrl Pts',(-25.9732891616148,25.6751105072152,-43.0820879757709));
#21796=CARTESIAN_POINT('Ctrl Pts',(-25.9774116055984,25.6704000822708,-43.0817038453381));
#21797=CARTESIAN_POINT('Ctrl Pts',(-25.9794106747698,25.6681093545422,-43.0815171343298));
#21798=CARTESIAN_POINT('Ctrl Pts',(-25.9841807974182,25.6626276453863,-43.0810705610262));
#21799=CARTESIAN_POINT('Ctrl Pts',(-25.9869488160599,25.6594340414561,-43.0808105731081));
#21800=CARTESIAN_POINT('Ctrl Pts',(-25.9926762278723,25.6527997124927,-43.0802708523722));
#21801=CARTESIAN_POINT('Ctrl Pts',(-25.9956346494727,25.6493581643023,-43.0799910800869));
#21802=CARTESIAN_POINT('Ctrl Pts',(-26.0033471803171,25.6403477022209,-43.079259129514));
#21803=CARTESIAN_POINT('Ctrl Pts',(-26.0080895774494,25.6347688381916,-43.0788064692659));
#21804=CARTESIAN_POINT('Ctrl Pts',(-26.0487693912511,25.5865820724542,-43.074901130033));
#21805=CARTESIAN_POINT('Ctrl Pts',(-26.083612896262,25.5430669061555,-43.0714040691947));
#21806=CARTESIAN_POINT('Ctrl Pts',(-26.1995141587219,25.3903661971389,-43.0592221502688));
#21807=CARTESIAN_POINT('Ctrl Pts',(-26.2747728396409,25.2769796538916,-43.0503212471366));
#21808=CARTESIAN_POINT('Ctrl Pts',(-26.3664187966465,25.1179239288207,-43.0380682233437));
#21809=CARTESIAN_POINT('Ctrl Pts',(-26.3892787681611,25.0761345294865,-43.034870294632));
#21810=CARTESIAN_POINT('Ctrl Pts',(-26.4331633108364,24.9915083879703,-43.0284456893695));
#21811=CARTESIAN_POINT('Ctrl Pts',(-26.4541797551028,24.9486800747144,-43.025219737639));
#21812=CARTESIAN_POINT('Ctrl Pts',(-26.5501661064703,24.7415717359503,-43.0097696610343));
#21813=CARTESIAN_POINT('Ctrl Pts',(-26.6121976813115,24.5716367142189,-42.9975176262422));
#21814=CARTESIAN_POINT('Ctrl Pts',(-26.6603536598788,24.3948798423677,-42.9857021713235));
#21815=CARTESIAN_POINT('Ctrl Pts',(-26.6610340135151,24.3923706314408,-42.9855346300338));
#21816=CARTESIAN_POINT('Ctrl Pts',(-26.6719771648019,24.3518169898049,-42.9828299238098));
#21817=CARTESIAN_POINT('Ctrl Pts',(-26.6815449905338,24.3135861115317,-42.9803239013369));
#21818=CARTESIAN_POINT('Ctrl Pts',(-26.6914839806191,24.2705339725259,-42.9775580317215));
#21819=CARTESIAN_POINT('Ctrl Pts',(-26.6925479018824,24.2658782557377,-42.9772596598676));
#21820=CARTESIAN_POINT('Ctrl Pts',(-26.6941334151144,24.2588683425161,-42.9768115347045));
#21821=CARTESIAN_POINT('Ctrl Pts',(-26.6946627145101,24.2565159236234,-42.976661340515));
#21822=CARTESIAN_POINT('Ctrl Pts',(-26.6955743450391,24.252442932867,-42.9764016244539));
#21823=CARTESIAN_POINT('Ctrl Pts',(-26.6959579047328,24.2507226417437,-42.976292031464));
#21824=CARTESIAN_POINT('Ctrl Pts',(-26.69675363905,24.2471398845384,-42.9760640019667));
#21825=CARTESIAN_POINT('Ctrl Pts',(-26.6971655709079,24.2452773692289,-42.9759455800912));
#21826=CARTESIAN_POINT('Ctrl Pts',(-26.6981396317212,24.240854615942,-42.9756646577238));
#21827=CARTESIAN_POINT('Ctrl Pts',(-26.6987002928595,24.2382940483295,-42.9755022423958));
#21828=CARTESIAN_POINT('Ctrl Pts',(-26.6998762477183,24.2328918678211,-42.9751600554505));
#21829=CARTESIAN_POINT('Ctrl Pts',(-26.7004908218055,24.2300500982119,-42.9749803252388));
#21830=CARTESIAN_POINT('Ctrl Pts',(-26.7021530328351,24.2223134298431,-42.9744917493741));
#21831=CARTESIAN_POINT('Ctrl Pts',(-26.7031931177195,24.2174168905245,-42.9741833314858));
#21832=CARTESIAN_POINT('Ctrl Pts',(-26.7064013641297,24.2021379541389,-42.9732234018969));
#21833=CARTESIAN_POINT('Ctrl Pts',(-26.7085297099783,24.1917471371085,-42.9725740935284));
#21834=CARTESIAN_POINT('Ctrl Pts',(-26.7519035106713,23.9745422120992,-42.9590709954143));
#21835=CARTESIAN_POINT('Ctrl Pts',(-26.7728071020175,23.7641565808426,-42.9472921418563));
#21836=CARTESIAN_POINT('Ctrl Pts',(-26.7730011678017,23.5532174882307,-42.9355036403026));
#21837=CARTESIAN_POINT('Ctrl Pts',(-26.7730011671007,23.5532182500986,-42.9355036828802));
#21838=CARTESIAN_POINT('Ctrl Pts',(-26.7732206776241,23.3146833849243,-42.9221729691654));
#21839=CARTESIAN_POINT('Ctrl Pts',(-26.7469586553834,23.076880648849,-42.9088692482139));
#21840=CARTESIAN_POINT('Ctrl Pts',(-26.684120406286,22.7970455993921,-42.8917955242866));
#21841=CARTESIAN_POINT('Ctrl Pts',(-26.6724855231058,22.7501842192223,-42.8888899037176));
#21842=CARTESIAN_POINT('Ctrl Pts',(-26.6580400778509,22.6971293547783,-42.8855413888005));
#21843=CARTESIAN_POINT('Ctrl Pts',(-26.6562570795019,22.6906605732828,-42.8851321150198));
#21844=CARTESIAN_POINT('Ctrl Pts',(-26.6533035181252,22.6800741228125,-42.8844606599944));
#21845=CARTESIAN_POINT('Ctrl Pts',(-26.6521449238131,22.6759531120956,-42.8841988683537));
#21846=CARTESIAN_POINT('Ctrl Pts',(-26.6498768780253,22.6679471435574,-42.8836894723828));
#21847=CARTESIAN_POINT('Ctrl Pts',(-26.6487683243971,22.6640619379524,-42.8834418977168));
#21848=CARTESIAN_POINT('Ctrl Pts',(-26.6468190278943,22.6572785098653,-42.8830089898229));
#21849=CARTESIAN_POINT('Ctrl Pts',(-26.6459815130836,22.6543793583389,-42.8828237622843));
#21850=CARTESIAN_POINT('Ctrl Pts',(-26.6442185335528,22.648308599153,-42.8824354618323));
#21851=CARTESIAN_POINT('Ctrl Pts',(-26.6432922616326,22.6451372313043,-42.8822323626942));
#21852=CARTESIAN_POINT('Ctrl Pts',(-26.6407079219387,22.6363392692763,-42.8816682286616));
#21853=CARTESIAN_POINT('Ctrl Pts',(-26.6390393728553,22.6307157899285,-42.8813068508859));
#21854=CARTESIAN_POINT('Ctrl Pts',(-26.6323691989374,22.6084584382784,-42.8798733681443));
#21855=CARTESIAN_POINT('Ctrl Pts',(-26.6272485568308,22.5918608021945,-42.8787973651135));
#21856=CARTESIAN_POINT('Ctrl Pts',(-26.5403119610899,22.317951780387,-42.8609213293141));
#21857=CARTESIAN_POINT('Ctrl Pts',(-26.4266305769215,22.0719403799912,-42.8429861118193));
#21858=CARTESIAN_POINT('Ctrl Pts',(-26.2612559937834,21.8071614899485,-42.8218631250814));
#21859=CARTESIAN_POINT('Ctrl Pts',(-26.2381484476058,21.7717358178402,-42.8189987985425));
#21860=CARTESIAN_POINT('Ctrl Pts',(-26.1919273127832,21.7038344314972,-42.8134433823286));
#21861=CARTESIAN_POINT('Ctrl Pts',(-26.1688949303604,21.6713120022597,-42.8107523034702));
#21862=CARTESIAN_POINT('Ctrl Pts',(-26.0840253181362,21.5560663168118,-42.8011240275994));
#21863=CARTESIAN_POINT('Ctrl Pts',(-26.0188182410852,21.4758923672966,-42.7942493961707));
#21864=CARTESIAN_POINT('Ctrl Pts',(-25.9195477237839,21.365161906826,-42.7846402675818));
#21865=CARTESIAN_POINT('Ctrl Pts',(-25.8885135381685,21.3319836701529,-42.7817453708159));
#21866=CARTESIAN_POINT('Ctrl Pts',(-25.8543161380089,21.2969392000632,-42.7786811436662));
#21867=CARTESIAN_POINT('Ctrl Pts',(-25.8518417443447,21.2944118527135,-42.7784601198127));
#21868=CARTESIAN_POINT('Ctrl Pts',(-25.8477530346648,21.2902493722076,-42.7780960456291));
#21869=CARTESIAN_POINT('Ctrl Pts',(-25.8461411297105,21.288611891005,-42.7779528085938));
#21870=CARTESIAN_POINT('Ctrl Pts',(-25.8429940370427,21.2854216947814,-42.7776737253421));
#21871=CARTESIAN_POINT('Ctrl Pts',(-25.8414590203296,21.2838688138119,-42.7775378658036));
#21872=CARTESIAN_POINT('Ctrl Pts',(-25.8387421032135,21.2811258590118,-42.7772978705684));
#21873=CARTESIAN_POINT('Ctrl Pts',(-25.8375608581509,21.2799351540174,-42.7771936839051));
#21874=CARTESIAN_POINT('Ctrl Pts',(-25.8350341483264,21.2773921827844,-42.7769711614507));
#21875=CARTESIAN_POINT('Ctrl Pts',(-25.8336884162037,21.2760401927231,-42.7768528479161));
#21876=CARTESIAN_POINT('Ctrl Pts',(-25.8297951966268,21.2721358082554,-42.7765111472974));
#21877=CARTESIAN_POINT('Ctrl Pts',(-25.8272446140629,21.2695864833671,-42.7762880062305));
#21878=CARTESIAN_POINT('Ctrl Pts',(-25.8158864839073,21.2582720000677,-42.7752974855546));
#21879=CARTESIAN_POINT('Ctrl Pts',(-25.8070324118643,21.2495533885912,-42.7745337646571));
#21880=CARTESIAN_POINT('Ctrl Pts',(-25.6544360638322,21.1010201942704,-42.7615101847948));
#21881=CARTESIAN_POINT('Ctrl Pts',(-25.4979786022824,20.9748463711242,-42.750240755244));
#21882=CARTESIAN_POINT('Ctrl Pts',(-25.2332578675626,20.7993798523723,-42.7324765783569));
#21883=CARTESIAN_POINT('Ctrl Pts',(-25.1322857510813,20.7400963744484,-42.725965492665));
#21884=CARTESIAN_POINT('Ctrl Pts',(-24.9114308274586,20.6261094757991,-42.71190530181));
#21885=CARTESIAN_POINT('Ctrl Pts',(-24.7909734846356,20.5730012596527,-42.7043391769411));
#21886=CARTESIAN_POINT('Ctrl Pts',(-24.6161511215678,20.5083800237233,-42.6932646385291));
#21887=CARTESIAN_POINT('Ctrl Pts',(-24.5642107892402,20.4906747416888,-42.6899641633517));
#21888=CARTESIAN_POINT('Ctrl Pts',(-24.5063626728252,20.4725904373069,-42.6862689599717));
#21889=CARTESIAN_POINT('Ctrl Pts',(-24.5008746828447,20.4708908942324,-42.6859182121876));
#21890=CARTESIAN_POINT('Ctrl Pts',(-24.4905118985441,20.4677120473752,-42.6852555405896));
#21891=CARTESIAN_POINT('Ctrl Pts',(-24.4856380783167,20.466229608123,-42.6849437205553));
#21892=CARTESIAN_POINT('Ctrl Pts',(-24.4774068247731,20.4637472666001,-42.6844168318767));
#21893=CARTESIAN_POINT('Ctrl Pts',(-24.4740512274464,20.4627412678766,-42.6842019634287));
#21894=CARTESIAN_POINT('Ctrl Pts',(-24.4674098343044,20.4607619930267,-42.6837765467458));
#21895=CARTESIAN_POINT('Ctrl Pts',(-24.4641241127102,20.4597884824765,-42.6835660065137));
#21896=CARTESIAN_POINT('Ctrl Pts',(-24.4568812580183,20.4576550927498,-42.6831017419829));
#21897=CARTESIAN_POINT('Ctrl Pts',(-24.4529234430589,20.4564975652672,-42.6828479410905));
#21898=CARTESIAN_POINT('Ctrl Pts',(-24.4391056344832,20.4524850945711,-42.6819614751238));
#21899=CARTESIAN_POINT('Ctrl Pts',(-24.4292343099713,20.4496696893271,-42.6813275202032));
#21900=CARTESIAN_POINT('Ctrl Pts',(-24.3285911623559,20.4214844522414,-42.6748568998874));
#21901=CARTESIAN_POINT('Ctrl Pts',(-24.2367699056705,20.4000633930816,-42.6688924297269));
#21902=CARTESIAN_POINT('Ctrl Pts',(-24.0877672710488,20.3721263306123,-42.6591018476719));
#21903=CARTESIAN_POINT('Ctrl Pts',(-24.0311158018936,20.3630628346784,-42.6553543966523));
#21904=CARTESIAN_POINT('Ctrl Pts',(-23.8590258064222,20.3402232013328,-42.6439030095324));
#21905=CARTESIAN_POINT('Ctrl Pts',(-23.743060690231,20.3311764155558,-42.6360912314604));
#21906=CARTESIAN_POINT('Ctrl Pts',(-23.469509084614,20.324671379708,-42.6175908269821));
#21907=CARTESIAN_POINT('Ctrl Pts',(-23.3120820798332,20.3324625932331,-42.606882461056));
#21908=CARTESIAN_POINT('Ctrl Pts',(-23.0718318341764,20.3620873026283,-42.5909171521204));
#21909=CARTESIAN_POINT('Ctrl Pts',(-22.9882455603358,20.375754921397,-42.5854368989521));
#21910=CARTESIAN_POINT('Ctrl Pts',(-22.8999458416692,20.3937911452664,-42.5797940930526));
#21911=CARTESIAN_POINT('Ctrl Pts',(-22.8946079193113,20.3948955917597,-42.5794535495129));
#21912=CARTESIAN_POINT('Ctrl Pts',(-22.8873347536634,20.3964197043327,-42.5789903545931));
#21913=CARTESIAN_POINT('Ctrl Pts',(-22.885397097424,20.3968276102883,-42.5788670326369));
#21914=CARTESIAN_POINT('Ctrl Pts',(-22.8815384804972,20.3976436221017,-42.5786216095497));
#21915=CARTESIAN_POINT('Ctrl Pts',(-22.8796175144712,20.398051698493,-42.5784995067757));
#21916=CARTESIAN_POINT('Ctrl Pts',(-22.8758284117761,20.3988602490264,-42.5782588151013));
#21917=CARTESIAN_POINT('Ctrl Pts',(-22.8739602578487,20.3992606286329,-42.5781402209454));
#21918=CARTESIAN_POINT('Ctrl Pts',(-22.8698344318877,20.4001487069191,-42.5778784684429));
#21919=CARTESIAN_POINT('Ctrl Pts',(-22.8675769220889,20.4006371727122,-42.5777353544868));
#21920=CARTESIAN_POINT('Ctrl Pts',(-22.8598738026146,20.4023125963778,-42.5772473808399));
#21921=CARTESIAN_POINT('Ctrl Pts',(-22.8544307078257,20.4035112623084,-42.5769031929591));
#21922=CARTESIAN_POINT('Ctrl Pts',(-22.8007619685356,20.4154761319894,-42.573515373625));
#21923=CARTESIAN_POINT('Ctrl Pts',(-22.7527836248303,20.4273367178229,-42.5705334773686));
#21924=CARTESIAN_POINT('Ctrl Pts',(-22.700620908369,20.4415124086974,-42.567323937469));
#21925=CARTESIAN_POINT('Ctrl Pts',(-22.6961505304403,20.442737637185,-42.5670491403152));
#21926=CARTESIAN_POINT('Ctrl Pts',(-22.6885457086712,20.4448395951023,-42.5665820896246));
#21927=CARTESIAN_POINT('Ctrl Pts',(-22.6854099335051,20.4457114325768,-42.5663896283113));
#21928=CARTESIAN_POINT('Ctrl Pts',(-22.6771142218807,20.4480314279735,-42.5658807822747));
#21929=CARTESIAN_POINT('Ctrl Pts',(-22.6719565490922,20.4494877144195,-42.5655647379029));
#21930=CARTESIAN_POINT('Ctrl Pts',(-22.5463802065858,20.4852830806667,-42.5578771048344));
#21931=CARTESIAN_POINT('Ctrl Pts',(-22.4280503090522,20.5266016275272,-42.5507930199896));
#21932=CARTESIAN_POINT('Ctrl Pts',(-22.1639468031365,20.6364693975172,-42.5347513626917));
#21933=CARTESIAN_POINT('Ctrl Pts',(-22.0203114438457,20.7092571453548,-42.5258485516385));
#21934=CARTESIAN_POINT('Ctrl Pts',(-21.784945288413,20.8515750104061,-42.5101915519607));
#21935=CARTESIAN_POINT('Ctrl Pts',(-21.690401976134,20.9158413788921,-42.5035760120963));
#21936=CARTESIAN_POINT('Ctrl Pts',(-21.5730955054729,21.0050480150739,-42.4948000201833));
#21937=CARTESIAN_POINT('Ctrl Pts',(-21.5470269147369,21.025514338664,-42.4928115779633));
#21938=CARTESIAN_POINT('Ctrl Pts',(-21.5052858286745,21.0593385428865,-42.4895622899014));
#21939=CARTESIAN_POINT('Ctrl Pts',(-21.4894172016046,21.0724512830528,-42.488311264693));
#21940=CARTESIAN_POINT('Ctrl Pts',(-21.4702677926775,21.0885862453312,-42.4867818801817));
#21941=CARTESIAN_POINT('Ctrl Pts',(-21.4668659922368,21.0914646297287,-42.4865094269757));
#21942=CARTESIAN_POINT('Ctrl Pts',(-21.4602948397567,21.0970481433587,-42.4859816480036));
#21943=CARTESIAN_POINT('Ctrl Pts',(-21.4571247410851,21.0997523833657,-42.4857263591457));
#21944=CARTESIAN_POINT('Ctrl Pts',(-21.4516568736177,21.1044350772573,-42.4852848594542));
#21945=CARTESIAN_POINT('Ctrl Pts',(-21.4493566305251,21.1064106446494,-42.4850987682156));
#21946=CARTESIAN_POINT('Ctrl Pts',(-21.4446018971717,21.110505928954,-42.4847133603286));
#21947=CARTESIAN_POINT('Ctrl Pts',(-21.4421478124377,21.112626109788,-42.4845140245361));
#21948=CARTESIAN_POINT('Ctrl Pts',(-21.4354939640871,21.1183921956698,-42.4839724319685));
#21949=CARTESIAN_POINT('Ctrl Pts',(-21.4313004453642,21.1220452612138,-42.4836298772822));
#21950=CARTESIAN_POINT('Ctrl Pts',(-21.4156372537136,21.1357612821073,-42.4823458006032));
#21951=CARTESIAN_POINT('Ctrl Pts',(-21.4042297787779,21.1458946734697,-42.4814013336977));
#21952=CARTESIAN_POINT('Ctrl Pts',(-21.2197080378602,21.3121667935714,-42.4659706429489));
#21953=CARTESIAN_POINT('Ctrl Pts',(-21.0640023915785,21.4865219398689,-42.4506571947122));
#21954=CARTESIAN_POINT('Ctrl Pts',(-20.8202759413773,21.8274735407479,-42.4224106028467));
#21955=CARTESIAN_POINT('Ctrl Pts',(-20.7253802154318,21.9879339366995,-42.4096938737346));
#21956=CARTESIAN_POINT('Ctrl Pts',(-20.6197384702381,22.2080249112809,-42.3935991930763));
#21957=CARTESIAN_POINT('Ctrl Pts',(-20.5960346960134,22.2610335680038,-42.3898206935629));
#21958=CARTESIAN_POINT('Ctrl Pts',(-20.5632978955307,22.3398946266288,-42.3843709213058));
#21959=CARTESIAN_POINT('Ctrl Pts',(-20.5531422519381,22.3652654643725,-42.3826432074838));
#21960=CARTESIAN_POINT('Ctrl Pts',(-20.5417313472854,22.3948577499956,-42.3806600929655));
#21961=CARTESIAN_POINT('Ctrl Pts',(-20.5401609101612,22.3989553289121,-42.3803862045866));
#21962=CARTESIAN_POINT('Ctrl Pts',(-20.5377771679084,22.4052131991109,-42.3799690145268));
#21963=CARTESIAN_POINT('Ctrl Pts',(-20.5369578142754,22.4073711569943,-42.3798253495786));
#21964=CARTESIAN_POINT('Ctrl Pts',(-20.5355436710302,22.4111077236578,-42.3795769352665));
#21965=CARTESIAN_POINT('Ctrl Pts',(-20.5349478035115,22.4126859162869,-42.379472120642));
#21966=CARTESIAN_POINT('Ctrl Pts',(-20.5337073360189,22.4159791951783,-42.3792536226877));
#21967=CARTESIAN_POINT('Ctrl Pts',(-20.533062961257,22.4176943585446,-42.3791399532259));
#21968=CARTESIAN_POINT('Ctrl Pts',(-20.5312859048332,22.4224367155131,-42.3788260070789));
#21969=CARTESIAN_POINT('Ctrl Pts',(-20.530156309988,22.4254650756905,-42.3786259169079));
#21970=CARTESIAN_POINT('Ctrl Pts',(-20.5257498663559,22.4373329192826,-42.3778432855927));
#21971=CARTESIAN_POINT('Ctrl Pts',(-20.5225072119643,22.4461851784877,-42.377262779662));
#21972=CARTESIAN_POINT('Ctrl Pts',(-20.4680769244173,22.5968200422595,-42.3674378399944));
#21973=CARTESIAN_POINT('Ctrl Pts',(-20.4268522834777,22.7420297008173,-42.3587636207706));
#21974=CARTESIAN_POINT('Ctrl Pts',(-20.3561252584886,23.0797241947437,-42.3392808543728));
#21975=CARTESIAN_POINT('Ctrl Pts',(-20.3335767316978,23.27304527895,-42.3286004926776));
#21976=CARTESIAN_POINT('Ctrl Pts',(-20.3266567460818,23.5415475013397,-42.3133036561125));
#21977=CARTESIAN_POINT('Ctrl Pts',(-20.3273139357936,23.6159136226975,-42.3090215667337));
#21978=CARTESIAN_POINT('Ctrl Pts',(-20.3342510288998,23.7755267159733,-42.2996677505248));
#21979=CARTESIAN_POINT('Ctrl Pts',(-20.3413511576586,23.8606781944279,-42.2945769069961));
#21980=CARTESIAN_POINT('Ctrl Pts',(-20.3530421880274,23.9552984771299,-42.288772300936));
#21981=CARTESIAN_POINT('Ctrl Pts',(-20.3543055973687,23.965149373171,-42.2881662061302));
#21982=CARTESIAN_POINT('Ctrl Pts',(-20.3562168559389,23.9795246510271,-42.2872790909032));
#21983=CARTESIAN_POINT('Ctrl Pts',(-20.3568288360085,23.9840538109985,-42.2869992067027));
#21984=CARTESIAN_POINT('Ctrl Pts',(-20.3579133582044,23.9919535025763,-42.2865103605113));
#21985=CARTESIAN_POINT('Ctrl Pts',(-20.358381610301,23.9953246239407,-42.2863015347766));
#21986=CARTESIAN_POINT('Ctrl Pts',(-20.3592964105011,24.0018349150251,-42.285897833687));
#21987=CARTESIAN_POINT('Ctrl Pts',(-20.359742253156,24.004974181428,-42.2857029809207));
#21988=CARTESIAN_POINT('Ctrl Pts',(-20.3608100592867,24.0124139307051,-42.2852407515276));
#21989=CARTESIAN_POINT('Ctrl Pts',(-20.3614360877227,24.0167138161565,-42.2849732461435));
#21990=CARTESIAN_POINT('Ctrl Pts',(-20.3636652413472,24.031810571916,-42.2840327886188));
#21991=CARTESIAN_POINT('Ctrl Pts',(-20.3653145074074,24.0426004593252,-42.2833583730647));
#21992=CARTESIAN_POINT('Ctrl Pts',(-20.3877457810092,24.1845202755145,-42.2744575736255));
#21993=CARTESIAN_POINT('Ctrl Pts',(-20.4165538904434,24.3142349241154,-42.2659744731459));
#21994=CARTESIAN_POINT('Ctrl Pts',(-20.5021913105235,24.6117178789863,-42.2456763070632));
#21995=CARTESIAN_POINT('Ctrl Pts',(-20.5650075577419,24.777317108335,-42.2337142487038));
#21996=CARTESIAN_POINT('Ctrl Pts',(-20.691989605443,25.0437219173645,-42.2137419564363));
#21997=CARTESIAN_POINT('Ctrl Pts',(-20.7487469394587,25.1476526813279,-42.2057543563908));
#21998=CARTESIAN_POINT('Ctrl Pts',(-20.8402470588704,25.2952595329839,-42.1943199097766));
#21999=CARTESIAN_POINT('Ctrl Pts',(-20.8706077820063,25.3415324951484,-42.190722158966));
#22000=CARTESIAN_POINT('Ctrl Pts',(-20.9176157539124,25.4093054683775,-42.1854585774973));
#22001=CARTESIAN_POINT('Ctrl Pts',(-20.9333663566295,25.4314120388532,-42.1837426506835));
#22002=CARTESIAN_POINT('Ctrl Pts',(-20.9519822572153,25.4568537852271,-42.1817714958368));
#22003=CARTESIAN_POINT('Ctrl Pts',(-20.9545767462618,25.4603844582049,-42.1814980320123));
#22004=CARTESIAN_POINT('Ctrl Pts',(-20.9582862513728,25.465410970247,-42.1811088411842));
#22005=CARTESIAN_POINT('Ctrl Pts',(-20.959395363661,25.4669111288306,-42.1809927042112));
#22006=CARTESIAN_POINT('Ctrl Pts',(-20.9616336660534,25.4699331097948,-42.1807587883019));
#22007=CARTESIAN_POINT('Ctrl Pts',(-20.9627628981817,25.4714549026143,-42.1806410122555));
#22008=CARTESIAN_POINT('Ctrl Pts',(-20.9649563855117,25.4744054811903,-42.1804126944697));
#22009=CARTESIAN_POINT('Ctrl Pts',(-20.966020480369,25.4758343766084,-42.1803021418879));
#22010=CARTESIAN_POINT('Ctrl Pts',(-20.9685708172373,25.4792531164804,-42.1800376736622));
#22011=CARTESIAN_POINT('Ctrl Pts',(-20.9700581783799,25.4812421303427,-42.1798838369192));
#22012=CARTESIAN_POINT('Ctrl Pts',(-20.9754156266279,25.4883892808974,-42.1793311539395));
#22013=CARTESIAN_POINT('Ctrl Pts',(-20.9792989277195,25.493537563341,-42.1789332305905));
#22014=CARTESIAN_POINT('Ctrl Pts',(-21.0389497853282,25.5721278522812,-42.172861100148));
#22015=CARTESIAN_POINT('Ctrl Pts',(-21.0978351733072,25.6431629750485,-42.1674033130144));
#22016=CARTESIAN_POINT('Ctrl Pts',(-21.3038262492651,25.8710014843749,-42.1496313096764));
#22017=CARTESIAN_POINT('Ctrl Pts',(-21.46355327227,26.0156137231694,-42.1378685133145));
#22018=CARTESIAN_POINT('Ctrl Pts',(-21.7541545066487,26.2300907812917,-42.1175227770986));
#22019=CARTESIAN_POINT('Ctrl Pts',(-21.8775727270662,26.3088095223983,-42.1091568557875));
#22020=CARTESIAN_POINT('Ctrl Pts',(-22.028797831367,26.3913744481203,-42.098935492406));
#22021=CARTESIAN_POINT('Ctrl Pts',(-22.051844796427,26.4035965737945,-42.0973788457045));
#22022=CARTESIAN_POINT('Ctrl Pts',(-22.0750360182176,26.4155367760347,-42.0958126606468));
#22023=CARTESIAN_POINT('Origin',(-23.5502525316942,23.5502525316942,-77.3107734492734));
#22024=CARTESIAN_POINT('',(-22.0750360128358,26.4155367732638,-40.5991777786305));
#22025=CARTESIAN_POINT('',(-22.0750362323924,26.4155368863044,-40.843547806833));
#22026=CARTESIAN_POINT('',(-22.0750360153461,26.4155367745563,-77.3107734492734));
#22027=CARTESIAN_POINT('',(-26.7730012307853,23.547356844137,-41.4399333015911));
#22028=CARTESIAN_POINT('Ctrl Pts',(-22.0750360128358,26.4155367732638,-40.5991777786305));
#22029=CARTESIAN_POINT('Ctrl Pts',(-22.0432934995088,26.3991938641274,-40.6014730868289));
#22030=CARTESIAN_POINT('Ctrl Pts',(-22.0118213416415,26.3823228448258,-40.6037424340515));
#22031=CARTESIAN_POINT('Ctrl Pts',(-21.9754060074539,26.3620156445295,-40.6063549716233));
#22032=CARTESIAN_POINT('Ctrl Pts',(-21.9701872941625,26.3590863153357,-40.6067290547247));
#22033=CARTESIAN_POINT('Ctrl Pts',(-21.9628830495296,26.3549595524493,-40.6072521461456));
#22034=CARTESIAN_POINT('Ctrl Pts',(-21.9607906939689,26.3537743189625,-40.6074019336674));
#22035=CARTESIAN_POINT('Ctrl Pts',(-21.9571685747305,26.3517171787888,-40.6076611342999));
#22036=CARTESIAN_POINT('Ctrl Pts',(-21.9556381993199,26.3508463604878,-40.6077706178724));
#22037=CARTESIAN_POINT('Ctrl Pts',(-21.9524504024701,26.3490289717419,-40.6079986083742));
#22038=CARTESIAN_POINT('Ctrl Pts',(-21.9507931099509,26.3480821840737,-40.6081171004054));
#22039=CARTESIAN_POINT('Ctrl Pts',(-21.946901795441,26.3458545438681,-40.6083952339539));
#22040=CARTESIAN_POINT('Ctrl Pts',(-21.9446684593625,26.3445724812884,-40.6085547967429));
#22041=CARTESIAN_POINT('Ctrl Pts',(-21.937329762816,26.3403479470576,-40.6090789078208));
#22042=CARTESIAN_POINT('Ctrl Pts',(-21.9322308972587,26.3373941278454,-40.6094427228674));
#22043=CARTESIAN_POINT('Ctrl Pts',(-21.9202072363063,26.3303845964982,-40.610299918883));
#22044=CARTESIAN_POINT('Ctrl Pts',(-21.9132893938102,26.3263169493796,-40.6107925439051));
#22045=CARTESIAN_POINT('Ctrl Pts',(-21.7553460920893,26.2326516119365,-40.6220285633252));
#22046=CARTESIAN_POINT('Ctrl Pts',(-21.6118543082005,26.1308697745232,-40.632008045173));
#22047=CARTESIAN_POINT('Ctrl Pts',(-21.3263820560977,25.8910631721327,-40.6529301307129));
#22048=CARTESIAN_POINT('Ctrl Pts',(-21.1873727925544,25.7506594924681,-40.6638126096245));
#22049=CARTESIAN_POINT('Ctrl Pts',(-21.0245667138745,25.5528784006703,-40.678554441625));
#22050=CARTESIAN_POINT('Ctrl Pts',(-20.988326242029,25.5063027226929,-40.6819860439143));
#22051=CARTESIAN_POINT('Ctrl Pts',(-20.9115256726508,25.4018017980419,-40.6896300726272));
#22052=CARTESIAN_POINT('Ctrl Pts',(-20.8715533008564,25.343485196444,-40.6938605905363));
#22053=CARTESIAN_POINT('Ctrl Pts',(-20.8284201034018,25.275893315976,-40.6987441460454));
#22054=CARTESIAN_POINT('Ctrl Pts',(-20.8233431361462,25.2678593055246,-40.6993242875166));
#22055=CARTESIAN_POINT('Ctrl Pts',(-20.8159723810519,25.2560804550531,-40.7001744232374));
#22056=CARTESIAN_POINT('Ctrl Pts',(-20.8136505603031,25.2523531445203,-40.7004433793124));
#22057=CARTESIAN_POINT('Ctrl Pts',(-20.8095515198767,25.2457427254587,-40.7009202712371));
#22058=CARTESIAN_POINT('Ctrl Pts',(-20.8077712097385,25.2428615331809,-40.701128092626));
#22059=CARTESIAN_POINT('Ctrl Pts',(-20.804085531738,25.2368756787653,-40.7015597845266));
#22060=CARTESIAN_POINT('Ctrl Pts',(-20.8021808801656,25.2337705832088,-40.7017836810255));
#22061=CARTESIAN_POINT('Ctrl Pts',(-20.797288733894,25.2257646426548,-40.7023608624063));
#22062=CARTESIAN_POINT('Ctrl Pts',(-20.7943090691751,25.220859049307,-40.7027144343105));
#22063=CARTESIAN_POINT('Ctrl Pts',(-20.7821714944207,25.2007554192019,-40.7041630530388));
#22064=CARTESIAN_POINT('Ctrl Pts',(-20.7731262078621,25.1854900593326,-40.7052622108381));
#22065=CARTESIAN_POINT('Ctrl Pts',(-20.713828851719,25.0835052126581,-40.7126009486155));
#22066=CARTESIAN_POINT('Ctrl Pts',(-20.6675245785196,24.9945651867569,-40.7189820284134));
#22067=CARTESIAN_POINT('Ctrl Pts',(-20.5253943462227,24.6874025347923,-40.7409802985979));
#22068=CARTESIAN_POINT('Ctrl Pts',(-20.4496407799648,24.4607777254294,-40.7572121609062));
#22069=CARTESIAN_POINT('Ctrl Pts',(-20.366753221088,24.075405770627,-40.7837930126721));
#22070=CARTESIAN_POINT('Ctrl Pts',(-20.3450625654275,23.9206904125846,-40.7941831181307));
#22071=CARTESIAN_POINT('Ctrl Pts',(-20.3340398577299,23.755634133418,-40.8045864742499));
#22072=CARTESIAN_POINT('Ctrl Pts',(-20.3334556330648,23.746271114154,-40.8051742783703));
#22073=CARTESIAN_POINT('Ctrl Pts',(-20.3327255117376,23.7336860036915,-40.8059610999286));
#22074=CARTESIAN_POINT('Ctrl Pts',(-20.3325435630609,23.7304661721168,-40.8061621170052));
#22075=CARTESIAN_POINT('Ctrl Pts',(-20.3322659051648,23.7254181259619,-40.806476815705));
#22076=CARTESIAN_POINT('Ctrl Pts',(-20.3321669207041,23.7235901049899,-40.8065906821769));
#22077=CARTESIAN_POINT('Ctrl Pts',(-20.3319797042548,23.7200771979515,-40.806809318125));
#22078=CARTESIAN_POINT('Ctrl Pts',(-20.3318912383243,23.7183923379803,-40.8069141000011));
#22079=CARTESIAN_POINT('Ctrl Pts',(-20.3317113052865,23.7149132855507,-40.8071302981922));
#22080=CARTESIAN_POINT('Ctrl Pts',(-20.331620015588,23.7131190913317,-40.807241704033));
#22081=CARTESIAN_POINT('Ctrl Pts',(-20.3313451896625,23.7076272195437,-40.8075824332072));
#22082=CARTESIAN_POINT('Ctrl Pts',(-20.3311665239998,23.7039292845032,-40.8078114814788));
#22083=CARTESIAN_POINT('Ctrl Pts',(-20.3302808052685,23.6849175097961,-40.8089871421737));
#22084=CARTESIAN_POINT('Ctrl Pts',(-20.3296766390113,23.6695987373537,-40.8099280322875));
#22085=CARTESIAN_POINT('Ctrl Pts',(-20.3249943078711,23.5246109043877,-40.8187776517996));
#22086=CARTESIAN_POINT('Ctrl Pts',(-20.3286396827023,23.3947940002073,-40.8262821490169));
#22087=CARTESIAN_POINT('Ctrl Pts',(-20.3534906693657,23.1146020807431,-40.8422336692604));
#22088=CARTESIAN_POINT('Ctrl Pts',(-20.3775056893194,22.9647975980669,-40.8506125597583));
#22089=CARTESIAN_POINT('Ctrl Pts',(-20.4602008992774,22.6107528428476,-40.871034316267));
#22090=CARTESIAN_POINT('Ctrl Pts',(-20.5286806293075,22.4095678241394,-40.8831815796233));
#22091=CARTESIAN_POINT('Ctrl Pts',(-20.6218112809924,22.2046969659725,-40.8968526716497));
#22092=CARTESIAN_POINT('Ctrl Pts',(-20.6272850267819,22.1928473244589,-40.8976480583589));
#22093=CARTESIAN_POINT('Ctrl Pts',(-20.6348226021802,22.1767868886069,-40.8987325445493));
#22094=CARTESIAN_POINT('Ctrl Pts',(-20.6368239114543,22.1725467499551,-40.8990194759824));
#22095=CARTESIAN_POINT('Ctrl Pts',(-20.6402337323474,22.1653630782633,-40.8995066465937));
#22096=CARTESIAN_POINT('Ctrl Pts',(-20.6416374789106,22.1624172801676,-40.8997067199838));
#22097=CARTESIAN_POINT('Ctrl Pts',(-20.6443516741591,22.1567436774391,-40.9000926418929));
#22098=CARTESIAN_POINT('Ctrl Pts',(-20.6456614960899,22.1540155759809,-40.9002784684017));
#22099=CARTESIAN_POINT('Ctrl Pts',(-20.6487639845143,22.1475769616932,-40.9007176541141));
#22100=CARTESIAN_POINT('Ctrl Pts',(-20.6505599259456,22.1438680408772,-40.900971127359));
#22101=CARTESIAN_POINT('Ctrl Pts',(-20.6558275099628,22.1330425777109,-40.901712375135));
#22102=CARTESIAN_POINT('Ctrl Pts',(-20.6593182539854,22.1259354110119,-40.9022008168593));
#22103=CARTESIAN_POINT('Ctrl Pts',(-20.6840404118411,22.0760663141361,-40.9056408251687));
#22104=CARTESIAN_POINT('Ctrl Pts',(-20.7061926050644,22.0337698715937,-40.9086246244019));
#22105=CARTESIAN_POINT('Ctrl Pts',(-20.7578405964213,21.9402701303874,-40.9153749919312));
#22106=CARTESIAN_POINT('Ctrl Pts',(-20.7878209454303,21.8893555579867,-40.9191579589856));
#22107=CARTESIAN_POINT('Ctrl Pts',(-20.8888284125464,21.7281249654028,-40.931489341758));
#22108=CARTESIAN_POINT('Ctrl Pts',(-20.9651909657424,21.6213207478701,-40.9402122509415));
#22109=CARTESIAN_POINT('Ctrl Pts',(-21.1326803110029,21.4149331532857,-40.9581100519102));
#22110=CARTESIAN_POINT('Ctrl Pts',(-21.2239860436928,21.3158111584823,-40.9672733942923));
#22111=CARTESIAN_POINT('Ctrl Pts',(-21.4202667118616,21.127839614961,-40.9855284813944));
#22112=CARTESIAN_POINT('Ctrl Pts',(-21.5252778375254,21.0393938226189,-40.9945963623213));
#22113=CARTESIAN_POINT('Ctrl Pts',(-21.6420967466228,20.9531148916416,-41.0037170206215));
#22114=CARTESIAN_POINT('Ctrl Pts',(-21.6485929151767,20.9483545460506,-41.0042211975721));
#22115=CARTESIAN_POINT('Ctrl Pts',(-21.6573115271566,20.9420157048091,-41.0048937638975));
#22116=CARTESIAN_POINT('Ctrl Pts',(-21.6595181541871,20.9404156583198,-41.005063636589));
#22117=CARTESIAN_POINT('Ctrl Pts',(-21.6632244935742,20.9377353237225,-41.0053483715488));
#22118=CARTESIAN_POINT('Ctrl Pts',(-21.6647231048641,20.9366535266443,-41.0054633389914));
#22119=CARTESIAN_POINT('Ctrl Pts',(-21.6675884228123,20.9345888970782,-41.0056828449056));
#22120=CARTESIAN_POINT('Ctrl Pts',(-21.6689549605112,20.9336058522581,-41.0057873978757));
#22121=CARTESIAN_POINT('Ctrl Pts',(-21.6717741582797,20.931581158971,-41.0060028162599));
#22122=CARTESIAN_POINT('Ctrl Pts',(-21.6732269101469,20.9305396516636,-41.0061136717063));
#22123=CARTESIAN_POINT('Ctrl Pts',(-21.6764935752806,20.9282018253849,-41.0063626042634));
#22124=CARTESIAN_POINT('Ctrl Pts',(-21.6783079710218,20.9269061773141,-41.0065006347267));
#22125=CARTESIAN_POINT('Ctrl Pts',(-21.6866549663795,20.920958711831,-41.0071345683827));
#22126=CARTESIAN_POINT('Ctrl Pts',(-21.6932036465316,20.9163293517254,-41.0076289279773));
#22127=CARTESIAN_POINT('Ctrl Pts',(-21.7094523123623,20.9049336503199,-41.0088483269352));
#22128=CARTESIAN_POINT('Ctrl Pts',(-21.7191724810835,20.8981961051158,-41.0095714665436));
#22129=CARTESIAN_POINT('Ctrl Pts',(-21.7570645642291,20.8722388075072,-41.0123669477128));
#22130=CARTESIAN_POINT('Ctrl Pts',(-21.7855048503091,20.8534124509287,-41.0144149410903));
#22131=CARTESIAN_POINT('Ctrl Pts',(-21.9270681574466,20.7629017756342,-41.024392365917));
#22132=CARTESIAN_POINT('Ctrl Pts',(-22.0442948594015,20.6978587579274,-41.0319868114597));
#22133=CARTESIAN_POINT('Ctrl Pts',(-22.2485282882908,20.6006525408893,-41.0446815122091));
#22134=CARTESIAN_POINT('Ctrl Pts',(-22.3334811711318,20.5646045708852,-41.0498154962284));
#22135=CARTESIAN_POINT('Ctrl Pts',(-22.5228278512153,20.4936850121312,-41.061142067035));
#22136=CARTESIAN_POINT('Ctrl Pts',(-22.6276935862244,20.4604160595815,-41.0673422706006));
#22137=CARTESIAN_POINT('Ctrl Pts',(-22.7728182913045,20.4224226780869,-41.0759889501458));
#22138=CARTESIAN_POINT('Ctrl Pts',(-22.8117718617175,20.4129974067641,-41.0783158153718));
#22139=CARTESIAN_POINT('Ctrl Pts',(-22.8710408503275,20.3998215808066,-41.0818719534878));
#22140=CARTESIAN_POINT('Ctrl Pts',(-22.8912339039355,20.3955357288362,-41.083086269913));
#22141=CARTESIAN_POINT('Ctrl Pts',(-22.9160185410587,20.3905236862489,-41.0845806915805));
#22142=CARTESIAN_POINT('Ctrl Pts',(-22.9205726199284,20.3896129856492,-41.084855449926));
#22143=CARTESIAN_POINT('Ctrl Pts',(-22.9290637893124,20.3879340468324,-41.0853680587963));
#22144=CARTESIAN_POINT('Ctrl Pts',(-22.9330003802871,20.3871633083652,-41.0856058360436));
#22145=CARTESIAN_POINT('Ctrl Pts',(-22.9417757990838,20.3854621897809,-41.0861361773071));
#22146=CARTESIAN_POINT('Ctrl Pts',(-22.946615335699,20.3845355548271,-41.0864288503791));
#22147=CARTESIAN_POINT('Ctrl Pts',(-22.9582741827282,20.3823309207351,-41.0871344121659));
#22148=CARTESIAN_POINT('Ctrl Pts',(-22.9650955123168,20.3810638404964,-41.087547622131));
#22149=CARTESIAN_POINT('Ctrl Pts',(-22.9738272149612,20.3794710551626,-41.0880770907203));
#22150=CARTESIAN_POINT('Ctrl Pts',(-22.9757338979725,20.3791250260317,-41.0881927398401));
#22151=CARTESIAN_POINT('Ctrl Pts',(-22.9833472789303,20.3777504243222,-41.0886546582467));
#22152=CARTESIAN_POINT('Ctrl Pts',(-22.9890564116827,20.3767355392818,-41.0890013376986));
#22153=CARTESIAN_POINT('Ctrl Pts',(-22.9981313129363,20.3751475918589,-41.0895528833153));
#22154=CARTESIAN_POINT('Ctrl Pts',(-23.0014953241061,20.3745644572517,-41.0897574435849));
#22155=CARTESIAN_POINT('Ctrl Pts',(-23.0100394512387,20.3730973568166,-41.0902772715961));
#22156=CARTESIAN_POINT('Ctrl Pts',(-23.015220800795,20.3722207156186,-41.0905927615423));
#22157=CARTESIAN_POINT('Ctrl Pts',(-23.0360606025066,20.3687472034512,-41.0918627376422));
#22158=CARTESIAN_POINT('Ctrl Pts',(-23.0517358032043,20.3662533873181,-41.0928203672257));
#22159=CARTESIAN_POINT('Ctrl Pts',(-23.0851453848522,20.3611909147347,-41.094866861615));
#22160=CARTESIAN_POINT('Ctrl Pts',(-23.1028839891881,20.3586541826271,-41.0959566860303));
#22161=CARTESIAN_POINT('Ctrl Pts',(-23.1265296172773,20.3554737069772,-41.0974140391901));
#22162=CARTESIAN_POINT('Ctrl Pts',(-23.1324188296568,20.3546981441494,-41.0977773895984));
#22163=CARTESIAN_POINT('Ctrl Pts',(-23.1416015884516,20.3535146658704,-41.0983445472564));
#22164=CARTESIAN_POINT('Ctrl Pts',(-23.1448936987909,20.3530955457675,-41.0985479996766));
#22165=CARTESIAN_POINT('Ctrl Pts',(-23.1514787300525,20.3522675367062,-41.0989551984449));
#22166=CARTESIAN_POINT('Ctrl Pts',(-23.1547716468684,20.3518586468433,-41.0991589445056));
#22167=CARTESIAN_POINT('Ctrl Pts',(-23.1621847244827,20.3509497693323,-41.0996178983906));
#22168=CARTESIAN_POINT('Ctrl Pts',(-23.1663052256749,20.3504526544841,-41.0998731967094));
#22169=CARTESIAN_POINT('Ctrl Pts',(-23.1784297368068,20.3490136585173,-41.1006249802945));
#22170=CARTESIAN_POINT('Ctrl Pts',(-23.1864362891244,20.3480938451692,-41.101122162093));
#22171=CARTESIAN_POINT('Ctrl Pts',(-23.2446068067932,20.34163205049,-41.1047398002909));
#22172=CARTESIAN_POINT('Ctrl Pts',(-23.2948889632535,20.3372393536117,-41.107896345652));
#22173=CARTESIAN_POINT('Ctrl Pts',(-23.4427189776245,20.3278167082093,-41.1172701344927));
#22174=CARTESIAN_POINT('Ctrl Pts',(-23.5404096379684,20.3260385084828,-41.123585541634));
#22175=CARTESIAN_POINT('Ctrl Pts',(-23.6626933520622,20.3293700880169,-41.1316364464788));
#22176=CARTESIAN_POINT('Ctrl Pts',(-23.6873550095875,20.3303255879416,-41.1332674052219));
#22177=CARTESIAN_POINT('Ctrl Pts',(-23.8664357991741,20.3393250222433,-41.1451609414709));
#22178=CARTESIAN_POINT('Ctrl Pts',(-24.0201022950793,20.3581899973974,-41.1556524600215));
#22179=CARTESIAN_POINT('Ctrl Pts',(-24.3149287880935,20.4161398880161,-41.1759710422544));
#22180=CARTESIAN_POINT('Ctrl Pts',(-24.4559866552663,20.4539570795694,-41.1857763285285));
#22181=CARTESIAN_POINT('Ctrl Pts',(-24.6321169354082,20.5142503177353,-41.1977706164867));
#22182=CARTESIAN_POINT('Ctrl Pts',(-24.6699800972826,20.5280098901398,-41.2003333002545));
#22183=CARTESIAN_POINT('Ctrl Pts',(-24.7125584764869,20.5443930976456,-41.203189244162));
#22184=CARTESIAN_POINT('Ctrl Pts',(-24.7175347881309,20.5463220762172,-41.2035226257905));
#22185=CARTESIAN_POINT('Ctrl Pts',(-24.7247913243225,20.5491556981223,-41.2040081530552));
#22186=CARTESIAN_POINT('Ctrl Pts',(-24.7270753109588,20.5500505841307,-41.2041608831111));
#22187=CARTESIAN_POINT('Ctrl Pts',(-24.7311141466304,20.5516383570446,-41.2044307992432));
#22188=CARTESIAN_POINT('Ctrl Pts',(-24.7328694101176,20.5523301776327,-41.2045480500412));
#22189=CARTESIAN_POINT('Ctrl Pts',(-24.736530655884,20.5537769390663,-41.2047925062444));
#22190=CARTESIAN_POINT('Ctrl Pts',(-24.7384365216074,20.5545321556717,-41.2049196943245));
#22191=CARTESIAN_POINT('Ctrl Pts',(-24.7423008707186,20.5560677069925,-41.205177454823));
#22192=CARTESIAN_POINT('Ctrl Pts',(-24.7442593119227,20.55684814607,-41.2053080208203));
#22193=CARTESIAN_POINT('Ctrl Pts',(-24.7490805188733,20.5587748819318,-41.2056292826122));
#22194=CARTESIAN_POINT('Ctrl Pts',(-24.75194241521,20.5599233698937,-41.2058198464075));
#22195=CARTESIAN_POINT('Ctrl Pts',(-24.7784501493837,20.5706052062699,-41.207583654508));
#22196=CARTESIAN_POINT('Ctrl Pts',(-24.8019846062008,20.5804150809967,-41.2091403952101));
#22197=CARTESIAN_POINT('Ctrl Pts',(-24.873588747951,20.6112642902991,-41.213855759496));
#22198=CARTESIAN_POINT('Ctrl Pts',(-24.92126525473,20.6332000103845,-41.2169661361109));
#22199=CARTESIAN_POINT('Ctrl Pts',(-25.036262504893,20.6895524063899,-41.2244465007727));
#22200=CARTESIAN_POINT('Ctrl Pts',(-25.1029500358421,20.725192789201,-41.2287657648536));
#22201=CARTESIAN_POINT('Ctrl Pts',(-25.2281691915179,20.7978896349126,-41.2369524295764));
#22202=CARTESIAN_POINT('Ctrl Pts',(-25.2868792512434,20.8345511795097,-41.2408249536195));
#22203=CARTESIAN_POINT('Ctrl Pts',(-25.5756334268529,21.0280599426682,-41.2602532543347));
#22204=CARTESIAN_POINT('Ctrl Pts',(-25.7858094553284,21.2123298231566,-41.2757817689584));
#22205=CARTESIAN_POINT('Ctrl Pts',(-25.9816131934687,21.4348498025244,-41.2937314684605));
#22206=CARTESIAN_POINT('Ctrl Pts',(-25.9934229694182,21.4485005087917,-41.2948292194641));
#22207=CARTESIAN_POINT('Ctrl Pts',(-26.0089771620235,21.4667875697421,-41.2962956321584));
#22208=CARTESIAN_POINT('Ctrl Pts',(-26.0128244469236,21.4713363195683,-41.2966600494951));
#22209=CARTESIAN_POINT('Ctrl Pts',(-26.0187974555728,21.4784382160732,-41.2972284914128));
#22210=CARTESIAN_POINT('Ctrl Pts',(-26.0209318955351,21.4809840424506,-41.2974321584621));
#22211=CARTESIAN_POINT('Ctrl Pts',(-26.0251899574683,21.4860787726058,-41.2978395353777));
#22212=CARTESIAN_POINT('Ctrl Pts',(-26.0273135877231,21.4886276643185,-41.2980432445581));
#22213=CARTESIAN_POINT('Ctrl Pts',(-26.0320806555424,21.4943673463982,-41.2985017388625));
#22214=CARTESIAN_POINT('Ctrl Pts',(-26.0347218792043,21.4975599603456,-41.2987566137074));
#22215=CARTESIAN_POINT('Ctrl Pts',(-26.0424612955657,21.5069519020422,-41.2995059465733));
#22216=CARTESIAN_POINT('Ctrl Pts',(-26.0475424666117,21.5131651587655,-41.3000010942477));
#22217=CARTESIAN_POINT('Ctrl Pts',(-26.08419763603,21.5583303585132,-41.3035963584072));
#22218=CARTESIAN_POINT('Ctrl Pts',(-26.1148804741778,21.5979936363339,-41.3067320927743));
#22219=CARTESIAN_POINT('Ctrl Pts',(-26.238180436743,21.7653069448418,-41.319881982047));
#22220=CARTESIAN_POINT('Ctrl Pts',(-26.3222789106189,21.898936571663,-41.3302170095324));
#22221=CARTESIAN_POINT('Ctrl Pts',(-26.4213855392045,22.0854719062387,-41.3443570466273));
#22222=CARTESIAN_POINT('Ctrl Pts',(-26.4453349988727,22.1333953416888,-41.3479644217399));
#22223=CARTESIAN_POINT('Ctrl Pts',(-26.4792415960228,22.2056961515084,-41.3533586454581));
#22224=CARTESIAN_POINT('Ctrl Pts',(-26.4901129953055,22.229635539159,-41.355136993744));
#22225=CARTESIAN_POINT('Ctrl Pts',(-26.5126652040435,22.2809555970855,-41.358930676814));
#22226=CARTESIAN_POINT('Ctrl Pts',(-26.5242620986793,22.3083706348182,-41.3609461042242));
#22227=CARTESIAN_POINT('Ctrl Pts',(-26.606196915914,22.509796824941,-41.3756602322384));
#22228=CARTESIAN_POINT('Ctrl Pts',(-26.6616030779943,22.6895202703745,-41.3883030925025));
#22229=CARTESIAN_POINT('Ctrl Pts',(-26.703486323747,22.8843933240804,-41.4008652751921));
#22230=CARTESIAN_POINT('Ctrl Pts',(-26.7058600934959,22.8957353376166,-41.401592317885));
#22231=CARTESIAN_POINT('Ctrl Pts',(-26.7088730476672,22.9105289082338,-41.4025350517631));
#22232=CARTESIAN_POINT('Ctrl Pts',(-26.709567801794,22.9139688663901,-41.4027538752986));
#22233=CARTESIAN_POINT('Ctrl Pts',(-26.7106276855379,22.9192612369036,-41.4030899265937));
#22234=CARTESIAN_POINT('Ctrl Pts',(-26.7109968058331,22.9211128328391,-41.4032073835035));
#22235=CARTESIAN_POINT('Ctrl Pts',(-26.7117272735557,22.924793902693,-41.4034406650717));
#22236=CARTESIAN_POINT('Ctrl Pts',(-26.7120886581515,22.9266233554342,-41.4035564909728));
#22237=CARTESIAN_POINT('Ctrl Pts',(-26.7127941393426,22.9302111198549,-41.4037834186036));
#22238=CARTESIAN_POINT('Ctrl Pts',(-26.7131383559935,22.9319693967255,-41.4038945269232));
#22239=CARTESIAN_POINT('Ctrl Pts',(-26.7139104331432,22.9359307254931,-41.4041446184921));
#22240=CARTESIAN_POINT('Ctrl Pts',(-26.7143374596209,22.938133941945,-41.4042835537636));
#22241=CARTESIAN_POINT('Ctrl Pts',(-26.7154074560907,22.9436855591339,-41.4046332385633));
#22242=CARTESIAN_POINT('Ctrl Pts',(-26.7160474163126,22.9470345475399,-41.4048438167735));
#22243=CARTESIAN_POINT('Ctrl Pts',(-26.7178480845425,22.9565394542218,-41.4054404413024));
#22244=CARTESIAN_POINT('Ctrl Pts',(-26.7189961681716,22.9626977916105,-41.4058257803048));
#22245=CARTESIAN_POINT('Ctrl Pts',(-26.7551253405349,23.1596814307465,-41.4181135486117));
#22246=CARTESIAN_POINT('Ctrl Pts',(-26.7728268687897,23.3533010686489,-41.4290673617155));
#22247=CARTESIAN_POINT('Ctrl Pts',(-26.7730012307853,23.547356844137,-41.4399333015911));
#22248=CARTESIAN_POINT('Ctrl Pts',(-26.7730012290087,23.5473548674995,-41.4399331909115));
#22249=CARTESIAN_POINT('Ctrl Pts',(-26.7732549751028,23.8295683468469,-41.4557354257885));
#22250=CARTESIAN_POINT('Ctrl Pts',(-26.7364422799603,24.1105702441252,-41.471339060762));
#22251=CARTESIAN_POINT('Ctrl Pts',(-26.6577818407815,24.4045763104569,-41.4896146590668));
#22252=CARTESIAN_POINT('Ctrl Pts',(-26.6518408398425,24.4258994099139,-41.4909506825791));
#22253=CARTESIAN_POINT('Ctrl Pts',(-26.6428721030603,24.4568525529689,-41.4929061893761));
#22254=CARTESIAN_POINT('Ctrl Pts',(-26.6400179490036,24.4665325512064,-41.4935200412948));
#22255=CARTESIAN_POINT('Ctrl Pts',(-26.6348078181353,24.4839017809155,-41.4946257185757));
#22256=CARTESIAN_POINT('Ctrl Pts',(-26.6324684288685,24.4915959318628,-41.4951169992824));
#22257=CARTESIAN_POINT('Ctrl Pts',(-26.6288791446778,24.5032441036286,-41.4958630406758));
#22258=CARTESIAN_POINT('Ctrl Pts',(-26.6276503642386,24.5072046403937,-41.4961171073852));
#22259=CARTESIAN_POINT('Ctrl Pts',(-26.625510675283,24.514054425397,-41.4965572191203));
#22260=CARTESIAN_POINT('Ctrl Pts',(-26.6246033284534,24.5169447879887,-41.4967431467471));
#22261=CARTESIAN_POINT('Ctrl Pts',(-26.6227136850914,24.5229346974024,-41.4971289086737));
#22262=CARTESIAN_POINT('Ctrl Pts',(-26.6217307708624,24.5260340445379,-41.4973287631529));
#22263=CARTESIAN_POINT('Ctrl Pts',(-26.6193318806055,24.5335587410399,-41.4978145875779));
#22264=CARTESIAN_POINT('Ctrl Pts',(-26.6179110243099,24.5379825168535,-41.4981007182623));
#22265=CARTESIAN_POINT('Ctrl Pts',(-26.6125479623647,24.554556986721,-41.49917469805));
#22266=CARTESIAN_POINT('Ctrl Pts',(-26.6085431316802,24.5666871540768,-41.4999646134527));
#22267=CARTESIAN_POINT('Ctrl Pts',(-26.5421483128516,24.7638441625642,-41.5128682361771));
#22268=CARTESIAN_POINT('Ctrl Pts',(-26.4631539291189,24.9428132072715,-41.5255512014073));
#22269=CARTESIAN_POINT('Ctrl Pts',(-26.3160828759179,25.2079508373001,-41.5458227855924));
#22270=CARTESIAN_POINT('Ctrl Pts',(-26.2589837452152,25.2996966976019,-41.553135220738));
#22271=CARTESIAN_POINT('Ctrl Pts',(-26.1565857635696,25.4471611953628,-41.5652864392093));
#22272=CARTESIAN_POINT('Ctrl Pts',(-26.1138361829237,25.5045490000209,-41.5701229853691));
#22273=CARTESIAN_POINT('Ctrl Pts',(-26.0071713807481,25.6382084548427,-41.5815828848347));
#22274=CARTESIAN_POINT('Ctrl Pts',(-25.9415597577651,25.713043222035,-41.5881618092428));
#22275=CARTESIAN_POINT('Ctrl Pts',(-25.8496097342557,25.8086086047686,-41.5966613082357));
#22276=CARTESIAN_POINT('Ctrl Pts',(-25.8262655079964,25.8321335196531,-41.5987619659739));
#22277=CARTESIAN_POINT('Ctrl Pts',(-25.8002254147379,25.8575778783746,-41.6010390641041));
#22278=CARTESIAN_POINT('Ctrl Pts',(-25.7978858901472,25.8598569385266,-41.6012430697628));
#22279=CARTESIAN_POINT('Ctrl Pts',(-25.7939760841933,25.8636541295277,-41.601583037118));
#22280=CARTESIAN_POINT('Ctrl Pts',(-25.7924077236666,25.8651742210988,-41.6017191514159));
#22281=CARTESIAN_POINT('Ctrl Pts',(-25.7893262399283,25.8681547975615,-41.6019860768491));
#22282=CARTESIAN_POINT('Ctrl Pts',(-25.7878132304284,25.869615397776,-41.6021168970389));
#22283=CARTESIAN_POINT('Ctrl Pts',(-25.7849497936105,25.8723742380507,-41.6023640241589));
#22284=CARTESIAN_POINT('Ctrl Pts',(-25.7835996739742,25.8736727721236,-41.6024803540403));
#22285=CARTESIAN_POINT('Ctrl Pts',(-25.7805224250256,25.8766272845157,-41.6027450637949));
#22286=CARTESIAN_POINT('Ctrl Pts',(-25.7787945859516,25.8782825143536,-41.6028933846121));
#22287=CARTESIAN_POINT('Ctrl Pts',(-25.7736456030834,25.8832041355715,-41.6033344648278));
#22288=CARTESIAN_POINT('Ctrl Pts',(-25.7702190907472,25.8864649392672,-41.6036267885935));
#22289=CARTESIAN_POINT('Ctrl Pts',(-25.7464606709271,25.9089749160287,-41.605645470376));
#22290=CARTESIAN_POINT('Ctrl Pts',(-25.7258850395607,25.9279667273317,-41.6073522625333));
#22291=CARTESIAN_POINT('Ctrl Pts',(-25.7034145397294,25.9481715979209,-41.6091754439544));
#22292=CARTESIAN_POINT('Ctrl Pts',(-25.7017638686874,25.9496527583899,-41.6093091395614));
#22293=CARTESIAN_POINT('Ctrl Pts',(-25.5875956696382,26.0518842641419,-41.6185400889902));
#22294=CARTESIAN_POINT('Ctrl Pts',(-25.468121622834,26.1446152191126,-41.6271270845099));
#22295=CARTESIAN_POINT('Ctrl Pts',(-25.2762305005434,26.2730248805874,-41.6400936534042));
#22296=CARTESIAN_POINT('Ctrl Pts',(-25.2082642282798,26.3149381605884,-41.6445419841237));
#22297=CARTESIAN_POINT('Ctrl Pts',(-25.0692751545718,26.3936791691689,-41.6534764349294));
#22298=CARTESIAN_POINT('Ctrl Pts',(-24.998299079205,26.4304722107358,-41.6579594880579));
#22299=CARTESIAN_POINT('Ctrl Pts',(-24.816383035907,26.5163497905119,-41.6693805940293));
#22300=CARTESIAN_POINT('Ctrl Pts',(-24.7039118856048,26.5618775222612,-41.6763828192389));
#22301=CARTESIAN_POINT('Ctrl Pts',(-24.5397743009979,26.6177735203112,-41.6866990681911));
#22302=CARTESIAN_POINT('Ctrl Pts',(-24.4899991431198,26.6333863551346,-41.6898390555056));
#22303=CARTESIAN_POINT('Ctrl Pts',(-24.4321297177894,26.6500065590867,-41.6935101497815));
#22304=CARTESIAN_POINT('Ctrl Pts',(-24.4243820599904,26.6522003016602,-41.6940020578227));
#22305=CARTESIAN_POINT('Ctrl Pts',(-24.4126301106743,26.655480331304,-41.6947488598523));
#22306=CARTESIAN_POINT('Ctrl Pts',(-24.4086317691149,26.6565879708744,-41.6950030576987));
#22307=CARTESIAN_POINT('Ctrl Pts',(-24.4014319503373,26.6585675365645,-41.6954610030516));
#22308=CARTESIAN_POINT('Ctrl Pts',(-24.3982312390713,26.6594422467045,-41.6956646596145));
#22309=CARTESIAN_POINT('Ctrl Pts',(-24.3918258295243,26.6611821299848,-41.6960723785811));
#22310=CARTESIAN_POINT('Ctrl Pts',(-24.3886211339709,26.6620472980193,-41.6962764408736));
#22311=CARTESIAN_POINT('Ctrl Pts',(-24.3796743897362,26.664447816578,-41.6968463494232));
#22312=CARTESIAN_POINT('Ctrl Pts',(-24.3739294433942,26.6659722295112,-41.6972125505028));
#22313=CARTESIAN_POINT('Ctrl Pts',(-24.3508212870671,26.6720355660777,-41.6986865559263));
#22314=CARTESIAN_POINT('Ctrl Pts',(-24.3334247766313,26.6764452416261,-41.6997985418428));
#22315=CARTESIAN_POINT('Ctrl Pts',(-24.0469970420699,26.7465082433639,-41.7181473188033));
#22316=CARTESIAN_POINT('Ctrl Pts',(-23.7707023933676,26.7773471806951,-41.7365835982629));
#22317=CARTESIAN_POINT('Ctrl Pts',(-23.3586260498454,26.7701457734939,-41.7644782713857));
#22318=CARTESIAN_POINT('Ctrl Pts',(-23.2235886587777,26.7592597380725,-41.7736539242004));
#22319=CARTESIAN_POINT('Ctrl Pts',(-23.0072130592677,26.728012751157,-41.7880887461222));
#22320=CARTESIAN_POINT('Ctrl Pts',(-22.9252789790243,26.7129195640813,-41.7934896225253));
#22321=CARTESIAN_POINT('Ctrl Pts',(-22.8358922271599,26.6928432159545,-41.7992441421683));
#22322=CARTESIAN_POINT('Ctrl Pts',(-22.8277774302417,26.690987570651,-41.799765289005));
#22323=CARTESIAN_POINT('Ctrl Pts',(-22.8174737565613,26.6885893385273,-41.8004253194329));
#22324=CARTESIAN_POINT('Ctrl Pts',(-22.8152782343547,26.6880758901278,-41.8005658620517));
#22325=CARTESIAN_POINT('Ctrl Pts',(-22.8113361452357,26.687149622324,-41.8008180304982));
#22326=CARTESIAN_POINT('Ctrl Pts',(-22.8095893837548,26.6867376479829,-41.8009297050371));
#22327=CARTESIAN_POINT('Ctrl Pts',(-22.8062019441193,26.685935731491,-41.8011461490999));
#22328=CARTESIAN_POINT('Ctrl Pts',(-22.8045612294843,26.6855459610584,-41.8012509282751));
#22329=CARTESIAN_POINT('Ctrl Pts',(-22.8011367646558,26.6847296003248,-41.8014695037635));
#22330=CARTESIAN_POINT('Ctrl Pts',(-22.7993530776284,26.6843027763649,-41.8015832859783));
#22331=CARTESIAN_POINT('Ctrl Pts',(-22.7944177915531,26.6831173414367,-41.8018979290573));
#22332=CARTESIAN_POINT('Ctrl Pts',(-22.7912669600591,26.6823554950077,-41.8020986019821));
#22333=CARTESIAN_POINT('Ctrl Pts',(-22.7788941859147,26.6793440882427,-41.8028858259199));
#22334=CARTESIAN_POINT('Ctrl Pts',(-22.7696809310803,26.6770585136065,-41.8034703115351));
#22335=CARTESIAN_POINT('Ctrl Pts',(-22.6032394702727,26.634987104226,-41.814000524529));
#22336=CARTESIAN_POINT('Ctrl Pts',(-22.4492004563193,26.5834227235543,-41.8232859860548));
#22337=CARTESIAN_POINT('Ctrl Pts',(-22.223442254299,26.4883700572603,-41.8370777691865));
#22338=CARTESIAN_POINT('Ctrl Pts',(-22.1485068890778,26.4533639009463,-41.8416872496156));
#22339=CARTESIAN_POINT('Ctrl Pts',(-22.0750357700609,26.4155366482691,-41.8463063580885));
#22340=CARTESIAN_POINT('Ctrl Pts',(-22.0750360182176,26.4155367760347,-42.0958126606468));
#22341=CARTESIAN_POINT('Ctrl Pts',(-22.103435529259,26.4301585112938,-42.093894741434));
#22342=CARTESIAN_POINT('Ctrl Pts',(-22.1320513665457,26.4443574752129,-42.0919625094324));
#22343=CARTESIAN_POINT('Ctrl Pts',(-22.1683441668222,26.4616981131291,-42.0895105782871));
#22344=CARTESIAN_POINT('Ctrl Pts',(-22.1758278533202,26.4652384500172,-42.0890049140397));
#22345=CARTESIAN_POINT('Ctrl Pts',(-22.1871562798716,26.4705443097697,-42.0882393316427));
#22346=CARTESIAN_POINT('Ctrl Pts',(-22.1909910311223,26.4723311811528,-42.0879801536813));
#22347=CARTESIAN_POINT('Ctrl Pts',(-22.1975882309723,26.4753894686044,-42.0875342273135));
#22348=CARTESIAN_POINT('Ctrl Pts',(-22.2003489878723,26.4766645382981,-42.0873476055562));
#22349=CARTESIAN_POINT('Ctrl Pts',(-22.2060345469055,26.4792806853404,-42.0869632440204));
#22350=CARTESIAN_POINT('Ctrl Pts',(-22.2089595604265,26.480621293571,-42.086765488274));
#22351=CARTESIAN_POINT('Ctrl Pts',(-22.2159999928765,26.4838353533811,-42.0862894550494));
#22352=CARTESIAN_POINT('Ctrl Pts',(-22.2201173486565,26.4857045247541,-42.0860110303155));
#22353=CARTESIAN_POINT('Ctrl Pts',(-22.232745567747,26.4914053803569,-42.0851569726685));
#22354=CARTESIAN_POINT('Ctrl Pts',(-22.2412690976381,26.4952087360663,-42.0845803665874));
#22355=CARTESIAN_POINT('Ctrl Pts',(-22.3396071702622,26.538577726151,-42.0779259131648));
#22356=CARTESIAN_POINT('Ctrl Pts',(-22.4311585816821,26.5740539474951,-42.0717090230067));
#22357=CARTESIAN_POINT('Ctrl Pts',(-22.7526212868407,26.6820211974404,-42.0497727200448));
#22358=CARTESIAN_POINT('Ctrl Pts',(-22.9889241678932,26.7328724651795,-42.0333929910934));
#22359=CARTESIAN_POINT('Ctrl Pts',(-23.3956309345114,26.7736631907734,-42.0057942892784));
#22360=CARTESIAN_POINT('Ctrl Pts',(-23.5636999074674,26.7773439349881,-41.9945832226695));
#22361=CARTESIAN_POINT('Ctrl Pts',(-23.7388994679134,26.767485453607,-41.9835693633143));
#22362=CARTESIAN_POINT('Ctrl Pts',(-23.7464871964222,26.7670315572932,-41.9830937107103));
#22363=CARTESIAN_POINT('Ctrl Pts',(-23.7569246860861,26.7663701206404,-41.982441335042));
#22364=CARTESIAN_POINT('Ctrl Pts',(-23.7597758048045,26.7661856347775,-41.9822633284325));
#22365=CARTESIAN_POINT('Ctrl Pts',(-23.764588515374,26.7658677938415,-41.9819631891564));
#22366=CARTESIAN_POINT('Ctrl Pts',(-23.7665502304858,26.765736435184,-41.9818409436172));
#22367=CARTESIAN_POINT('Ctrl Pts',(-23.7704162493744,26.7654740082709,-41.9816002182953));
#22368=CARTESIAN_POINT('Ctrl Pts',(-23.7723205570652,26.765343043354,-41.9814817328617));
#22369=CARTESIAN_POINT('Ctrl Pts',(-23.7765221849072,26.7650503340997,-41.9812205054206));
#22370=CARTESIAN_POINT('Ctrl Pts',(-23.7788194542811,26.7648878186735,-41.9810778071544));
#22371=CARTESIAN_POINT('Ctrl Pts',(-23.7868604681311,26.7643103111411,-41.980578775518));
#22372=CARTESIAN_POINT('Ctrl Pts',(-23.7926033169498,26.7638823833276,-41.9802231696573));
#22373=CARTESIAN_POINT('Ctrl Pts',(-23.8513920459098,26.7593432620782,-41.9765907926088));
#22374=CARTESIAN_POINT('Ctrl Pts',(-23.9043333245994,26.7539341522394,-41.9733856488535));
#22375=CARTESIAN_POINT('Ctrl Pts',(-24.2452295993857,26.7105493527416,-41.953034396382));
#22376=CARTESIAN_POINT('Ctrl Pts',(-24.5270920610261,26.6351022259567,-41.9374305435732));
#22377=CARTESIAN_POINT('Ctrl Pts',(-24.9041715074109,26.4771989149843,-41.9141955019111));
#22378=CARTESIAN_POINT('Ctrl Pts',(-25.0106792040042,26.4255371264115,-41.9073561122829));
#22379=CARTESIAN_POINT('Ctrl Pts',(-25.1590189618754,26.3432128494596,-41.8972586203119));
#22380=CARTESIAN_POINT('Ctrl Pts',(-25.2033337081218,26.3172145711945,-41.8941653871063));
#22381=CARTESIAN_POINT('Ctrl Pts',(-25.2537744956299,26.2859780033777,-41.8905478244237));
#22382=CARTESIAN_POINT('Ctrl Pts',(-25.2605270684221,26.2817616283763,-41.8900615000232));
#22383=CARTESIAN_POINT('Ctrl Pts',(-25.2707875565535,26.275301912558,-41.8893193976525));
#22384=CARTESIAN_POINT('Ctrl Pts',(-25.2743068952844,26.2730766999138,-41.8890642926153));
#22385=CARTESIAN_POINT('Ctrl Pts',(-25.2803812692958,26.26921948726,-41.8886230007464));
#22386=CARTESIAN_POINT('Ctrl Pts',(-25.2829383383632,26.2675906868379,-41.8884369331774));
#22387=CARTESIAN_POINT('Ctrl Pts',(-25.2882270394536,26.2642113926472,-41.8880514696754));
#22388=CARTESIAN_POINT('Ctrl Pts',(-25.2909583332358,26.2624603778809,-41.8878520544404));
#22389=CARTESIAN_POINT('Ctrl Pts',(-25.2975726966992,26.2582058454247,-41.8873682876139));
#22390=CARTESIAN_POINT('Ctrl Pts',(-25.3014530280401,26.255698101213,-41.8870837781584));
#22391=CARTESIAN_POINT('Ctrl Pts',(-25.3158979355521,26.2463186845774,-41.8860220159166));
#22392=CARTESIAN_POINT('Ctrl Pts',(-25.3264274601538,26.2393934742905,-41.8852427567348));
#22393=CARTESIAN_POINT('Ctrl Pts',(-25.5051668519446,26.1203298000408,-41.8719233000398));
#22394=CARTESIAN_POINT('Ctrl Pts',(-25.6624657071992,25.9926928642343,-41.8587706239451));
#22395=CARTESIAN_POINT('Ctrl Pts',(-26.0176260912968,25.6443916279302,-41.8254602185934));
#22396=CARTESIAN_POINT('Ctrl Pts',(-26.199071050756,25.4095864743887,-41.8049573570652));
#22397=CARTESIAN_POINT('Ctrl Pts',(-26.3501372397187,25.1461323551671,-41.7858036819124));
#22398=CARTESIAN_POINT('Ctrl Pts',(-26.3542480852093,25.1388984106195,-41.785280593873));
#22399=CARTESIAN_POINT('Ctrl Pts',(-26.3613286502356,25.1263254803698,-41.7843764573285));
#22400=CARTESIAN_POINT('Ctrl Pts',(-26.3643112662188,25.1209938610937,-41.78399460873));
#22401=CARTESIAN_POINT('Ctrl Pts',(-26.3685518275275,25.113362736088,-41.7834503252597));
#22402=CARTESIAN_POINT('Ctrl Pts',(-26.3698221326855,25.1110701691067,-41.783287099844));
#22403=CARTESIAN_POINT('Ctrl Pts',(-26.3720120992346,25.1071064567436,-41.7830053968559));
#22404=CARTESIAN_POINT('Ctrl Pts',(-26.3729330749773,25.1054360422781,-41.7828868341231));
#22405=CARTESIAN_POINT('Ctrl Pts',(-26.3747022190419,25.1022205187516,-41.782658900918));
#22406=CARTESIAN_POINT('Ctrl Pts',(-26.3755506011701,25.1006755345753,-41.7825495164983));
#22407=CARTESIAN_POINT('Ctrl Pts',(-26.377556678072,25.0970151642473,-41.7822906743768));
#22408=CARTESIAN_POINT('Ctrl Pts',(-26.3787132688805,25.0948991695606,-41.7821412880803));
#22409=CARTESIAN_POINT('Ctrl Pts',(-26.3821537440466,25.0885879638409,-41.7816964516389));
#22410=CARTESIAN_POINT('Ctrl Pts',(-26.3844306906493,25.0843889475049,-41.7814014448405));
#22411=CARTESIAN_POINT('Ctrl Pts',(-26.4054171084777,25.0454807974827,-41.7786765895041));
#22412=CARTESIAN_POINT('Ctrl Pts',(-26.4234984646403,25.0104341920233,-41.7762860155738));
#22413=CARTESIAN_POINT('Ctrl Pts',(-26.5134741122263,24.8278899737184,-41.7641152868074));
#22414=CARTESIAN_POINT('Ctrl Pts',(-26.5746787837715,24.675373913756,-41.7548728277085));
#22415=CARTESIAN_POINT('Ctrl Pts',(-26.6734921586445,24.3617970430938,-41.7364715947313));
#22416=CARTESIAN_POINT('Ctrl Pts',(-26.7108705776233,24.2011912606758,-41.7273353721418));
#22417=CARTESIAN_POINT('Ctrl Pts',(-26.755251966279,23.9115902208762,-41.7105552290491));
#22418=CARTESIAN_POINT('Ctrl Pts',(-26.7670956244258,23.7837067609564,-41.7030451021251));
#22419=CARTESIAN_POINT('Ctrl Pts',(-26.7717319542035,23.6417713003537,-41.694456879179));
#22420=CARTESIAN_POINT('Ctrl Pts',(-26.7720919790689,23.6280723301105,-41.6936254608581));
#22421=CARTESIAN_POINT('Ctrl Pts',(-26.7725694938201,23.6040762696143,-41.6921644978409));
#22422=CARTESIAN_POINT('Ctrl Pts',(-26.7727250216825,23.5937800697245,-41.6915361491234));
#22423=CARTESIAN_POINT('Ctrl Pts',(-26.7728785049626,23.5788959558208,-41.6906256165344));
#22424=CARTESIAN_POINT('Ctrl Pts',(-26.7729160143181,23.5743084404711,-41.6903446747312));
#22425=CARTESIAN_POINT('Ctrl Pts',(-26.7729643056428,23.5663145403464,-41.6898545932175));
#22426=CARTESIAN_POINT('Ctrl Pts',(-26.7729794826565,23.5629081812731,-41.6896455917956));
#22427=CARTESIAN_POINT('Ctrl Pts',(-26.7729983462488,23.556335521612,-41.6892419914677));
#22428=CARTESIAN_POINT('Ctrl Pts',(-26.7730027672509,23.5531692255332,-41.689047415855));
#22429=CARTESIAN_POINT('Ctrl Pts',(-26.7730021219335,23.5448369336704,-41.6885349914323));
#22430=CARTESIAN_POINT('Ctrl Pts',(-26.7729893003427,23.5396709631253,-41.6882168994899));
#22431=CARTESIAN_POINT('Ctrl Pts',(-26.7728965858869,23.5206969884614,-41.687047132472));
#22432=CARTESIAN_POINT('Ctrl Pts',(-26.7727403721608,23.5068896597323,-41.6861930650199));
#22433=CARTESIAN_POINT('Ctrl Pts',(-26.7692984497465,23.3128896303722,-41.6741522272646));
#22434=CARTESIAN_POINT('Ctrl Pts',(-26.750993015845,23.1333135249129,-41.6624845816784));
#22435=CARTESIAN_POINT('Ctrl Pts',(-26.6603131905545,22.6497749137069,-41.6297077263732));
#22436=CARTESIAN_POINT('Ctrl Pts',(-26.558677767537,22.3532920686262,-41.6079762439181));
#22437=CARTESIAN_POINT('Ctrl Pts',(-26.408750229919,22.0618430067611,-41.587238713448));
#22438=CARTESIAN_POINT('Ctrl Pts',(-26.4013480512056,22.0477125594052,-41.5862354230954));
#22439=CARTESIAN_POINT('Ctrl Pts',(-26.3921631841033,22.0304913271692,-41.5850158436686));
#22440=CARTESIAN_POINT('Ctrl Pts',(-26.3904800577144,22.0273481105974,-41.5847933759045));
#22441=CARTESIAN_POINT('Ctrl Pts',(-26.3876937039386,22.022165317757,-41.5844267752399));
#22442=CARTESIAN_POINT('Ctrl Pts',(-26.3865934915174,22.0201241387003,-41.5842824511349));
#22443=CARTESIAN_POINT('Ctrl Pts',(-26.3846036755462,22.0164420349798,-41.5840222089095));
#22444=CARTESIAN_POINT('Ctrl Pts',(-26.3837148517011,22.0148006999372,-41.583906241351));
#22445=CARTESIAN_POINT('Ctrl Pts',(-26.3817981199284,22.011268523962,-41.5836567598176));
#22446=CARTESIAN_POINT('Ctrl Pts',(-26.3807697466107,22.0093779454833,-41.5835232766579));
#22447=CARTESIAN_POINT('Ctrl Pts',(-26.3779422157224,22.0041921484269,-41.5831572713244));
#22448=CARTESIAN_POINT('Ctrl Pts',(-26.3761391853438,22.0008990281535,-41.5829249976214));
#22449=CARTESIAN_POINT('Ctrl Pts',(-26.3666618003489,21.9836607674687,-41.5817098752807));
#22450=CARTESIAN_POINT('Ctrl Pts',(-26.3588897891211,21.9697691546514,-41.5807332129175));
#22451=CARTESIAN_POINT('Ctrl Pts',(-26.2607467820825,21.7973597658276,-41.5686365518939));
#22452=CARTESIAN_POINT('Ctrl Pts',(-26.1571593423471,21.646711271517,-41.5583192103698));
#22453=CARTESIAN_POINT('Ctrl Pts',(-25.9019960897186,21.3358287241443,-41.5357884006329));
#22454=CARTESIAN_POINT('Ctrl Pts',(-25.7456488990525,21.1807381398713,-41.5236472019806));
#22455=CARTESIAN_POINT('Ctrl Pts',(-25.5009540886434,20.9831771098063,-41.5053098041991));
#22456=CARTESIAN_POINT('Ctrl Pts',(-25.4245726722362,20.9268894038697,-41.4996724978878));
#22457=CARTESIAN_POINT('Ctrl Pts',(-25.3372882867543,20.8683266420224,-41.4932742181114));
#22458=CARTESIAN_POINT('Ctrl Pts',(-25.3287233313674,20.8626393008863,-41.4926468479523));
#22459=CARTESIAN_POINT('Ctrl Pts',(-25.3166830253648,20.8547269985375,-41.4917655211818));
#22460=CARTESIAN_POINT('Ctrl Pts',(-25.3132303292048,20.8524675376489,-41.4915128602624));
#22461=CARTESIAN_POINT('Ctrl Pts',(-25.3069016403312,20.8483433511008,-41.4910498634251));
#22462=CARTESIAN_POINT('Ctrl Pts',(-25.3040269896045,20.846476568029,-41.4908396048734));
#22463=CARTESIAN_POINT('Ctrl Pts',(-25.2982090228235,20.8427115931514,-41.4904141563898));
#22464=CARTESIAN_POINT('Ctrl Pts',(-25.2952655805354,20.8408136067531,-41.4901989592079));
#22465=CARTESIAN_POINT('Ctrl Pts',(-25.2880365735255,20.8361688746953,-41.4896705530323));
#22466=CARTESIAN_POINT('Ctrl Pts',(-25.2837475944094,20.8334274839043,-41.4893571450565));
#22467=CARTESIAN_POINT('Ctrl Pts',(-25.2684774740081,20.823718147515,-41.4882416407818));
#22468=CARTESIAN_POINT('Ctrl Pts',(-25.2574607822162,20.8168065962708,-41.4874374547109));
#22469=CARTESIAN_POINT('Ctrl Pts',(-25.1069945473078,20.7236729214604,-41.476461179445));
#22470=CARTESIAN_POINT('Ctrl Pts',(-24.9612283174509,20.6481618870958,-41.4658937522375));
#22471=CARTESIAN_POINT('Ctrl Pts',(-24.5360806544897,20.4675468710269,-41.4352680821289));
#22472=CARTESIAN_POINT('Ctrl Pts',(-24.2469792010347,20.3896372875369,-41.414548609095));
#22473=CARTESIAN_POINT('Ctrl Pts',(-23.945568945234,20.3518348135755,-41.3949246539071));
#22474=CARTESIAN_POINT('Ctrl Pts',(-23.9398322955239,20.3511309999318,-41.3945519317201));
#22475=CARTESIAN_POINT('Ctrl Pts',(-23.895416897762,20.3458030396867,-41.3916723187784));
#22476=CARTESIAN_POINT('Ctrl Pts',(-23.8566569034844,20.3418648233006,-41.3891954182124));
#22477=CARTESIAN_POINT('Ctrl Pts',(-23.8130892639357,20.3382349300513,-41.3864587722502));
#22478=CARTESIAN_POINT('Ctrl Pts',(-23.8083446908445,20.3378502126881,-41.3861613788571));
#22479=CARTESIAN_POINT('Ctrl Pts',(-23.8011994424737,20.3372867669619,-41.3857144769748));
#22480=CARTESIAN_POINT('Ctrl Pts',(-23.7987994173122,20.3371002161146,-41.3855645309411));
#22481=CARTESIAN_POINT('Ctrl Pts',(-23.7946428199316,20.3367818141671,-41.3853051269828));
#22482=CARTESIAN_POINT('Ctrl Pts',(-23.7928863489686,20.3366487141495,-41.3851955983429));
#22483=CARTESIAN_POINT('Ctrl Pts',(-23.7892267996733,20.3363744220945,-41.3849675852566));
#22484=CARTESIAN_POINT('Ctrl Pts',(-23.7873237070643,20.336233480421,-41.3848491156088));
#22485=CARTESIAN_POINT('Ctrl Pts',(-23.7828547191302,20.3359065012697,-41.3845711606338));
#22486=CARTESIAN_POINT('Ctrl Pts',(-23.7802887168432,20.3357218451805,-41.3844117537296));
#22487=CARTESIAN_POINT('Ctrl Pts',(-23.7718611315177,20.3351255173343,-41.3838888229272));
#22488=CARTESIAN_POINT('Ctrl Pts',(-23.765998599524,20.3347268008863,-41.3835260275347));
#22489=CARTESIAN_POINT('Ctrl Pts',(-23.7521538944338,20.3338232427365,-41.3826714960594));
#22490=CARTESIAN_POINT('Ctrl Pts',(-23.7441708246661,20.3333320741879,-41.3821805099766));
#22491=CARTESIAN_POINT('Ctrl Pts',(-23.4655252720813,20.31722907153,-41.365101337049));
#22492=CARTESIAN_POINT('Ctrl Pts',(-23.1939201396167,20.3358004696038,-41.350319306804));
#22493=CARTESIAN_POINT('Ctrl Pts',(-22.7803686303355,20.4172063535288,-41.326696484936));
#22494=CARTESIAN_POINT('Ctrl Pts',(-22.6351461133296,20.4565049949696,-41.3181880925579));
#22495=CARTESIAN_POINT('Ctrl Pts',(-22.4793226777967,20.5106073610616,-41.3085104758978));
#22496=CARTESIAN_POINT('Ctrl Pts',(-22.4654735885125,20.5155222059206,-41.3076455876232));
#22497=CARTESIAN_POINT('Ctrl Pts',(-22.4466104674205,20.5223620791715,-41.3064607775932));
#22498=CARTESIAN_POINT('Ctrl Pts',(-22.4415667895831,20.5242052215435,-41.3061433138948));
#22499=CARTESIAN_POINT('Ctrl Pts',(-22.4327959905675,20.5274352603334,-41.3055900794697));
#22500=CARTESIAN_POINT('Ctrl Pts',(-22.4290667769955,20.5288164690567,-41.3053544818526));
#22501=CARTESIAN_POINT('Ctrl Pts',(-22.4133112736714,20.5346851046373,-41.3043575263415));
#22502=CARTESIAN_POINT('Ctrl Pts',(-22.4013094091478,20.539237416211,-41.3035941857172));
#22503=CARTESIAN_POINT('Ctrl Pts',(-22.3879232405241,20.54440648237,-41.3027383035881));
#22504=CARTESIAN_POINT('Ctrl Pts',(-22.3865116834171,20.5449526978357,-41.3026479956832));
#22505=CARTESIAN_POINT('Ctrl Pts',(-22.3433282057686,20.5616979419278,-41.2998835033141));
#22506=CARTESIAN_POINT('Ctrl Pts',(-22.3018999252261,20.5787646337453,-41.2971819737084));
#22507=CARTESIAN_POINT('Ctrl Pts',(-22.2540071130783,20.599672757732,-41.2939962608039));
#22508=CARTESIAN_POINT('Ctrl Pts',(-22.247182264298,20.6026804690377,-41.2935407897615));
#22509=CARTESIAN_POINT('Ctrl Pts',(-22.2363108311614,20.6075166468755,-41.2928128432412));
#22510=CARTESIAN_POINT('Ctrl Pts',(-22.2322574505955,20.6093298455147,-41.2925408925523));
#22511=CARTESIAN_POINT('Ctrl Pts',(-22.2251116970178,20.6125440954311,-41.2920605119716));
#22512=CARTESIAN_POINT('Ctrl Pts',(-22.2220177597086,20.6139416696488,-41.2918522020798));
#22513=CARTESIAN_POINT('Ctrl Pts',(-22.2156271802226,20.616840549802,-41.2914212766334));
#22514=CARTESIAN_POINT('Ctrl Pts',(-22.212330850669,20.6183425297379,-41.2911986380487));
#22515=CARTESIAN_POINT('Ctrl Pts',(-22.2039019268377,20.6222003626003,-41.2906284046718));
#22516=CARTESIAN_POINT('Ctrl Pts',(-22.1987729956677,20.62456414788,-41.2902805360312));
#22517=CARTESIAN_POINT('Ctrl Pts',(-22.1782399960408,20.634092764969,-41.2888843118443));
#22518=CARTESIAN_POINT('Ctrl Pts',(-22.1628866942515,20.6413657689669,-41.2878322121485));
#22519=CARTESIAN_POINT('Ctrl Pts',(-21.9669040196301,20.736109133789,-41.274296651749));
#22520=CARTESIAN_POINT('Ctrl Pts',(-21.7948053974029,20.840128202668,-41.2612126617682));
#22521=CARTESIAN_POINT('Ctrl Pts',(-21.4588321651595,21.0886886834058,-41.2332023353009));
#22522=CARTESIAN_POINT('Ctrl Pts',(-21.2976670178716,21.2352592402422,-41.2182828203036));
#22523=CARTESIAN_POINT('Ctrl Pts',(-21.1442591332912,21.4060826185995,-41.2031511624606));
#22524=CARTESIAN_POINT('Ctrl Pts',(-21.1360931729729,21.4152809985134,-41.2023427174215));
#22525=CARTESIAN_POINT('Ctrl Pts',(-21.116767070109,21.4373031580937,-41.2004226858236));
#22526=CARTESIAN_POINT('Ctrl Pts',(-21.1056552224726,21.4501690655643,-41.1993133157525));
#22527=CARTESIAN_POINT('Ctrl Pts',(-21.0601424422341,21.5037170015254,-41.1947489149165));
#22528=CARTESIAN_POINT('Ctrl Pts',(-21.0266487222162,21.5451638607388,-41.1913405167319));
#22529=CARTESIAN_POINT('Ctrl Pts',(-20.9906872093283,21.5919940939217,-41.1876423650181));
#22530=CARTESIAN_POINT('Ctrl Pts',(-20.9871908378303,21.5965725417172,-41.1872823913285));
#22531=CARTESIAN_POINT('Ctrl Pts',(-20.9823136927706,21.602994719438,-41.1867796981482));
#22532=CARTESIAN_POINT('Ctrl Pts',(-20.9809226175676,21.6048305568257,-41.1866362541777));
#22533=CARTESIAN_POINT('Ctrl Pts',(-20.9783822909749,21.6081905678924,-41.1863741873715));
#22534=CARTESIAN_POINT('Ctrl Pts',(-20.9772324240969,21.6097142732977,-41.1862555207826));
#22535=CARTESIAN_POINT('Ctrl Pts',(-20.974901042143,21.6128093369461,-41.1860148350656));
#22536=CARTESIAN_POINT('Ctrl Pts',(-20.9737196107308,21.6143807552455,-41.1858928219053));
#22537=CARTESIAN_POINT('Ctrl Pts',(-20.9708251933189,21.6182379542092,-41.1855937849705));
#22538=CARTESIAN_POINT('Ctrl Pts',(-20.9691138027421,21.6205249385798,-41.1854168743607));
#22539=CARTESIAN_POINT('Ctrl Pts',(-20.9628961227953,21.628856886901,-41.1847737674746));
#22540=CARTESIAN_POINT('Ctrl Pts',(-20.9584079644878,21.6349154457887,-41.184308838526));
#22541=CARTESIAN_POINT('Ctrl Pts',(-20.8571208722336,21.7726507252989,-41.1737989198239));
#22542=CARTESIAN_POINT('Ctrl Pts',(-20.77044005158,21.9115074401729,-41.1644338798672));
#22543=CARTESIAN_POINT('Ctrl Pts',(-20.6130449901211,22.2123702043084,-41.145309559751));
#22544=CARTESIAN_POINT('Ctrl Pts',(-20.544352601722,22.3748023577325,-41.1355988020526));
#22545=CARTESIAN_POINT('Ctrl Pts',(-20.4684540834213,22.6052322037622,-41.1218151630692));
#22546=CARTESIAN_POINT('Ctrl Pts',(-20.4496006420701,22.6690588618789,-41.1179987580406));
#22547=CARTESIAN_POINT('Ctrl Pts',(-20.407213325427,22.8308340946823,-41.1082718354867));
#22548=CARTESIAN_POINT('Ctrl Pts',(-20.3862718482243,22.929381060805,-41.1022963742722));
#22549=CARTESIAN_POINT('Ctrl Pts',(-20.3684585423071,23.0380096054786,-41.0955963437874));
#22550=CARTESIAN_POINT('Ctrl Pts',(-20.3669789634239,23.0472861382102,-41.0950233108014));
#22551=CARTESIAN_POINT('Ctrl Pts',(-20.3648450352697,23.0610519343051,-41.094171629853));
#22552=CARTESIAN_POINT('Ctrl Pts',(-20.3641595643392,23.0655363819819,-41.0938939700616));
#22553=CARTESIAN_POINT('Ctrl Pts',(-20.3630035087695,23.073207872309,-41.093418616612));
#22554=CARTESIAN_POINT('Ctrl Pts',(-20.3625282286861,23.0763942099552,-41.093221072174));
#22555=CARTESIAN_POINT('Ctrl Pts',(-20.361613823296,23.0825881346818,-41.0928368546349));
#22556=CARTESIAN_POINT('Ctrl Pts',(-20.3611741734397,23.0855956413501,-41.0926501984311));
#22557=CARTESIAN_POINT('Ctrl Pts',(-20.360134257406,23.0927803815169,-41.0922040562289));
#22558=CARTESIAN_POINT('Ctrl Pts',(-20.3595379414966,23.0969581728459,-41.091944445281));
#22559=CARTESIAN_POINT('Ctrl Pts',(-20.3578118742822,23.1092231779174,-41.091181731827));
#22560=CARTESIAN_POINT('Ctrl Pts',(-20.3567046581239,23.1173134837474,-41.0906779160879));
#22561=CARTESIAN_POINT('Ctrl Pts',(-20.3479972685934,23.1827887965849,-41.0865946353172));
#22562=CARTESIAN_POINT('Ctrl Pts',(-20.3419141287191,23.2403616559554,-41.0829674321972));
#22563=CARTESIAN_POINT('Ctrl Pts',(-20.3260890129233,23.4419729159951,-41.0701255465557));
#22564=CARTESIAN_POINT('Ctrl Pts',(-20.3244759724534,23.5864592719757,-41.060664015175));
#22565=CARTESIAN_POINT('Ctrl Pts',(-20.3421994921574,23.9027616759515,-41.0394827368443));
#22566=CARTESIAN_POINT('Ctrl Pts',(-20.3656586222808,24.0739178112076,-41.0277107909783));
#22567=CARTESIAN_POINT('Ctrl Pts',(-20.419335767569,24.3180283047237,-41.0109317457834));
#22568=CARTESIAN_POINT('Ctrl Pts',(-20.4386974460152,24.3930727115073,-41.0057784802));
#22569=CARTESIAN_POINT('Ctrl Pts',(-20.4625734306141,24.4735057780515,-41.0003077128355));
#22570=CARTESIAN_POINT('Ctrl Pts',(-20.4644189794074,24.4796556073032,-40.9998897642706));
#22571=CARTESIAN_POINT('Ctrl Pts',(-20.4819635472328,24.5374901057151,-40.9959627361969));
#22572=CARTESIAN_POINT('Ctrl Pts',(-20.4989424691347,24.5887818219202,-40.9925059319402));
#22573=CARTESIAN_POINT('Ctrl Pts',(-20.5189639438809,24.6445258820784,-40.9887960581018));
#22574=CARTESIAN_POINT('Ctrl Pts',(-20.5207356915099,24.6494214831798,-40.988470648904));
#22575=CARTESIAN_POINT('Ctrl Pts',(-20.5233821793103,24.6566791114033,-40.9879888569771));
#22576=CARTESIAN_POINT('Ctrl Pts',(-20.5242478264575,24.6590444104607,-40.9878319364289));
#22577=CARTESIAN_POINT('Ctrl Pts',(-20.5257337623024,24.6630898889978,-40.9875637187772));
#22578=CARTESIAN_POINT('Ctrl Pts',(-20.5263526785113,24.6647705657205,-40.9874523393662));
#22579=CARTESIAN_POINT('Ctrl Pts',(-20.5275620598334,24.6680462364788,-40.9872353584309));
#22580=CARTESIAN_POINT('Ctrl Pts',(-20.5281523849009,24.6696412746679,-40.9871297491306));
#22581=CARTESIAN_POINT('Ctrl Pts',(-20.5295817197724,24.6734939167906,-40.9868747718376));
#22582=CARTESIAN_POINT('Ctrl Pts',(-20.5304220000345,24.6757510538329,-40.98672548065));
#22583=CARTESIAN_POINT('Ctrl Pts',(-20.5329691598665,24.6825697743285,-40.986274749046));
#22584=CARTESIAN_POINT('Ctrl Pts',(-20.5346838605444,24.6871284590463,-40.9859737774661));
#22585=CARTESIAN_POINT('Ctrl Pts',(-20.5517009973861,24.7320606546993,-40.9830107417448));
#22586=CARTESIAN_POINT('Ctrl Pts',(-20.5678038982715,24.7721290975503,-40.9803960175176));
#22587=CARTESIAN_POINT('Ctrl Pts',(-20.6175619192247,24.8890903030063,-40.972811274157));
#22588=CARTESIAN_POINT('Ctrl Pts',(-20.6534223947086,24.9650098056607,-40.9679494360663));
#22589=CARTESIAN_POINT('Ctrl Pts',(-20.7613381090476,25.1721201853498,-40.9546304121617));
#22590=CARTESIAN_POINT('Ctrl Pts',(-20.8396240128365,25.2998224030676,-40.9463463719579));
#22591=CARTESIAN_POINT('Ctrl Pts',(-20.9924913106465,25.5141491800164,-40.9315988283507));
#22592=CARTESIAN_POINT('Ctrl Pts',(-21.0633262226755,25.6031109674793,-40.925188582805));
#22593=CARTESIAN_POINT('Ctrl Pts',(-21.2180228873768,25.7776091955496,-40.9117283524356));
#22594=CARTESIAN_POINT('Ctrl Pts',(-21.302246410084,25.8625838599812,-40.9046723818301));
#22595=CARTESIAN_POINT('Ctrl Pts',(-21.3989027274113,25.9498202505893,-40.8967499969482));
#22596=CARTESIAN_POINT('Ctrl Pts',(-21.4068522424466,25.9569237626098,-40.8960996742361));
#22597=CARTESIAN_POINT('Ctrl Pts',(-21.4180584652827,25.9668378350808,-40.8951846240528));
#22598=CARTESIAN_POINT('Ctrl Pts',(-21.4212858382461,25.9696815724559,-40.8949212867044));
#22599=CARTESIAN_POINT('Ctrl Pts',(-21.4268935991946,25.9746028340699,-40.8944640556367));
#22600=CARTESIAN_POINT('Ctrl Pts',(-21.4292713728239,25.9766833401997,-40.8942702865844));
#22601=CARTESIAN_POINT('Ctrl Pts',(-21.4342226063569,25.9810027354216,-40.8938670148815));
#22602=CARTESIAN_POINT('Ctrl Pts',(-21.4367965676254,25.9832410408421,-40.893657488353));
#22603=CARTESIAN_POINT('Ctrl Pts',(-21.4428613753187,25.9884980844153,-40.8931640762106));
#22604=CARTESIAN_POINT('Ctrl Pts',(-21.4463551552772,25.9915134129778,-40.8928800497575));
#22605=CARTESIAN_POINT('Ctrl Pts',(-21.4575313264692,26.0011172663696,-40.8919721618911));
#22606=CARTESIAN_POINT('Ctrl Pts',(-21.4652382245715,26.0076770627464,-40.8913471164866));
#22607=CARTESIAN_POINT('Ctrl Pts',(-21.4833625541543,26.022957113248,-40.8898795049966));
#22608=CARTESIAN_POINT('Ctrl Pts',(-21.493804420512,26.0316479624535,-40.8890357473646));
#22609=CARTESIAN_POINT('Ctrl Pts',(-21.5297999024927,26.0612240389298,-40.8861329518472));
#22610=CARTESIAN_POINT('Ctrl Pts',(-21.5556185344741,26.0817820740018,-40.8840608032956));
#22611=CARTESIAN_POINT('Ctrl Pts',(-21.671582268812,26.1712425756115,-40.8747947891684));
#22612=CARTESIAN_POINT('Ctrl Pts',(-21.7650044344306,26.235745991501,-40.8674337730804));
#22613=CARTESIAN_POINT('Ctrl Pts',(-21.9312387053325,26.3380100516388,-40.8545249368777));
#22614=CARTESIAN_POINT('Ctrl Pts',(-22.002428899923,26.3781543765597,-40.8490530641783));
#22615=CARTESIAN_POINT('Ctrl Pts',(-22.0750362323924,26.4155368863044,-40.843547806833));
#22616=CARTESIAN_POINT('Origin',(-23.5502525316942,23.5502525316942,-77.3107734492734));
#22617=CARTESIAN_POINT('',(-22.0750358008163,26.4155366641038,-39.3444748119239));
#22618=CARTESIAN_POINT('',(-22.0750360153868,26.4155367745772,-39.5898217886697));
#22619=CARTESIAN_POINT('',(-22.0750360153461,26.4155367745563,-77.3107734492734));
#22620=CARTESIAN_POINT('Ctrl Pts',(-22.0750358008163,26.4155366641038,-39.3444748119239));
#22621=CARTESIAN_POINT('Ctrl Pts',(-22.0193043812446,26.3868428526741,-39.3486299213752));
#22622=CARTESIAN_POINT('Ctrl Pts',(-21.964396741262,26.3565161533716,-39.3528254761847));
#22623=CARTESIAN_POINT('Ctrl Pts',(-21.8092759268395,26.2648266674662,-39.3649499025387));
#22624=CARTESIAN_POINT('Ctrl Pts',(-21.7115103339792,26.1995805190266,-39.3729312042456));
#22625=CARTESIAN_POINT('Ctrl Pts',(-21.488195273045,26.032219219904,-39.3917525180478));
#22626=CARTESIAN_POINT('Ctrl Pts',(-21.3663191215635,25.9256868952839,-39.4025170211158));
#22627=CARTESIAN_POINT('Ctrl Pts',(-21.2486247535757,25.806059475927,-39.4130327228697));
#22628=CARTESIAN_POINT('Ctrl Pts',(-21.2443233526389,25.8016623169899,-39.4134172089316));
#22629=CARTESIAN_POINT('Ctrl Pts',(-21.2382020459838,25.7953687918453,-39.4139645715471));
#22630=CARTESIAN_POINT('Ctrl Pts',(-21.2363718641137,25.7934825079525,-39.4141282509411));
#22631=CARTESIAN_POINT('Ctrl Pts',(-21.2332165365611,25.7902224874891,-39.4144104839769));
#22632=CARTESIAN_POINT('Ctrl Pts',(-21.2318903019685,25.7888498106751,-39.4145291236578));
#22633=CARTESIAN_POINT('Ctrl Pts',(-21.229342977327,25.7862085918987,-39.4147570201795));
#22634=CARTESIAN_POINT('Ctrl Pts',(-21.2281217096894,25.7849402298415,-39.4148662912695));
#22635=CARTESIAN_POINT('Ctrl Pts',(-21.2252350719002,25.7819373562412,-39.4151245951554));
#22636=CARTESIAN_POINT('Ctrl Pts',(-21.2235705994816,25.7802019775032,-39.4152735572443));
#22637=CARTESIAN_POINT('Ctrl Pts',(-21.2186240262652,25.7750331132523,-39.415716318974));
#22638=CARTESIAN_POINT('Ctrl Pts',(-21.2153475536939,25.7715942136061,-39.4160096810171));
#22639=CARTESIAN_POINT('Ctrl Pts',(-21.1854690283587,25.7400953507706,-39.4186858391908));
#22640=CARTESIAN_POINT('Ctrl Pts',(-21.1593649343925,25.711564497402,-39.4210308816463));
#22641=CARTESIAN_POINT('Ctrl Pts',(-21.1316739996977,25.6801834158288,-39.4235351543124));
#22642=CARTESIAN_POINT('Ctrl Pts',(-21.1295722750046,25.6777944893671,-39.4237253334619));
#22643=CARTESIAN_POINT('Ctrl Pts',(-21.1261770698113,25.6739237836257,-39.4240327359742));
#22644=CARTESIAN_POINT('Ctrl Pts',(-21.1248814070281,25.6724439318412,-39.4241500880913));
#22645=CARTESIAN_POINT('Ctrl Pts',(-21.1179755339058,25.6645417477779,-39.424775807182));
#22646=CARTESIAN_POINT('Ctrl Pts',(-21.1123894228983,25.6580982919244,-39.4252827691741));
#22647=CARTESIAN_POINT('Ctrl Pts',(-20.9810475646201,25.5053778040405,-39.4372241754453));
#22648=CARTESIAN_POINT('Ctrl Pts',(-20.868637098761,25.34810803634,-39.4479312832544));
#22649=CARTESIAN_POINT('Ctrl Pts',(-20.6946046782655,25.051633148377,-39.4671429162764));
#22650=CARTESIAN_POINT('Ctrl Pts',(-20.6274775815421,24.9163604260466,-39.4755924773899));
#22651=CARTESIAN_POINT('Ctrl Pts',(-20.5401133729809,24.7041049465896,-39.4888726865368));
#22652=CARTESIAN_POINT('Ctrl Pts',(-20.5128326893871,24.6302490213189,-39.4934952468059));
#22653=CARTESIAN_POINT('Ctrl Pts',(-20.4801244786856,24.5306175908253,-39.4997723622537));
#22654=CARTESIAN_POINT('Ctrl Pts',(-20.472267921572,24.5056647934783,-39.5013477594362));
#22655=CARTESIAN_POINT('Ctrl Pts',(-20.4614172952391,24.4696789970701,-39.5036255687295));
#22656=CARTESIAN_POINT('Ctrl Pts',(-20.4581766566244,24.4587209795667,-39.5043199545695));
#22657=CARTESIAN_POINT('Ctrl Pts',(-20.452536819609,24.4392704200904,-39.5055539605528));
#22658=CARTESIAN_POINT('Ctrl Pts',(-20.4501140842354,24.4307847814935,-39.5060928092514));
#22659=CARTESIAN_POINT('Ctrl Pts',(-20.4465661128762,24.4181618348877,-39.5068951490833));
#22660=CARTESIAN_POINT('Ctrl Pts',(-20.4454142173505,24.4140320095859,-39.5071577707357));
#22661=CARTESIAN_POINT('Ctrl Pts',(-20.4434107258247,24.4067932176488,-39.5076183137289));
#22662=CARTESIAN_POINT('Ctrl Pts',(-20.4425555449002,24.4036852423064,-39.5078161180339));
#22663=CARTESIAN_POINT('Ctrl Pts',(-20.4408609343673,24.3974902147152,-39.508210536894));
#22664=CARTESIAN_POINT('Ctrl Pts',(-20.4400214355155,24.3944031848937,-39.5084071489515));
#22665=CARTESIAN_POINT('Ctrl Pts',(-20.4380242926073,24.3870158097381,-39.5088778188505));
#22666=CARTESIAN_POINT('Ctrl Pts',(-20.4368709652479,24.3827143128325,-39.5091520167178));
#22667=CARTESIAN_POINT('Ctrl Pts',(-20.4327555908068,24.3672372640745,-39.5101391018188));
#22668=CARTESIAN_POINT('Ctrl Pts',(-20.4298447974355,24.356048284828,-39.5108536504688));
#22669=CARTESIAN_POINT('Ctrl Pts',(-20.382191737911,24.1687409501885,-39.522831920012));
#22670=CARTESIAN_POINT('Ctrl Pts',(-20.3523712358977,23.9891964742879,-39.5345858927473));
#22671=CARTESIAN_POINT('Ctrl Pts',(-20.3273887690622,23.6779774345387,-39.5553802070713));
#22672=CARTESIAN_POINT('Ctrl Pts',(-20.3248606230775,23.5473228731805,-39.5642274684996));
#22673=CARTESIAN_POINT('Ctrl Pts',(-20.3378158785744,23.2345415298741,-39.5854097861483));
#22674=CARTESIAN_POINT('Ctrl Pts',(-20.3608440264336,23.0531484861227,-39.5977025204903));
#22675=CARTESIAN_POINT('Ctrl Pts',(-20.4024449319433,22.8591100853893,-39.6102548582153));
#22676=CARTESIAN_POINT('Ctrl Pts',(-20.4058945269916,22.8435819370975,-39.6112549994919));
#22677=CARTESIAN_POINT('Ctrl Pts',(-20.4103001093683,22.8244216727545,-39.6124831234204));
#22678=CARTESIAN_POINT('Ctrl Pts',(-20.4111475807279,22.820765206636,-39.6127172247817));
#22679=CARTESIAN_POINT('Ctrl Pts',(-20.412490969693,22.8150147653623,-39.6130849585368));
#22680=CARTESIAN_POINT('Ctrl Pts',(-20.4129825965446,22.8129198068781,-39.6132188382784));
#22681=CARTESIAN_POINT('Ctrl Pts',(-20.4139045632166,22.8090086671001,-39.6134686115778));
#22682=CARTESIAN_POINT('Ctrl Pts',(-20.4143343796771,22.807192379318,-39.6135845343494));
#22683=CARTESIAN_POINT('Ctrl Pts',(-20.4153017471695,22.8031203356083,-39.6138442744832));
#22684=CARTESIAN_POINT('Ctrl Pts',(-20.4158401539492,22.8008647908342,-39.6139880412715));
#22685=CARTESIAN_POINT('Ctrl Pts',(-20.4172127016631,22.7951421407762,-39.6143525348038));
#22686=CARTESIAN_POINT('Ctrl Pts',(-20.4180501660424,22.7916758250126,-39.6145730692289));
#22687=CARTESIAN_POINT('Ctrl Pts',(-20.4226672552121,22.7727034177944,-39.6157788220425));
#22688=CARTESIAN_POINT('Ctrl Pts',(-20.4265563601074,22.7572238193735,-39.6167577938703));
#22689=CARTESIAN_POINT('Ctrl Pts',(-20.5035058299617,22.4602976033242,-39.6354549986704));
#22690=CARTESIAN_POINT('Ctrl Pts',(-20.6142228998984,22.1899360936725,-39.6511598327141));
#22691=CARTESIAN_POINT('Ctrl Pts',(-20.861312833267,21.7622510921412,-39.6789569481323));
#22692=CARTESIAN_POINT('Ctrl Pts',(-20.9792582517433,21.5964574043754,-39.6906304146278));
#22693=CARTESIAN_POINT('Ctrl Pts',(-21.117490810232,21.4365216070641,-39.7034800319533));
#22694=CARTESIAN_POINT('Ctrl Pts',(-21.1230042007556,21.4301927322972,-39.7039912523034));
#22695=CARTESIAN_POINT('Ctrl Pts',(-21.1318310673715,21.4201398515844,-39.7048077050071));
#22696=CARTESIAN_POINT('Ctrl Pts',(-21.1351285936242,21.4164018404831,-39.7051122724734));
#22697=CARTESIAN_POINT('Ctrl Pts',(-21.1414142525737,21.4093097752986,-39.7056920019537));
#22698=CARTESIAN_POINT('Ctrl Pts',(-21.1444007542759,21.4059542861396,-39.7059670952487));
#22699=CARTESIAN_POINT('Ctrl Pts',(-21.1496229120234,21.4001115651206,-39.7064475102501));
#22700=CARTESIAN_POINT('Ctrl Pts',(-21.1518554475422,21.3976215429798,-39.7066527002497));
#22701=CARTESIAN_POINT('Ctrl Pts',(-21.1562025901155,21.3927881860953,-39.7070518689786));
#22702=CARTESIAN_POINT('Ctrl Pts',(-21.1583167727293,21.3904444730533,-39.7072458296332));
#22703=CARTESIAN_POINT('Ctrl Pts',(-21.1633124635531,21.3849227469965,-39.7077037482568));
#22704=CARTESIAN_POINT('Ctrl Pts',(-21.1661968759341,21.3817473794389,-39.7079678293286));
#22705=CARTESIAN_POINT('Ctrl Pts',(-21.1762269111128,21.370749798858,-39.7088850526205));
#22706=CARTESIAN_POINT('Ctrl Pts',(-21.1834047016666,21.36295713445,-39.7095395646226));
#22707=CARTESIAN_POINT('Ctrl Pts',(-21.2699943751491,21.2698751910248,-39.7174132592279));
#22708=CARTESIAN_POINT('Ctrl Pts',(-21.3539280994796,21.1889284455533,-39.7248292125155));
#22709=CARTESIAN_POINT('Ctrl Pts',(-21.6497989526624,20.9330332595097,-39.7503226063137));
#22710=CARTESIAN_POINT('Ctrl Pts',(-21.8796548596196,20.7806628045816,-39.769218612152));
#22711=CARTESIAN_POINT('Ctrl Pts',(-22.1653336071807,20.6399190007228,-39.7904829088811));
#22712=CARTESIAN_POINT('Ctrl Pts',(-22.205075492554,20.6213379366103,-39.793392149016));
#22713=CARTESIAN_POINT('Ctrl Pts',(-22.2923759542161,20.5826730770439,-39.7996600518868));
#22714=CARTESIAN_POINT('Ctrl Pts',(-22.340064500163,20.5629080759267,-39.8030065816337));
#22715=CARTESIAN_POINT('Ctrl Pts',(-22.4112024407974,20.5354075762282,-39.8078646106639));
#22716=CARTESIAN_POINT('Ctrl Pts',(-22.4342968984392,20.5267829469499,-39.8094212254556));
#22717=CARTESIAN_POINT('Ctrl Pts',(-22.4615170774918,20.51697196314,-39.811230049917));
#22718=CARTESIAN_POINT('Ctrl Pts',(-22.4655481879374,20.5155280987436,-39.8114972613409));
#22719=CARTESIAN_POINT('Ctrl Pts',(-22.4717177917273,20.5133321317214,-39.8119052023128));
#22720=CARTESIAN_POINT('Ctrl Pts',(-22.4738542010116,20.5125742513514,-39.8120462762675));
#22721=CARTESIAN_POINT('Ctrl Pts',(-22.4777319669671,20.5112032380905,-39.8123019946953));
#22722=CARTESIAN_POINT('Ctrl Pts',(-22.4794730441465,20.5105893497264,-39.8124166841769));
#22723=CARTESIAN_POINT('Ctrl Pts',(-22.4830059943339,20.5093470749909,-39.8126491547138));
#22724=CARTESIAN_POINT('Ctrl Pts',(-22.4847978881922,20.5087187786674,-39.8127669301088));
#22725=CARTESIAN_POINT('Ctrl Pts',(-22.4899537820387,20.5069160699025,-39.8131054323337));
#22726=CARTESIAN_POINT('Ctrl Pts',(-22.4933191893341,20.5057456474368,-39.8133259203452));
#22727=CARTESIAN_POINT('Ctrl Pts',(-22.5080720104234,20.5006423166081,-39.8142904691134));
#22728=CARTESIAN_POINT('Ctrl Pts',(-22.5194796776835,20.4967676312706,-39.8150311016987));
#22729=CARTESIAN_POINT('Ctrl Pts',(-22.5341846714721,20.4918647883519,-39.8159794463193));
#22730=CARTESIAN_POINT('Ctrl Pts',(-22.5374620964976,20.4907779003529,-39.8161904063017));
#22731=CARTESIAN_POINT('Ctrl Pts',(-22.5417188482794,20.4893738291756,-39.8164638847554));
#22732=CARTESIAN_POINT('Ctrl Pts',(-22.5426965737359,20.4890518499832,-39.8165266640416));
#22733=CARTESIAN_POINT('Ctrl Pts',(-22.8524420315311,20.3872126447571,-39.8364040873027));
#22734=CARTESIAN_POINT('Ctrl Pts',(-23.1748481546112,20.33296841668,-39.8537182973952));
#22735=CARTESIAN_POINT('Ctrl Pts',(-23.6553486680242,20.3254701005996,-39.8809858788801));
#22736=CARTESIAN_POINT('Ctrl Pts',(-23.8106822747038,20.3342870950583,-39.8899977857389));
#22737=CARTESIAN_POINT('Ctrl Pts',(-23.9798908472098,20.3562329285497,-39.9003023449612));
#22738=CARTESIAN_POINT('Ctrl Pts',(-23.995005781739,20.3583025255617,-39.9012270003272));
#22739=CARTESIAN_POINT('Ctrl Pts',(-24.0176898902132,20.3615727734449,-39.9026211948382));
#22740=CARTESIAN_POINT('Ctrl Pts',(-24.0252705502291,20.3626932514166,-39.9030882037144));
#22741=CARTESIAN_POINT('Ctrl Pts',(-24.0374753019795,20.3645417089266,-39.9038418671412));
#22742=CARTESIAN_POINT('Ctrl Pts',(-24.0421019609835,20.3652527494764,-39.9041279848361));
#22743=CARTESIAN_POINT('Ctrl Pts',(-24.0509455767538,20.3666315954283,-39.9046756822619));
#22744=CARTESIAN_POINT('Ctrl Pts',(-24.0551627907752,20.3672977061904,-39.9049372077152));
#22745=CARTESIAN_POINT('Ctrl Pts',(-24.0626441051334,20.3684946254285,-39.9054017738816));
#22746=CARTESIAN_POINT('Ctrl Pts',(-24.0659087418275,20.3690220824129,-39.9056047077545));
#22747=CARTESIAN_POINT('Ctrl Pts',(-24.0723514701997,20.3700731915604,-39.9060056130027));
#22748=CARTESIAN_POINT('Ctrl Pts',(-24.075529600815,20.3705965852856,-39.9062035759461));
#22749=CARTESIAN_POINT('Ctrl Pts',(-24.0831801202355,20.3718683022208,-39.9066806055717));
#22750=CARTESIAN_POINT('Ctrl Pts',(-24.0876517159908,20.3726213005435,-39.9069598208863));
#22751=CARTESIAN_POINT('Ctrl Pts',(-24.1013743183089,20.3749619244198,-39.9078179236273));
#22752=CARTESIAN_POINT('Ctrl Pts',(-24.1106199281166,20.3765805192833,-39.9083977969088));
#22753=CARTESIAN_POINT('Ctrl Pts',(-24.2186704867407,20.3959834081086,-39.9151950639356));
#22754=CARTESIAN_POINT('Ctrl Pts',(-24.3165895560363,20.4183329591346,-39.9215580347125));
#22755=CARTESIAN_POINT('Ctrl Pts',(-24.4739914952224,20.462082820137,-39.9321359420316));
#22756=CARTESIAN_POINT('Ctrl Pts',(-24.5341740796881,20.4807275748041,-39.936265418512));
#22757=CARTESIAN_POINT('Ctrl Pts',(-24.7984724093166,20.5711794953779,-39.9547626052912));
#22758=CARTESIAN_POINT('Ctrl Pts',(-24.9955952148721,20.6616712136987,-39.9695795652277));
#22759=CARTESIAN_POINT('Ctrl Pts',(-25.2913012167031,20.8353140012914,-39.9925530879096));
#22760=CARTESIAN_POINT('Ctrl Pts',(-25.3966028411608,20.9057978413637,-40.0008910013439));
#22761=CARTESIAN_POINT('Ctrl Pts',(-25.5038363777757,20.9871116772185,-40.0093405600064));
#22762=CARTESIAN_POINT('Ctrl Pts',(-25.5101592793117,20.9919432408942,-40.0098386045528));
#22763=CARTESIAN_POINT('Ctrl Pts',(-25.5187743392916,20.9985770123843,-40.0105168851808));
#22764=CARTESIAN_POINT('Ctrl Pts',(-25.5210819748955,21.0003589321878,-40.0106985389872));
#22765=CARTESIAN_POINT('Ctrl Pts',(-25.5249416578276,21.0033476879949,-40.0110023114422));
#22766=CARTESIAN_POINT('Ctrl Pts',(-25.5264950187851,21.0045528125608,-40.0111245518396));
#22767=CARTESIAN_POINT('Ctrl Pts',(-25.5295542536041,21.0069307079442,-40.011365263836));
#22768=CARTESIAN_POINT('Ctrl Pts',(-25.5310601885078,21.0081033951837,-40.0114837410902));
#22769=CARTESIAN_POINT('Ctrl Pts',(-25.5343807105304,21.0106938623091,-40.0117449467312));
#22770=CARTESIAN_POINT('Ctrl Pts',(-25.5361948247782,21.012112253081,-40.0118876313892));
#22771=CARTESIAN_POINT('Ctrl Pts',(-25.5425395827863,21.017083958303,-40.0123865956124));
#22772=CARTESIAN_POINT('Ctrl Pts',(-25.5470622576685,21.0206474963903,-40.0127421479018));
#22773=CARTESIAN_POINT('Ctrl Pts',(-25.5932603644229,21.0572493383338,-40.0163730878217));
#22774=CARTESIAN_POINT('Ctrl Pts',(-25.6341244494885,21.0913046739964,-40.0195769088653));
#22775=CARTESIAN_POINT('Ctrl Pts',(-25.6773037562032,21.1291394693697,-40.0229768807352));
#22776=CARTESIAN_POINT('Ctrl Pts',(-25.6804723707524,21.1319269105535,-40.0232264669171));
#22777=CARTESIAN_POINT('Ctrl Pts',(-25.6893365278733,21.1397556796846,-40.0239249552417));
#22778=CARTESIAN_POINT('Ctrl Pts',(-25.6950197433927,21.144810986827,-40.0243731064914));
#22779=CARTESIAN_POINT('Ctrl Pts',(-25.7254692191221,21.1720899682558,-40.0267762598433));
#22780=CARTESIAN_POINT('Ctrl Pts',(-25.7499087912535,21.1946767439125,-40.028712438279));
#22781=CARTESIAN_POINT('Ctrl Pts',(-25.8851971439204,21.3236507005305,-40.0395012291548));
#22782=CARTESIAN_POINT('Ctrl Pts',(-25.9886829489201,21.4374854211448,-40.0480344162214));
#22783=CARTESIAN_POINT('Ctrl Pts',(-26.175137740566,21.6746193257529,-40.0648975549305));
#22784=CARTESIAN_POINT('Ctrl Pts',(-26.2584899917043,21.7971216767046,-40.0732048404906));
#22785=CARTESIAN_POINT('Ctrl Pts',(-26.3682548041575,21.9850584135228,-40.0858199247245));
#22786=CARTESIAN_POINT('Ctrl Pts',(-26.4014231165206,22.0463260930644,-40.0899119294625));
#22787=CARTESIAN_POINT('Ctrl Pts',(-26.4522654039221,22.1479773705553,-40.0967014799763));
#22788=CARTESIAN_POINT('Ctrl Pts',(-26.4711428138771,22.187735006646,-40.0993569430766));
#22789=CARTESIAN_POINT('Ctrl Pts',(-26.4923460979797,22.2348583649895,-40.1025086019364));
#22790=CARTESIAN_POINT('Ctrl Pts',(-26.4954676648637,22.2418626110948,-40.1029771586341));
#22791=CARTESIAN_POINT('Ctrl Pts',(-26.5002068949672,22.2525995094628,-40.1036956003655));
#22792=CARTESIAN_POINT('Ctrl Pts',(-26.5018425534703,22.2563242281902,-40.1039448677161));
#22793=CARTESIAN_POINT('Ctrl Pts',(-26.504680312456,22.2628197477584,-40.1043796269023));
#22794=CARTESIAN_POINT('Ctrl Pts',(-26.5058855809764,22.2655891661459,-40.1045650099888));
#22795=CARTESIAN_POINT('Ctrl Pts',(-26.508395158224,22.2713777995516,-40.1049525408));
#22796=CARTESIAN_POINT('Ctrl Pts',(-26.5096987412893,22.2743973236896,-40.1051547130781));
#22797=CARTESIAN_POINT('Ctrl Pts',(-26.5132851939323,22.2827397900305,-40.1057133539995));
#22798=CARTESIAN_POINT('Ctrl Pts',(-26.51555833157,22.288066879624,-40.1060701543683));
#22799=CARTESIAN_POINT('Ctrl Pts',(-26.5243847909365,22.3089071040138,-40.1074663342694));
#22800=CARTESIAN_POINT('Ctrl Pts',(-26.5308307446904,22.324465166293,-40.1085093607361));
#22801=CARTESIAN_POINT('Ctrl Pts',(-26.5435867323968,22.3559488229183,-40.1106217534887));
#22802=CARTESIAN_POINT('Ctrl Pts',(-26.5498923149257,22.371875623209,-40.1116912299134));
#22803=CARTESIAN_POINT('Ctrl Pts',(-26.5573628858436,22.3911935518822,-40.1129895902443));
#22804=CARTESIAN_POINT('Ctrl Pts',(-26.5586496618932,22.3945375549122,-40.1132143832554));
#22805=CARTESIAN_POINT('Ctrl Pts',(-26.5615812069348,22.4021939642269,-40.1137291661877));
#22806=CARTESIAN_POINT('Ctrl Pts',(-26.5632222912403,22.4065077645519,-40.11401927812));
#22807=CARTESIAN_POINT('Ctrl Pts',(-26.5654514358838,22.4124054483284,-40.1144160087214));
#22808=CARTESIAN_POINT('Ctrl Pts',(-26.5660475317198,22.4139863063961,-40.114522361005));
#22809=CARTESIAN_POINT('Ctrl Pts',(-26.5682404733335,22.4198159132048,-40.1149145841221));
#22810=CARTESIAN_POINT('Ctrl Pts',(-26.5698295801112,22.4240675501587,-40.1152007101685));
#22811=CARTESIAN_POINT('Ctrl Pts',(-26.5738306163833,22.4348416262432,-40.1159259644523));
#22812=CARTESIAN_POINT('Ctrl Pts',(-26.5762304172222,22.4413685173391,-40.1163654892191));
#22813=CARTESIAN_POINT('Ctrl Pts',(-26.5807171654634,22.4536944393504,-40.1171958495523));
#22814=CARTESIAN_POINT('Ctrl Pts',(-26.5828086427921,22.459491797797,-40.1175865354797));
#22815=CARTESIAN_POINT('Ctrl Pts',(-26.5862561019136,22.4691343567345,-40.1182365791334));
#22816=CARTESIAN_POINT('Ctrl Pts',(-26.5876214455889,22.4729762127876,-40.118495634177));
#22817=CARTESIAN_POINT('Ctrl Pts',(-26.5909282573542,22.4823373078819,-40.1191269971723));
#22818=CARTESIAN_POINT('Ctrl Pts',(-26.5928619880055,22.4878592478708,-40.1194995514436));
#22819=CARTESIAN_POINT('Ctrl Pts',(-26.6031367635958,22.5174579285306,-40.1214971895168));
#22820=CARTESIAN_POINT('Ctrl Pts',(-26.6112068981729,22.5416271630281,-40.1231307862509));
#22821=CARTESIAN_POINT('Ctrl Pts',(-26.6955735338472,22.8046387483594,-40.1409338551455));
#22822=CARTESIAN_POINT('Ctrl Pts',(-26.7440238002873,23.0514817893682,-40.1579746615357));
#22823=CARTESIAN_POINT('Ctrl Pts',(-26.7698317099746,23.3846965035763,-40.1805383707152));
#22824=CARTESIAN_POINT('Ctrl Pts',(-26.7730419584783,23.4682248964479,-40.186148437505));
#22825=CARTESIAN_POINT('Ctrl Pts',(-26.7729616907037,23.6367855573696,-40.1972739748567));
#22826=CARTESIAN_POINT('Ctrl Pts',(-26.7695585239657,23.7217583255444,-40.2027819157312));
#22827=CARTESIAN_POINT('Ctrl Pts',(-26.7622951592415,23.8128164386024,-40.2085079375289));
#22828=CARTESIAN_POINT('Ctrl Pts',(-26.7617731417886,23.8191261431661,-40.2089037955238));
#22829=CARTESIAN_POINT('Ctrl Pts',(-26.7610221302478,23.8278893790836,-40.2094522714681));
#22830=CARTESIAN_POINT('Ctrl Pts',(-26.7608089156665,23.830344194295,-40.2096057711108));
#22831=CARTESIAN_POINT('Ctrl Pts',(-26.7604371519985,23.834568238835,-40.2098696516874));
#22832=CARTESIAN_POINT('Ctrl Pts',(-26.7602799556067,23.8363375811637,-40.2099801091898));
#22833=CARTESIAN_POINT('Ctrl Pts',(-26.759951771976,23.8399971634916,-40.2102084148184));
#22834=CARTESIAN_POINT('Ctrl Pts',(-26.7597805780771,23.8418873790929,-40.210326250478));
#22835=CARTESIAN_POINT('Ctrl Pts',(-26.7593739622225,23.8463332528007,-40.2106032032153));
#22836=CARTESIAN_POINT('Ctrl Pts',(-26.759137156407,23.8488887898389,-40.2107622416241));
#22837=CARTESIAN_POINT('Ctrl Pts',(-26.7583548826092,23.8572224863665,-40.2112803671126));
#22838=CARTESIAN_POINT('Ctrl Pts',(-26.7577968545562,23.8629994983255,-40.2116387465621));
#22839=CARTESIAN_POINT('Ctrl Pts',(-26.7437398286368,24.0045294407308,-40.2203999202259));
#22840=CARTESIAN_POINT('Ctrl Pts',(-26.7216480144846,24.1393110578934,-40.2283235834077));
#22841=CARTESIAN_POINT('Ctrl Pts',(-26.6107496905108,24.6217035391429,-40.2564428437242));
#22842=CARTESIAN_POINT('Ctrl Pts',(-26.4727030976038,24.9552220863105,-40.2757435691211));
#22843=CARTESIAN_POINT('Ctrl Pts',(-26.2711447527167,25.2774840644441,-40.2987143824648));
#22844=CARTESIAN_POINT('Ctrl Pts',(-26.2595183758889,25.2956641726692,-40.3000251262651));
#22845=CARTESIAN_POINT('Ctrl Pts',(-26.244211932783,25.3190773355242,-40.3017330570757));
#22846=CARTESIAN_POINT('Ctrl Pts',(-26.2406974564878,25.3244184053037,-40.3021240303567));
#22847=CARTESIAN_POINT('Ctrl Pts',(-26.2350749947224,25.3329079276356,-40.3027476521517));
#22848=CARTESIAN_POINT('Ctrl Pts',(-26.2329772977947,25.3360632013388,-40.3029799128244));
#22849=CARTESIAN_POINT('Ctrl Pts',(-26.2291993335496,25.3417241885289,-40.3033974882909));
#22850=CARTESIAN_POINT('Ctrl Pts',(-26.2275211002365,25.3442312596081,-40.3035827260705));
#22851=CARTESIAN_POINT('Ctrl Pts',(-26.2235908134966,25.350084819525,-40.3040159428671));
#22852=CARTESIAN_POINT('Ctrl Pts',(-26.2213359962547,25.3534294388183,-40.3042640263814));
#22853=CARTESIAN_POINT('Ctrl Pts',(-26.2148664522571,25.3629870910404,-40.3049745396833));
#22854=CARTESIAN_POINT('Ctrl Pts',(-26.2106363067511,25.3691896103726,-40.3054375546134));
#22855=CARTESIAN_POINT('Ctrl Pts',(-26.183298377065,25.408974919158,-40.3084199682001));
#22856=CARTESIAN_POINT('Ctrl Pts',(-26.1595777154717,25.4421302171039,-40.310962721746));
#22857=CARTESIAN_POINT('Ctrl Pts',(-26.0871757867881,25.5393765933113,-40.3185977732205));
#22858=CARTESIAN_POINT('Ctrl Pts',(-26.0367188712131,25.6020998598379,-40.3237584064895));
#22859=CARTESIAN_POINT('Ctrl Pts',(-25.8841030917694,25.7779124274078,-40.3389285097516));
#22860=CARTESIAN_POINT('Ctrl Pts',(-25.7762127085705,25.8857224845346,-40.3491423694584));
#22861=CARTESIAN_POINT('Ctrl Pts',(-25.5144132645354,26.1126500919241,-40.3725695110983));
#22862=CARTESIAN_POINT('Ctrl Pts',(-25.3565121075421,26.2263028725007,-40.3857975470013));
#22863=CARTESIAN_POINT('Ctrl Pts',(-25.1842916925768,26.3280336335191,-40.3987360348031));
#22864=CARTESIAN_POINT('Ctrl Pts',(-25.1792434403606,26.3309971171321,-40.3991140323917));
#22865=CARTESIAN_POINT('Ctrl Pts',(-25.1685615708219,26.3372286408767,-40.3999111458774));
#22866=CARTESIAN_POINT('Ctrl Pts',(-25.1629260535916,26.3404933980867,-40.400330098746));
#22867=CARTESIAN_POINT('Ctrl Pts',(-25.127107343058,26.3610990577738,-40.4029826837996));
#22868=CARTESIAN_POINT('Ctrl Pts',(-25.0966532459377,26.3779679286133,-40.4051920149658));
#22869=CARTESIAN_POINT('Ctrl Pts',(-25.0618643214626,26.3965077182443,-40.4076591053477));
#22870=CARTESIAN_POINT('Ctrl Pts',(-25.0577936699645,26.3986658631789,-40.4079469097147));
#22871=CARTESIAN_POINT('Ctrl Pts',(-25.0516238190644,26.4019200136322,-40.4083818006319));
#22872=CARTESIAN_POINT('Ctrl Pts',(-25.0495280385203,26.4030224356301,-40.4085292926888));
#22873=CARTESIAN_POINT('Ctrl Pts',(-25.0458800917313,26.4049361974634,-40.4087856135165));
#22874=CARTESIAN_POINT('Ctrl Pts',(-25.0443284793919,26.4057485818574,-40.4088945090383));
#22875=CARTESIAN_POINT('Ctrl Pts',(-25.0410776524406,26.4074472563621,-40.4091223907735));
#22876=CARTESIAN_POINT('Ctrl Pts',(-25.0393783103464,26.4083332951952,-40.4092413605066));
#22877=CARTESIAN_POINT('Ctrl Pts',(-25.035357009636,26.4104254457452,-40.4095225282901));
#22878=CARTESIAN_POINT('Ctrl Pts',(-25.0330343638712,26.4116302500242,-40.409684642745));
#22879=CARTESIAN_POINT('Ctrl Pts',(-25.0252696727443,26.415645962449,-40.4102256576603));
#22880=CARTESIAN_POINT('Ctrl Pts',(-25.0198210385415,26.4184442066952,-40.4106037579009));
#22881=CARTESIAN_POINT('Ctrl Pts',(-25.0068620581773,26.4250529027084,-40.4114994534875));
#22882=CARTESIAN_POINT('Ctrl Pts',(-24.999344645047,26.428849505306,-40.412016199166));
#22883=CARTESIAN_POINT('Ctrl Pts',(-24.7280357745039,26.5645394972366,-40.4305668905324));
#22884=CARTESIAN_POINT('Ctrl Pts',(-24.4473474058066,26.6596556994222,-40.4464829212868));
#22885=CARTESIAN_POINT('Ctrl Pts',(-23.9588604612326,26.753392499944,-40.4744755421013));
#22886=CARTESIAN_POINT('Ctrl Pts',(-23.7570114492831,26.772720247831,-40.4861086074569));
#22887=CARTESIAN_POINT('Ctrl Pts',(-23.5421097332939,26.773016839029,-40.4991674843511));
#22888=CARTESIAN_POINT('Ctrl Pts',(-23.529519290729,26.7729604321195,-40.4999348546891));
#22889=CARTESIAN_POINT('Ctrl Pts',(-23.5123117633937,26.7727824986097,-40.5009868594883));
#22890=CARTESIAN_POINT('Ctrl Pts',(-23.5076940135634,26.7727248219926,-40.5012694895278));
#22891=CARTESIAN_POINT('Ctrl Pts',(-23.4998330520786,26.772609737263,-40.5017511675346));
#22892=CARTESIAN_POINT('Ctrl Pts',(-23.4965897640427,26.7725573576625,-40.5019500574627));
#22893=CARTESIAN_POINT('Ctrl Pts',(-23.4903152951151,26.7724465484567,-40.5023351388454));
#22894=CARTESIAN_POINT('Ctrl Pts',(-23.4872841061145,26.7723887378889,-40.5025213106258));
#22895=CARTESIAN_POINT('Ctrl Pts',(-23.4800891579364,26.7722413597989,-40.5029635481683));
#22896=CARTESIAN_POINT('Ctrl Pts',(-23.4759254895573,26.7721479983406,-40.5032197327881));
#22897=CARTESIAN_POINT('Ctrl Pts',(-23.4636362900537,26.7718486044526,-40.5039766576652));
#22898=CARTESIAN_POINT('Ctrl Pts',(-23.455511389138,26.7716199033696,-40.5044781089932));
#22899=CARTESIAN_POINT('Ctrl Pts',(-23.3962879282221,26.7697286214481,-40.5081407771957));
#22900=CARTESIAN_POINT('Ctrl Pts',(-23.3452369727204,26.7668811280424,-40.5113390353455));
#22901=CARTESIAN_POINT('Ctrl Pts',(-23.1766186828373,26.7534457544234,-40.5220468777366));
#22902=CARTESIAN_POINT('Ctrl Pts',(-23.05957666139,26.7376152056598,-40.5297163611454));
#22903=CARTESIAN_POINT('Ctrl Pts',(-22.6816014622723,26.6651793368112,-40.5552167909542));
#22904=CARTESIAN_POINT('Ctrl Pts',(-22.4268035424485,26.5826066103071,-40.5736589341423));
#22905=CARTESIAN_POINT('Ctrl Pts',(-22.1765026572863,26.4655602462323,-40.5918247588175));
#22906=CARTESIAN_POINT('Ctrl Pts',(-22.1679159917987,26.4614985676578,-40.5924478687849));
#22907=CARTESIAN_POINT('Ctrl Pts',(-22.1310407320159,26.4438558405741,-40.5951231116031));
#22908=CARTESIAN_POINT('Ctrl Pts',(-22.1029339564756,26.4299002722503,-40.5971604721212));
#22909=CARTESIAN_POINT('Ctrl Pts',(-22.0750360128358,26.4155367732638,-40.5991777786305));
#22910=CARTESIAN_POINT('',(-26.7730012248527,23.5473502489538,-40.4353769712642));
#22911=CARTESIAN_POINT('Ctrl Pts',(-22.0750362323924,26.4155368863044,-40.843547806833));
#22912=CARTESIAN_POINT('Ctrl Pts',(-22.1513564730552,26.4548310187738,-40.837761028126));
#22913=CARTESIAN_POINT('Ctrl Pts',(-22.2292424792406,26.4910736721318,-40.8319373078903));
#22914=CARTESIAN_POINT('Ctrl Pts',(-22.4488693000598,26.5827774917964,-40.815847588764));
#22915=CARTESIAN_POINT('Ctrl Pts',(-22.5932160538874,26.6313795249419,-40.8056365593697));
#22916=CARTESIAN_POINT('Ctrl Pts',(-22.744709524646,26.6707071808935,-40.795616046995));
#22917=CARTESIAN_POINT('Ctrl Pts',(-22.7489520407912,26.6717993081585,-40.7953359836428));
#22918=CARTESIAN_POINT('Ctrl Pts',(-22.7581497491691,26.6741470360723,-40.7947300368079));
#22919=CARTESIAN_POINT('Ctrl Pts',(-22.763105740177,26.6753995077501,-40.794404305159));
#22920=CARTESIAN_POINT('Ctrl Pts',(-22.775744800319,26.6785616615831,-40.7935756028079));
#22921=CARTESIAN_POINT('Ctrl Pts',(-22.7834320173745,26.6804548478066,-40.7930734556238));
#22922=CARTESIAN_POINT('Ctrl Pts',(-22.7991796185297,26.6842716300435,-40.7920487361023));
#22923=CARTESIAN_POINT('Ctrl Pts',(-22.8072406164304,26.6861925067163,-40.791526308102));
#22924=CARTESIAN_POINT('Ctrl Pts',(-22.8236892354184,26.6900451075517,-40.7904647132452));
#22925=CARTESIAN_POINT('Ctrl Pts',(-22.8320773803821,26.6919743683588,-40.7899256835826));
#22926=CARTESIAN_POINT('Ctrl Pts',(-22.8435095494201,26.6945555718746,-40.7891943227393));
#22927=CARTESIAN_POINT('Ctrl Pts',(-22.8465468386675,26.695236720729,-40.7890003301954));
#22928=CARTESIAN_POINT('Ctrl Pts',(-22.8513502031162,26.6963066265373,-40.7886940406786));
#22929=CARTESIAN_POINT('Ctrl Pts',(-22.853115616823,26.6966982970831,-40.7885815752708));
#22930=CARTESIAN_POINT('Ctrl Pts',(-22.8565353884731,26.6974539801377,-40.7883639282661));
#22931=CARTESIAN_POINT('Ctrl Pts',(-22.8581896925598,26.6978181717698,-40.7882587370526));
#22932=CARTESIAN_POINT('Ctrl Pts',(-22.8621518649697,26.6986871611526,-40.7880070228545));
#22933=CARTESIAN_POINT('Ctrl Pts',(-22.8644600004047,26.6991907253768,-40.7878605719427));
#22934=CARTESIAN_POINT('Ctrl Pts',(-22.8692578584121,26.7002319451502,-40.7875565255609));
#22935=CARTESIAN_POINT('Ctrl Pts',(-22.87174767021,26.7007691882577,-40.7873989539083));
#22936=CARTESIAN_POINT('Ctrl Pts',(-22.8863910495771,26.7039107227969,-40.7864734503695));
#22937=CARTESIAN_POINT('Ctrl Pts',(-22.8985591876554,26.7064476858235,-40.7857093519794));
#22938=CARTESIAN_POINT('Ctrl Pts',(-22.9943078695785,26.7258332050058,-40.779733597182));
#22939=CARTESIAN_POINT('Ctrl Pts',(-23.078520773411,26.7394309678924,-40.774697527537));
#22940=CARTESIAN_POINT('Ctrl Pts',(-23.3050181855836,26.7668329683103,-40.7615003002726));
#22941=CARTESIAN_POINT('Ctrl Pts',(-23.4478478175809,26.7745428387671,-40.7535360495702));
#22942=CARTESIAN_POINT('Ctrl Pts',(-23.8548297887662,26.7694313910848,-40.730794007933));
#22943=CARTESIAN_POINT('Ctrl Pts',(-24.1174803372404,26.7336636119848,-40.7159687673348));
#22944=CARTESIAN_POINT('Ctrl Pts',(-24.38788742692,26.662282179612,-40.6990161378172));
#22945=CARTESIAN_POINT('Ctrl Pts',(-24.4029360095259,26.6581926245072,-40.6980673790172));
#22946=CARTESIAN_POINT('Ctrl Pts',(-24.4239099614613,26.6523290140556,-40.6967374069354));
#22947=CARTESIAN_POINT('Ctrl Pts',(-24.4298609693977,26.6506468295997,-40.696359187684));
#22948=CARTESIAN_POINT('Ctrl Pts',(-24.4390454245989,26.6480220679056,-40.6957741202273));
#22949=CARTESIAN_POINT('Ctrl Pts',(-24.4422823205954,26.6470915267879,-40.695567665271));
#22950=CARTESIAN_POINT('Ctrl Pts',(-24.4487303033242,26.6452269160755,-40.695155883721));
#22951=CARTESIAN_POINT('Ctrl Pts',(-24.4519414068243,26.6442929190231,-40.6949505597168));
#22952=CARTESIAN_POINT('Ctrl Pts',(-24.4590637188037,26.6422092597221,-40.694494574123));
#22953=CARTESIAN_POINT('Ctrl Pts',(-24.4629742065211,26.6410571722158,-40.6942438334242));
#22954=CARTESIAN_POINT('Ctrl Pts',(-24.4710348916886,26.6386657437119,-40.6937261873489));
#22955=CARTESIAN_POINT('Ctrl Pts',(-24.4751847958731,26.6374254502443,-40.6934592511492));
#22956=CARTESIAN_POINT('Ctrl Pts',(-24.4972610999111,26.6307789343835,-40.6920368970287));
#22957=CARTESIAN_POINT('Ctrl Pts',(-24.5151423338614,26.6252250180423,-40.6908766393347));
#22958=CARTESIAN_POINT('Ctrl Pts',(-24.5609105414444,26.6105708840475,-40.6878853850498));
#22959=CARTESIAN_POINT('Ctrl Pts',(-24.5887230219044,26.6012453175943,-40.6860470286971));
#22960=CARTESIAN_POINT('Ctrl Pts',(-24.6442329533307,26.5817858150694,-40.6823354778324));
#22961=CARTESIAN_POINT('Ctrl Pts',(-24.671926316966,26.5716487385447,-40.6804623271743));
#22962=CARTESIAN_POINT('Ctrl Pts',(-24.8259121274272,26.5128738771706,-40.6699249836441));
#22963=CARTESIAN_POINT('Ctrl Pts',(-24.9491682751369,26.4567039424799,-40.6610202831163));
#22964=CARTESIAN_POINT('Ctrl Pts',(-25.1592811798299,26.3444845037842,-40.6450703241916));
#22965=CARTESIAN_POINT('Ctrl Pts',(-25.2476685405325,26.2916906968821,-40.6381017438154));
#22966=CARTESIAN_POINT('Ctrl Pts',(-25.4946700202883,26.127625602962,-40.6180327134718));
#22967=CARTESIAN_POINT('Ctrl Pts',(-25.6460014370845,26.0061570290951,-40.6049666664731));
#22968=CARTESIAN_POINT('Ctrl Pts',(-25.7936628702886,25.8639844225203,-40.5920514785592));
#22969=CARTESIAN_POINT('Ctrl Pts',(-25.8017605601856,25.8561052625966,-40.5913427122474));
#22970=CARTESIAN_POINT('Ctrl Pts',(-25.8122944611703,25.8457472379028,-40.5904202560485));
#22971=CARTESIAN_POINT('Ctrl Pts',(-25.8147682054961,25.843306914023,-40.5902035965511));
#22972=CARTESIAN_POINT('Ctrl Pts',(-25.8185750417222,25.8395393402032,-40.5898701359819));
#22973=CARTESIAN_POINT('Ctrl Pts',(-25.819910916704,25.8382149257275,-40.5897531113613));
#22974=CARTESIAN_POINT('Ctrl Pts',(-25.8224369205943,25.8357062031361,-40.5895318151854));
#22975=CARTESIAN_POINT('Ctrl Pts',(-25.823627277617,25.8345221405837,-40.589427525368));
#22976=CARTESIAN_POINT('Ctrl Pts',(-25.826390214499,25.8317695149214,-40.5891854441443));
#22977=CARTESIAN_POINT('Ctrl Pts',(-25.827962095859,25.8302002585559,-40.5890477091122));
#22978=CARTESIAN_POINT('Ctrl Pts',(-25.8311939929272,25.8269670805934,-40.5887644905391));
#22979=CARTESIAN_POINT('Ctrl Pts',(-25.8328538138293,25.8253029648979,-40.5886190225669));
#22980=CARTESIAN_POINT('Ctrl Pts',(-25.8370952525269,25.8210412371743,-40.5882472588726));
#22981=CARTESIAN_POINT('Ctrl Pts',(-25.8396742744496,25.8184410289035,-40.5880211679012));
#22982=CARTESIAN_POINT('Ctrl Pts',(-25.874269672473,25.7834423134307,-40.5849877322549));
#22983=CARTESIAN_POINT('Ctrl Pts',(-25.9056021359536,25.7503709458318,-40.5822332859898));
#22984=CARTESIAN_POINT('Ctrl Pts',(-26.0028183027167,25.643301173013,-40.5736207399938));
#22985=CARTESIAN_POINT('Ctrl Pts',(-26.0660004207196,25.5669199209323,-40.5679216041295));
#22986=CARTESIAN_POINT('Ctrl Pts',(-26.1486623643995,25.4570455472252,-40.5601296995412));
#22987=CARTESIAN_POINT('Ctrl Pts',(-26.1712066981876,25.4259371027024,-40.5579661649992));
#22988=CARTESIAN_POINT('Ctrl Pts',(-26.2167651003378,25.3606462990484,-40.5534972349297));
#22989=CARTESIAN_POINT('Ctrl Pts',(-26.2396905324993,25.3264107902338,-40.5511933336223));
#22990=CARTESIAN_POINT('Ctrl Pts',(-26.4109220997595,25.05978385017,-40.5334843747185));
#22991=CARTESIAN_POINT('Ctrl Pts',(-26.5294909902898,24.8097077193418,-40.5180900092991));
#22992=CARTESIAN_POINT('Ctrl Pts',(-26.6203180774493,24.5306269804338,-40.5003147057651));
#22993=CARTESIAN_POINT('Ctrl Pts',(-26.6257036957868,24.5135991111972,-40.4992284949293));
#22994=CARTESIAN_POINT('Ctrl Pts',(-26.6326892756781,24.4908568446712,-40.497775261441));
#22995=CARTESIAN_POINT('Ctrl Pts',(-26.6344154573406,24.4851812998778,-40.4974123871669));
#22996=CARTESIAN_POINT('Ctrl Pts',(-26.6370824428728,24.4763247027596,-40.4968457951887));
#22997=CARTESIAN_POINT('Ctrl Pts',(-26.6380340284793,24.4731468888921,-40.4966424310991));
#22998=CARTESIAN_POINT('Ctrl Pts',(-26.6399277949692,24.466786952021,-40.4962352915862));
#22999=CARTESIAN_POINT('Ctrl Pts',(-26.6408699703951,24.4636048315246,-40.4960315162637));
#23000=CARTESIAN_POINT('Ctrl Pts',(-26.6429803550894,24.4564365236835,-40.4955723199325));
#23001=CARTESIAN_POINT('Ctrl Pts',(-26.6441457744967,24.4524495272685,-40.4953168080562));
#23002=CARTESIAN_POINT('Ctrl Pts',(-26.6465404396048,24.4441979726282,-40.4947877687786));
#23003=CARTESIAN_POINT('Ctrl Pts',(-26.6477685900406,24.4399331080866,-40.4945142061628));
#23004=CARTESIAN_POINT('Ctrl Pts',(-26.6509341031461,24.4288545659702,-40.493803259246));
#23005=CARTESIAN_POINT('Ctrl Pts',(-26.6528578096559,24.4220370406488,-40.4933654299952));
#23006=CARTESIAN_POINT('Ctrl Pts',(-26.6584373812404,24.4020109107513,-40.4920783450723));
#23007=CARTESIAN_POINT('Ctrl Pts',(-26.6620314498309,24.3887853876545,-40.4912270823696));
#23008=CARTESIAN_POINT('Ctrl Pts',(-26.6740925769035,24.3432570048757,-40.488292126506));
#23009=CARTESIAN_POINT('Ctrl Pts',(-26.6821416267725,24.3108465649558,-40.4861949952005));
#23010=CARTESIAN_POINT('Ctrl Pts',(-26.7452809481041,24.038588497622,-40.4685082034141));
#23011=CARTESIAN_POINT('Ctrl Pts',(-26.7732227470116,23.7933325710728,-40.452027638618));
#23012=CARTESIAN_POINT('Ctrl Pts',(-26.7730012248527,23.5473502489538,-40.4353769712642));
#23013=CARTESIAN_POINT('Ctrl Pts',(-26.7730012238456,23.5473491308651,-40.4353768955802));
#23014=CARTESIAN_POINT('Ctrl Pts',(-26.7728090040715,23.33398691809,-40.4209342997964));
#23015=CARTESIAN_POINT('Ctrl Pts',(-26.7514288037154,23.1211364370925,-40.4064672452439));
#23016=CARTESIAN_POINT('Ctrl Pts',(-26.7080768764898,22.9065968620062,-40.3927228443158));
#23017=CARTESIAN_POINT('Ctrl Pts',(-26.706984812474,22.901262144858,-40.3923816401998));
#23018=CARTESIAN_POINT('Ctrl Pts',(-26.705252840185,22.8929092925769,-40.3918483080951));
#23019=CARTESIAN_POINT('Ctrl Pts',(-26.7046221164231,22.8898892955003,-40.3916556668281));
#23020=CARTESIAN_POINT('Ctrl Pts',(-26.7035529623943,22.8848065132523,-40.3913317628625));
#23021=CARTESIAN_POINT('Ctrl Pts',(-26.7031168439663,22.8827432522273,-40.3912003687335));
#23022=CARTESIAN_POINT('Ctrl Pts',(-26.7022526773045,22.8786746515126,-40.3909414460159));
#23023=CARTESIAN_POINT('Ctrl Pts',(-26.7018247398349,22.8766692896164,-40.3908139111171));
#23024=CARTESIAN_POINT('Ctrl Pts',(-26.7009993821942,22.8728195784806,-40.390569245984));
#23025=CARTESIAN_POINT('Ctrl Pts',(-26.7006022575248,22.8709751752274,-40.3904520993814));
#23026=CARTESIAN_POINT('Ctrl Pts',(-26.6996851997146,22.8667341000169,-40.3901828949823));
#23027=CARTESIAN_POINT('Ctrl Pts',(-26.6991641490948,22.8643376661808,-40.390030901957));
#23028=CARTESIAN_POINT('Ctrl Pts',(-26.6975012763788,22.8567315543887,-40.3895488669505));
#23029=CARTESIAN_POINT('Ctrl Pts',(-26.696349249691,22.8515240802496,-40.3892194112805));
#23030=CARTESIAN_POINT('Ctrl Pts',(-26.6864089187849,22.8071140887442,-40.3864144214184));
#23031=CARTESIAN_POINT('Ctrl Pts',(-26.6769007028632,22.7680740306628,-40.3839795347652));
#23032=CARTESIAN_POINT('Ctrl Pts',(-26.6649277605561,22.722628070755,-40.3811705483139));
#23033=CARTESIAN_POINT('Ctrl Pts',(-26.6631702085471,22.7160417859539,-40.3807640830489));
#23034=CARTESIAN_POINT('Ctrl Pts',(-26.6609689012003,22.707896396793,-40.3802621224018));
#23035=CARTESIAN_POINT('Ctrl Pts',(-26.6605448633145,22.7063320369776,-40.3801657515795));
#23036=CARTESIAN_POINT('Ctrl Pts',(-26.6593613663262,22.7019788901117,-40.3798976706361));
#23037=CARTESIAN_POINT('Ctrl Pts',(-26.6585993336444,22.6991907974415,-40.3797260740336));
#23038=CARTESIAN_POINT('Ctrl Pts',(-26.6526237517894,22.6774426793,-40.3783883380882));
#23039=CARTESIAN_POINT('Ctrl Pts',(-26.6472404150811,22.6585293074089,-40.3772295888355));
#23040=CARTESIAN_POINT('Ctrl Pts',(-26.6296783214793,22.5989061852302,-40.3735879415328));
#23041=CARTESIAN_POINT('Ctrl Pts',(-26.6168670621754,22.5583862854609,-40.3711296870645));
#23042=CARTESIAN_POINT('Ctrl Pts',(-26.5716482755289,22.4246296693829,-40.3630350486516));
#23043=CARTESIAN_POINT('Ctrl Pts',(-26.5357587975781,22.3326265459007,-40.3574989022638));
#23044=CARTESIAN_POINT('Ctrl Pts',(-26.4841783225591,22.2164596865587,-40.3503908882467));
#23045=CARTESIAN_POINT('Ctrl Pts',(-26.4723122462374,22.1906603395344,-40.348804659764));
#23046=CARTESIAN_POINT('Ctrl Pts',(-26.4497429699397,22.1432507117845,-40.3458706615062));
#23047=CARTESIAN_POINT('Ctrl Pts',(-26.4391352160234,22.1215973059098,-40.3445231247795));
#23048=CARTESIAN_POINT('Ctrl Pts',(-26.4061624347003,22.0561597323288,-40.3404232162477));
#23049=CARTESIAN_POINT('Ctrl Pts',(-26.3830378614903,22.0127669787064,-40.3376664425618));
#23050=CARTESIAN_POINT('Ctrl Pts',(-26.2898167477981,21.8470878184802,-40.3269452703998));
#23051=CARTESIAN_POINT('Ctrl Pts',(-26.2127272691422,21.7289331720181,-40.3188703249029));
#23052=CARTESIAN_POINT('Ctrl Pts',(-26.0948272382408,21.5717829548074,-40.3072157363963));
#23053=CARTESIAN_POINT('Ctrl Pts',(-26.0603549912444,21.5282269700936,-40.3038799579491));
#23054=CARTESIAN_POINT('Ctrl Pts',(-26.0203627061881,21.4802958303968,-40.3000792748139));
#23055=CARTESIAN_POINT('Ctrl Pts',(-26.0159323870267,21.4750205279814,-40.2996591599074));
#23056=CARTESIAN_POINT('Ctrl Pts',(-26.0086730255115,21.4664326704055,-40.2989722551929));
#23057=CARTESIAN_POINT('Ctrl Pts',(-26.0058541049344,21.4631115561181,-40.2987058809369));
#23058=CARTESIAN_POINT('Ctrl Pts',(-26.0003724684329,21.4566798379406,-40.2981885867273));
#23059=CARTESIAN_POINT('Ctrl Pts',(-25.9977105396042,21.4535685717934,-40.2979376995041));
#23060=CARTESIAN_POINT('Ctrl Pts',(-25.9930728243981,21.4481688700075,-40.2975011368674));
#23061=CARTESIAN_POINT('Ctrl Pts',(-25.9910997292911,21.4458781208396,-40.2973155731066));
#23062=CARTESIAN_POINT('Ctrl Pts',(-25.9869819964881,21.4411110453085,-40.2969286639918));
#23063=CARTESIAN_POINT('Ctrl Pts',(-25.9848368015399,21.4386352067335,-40.2967272955936));
#23064=CARTESIAN_POINT('Ctrl Pts',(-25.9795821933868,21.43258934533,-40.2962345280942));
#23065=CARTESIAN_POINT('Ctrl Pts',(-25.9764686879894,21.4290229027711,-40.2959429585393));
#23066=CARTESIAN_POINT('Ctrl Pts',(-25.9645421633474,21.415421976963,-40.2948276264822));
#23067=CARTESIAN_POINT('Ctrl Pts',(-25.9556747546757,21.4054355596711,-40.294001588334));
#23068=CARTESIAN_POINT('Ctrl Pts',(-25.9438943778807,21.3923335201162,-40.2929083217936));
#23069=CARTESIAN_POINT('Ctrl Pts',(-25.941036839078,21.3891680484706,-40.29264344752));
#23070=CARTESIAN_POINT('Ctrl Pts',(-25.7604561116888,21.1899241694814,-40.2759246704034));
#23071=CARTESIAN_POINT('Ctrl Pts',(-25.5593040574696,21.0165196869184,-40.2583799044899));
#23072=CARTESIAN_POINT('Ctrl Pts',(-25.276053420008,20.8274768284793,-40.2353463814289));
#23073=CARTESIAN_POINT('Ctrl Pts',(-25.2113509371624,20.7875277079221,-40.2301926783903));
#23074=CARTESIAN_POINT('Ctrl Pts',(-25.0715661907385,20.7079080676913,-40.2193464386802));
#23075=CARTESIAN_POINT('Ctrl Pts',(-24.9962021987853,20.6688382172622,-40.2136647681925));
#23076=CARTESIAN_POINT('Ctrl Pts',(-24.8719456507937,20.6105262815491,-40.2046484729325));
#23077=CARTESIAN_POINT('Ctrl Pts',(-24.8239721592532,20.5894245851671,-40.201248924994));
#23078=CARTESIAN_POINT('Ctrl Pts',(-24.7601364639828,20.5631846643062,-40.1968509746676));
#23079=CARTESIAN_POINT('Ctrl Pts',(-24.7447214051119,20.5569871389449,-40.1957984551897));
#23080=CARTESIAN_POINT('Ctrl Pts',(-24.7195310323174,20.5470851037085,-40.1940947209419));
#23081=CARTESIAN_POINT('Ctrl Pts',(-24.709784621622,20.5433085428342,-40.1934394599967));
#23082=CARTESIAN_POINT('Ctrl Pts',(-24.6977599725807,20.5387163643039,-40.1926360161078));
#23083=CARTESIAN_POINT('Ctrl Pts',(-24.6954991143757,20.5378558646967,-40.1924851701086));
#23084=CARTESIAN_POINT('Ctrl Pts',(-24.6911145042708,20.5361926987496,-40.1921930483267));
#23085=CARTESIAN_POINT('Ctrl Pts',(-24.6889908697662,20.5353897297539,-40.1920517544081));
#23086=CARTESIAN_POINT('Ctrl Pts',(-24.685138638256,20.5339378105854,-40.1917958000539));
#23087=CARTESIAN_POINT('Ctrl Pts',(-24.68341033856,20.5332881042552,-40.1916810942011));
#23088=CARTESIAN_POINT('Ctrl Pts',(-24.6799054108221,20.5319739605548,-40.1914487340515));
#23089=CARTESIAN_POINT('Ctrl Pts',(-24.678128761504,20.5313096089814,-40.1913310851819));
#23090=CARTESIAN_POINT('Ctrl Pts',(-24.6730228846216,20.5294054786565,-40.1909933601625));
#23091=CARTESIAN_POINT('Ctrl Pts',(-24.6696921788465,20.528169630791,-40.1907735210759));
#23092=CARTESIAN_POINT('Ctrl Pts',(-24.6551442317445,20.5227990116683,-40.1898153169774));
#23093=CARTESIAN_POINT('Ctrl Pts',(-24.6439058878432,20.5187210982591,-40.1890803249247));
#23094=CARTESIAN_POINT('Ctrl Pts',(-24.4500431854462,20.4495949983909,-40.1764871510084));
#23095=CARTESIAN_POINT('Ctrl Pts',(-24.2619072617459,20.4010824404704,-40.1655576380878));
#23096=CARTESIAN_POINT('Ctrl Pts',(-23.9194117925328,20.3450559118602,-40.1461324522901));
#23097=CARTESIAN_POINT('Ctrl Pts',(-23.76673065637,20.3311378554512,-40.1376331373063));
#23098=CARTESIAN_POINT('Ctrl Pts',(-23.5883020509026,20.3276274723848,-40.1274528576264));
#23099=CARTESIAN_POINT('Ctrl Pts',(-23.5629552083704,20.3274278941249,-40.1260011891407));
#23100=CARTESIAN_POINT('Ctrl Pts',(-23.4210353583722,20.327984679949,-40.1178350533521));
#23101=CARTESIAN_POINT('Ctrl Pts',(-23.304584291837,20.3347666136513,-40.1109861129622));
#23102=CARTESIAN_POINT('Ctrl Pts',(-23.1693525475861,20.350031537355,-40.1027503946933));
#23103=CARTESIAN_POINT('Ctrl Pts',(-23.1499606870289,20.3523992480943,-40.1015627158175));
#23104=CARTESIAN_POINT('Ctrl Pts',(-23.1262431227944,20.3555142291803,-40.1001015446441));
#23105=CARTESIAN_POINT('Ctrl Pts',(-23.1218955551241,20.3560942543528,-40.0998333508604));
#23106=CARTESIAN_POINT('Ctrl Pts',(-23.1134702466269,20.357235816851,-40.0993129191522));
#23107=CARTESIAN_POINT('Ctrl Pts',(-23.1093923689749,20.357796295112,-40.0990607151952));
#23108=CARTESIAN_POINT('Ctrl Pts',(-23.1023187221247,20.3587823343579,-40.09862268464));
#23109=CARTESIAN_POINT('Ctrl Pts',(-23.099322450921,20.3592043057354,-40.0984369720671));
#23110=CARTESIAN_POINT('Ctrl Pts',(-23.0930937173308,20.3600904597528,-40.0980505508678));
#23111=CARTESIAN_POINT('Ctrl Pts',(-23.0898613585859,20.3605553369116,-40.097849820402));
#23112=CARTESIAN_POINT('Ctrl Pts',(-23.0810139460352,20.3618414986518,-40.0972998432591));
#23113=CARTESIAN_POINT('Ctrl Pts',(-23.0754003658151,20.3626726996274,-40.0969502822247));
#23114=CARTESIAN_POINT('Ctrl Pts',(-23.0539459556236,20.3659073786006,-40.0956119611507));
#23115=CARTESIAN_POINT('Ctrl Pts',(-23.038121141403,20.3684141172482,-40.0946199265348));
#23116=CARTESIAN_POINT('Ctrl Pts',(-22.7773741527612,20.4117134654495,-40.0781916151624));
#23117=CARTESIAN_POINT('Ctrl Pts',(-22.5380074425618,20.4805492046857,-40.061808441389));
#23118=CARTESIAN_POINT('Ctrl Pts',(-22.1602701591182,20.6382039929131,-40.0341642434919));
#23119=CARTESIAN_POINT('Ctrl Pts',(-22.0164392940135,20.7113270832848,-40.0231871039986));
#23120=CARTESIAN_POINT('Ctrl Pts',(-21.8225074920731,20.8289787688683,-40.0081780160742));
#23121=CARTESIAN_POINT('Ctrl Pts',(-21.7673884618637,20.864767325848,-40.0038885083397));
#23122=CARTESIAN_POINT('Ctrl Pts',(-21.6900635048681,20.9184051065155,-39.9978773981317));
#23123=CARTESIAN_POINT('Ctrl Pts',(-21.6669426234804,20.9349001632806,-39.9960809289446));
#23124=CARTESIAN_POINT('Ctrl Pts',(-21.6404687670021,20.9543204887099,-39.9940278510597));
#23125=CARTESIAN_POINT('Ctrl Pts',(-21.6369010570518,20.9569489754713,-39.9937512544272));
#23126=CARTESIAN_POINT('Ctrl Pts',(-21.6314758351121,20.9609632620887,-39.9933307906694));
#23127=CARTESIAN_POINT('Ctrl Pts',(-21.6296143959316,20.9623437070684,-39.9931865515019));
#23128=CARTESIAN_POINT('Ctrl Pts',(-21.6262564594201,20.96483957435,-39.9929264002738));
#23129=CARTESIAN_POINT('Ctrl Pts',(-21.624759445966,20.9659542859416,-39.9928104389379));
#23130=CARTESIAN_POINT('Ctrl Pts',(-21.621761414811,20.9681907419793,-39.9925782416574));
#23131=CARTESIAN_POINT('Ctrl Pts',(-21.620260413109,20.9693124905376,-39.9924620068526));
#23132=CARTESIAN_POINT('Ctrl Pts',(-21.6160076320632,20.9724965199665,-39.9921327267443));
#23133=CARTESIAN_POINT('Ctrl Pts',(-21.6132581633257,20.9745619049072,-39.9919198999694));
#23134=CARTESIAN_POINT('Ctrl Pts',(-21.6017248823035,20.9832545501021,-39.99102736134));
#23135=CARTESIAN_POINT('Ctrl Pts',(-21.5929716003735,20.9899224744371,-39.9903504799354));
#23136=CARTESIAN_POINT('Ctrl Pts',(-21.4466027048217,21.1026101713468,-39.9790374519262));
#23137=CARTESIAN_POINT('Ctrl Pts',(-21.3177243421066,21.2195590048627,-39.9691515165728));
#23138=CARTESIAN_POINT('Ctrl Pts',(-21.0556571676399,21.49916037971,-39.9476349681803));
#23139=CARTESIAN_POINT('Ctrl Pts',(-20.9276705892199,21.6655653903238,-39.9360912263759));
#23140=CARTESIAN_POINT('Ctrl Pts',(-20.7733354955943,21.9127048323666,-39.9192658599859));
#23141=CARTESIAN_POINT('Ctrl Pts',(-20.7326053494256,21.9838255614106,-39.9144619955773));
#23142=CARTESIAN_POINT('Ctrl Pts',(-20.6754939923929,22.0929998259467,-39.9070929794505));
#23143=CARTESIAN_POINT('Ctrl Pts',(-20.6570621736822,22.1299457272625,-39.904600285239));
#23144=CARTESIAN_POINT('Ctrl Pts',(-20.636053319676,22.1741640976276,-39.9016146378716));
#23145=CARTESIAN_POINT('Ctrl Pts',(-20.6327856184943,22.1811056314392,-39.9011458783804));
#23146=CARTESIAN_POINT('Ctrl Pts',(-20.6278041554539,22.1917864961383,-39.900424481549));
#23147=CARTESIAN_POINT('Ctrl Pts',(-20.6260726979322,22.1955175830353,-39.9001724573281));
#23148=CARTESIAN_POINT('Ctrl Pts',(-20.6230800834447,22.2019987817099,-39.8997346276199));
#23149=CARTESIAN_POINT('Ctrl Pts',(-20.6218156444841,22.2047473798406,-39.8995489358337));
#23150=CARTESIAN_POINT('Ctrl Pts',(-20.6191938874503,22.2104676758951,-39.8991624500491));
#23151=CARTESIAN_POINT('Ctrl Pts',(-20.617837214419,22.2134396641982,-39.8989616340473));
#23152=CARTESIAN_POINT('Ctrl Pts',(-20.6145389230538,22.2206942287483,-39.8984714027439));
#23153=CARTESIAN_POINT('Ctrl Pts',(-20.6126021579517,22.2249789923167,-39.8981818205634));
#23154=CARTESIAN_POINT('Ctrl Pts',(-20.6052884030514,22.2412542400645,-39.8970817200948));
#23155=CARTESIAN_POINT('Ctrl Pts',(-20.5999754486934,22.253273205806,-39.8962690045195));
#23156=CARTESIAN_POINT('Ctrl Pts',(-20.509508474693,22.4613599985542,-39.8821918755898));
#23157=CARTESIAN_POINT('Ctrl Pts',(-20.444013136071,22.6653483051592,-39.8682386522577));
#23158=CARTESIAN_POINT('Ctrl Pts',(-20.3618525863434,23.0483411039515,-39.8419403043687));
#23159=CARTESIAN_POINT('Ctrl Pts',(-20.3389996104594,23.2251937547888,-39.8297744148685));
#23160=CARTESIAN_POINT('Ctrl Pts',(-20.3270334938343,23.4868580572614,-39.8123081553058));
#23161=CARTESIAN_POINT('Ctrl Pts',(-20.3264753292174,23.57081386154,-39.8067883555873));
#23162=CARTESIAN_POINT('Ctrl Pts',(-20.3302133716348,23.6860889507761,-39.7994054389666));
#23163=CARTESIAN_POINT('Ctrl Pts',(-20.3316899070629,23.7174606032992,-39.7974162820961));
#23164=CARTESIAN_POINT('Ctrl Pts',(-20.3339046919158,23.753340609348,-39.795168075968));
#23165=CARTESIAN_POINT('Ctrl Pts',(-20.334194121901,23.7578735786363,-39.794884535014));
#23166=CARTESIAN_POINT('Ctrl Pts',(-20.3346472320892,23.7647416900706,-39.794455687903));
#23167=CARTESIAN_POINT('Ctrl Pts',(-20.3348038730589,23.7670772666142,-39.7943099867682));
#23168=CARTESIAN_POINT('Ctrl Pts',(-20.3350780525419,23.7710997424826,-39.794059282733));
#23169=CARTESIAN_POINT('Ctrl Pts',(-20.3351943739232,23.7727867180712,-39.7939542108686));
#23170=CARTESIAN_POINT('Ctrl Pts',(-20.335438465745,23.7762865704525,-39.7937363717669));
#23171=CARTESIAN_POINT('Ctrl Pts',(-20.3355664415592,23.7780994259754,-39.7936236165767));
#23172=CARTESIAN_POINT('Ctrl Pts',(-20.3359209985551,23.7830621764835,-39.7933151656401));
#23173=CARTESIAN_POINT('Ctrl Pts',(-20.3361506770967,23.786211858943,-39.7931196454302));
#23174=CARTESIAN_POINT('Ctrl Pts',(-20.3370462209025,23.7982488922111,-39.7923733429715));
#23175=CARTESIAN_POINT('Ctrl Pts',(-20.3377443291862,23.8071339124758,-39.7918243642188));
#23176=CARTESIAN_POINT('Ctrl Pts',(-20.3499378417435,23.9544934827857,-39.7827492537357));
#23177=CARTESIAN_POINT('Ctrl Pts',(-20.370341955992,24.0921052883501,-39.7747088752091));
#23178=CARTESIAN_POINT('Ctrl Pts',(-20.4461861410096,24.4446931552396,-39.754268003905));
#23179=CARTESIAN_POINT('Ctrl Pts',(-20.5150332037432,24.656009666628,-39.742138835494));
#23180=CARTESIAN_POINT('Ctrl Pts',(-20.6580060693181,24.9778588574961,-39.7219850162191));
#23181=CARTESIAN_POINT('Ctrl Pts',(-20.718177191576,25.0937850009049,-39.7143531401263));
#23182=CARTESIAN_POINT('Ctrl Pts',(-20.7959372328057,25.2236626301882,-39.7051996612479));
#23183=CARTESIAN_POINT('Ctrl Pts',(-20.8068441001825,25.2414841152972,-39.7039300224255));
#23184=CARTESIAN_POINT('Ctrl Pts',(-20.8211630680579,25.2643778448708,-39.7022808678945));
#23185=CARTESIAN_POINT('Ctrl Pts',(-20.8244175488238,25.2695484733955,-39.7019071922724));
#23186=CARTESIAN_POINT('Ctrl Pts',(-20.8296801696184,25.277857076888,-39.7013047775619));
#23187=CARTESIAN_POINT('Ctrl Pts',(-20.8316790930147,25.2810008958957,-39.7010763813924));
#23188=CARTESIAN_POINT('Ctrl Pts',(-20.8354931096982,25.2869765042359,-39.7006413901369));
#23189=CARTESIAN_POINT('Ctrl Pts',(-20.837307194958,25.2898089337294,-39.700434832831));
#23190=CARTESIAN_POINT('Ctrl Pts',(-20.8414480063552,25.2962519750551,-39.6999641177813));
#23191=CARTESIAN_POINT('Ctrl Pts',(-20.8437775198776,25.299860780086,-39.6996998560868));
#23192=CARTESIAN_POINT('Ctrl Pts',(-20.8508842577332,25.3108221458232,-39.6988953241589));
#23193=CARTESIAN_POINT('Ctrl Pts',(-20.8556842507498,25.3181598317395,-39.6983542011337));
#23194=CARTESIAN_POINT('Ctrl Pts',(-20.8900549062457,25.3702366447541,-39.6944953684415));
#23195=CARTESIAN_POINT('Ctrl Pts',(-20.9207067849185,25.4142488256529,-39.6911369679976));
#23196=CARTESIAN_POINT('Ctrl Pts',(-20.9589469199173,25.466335422606,-39.6870400413801));
#23197=CARTESIAN_POINT('Ctrl Pts',(-20.9654980726549,25.4751636465597,-39.6863413099574));
#23198=CARTESIAN_POINT('Ctrl Pts',(-21.0113117009467,25.5362457419083,-39.6814765026779));
#23199=CARTESIAN_POINT('Ctrl Pts',(-21.0521084289258,25.5873251053595,-39.6772529959035));
#23200=CARTESIAN_POINT('Ctrl Pts',(-21.2251427188022,25.7909511895672,-39.6597711194017));
#23201=CARTESIAN_POINT('Ctrl Pts',(-21.3700103895921,25.9321413639984,-39.646068561947));
#23202=CARTESIAN_POINT('Ctrl Pts',(-21.6623120715856,26.1678788641579,-39.6206869424311));
#23203=CARTESIAN_POINT('Ctrl Pts',(-21.8061276032853,26.2658245013485,-39.6090450385963));
#23204=CARTESIAN_POINT('Ctrl Pts',(-21.9663039778016,26.3569116342803,-39.5974455962901));
#23205=CARTESIAN_POINT('Ctrl Pts',(-21.9754787399383,26.3620697113195,-39.5967857451467));
#23206=CARTESIAN_POINT('Ctrl Pts',(-21.9875110948863,26.3687569691971,-39.5959264823079));
#23207=CARTESIAN_POINT('Ctrl Pts',(-21.9903458194818,26.3703268413455,-39.5957244883641));
#23208=CARTESIAN_POINT('Ctrl Pts',(-21.9949796181568,26.3728839171312,-39.5953950241984));
#23209=CARTESIAN_POINT('Ctrl Pts',(-21.9967772670928,26.3738736776636,-39.595267389153));
#23210=CARTESIAN_POINT('Ctrl Pts',(-22.0002289989648,26.3757698592013,-39.5950226560652));
#23211=CARTESIAN_POINT('Ctrl Pts',(-22.001882927348,26.3766765424203,-39.5949055414335));
#23212=CARTESIAN_POINT('Ctrl Pts',(-22.0056861693659,26.3787571388064,-39.5946365801415));
#23213=CARTESIAN_POINT('Ctrl Pts',(-22.0078360309838,26.3799300572301,-39.5944847978675));
#23214=CARTESIAN_POINT('Ctrl Pts',(-22.0146560710465,26.3836408431977,-39.5940040936381));
#23215=CARTESIAN_POINT('Ctrl Pts',(-22.0193312229294,26.386169625166,-39.5936757534056));
#23216=CARTESIAN_POINT('Ctrl Pts',(-22.0409399380988,26.3977887359841,-39.5921635094053));
#23217=CARTESIAN_POINT('Ctrl Pts',(-22.0579484072219,26.4067390708759,-39.5909883551281));
#23218=CARTESIAN_POINT('Ctrl Pts',(-22.0750360153868,26.4155367745772,-39.5898217886697));
#23219=CARTESIAN_POINT('Origin',(-23.5502525316942,23.5502525316942,-77.3107734492734));
#23220=CARTESIAN_POINT('',(-22.0750360152969,26.415536774531,-38.0939694478973));
#23221=CARTESIAN_POINT('',(-22.0750360565132,26.4155367957515,-38.344122456765));
#23222=CARTESIAN_POINT('',(-22.0750360153461,26.4155367745563,-77.3107734492734));
#23223=CARTESIAN_POINT('',(-26.7730017872581,23.5524430253128,-38.936921602977));
#23224=CARTESIAN_POINT('Ctrl Pts',(-22.0750360152969,26.415536774531,-38.0939694478973));
#23225=CARTESIAN_POINT('Ctrl Pts',(-22.0709270299416,26.4134212276783,-38.0942379738773));
#23226=CARTESIAN_POINT('Ctrl Pts',(-22.0668223643516,26.4112967231257,-38.0945067643071));
#23227=CARTESIAN_POINT('Ctrl Pts',(-21.9751324508798,26.3635892031279,-38.1005233920934));
#23228=CARTESIAN_POINT('Ctrl Pts',(-21.8896913901989,26.3140181099801,-38.1063855786955));
#23229=CARTESIAN_POINT('Ctrl Pts',(-21.7988048027281,26.2555502581609,-38.1129634702086));
#23230=CARTESIAN_POINT('Ctrl Pts',(-21.7909656919704,26.2504589587677,-38.1135336850914));
#23231=CARTESIAN_POINT('Ctrl Pts',(-21.7793647659388,26.2428524944705,-38.1143818353013));
#23232=CARTESIAN_POINT('Ctrl Pts',(-21.7755858711397,26.2403633625005,-38.1146587936373));
#23233=CARTESIAN_POINT('Ctrl Pts',(-21.7691282865532,26.236090267628,-38.1151332480238));
#23234=CARTESIAN_POINT('Ctrl Pts',(-21.7664469959437,26.2343102305726,-38.1153305960743));
#23235=CARTESIAN_POINT('Ctrl Pts',(-21.7610128888376,26.2306909331183,-38.1157312637284));
#23236=CARTESIAN_POINT('Ctrl Pts',(-21.7582602320776,26.2288514418309,-38.11593459187));
#23237=CARTESIAN_POINT('Ctrl Pts',(-21.7519572955152,26.2246253752415,-38.1164010152609));
#23238=CARTESIAN_POINT('Ctrl Pts',(-21.7484089290834,26.2222359699319,-38.1166642174274));
#23239=CARTESIAN_POINT('Ctrl Pts',(-21.7409779281124,26.2172105356521,-38.1172167223357));
#23240=CARTESIAN_POINT('Ctrl Pts',(-21.7370962756336,26.2145730786207,-38.1175060789575));
#23241=CARTESIAN_POINT('Ctrl Pts',(-21.7268678973606,26.2075905227487,-38.1182705417728));
#23242=CARTESIAN_POINT('Ctrl Pts',(-21.7205309707127,26.2032311842765,-38.1187461900505));
#23243=CARTESIAN_POINT('Ctrl Pts',(-21.7016081185116,26.1901136091846,-38.1201726637776));
#23244=CARTESIAN_POINT('Ctrl Pts',(-21.6890691669111,26.1812882867504,-38.1211260535671));
#23245=CARTESIAN_POINT('Ctrl Pts',(-21.5489092520977,26.0811358525208,-38.1318760480398));
#23246=CARTESIAN_POINT('Ctrl Pts',(-21.4280791115379,25.98070765852,-38.1420314087641));
#23247=CARTESIAN_POINT('Ctrl Pts',(-21.0821440450911,25.647653310951,-38.1739234167877));
#23248=CARTESIAN_POINT('Ctrl Pts',(-20.8843151276914,25.389659725045,-38.1965121002003));
#23249=CARTESIAN_POINT('Ctrl Pts',(-20.7205405263816,25.0926851585918,-38.2179697241785));
#23250=CARTESIAN_POINT('Ctrl Pts',(-20.7129937831087,25.0787587500689,-38.2189659817496));
#23251=CARTESIAN_POINT('Ctrl Pts',(-20.7038549265296,25.0615934076616,-38.2201812071793));
#23252=CARTESIAN_POINT('Ctrl Pts',(-20.7021653481048,25.0584070214745,-38.2204062525793));
#23253=CARTESIAN_POINT('Ctrl Pts',(-20.6993923305966,25.0531560922515,-38.2207762210184));
#23254=CARTESIAN_POINT('Ctrl Pts',(-20.6983057828304,25.0510932095327,-38.2209213413679));
#23255=CARTESIAN_POINT('Ctrl Pts',(-20.6963530149324,25.0473759728002,-38.221182434114));
#23256=CARTESIAN_POINT('Ctrl Pts',(-20.6954859960088,25.0457220487599,-38.2212984574647));
#23257=CARTESIAN_POINT('Ctrl Pts',(-20.6936272148162,25.0421687333229,-38.221547410831));
#23258=CARTESIAN_POINT('Ctrl Pts',(-20.6926359118676,25.0402691114227,-38.2216803111981));
#23259=CARTESIAN_POINT('Ctrl Pts',(-20.6899324047292,25.0350757918172,-38.2220431245093));
#23260=CARTESIAN_POINT('Ctrl Pts',(-20.6882239888641,25.0317801091894,-38.2222727961594));
#23261=CARTESIAN_POINT('Ctrl Pts',(-20.6794656054694,25.0148127397329,-38.2234523385782));
#23262=CARTESIAN_POINT('Ctrl Pts',(-20.6725077366294,25.0010933553143,-38.2243964462812));
#23263=CARTESIAN_POINT('Ctrl Pts',(-20.6077230931501,24.8710524904951,-38.233259516684));
#23264=CARTESIAN_POINT('Ctrl Pts',(-20.5568732369388,24.7513691183257,-38.2407732282274));
#23265=CARTESIAN_POINT('Ctrl Pts',(-20.3953358254907,24.2965819194516,-38.2681403222025));
#23266=CARTESIAN_POINT('Ctrl Pts',(-20.3326472514567,23.9471472591325,-38.2871754025));
#23267=CARTESIAN_POINT('Ctrl Pts',(-20.3275065378465,23.572663417507,-38.3098055194338));
#23268=CARTESIAN_POINT('Ctrl Pts',(-20.3274286749555,23.5508362351364,-38.3111311815913));
#23269=CARTESIAN_POINT('Ctrl Pts',(-20.3276148685454,23.522588549216,-38.3128559052357));
#23270=CARTESIAN_POINT('Ctrl Pts',(-20.3276763923069,23.5161669221205,-38.3132486008971));
#23271=CARTESIAN_POINT('Ctrl Pts',(-20.3278048123216,23.5059505846615,-38.3138743347191));
#23272=CARTESIAN_POINT('Ctrl Pts',(-20.327859218912,23.5021557112028,-38.3141069804427));
#23273=CARTESIAN_POINT('Ctrl Pts',(-20.3279735285888,23.4950573769451,-38.3145425530568));
#23274=CARTESIAN_POINT('Ctrl Pts',(-20.3280318086554,23.4917538919533,-38.3147454287036));
#23275=CARTESIAN_POINT('Ctrl Pts',(-20.3281732709396,23.4843785060941,-38.3151987414645));
#23276=CARTESIAN_POINT('Ctrl Pts',(-20.3282590919795,23.4803066667307,-38.315449261137));
#23277=CARTESIAN_POINT('Ctrl Pts',(-20.3285314820217,23.4684498320328,-38.316179493546));
#23278=CARTESIAN_POINT('Ctrl Pts',(-20.3287385485403,23.4606653774087,-38.3166598492434));
#23279=CARTESIAN_POINT('Ctrl Pts',(-20.3292700634214,23.4430814729808,-38.3177470334374));
#23280=CARTESIAN_POINT('Ctrl Pts',(-20.3296110216558,23.433282633241,-38.3183543771412));
#23281=CARTESIAN_POINT('Ctrl Pts',(-20.3308341740776,23.4022109387528,-38.3202850638725));
#23282=CARTESIAN_POINT('Ctrl Pts',(-20.3318824503267,23.3809455358753,-38.3216136033708));
#23283=CARTESIAN_POINT('Ctrl Pts',(-20.3370068048824,23.2944341255461,-38.3270483924466));
#23284=CARTESIAN_POINT('Ctrl Pts',(-20.3428567434016,23.2293126301799,-38.3312095247524));
#23285=CARTESIAN_POINT('Ctrl Pts',(-20.3706662053572,22.9987001952099,-38.3462014970982));
#23286=CARTESIAN_POINT('Ctrl Pts',(-20.4034919239815,22.8348054631395,-38.357345225422));
#23287=CARTESIAN_POINT('Ctrl Pts',(-20.4859755520085,22.5427945099748,-38.3778456214333));
#23288=CARTESIAN_POINT('Ctrl Pts',(-20.5314112047669,22.4138707363317,-38.3871335951902));
#23289=CARTESIAN_POINT('Ctrl Pts',(-20.601209406924,22.2498683139141,-38.3990180872388));
#23290=CARTESIAN_POINT('Ctrl Pts',(-20.6182728260268,22.2118393960573,-38.4017783108198));
#23291=CARTESIAN_POINT('Ctrl Pts',(-20.6455219816844,22.1541336146427,-38.4059630508232));
#23292=CARTESIAN_POINT('Ctrl Pts',(-20.6551805242275,22.1342137896937,-38.4074069142896));
#23293=CARTESIAN_POINT('Ctrl Pts',(-20.6871831537003,22.0699077998681,-38.4120622380886));
#23294=CARTESIAN_POINT('Ctrl Pts',(-20.7103500417138,22.0259358591252,-38.4152364884836));
#23295=CARTESIAN_POINT('Ctrl Pts',(-20.7372414254265,21.9776377559863,-38.4186983803039));
#23296=CARTESIAN_POINT('Ctrl Pts',(-20.7399693380059,21.972768113658,-38.4190471406211));
#23297=CARTESIAN_POINT('Ctrl Pts',(-20.7438446490465,21.9658921876036,-38.4195391605764));
#23298=CARTESIAN_POINT('Ctrl Pts',(-20.7449815554936,21.9638800489896,-38.4196830908934));
#23299=CARTESIAN_POINT('Ctrl Pts',(-20.7470624248403,21.9602064824542,-38.4199457671533));
#23300=CARTESIAN_POINT('Ctrl Pts',(-20.7480057020834,21.9585446690951,-38.4200645575819));
#23301=CARTESIAN_POINT('Ctrl Pts',(-20.7499210982433,21.9551772107352,-38.4203051958952));
#23302=CARTESIAN_POINT('Ctrl Pts',(-20.7508932981427,21.953471614259,-38.4204270383075));
#23303=CARTESIAN_POINT('Ctrl Pts',(-20.7533066120163,21.9492467514526,-38.4207287541832));
#23304=CARTESIAN_POINT('Ctrl Pts',(-20.7547495754288,21.9467285351042,-38.4209085072216));
#23305=CARTESIAN_POINT('Ctrl Pts',(-20.7601162927693,21.9373919622969,-38.4215746639933));
#23306=CARTESIAN_POINT('Ctrl Pts',(-20.7640616479999,21.9305859577467,-38.4220596762919));
#23307=CARTESIAN_POINT('Ctrl Pts',(-20.865048068485,21.757838506748,-38.4343568082435));
#23308=CARTESIAN_POINT('Ctrl Pts',(-20.9767357585437,21.6008661500425,-38.4452296503135));
#23309=CARTESIAN_POINT('Ctrl Pts',(-21.2664802519023,21.2623123414656,-38.4701930482823));
#23310=CARTESIAN_POINT('Ctrl Pts',(-21.453287296292,21.0899657653491,-38.4841816101874));
#23311=CARTESIAN_POINT('Ctrl Pts',(-21.6668370944805,20.9351093184205,-38.4997867690571));
#23312=CARTESIAN_POINT('Ctrl Pts',(-21.6753643779828,20.9289890686908,-38.5004091605558));
#23313=CARTESIAN_POINT('Ctrl Pts',(-21.72723932311,20.8921397235655,-38.5041913350193));
#23314=CARTESIAN_POINT('Ctrl Pts',(-21.771309573592,20.8624463063867,-38.5073874554204));
#23315=CARTESIAN_POINT('Ctrl Pts',(-21.8234604792933,20.8291529015466,-38.5111579670032));
#23316=CARTESIAN_POINT('Ctrl Pts',(-21.8308482100331,20.8244787395931,-38.511691828201));
#23317=CARTESIAN_POINT('Ctrl Pts',(-21.8418894549863,20.8175557748403,-38.5124893348566));
#23318=CARTESIAN_POINT('Ctrl Pts',(-21.8455286319444,20.8152840872476,-38.5127521322715));
#23319=CARTESIAN_POINT('Ctrl Pts',(-21.8520284827236,20.8112446912064,-38.5132214073414));
#23320=CARTESIAN_POINT('Ctrl Pts',(-21.8548874131356,20.8094741777601,-38.5134277810098));
#23321=CARTESIAN_POINT('Ctrl Pts',(-21.8608579327841,20.8057895974676,-38.5138586965083));
#23322=CARTESIAN_POINT('Ctrl Pts',(-21.8639700143954,20.8038763411756,-38.5140832678213));
#23323=CARTESIAN_POINT('Ctrl Pts',(-21.8721251831407,20.7988817657189,-38.5146716542104));
#23324=CARTESIAN_POINT('Ctrl Pts',(-21.8771734878629,20.795809030336,-38.5150357841794));
#23325=CARTESIAN_POINT('Ctrl Pts',(-21.8882200107703,20.7891269518107,-38.5158323565103));
#23326=CARTESIAN_POINT('Ctrl Pts',(-21.8942215836132,20.7855232382096,-38.5162650032033));
#23327=CARTESIAN_POINT('Ctrl Pts',(-21.9118186765147,20.7750347165431,-38.5175332032106));
#23328=CARTESIAN_POINT('Ctrl Pts',(-21.9234456182678,20.7682031653377,-38.5183706936456));
#23329=CARTESIAN_POINT('Ctrl Pts',(-21.963392287403,20.7450680573231,-38.5212467302993));
#23330=CARTESIAN_POINT('Ctrl Pts',(-21.9919161873216,20.7291227790547,-38.523298118158));
#23331=CARTESIAN_POINT('Ctrl Pts',(-22.1189053503157,20.6606475147691,-38.5324236795815));
#23332=CARTESIAN_POINT('Ctrl Pts',(-22.2198084383479,20.612824103726,-38.5396594003099));
#23333=CARTESIAN_POINT('Ctrl Pts',(-22.6380989874006,20.440552052251,-38.5695577646503));
#23334=CARTESIAN_POINT('Ctrl Pts',(-22.9717726182782,20.3615851558951,-38.5934515420524));
#23335=CARTESIAN_POINT('Ctrl Pts',(-23.3144541107854,20.3361391478788,-38.6151715652336));
#23336=CARTESIAN_POINT('Ctrl Pts',(-23.3173060645698,20.3359311907415,-38.6153521174194));
#23337=CARTESIAN_POINT('Ctrl Pts',(-23.3325205941522,20.3348421418486,-38.6163141789226));
#23338=CARTESIAN_POINT('Ctrl Pts',(-23.3448881268445,20.3340285586392,-38.6170921890727));
#23339=CARTESIAN_POINT('Ctrl Pts',(-23.3608562733654,20.3330705975283,-38.6180912415476));
#23340=CARTESIAN_POINT('Ctrl Pts',(-23.3644526447544,20.3328608952116,-38.6183158922679));
#23341=CARTESIAN_POINT('Ctrl Pts',(-23.3699530967615,20.3325494204645,-38.6186589287064));
#23342=CARTESIAN_POINT('Ctrl Pts',(-23.3718569134409,20.3324433077522,-38.6187775589311));
#23343=CARTESIAN_POINT('Ctrl Pts',(-23.3754354823829,20.332247035324,-38.6190003536484));
#23344=CARTESIAN_POINT('Ctrl Pts',(-23.3771102041661,20.3321564936849,-38.6191045392542));
#23345=CARTESIAN_POINT('Ctrl Pts',(-23.3809662197221,20.3319510420467,-38.6193442422244));
#23346=CARTESIAN_POINT('Ctrl Pts',(-23.3831475561887,20.331837042526,-38.6194797073406));
#23347=CARTESIAN_POINT('Ctrl Pts',(-23.3892242340005,20.3315256618876,-38.6198567110566));
#23348=CARTESIAN_POINT('Ctrl Pts',(-23.3931198369066,20.3313331335601,-38.6200979756529));
#23349=CARTESIAN_POINT('Ctrl Pts',(-23.4149260377442,20.3302951087031,-38.6214461703602));
#23350=CARTESIAN_POINT('Ctrl Pts',(-23.432843561434,20.3295920040264,-38.6225451885319));
#23351=CARTESIAN_POINT('Ctrl Pts',(-23.4847049261458,20.3279902845939,-38.6257033198866));
#23352=CARTESIAN_POINT('Ctrl Pts',(-23.5186593060064,20.3274784859633,-38.627742602826));
#23353=CARTESIAN_POINT('Ctrl Pts',(-23.6489224329086,20.327574053701,-38.6354788098027));
#23354=CARTESIAN_POINT('Ctrl Pts',(-23.7451844692565,20.3319615494773,-38.6410133377783));
#23355=CARTESIAN_POINT('Ctrl Pts',(-23.8708419267743,20.3433488686657,-38.6481604673383));
#23356=CARTESIAN_POINT('Ctrl Pts',(-23.9005329352196,20.3464559796316,-38.6498434572126));
#23357=CARTESIAN_POINT('Ctrl Pts',(-23.9549486958095,20.3529160040897,-38.6529236396775));
#23358=CARTESIAN_POINT('Ctrl Pts',(-23.9796857356447,20.3561443627306,-38.6543222325836));
#23359=CARTESIAN_POINT('Ctrl Pts',(-24.0256459794075,20.3626860761626,-38.6569212921574));
#23360=CARTESIAN_POINT('Ctrl Pts',(-24.0468782863967,20.365925019757,-38.6581221973717));
#23361=CARTESIAN_POINT('Ctrl Pts',(-24.0866552913762,20.3724004341239,-38.6603746233747));
#23362=CARTESIAN_POINT('Ctrl Pts',(-24.1052070535752,20.3755876117693,-38.6614262183962));
#23363=CARTESIAN_POINT('Ctrl Pts',(-24.2930132355238,20.4095490974281,-38.6720906220807));
#23364=CARTESIAN_POINT('Ctrl Pts',(-24.4595648318882,20.4536646830282,-38.6817217188843));
#23365=CARTESIAN_POINT('Ctrl Pts',(-24.7133213184869,20.5431263193665,-38.6973954523031));
#23366=CARTESIAN_POINT('Ctrl Pts',(-24.8033411230658,20.5795113506491,-38.7031605223613));
#23367=CARTESIAN_POINT('Ctrl Pts',(-24.900038843731,20.6237732309721,-38.7096337815531));
#23368=CARTESIAN_POINT('Ctrl Pts',(-24.9084846825761,20.6276835235829,-38.7102015549486));
#23369=CARTESIAN_POINT('Ctrl Pts',(-24.9210024574019,20.633545040314,-38.7110466518537));
#23370=CARTESIAN_POINT('Ctrl Pts',(-24.9250874743176,20.6354683494081,-38.7113230080222));
#23371=CARTESIAN_POINT('Ctrl Pts',(-24.9320748997358,20.6387761284917,-38.7117966969004));
#23372=CARTESIAN_POINT('Ctrl Pts',(-24.9349793110448,20.6401563735472,-38.7119938826647));
#23373=CARTESIAN_POINT('Ctrl Pts',(-24.940801325696,20.6429338221945,-38.7123897361764));
#23374=CARTESIAN_POINT('Ctrl Pts',(-24.9437189002218,20.6443310759816,-38.7125884054716));
#23375=CARTESIAN_POINT('Ctrl Pts',(-24.9495844178916,20.6471509921107,-38.712988410093));
#23376=CARTESIAN_POINT('Ctrl Pts',(-24.9525323067969,20.6485737574201,-38.7131897488243));
#23377=CARTESIAN_POINT('Ctrl Pts',(-24.9619282086737,20.6531262455882,-38.7138324580012));
#23378=CARTESIAN_POINT('Ctrl Pts',(-24.968367917015,20.6562729728153,-38.7142744220959));
#23379=CARTESIAN_POINT('Ctrl Pts',(-25.0062857236675,20.6749582468026,-38.7168854950162));
#23380=CARTESIAN_POINT('Ctrl Pts',(-25.037517721745,20.6909882945055,-38.7190717920934));
#23381=CARTESIAN_POINT('Ctrl Pts',(-25.127583706784,20.7390902328692,-38.725483780976));
#23382=CARTESIAN_POINT('Ctrl Pts',(-25.1856841218339,20.7724891232371,-38.7297559170129));
#23383=CARTESIAN_POINT('Ctrl Pts',(-25.3018723350526,20.8441888503961,-38.7385842224833));
#23384=CARTESIAN_POINT('Ctrl Pts',(-25.3598457257626,20.8826086231841,-38.743142740589));
#23385=CARTESIAN_POINT('Ctrl Pts',(-25.6718270883493,21.1042145419277,-38.7685065363326));
#23386=CARTESIAN_POINT('Ctrl Pts',(-25.8993107503608,21.3217797425351,-38.7903415970462));
#23387=CARTESIAN_POINT('Ctrl Pts',(-26.0945902405359,21.572252729701,-38.8106777682662));
#23388=CARTESIAN_POINT('Ctrl Pts',(-26.0973347423982,21.5757880965304,-38.81096391692));
#23389=CARTESIAN_POINT('Ctrl Pts',(-26.1032759194925,21.5834743053425,-38.8115840773288));
#23390=CARTESIAN_POINT('Ctrl Pts',(-26.1064698635435,21.5876272583711,-38.8119179268595));
#23391=CARTESIAN_POINT('Ctrl Pts',(-26.1149622516928,21.5987254569065,-38.8128067763762));
#23392=CARTESIAN_POINT('Ctrl Pts',(-26.1202426527369,21.6056845454561,-38.8133606751812));
#23393=CARTESIAN_POINT('Ctrl Pts',(-26.1262792062198,21.6137077124307,-38.8139952307614));
#23394=CARTESIAN_POINT('Ctrl Pts',(-26.1270630211751,21.6147507966916,-38.8140776506099));
#23395=CARTESIAN_POINT('Ctrl Pts',(-26.1359709452535,21.6266202746976,-38.8150146328091));
#23396=CARTESIAN_POINT('Ctrl Pts',(-26.1440275744639,21.6374974984242,-38.8158648613245));
#23397=CARTESIAN_POINT('Ctrl Pts',(-26.1541884732738,21.6513979474395,-38.8169403930653));
#23398=CARTESIAN_POINT('Ctrl Pts',(-26.1563562623996,21.6543742483854,-38.8171700435305));
#23399=CARTESIAN_POINT('Ctrl Pts',(-26.1597862583037,21.6591005157023,-38.8175337023592));
#23400=CARTESIAN_POINT('Ctrl Pts',(-26.1610518083004,21.6608480341763,-38.8176679435231));
#23401=CARTESIAN_POINT('Ctrl Pts',(-26.1634085349553,21.6641091790254,-38.8179180462281));
#23402=CARTESIAN_POINT('Ctrl Pts',(-26.1645001449014,21.6656224722222,-38.8180339377072));
#23403=CARTESIAN_POINT('Ctrl Pts',(-26.1669409214777,21.6690123091645,-38.8182931696697));
#23404=CARTESIAN_POINT('Ctrl Pts',(-26.1682893810629,21.6708893524445,-38.8184364604693));
#23405=CARTESIAN_POINT('Ctrl Pts',(-26.172252968614,21.6764191738728,-38.8188578605596));
#23406=CARTESIAN_POINT('Ctrl Pts',(-26.1748624931291,21.6800759905597,-38.8191355811265));
#23407=CARTESIAN_POINT('Ctrl Pts',(-26.1946258169644,21.7078938539758,-38.8212411515043));
#23408=CARTESIAN_POINT('Ctrl Pts',(-26.211454036139,21.732286010094,-38.8230469090003));
#23409=CARTESIAN_POINT('Ctrl Pts',(-26.2675138870268,21.8159904945888,-38.8291198742974));
#23410=CARTESIAN_POINT('Ctrl Pts',(-26.3051203927875,21.8763712069852,-38.8332932196779));
#23411=CARTESIAN_POINT('Ctrl Pts',(-26.4851727929966,22.1879921757956,-38.8540616426538));
#23412=CARTESIAN_POINT('Ctrl Pts',(-26.5953876040318,22.4563216130441,-38.869605038021));
#23413=CARTESIAN_POINT('Ctrl Pts',(-26.6731340114945,22.7539595137322,-38.8873491113756));
#23414=CARTESIAN_POINT('Ctrl Pts',(-26.6777279599063,22.7721980760058,-38.8884377699653));
#23415=CARTESIAN_POINT('Ctrl Pts',(-26.6880924048193,22.8149218026988,-38.89099219322));
#23416=CARTESIAN_POINT('Ctrl Pts',(-26.6937363310034,22.8394361639169,-38.8924611382815));
#23417=CARTESIAN_POINT('Ctrl Pts',(-26.7012419324503,22.8738759769489,-38.8945308265083));
#23418=CARTESIAN_POINT('Ctrl Pts',(-26.7033449037185,22.883748264714,-38.8951247950048));
#23419=CARTESIAN_POINT('Ctrl Pts',(-26.7195435886887,22.9615848847503,-38.8998137319719));
#23420=CARTESIAN_POINT('Ctrl Pts',(-26.7314857770043,23.0299743964491,-38.9039694122927));
#23421=CARTESIAN_POINT('Ctrl Pts',(-26.7424026479158,23.1071186682467,-38.9087149389453));
#23422=CARTESIAN_POINT('Ctrl Pts',(-26.743561671773,23.115549507629,-38.9092343240731));
#23423=CARTESIAN_POINT('Ctrl Pts',(-26.7452580762712,23.1282623000011,-38.9100186819118));
#23424=CARTESIAN_POINT('Ctrl Pts',(-26.745820277752,23.1325409498791,-38.9102828688248));
#23425=CARTESIAN_POINT('Ctrl Pts',(-26.7467796422115,23.1399575177152,-38.9107411613539));
#23426=CARTESIAN_POINT('Ctrl Pts',(-26.7471807836753,23.1430949229658,-38.910935140868));
#23427=CARTESIAN_POINT('Ctrl Pts',(-26.7479783796296,23.1494069264842,-38.9113256219343));
#23428=CARTESIAN_POINT('Ctrl Pts',(-26.7483747268683,23.1525815340213,-38.9115221266142));
#23429=CARTESIAN_POINT('Ctrl Pts',(-26.7491719705486,23.159045468068,-38.9119224693054));
#23430=CARTESIAN_POINT('Ctrl Pts',(-26.7495725221486,23.1623348323563,-38.9121263179657));
#23431=CARTESIAN_POINT('Ctrl Pts',(-26.7504850836596,23.1699264252955,-38.9125970695511));
#23432=CARTESIAN_POINT('Ctrl Pts',(-26.7509934915757,23.1742290732365,-38.9128640860952));
#23433=CARTESIAN_POINT('Ctrl Pts',(-26.7522813691773,23.1853202392472,-38.9135529389263));
#23434=CARTESIAN_POINT('Ctrl Pts',(-26.7530479247396,23.1921102090388,-38.9139751827672));
#23435=CARTESIAN_POINT('Ctrl Pts',(-26.7666711062891,23.3163237018742,-38.9217094353355));
#23436=CARTESIAN_POINT('Ctrl Pts',(-26.7730820564623,23.4343474892183,-38.9292245611143));
#23437=CARTESIAN_POINT('Ctrl Pts',(-26.7730017872581,23.5524430253128,-38.936921602977));
#23438=CARTESIAN_POINT('Ctrl Pts',(-26.7730017900261,23.5524389491122,-38.936921337305));
#23439=CARTESIAN_POINT('Ctrl Pts',(-26.7727891409872,23.8658807131493,-38.9573503324916));
#23440=CARTESIAN_POINT('Ctrl Pts',(-26.7268561765285,24.1775704728378,-38.9791096181834));
#23441=CARTESIAN_POINT('Ctrl Pts',(-26.6160288655546,24.5463820947226,-39.0044493874676));
#23442=CARTESIAN_POINT('Ctrl Pts',(-26.5931064491004,24.6143486286855,-39.009090152085));
#23443=CARTESIAN_POINT('Ctrl Pts',(-26.5639619025229,24.6920937661945,-39.0143204808516));
#23444=CARTESIAN_POINT('Ctrl Pts',(-26.559934520511,24.7026673493275,-39.0150301143754));
#23445=CARTESIAN_POINT('Ctrl Pts',(-26.5546481129803,24.7163296619211,-39.0159446246109));
#23446=CARTESIAN_POINT('Ctrl Pts',(-26.5534399273114,24.7194377820012,-39.0161525092692));
#23447=CARTESIAN_POINT('Ctrl Pts',(-26.5514781975387,24.7244613298895,-39.0164882363002));
#23448=CARTESIAN_POINT('Ctrl Pts',(-26.5507276428001,24.7263779105439,-39.0166162590548));
#23449=CARTESIAN_POINT('Ctrl Pts',(-26.5492865537635,24.7300474488885,-39.0168612512661));
#23450=CARTESIAN_POINT('Ctrl Pts',(-26.5485963205605,24.7318005146165,-39.0169782381755));
#23451=CARTESIAN_POINT('Ctrl Pts',(-26.5470102381166,24.735818533241,-39.017246248575));
#23452=CARTESIAN_POINT('Ctrl Pts',(-26.5461133561898,24.7380830816349,-39.0173972091676));
#23453=CARTESIAN_POINT('Ctrl Pts',(-26.5432769482755,24.7452211156974,-39.0178727726439));
#23454=CARTESIAN_POINT('Ctrl Pts',(-26.5413280786034,24.7500909160648,-39.0181968113259));
#23455=CARTESIAN_POINT('Ctrl Pts',(-26.525202563625,24.7901016052808,-39.0208559667316));
#23456=CARTESIAN_POINT('Ctrl Pts',(-26.5104182975749,24.8249965703154,-39.0231549691498));
#23457=CARTESIAN_POINT('Ctrl Pts',(-26.4934706601035,24.8631116924203,-39.0256523947349));
#23458=CARTESIAN_POINT('Ctrl Pts',(-26.4919138992812,24.8665961517352,-39.0258805801986));
#23459=CARTESIAN_POINT('Ctrl Pts',(-26.4310819913155,25.0021078691367,-39.0347501266444));
#23460=CARTESIAN_POINT('Ctrl Pts',(-26.3629799280313,25.1300107468675,-39.0429536562685));
#23461=CARTESIAN_POINT('Ctrl Pts',(-26.1965200527715,25.3975189945531,-39.0606290746895));
#23462=CARTESIAN_POINT('Ctrl Pts',(-26.0952190336246,25.5347598284421,-39.0700494660762));
#23463=CARTESIAN_POINT('Ctrl Pts',(-25.9492366651927,25.7028628382718,-39.0827526571655));
#23464=CARTESIAN_POINT('Ctrl Pts',(-25.9139686199556,25.7415311348619,-39.0857630114142));
#23465=CARTESIAN_POINT('Ctrl Pts',(-25.8295374576346,25.8296914466893,-39.092862098233));
#23466=CARTESIAN_POINT('Ctrl Pts',(-25.7796796035239,25.8784783461387,-39.0969746071866));
#23467=CARTESIAN_POINT('Ctrl Pts',(-25.7016089436013,25.9500634947489,-39.1033270409454));
#23468=CARTESIAN_POINT('Ctrl Pts',(-25.6745277880891,25.9740680240629,-39.1055154604634));
#23469=CARTESIAN_POINT('Ctrl Pts',(-25.6415560549796,26.0023168571015,-39.1081643955096));
#23470=CARTESIAN_POINT('Ctrl Pts',(-25.6360473262915,26.0070044434521,-39.1086064539987));
#23471=CARTESIAN_POINT('Ctrl Pts',(-25.6280177702024,26.0137906244364,-39.109250080421));
#23472=CARTESIAN_POINT('Ctrl Pts',(-25.6255094185427,26.0159040022403,-39.1094510410873));
#23473=CARTESIAN_POINT('Ctrl Pts',(-25.6205260466589,26.020089683396,-39.1098500928349));
#23474=CARTESIAN_POINT('Ctrl Pts',(-25.6180511303116,26.0221621049034,-39.1100481787474));
#23475=CARTESIAN_POINT('Ctrl Pts',(-25.6131121708935,26.0262852351134,-39.1104432891441));
#23476=CARTESIAN_POINT('Ctrl Pts',(-25.6106481731128,26.0283359927861,-39.1106403113213));
#23477=CARTESIAN_POINT('Ctrl Pts',(-25.6047348379815,26.0332426786641,-39.1111129200721));
#23478=CARTESIAN_POINT('Ctrl Pts',(-25.601282606284,26.0360950950138,-39.111388649283));
#23479=CARTESIAN_POINT('Ctrl Pts',(-25.5907528557781,26.0447584644402,-39.1122291140262));
#23480=CARTESIAN_POINT('Ctrl Pts',(-25.5836565506183,26.0505464172475,-39.1127947809014));
#23481=CARTESIAN_POINT('Ctrl Pts',(-25.5057535982969,26.1135353245246,-39.1189967396267));
#23482=CARTESIAN_POINT('Ctrl Pts',(-25.4325850893556,26.1677369212249,-39.1247524097535));
#23483=CARTESIAN_POINT('Ctrl Pts',(-25.2498357968397,26.2914849517779,-39.138986452077));
#23484=CARTESIAN_POINT('Ctrl Pts',(-25.1381642111273,26.357647894685,-39.1475729565328));
#23485=CARTESIAN_POINT('Ctrl Pts',(-24.9393873411553,26.4597576695493,-39.1625837392987));
#23486=CARTESIAN_POINT('Ctrl Pts',(-24.8541237161061,26.4989530784927,-39.1689401571942));
#23487=CARTESIAN_POINT('Ctrl Pts',(-24.5982850129614,26.6032924428686,-39.187635652949));
#23488=CARTESIAN_POINT('Ctrl Pts',(-24.4237251158533,26.6577413547762,-39.1999287861783));
#23489=CARTESIAN_POINT('Ctrl Pts',(-24.2299462023557,26.7005520439217,-39.2124813394223));
#23490=CARTESIAN_POINT('Ctrl Pts',(-24.2143910110535,26.7038680136092,-39.2134813542311));
#23491=CARTESIAN_POINT('Ctrl Pts',(-24.1951351060878,26.7078240850156,-39.2147093436109));
#23492=CARTESIAN_POINT('Ctrl Pts',(-24.1914573414103,26.708572977982,-39.2149434353068));
#23493=CARTESIAN_POINT('Ctrl Pts',(-24.1856689499649,26.7097411245297,-39.215311157281));
#23494=CARTESIAN_POINT('Ctrl Pts',(-24.1835592120875,26.7101646889385,-39.2154450348809));
#23495=CARTESIAN_POINT('Ctrl Pts',(-24.1796187297119,26.7109517003872,-39.2156948062384));
#23496=CARTESIAN_POINT('Ctrl Pts',(-24.1777881058823,26.7113156676249,-39.2158107292045));
#23497=CARTESIAN_POINT('Ctrl Pts',(-24.1736823269789,26.7121282772582,-39.2160704723937));
#23498=CARTESIAN_POINT('Ctrl Pts',(-24.1714070082653,26.7125760534678,-39.2162142420374));
#23499=CARTESIAN_POINT('Ctrl Pts',(-24.1656313986041,26.7137062029615,-39.2165787475968));
#23500=CARTESIAN_POINT('Ctrl Pts',(-24.1621304443666,26.7143852249228,-39.2167992911714));
#23501=CARTESIAN_POINT('Ctrl Pts',(-24.1429533793866,26.7180716635112,-39.2180051700298));
#23502=CARTESIAN_POINT('Ctrl Pts',(-24.1272558567958,26.7209684657301,-39.2189842572234));
#23503=CARTESIAN_POINT('Ctrl Pts',(-23.8073921281599,26.7775415842178,-39.2387843016447));
#23504=CARTESIAN_POINT('Ctrl Pts',(-23.4970366042432,26.7873434470794,-39.2553438885612));
#23505=CARTESIAN_POINT('Ctrl Pts',(-23.0649052344691,26.7387316725795,-39.2799150309674));
#23506=CARTESIAN_POINT('Ctrl Pts',(-22.9407654334487,26.7173461815343,-39.2871362177386));
#23507=CARTESIAN_POINT('Ctrl Pts',(-22.7762798230726,26.6789802059643,-39.2971246565931));
#23508=CARTESIAN_POINT('Ctrl Pts',(-22.7345597127801,26.668363430544,-39.2996946121722));
#23509=CARTESIAN_POINT('Ctrl Pts',(-22.6771076645535,26.6525113323316,-39.3032899199832));
#23510=CARTESIAN_POINT('Ctrl Pts',(-22.6611835555385,26.6479852453151,-39.3042924719312));
#23511=CARTESIAN_POINT('Ctrl Pts',(-22.6374843367405,26.6410514603901,-39.3057938222366));
#23512=CARTESIAN_POINT('Ctrl Pts',(-22.6296821643339,26.6387366246081,-39.3062896000534));
#23513=CARTESIAN_POINT('Ctrl Pts',(-22.6154953640493,26.6344689923783,-39.3071938651611));
#23514=CARTESIAN_POINT('Ctrl Pts',(-22.60910785923,26.6325258555983,-39.3076020349696));
#23515=CARTESIAN_POINT('Ctrl Pts',(-22.5990628602071,26.6294359402407,-39.3082455638051));
#23516=CARTESIAN_POINT('Ctrl Pts',(-22.5954012700646,26.6283024537349,-39.3084804859153));
#23517=CARTESIAN_POINT('Ctrl Pts',(-22.588853234784,26.626262627164,-39.3089012168007));
#23518=CARTESIAN_POINT('Ctrl Pts',(-22.5859660226315,26.6253587483755,-39.3090869444046));
#23519=CARTESIAN_POINT('Ctrl Pts',(-22.5798475825342,26.6234338280926,-39.3094809884327));
#23520=CARTESIAN_POINT('Ctrl Pts',(-22.5766166856722,26.6224117536565,-39.3096893386938));
#23521=CARTESIAN_POINT('Ctrl Pts',(-22.5673956480093,26.6194787277068,-39.3102847539681));
#23522=CARTESIAN_POINT('Ctrl Pts',(-22.5614095039608,26.61755534715,-39.310672228431));
#23523=CARTESIAN_POINT('Ctrl Pts',(-22.5357663752409,26.6092332022219,-39.3123361397588));
#23524=CARTESIAN_POINT('Ctrl Pts',(-22.5161659239285,26.6026630152079,-39.3136182299218));
#23525=CARTESIAN_POINT('Ctrl Pts',(-22.4922984392233,26.5944062256511,-39.3151922875919));
#23526=CARTESIAN_POINT('Ctrl Pts',(-22.4879697002519,26.592898380274,-39.3154782862847));
#23527=CARTESIAN_POINT('Ctrl Pts',(-22.3434652145688,26.5422166439851,-39.3250430756226));
#23528=CARTESIAN_POINT('Ctrl Pts',(-22.2069428185356,26.4834501520747,-39.3346403576747));
#23529=CARTESIAN_POINT('Ctrl Pts',(-22.0750358008163,26.4155366641038,-39.3444748119239));
#23530=CARTESIAN_POINT('Ctrl Pts',(-22.0750360153868,26.4155367745772,-39.5898217886697));
#23531=CARTESIAN_POINT('Ctrl Pts',(-22.0932423762876,26.4249104778562,-39.5885788452598));
#23532=CARTESIAN_POINT('Ctrl Pts',(-22.1115385781612,26.4341109096722,-39.5873456507141));
#23533=CARTESIAN_POINT('Ctrl Pts',(-22.1727952271205,26.4641863197141,-39.5832654164282));
#23534=CARTESIAN_POINT('Ctrl Pts',(-22.2161331629954,26.4842812843866,-39.5804575944052));
#23535=CARTESIAN_POINT('Ctrl Pts',(-22.3103876959713,26.5254647822196,-39.5744857489971));
#23536=CARTESIAN_POINT('Ctrl Pts',(-22.3614308422891,26.5462258643955,-39.5713341283085));
#23537=CARTESIAN_POINT('Ctrl Pts',(-22.512876291122,26.6033437788414,-39.5621557844431));
#23538=CARTESIAN_POINT('Ctrl Pts',(-22.6145825408525,26.6360325766563,-39.5562085348476));
#23539=CARTESIAN_POINT('Ctrl Pts',(-22.8619347815826,26.7021756726782,-39.5418976600202));
#23540=CARTESIAN_POINT('Ctrl Pts',(-23.008641590572,26.730669814653,-39.533526120418));
#23541=CARTESIAN_POINT('Ctrl Pts',(-23.2331159947678,26.7582825133143,-39.5204270958889));
#23542=CARTESIAN_POINT('Ctrl Pts',(-23.3097524252681,26.7649360772788,-39.5159068653008));
#23543=CARTESIAN_POINT('Ctrl Pts',(-23.4252767611635,26.7708118473049,-39.5089798669498));
#23544=CARTESIAN_POINT('Ctrl Pts',(-23.4640351215891,26.7720823854119,-39.5066369571666));
#23545=CARTESIAN_POINT('Ctrl Pts',(-23.5103790111826,26.7727647554029,-39.5038100036337));
#23546=CARTESIAN_POINT('Ctrl Pts',(-23.5179526148532,26.7728495656743,-39.5033472059705));
#23547=CARTESIAN_POINT('Ctrl Pts',(-23.5296072448996,26.7729389869574,-39.5026337581692));
#23548=CARTESIAN_POINT('Ctrl Pts',(-23.5336881341118,26.7729625461531,-39.5023837031664));
#23549=CARTESIAN_POINT('Ctrl Pts',(-23.5411134306535,26.7729913086406,-39.501928280077));
#23550=CARTESIAN_POINT('Ctrl Pts',(-23.5444578271249,26.7729990573871,-39.5017229922026));
#23551=CARTESIAN_POINT('Ctrl Pts',(-23.5511676688409,26.7730041589964,-39.5013107956578));
#23552=CARTESIAN_POINT('Ctrl Pts',(-23.5545331098365,26.7730014460947,-39.5011038851784));
#23553=CARTESIAN_POINT('Ctrl Pts',(-23.5640700551311,26.7729788195566,-39.5005170712636));
#23554=CARTESIAN_POINT('Ctrl Pts',(-23.5702414904978,26.772946450004,-39.5001367771977));
#23555=CARTESIAN_POINT('Ctrl Pts',(-23.5961264173647,26.7727363257548,-39.4985393192452));
#23556=CARTESIAN_POINT('Ctrl Pts',(-23.6158378276935,26.7723954145451,-39.497317044365));
#23557=CARTESIAN_POINT('Ctrl Pts',(-23.641491330684,26.771716241464,-39.4957184982719));
#23558=CARTESIAN_POINT('Ctrl Pts',(-23.647437658205,26.7715423358291,-39.4953474187107));
#23559=CARTESIAN_POINT('Ctrl Pts',(-23.661674775309,26.7710865017822,-39.4944576353208));
#23560=CARTESIAN_POINT('Ctrl Pts',(-23.6699649932557,26.7707890248447,-39.4939384469682));
#23561=CARTESIAN_POINT('Ctrl Pts',(-23.6829113594129,26.7702744142369,-39.4931259702669));
#23562=CARTESIAN_POINT('Ctrl Pts',(-23.6875683836914,26.7700791799857,-39.4928333672754));
#23563=CARTESIAN_POINT('Ctrl Pts',(-23.6956196694502,26.7697241505006,-39.4923269077802));
#23564=CARTESIAN_POINT('Ctrl Pts',(-23.6990141411132,26.7695690884279,-39.4921131988973));
#23565=CARTESIAN_POINT('Ctrl Pts',(-23.7037934309529,26.7693431917235,-39.4918120469891));
#23566=CARTESIAN_POINT('Ctrl Pts',(-23.705178467019,26.7692768310413,-39.4917247428162));
#23567=CARTESIAN_POINT('Ctrl Pts',(-23.9995241773085,26.7549835521879,-39.4731645087463));
#23568=CARTESIAN_POINT('Ctrl Pts',(-24.2891177986754,26.700831920194,-39.4533464569585));
#23569=CARTESIAN_POINT('Ctrl Pts',(-24.7321004770689,26.553502542047,-39.4217922953102));
#23570=CARTESIAN_POINT('Ctrl Pts',(-24.8922091912962,26.4854601227076,-39.410152826775));
#23571=CARTESIAN_POINT('Ctrl Pts',(-25.0553817782095,26.3999567288016,-39.3985564710867));
#23572=CARTESIAN_POINT('Ctrl Pts',(-25.0646689085598,26.3950321548831,-39.3978974588925));
#23573=CARTESIAN_POINT('Ctrl Pts',(-25.0767855816174,26.3885310412153,-39.3970391480163));
#23574=CARTESIAN_POINT('Ctrl Pts',(-25.0796369392056,26.3869956262303,-39.3968372739275));
#23575=CARTESIAN_POINT('Ctrl Pts',(-25.084291130095,26.3844803544605,-39.3965079432199));
#23576=CARTESIAN_POINT('Ctrl Pts',(-25.0860953416799,26.3835030740568,-39.3963803220784));
#23577=CARTESIAN_POINT('Ctrl Pts',(-25.0895563054749,26.3816241096321,-39.3961355984569));
#23578=CARTESIAN_POINT('Ctrl Pts',(-25.091213194494,26.3807226968873,-39.3960184794185));
#23579=CARTESIAN_POINT('Ctrl Pts',(-25.0950199253506,26.3786473524187,-39.3957494845215));
#23580=CARTESIAN_POINT('Ctrl Pts',(-25.0971692260515,26.3774724211297,-39.395597673103));
#23581=CARTESIAN_POINT('Ctrl Pts',(-25.1039803009785,26.3737390040052,-39.3951167849742));
#23582=CARTESIAN_POINT('Ctrl Pts',(-25.1086371142829,26.3711714128528,-39.3947882906196));
#23583=CARTESIAN_POINT('Ctrl Pts',(-25.1480604752523,26.3493074430281,-39.3920096607518));
#23584=CARTESIAN_POINT('Ctrl Pts',(-25.1824754282531,26.3293796231635,-39.3895993330433));
#23585=CARTESIAN_POINT('Ctrl Pts',(-25.2228016290224,26.305021310973,-39.3867826003589));
#23586=CARTESIAN_POINT('Ctrl Pts',(-25.2290756856143,26.3012022458936,-39.3863445871515));
#23587=CARTESIAN_POINT('Ctrl Pts',(-25.2364305515811,26.2966907513715,-39.3858313131038));
#23588=CARTESIAN_POINT('Ctrl Pts',(-25.2375240170949,26.2960191175163,-39.3857550084788));
#23589=CARTESIAN_POINT('Ctrl Pts',(-25.333492935482,26.236993633428,-39.3790584865481));
#23590=CARTESIAN_POINT('Ctrl Pts',(-25.4252886273435,26.1737555604773,-39.3726876067116));
#23591=CARTESIAN_POINT('Ctrl Pts',(-25.5746244884009,26.0590274272147,-39.3620627561516));
#23592=CARTESIAN_POINT('Ctrl Pts',(-25.6339209491184,26.0100004073171,-39.357767846591));
#23593=CARTESIAN_POINT('Ctrl Pts',(-25.8242447276136,25.8408129330366,-39.3435391570483));
#23594=CARTESIAN_POINT('Ctrl Pts',(-25.9470789984944,25.711947146339,-39.3335997846822));
#23595=CARTESIAN_POINT('Ctrl Pts',(-26.0933666167257,25.5305920858653,-39.3200190247008));
#23596=CARTESIAN_POINT('Ctrl Pts',(-26.126962173982,25.4866773058263,-39.3167604256944));
#23597=CARTESIAN_POINT('Ctrl Pts',(-26.1855328362358,25.4058914676214,-39.3108010774403));
#23598=CARTESIAN_POINT('Ctrl Pts',(-26.2109051593026,25.3693252179693,-39.3081161342583));
#23599=CARTESIAN_POINT('Ctrl Pts',(-26.2397644743913,25.3258375729456,-39.3049329174268));
#23600=CARTESIAN_POINT('Ctrl Pts',(-26.2439946899147,25.3194133248484,-39.3044629268465));
#23601=CARTESIAN_POINT('Ctrl Pts',(-26.2504297221017,25.3095641282728,-39.3037427324284));
#23602=CARTESIAN_POINT('Ctrl Pts',(-26.2526511322236,25.3061500107823,-39.3034931509501));
#23603=CARTESIAN_POINT('Ctrl Pts',(-26.2566844740497,25.2999253257613,-39.3030382253907));
#23604=CARTESIAN_POINT('Ctrl Pts',(-26.2584985177404,25.2971161279234,-39.3028329606348));
#23605=CARTESIAN_POINT('Ctrl Pts',(-26.2621319694266,25.2914701617539,-39.3024205003739));
#23606=CARTESIAN_POINT('Ctrl Pts',(-26.2639513064707,25.2886333529373,-39.3022133025649));
#23607=CARTESIAN_POINT('Ctrl Pts',(-26.2691021359829,25.2805741100404,-39.3016247798802));
#23608=CARTESIAN_POINT('Ctrl Pts',(-26.2724230120537,25.2753449379825,-39.3012430606711));
#23609=CARTESIAN_POINT('Ctrl Pts',(-26.2863492143308,25.2532758905025,-39.2996326182813));
#23610=CARTESIAN_POINT('Ctrl Pts',(-26.2968133345332,25.2363478270673,-39.2983986804764));
#23611=CARTESIAN_POINT('Ctrl Pts',(-26.4823487884561,24.9298920755265,-39.276080840194));
#23612=CARTESIAN_POINT('Ctrl Pts',(-26.6108687141934,24.6147254472101,-39.2531208396004));
#23613=CARTESIAN_POINT('Ctrl Pts',(-26.7062238952158,24.2077720078999,-39.2249467055564));
#23614=CARTESIAN_POINT('Ctrl Pts',(-26.7215394973034,24.1294134797271,-39.2196027893835));
#23615=CARTESIAN_POINT('Ctrl Pts',(-26.7450395194514,23.9798734724943,-39.2096430367205));
#23616=CARTESIAN_POINT('Ctrl Pts',(-26.7537919121531,23.9088265248681,-39.2050118618062));
#23617=CARTESIAN_POINT('Ctrl Pts',(-26.7611793656268,23.8262853865113,-39.1997915080681));
#23618=CARTESIAN_POINT('Ctrl Pts',(-26.7621275677949,23.8150241905454,-39.1990827309674));
#23619=CARTESIAN_POINT('Ctrl Pts',(-26.7632787348086,23.8004350483455,-39.1981691535799));
#23620=CARTESIAN_POINT('Ctrl Pts',(-26.7635357838307,23.7971116318246,-39.1979613529638));
#23621=CARTESIAN_POINT('Ctrl Pts',(-26.7639432008042,23.7917356189463,-39.1976257239533));
#23622=CARTESIAN_POINT('Ctrl Pts',(-26.7640967587815,23.7896832778982,-39.1974977153865));
#23623=CARTESIAN_POINT('Ctrl Pts',(-26.7643871408432,23.7857516341098,-39.1972527242374));
#23624=CARTESIAN_POINT('Ctrl Pts',(-26.7645242823066,23.7838723643227,-39.1971357242475));
#23625=CARTESIAN_POINT('Ctrl Pts',(-26.7648349807767,23.7795627521495,-39.1968676483867));
#23626=CARTESIAN_POINT('Ctrl Pts',(-26.7650074302428,23.7771323269742,-39.1967166355008));
#23627=CARTESIAN_POINT('Ctrl Pts',(-26.7655427103242,23.7694651784681,-39.1962407709202));
#23628=CARTESIAN_POINT('Ctrl Pts',(-26.7658955052301,23.7642277287888,-39.19591648442));
#23629=CARTESIAN_POINT('Ctrl Pts',(-26.7686960197496,23.7210805491599,-39.193251180697));
#23630=CARTESIAN_POINT('Ctrl Pts',(-26.7704861910868,23.6831291144767,-39.1909464627932));
#23631=CARTESIAN_POINT('Ctrl Pts',(-26.7717150203731,23.6414170278344,-39.1884481962684));
#23632=CARTESIAN_POINT('Ctrl Pts',(-26.7718185798421,23.6376809538629,-39.188224737885));
#23633=CARTESIAN_POINT('Ctrl Pts',(-26.7719484703991,23.6326809201674,-39.187926081204));
#23634=CARTESIAN_POINT('Ctrl Pts',(-26.7719805569873,23.6314171283385,-39.1878506279693));
#23635=CARTESIAN_POINT('Ctrl Pts',(-26.7722456878373,23.6207265223034,-39.1872126447667));
#23636=CARTESIAN_POINT('Ctrl Pts',(-26.7724381032979,23.6112986429933,-39.1866519056317));
#23637=CARTESIAN_POINT('Ctrl Pts',(-26.7726452285354,23.5983683715461,-39.185885281006));
#23638=CARTESIAN_POINT('Ctrl Pts',(-26.7726956116885,23.5948666896791,-39.1856779132015));
#23639=CARTESIAN_POINT('Ctrl Pts',(-26.7727895913231,23.5875003399322,-39.1852421819196));
#23640=CARTESIAN_POINT('Ctrl Pts',(-26.7728319437466,23.5836356589857,-39.1850138694899));
#23641=CARTESIAN_POINT('Ctrl Pts',(-26.7729526730352,23.570455253057,-39.1842361747661));
#23642=CARTESIAN_POINT('Ctrl Pts',(-26.7729976092543,23.5611391940742,-39.1836881261123));
#23643=CARTESIAN_POINT('Ctrl Pts',(-26.7730486752823,23.4563455716258,-39.1775403865788));
#23644=CARTESIAN_POINT('Ctrl Pts',(-26.7688522351414,23.3609065026718,-39.1721002447795));
#23645=CARTESIAN_POINT('Ctrl Pts',(-26.7402590594943,23.0382326593435,-39.1538455788826));
#23646=CARTESIAN_POINT('Ctrl Pts',(-26.6959581266797,22.813475199057,-39.1413157819931));
#23647=CARTESIAN_POINT('Ctrl Pts',(-26.5937217524624,22.4839492165254,-39.1213777090175));
#23648=CARTESIAN_POINT('Ctrl Pts',(-26.5531658202046,22.3745762778425,-39.1144919655493));
#23649=CARTESIAN_POINT('Ctrl Pts',(-26.5025603998996,22.2579258944259,-39.1067546974105));
#23650=CARTESIAN_POINT('Ctrl Pts',(-26.4982945552024,22.2482240721448,-39.1061081773821));
#23651=CARTESIAN_POINT('Ctrl Pts',(-26.4922346207983,22.2346244081838,-39.1051976104198));
#23652=CARTESIAN_POINT('Ctrl Pts',(-26.4904804511666,22.2307087646117,-39.1049349355158));
#23653=CARTESIAN_POINT('Ctrl Pts',(-26.4874221406496,22.2239184050482,-39.1044785370549));
#23654=CARTESIAN_POINT('Ctrl Pts',(-26.4861215826788,22.2210420733241,-39.1042849370573));
#23655=CARTESIAN_POINT('Ctrl Pts',(-26.4834060626907,22.2150598208892,-39.1038817112614));
#23656=CARTESIAN_POINT('Ctrl Pts',(-26.4819903893174,22.2119542295871,-39.1036720611305));
#23657=CARTESIAN_POINT('Ctrl Pts',(-26.4786440768848,22.2046441467181,-39.1031778154211));
#23658=CARTESIAN_POINT('Ctrl Pts',(-26.4767093157951,22.2004415604487,-39.1028930776483));
#23659=CARTESIAN_POINT('Ctrl Pts',(-26.47034901248,22.1867039968745,-39.1019603595255));
#23660=CARTESIAN_POINT('Ctrl Pts',(-26.465885901955,22.1771865791904,-39.101311078936));
#23661=CARTESIAN_POINT('Ctrl Pts',(-26.4031269685584,22.0450412420135,-39.0922525295016));
#23662=CARTESIAN_POINT('Ctrl Pts',(-26.3371929966061,21.9262120128547,-39.083574323288));
#23663=CARTESIAN_POINT('Ctrl Pts',(-26.1603722218138,21.6501784685629,-39.0620637524151));
#23664=CARTESIAN_POINT('Ctrl Pts',(-26.042530731541,21.4980482048361,-39.049027721206));
#23665=CARTESIAN_POINT('Ctrl Pts',(-25.8083654898574,21.2458700797627,-39.0257643943012));
#23666=CARTESIAN_POINT('Ctrl Pts',(-25.69709503596,21.1418651779893,-39.0155550452248));
#23667=CARTESIAN_POINT('Ctrl Pts',(-25.5757858851582,21.0435917876213,-39.0055631286601));
#23668=CARTESIAN_POINT('Ctrl Pts',(-25.5726838864335,21.0410883546052,-39.0053083481025));
#23669=CARTESIAN_POINT('Ctrl Pts',(-25.5656343491558,21.035420670997,-39.0047309924384));
#23670=CARTESIAN_POINT('Ctrl Pts',(-25.5616839760502,21.0322599377526,-39.0044086295388));
#23671=CARTESIAN_POINT('Ctrl Pts',(-25.550677867339,21.0234962683389,-39.0035137874245));
#23672=CARTESIAN_POINT('Ctrl Pts',(-25.5436059895911,21.0179135468737,-39.0029425607112));
#23673=CARTESIAN_POINT('Ctrl Pts',(-25.5251747178205,21.0034884793743,-39.0014636893473));
#23674=CARTESIAN_POINT('Ctrl Pts',(-25.5137791653583,20.9946923275849,-39.0005590428813));
#23675=CARTESIAN_POINT('Ctrl Pts',(-25.499326542693,20.9836901885431,-38.9994242929052));
#23676=CARTESIAN_POINT('Ctrl Pts',(-25.4963242607295,20.9814129906899,-38.9991892481636));
#23677=CARTESIAN_POINT('Ctrl Pts',(-25.4915805624859,20.977828036794,-38.9988189509027));
#23678=CARTESIAN_POINT('Ctrl Pts',(-25.4898418148762,20.9765167803526,-38.9986834511783));
#23679=CARTESIAN_POINT('Ctrl Pts',(-25.4866118939054,20.9740861047065,-38.9984321708902));
#23680=CARTESIAN_POINT('Ctrl Pts',(-25.4851210872734,20.9729662240006,-38.9983163578943));
#23681=CARTESIAN_POINT('Ctrl Pts',(-25.4818003558064,20.970476225221,-38.9980587612886));
#23682=CARTESIAN_POINT('Ctrl Pts',(-25.4799699490454,20.9691067633343,-38.9979170244393));
#23683=CARTESIAN_POINT('Ctrl Pts',(-25.4746347209277,20.9651239341897,-38.9975046212025));
#23684=CARTESIAN_POINT('Ctrl Pts',(-25.4711260192739,20.962515736515,-38.9972343187156));
#23685=CARTESIAN_POINT('Ctrl Pts',(-25.4462009303649,20.9440662686637,-38.9953205314022));
#23686=CARTESIAN_POINT('Ctrl Pts',(-25.4245933479867,20.928483322992,-38.9936948383992));
#23687=CARTESIAN_POINT('Ctrl Pts',(-25.3742452377572,20.8931139508161,-38.9899768912755));
#23688=CARTESIAN_POINT('Ctrl Pts',(-25.345371257397,20.8735224746188,-38.9878962927704));
#23689=CARTESIAN_POINT('Ctrl Pts',(-25.2507200066345,20.8115206530372,-38.9812216896764));
#23690=CARTESIAN_POINT('Ctrl Pts',(-25.1837117962571,20.7710342353063,-38.97671980131));
#23691=CARTESIAN_POINT('Ctrl Pts',(-24.8016863189287,20.5588096233239,-38.951903108673));
#23692=CARTESIAN_POINT('Ctrl Pts',(-24.4612266344838,20.4381874504242,-38.9325812485604));
#23693=CARTESIAN_POINT('Ctrl Pts',(-24.087748730154,20.3725751907067,-38.9096500643141));
#23694=CARTESIAN_POINT('Ctrl Pts',(-24.067582021627,20.369229800607,-38.9084079163962));
#23695=CARTESIAN_POINT('Ctrl Pts',(-24.0411998473406,20.3651108571395,-38.9067773781893));
#23696=CARTESIAN_POINT('Ctrl Pts',(-24.0350117230723,20.3641631922019,-38.9063945261255));
#23697=CARTESIAN_POINT('Ctrl Pts',(-24.0254750845162,20.3627311537633,-38.9058038798318));
#23698=CARTESIAN_POINT('Ctrl Pts',(-24.0221284789622,20.3622340092059,-38.9055964911678));
#23699=CARTESIAN_POINT('Ctrl Pts',(-24.0154736029002,20.36125612323,-38.905183851314));
#23700=CARTESIAN_POINT('Ctrl Pts',(-24.0121653546962,20.3607752575779,-38.9049786043428));
#23701=CARTESIAN_POINT('Ctrl Pts',(-24.0049265917876,20.3597345762591,-38.9045292460742));
#23702=CARTESIAN_POINT('Ctrl Pts',(-24.0009957828965,20.3591768750941,-38.9042850680633));
#23703=CARTESIAN_POINT('Ctrl Pts',(-23.9898145414582,20.3576115581056,-38.9035900214863));
#23704=CARTESIAN_POINT('Ctrl Pts',(-23.9825617271207,20.3566213844266,-38.9031386009302));
#23705=CARTESIAN_POINT('Ctrl Pts',(-23.9662991876153,20.3544575922485,-38.9021251012972));
#23706=CARTESIAN_POINT('Ctrl Pts',(-23.9572877731582,20.3532973514679,-38.9015626017115));
#23707=CARTESIAN_POINT('Ctrl Pts',(-23.7642331733247,20.3292705960213,-38.8894923430329));
#23708=CARTESIAN_POINT('Ctrl Pts',(-23.5785951476054,20.3222984865728,-38.8774724276307));
#23709=CARTESIAN_POINT('Ctrl Pts',(-23.135048398545,20.3439096130843,-38.8478493236458));
#23710=CARTESIAN_POINT('Ctrl Pts',(-22.8791498539228,20.3875564603773,-38.8299819763953));
#23711=CARTESIAN_POINT('Ctrl Pts',(-22.6268057410478,20.4626345424977,-38.8128087988759));
#23712=CARTESIAN_POINT('Ctrl Pts',(-22.6223891570548,20.4639589000362,-38.8125084032396));
#23713=CARTESIAN_POINT('Ctrl Pts',(-22.6152632715626,20.4661123478861,-38.812024029301));
#23714=CARTESIAN_POINT('Ctrl Pts',(-22.6125522086587,20.4669355362774,-38.8118398171331));
#23715=CARTESIAN_POINT('Ctrl Pts',(-22.6065830618418,20.468756611695,-38.8114343813186));
#23716=CARTESIAN_POINT('Ctrl Pts',(-22.6033254635168,20.4697560942601,-38.8112132226204));
#23717=CARTESIAN_POINT('Ctrl Pts',(-22.551863483497,20.4856347867528,-38.8077211652514));
#23718=CARTESIAN_POINT('Ctrl Pts',(-22.5040099610582,20.5016397635422,-38.8044975096326));
#23719=CARTESIAN_POINT('Ctrl Pts',(-22.4517385317311,20.520498299976,-38.8010173840174));
#23720=CARTESIAN_POINT('Ctrl Pts',(-22.4469323844136,20.5222452057141,-38.8006977880717));
#23721=CARTESIAN_POINT('Ctrl Pts',(-22.4397866227068,20.5248617706211,-38.8002232130513));
#23722=CARTESIAN_POINT('Ctrl Pts',(-22.4374438571534,20.5257227093614,-38.8000677177786));
#23723=CARTESIAN_POINT('Ctrl Pts',(-22.4334274688164,20.5272039830913,-38.7998013075428));
#23724=CARTESIAN_POINT('Ctrl Pts',(-22.4317533616541,20.52782298662,-38.7996903126786));
#23725=CARTESIAN_POINT('Ctrl Pts',(-22.4284823478305,20.5290355385796,-38.799473540385));
#23726=CARTESIAN_POINT('Ctrl Pts',(-22.4268854016135,20.5296289609801,-38.7993677559942));
#23727=CARTESIAN_POINT('Ctrl Pts',(-22.4230151135705,20.5310706469291,-38.7991114925794));
#23728=CARTESIAN_POINT('Ctrl Pts',(-22.4207422523699,20.5319202141542,-38.7989610923702));
#23729=CARTESIAN_POINT('Ctrl Pts',(-22.4137314264188,20.5345498015775,-38.7984974506926));
#23730=CARTESIAN_POINT('Ctrl Pts',(-22.4089966644922,20.536338427813,-38.7981847252591));
#23731=CARTESIAN_POINT('Ctrl Pts',(-22.3557718815407,20.5565882831664,-38.7946735295146));
#23732=CARTESIAN_POINT('Ctrl Pts',(-22.3077268482433,20.5762080898295,-38.7915436464208));
#23733=CARTESIAN_POINT('Ctrl Pts',(-22.207509093983,20.6199862666761,-38.7850569635846));
#23734=CARTESIAN_POINT('Ctrl Pts',(-22.1554667641143,20.6443974588126,-38.7817131058483));
#23735=CARTESIAN_POINT('Ctrl Pts',(-21.7564467706001,20.8447550983272,-38.7560618987133));
#23736=CARTESIAN_POINT('Ctrl Pts',(-21.4432808432482,21.0808065500301,-38.7354008162317));
#23737=CARTESIAN_POINT('Ctrl Pts',(-21.166264554272,21.3815864747838,-38.7106641527116));
#23738=CARTESIAN_POINT('Ctrl Pts',(-21.1529599503505,21.3963028120065,-38.7094584087346));
#23739=CARTESIAN_POINT('Ctrl Pts',(-21.135685705938,21.4157683119338,-38.7078690852102));
#23740=CARTESIAN_POINT('Ctrl Pts',(-21.1315924744366,21.4204076155015,-38.7074907013341));
#23741=CARTESIAN_POINT('Ctrl Pts',(-21.1252913105234,21.4275909982777,-38.7069054356348));
#23742=CARTESIAN_POINT('Ctrl Pts',(-21.1230739495771,21.4301268184397,-38.7066989474958));
#23743=CARTESIAN_POINT('Ctrl Pts',(-21.1186632261384,21.4351870020044,-38.7062871357867));
#23744=CARTESIAN_POINT('Ctrl Pts',(-21.1164698088574,21.4377113122944,-38.706081814864));
#23745=CARTESIAN_POINT('Ctrl Pts',(-21.1116658369091,21.4432574104965,-38.7056309575757));
#23746=CARTESIAN_POINT('Ctrl Pts',(-21.1090569644764,21.4462806423617,-38.705385351923));
#23747=CARTESIAN_POINT('Ctrl Pts',(-21.1016265954841,21.4549235801813,-38.7046836578551));
#23748=CARTESIAN_POINT('Ctrl Pts',(-21.0968188619471,21.4605550375067,-38.7042270019769));
#23749=CARTESIAN_POINT('Ctrl Pts',(-21.0860627788269,21.4732422786722,-38.7031993862068));
#23750=CARTESIAN_POINT('Ctrl Pts',(-21.0801252614929,21.4803071228846,-38.7026279858899));
#23751=CARTESIAN_POINT('Ctrl Pts',(-20.9346536369767,21.6549159517201,-38.6885254399982));
#23752=CARTESIAN_POINT('Ctrl Pts',(-20.8124781729958,21.8361302177024,-38.674274671901));
#23753=CARTESIAN_POINT('Ctrl Pts',(-20.5888384101235,22.253538310913,-38.6424530666805));
#23754=CARTESIAN_POINT('Ctrl Pts',(-20.4953589859098,22.4923880830987,-38.6248339770699));
#23755=CARTESIAN_POINT('Ctrl Pts',(-20.4289638884117,22.7479150490506,-38.6079130829125));
#23756=CARTESIAN_POINT('Ctrl Pts',(-20.426881611823,22.7560596515223,-38.6073757882279));
#23757=CARTESIAN_POINT('Ctrl Pts',(-20.4187807501092,22.7882699738928,-38.6052591834939));
#23758=CARTESIAN_POINT('Ctrl Pts',(-20.4130080408678,22.8123975095682,-38.6036919675688));
#23759=CARTESIAN_POINT('Ctrl Pts',(-20.406595243375,22.8406373960494,-38.6018808046979));
#23760=CARTESIAN_POINT('Ctrl Pts',(-20.4056840016763,22.8446864131629,-38.6016216754846));
#23761=CARTESIAN_POINT('Ctrl Pts',(-20.4042428745779,22.8511481748732,-38.6012090314488));
#23762=CARTESIAN_POINT('Ctrl Pts',(-20.4037079409947,22.8535597706917,-38.6010552273767));
#23763=CARTESIAN_POINT('Ctrl Pts',(-20.4027687313411,22.857817076903,-38.6007840635495));
#23764=CARTESIAN_POINT('Ctrl Pts',(-20.4023633053635,22.8596625293318,-38.6006666371014));
#23765=CARTESIAN_POINT('Ctrl Pts',(-20.4015230093326,22.8635035754098,-38.6004224759807));
#23766=CARTESIAN_POINT('Ctrl Pts',(-20.4010884141573,22.865499222229,-38.6002957575149));
#23767=CARTESIAN_POINT('Ctrl Pts',(-20.3999643607833,22.8706845424272,-38.5999668567238));
#23768=CARTESIAN_POINT('Ctrl Pts',(-20.3992778474872,22.8738748623933,-38.5997648448158));
#23769=CARTESIAN_POINT('Ctrl Pts',(-20.3963676842562,22.8874993739185,-38.5989035991954));
#23770=CARTESIAN_POINT('Ctrl Pts',(-20.3941909739352,22.8979436859525,-38.5982470423296));
#23771=CARTESIAN_POINT('Ctrl Pts',(-20.360075847711,23.0658042439155,-38.5877507659688));
#23772=CARTESIAN_POINT('Ctrl Pts',(-20.3398931067016,23.2254060633344,-38.5785542679436));
#23773=CARTESIAN_POINT('Ctrl Pts',(-20.3160933883911,23.6913918255792,-38.552281188942));
#23774=CARTESIAN_POINT('Ctrl Pts',(-20.3440673797946,23.9975471959323,-38.5355747057476));
#23775=CARTESIAN_POINT('Ctrl Pts',(-20.415308618021,24.2974135211587,-38.5171371937451));
#23776=CARTESIAN_POINT('Ctrl Pts',(-20.4158443398733,24.2996577445527,-38.5169990967291));
#23777=CARTESIAN_POINT('Ctrl Pts',(-20.4174801052446,24.3064777857092,-38.5165790954939));
#23778=CARTESIAN_POINT('Ctrl Pts',(-20.4185877589123,24.3110517570495,-38.5162969577598));
#23779=CARTESIAN_POINT('Ctrl Pts',(-20.4224628120379,24.3269016397078,-38.5153176817106));
#23780=CARTESIAN_POINT('Ctrl Pts',(-20.4252811017223,24.3381649150901,-38.5146189711511));
#23781=CARTESIAN_POINT('Ctrl Pts',(-20.4293296674554,24.3539815162727,-38.5136337349374));
#23782=CARTESIAN_POINT('Ctrl Pts',(-20.4305091918925,24.3585478357641,-38.5133488157572));
#23783=CARTESIAN_POINT('Ctrl Pts',(-20.4367996007471,24.3826811460373,-38.5118404494558));
#23784=CARTESIAN_POINT('Ctrl Pts',(-20.442084469958,24.4022019563733,-38.5106114983937));
#23785=CARTESIAN_POINT('Ctrl Pts',(-20.4492382432972,24.4276730734682,-38.508995889728));
#23786=CARTESIAN_POINT('Ctrl Pts',(-20.4509412653042,24.4336698153914,-38.5086146448955));
#23787=CARTESIAN_POINT('Ctrl Pts',(-20.4535939263364,24.4429083754428,-38.5080259340157));
#23788=CARTESIAN_POINT('Ctrl Pts',(-20.4545312878063,24.4461537279864,-38.5078188692428));
#23789=CARTESIAN_POINT('Ctrl Pts',(-20.4564065506702,24.4526082190238,-38.5074065293576));
#23790=CARTESIAN_POINT('Ctrl Pts',(-20.4573443469707,24.4558173838672,-38.5072012579016));
#23791=CARTESIAN_POINT('Ctrl Pts',(-20.4594089869835,24.462842018948,-38.5067513684569));
#23792=CARTESIAN_POINT('Ctrl Pts',(-20.4605379041815,24.4666568695458,-38.5065066828386));
#23793=CARTESIAN_POINT('Ctrl Pts',(-20.4637719750084,24.4775115715444,-38.5058094130951));
#23794=CARTESIAN_POINT('Ctrl Pts',(-20.4658941350117,24.4845462934012,-38.5053562719896));
#23795=CARTESIAN_POINT('Ctrl Pts',(-20.47070837086,24.5003097732951,-38.5043380271204));
#23796=CARTESIAN_POINT('Ctrl Pts',(-20.4734135288772,24.5090344405901,-38.5037724958873));
#23797=CARTESIAN_POINT('Ctrl Pts',(-20.4819653883701,24.5362069294395,-38.5020049991495));
#23798=CARTESIAN_POINT('Ctrl Pts',(-20.4879411037314,24.5546134031521,-38.5007987964809));
#23799=CARTESIAN_POINT('Ctrl Pts',(-20.5109360472797,24.6233291898409,-38.4962617079172));
#23800=CARTESIAN_POINT('Ctrl Pts',(-20.5290315062651,24.6732668611825,-38.4928956075717));
#23801=CARTESIAN_POINT('Ctrl Pts',(-20.5686608925694,24.7747300028441,-38.4859109089954));
#23802=CARTESIAN_POINT('Ctrl Pts',(-20.5903166641487,24.826188605418,-38.4822893721913));
#23803=CARTESIAN_POINT('Ctrl Pts',(-20.7551474692525,25.1910508948088,-38.4560472467813));
#23804=CARTESIAN_POINT('Ctrl Pts',(-20.9464020619259,25.4802129667489,-38.4319036663617));
#23805=CARTESIAN_POINT('Ctrl Pts',(-21.2026393636181,25.7584120557744,-38.4076428558123));
#23806=CARTESIAN_POINT('Ctrl Pts',(-21.2258881765836,25.7828713168629,-38.4055023383247));
#23807=CARTESIAN_POINT('Ctrl Pts',(-21.2530684231166,25.810581809001,-38.4030732725928));
#23808=CARTESIAN_POINT('Ctrl Pts',(-21.2566274413075,25.8141931705223,-38.402756625475));
#23809=CARTESIAN_POINT('Ctrl Pts',(-21.2619034981501,25.819521612122,-38.4022893260839));
#23810=CARTESIAN_POINT('Ctrl Pts',(-21.2636139562817,25.8212451526063,-38.402138158058));
#23811=CARTESIAN_POINT('Ctrl Pts',(-21.2666504141445,25.8242979262086,-38.4018703817965));
#23812=CARTESIAN_POINT('Ctrl Pts',(-21.2679756270664,25.8256279333065,-38.4017537112319));
#23813=CARTESIAN_POINT('Ctrl Pts',(-21.2707736612757,25.8284311861039,-38.4015077888508));
#23814=CARTESIAN_POINT('Ctrl Pts',(-21.2722467452791,25.829904158415,-38.4013785589503));
#23815=CARTESIAN_POINT('Ctrl Pts',(-21.2761599208513,25.8338094567587,-38.4010359018618));
#23816=CARTESIAN_POINT('Ctrl Pts',(-21.2786024949575,25.8362393084623,-38.4008226726297));
#23817=CARTESIAN_POINT('Ctrl Pts',(-21.2898426114642,25.8473850743172,-38.3998444210227));
#23818=CARTESIAN_POINT('Ctrl Pts',(-21.2986866049169,25.8560543043904,-38.3990830648251));
#23819=CARTESIAN_POINT('Ctrl Pts',(-21.5200191545621,26.070525454943,-38.3802290907101));
#23820=CARTESIAN_POINT('Ctrl Pts',(-21.7598298502829,26.2461899450686,-38.3642695403191));
#23821=CARTESIAN_POINT('Ctrl Pts',(-22.0384463579977,26.3964755451759,-38.3464523789056));
#23822=CARTESIAN_POINT('Ctrl Pts',(-22.0566974805562,26.4060950207338,-38.3452888360464));
#23823=CARTESIAN_POINT('Ctrl Pts',(-22.0750360565132,26.4155367957515,-38.344122456765));
#23824=CARTESIAN_POINT('Origin',(-23.5502525316942,23.5502525316942,-77.3107734492734));
#23825=CARTESIAN_POINT('',(-22.0750359454076,26.4155367385478,-36.8487079434683));
#23826=CARTESIAN_POINT('',(-22.0750364532454,26.4155370000125,-37.0955933117774));
#23827=CARTESIAN_POINT('',(-22.0750360153461,26.4155367745563,-77.3107734492734));
#23828=CARTESIAN_POINT('Ctrl Pts',(-22.0750359454076,26.4155367385478,-36.8487079434683));
#23829=CARTESIAN_POINT('Ctrl Pts',(-21.9862064593613,26.3698021022233,-36.8544705918441));
#23830=CARTESIAN_POINT('Ctrl Pts',(-21.8995139251075,26.3199418552687,-36.8600951447363));
#23831=CARTESIAN_POINT('Ctrl Pts',(-21.6884902932866,26.1851307091665,-36.8741149760281));
#23832=CARTESIAN_POINT('Ctrl Pts',(-21.5675611975838,26.0953802592486,-36.8824619548554));
#23833=CARTESIAN_POINT('Ctrl Pts',(-21.3786124843708,25.9334819647741,-36.8966333656106));
#23834=CARTESIAN_POINT('Ctrl Pts',(-21.3068569595978,25.8660627417802,-36.9023222916117));
#23835=CARTESIAN_POINT('Ctrl Pts',(-21.1938838215147,25.7497318017075,-36.9119171374906));
#23836=CARTESIAN_POINT('Ctrl Pts',(-21.1508352023558,25.7026879366804,-36.9157428737853));
#23837=CARTESIAN_POINT('Ctrl Pts',(-21.1037257343339,25.6480358391879,-36.9201410790945));
#23838=CARTESIAN_POINT('Ctrl Pts',(-21.0982642369984,25.6416495709885,-36.9206543240258));
#23839=CARTESIAN_POINT('Ctrl Pts',(-21.0900967532386,25.6320231550633,-36.9214269542763));
#23840=CARTESIAN_POINT('Ctrl Pts',(-21.0873720246064,25.6287988963756,-36.9216855679607));
#23841=CARTESIAN_POINT('Ctrl Pts',(-21.0826963264578,25.6232438908574,-36.9221308401683));
#23842=CARTESIAN_POINT('Ctrl Pts',(-21.0807423000963,25.6209157146127,-36.9223173730561));
#23843=CARTESIAN_POINT('Ctrl Pts',(-21.0767244653231,25.6161147829647,-36.9227018462092));
#23844=CARTESIAN_POINT('Ctrl Pts',(-21.07466106479,25.6136416915994,-36.9228998028758));
#23845=CARTESIAN_POINT('Ctrl Pts',(-21.0697018152412,25.6076796299177,-36.9233768031177));
#23846=CARTESIAN_POINT('Ctrl Pts',(-21.066809620837,25.6041876401109,-36.9236559952858));
#23847=CARTESIAN_POINT('Ctrl Pts',(-21.0579538920438,25.5934493226209,-36.9245139804155));
#23848=CARTESIAN_POINT('Ctrl Pts',(-21.0520146728033,25.5861830887293,-36.925093758863));
#23849=CARTESIAN_POINT('Ctrl Pts',(-21.0302201504765,25.5592799971502,-36.9272375597684));
#23850=CARTESIAN_POINT('Ctrl Pts',(-21.0145642756995,25.5394834306282,-36.9288095747776));
#23851=CARTESIAN_POINT('Ctrl Pts',(-20.9954523337661,25.5147244681888,-36.9307693378903));
#23852=CARTESIAN_POINT('Ctrl Pts',(-20.9917752519811,25.509933130414,-36.9311483004828));
#23853=CARTESIAN_POINT('Ctrl Pts',(-20.9839470684788,25.4996732069322,-36.9319591822748));
#23854=CARTESIAN_POINT('Ctrl Pts',(-20.9797999353628,25.4942016432743,-36.9323912537161));
#23855=CARTESIAN_POINT('Ctrl Pts',(-20.9747802443278,25.4875347128332,-36.9329172794883));
#23856=CARTESIAN_POINT('Ctrl Pts',(-20.973890960488,25.4863519110524,-36.9330105866549));
#23857=CARTESIAN_POINT('Ctrl Pts',(-20.9691736348736,25.4800685748094,-36.9335061686704));
#23858=CARTESIAN_POINT('Ctrl Pts',(-20.9653599454045,25.4749573267952,-36.9339089948932));
#23859=CARTESIAN_POINT('Ctrl Pts',(-20.9559620080961,25.4622835506337,-36.9349070787097));
#23860=CARTESIAN_POINT('Ctrl Pts',(-20.9503956579061,25.4547078793064,-36.9355030127565));
#23861=CARTESIAN_POINT('Ctrl Pts',(-20.9425193889019,25.4438895791304,-36.936353094461));
#23862=CARTESIAN_POINT('Ctrl Pts',(-20.9401821716337,25.440666805537,-36.9366062169893));
#23863=CARTESIAN_POINT('Ctrl Pts',(-20.934802916789,25.4332203932271,-36.9371908034007));
#23864=CARTESIAN_POINT('Ctrl Pts',(-20.9317651341023,25.4289937070079,-36.9375224241165));
#23865=CARTESIAN_POINT('Ctrl Pts',(-20.9149059765851,25.4054160255719,-36.939371201553));
#23866=CARTESIAN_POINT('Ctrl Pts',(-20.9012891548179,25.3859202673106,-36.9408958021572));
#23867=CARTESIAN_POINT('Ctrl Pts',(-20.7214655696302,25.1222917104592,-36.9614576145724));
#23868=CARTESIAN_POINT('Ctrl Pts',(-20.5893874971589,24.8566079250204,-36.9817484269859));
#23869=CARTESIAN_POINT('Ctrl Pts',(-20.4687214864829,24.4974972777398,-37.0071034550484));
#23870=CARTESIAN_POINT('Ctrl Pts',(-20.4451857494766,24.4172407694423,-37.0126334082737));
#23871=CARTESIAN_POINT('Ctrl Pts',(-20.4176239439082,24.307630086382,-37.0199273645475));
#23872=CARTESIAN_POINT('Ctrl Pts',(-20.4108420365341,24.2790079858269,-37.0218084847883));
#23873=CARTESIAN_POINT('Ctrl Pts',(-20.4021474901377,24.2399371179548,-37.0243407628174));
#23874=CARTESIAN_POINT('Ctrl Pts',(-20.3998934591274,24.2295668200619,-37.0250094950629));
#23875=CARTESIAN_POINT('Ctrl Pts',(-20.3966512292315,24.2142867663075,-37.0259896566054));
#23876=CARTESIAN_POINT('Ctrl Pts',(-20.3956232110241,24.2093856666493,-37.026303262367));
#23877=CARTESIAN_POINT('Ctrl Pts',(-20.3940162371474,24.2016345034524,-37.0267979766154));
#23878=CARTESIAN_POINT('Ctrl Pts',(-20.3934297137064,24.1987860436546,-37.0269795099188));
#23879=CARTESIAN_POINT('Ctrl Pts',(-20.3923284321414,24.19340076058,-37.0273222038245));
#23880=CARTESIAN_POINT('Ctrl Pts',(-20.3918128736046,24.190864106032,-37.0274834099621));
#23881=CARTESIAN_POINT('Ctrl Pts',(-20.3909285335232,24.186485951242,-37.027761271306));
#23882=CARTESIAN_POINT('Ctrl Pts',(-20.3905583049911,24.1846447474206,-37.0278780101468));
#23883=CARTESIAN_POINT('Ctrl Pts',(-20.3898459058394,24.1810857818507,-37.0281034397636));
#23884=CARTESIAN_POINT('Ctrl Pts',(-20.3895035265542,24.1793680670233,-37.0282121426025));
#23885=CARTESIAN_POINT('Ctrl Pts',(-20.3887014777102,24.175327011045,-37.0284676421757));
#23886=CARTESIAN_POINT('Ctrl Pts',(-20.3882429678253,24.1730034367669,-37.0286143718853));
#23887=CARTESIAN_POINT('Ctrl Pts',(-20.3868997885128,24.1661569270317,-37.0290461912863));
#23888=CARTESIAN_POINT('Ctrl Pts',(-20.3860222543053,24.1616325724779,-37.0293308731611));
#23889=CARTESIAN_POINT('Ctrl Pts',(-20.3785932946037,24.1228861942835,-37.0317632144203));
#23890=CARTESIAN_POINT('Ctrl Pts',(-20.372587238311,24.088560206377,-37.0338802718932));
#23891=CARTESIAN_POINT('Ctrl Pts',(-20.3347577116185,23.8495877274757,-37.048399557004));
#23892=CARTESIAN_POINT('Ctrl Pts',(-20.3221651414928,23.6423594290496,-37.0598975835856));
#23893=CARTESIAN_POINT('Ctrl Pts',(-20.3349756002533,23.2833358887545,-37.0799720134211));
#23894=CARTESIAN_POINT('Ctrl Pts',(-20.3511520747039,23.1319197036788,-37.0884843540948));
#23895=CARTESIAN_POINT('Ctrl Pts',(-20.3965823436478,22.878204972137,-37.1033839675376));
#23896=CARTESIAN_POINT('Ctrl Pts',(-20.4203099630275,22.7751786292987,-37.1096149271084));
#23897=CARTESIAN_POINT('Ctrl Pts',(-20.4540633652893,22.6557865073395,-37.1171285287607));
#23898=CARTESIAN_POINT('Ctrl Pts',(-20.4592259924193,22.6381057592781,-37.1182488031723));
#23899=CARTESIAN_POINT('Ctrl Pts',(-20.4662058109562,22.6149414965673,-37.1197268194982));
#23900=CARTESIAN_POINT('Ctrl Pts',(-20.4678866557682,22.6094169911422,-37.1200800879395));
#23901=CARTESIAN_POINT('Ctrl Pts',(-20.4706542902299,22.6004075129069,-37.1206574779322));
#23902=CARTESIAN_POINT('Ctrl Pts',(-20.4717321743401,22.5969197997859,-37.1208813066544));
#23903=CARTESIAN_POINT('Ctrl Pts',(-20.4738207054707,22.5902024114755,-37.1213130084052));
#23904=CARTESIAN_POINT('Ctrl Pts',(-20.4748305187923,22.5869724804359,-37.1215208537655));
#23905=CARTESIAN_POINT('Ctrl Pts',(-20.4771571080245,22.5795717349568,-37.1219977112859));
#23906=CARTESIAN_POINT('Ctrl Pts',(-20.4784772887738,22.575402005298,-37.122266835296));
#23907=CARTESIAN_POINT('Ctrl Pts',(-20.482664822148,22.5622688416679,-37.1231159161463));
#23908=CARTESIAN_POINT('Ctrl Pts',(-20.4855629311026,22.5533153338082,-37.1236968863837));
#23909=CARTESIAN_POINT('Ctrl Pts',(-20.509813297564,22.4795005864367,-37.1285041820101));
#23910=CARTESIAN_POINT('Ctrl Pts',(-20.5331814425093,22.4153246243153,-37.1327969966594));
#23911=CARTESIAN_POINT('Ctrl Pts',(-20.5631375081219,22.340536707713,-37.1379405398788));
#23912=CARTESIAN_POINT('Ctrl Pts',(-20.5677713972584,22.3291567880818,-37.1387270915316));
#23913=CARTESIAN_POINT('Ctrl Pts',(-20.6719243465873,22.0775075340091,-37.1562071435215));
#23914=CARTESIAN_POINT('Ctrl Pts',(-20.8000870842649,21.8501649807577,-37.1738716044171));
#23915=CARTESIAN_POINT('Ctrl Pts',(-21.0511495958757,21.508827937758,-37.2024815974632));
#23916=CARTESIAN_POINT('Ctrl Pts',(-21.1580960415551,21.3844890403788,-37.213422487203));
#23917=CARTESIAN_POINT('Ctrl Pts',(-21.2791325551319,21.263730442552,-37.2241881177271));
#23918=CARTESIAN_POINT('Ctrl Pts',(-21.2842372243073,21.2586714528152,-37.2246393831163));
#23919=CARTESIAN_POINT('Ctrl Pts',(-21.2920419346938,21.2509881628283,-37.2253250684331));
#23920=CARTESIAN_POINT('Ctrl Pts',(-21.2947296816396,21.2483514887378,-37.2255604347402));
#23921=CARTESIAN_POINT('Ctrl Pts',(-21.2991336031428,21.2440463698745,-37.2259448253721));
#23922=CARTESIAN_POINT('Ctrl Pts',(-21.3008470171249,21.2423751254155,-37.2260940674365));
#23923=CARTESIAN_POINT('Ctrl Pts',(-21.3041536115529,21.2391570913953,-37.2263814770422));
#23924=CARTESIAN_POINT('Ctrl Pts',(-21.3057465310845,21.2376100373754,-37.2265196653597));
#23925=CARTESIAN_POINT('Ctrl Pts',(-21.3086508620539,21.2347951590987,-37.2267711300451));
#23926=CARTESIAN_POINT('Ctrl Pts',(-21.3099617461334,21.2335268064907,-37.2268844481109));
#23927=CARTESIAN_POINT('Ctrl Pts',(-21.3126352302189,21.2309444543032,-37.2271151846351));
#23928=CARTESIAN_POINT('Ctrl Pts',(-21.3139979059482,21.2296305472711,-37.2272325958903));
#23929=CARTESIAN_POINT('Ctrl Pts',(-21.3179077626614,21.2258672619489,-37.2275689216671));
#23930=CARTESIAN_POINT('Ctrl Pts',(-21.3204578258751,21.223420861757,-37.2277876022259));
#23931=CARTESIAN_POINT('Ctrl Pts',(-21.3315364505952,21.2128275334951,-37.2287347499183));
#23932=CARTESIAN_POINT('Ctrl Pts',(-21.3401058165719,21.2047231290821,-37.2294599389173));
#23933=CARTESIAN_POINT('Ctrl Pts',(-21.3516495521591,21.1939251783085,-37.2304272415321));
#23934=CARTESIAN_POINT('Ctrl Pts',(-21.3545845990371,21.1911900086105,-37.2306723585473));
#23935=CARTESIAN_POINT('Ctrl Pts',(-21.3635012406099,21.1829116480487,-37.2314145548947));
#23936=CARTESIAN_POINT('Ctrl Pts',(-21.3694988274484,21.1773856258219,-37.2319104225743));
#23937=CARTESIAN_POINT('Ctrl Pts',(-21.3793320306121,21.1683943372869,-37.2327180764042));
#23938=CARTESIAN_POINT('Ctrl Pts',(-21.3831550784082,21.164915467676,-37.2330307768298));
#23939=CARTESIAN_POINT('Ctrl Pts',(-21.3905102723815,21.1582547190517,-37.2336299182521));
#23940=CARTESIAN_POINT('Ctrl Pts',(-21.3940411179842,21.1550714315876,-37.2339164508576));
#23941=CARTESIAN_POINT('Ctrl Pts',(-21.6292109496368,20.943991948395,-37.252929894876));
#23942=CARTESIAN_POINT('Ctrl Pts',(-21.8897738431502,20.7707073969846,-37.2695640823201));
#23943=CARTESIAN_POINT('Ctrl Pts',(-22.2796787110397,20.5861051857925,-37.2940671947847));
#23944=CARTESIAN_POINT('Ctrl Pts',(-22.3909488960132,20.5408442685849,-37.3010027472906));
#23945=CARTESIAN_POINT('Ctrl Pts',(-22.5535652106443,20.4850567430032,-37.3112328660317));
#23946=CARTESIAN_POINT('Ctrl Pts',(-22.6030509572489,20.469405319842,-37.3143572633185));
#23947=CARTESIAN_POINT('Ctrl Pts',(-22.660579327027,20.4527271918678,-37.3180094928179));
#23948=CARTESIAN_POINT('Ctrl Pts',(-22.6682759339228,20.4505269113965,-37.3184985232653));
#23949=CARTESIAN_POINT('Ctrl Pts',(-22.6799644502443,20.4472324947613,-37.3192418356578));
#23950=CARTESIAN_POINT('Ctrl Pts',(-22.6839504409069,20.4461173249796,-37.3194954313638));
#23951=CARTESIAN_POINT('Ctrl Pts',(-22.6911644731956,20.4441140158997,-37.319954609326));
#23952=CARTESIAN_POINT('Ctrl Pts',(-22.6943917765104,20.4432232207354,-37.3201601047418));
#23953=CARTESIAN_POINT('Ctrl Pts',(-22.7008342218527,20.4414557864781,-37.3205704739989));
#23954=CARTESIAN_POINT('Ctrl Pts',(-22.7040493473421,20.4405791020844,-37.3207753460816));
#23955=CARTESIAN_POINT('Ctrl Pts',(-22.7130653573476,20.4381356793561,-37.321350073915));
#23956=CARTESIAN_POINT('Ctrl Pts',(-22.7188692499781,20.4365801813018,-37.3217202945575));
#23957=CARTESIAN_POINT('Ctrl Pts',(-22.7424998708982,20.430317732764,-37.3232286948233));
#23958=CARTESIAN_POINT('Ctrl Pts',(-22.7603622126316,20.4257476474437,-37.3243713049434));
#23959=CARTESIAN_POINT('Ctrl Pts',(-23.0731096249258,20.3485843510148,-37.3444218304116));
#23960=CARTESIAN_POINT('Ctrl Pts',(-23.3766952589901,20.3178951344871,-37.3648010753388));
#23961=CARTESIAN_POINT('Ctrl Pts',(-23.8709422811502,20.3378085359216,-37.3982708681225));
#23962=CARTESIAN_POINT('Ctrl Pts',(-24.0608554988106,20.362472357072,-37.4111405717495));
#23963=CARTESIAN_POINT('Ctrl Pts',(-24.2531145330685,20.4050759331034,-37.4235129173923));
#23964=CARTESIAN_POINT('Ctrl Pts',(-24.2587423626297,20.4063388894376,-37.4238744730507));
#23965=CARTESIAN_POINT('Ctrl Pts',(-24.267500776313,20.4083291005925,-37.4244361690166));
#23966=CARTESIAN_POINT('Ctrl Pts',(-24.2706336797585,20.4090459334199,-37.4246368930234));
#23967=CARTESIAN_POINT('Ctrl Pts',(-24.2758726339705,20.4102528971005,-37.4249722171388));
#23968=CARTESIAN_POINT('Ctrl Pts',(-24.2779792643693,20.410740461214,-37.4251069636069));
#23969=CARTESIAN_POINT('Ctrl Pts',(-24.2820877060613,20.411695687223,-37.4253695735218));
#23970=CARTESIAN_POINT('Ctrl Pts',(-24.2840895631321,20.4121631448594,-37.4254974486969));
#23971=CARTESIAN_POINT('Ctrl Pts',(-24.2877787718882,20.4130283425664,-37.4257329547294));
#23972=CARTESIAN_POINT('Ctrl Pts',(-24.2894662381035,20.4134255259292,-37.4258406168796));
#23973=CARTESIAN_POINT('Ctrl Pts',(-24.2934200219409,20.4143595060595,-37.4260927334758));
#23974=CARTESIAN_POINT('Ctrl Pts',(-24.2956860759983,20.4148973974385,-37.4262371235293));
#23975=CARTESIAN_POINT('Ctrl Pts',(-24.3014518595442,20.4162726208633,-37.4266042442665));
#23976=CARTESIAN_POINT('Ctrl Pts',(-24.3049507838178,20.4171133614396,-37.4268267777928));
#23977=CARTESIAN_POINT('Ctrl Pts',(-24.3243528887679,20.4218097918628,-37.4280594064011));
#23978=CARTESIAN_POINT('Ctrl Pts',(-24.3402283087102,20.4257807943281,-37.4290629255336));
#23979=CARTESIAN_POINT('Ctrl Pts',(-24.6599465350137,20.5083462381508,-37.4491835003535));
#23980=CARTESIAN_POINT('Ctrl Pts',(-24.9507845281354,20.630800225073,-37.4659750232047));
#23981=CARTESIAN_POINT('Ctrl Pts',(-25.2791100211497,20.829582032101,-37.4876914839827));
#23982=CARTESIAN_POINT('Ctrl Pts',(-25.3376653696716,20.8676883070834,-37.4916784197165));
#23983=CARTESIAN_POINT('Ctrl Pts',(-25.4482144073005,20.9448580635898,-37.4994835176825));
#23984=CARTESIAN_POINT('Ctrl Pts',(-25.5003546619567,20.9836515694298,-37.5032921868166));
#23985=CARTESIAN_POINT('Ctrl Pts',(-25.5914375333036,21.0557976469041,-37.5102086386598));
#23986=CARTESIAN_POINT('Ctrl Pts',(-25.6308247159875,21.0885538675047,-37.5132930721422));
#23987=CARTESIAN_POINT('Ctrl Pts',(-25.6754241823579,21.127480012607,-37.5169027193317));
#23988=CARTESIAN_POINT('Ctrl Pts',(-25.6814158737262,21.1327488539714,-37.5173901594325));
#23989=CARTESIAN_POINT('Ctrl Pts',(-25.6904818669095,21.1407810042118,-37.5181315425866));
#23990=CARTESIAN_POINT('Ctrl Pts',(-25.6935705505238,21.1435280940046,-37.5183848048454));
#23991=CARTESIAN_POINT('Ctrl Pts',(-25.6991510210782,21.1485106531483,-37.5188436249328));
#23992=CARTESIAN_POINT('Ctrl Pts',(-25.7016446301775,21.1507440805139,-37.5190490965428));
#23993=CARTESIAN_POINT('Ctrl Pts',(-25.7066158415379,21.1552105772397,-37.5194596224815));
#23994=CARTESIAN_POINT('Ctrl Pts',(-25.7090934660444,21.1574436158633,-37.5196646753754));
#23995=CARTESIAN_POINT('Ctrl Pts',(-25.7160355338494,21.1637199361649,-37.5202404788553));
#23996=CARTESIAN_POINT('Ctrl Pts',(-25.7204920978669,21.1677718777164,-37.5206115965965));
#23997=CARTESIAN_POINT('Ctrl Pts',(-25.7386263407493,21.1843527687509,-37.5221277616929));
#23998=CARTESIAN_POINT('Ctrl Pts',(-25.7522068783411,21.1969870029921,-37.5232772968109));
#23999=CARTESIAN_POINT('Ctrl Pts',(-26.0535389158611,21.4822141807541,-37.5491051998075));
#24000=CARTESIAN_POINT('Ctrl Pts',(-26.2886177969138,21.8054348717724,-37.5764952710242));
#24001=CARTESIAN_POINT('Ctrl Pts',(-26.4910984623381,22.2300038847135,-37.6077460902152));
#24002=CARTESIAN_POINT('Ctrl Pts',(-26.5207388614044,22.2981167620192,-37.61261279651));
#24003=CARTESIAN_POINT('Ctrl Pts',(-26.559157874808,22.3954669239625,-37.6193071854443));
#24004=CARTESIAN_POINT('Ctrl Pts',(-26.5699142628081,22.423893637066,-37.6212312972315));
#24005=CARTESIAN_POINT('Ctrl Pts',(-26.5818072552407,22.4567197446316,-37.6234146595572));
#24006=CARTESIAN_POINT('Ctrl Pts',(-26.58333819552,22.4609732494497,-37.623696834542));
#24007=CARTESIAN_POINT('Ctrl Pts',(-26.5856402897465,22.4674117818494,-37.6241228317478));
#24008=CARTESIAN_POINT('Ctrl Pts',(-26.5864180373342,22.4695944203095,-37.6242670468858));
#24009=CARTESIAN_POINT('Ctrl Pts',(-26.5878179878697,22.473536624356,-37.6245271663509));
#24010=CARTESIAN_POINT('Ctrl Pts',(-26.5884410146447,22.4752958870842,-37.62464311992));
#24011=CARTESIAN_POINT('Ctrl Pts',(-26.5897795584501,22.479086040186,-37.6248926535408));
#24012=CARTESIAN_POINT('Ctrl Pts',(-26.5904945664649,22.4811171010828,-37.6250262026329));
#24013=CARTESIAN_POINT('Ctrl Pts',(-26.5924204735578,22.4866054122092,-37.6253866208667));
#24014=CARTESIAN_POINT('Ctrl Pts',(-26.5936275191521,22.4900640261333,-37.6256132594245));
#24015=CARTESIAN_POINT('Ctrl Pts',(-26.5992070193244,22.5061393226923,-37.6266644151307));
#24016=CARTESIAN_POINT('Ctrl Pts',(-26.6035070147381,22.5187812828148,-37.6274846690028));
#24017=CARTESIAN_POINT('Ctrl Pts',(-26.6082170898878,22.532916445135,-37.6283950661363));
#24018=CARTESIAN_POINT('Ctrl Pts',(-26.6087047259833,22.5343833829003,-37.628489465751));
#24019=CARTESIAN_POINT('Ctrl Pts',(-26.717427976832,22.8622394158628,-37.6495695564401));
#24020=CARTESIAN_POINT('Ctrl Pts',(-26.7727528314061,23.2039094479507,-37.6677547064651));
#24021=CARTESIAN_POINT('Ctrl Pts',(-26.7731123298941,23.7008682127994,-37.696099867811));
#24022=CARTESIAN_POINT('Ctrl Pts',(-26.762335296893,23.8536085215606,-37.7050364969116));
#24023=CARTESIAN_POINT('Ctrl Pts',(-26.7391736259298,24.0161129948632,-37.7150203235191));
#24024=CARTESIAN_POINT('Ctrl Pts',(-26.7375306741415,24.0272239711745,-37.715705290494));
#24025=CARTESIAN_POINT('Ctrl Pts',(-26.7351635184718,24.0426740154106,-37.7166610800836));
#24026=CARTESIAN_POINT('Ctrl Pts',(-26.7344884487135,24.0470206222298,-37.7169303423269));
#24027=CARTESIAN_POINT('Ctrl Pts',(-26.733309295666,24.054511732735,-37.7173950373301));
#24028=CARTESIAN_POINT('Ctrl Pts',(-26.7328094450094,24.0576569048535,-37.7175903353991));
#24029=CARTESIAN_POINT('Ctrl Pts',(-26.7317671207605,24.0641533072367,-37.7179941297855));
#24030=CARTESIAN_POINT('Ctrl Pts',(-26.7312240124271,24.0675044298742,-37.7182026460326));
#24031=CARTESIAN_POINT('Ctrl Pts',(-26.7299457291426,24.0753136209977,-37.7186890757952));
#24032=CARTESIAN_POINT('Ctrl Pts',(-26.7292064732751,24.0797710057584,-37.7189671188525));
#24033=CARTESIAN_POINT('Ctrl Pts',(-26.7268138571492,24.0940118141665,-37.7198567055706));
#24034=CARTESIAN_POINT('Ctrl Pts',(-26.7251246999613,24.1037890917161,-37.7204693880731));
#24035=CARTESIAN_POINT('Ctrl Pts',(-26.6897909629276,24.3028263133023,-37.7329815617794));
#24036=CARTESIAN_POINT('Ctrl Pts',(-26.6393321704379,24.4886722524044,-37.7454331150915));
#24037=CARTESIAN_POINT('Ctrl Pts',(-26.4732111835675,24.9375049430528,-37.777372680108));
#24038=CARTESIAN_POINT('Ctrl Pts',(-26.3384312776336,25.1916591337613,-37.7972449007599));
#24039=CARTESIAN_POINT('Ctrl Pts',(-26.1526947013432,25.4514353619639,-37.8177173445063));
#24040=CARTESIAN_POINT('Ctrl Pts',(-26.1331367475636,25.4779223003326,-37.8198050650802));
#24041=CARTESIAN_POINT('Ctrl Pts',(-26.1101240450259,25.5081086880994,-37.8221803551214));
#24042=CARTESIAN_POINT('Ctrl Pts',(-26.1070632748303,25.5121041363126,-37.822494664012));
#24043=CARTESIAN_POINT('Ctrl Pts',(-26.1025164724738,25.5180106975703,-37.8229591704877));
#24044=CARTESIAN_POINT('Ctrl Pts',(-26.1010376455779,25.5199273083154,-37.8231098750125));
#24045=CARTESIAN_POINT('Ctrl Pts',(-26.0984086558008,25.523326643576,-37.8233771246168));
#24046=CARTESIAN_POINT('Ctrl Pts',(-26.0972593579814,25.5248100291394,-37.8234937311626));
#24047=CARTESIAN_POINT('Ctrl Pts',(-26.0948291118705,25.5279410677493,-37.8237398255017));
#24048=CARTESIAN_POINT('Ctrl Pts',(-26.0935478617617,25.5295884764347,-37.8238692908511));
#24049=CARTESIAN_POINT('Ctrl Pts',(-26.0901365341274,25.533965920001,-37.8242132572683));
#24050=CARTESIAN_POINT('Ctrl Pts',(-26.0880036478941,25.5366937780586,-37.8244275576568));
#24051=CARTESIAN_POINT('Ctrl Pts',(-26.0781128578401,25.5493016891547,-37.8254178465574));
#24052=CARTESIAN_POINT('Ctrl Pts',(-26.0703014874354,25.5591399440098,-37.82619005753));
#24053=CARTESIAN_POINT('Ctrl Pts',(-25.8774118333608,25.7991847101451,-37.8450251496007));
#24054=CARTESIAN_POINT('Ctrl Pts',(-25.6615785201261,26.0029525353146,-37.8609634119767));
#24055=CARTESIAN_POINT('Ctrl Pts',(-25.2569468905883,26.2913989095563,-37.8889301948338));
#24056=CARTESIAN_POINT('Ctrl Pts',(-25.0823583613597,26.3926674226764,-37.9005093404163));
#24057=CARTESIAN_POINT('Ctrl Pts',(-24.8875740081073,26.4824634126707,-37.9135385063693));
#24058=CARTESIAN_POINT('Ctrl Pts',(-24.8756368316123,26.4878784151874,-37.9143372345919));
#24059=CARTESIAN_POINT('Ctrl Pts',(-24.8593778119122,26.4951346389228,-37.9154255893999));
#24060=CARTESIAN_POINT('Ctrl Pts',(-24.8550843730841,26.497039509081,-37.9157130279965));
#24061=CARTESIAN_POINT('Ctrl Pts',(-24.8477990294346,26.5002527540713,-37.9162008469323));
#24062=CARTESIAN_POINT('Ctrl Pts',(-24.8448092628699,26.5015659842901,-37.9164010605617));
#24063=CARTESIAN_POINT('Ctrl Pts',(-24.8387990335586,26.5041950378442,-37.9168035898922));
#24064=CARTESIAN_POINT('Ctrl Pts',(-24.8357785393923,26.5055107776877,-37.9170059081121));
#24065=CARTESIAN_POINT('Ctrl Pts',(-24.8289429006226,26.5084759476815,-37.9174638274077));
#24066=CARTESIAN_POINT('Ctrl Pts',(-24.8251265775759,26.5101226311013,-37.9177195219952));
#24067=CARTESIAN_POINT('Ctrl Pts',(-24.8171486007868,26.5135467106708,-37.9182541347397));
#24068=CARTESIAN_POINT('Ctrl Pts',(-24.8129863701936,26.5153227321805,-37.9185330992097));
#24069=CARTESIAN_POINT('Ctrl Pts',(-24.8021080829578,26.5199374316262,-37.9192623275035));
#24070=CARTESIAN_POINT('Ctrl Pts',(-24.7953861369903,26.5227620825069,-37.9197130684312));
#24071=CARTESIAN_POINT('Ctrl Pts',(-24.7754924057297,26.5310423722638,-37.9210474710432));
#24072=CARTESIAN_POINT('Ctrl Pts',(-24.7622940692926,26.5364333907799,-37.9219333208787));
#24073=CARTESIAN_POINT('Ctrl Pts',(-24.6215405100037,26.5928390056621,-37.9313870326363));
#24074=CARTESIAN_POINT('Ctrl Pts',(-24.4909010189325,26.6357284812981,-37.9402280687868));
#24075=CARTESIAN_POINT('Ctrl Pts',(-24.193664843396,26.7126776490549,-37.9604849509993));
#24076=CARTESIAN_POINT('Ctrl Pts',(-24.0262993773536,26.7421615604559,-37.9719922135855));
#24077=CARTESIAN_POINT('Ctrl Pts',(-23.7312699386574,26.7704088236321,-37.9920375896965));
#24078=CARTESIAN_POINT('Ctrl Pts',(-23.6045213776598,26.7750367690352,-38.0005672642319));
#24079=CARTESIAN_POINT('Ctrl Pts',(-23.4736576171515,26.7720948819442,-38.0091046607864));
#24080=CARTESIAN_POINT('Ctrl Pts',(-23.4694937060768,26.7719931983542,-38.0093760227726));
#24081=CARTESIAN_POINT('Ctrl Pts',(-23.4547782165255,26.7716052964206,-38.010333991924));
#24082=CARTESIAN_POINT('Ctrl Pts',(-23.4442277450624,26.7712753086864,-38.0110189331095));
#24083=CARTESIAN_POINT('Ctrl Pts',(-23.4273732920593,26.7706652487915,-38.0121099220112));
#24084=CARTESIAN_POINT('Ctrl Pts',(-23.4210682641499,26.7704184904986,-38.0125173286109));
#24085=CARTESIAN_POINT('Ctrl Pts',(-23.3742217693644,26.7684472604301,-38.015538839341));
#24086=CARTESIAN_POINT('Ctrl Pts',(-23.3337130194319,26.7659756484109,-38.0181208296042));
#24087=CARTESIAN_POINT('Ctrl Pts',(-23.2879964020829,26.7623184031118,-38.0209919059351));
#24088=CARTESIAN_POINT('Ctrl Pts',(-23.2827343142593,26.7618844290524,-38.0213217301709));
#24089=CARTESIAN_POINT('Ctrl Pts',(-23.2750020254963,26.7612275973817,-38.0218054156971));
#24090=CARTESIAN_POINT('Ctrl Pts',(-23.272531011789,26.7610148198604,-38.0219598419226));
#24091=CARTESIAN_POINT('Ctrl Pts',(-23.2681764252666,26.7606347843948,-38.0222317227072));
#24092=CARTESIAN_POINT('Ctrl Pts',(-23.2662927522785,26.7604687209907,-38.022349245116));
#24093=CARTESIAN_POINT('Ctrl Pts',(-23.2623793743014,26.7601202486994,-38.0225932217337));
#24094=CARTESIAN_POINT('Ctrl Pts',(-23.2603496997557,26.759937572864,-38.0227196603866));
#24095=CARTESIAN_POINT('Ctrl Pts',(-23.2550902011703,26.7594591751348,-38.0230470453279));
#24096=CARTESIAN_POINT('Ctrl Pts',(-23.2518606376958,26.7591605016242,-38.0232478241203));
#24097=CARTESIAN_POINT('Ctrl Pts',(-23.2381828866658,26.7578747410101,-38.0240971183542));
#24098=CARTESIAN_POINT('Ctrl Pts',(-23.2277389490282,26.7568414821584,-38.0247430485934));
#24099=CARTESIAN_POINT('Ctrl Pts',(-23.0447221993495,26.737831721578,-38.0360200570815));
#24100=CARTESIAN_POINT('Ctrl Pts',(-22.8738451634382,26.7059955278453,-38.0458992619199));
#24101=CARTESIAN_POINT('Ctrl Pts',(-22.4878650167069,26.6012681101516,-38.0683590644733));
#24102=CARTESIAN_POINT('Ctrl Pts',(-22.2762690101925,26.5191433323991,-38.0808186862156));
#24103=CARTESIAN_POINT('Ctrl Pts',(-22.0750360152969,26.415536774531,-38.0939694478973));
#24104=CARTESIAN_POINT('',(-26.7730018305864,23.5523783233448,-37.9378739682608));
#24105=CARTESIAN_POINT('Ctrl Pts',(-22.0750360565132,26.4155367957515,-38.344122456765));
#24106=CARTESIAN_POINT('Ctrl Pts',(-22.220339252178,26.4903474073303,-38.3348808102299));
#24107=CARTESIAN_POINT('Ctrl Pts',(-22.3711316413935,26.5540020787549,-38.3254440950023));
#24108=CARTESIAN_POINT('Ctrl Pts',(-22.5361980506722,26.6093249462508,-38.314953907139));
#24109=CARTESIAN_POINT('Ctrl Pts',(-22.5462921837423,26.6126525943229,-38.3143118672905));
#24110=CARTESIAN_POINT('Ctrl Pts',(-22.5735065165015,26.6214751021643,-38.3125792932629));
#24111=CARTESIAN_POINT('Ctrl Pts',(-22.5906563584353,26.6268766587861,-38.3114857654085));
#24112=CARTESIAN_POINT('Ctrl Pts',(-22.613538704027,26.6338738041531,-38.3100241665223));
#24113=CARTESIAN_POINT('Ctrl Pts',(-22.6192319465339,26.6355975069218,-38.3096603045723));
#24114=CARTESIAN_POINT('Ctrl Pts',(-22.628110587026,26.6382588176517,-38.3090925237686));
#24115=CARTESIAN_POINT('Ctrl Pts',(-22.6312927374655,26.639207287706,-38.3088889610273));
#24116=CARTESIAN_POINT('Ctrl Pts',(-22.6376503362765,26.6410915366569,-38.3084821278023));
#24117=CARTESIAN_POINT('Ctrl Pts',(-22.6408257721307,26.6420273440861,-38.308278858531));
#24118=CARTESIAN_POINT('Ctrl Pts',(-22.6478994578794,26.6441001332727,-38.307825896811));
#24119=CARTESIAN_POINT('Ctrl Pts',(-22.6517984211596,26.6452346419234,-38.3075761238706));
#24120=CARTESIAN_POINT('Ctrl Pts',(-22.6630936235026,26.648498143519,-38.3068522314727));
#24121=CARTESIAN_POINT('Ctrl Pts',(-22.6704953203636,26.6506080027717,-38.3063774881166));
#24122=CARTESIAN_POINT('Ctrl Pts',(-22.6872281685213,26.6553129684358,-38.3053033603492));
#24123=CARTESIAN_POINT('Ctrl Pts',(-22.6965635718138,26.6578925564928,-38.3047034741235));
#24124=CARTESIAN_POINT('Ctrl Pts',(-22.7261207255491,26.6659166486943,-38.3028021181087));
#24125=CARTESIAN_POINT('Ctrl Pts',(-22.7463836733696,26.6712060637182,-38.3014956320197));
#24126=CARTESIAN_POINT('Ctrl Pts',(-22.8239776040435,26.6906553051489,-38.2964804445852));
#24127=CARTESIAN_POINT('Ctrl Pts',(-22.8816393937993,26.7034351439089,-38.2927279388175));
#24128=CARTESIAN_POINT('Ctrl Pts',(-23.0531109399128,26.7365243944657,-38.2814888303056));
#24129=CARTESIAN_POINT('Ctrl Pts',(-23.1676902871832,26.7523018245957,-38.2738720218936));
#24130=CARTESIAN_POINT('Ctrl Pts',(-23.5030642062501,26.7802241855337,-38.2513590792522));
#24131=CARTESIAN_POINT('Ctrl Pts',(-23.7245620824923,26.7758621616094,-38.2361799841178));
#24132=CARTESIAN_POINT('Ctrl Pts',(-24.0294572807363,26.7383423510628,-38.2158932899358));
#24133=CARTESIAN_POINT('Ctrl Pts',(-24.1145980491553,26.7243777926618,-38.2103025684005));
#24134=CARTESIAN_POINT('Ctrl Pts',(-24.2053065332842,26.7057338213283,-38.2044975888197));
#24135=CARTESIAN_POINT('Ctrl Pts',(-24.2115250312575,26.7044365144673,-38.2041004039014));
#24136=CARTESIAN_POINT('Ctrl Pts',(-24.2201538743822,26.7026097200451,-38.2035503808946));
#24137=CARTESIAN_POINT('Ctrl Pts',(-24.2225674553539,26.7020958487719,-38.2033966546799));
#24138=CARTESIAN_POINT('Ctrl Pts',(-24.2267183946613,26.7012070946237,-38.2031324836929));
#24139=CARTESIAN_POINT('Ctrl Pts',(-24.2284560326731,26.7008335467931,-38.2030219619794));
#24140=CARTESIAN_POINT('Ctrl Pts',(-24.23204815015,26.7000582237408,-38.2027936200136));
#24141=CARTESIAN_POINT('Ctrl Pts',(-24.2339025804704,26.699656248879,-38.2026758120908));
#24142=CARTESIAN_POINT('Ctrl Pts',(-24.2382612498682,26.6987074124988,-38.2023990863687));
#24143=CARTESIAN_POINT('Ctrl Pts',(-24.2407652002322,26.6981591992185,-38.2022402468497));
#24144=CARTESIAN_POINT('Ctrl Pts',(-24.2489187351671,26.6963638729499,-38.2017234472441));
#24145=CARTESIAN_POINT('Ctrl Pts',(-24.2545656575119,26.6951045246321,-38.2013661897206));
#24146=CARTESIAN_POINT('Ctrl Pts',(-24.441831943373,26.6528116423814,-38.1895397505751));
#24147=CARTESIAN_POINT('Ctrl Pts',(-24.6195908352636,26.5961228276987,-38.1789646639608));
#24148=CARTESIAN_POINT('Ctrl Pts',(-24.8762104082217,26.4890248276558,-38.1633662781439));
#24149=CARTESIAN_POINT('Ctrl Pts',(-24.9593894964257,26.4500594289783,-38.1582561380689));
#24150=CARTESIAN_POINT('Ctrl Pts',(-25.1467671142189,26.3523135034442,-38.1464130241019));
#24151=CARTESIAN_POINT('Ctrl Pts',(-25.2495794807149,26.291181142095,-38.1396630767961));
#24152=CARTESIAN_POINT('Ctrl Pts',(-25.3798380893999,26.2035782744985,-38.1305727889708));
#24153=CARTESIAN_POINT('Ctrl Pts',(-25.410554559422,26.1821334235194,-38.128387861814));
#24154=CARTESIAN_POINT('Ctrl Pts',(-25.4464137455449,26.1561567405847,-38.1257835906815));
#24155=CARTESIAN_POINT('Ctrl Pts',(-25.4519252763339,26.1521373996613,-38.1253817969592));
#24156=CARTESIAN_POINT('Ctrl Pts',(-25.512974411524,26.1073190870485,-38.1209141667691));
#24157=CARTESIAN_POINT('Ctrl Pts',(-25.5671989968098,26.0647688713247,-38.1167877037574));
#24158=CARTESIAN_POINT('Ctrl Pts',(-25.6272480673598,26.0144554752171,-38.1120160278631));
#24159=CARTESIAN_POINT('Ctrl Pts',(-25.634454181825,26.0083636114979,-38.1114399992281));
#24160=CARTESIAN_POINT('Ctrl Pts',(-25.64496483301,25.9993987318965,-38.1105947653059));
#24161=CARTESIAN_POINT('Ctrl Pts',(-25.6482904797533,25.9965504496619,-38.1103265810841));
#24162=CARTESIAN_POINT('Ctrl Pts',(-25.6541767817733,25.9914882374128,-38.1098505724784));
#24163=CARTESIAN_POINT('Ctrl Pts',(-25.6567397781702,25.9892770295706,-38.1096428611134));
#24164=CARTESIAN_POINT('Ctrl Pts',(-25.6616678936001,25.9850117692677,-38.109242606601));
#24165=CARTESIAN_POINT('Ctrl Pts',(-25.6640335119872,25.982958297438,-38.1090500877378));
#24166=CARTESIAN_POINT('Ctrl Pts',(-25.669094474322,25.9785521805244,-38.1086373848275));
#24167=CARTESIAN_POINT('Ctrl Pts',(-25.6717889001209,25.9761984914438,-38.1084171573502));
#24168=CARTESIAN_POINT('Ctrl Pts',(-25.6819706761241,25.9672743657706,-38.1075830288669));
#24169=CARTESIAN_POINT('Ctrl Pts',(-25.6894314081591,25.9606737655461,-38.1069678659395));
#24170=CARTESIAN_POINT('Ctrl Pts',(-25.7641011847868,25.8939927934585,-38.1007709303699));
#24171=CARTESIAN_POINT('Ctrl Pts',(-25.8287858657781,25.831157502303,-38.095072326474));
#24172=CARTESIAN_POINT('Ctrl Pts',(-25.9356691294068,25.7182413207325,-38.085049235901));
#24173=CARTESIAN_POINT('Ctrl Pts',(-25.9791346323418,25.6694312860357,-38.0807806092283));
#24174=CARTESIAN_POINT('Ctrl Pts',(-26.2415279374595,25.3560898226492,-38.0537899634624));
#24175=CARTESIAN_POINT('Ctrl Pts',(-26.4184644611853,25.0593406610344,-38.0297048515405));
#24176=CARTESIAN_POINT('Ctrl Pts',(-26.5459647107448,24.7384570453726,-38.0078817314065));
#24177=CARTESIAN_POINT('Ctrl Pts',(-26.546688852276,24.736629707286,-38.0077575920336));
#24178=CARTESIAN_POINT('Ctrl Pts',(-26.5522039938893,24.7226752378697,-38.0068106524994));
#24179=CARTESIAN_POINT('Ctrl Pts',(-26.5569231225259,24.7105195506874,-38.0059918327726));
#24180=CARTESIAN_POINT('Ctrl Pts',(-26.5628617325031,24.6949431210107,-38.0049506206503));
#24181=CARTESIAN_POINT('Ctrl Pts',(-26.5641493010733,24.6915487272123,-38.0047242070457));
#24182=CARTESIAN_POINT('Ctrl Pts',(-26.5661887303245,24.6861446973871,-38.0043645271752));
#24183=CARTESIAN_POINT('Ctrl Pts',(-26.5669443196199,24.6841364865229,-38.0042310365903));
#24184=CARTESIAN_POINT('Ctrl Pts',(-26.5683536949427,24.6803792579344,-38.0039816069649));
#24185=CARTESIAN_POINT('Ctrl Pts',(-26.5690079620882,24.6786304384514,-38.003865639507));
#24186=CARTESIAN_POINT('Ctrl Pts',(-26.5704744576226,24.6747001734212,-38.0036053090666));
#24187=CARTESIAN_POINT('Ctrl Pts',(-26.5712858409402,24.6725184205782,-38.0034609976653));
#24188=CARTESIAN_POINT('Ctrl Pts',(-26.573683780796,24.6660490834463,-38.0030336789075));
#24189=CARTESIAN_POINT('Ctrl Pts',(-26.5752635871121,24.6617589770909,-38.0027510770052));
#24190=CARTESIAN_POINT('Ctrl Pts',(-26.5877688586537,24.6275756466584,-38.0005053548184));
#24191=CARTESIAN_POINT('Ctrl Pts',(-26.5982605737062,24.5975240786653,-37.9985677765294));
#24192=CARTESIAN_POINT('Ctrl Pts',(-26.6402095798588,24.4713945743225,-37.9905686550977));
#24193=CARTESIAN_POINT('Ctrl Pts',(-26.6675852583896,24.3740108820585,-37.9847117335336));
#24194=CARTESIAN_POINT('Ctrl Pts',(-26.7451118263248,24.0383425423474,-37.9651031045121));
#24195=CARTESIAN_POINT('Ctrl Pts',(-26.7728412889899,23.7957630959875,-37.9518467202304));
#24196=CARTESIAN_POINT('Ctrl Pts',(-26.7730018305864,23.5523783233448,-37.9378739682608));
#24197=CARTESIAN_POINT('Ctrl Pts',(-26.7730018333001,23.5523742052866,-37.9378737318424));
#24198=CARTESIAN_POINT('Ctrl Pts',(-26.7730911924932,23.416640660648,-37.9300812473323));
#24199=CARTESIAN_POINT('Ctrl Pts',(-26.7646056339369,23.2810495026856,-37.922102003823));
#24200=CARTESIAN_POINT('Ctrl Pts',(-26.7467405997613,23.1396085107992,-37.9134215880712));
#24201=CARTESIAN_POINT('Ctrl Pts',(-26.745860591116,23.1328155776368,-37.9130038473182));
#24202=CARTESIAN_POINT('Ctrl Pts',(-26.7443876856687,23.1217236372626,-37.9123203257416));
#24203=CARTESIAN_POINT('Ctrl Pts',(-26.7438077466349,23.1174229069543,-37.9120549547208));
#24204=CARTESIAN_POINT('Ctrl Pts',(-26.7427693146334,23.109837783291,-37.911586308981));
#24205=CARTESIAN_POINT('Ctrl Pts',(-26.7423144346312,23.106552894949,-37.9113831488627));
#24206=CARTESIAN_POINT('Ctrl Pts',(-26.7414109738936,23.1001019072215,-37.9109837726291));
#24207=CARTESIAN_POINT('Ctrl Pts',(-26.7409627493984,23.0969357611553,-37.9107875680176));
#24208=CARTESIAN_POINT('Ctrl Pts',(-26.7400621506442,23.0906416679477,-37.9103971446756));
#24209=CARTESIAN_POINT('Ctrl Pts',(-26.7396098858449,23.0875137083546,-37.9102029296104));
#24210=CARTESIAN_POINT('Ctrl Pts',(-26.7385306499885,23.0801262300063,-37.9097437959496));
#24211=CARTESIAN_POINT('Ctrl Pts',(-26.7378997440641,23.0758672997106,-37.9094787526768));
#24212=CARTESIAN_POINT('Ctrl Pts',(-26.7356735811365,23.0610445602166,-37.9085550726694));
#24213=CARTESIAN_POINT('Ctrl Pts',(-26.7340343438519,23.0504875171673,-37.9078950404987));
#24214=CARTESIAN_POINT('Ctrl Pts',(-26.7132428107517,22.9208407061477,-37.8997623580592));
#24215=CARTESIAN_POINT('Ctrl Pts',(-26.6874741824173,22.802923393408,-37.8920786390624));
#24216=CARTESIAN_POINT('Ctrl Pts',(-26.6500507099806,22.6683609958214,-37.882961914188));
#24217=CARTESIAN_POINT('Ctrl Pts',(-26.6447766435176,22.6500292664898,-37.881712422312));
#24218=CARTESIAN_POINT('Ctrl Pts',(-26.5580415993947,22.3583252216658,-37.8617116604438));
#24219=CARTESIAN_POINT('Ctrl Pts',(-26.4408172739069,22.0969486228799,-37.8419721927852));
#24220=CARTESIAN_POINT('Ctrl Pts',(-26.2529896595378,21.7934152364845,-37.8184328817572));
#24221=CARTESIAN_POINT('Ctrl Pts',(-26.2132055083436,21.7336764983389,-37.8137754473313));
#24222=CARTESIAN_POINT('Ctrl Pts',(-26.1624174854656,21.6626738644952,-37.8082554129752));
#24223=CARTESIAN_POINT('Ctrl Pts',(-26.1532866507094,21.6501019142361,-37.8072786473201));
#24224=CARTESIAN_POINT('Ctrl Pts',(-26.1418545165122,21.6345984429613,-37.8060754089791));
#24225=CARTESIAN_POINT('Ctrl Pts',(-26.1396387911324,21.6316045089557,-37.8058431071608));
#24226=CARTESIAN_POINT('Ctrl Pts',(-26.1361385275616,21.6268919876704,-37.8054775624829));
#24227=CARTESIAN_POINT('Ctrl Pts',(-26.1348574638511,21.6251708423455,-37.8053440771567));
#24228=CARTESIAN_POINT('Ctrl Pts',(-26.1324583157192,21.6219542306148,-37.805094652248));
#24229=CARTESIAN_POINT('Ctrl Pts',(-26.1313406580072,21.6204584667146,-37.8049786842592));
#24230=CARTESIAN_POINT('Ctrl Pts',(-26.1288266872455,21.6171001047736,-37.804718346094));
#24231=CARTESIAN_POINT('Ctrl Pts',(-26.1274296586768,21.6152380517389,-37.8045740275124));
#24232=CARTESIAN_POINT('Ctrl Pts',(-26.1238702850407,21.6105045730915,-37.8042072220258));
#24233=CARTESIAN_POINT('Ctrl Pts',(-26.1217051447657,21.6076352399307,-37.8039849316785));
#24234=CARTESIAN_POINT('Ctrl Pts',(-26.109958055491,21.5921215640767,-37.8027833554382));
#24235=CARTESIAN_POINT('Ctrl Pts',(-26.1002874195711,21.5795441946163,-37.8018102309805));
#24236=CARTESIAN_POINT('Ctrl Pts',(-25.8916731374845,21.3123330410741,-37.7811455902863));
#24237=CARTESIAN_POINT('Ctrl Pts',(-25.6556096173356,21.0889339852216,-37.7639195264112));
#24238=CARTESIAN_POINT('Ctrl Pts',(-25.3274488139758,20.8607294092138,-37.7412507108422));
#24239=CARTESIAN_POINT('Ctrl Pts',(-25.2631581742556,20.8193342779402,-37.7368701272085));
#24240=CARTESIAN_POINT('Ctrl Pts',(-25.1398520844474,20.746008790555,-37.7285136863625));
#24241=CARTESIAN_POINT('Ctrl Pts',(-25.0811934317816,20.713559256619,-37.7245566707447));
#24242=CARTESIAN_POINT('Ctrl Pts',(-24.9903287363559,20.6669330915358,-37.718428289608));
#24243=CARTESIAN_POINT('Ctrl Pts',(-24.9588299135796,20.6514148199631,-37.7163041616954));
#24244=CARTESIAN_POINT('Ctrl Pts',(-24.9206037007261,20.633352358851,-37.7137245964049));
#24245=CARTESIAN_POINT('Ctrl Pts',(-24.9141124910627,20.6303116153877,-37.7132864999427));
#24246=CARTESIAN_POINT('Ctrl Pts',(-24.9046422456555,20.6259138404689,-37.7126472412767));
#24247=CARTESIAN_POINT('Ctrl Pts',(-24.901671169247,20.6245396366494,-37.712446673268));
#24248=CARTESIAN_POINT('Ctrl Pts',(-24.8957597525138,20.6218163710761,-37.7120475800729));
#24249=CARTESIAN_POINT('Ctrl Pts',(-24.8928194641838,20.6204672051293,-37.7118490587729));
#24250=CARTESIAN_POINT('Ctrl Pts',(-24.8869523147816,20.6177857213099,-37.7114528892212));
#24251=CARTESIAN_POINT('Ctrl Pts',(-24.8840254807978,20.6164533524346,-37.7112552429972));
#24252=CARTESIAN_POINT('Ctrl Pts',(-24.8769844030212,20.6132607898822,-37.7107797235714));
#24253=CARTESIAN_POINT('Ctrl Pts',(-24.8728682424817,20.6114048610719,-37.7105017038119));
#24254=CARTESIAN_POINT('Ctrl Pts',(-24.8602557659334,20.6057499066467,-37.7096496988535));
#24255=CARTESIAN_POINT('Ctrl Pts',(-24.8517469384179,20.6019790557464,-37.7090747468707));
#24256=CARTESIAN_POINT('Ctrl Pts',(-24.7543411964697,20.5593156641087,-37.7024908544431));
#24257=CARTESIAN_POINT('Ctrl Pts',(-24.6637563863077,20.5244239263854,-37.6963460408941));
#24258=CARTESIAN_POINT('Ctrl Pts',(-24.4685154243611,20.4591755513086,-37.6830358744338));
#24259=CARTESIAN_POINT('Ctrl Pts',(-24.3636153366538,20.4299318959456,-37.6758452508028));
#24260=CARTESIAN_POINT('Ctrl Pts',(-23.9698542146281,20.3413672663898,-37.6488175042016));
#24261=CARTESIAN_POINT('Ctrl Pts',(-23.6747481804493,20.3164432459355,-37.6283569729549));
#24262=CARTESIAN_POINT('Ctrl Pts',(-23.367525399613,20.3326612552132,-37.608949201336));
#24263=CARTESIAN_POINT('Ctrl Pts',(-23.3546916501153,20.3334157652203,-37.6081421956051));
#24264=CARTESIAN_POINT('Ctrl Pts',(-23.3383785854944,20.3344728156572,-37.6071214357889));
#24265=CARTESIAN_POINT('Ctrl Pts',(-23.3348950160892,20.3347042282315,-37.6069037497585));
#24266=CARTESIAN_POINT('Ctrl Pts',(-23.3293231852453,20.3350834585444,-37.6065560440157));
#24267=CARTESIAN_POINT('Ctrl Pts',(-23.3272346923707,20.3352276502251,-37.606425819899));
#24268=CARTESIAN_POINT('Ctrl Pts',(-23.3234710161034,20.3354911832986,-37.6061913368474));
#24269=CARTESIAN_POINT('Ctrl Pts',(-23.3217957972366,20.3356097982869,-37.6060870375014));
#24270=CARTESIAN_POINT('Ctrl Pts',(-23.3178166874997,20.3358946679321,-37.6058394617778));
#24271=CARTESIAN_POINT('Ctrl Pts',(-23.3155128844092,20.3360620899066,-37.6056962523213));
#24272=CARTESIAN_POINT('Ctrl Pts',(-23.3096820062453,20.3364921339764,-37.6053341181821));
#24273=CARTESIAN_POINT('Ctrl Pts',(-23.3061551695585,20.3367580864327,-37.6051153815033));
#24274=CARTESIAN_POINT('Ctrl Pts',(-23.2870725623711,20.3382286683548,-37.6039334660248));
#24275=CARTESIAN_POINT('Ctrl Pts',(-23.2715249070147,20.339540472148,-37.602976248949));
#24276=CARTESIAN_POINT('Ctrl Pts',(-23.2494973994386,20.3415602151536,-37.6016274770452));
#24277=CARTESIAN_POINT('Ctrl Pts',(-23.2430095342069,20.3421749494169,-37.6012311265864));
#24278=CARTESIAN_POINT('Ctrl Pts',(-23.2298265175743,20.3434644172591,-37.60042753084));
#24279=CARTESIAN_POINT('Ctrl Pts',(-23.2231315240253,20.3441404485936,-37.6000203527169));
#24280=CARTESIAN_POINT('Ctrl Pts',(-23.2134295765215,20.3451508153668,-37.5994315787618));
#24281=CARTESIAN_POINT('Ctrl Pts',(-23.2104209476566,20.3454684188755,-37.5992491754425));
#24282=CARTESIAN_POINT('Ctrl Pts',(-22.952987816507,20.3730107360728,-37.5836568122294));
#24283=CARTESIAN_POINT('Ctrl Pts',(-22.7026704144217,20.4304391031466,-37.5696942306749));
#24284=CARTESIAN_POINT('Ctrl Pts',(-22.3523547669669,20.5561469630578,-37.5488180481327));
#24285=CARTESIAN_POINT('Ctrl Pts',(-22.2451638950221,20.6012920069948,-37.5422426250867));
#24286=CARTESIAN_POINT('Ctrl Pts',(-22.0733034872909,20.6848820877628,-37.5311612219253));
#24287=CARTESIAN_POINT('Ctrl Pts',(-22.0071224250281,20.7199743683063,-37.5267553135996));
#24288=CARTESIAN_POINT('Ctrl Pts',(-21.9204824229074,20.7698575015982,-37.5207659244494));
#24289=CARTESIAN_POINT('Ctrl Pts',(-21.8988852029996,20.7826302629006,-37.5192540037917));
#24290=CARTESIAN_POINT('Ctrl Pts',(-21.8679709681075,20.8014038587516,-37.5170613959897));
#24291=CARTESIAN_POINT('Ctrl Pts',(-21.8585319620951,20.8072028063799,-37.5163880570586));
#24292=CARTESIAN_POINT('Ctrl Pts',(-21.8418169273968,20.8175909450668,-37.5151886833604));
#24293=CARTESIAN_POINT('Ctrl Pts',(-21.834528987411,20.8221608399814,-37.5146633618816));
#24294=CARTESIAN_POINT('Ctrl Pts',(-21.8236729171408,20.8290288347158,-37.5138772479634));
#24295=CARTESIAN_POINT('Ctrl Pts',(-21.8200908471788,20.8313049191886,-37.5136172737665));
#24296=CARTESIAN_POINT('Ctrl Pts',(-21.8137847283613,20.8353294005856,-37.5131585554059));
#24297=CARTESIAN_POINT('Ctrl Pts',(-21.8110587924965,20.8370748417425,-37.5129599216046));
#24298=CARTESIAN_POINT('Ctrl Pts',(-21.8056276915693,20.840563972447,-37.5125634779765));
#24299=CARTESIAN_POINT('Ctrl Pts',(-21.8029224995125,20.842307613605,-37.5123656701036));
#24300=CARTESIAN_POINT('Ctrl Pts',(-21.7964202985438,20.8465124304327,-37.5118893925015));
#24301=CARTESIAN_POINT('Ctrl Pts',(-21.7926258596277,20.8489775515186,-37.5116107751841));
#24302=CARTESIAN_POINT('Ctrl Pts',(-21.781009828686,20.8565589385068,-37.5107557406637));
#24303=CARTESIAN_POINT('Ctrl Pts',(-21.7732053434902,20.8617012109886,-37.5101783472467));
#24304=CARTESIAN_POINT('Ctrl Pts',(-21.6832618142842,20.9215265496103,-37.5034900219499));
#24305=CARTESIAN_POINT('Ctrl Pts',(-21.6036617103341,20.9799149353121,-37.497238512054));
#24306=CARTESIAN_POINT('Ctrl Pts',(-21.3005672212918,21.2244041971574,-37.4720426621432));
#24307=CARTESIAN_POINT('Ctrl Pts',(-21.1000259739087,21.4367260775146,-37.4520412058787));
#24308=CARTESIAN_POINT('Ctrl Pts',(-20.9033981251815,21.7111010955547,-37.4294856851029));
#24309=CARTESIAN_POINT('Ctrl Pts',(-20.8769183579128,21.7498078666695,-37.4263743093721));
#24310=CARTESIAN_POINT('Ctrl Pts',(-20.8232879092614,21.8319954354808,-37.4199336265357));
#24311=CARTESIAN_POINT('Ctrl Pts',(-20.7963098405424,21.8755753068791,-37.416611719997));
#24312=CARTESIAN_POINT('Ctrl Pts',(-20.7580016842836,21.9408888413386,-37.4117893525362));
#24313=CARTESIAN_POINT('Ctrl Pts',(-20.745862639751,21.9621361301263,-37.4102443515039));
#24314=CARTESIAN_POINT('Ctrl Pts',(-20.7318888418725,21.9872547914026,-37.4084474481515));
#24315=CARTESIAN_POINT('Ctrl Pts',(-20.729818764783,21.9909933514319,-37.4081807681304));
#24316=CARTESIAN_POINT('Ctrl Pts',(-20.7266628173735,21.996719841842,-37.4077734649862));
#24317=CARTESIAN_POINT('Ctrl Pts',(-20.7255716066598,21.9987047995635,-37.4076324991341));
#24318=CARTESIAN_POINT('Ctrl Pts',(-20.7235948133116,22.0023096664916,-37.4073768871936));
#24319=CARTESIAN_POINT('Ctrl Pts',(-20.7227085333588,22.0039291798857,-37.4072621963129));
#24320=CARTESIAN_POINT('Ctrl Pts',(-20.7209128720518,22.0072171259262,-37.4070296436872));
#24321=CARTESIAN_POINT('Ctrl Pts',(-20.720003578197,22.0088855947343,-37.4069117877323));
#24322=CARTESIAN_POINT('Ctrl Pts',(-20.7173905133876,22.0136904316385,-37.4065728246397));
#24323=CARTESIAN_POINT('Ctrl Pts',(-20.7156904695907,22.0168288399285,-37.4063519573378));
#24324=CARTESIAN_POINT('Ctrl Pts',(-20.7082501022682,22.0306189694418,-37.4053837892313));
#24325=CARTESIAN_POINT('Ctrl Pts',(-20.7025644820483,22.0413003272697,-37.4046399481648));
#24326=CARTESIAN_POINT('Ctrl Pts',(-20.6953953128578,22.0549536154031,-37.4036965300417));
#24327=CARTESIAN_POINT('Ctrl Pts',(-20.6938561129204,22.0578959764312,-37.4034936532149));
#24328=CARTESIAN_POINT('Ctrl Pts',(-20.5756865080555,22.2846435989383,-37.3878923976318));
#24329=CARTESIAN_POINT('Ctrl Pts',(-20.4857224821955,22.5214134780311,-37.3740369717105));
#24330=CARTESIAN_POINT('Ctrl Pts',(-20.36947754347,22.9849249398032,-37.3472999912089));
#24331=CARTESIAN_POINT('Ctrl Pts',(-20.3377413117578,23.2086734106484,-37.3345351957606));
#24332=CARTESIAN_POINT('Ctrl Pts',(-20.3289818622113,23.451107263167,-37.3199092343669));
#24333=CARTESIAN_POINT('Ctrl Pts',(-20.3284977884434,23.4683326504266,-37.3188661031795));
#24334=CARTESIAN_POINT('Ctrl Pts',(-20.3279836143102,23.4939421331828,-37.317309100605));
#24335=CARTESIAN_POINT('Ctrl Pts',(-20.3278480428498,23.5023239899203,-37.3167985229184));
#24336=CARTESIAN_POINT('Ctrl Pts',(-20.327661148346,23.5175534479343,-37.3158690091136));
#24337=CARTESIAN_POINT('Ctrl Pts',(-20.3275989441436,23.5244008854489,-37.3154504157493));
#24338=CARTESIAN_POINT('Ctrl Pts',(-20.3275357555449,23.5351163349462,-37.3147943039746));
#24339=CARTESIAN_POINT('Ctrl Pts',(-20.3275199101879,23.5389842665981,-37.3145572523741));
#24340=CARTESIAN_POINT('Ctrl Pts',(-20.3275041154014,23.5458626801855,-37.3141353109646));
#24341=CARTESIAN_POINT('Ctrl Pts',(-20.3275014208047,23.5488731563455,-37.313950507572));
#24342=CARTESIAN_POINT('Ctrl Pts',(-20.3275046447199,23.5552430430979,-37.3135591991931));
#24343=CARTESIAN_POINT('Ctrl Pts',(-20.3275115978042,23.5586024475927,-37.3133526619352));
#24344=CARTESIAN_POINT('Ctrl Pts',(-20.3275461181161,23.568103413846,-37.3127680674434));
#24345=CARTESIAN_POINT('Ctrl Pts',(-20.3275859886088,23.5742448920037,-37.312389624366));
#24346=CARTESIAN_POINT('Ctrl Pts',(-20.3278254997188,23.5998591341043,-37.3108088980295));
#24347=CARTESIAN_POINT('Ctrl Pts',(-20.3281840792349,23.6193296789279,-37.3096016356698));
#24348=CARTESIAN_POINT('Ctrl Pts',(-20.3370226346138,23.9409105053207,-37.289565248298));
#24349=CARTESIAN_POINT('Ctrl Pts',(-20.3877817446493,24.2402902391441,-37.2692818246888));
#24350=CARTESIAN_POINT('Ctrl Pts',(-20.5348091599203,24.7019955607147,-37.2364950397347));
#24351=CARTESIAN_POINT('Ctrl Pts',(-20.6048470078265,24.870863520532,-37.2242045672926));
#24352=CARTESIAN_POINT('Ctrl Pts',(-20.6961365338836,25.0470467393533,-37.2116532244708));
#24353=CARTESIAN_POINT('Ctrl Pts',(-20.7035658090274,25.0611283561654,-37.2106521608968));
#24354=CARTESIAN_POINT('Ctrl Pts',(-20.7128758861987,25.0784624097464,-37.2094230467821));
#24355=CARTESIAN_POINT('Ctrl Pts',(-20.7146582489451,25.0817670512998,-37.2091888660066));
#24356=CARTESIAN_POINT('Ctrl Pts',(-20.7174713754834,25.0869610647491,-37.2088210307773));
#24357=CARTESIAN_POINT('Ctrl Pts',(-20.7184982564737,25.0888525184948,-37.2086871287678));
#24358=CARTESIAN_POINT('Ctrl Pts',(-20.7204192523342,25.0923824411095,-37.208437327933));
#24359=CARTESIAN_POINT('Ctrl Pts',(-20.7213128899545,25.0940211509854,-37.208321399862));
#24360=CARTESIAN_POINT('Ctrl Pts',(-20.7233198567875,25.0976938360824,-37.2080616655897));
#24361=CARTESIAN_POINT('Ctrl Pts',(-20.7244339552934,25.0997273821973,-37.2079179099321));
#24362=CARTESIAN_POINT('Ctrl Pts',(-20.7272666339521,25.1048846085758,-37.2075534769928));
#24363=CARTESIAN_POINT('Ctrl Pts',(-20.7289882096909,25.1080066518915,-37.2073329919028));
#24364=CARTESIAN_POINT('Ctrl Pts',(-20.7384391096953,25.1250786123352,-37.2061280258586));
#24365=CARTESIAN_POINT('Ctrl Pts',(-20.7462668983485,25.1389741867031,-37.2051497817923));
#24366=CARTESIAN_POINT('Ctrl Pts',(-20.8976297148873,25.4030635365318,-37.1865952625104));
#24367=CARTESIAN_POINT('Ctrl Pts',(-21.0740356253437,25.632973971005,-37.1710014150161));
#24368=CARTESIAN_POINT('Ctrl Pts',(-21.3631692652182,25.9202643720146,-37.1480736256099));
#24369=CARTESIAN_POINT('Ctrl Pts',(-21.4521946198288,25.9994236205104,-37.1413004721716));
#24370=CARTESIAN_POINT('Ctrl Pts',(-21.609436713965,26.1243627526132,-37.1295627659001));
#24371=CARTESIAN_POINT('Ctrl Pts',(-21.6753940791134,26.1727920478462,-37.1247006189206));
#24372=CARTESIAN_POINT('Ctrl Pts',(-21.7517958183193,26.2245339023315,-37.1191035305024));
#24373=CARTESIAN_POINT('Ctrl Pts',(-21.7605019365269,26.2303682385762,-37.118466246416));
#24374=CARTESIAN_POINT('Ctrl Pts',(-21.7760918485895,26.2407058572732,-37.1173259087012));
#24375=CARTESIAN_POINT('Ctrl Pts',(-21.7829647471771,26.2452254650116,-37.1168234726104));
#24376=CARTESIAN_POINT('Ctrl Pts',(-21.7933428598706,26.2519933238434,-37.1160651949351));
#24377=CARTESIAN_POINT('Ctrl Pts',(-21.7968352881665,26.2542611989791,-37.1158100888637));
#24378=CARTESIAN_POINT('Ctrl Pts',(-21.8030737032703,26.2582950651831,-37.115354518675));
#24379=CARTESIAN_POINT('Ctrl Pts',(-21.8058180016007,26.2600636675057,-37.1151541524579));
#24380=CARTESIAN_POINT('Ctrl Pts',(-21.8113061893956,26.2635888166979,-37.1147535285637));
#24381=CARTESIAN_POINT('Ctrl Pts',(-21.8140500645629,26.2653453790765,-37.1145532717651));
#24382=CARTESIAN_POINT('Ctrl Pts',(-21.8207330997167,26.2696094228366,-37.1140656151049));
#24383=CARTESIAN_POINT('Ctrl Pts',(-21.8246750467624,26.2721125042369,-37.1137780519711));
#24384=CARTESIAN_POINT('Ctrl Pts',(-21.8395486749748,26.2815117533965,-37.11269331063));
#24385=CARTESIAN_POINT('Ctrl Pts',(-21.8505162550517,26.2883506313925,-37.1118940127062));
#24386=CARTESIAN_POINT('Ctrl Pts',(-21.931184689076,26.3379803060511,-37.1060188005543));
#24387=CARTESIAN_POINT('Ctrl Pts',(-22.0024085419043,26.3781439021406,-37.1008507620103));
#24388=CARTESIAN_POINT('Ctrl Pts',(-22.0750364532454,26.4155370000125,-37.0955933117774));
#24389=CARTESIAN_POINT('Origin',(-23.5502525316942,23.5502525316942,-77.3107734492734));
#24390=CARTESIAN_POINT('',(-22.075035776554,26.4155366516121,-35.5970690335682));
#24391=CARTESIAN_POINT('',(-22.0750360716487,26.4155368035442,-35.8409625058884));
#24392=CARTESIAN_POINT('',(-22.0750360153461,26.4155367745563,-77.3107734492734));
#24393=CARTESIAN_POINT('',(-26.7730022894476,23.5490029715869,-36.4420349701589));
#24394=CARTESIAN_POINT('Ctrl Pts',(-22.075035776554,26.4155366516121,-35.5970690335682));
#24395=CARTESIAN_POINT('Ctrl Pts',(-22.0107532744414,26.3824402394554,-35.6019587179599));
#24396=CARTESIAN_POINT('Ctrl Pts',(-21.9475664300769,26.3471712705029,-35.6068371265654));
#24397=CARTESIAN_POINT('Ctrl Pts',(-21.812752629119,26.2658457728297,-35.6173377908743));
#24398=CARTESIAN_POINT('Ctrl Pts',(-21.7416811243655,26.2190396190175,-35.6229332802173));
#24399=CARTESIAN_POINT('Ctrl Pts',(-21.6697392827418,26.1674646657295,-35.6285977129969));
#24400=CARTESIAN_POINT('Ctrl Pts',(-21.6669422290827,26.1654526652079,-35.6288179420446));
#24401=CARTESIAN_POINT('Ctrl Pts',(-21.6596836161164,26.1602136534026,-35.6293894441198));
#24402=CARTESIAN_POINT('Ctrl Pts',(-21.6552270684156,26.1569796704396,-35.6297403149775));
#24403=CARTESIAN_POINT('Ctrl Pts',(-21.6385285653988,26.1447966128086,-35.6310549001775));
#24404=CARTESIAN_POINT('Ctrl Pts',(-21.6263412904979,26.1357724153682,-35.6320141105692));
#24405=CARTESIAN_POINT('Ctrl Pts',(-21.6068196793789,26.1211029651447,-35.6335495998462));
#24406=CARTESIAN_POINT('Ctrl Pts',(-21.5994453353503,26.1155116785104,-35.6341294081067));
#24407=CARTESIAN_POINT('Ctrl Pts',(-21.5895480491372,26.1079401159358,-35.6349071595911));
#24408=CARTESIAN_POINT('Ctrl Pts',(-21.5870039235966,26.1059877976245,-35.635107044945));
#24409=CARTESIAN_POINT('Ctrl Pts',(-21.5830148951747,26.1029172143605,-35.6354203873788));
#24410=CARTESIAN_POINT('Ctrl Pts',(-21.5815680307641,26.1018015193699,-35.635534026623));
#24411=CARTESIAN_POINT('Ctrl Pts',(-21.5786670675373,26.0995606143909,-35.6357618448728));
#24412=CARTESIAN_POINT('Ctrl Pts',(-21.5772129929577,26.098435398283,-35.6358760215629));
#24413=CARTESIAN_POINT('Ctrl Pts',(-21.5739057803371,26.0958716281792,-35.6361356781596));
#24414=CARTESIAN_POINT('Ctrl Pts',(-21.5720532523937,26.0944322968539,-35.6362811014948));
#24415=CARTESIAN_POINT('Ctrl Pts',(-21.5681752932737,26.0914124998234,-35.6365854772679));
#24416=CARTESIAN_POINT('Ctrl Pts',(-21.5661501756678,26.089831631389,-35.6367444009259));
#24417=CARTESIAN_POINT('Ctrl Pts',(-21.5608313389227,26.0856693401253,-35.6371617437551));
#24418=CARTESIAN_POINT('Ctrl Pts',(-21.5575407402255,26.0830839100785,-35.6374198805694));
#24419=CARTESIAN_POINT('Ctrl Pts',(-21.5477315113824,26.0753458304564,-35.6381892343352));
#24420=CARTESIAN_POINT('Ctrl Pts',(-21.5412277019549,26.0701743243771,-35.6386991423172));
#24421=CARTESIAN_POINT('Ctrl Pts',(-21.3042996221875,25.8802805706437,-35.6572704669888));
#24422=CARTESIAN_POINT('Ctrl Pts',(-21.1002912278067,25.6647484709882,-35.6732061335021));
#24423=CARTESIAN_POINT('Ctrl Pts',(-20.810916755184,25.2599385144847,-35.7012112887636));
#24424=CARTESIAN_POINT('Ctrl Pts',(-20.7091064032451,25.0848067685651,-35.7128337841577));
#24425=CARTESIAN_POINT('Ctrl Pts',(-20.6190949321161,24.8898760992118,-35.7258809176289));
#24426=CARTESIAN_POINT('Ctrl Pts',(-20.6138822602348,24.8784113317043,-35.7266485055955));
#24427=CARTESIAN_POINT('Ctrl Pts',(-20.6068500053658,24.8627008021803,-35.7277007631107));
#24428=CARTESIAN_POINT('Ctrl Pts',(-20.6049721029363,24.8584811395121,-35.7279834269913));
#24429=CARTESIAN_POINT('Ctrl Pts',(-20.6017907348512,24.8512910083547,-35.7284651481662));
#24430=CARTESIAN_POINT('Ctrl Pts',(-20.6004826672937,24.8483225730069,-35.7286640473611));
#24431=CARTESIAN_POINT('Ctrl Pts',(-20.5979607632436,24.84257604678,-35.7290491350927));
#24432=CARTESIAN_POINT('Ctrl Pts',(-20.5967463604463,24.839798207507,-35.7292353039367));
#24433=CARTESIAN_POINT('Ctrl Pts',(-20.5938731506484,24.8332006443605,-35.7296775164491));
#24434=CARTESIAN_POINT('Ctrl Pts',(-20.5922178270948,24.8293794177352,-35.7299336789351));
#24435=CARTESIAN_POINT('Ctrl Pts',(-20.5873541418367,24.818091927156,-35.7306904752169));
#24436=CARTESIAN_POINT('Ctrl Pts',(-20.584166626418,24.8106167655123,-35.7311918197179));
#24437=CARTESIAN_POINT('Ctrl Pts',(-20.559555583198,24.7522900419256,-35.7351050015084));
#24438=CARTESIAN_POINT('Ctrl Pts',(-20.5394141374281,24.7009105901345,-35.7385601412958));
#24439=CARTESIAN_POINT('Ctrl Pts',(-20.4754161374854,24.5244513408863,-35.7504641440356));
#24440=CARTESIAN_POINT('Ctrl Pts',(-20.4379636232018,24.3972073062952,-35.759117948007));
#24441=CARTESIAN_POINT('Ctrl Pts',(-20.3617179822319,24.063471871596,-35.7819213069152));
#24442=CARTESIAN_POINT('Ctrl Pts',(-20.3350759002588,23.8548495147009,-35.796302933041));
#24443=CARTESIAN_POINT('Ctrl Pts',(-20.325566288178,23.5319547208434,-35.8178560890464));
#24444=CARTESIAN_POINT('Ctrl Pts',(-20.3281989534184,23.4186725917476,-35.8252745650799));
#24445=CARTESIAN_POINT('Ctrl Pts',(-20.3373340016874,23.2986111958647,-35.8328292915484));
#24446=CARTESIAN_POINT('Ctrl Pts',(-20.3379010899486,23.2914725877073,-35.8332773110015));
#24447=CARTESIAN_POINT('Ctrl Pts',(-20.3387060279458,23.2817504895048,-35.8338858223845));
#24448=CARTESIAN_POINT('Ctrl Pts',(-20.3389232044211,23.2791653790839,-35.8340474670351));
#24449=CARTESIAN_POINT('Ctrl Pts',(-20.3392973391131,23.2747754990508,-35.8343216893323));
#24450=CARTESIAN_POINT('Ctrl Pts',(-20.3394526975793,23.2729706001473,-35.8344343574221));
#24451=CARTESIAN_POINT('Ctrl Pts',(-20.3397692195624,23.2693292977828,-35.8346615007339));
#24452=CARTESIAN_POINT('Ctrl Pts',(-20.339930435754,23.2674929144211,-35.8347759716679));
#24453=CARTESIAN_POINT('Ctrl Pts',(-20.3402890003258,23.2634484095675,-35.8350279063718));
#24454=CARTESIAN_POINT('Ctrl Pts',(-20.3404870511784,23.2612403566126,-35.8351653296351));
#24455=CARTESIAN_POINT('Ctrl Pts',(-20.340917081729,23.2565009467963,-35.8354600483712));
#24456=CARTESIAN_POINT('Ctrl Pts',(-20.3411497784812,23.2539696542649,-35.8356173032819));
#24457=CARTESIAN_POINT('Ctrl Pts',(-20.3417674504216,23.2473366725673,-35.8360289788639));
#24458=CARTESIAN_POINT('Ctrl Pts',(-20.3421572975742,23.2432354251391,-35.8362831274776));
#24459=CARTESIAN_POINT('Ctrl Pts',(-20.3433401340824,23.2310400962046,-35.8370377099155));
#24460=CARTESIAN_POINT('Ctrl Pts',(-20.3441559062838,23.2229481828873,-35.8375368938698));
#24461=CARTESIAN_POINT('Ctrl Pts',(-20.3471332320261,23.1944947904442,-35.8392871530239));
#24462=CARTESIAN_POINT('Ctrl Pts',(-20.3494582447802,23.1741504183958,-35.8405295716965));
#24463=CARTESIAN_POINT('Ctrl Pts',(-20.3613400889921,23.0782897836147,-35.8463469133889));
#24464=CARTESIAN_POINT('Ctrl Pts',(-20.3733771535952,23.0030998383003,-35.8508020949629));
#24465=CARTESIAN_POINT('Ctrl Pts',(-20.4639258741595,22.5426491677104,-35.8778012663908));
#24466=CARTESIAN_POINT('Ctrl Pts',(-20.6097125958165,22.1740461255419,-35.8986459756614));
#24467=CARTESIAN_POINT('Ctrl Pts',(-20.8284406141648,21.8244993508741,-35.9236004287715));
#24468=CARTESIAN_POINT('Ctrl Pts',(-20.8387412907576,21.8083596184647,-35.9247643901203));
#24469=CARTESIAN_POINT('Ctrl Pts',(-20.8525125137447,21.787200186984,-35.9263062687488));
#24470=CARTESIAN_POINT('Ctrl Pts',(-20.8558545171871,21.7820969635255,-35.9266793698951));
#24471=CARTESIAN_POINT('Ctrl Pts',(-20.8610547556704,21.7742052032874,-35.9272582668279));
#24472=CARTESIAN_POINT('Ctrl Pts',(-20.8629028972423,21.7714100053901,-35.9274636827707));
#24473=CARTESIAN_POINT('Ctrl Pts',(-20.8666049759286,21.7658297812189,-35.9278745204069));
#24474=CARTESIAN_POINT('Ctrl Pts',(-20.8684588971314,21.7630447492958,-35.9280799413335));
#24475=CARTESIAN_POINT('Ctrl Pts',(-20.8725974085051,21.7568486568007,-35.9285377995463));
#24476=CARTESIAN_POINT('Ctrl Pts',(-20.8748841837157,21.7534390690305,-35.9287903192331));
#24477=CARTESIAN_POINT('Ctrl Pts',(-20.8815596025397,21.7435269977569,-35.9295260889908));
#24478=CARTESIAN_POINT('Ctrl Pts',(-20.8859654585306,21.7370361918357,-35.930009991253));
#24479=CARTESIAN_POINT('Ctrl Pts',(-20.9174654049111,21.6909924547873,-35.9334576521994));
#24480=CARTESIAN_POINT('Ctrl Pts',(-20.9454142048388,21.6520341619841,-35.9364539388022));
#24481=CARTESIAN_POINT('Ctrl Pts',(-21.0369911254623,21.5302161579891,-35.9460854020439));
#24482=CARTESIAN_POINT('Ctrl Pts',(-21.1037782166715,21.4498265228752,-35.9528423729644));
#24483=CARTESIAN_POINT('Ctrl Pts',(-21.2031151964104,21.3414344825106,-35.9625313422311));
#24484=CARTESIAN_POINT('Ctrl Pts',(-21.2325043644562,21.3106154901051,-35.9653570535876));
#24485=CARTESIAN_POINT('Ctrl Pts',(-21.2878468837449,21.2548366908736,-35.970600418019));
#24486=CARTESIAN_POINT('Ctrl Pts',(-21.3136248668869,21.2297116904468,-35.9730132153234));
#24487=CARTESIAN_POINT('Ctrl Pts',(-21.53682963324,21.0193357749232,-35.9936416703867));
#24488=CARTESIAN_POINT('Ctrl Pts',(-21.7564614118215,20.8592040068082,-36.0123286391318));
#24489=CARTESIAN_POINT('Ctrl Pts',(-21.9964054539959,20.7268348262275,-36.0296510884112));
#24490=CARTESIAN_POINT('Ctrl Pts',(-21.9992744316147,20.7252578036107,-36.0298577823779));
#24491=CARTESIAN_POINT('Ctrl Pts',(-22.0127806142454,20.7178604876721,-36.0308287980162));
#24492=CARTESIAN_POINT('Ctrl Pts',(-22.0234483972759,20.7120957822807,-36.0315898340349));
#24493=CARTESIAN_POINT('Ctrl Pts',(-22.037300748517,20.7047108919092,-36.0325701699526));
#24494=CARTESIAN_POINT('Ctrl Pts',(-22.0404556446343,20.7030357008068,-36.0327929160674));
#24495=CARTESIAN_POINT('Ctrl Pts',(-22.0452934941549,20.7004771948856,-36.0331336698577));
#24496=CARTESIAN_POINT('Ctrl Pts',(-22.0469744414965,20.6995901247212,-36.0332519169738));
#24497=CARTESIAN_POINT('Ctrl Pts',(-22.0502729060431,20.6978531866265,-36.0334836529248));
#24498=CARTESIAN_POINT('Ctrl Pts',(-22.0518903530655,20.6970032115679,-36.0335971480675));
#24499=CARTESIAN_POINT('Ctrl Pts',(-22.055309555937,20.6952101156397,-36.0338367764709));
#24500=CARTESIAN_POINT('Ctrl Pts',(-22.0571114760069,20.6942673275811,-36.0339628881732));
#24501=CARTESIAN_POINT('Ctrl Pts',(-22.060959238576,20.6922587649265,-36.0342318177175));
#24502=CARTESIAN_POINT('Ctrl Pts',(-22.0630053369255,20.6911934792189,-36.0343746043967));
#24503=CARTESIAN_POINT('Ctrl Pts',(-22.0682108095909,20.6884903891633,-36.0347373126078));
#24504=CARTESIAN_POINT('Ctrl Pts',(-22.0713717664647,20.6868556138711,-36.0349570434245));
#24505=CARTESIAN_POINT('Ctrl Pts',(-22.0804454986702,20.6821819182352,-36.0355863260023));
#24506=CARTESIAN_POINT('Ctrl Pts',(-22.0863650207473,20.679156031187,-36.0359950715101));
#24507=CARTESIAN_POINT('Ctrl Pts',(-22.1061886317833,20.669100026416,-36.0373580797539));
#24508=CARTESIAN_POINT('Ctrl Pts',(-22.1201345843245,20.6621522937717,-36.0383074131655));
#24509=CARTESIAN_POINT('Ctrl Pts',(-22.1783906689232,20.6336551496001,-36.0422357162036));
#24510=CARTESIAN_POINT('Ctrl Pts',(-22.2231439871517,20.6130210558798,-36.0451641767871));
#24511=CARTESIAN_POINT('Ctrl Pts',(-22.3080330336073,20.5762184882778,-36.0505850899094));
#24512=CARTESIAN_POINT('Ctrl Pts',(-22.3480543488825,20.5598165135141,-36.0530864616433));
#24513=CARTESIAN_POINT('Ctrl Pts',(-22.7461404371178,20.4059525856993,-36.0775464195381));
#24514=CARTESIAN_POINT('Ctrl Pts',(-23.1256716661585,20.3326478177814,-36.0979705292624));
#24515=CARTESIAN_POINT('Ctrl Pts',(-23.529044166655,20.3275113198189,-36.1223744024461));
#24516=CARTESIAN_POINT('Ctrl Pts',(-23.5488721469664,20.3274418359398,-36.1235794933329));
#24517=CARTESIAN_POINT('Ctrl Pts',(-23.5748844384185,20.3275907296277,-36.1251680636295));
#24518=CARTESIAN_POINT('Ctrl Pts',(-23.5810695600084,20.3276439406223,-36.1255463533756));
#24519=CARTESIAN_POINT('Ctrl Pts',(-23.5906223516881,20.327753627994,-36.1261314983182));
#24520=CARTESIAN_POINT('Ctrl Pts',(-23.59399017427,20.3277975785257,-36.1263379600673));
#24521=CARTESIAN_POINT('Ctrl Pts',(-23.6007015249633,20.3278956855772,-36.1267497350127));
#24522=CARTESIAN_POINT('Ctrl Pts',(-23.6040450501422,20.3279497666728,-36.1269550455878));
#24523=CARTESIAN_POINT('Ctrl Pts',(-23.6114637722123,20.3280813134312,-36.1274109720261));
#24524=CARTESIAN_POINT('Ctrl Pts',(-23.6155389134977,20.3281613064376,-36.127661666931));
#24525=CARTESIAN_POINT('Ctrl Pts',(-23.6273175819483,20.3284148704984,-36.1283870031222));
#24526=CARTESIAN_POINT('Ctrl Pts',(-23.6350206129404,20.3286083384569,-36.1288622684781));
#24527=CARTESIAN_POINT('Ctrl Pts',(-23.687506291901,20.3301149291335,-36.132106838458));
#24528=CARTESIAN_POINT('Ctrl Pts',(-23.7322561429733,20.3323340845006,-36.1349044716053));
#24529=CARTESIAN_POINT('Ctrl Pts',(-23.8295118432328,20.339192118562,-36.1410566749563));
#24530=CARTESIAN_POINT('Ctrl Pts',(-23.8819787816607,20.3441876668337,-36.1444215667582));
#24531=CARTESIAN_POINT('Ctrl Pts',(-24.039590509736,20.3631045483227,-36.1546703911332));
#24532=CARTESIAN_POINT('Ctrl Pts',(-24.1441866825067,20.3809304203879,-36.1616639437822));
#24533=CARTESIAN_POINT('Ctrl Pts',(-24.2777969106109,20.4105476600026,-36.1708149920407));
#24534=CARTESIAN_POINT('Ctrl Pts',(-24.307789943283,20.4176490584613,-36.1728833657153));
#24535=CARTESIAN_POINT('Ctrl Pts',(-24.3626069429963,20.4314612783026,-36.1766873859001));
#24536=CARTESIAN_POINT('Ctrl Pts',(-24.3874615326543,20.4380411573352,-36.178421201947));
#24537=CARTESIAN_POINT('Ctrl Pts',(-24.4334747499402,20.4508135527225,-36.1816462420641));
#24538=CARTESIAN_POINT('Ctrl Pts',(-24.4546538373334,20.4569271783729,-36.1831367185419));
#24539=CARTESIAN_POINT('Ctrl Pts',(-24.4942109175978,20.4687868373105,-36.1859307478422));
#24540=CARTESIAN_POINT('Ctrl Pts',(-24.5126034469167,20.4744812505075,-36.1872340311218));
#24541=CARTESIAN_POINT('Ctrl Pts',(-24.588862307113,20.4988423364142,-36.1926531725849));
#24542=CARTESIAN_POINT('Ctrl Pts',(-24.6462462659162,20.5189801334397,-36.1967685338156));
#24543=CARTESIAN_POINT('Ctrl Pts',(-24.7535890193624,20.5600969332142,-36.2045067533525));
#24544=CARTESIAN_POINT('Ctrl Pts',(-24.8036569302077,20.5807362393794,-36.208132980153));
#24545=CARTESIAN_POINT('Ctrl Pts',(-24.9408526069044,20.6413804498724,-36.2180779359786));
#24546=CARTESIAN_POINT('Ctrl Pts',(-25.0267605246285,20.6840296390332,-36.2243154452348));
#24547=CARTESIAN_POINT('Ctrl Pts',(-25.1163379353043,20.7335991338964,-36.2307341824454));
#24548=CARTESIAN_POINT('Ctrl Pts',(-25.1220185819203,20.736765133493,-36.2311408527865));
#24549=CARTESIAN_POINT('Ctrl Pts',(-25.1298631362062,20.7411683191897,-36.2317018654794));
#24550=CARTESIAN_POINT('Ctrl Pts',(-25.1320352006461,20.7423908251397,-36.2318571427362));
#24551=CARTESIAN_POINT('Ctrl Pts',(-25.1357594016681,20.744492615025,-36.2321232728048));
#24552=CARTESIAN_POINT('Ctrl Pts',(-25.1373122260006,20.7453706676105,-36.2322342051563));
#24553=CARTESIAN_POINT('Ctrl Pts',(-25.1404239611635,20.7471336257898,-36.2324564394005));
#24554=CARTESIAN_POINT('Ctrl Pts',(-25.141982859173,20.7480185406908,-36.2325677398724));
#24555=CARTESIAN_POINT('Ctrl Pts',(-25.1456527913991,20.7501058433916,-36.2328296852688));
#24556=CARTESIAN_POINT('Ctrl Pts',(-25.1477632107688,20.7513093212995,-36.2329802592536));
#24557=CARTESIAN_POINT('Ctrl Pts',(-25.1543247578681,20.7550609173236,-36.2334482330704));
#24558=CARTESIAN_POINT('Ctrl Pts',(-25.1587711930919,20.7576172915265,-36.2337650994647));
#24559=CARTESIAN_POINT('Ctrl Pts',(-25.1690552434334,20.763562576816,-36.2344974226032));
#24560=CARTESIAN_POINT('Ctrl Pts',(-25.1748883768447,20.766959249141,-36.2349123863569));
#24561=CARTESIAN_POINT('Ctrl Pts',(-25.194429921806,20.7784207850511,-36.2363013194906));
#24562=CARTESIAN_POINT('Ctrl Pts',(-25.2080895502048,20.7865689453835,-36.2372701443971));
#24563=CARTESIAN_POINT('Ctrl Pts',(-25.2648322335758,20.8209888417406,-36.241288529141));
#24564=CARTESIAN_POINT('Ctrl Pts',(-25.307357867116,20.8481708724137,-36.2442852071017));
#24565=CARTESIAN_POINT('Ctrl Pts',(-25.3853745700375,20.9006596492826,-36.2497888798089));
#24566=CARTESIAN_POINT('Ctrl Pts',(-25.4210236781023,20.9257085837828,-36.252306193674));
#24567=CARTESIAN_POINT('Ctrl Pts',(-25.6514857867871,21.0947257802935,-36.2686715727514));
#24568=CARTESIAN_POINT('Ctrl Pts',(-25.8300470098783,21.2595451344025,-36.2818490202066));
#24569=CARTESIAN_POINT('Ctrl Pts',(-26.0247025691532,21.4847535087805,-36.2988437550976));
#24570=CARTESIAN_POINT('Ctrl Pts',(-26.059855527674,21.5276103016235,-36.3020358228998));
#24571=CARTESIAN_POINT('Ctrl Pts',(-26.1529170837994,21.6472293699759,-36.3108678134954));
#24572=CARTESIAN_POINT('Ctrl Pts',(-26.2085193316717,21.7257047127247,-36.316579920768));
#24573=CARTESIAN_POINT('Ctrl Pts',(-26.2660363772201,21.8151043180859,-36.3230506979617));
#24574=CARTESIAN_POINT('Ctrl Pts',(-26.2715043773558,21.823692481319,-36.3236719287236));
#24575=CARTESIAN_POINT('Ctrl Pts',(-26.279159199267,21.8358420132757,-36.3245502871064));
#24576=CARTESIAN_POINT('Ctrl Pts',(-26.2813799692715,21.8393820089977,-36.324806155445));
#24577=CARTESIAN_POINT('Ctrl Pts',(-26.2852512800227,21.8455797779992,-36.3252540287319));
#24578=CARTESIAN_POINT('Ctrl Pts',(-26.2869048514074,21.8482356600234,-36.3254459213565));
#24579=CARTESIAN_POINT('Ctrl Pts',(-26.2903662573083,21.853813279013,-36.3258488521215));
#24580=CARTESIAN_POINT('Ctrl Pts',(-26.2921732909445,21.8567355057433,-36.3260599194598));
#24581=CARTESIAN_POINT('Ctrl Pts',(-26.2964695625054,21.8637080810914,-36.3265634532502));
#24582=CARTESIAN_POINT('Ctrl Pts',(-26.2989545125176,21.8677610504655,-36.3268560770918));
#24583=CARTESIAN_POINT('Ctrl Pts',(-26.3072826547232,21.8814119978205,-36.3278414603365));
#24584=CARTESIAN_POINT('Ctrl Pts',(-26.3130845649748,21.8910349517692,-36.3285357324788));
#24585=CARTESIAN_POINT('Ctrl Pts',(-26.3841916826027,22.0103791660734,-36.337142244481));
#24586=CARTESIAN_POINT('Ctrl Pts',(-26.442962298592,22.1238430735884,-36.3452913915235));
#24587=CARTESIAN_POINT('Ctrl Pts',(-26.6279278366797,22.5396774662571,-36.3750807452723));
#24588=CARTESIAN_POINT('Ctrl Pts',(-26.7146150198231,22.8573518750094,-36.3979247463531));
#24589=CARTESIAN_POINT('Ctrl Pts',(-26.753287476269,23.1941353647863,-36.4199456109359));
#24590=CARTESIAN_POINT('Ctrl Pts',(-26.7545493415196,23.2056741589855,-36.4206971687716));
#24591=CARTESIAN_POINT('Ctrl Pts',(-26.7559004212636,23.2186785251735,-36.421540720098));
#24592=CARTESIAN_POINT('Ctrl Pts',(-26.7560509913265,23.2201374760914,-36.4216353084687));
#24593=CARTESIAN_POINT('Ctrl Pts',(-26.7567841785441,23.2272895138481,-36.4220987553971));
#24594=CARTESIAN_POINT('Ctrl Pts',(-26.7573526307428,23.2329840825815,-36.4224670073818));
#24595=CARTESIAN_POINT('Ctrl Pts',(-26.7613538512331,23.2741768529497,-36.4251252510713));
#24596=CARTESIAN_POINT('Ctrl Pts',(-26.7642125082382,23.3097301887667,-36.4273896384842));
#24597=CARTESIAN_POINT('Ctrl Pts',(-26.7667755798403,23.3499563128329,-36.4299123549273));
#24598=CARTESIAN_POINT('Ctrl Pts',(-26.7670606435202,23.3545878520096,-36.4302022265622));
#24599=CARTESIAN_POINT('Ctrl Pts',(-26.7674765760817,23.3615923648447,-36.4306397088367));
#24600=CARTESIAN_POINT('Ctrl Pts',(-26.7676148235739,23.3639648691379,-36.4307877317938));
#24601=CARTESIAN_POINT('Ctrl Pts',(-26.7678505189788,23.368088238524,-36.4310447175752));
#24602=CARTESIAN_POINT('Ctrl Pts',(-26.7679491621894,23.3698390299326,-36.4311537480022));
#24603=CARTESIAN_POINT('Ctrl Pts',(-26.7681446429079,23.3733597251561,-36.4313728243968));
#24604=CARTESIAN_POINT('Ctrl Pts',(-26.7682414491004,23.3751296266156,-36.4314828682035));
#24605=CARTESIAN_POINT('Ctrl Pts',(-26.7684374609901,23.378768346817,-36.4317089248428));
#24606=CARTESIAN_POINT('Ctrl Pts',(-26.7685364993016,23.380637176569,-36.4318249282692));
#24607=CARTESIAN_POINT('Ctrl Pts',(-26.7687633113254,23.3849887897407,-36.432094818453));
#24608=CARTESIAN_POINT('Ctrl Pts',(-26.768889840363,23.3874716410754,-36.4322486350512));
#24609=CARTESIAN_POINT('Ctrl Pts',(-26.7692117558304,23.3939356623409,-36.432648650449));
#24610=CARTESIAN_POINT('Ctrl Pts',(-26.7694026302722,23.3979170679239,-36.4328945977752));
#24611=CARTESIAN_POINT('Ctrl Pts',(-26.7718441184784,23.4508983252572,-36.4361617893169));
#24612=CARTESIAN_POINT('Ctrl Pts',(-26.7729832684713,23.4999458302695,-36.4391218570173));
#24613=CARTESIAN_POINT('Ctrl Pts',(-26.7730022894476,23.5490029715869,-36.4420349701589));
#24614=CARTESIAN_POINT('Ctrl Pts',(-26.7730022880352,23.5489993342442,-36.442034754166));
#24615=CARTESIAN_POINT('Ctrl Pts',(-26.7731226824236,23.8586081559639,-36.4604199725195));
#24616=CARTESIAN_POINT('Ctrl Pts',(-26.7286291185953,24.166677826155,-36.4769583830802));
#24617=CARTESIAN_POINT('Ctrl Pts',(-26.6106445971748,24.5658621958784,-36.5007266761024));
#24618=CARTESIAN_POINT('Ctrl Pts',(-26.5754115693603,24.6664389785736,-36.5069124079058));
#24619=CARTESIAN_POINT('Ctrl Pts',(-26.5170162811,24.8099249044776,-36.5161463037913));
#24620=CARTESIAN_POINT('Ctrl Pts',(-26.497758421538,24.8543500260352,-36.5190639922646));
#24621=CARTESIAN_POINT('Ctrl Pts',(-26.4742180647302,24.9054665298931,-36.5224958313224));
#24622=CARTESIAN_POINT('Ctrl Pts',(-26.4709020715227,24.9125981864629,-36.5229763430071));
#24623=CARTESIAN_POINT('Ctrl Pts',(-26.4658136804945,24.9234377484307,-36.523709316094));
#24624=CARTESIAN_POINT('Ctrl Pts',(-26.4640602241464,24.9271545554474,-36.5239611201872));
#24625=CARTESIAN_POINT('Ctrl Pts',(-26.4608662819037,24.9338913410934,-36.5244183829616));
#24626=CARTESIAN_POINT('Ctrl Pts',(-26.4594281910258,24.9369124542422,-36.5246237581444));
#24627=CARTESIAN_POINT('Ctrl Pts',(-26.4565414703001,24.942952564269,-36.5250349988974));
#24628=CARTESIAN_POINT('Ctrl Pts',(-26.4550928347767,24.9459715538654,-36.5252408644747));
#24629=CARTESIAN_POINT('Ctrl Pts',(-26.4509970218497,24.9544733241031,-36.5258215014578));
#24630=CARTESIAN_POINT('Ctrl Pts',(-26.448339019196,24.9599508473441,-36.5261966502611));
#24631=CARTESIAN_POINT('Ctrl Pts',(-26.4372985426765,24.9825394966469,-36.5277481121702));
#24632=CARTESIAN_POINT('Ctrl Pts',(-26.4287800554097,24.9995833737066,-36.5289291783312));
#24633=CARTESIAN_POINT('Ctrl Pts',(-26.2409413313698,25.367223926891,-36.5546359636457));
#24634=CARTESIAN_POINT('Ctrl Pts',(-25.9990264197442,25.6820380512695,-36.5818310567475));
#24635=CARTESIAN_POINT('Ctrl Pts',(-25.6553338039435,25.9914608353772,-36.6125765604811));
#24636=CARTESIAN_POINT('Ctrl Pts',(-25.6026570842799,26.0359118095854,-36.6171012353082));
#24637=CARTESIAN_POINT('Ctrl Pts',(-25.5290207380977,26.0941110702211,-36.6231335693796));
#24638=CARTESIAN_POINT('Ctrl Pts',(-25.5092696464521,26.1093523558736,-36.6247241166773));
#24639=CARTESIAN_POINT('Ctrl Pts',(-25.4818311405541,26.130021918061,-36.6268939578447));
#24640=CARTESIAN_POINT('Ctrl Pts',(-25.4742945496475,26.1356477292025,-36.6274858839073));
#24641=CARTESIAN_POINT('Ctrl Pts',(-25.4630494465266,26.1439654149974,-36.6283629119021));
#24642=CARTESIAN_POINT('Ctrl Pts',(-25.4593597273105,26.1466824411394,-36.6286496995457));
#24643=CARTESIAN_POINT('Ctrl Pts',(-25.4534593734024,26.1510079515668,-36.629106730802));
#24644=CARTESIAN_POINT('Ctrl Pts',(-25.4512524821438,26.1526214957045,-36.6292773209922));
#24645=CARTESIAN_POINT('Ctrl Pts',(-25.4470517031678,26.1556846537209,-36.6296013637599));
#24646=CARTESIAN_POINT('Ctrl Pts',(-25.445058201822,26.1571347906275,-36.6297548525911));
#24647=CARTESIAN_POINT('Ctrl Pts',(-25.4415612856786,26.1596724293861,-36.6300235901554));
#24648=CARTESIAN_POINT('Ctrl Pts',(-25.4400585941273,26.1607609212289,-36.6301389083117));
#24649=CARTESIAN_POINT('Ctrl Pts',(-25.4371091201912,26.1628935250664,-36.6303649325153));
#24650=CARTESIAN_POINT('Ctrl Pts',(-25.4356624146057,26.163937730654,-36.6304756452222));
#24651=CARTESIAN_POINT('Ctrl Pts',(-25.4321917051512,26.1664384440263,-36.6307408892423));
#24652=CARTESIAN_POINT('Ctrl Pts',(-25.4301668727679,26.1678938078817,-36.6308953405985));
#24653=CARTESIAN_POINT('Ctrl Pts',(-25.4228495316242,26.1731403336719,-36.6314524459631));
#24654=CARTESIAN_POINT('Ctrl Pts',(-25.4175471807539,26.1769178398844,-36.6318541576432));
#24655=CARTESIAN_POINT('Ctrl Pts',(-25.3336242772035,26.2363237280344,-36.6381816288635));
#24656=CARTESIAN_POINT('Ctrl Pts',(-25.2525511894166,26.2884228562152,-36.6438712508975));
#24657=CARTESIAN_POINT('Ctrl Pts',(-25.1302072874201,26.3595051331081,-36.6520411793723));
#24658=CARTESIAN_POINT('Ctrl Pts',(-25.0906835825734,26.3813706203207,-36.6546198534541));
#24659=CARTESIAN_POINT('Ctrl Pts',(-24.9803745014667,26.4394021226365,-36.6616858728934));
#24660=CARTESIAN_POINT('Ctrl Pts',(-24.9086902925355,26.4737917666175,-36.6661328846431));
#24661=CARTESIAN_POINT('Ctrl Pts',(-24.6770562572351,26.5745543578447,-36.6802504920292));
#24662=CARTESIAN_POINT('Ctrl Pts',(-24.5130054242364,26.6307054342304,-36.6898950837052));
#24663=CARTESIAN_POINT('Ctrl Pts',(-24.2731425967293,26.6917623219269,-36.7042158602862));
#24664=CARTESIAN_POINT('Ctrl Pts',(-24.2004264567975,26.7076132126749,-36.7085820788708));
#24665=CARTESIAN_POINT('Ctrl Pts',(-24.0840942168914,26.7287825356893,-36.7156461421667));
#24666=CARTESIAN_POINT('Ctrl Pts',(-24.0408038186365,26.7357507780778,-36.7182918351085));
#24667=CARTESIAN_POINT('Ctrl Pts',(-23.989799781951,26.7428963361587,-36.7214330390408));
#24668=CARTESIAN_POINT('Ctrl Pts',(-23.9822095521032,26.7439321302631,-36.7219011227311));
#24669=CARTESIAN_POINT('Ctrl Pts',(-23.9705847695364,26.745476296607,-36.7226189890103));
#24670=CARTESIAN_POINT('Ctrl Pts',(-23.966552791346,26.7460041164715,-36.7228681554607));
#24671=CARTESIAN_POINT('Ctrl Pts',(-23.9592038132562,26.7469520156586,-36.7233226351609));
#24672=CARTESIAN_POINT('Ctrl Pts',(-23.9558871333161,26.7473745674167,-36.7235278698452));
#24673=CARTESIAN_POINT('Ctrl Pts',(-23.9492223186844,26.7482131403752,-36.7239405344045));
#24674=CARTESIAN_POINT('Ctrl Pts',(-23.9458741764859,26.7486290666945,-36.7241479670068));
#24675=CARTESIAN_POINT('Ctrl Pts',(-23.936357612786,26.7497960995351,-36.7247379228437));
#24676=CARTESIAN_POINT('Ctrl Pts',(-23.9301876883476,26.7505346211404,-36.725120843557));
#24677=CARTESIAN_POINT('Ctrl Pts',(-23.9040895705754,26.7535819522264,-36.7267424105417));
#24678=CARTESIAN_POINT('Ctrl Pts',(-23.884142523074,26.7557224614983,-36.7279863612598));
#24679=CARTESIAN_POINT('Ctrl Pts',(-23.4791881563278,26.7953571162515,-36.7533370871899));
#24680=CARTESIAN_POINT('Ctrl Pts',(-23.0906110243216,26.7633983339045,-36.7800015629711));
#24681=CARTESIAN_POINT('Ctrl Pts',(-22.6511380218023,26.6457945974664,-36.8103056219682));
#24682=CARTESIAN_POINT('Ctrl Pts',(-22.5856972573706,26.6260324265928,-36.8148056323885));
#24683=CARTESIAN_POINT('Ctrl Pts',(-22.4933035148485,26.5948914732856,-36.8210964104967));
#24684=CARTESIAN_POINT('Ctrl Pts',(-22.4658031784721,26.5852051252937,-36.8229606918076));
#24685=CARTESIAN_POINT('Ctrl Pts',(-22.4285404656924,26.5715090213875,-36.8254720875161));
#24686=CARTESIAN_POINT('Ctrl Pts',(-22.4186616794711,26.567822893068,-36.8261364696084));
#24687=CARTESIAN_POINT('Ctrl Pts',(-22.4041401391437,26.5623230464548,-36.8271108126719));
#24688=CARTESIAN_POINT('Ctrl Pts',(-22.399483338135,26.5605469801139,-36.8274229206833));
#24689=CARTESIAN_POINT('Ctrl Pts',(-22.3921247995831,26.5577209222319,-36.827915534507));
#24690=CARTESIAN_POINT('Ctrl Pts',(-22.3894203502868,26.5566780855262,-36.8280964605658));
#24691=CARTESIAN_POINT('Ctrl Pts',(-22.3843084645858,26.5546990143375,-36.8284382068131));
#24692=CARTESIAN_POINT('Ctrl Pts',(-22.3819007421156,26.5537635322724,-36.8285990718142));
#24693=CARTESIAN_POINT('Ctrl Pts',(-22.3777458456606,26.5521434615801,-36.8288764947333));
#24694=CARTESIAN_POINT('Ctrl Pts',(-22.3759981426294,26.5514602408596,-36.8289931357014));
#24695=CARTESIAN_POINT('Ctrl Pts',(-22.372618688603,26.550135724077,-36.8292185744765));
#24696=CARTESIAN_POINT('Ctrl Pts',(-22.3709868664623,26.5494946238196,-36.8293273840237));
#24697=CARTESIAN_POINT('Ctrl Pts',(-22.3671455372906,26.5479818463603,-36.829583413938));
#24698=CARTESIAN_POINT('Ctrl Pts',(-22.3649364655062,26.5471090560438,-36.8297305665844));
#24699=CARTESIAN_POINT('Ctrl Pts',(-22.3584192602511,26.5445258160049,-36.8301644509922));
#24700=CARTESIAN_POINT('Ctrl Pts',(-22.3541138262804,26.5428085037858,-36.8304507693996));
#24701=CARTESIAN_POINT('Ctrl Pts',(-22.3168365836751,26.5278463964645,-36.832927143454));
#24702=CARTESIAN_POINT('Ctrl Pts',(-22.2840805585796,26.5140657705026,-36.8350853630388));
#24703=CARTESIAN_POINT('Ctrl Pts',(-22.1918605764379,26.473460272828,-36.8411290034926));
#24704=CARTESIAN_POINT('Ctrl Pts',(-22.1329934191378,26.4453766498354,-36.8449480597098));
#24705=CARTESIAN_POINT('Ctrl Pts',(-22.0750359454076,26.4155367385478,-36.8487079434683));
#24706=CARTESIAN_POINT('Ctrl Pts',(-22.0750364532454,26.4155370000125,-37.0955933117774));
#24707=CARTESIAN_POINT('Ctrl Pts',(-22.1818001580695,26.4705052014922,-37.0878648110614));
#24708=CARTESIAN_POINT('Ctrl Pts',(-22.2915977141445,26.5194865689918,-37.0799401779364));
#24709=CARTESIAN_POINT('Ctrl Pts',(-22.6793682912363,26.6670676261741,-37.0521550768679));
#24710=CARTESIAN_POINT('Ctrl Pts',(-22.9678889264498,26.7336217801294,-37.0316988392698));
#24711=CARTESIAN_POINT('Ctrl Pts',(-23.2742693173491,26.7611895858928,-37.0122926530374));
#24712=CARTESIAN_POINT('Ctrl Pts',(-23.2871062481768,26.7622670938395,-37.0114839932028));
#24713=CARTESIAN_POINT('Ctrl Pts',(-23.303432721765,26.7635389724028,-37.0104614394955));
#24714=CARTESIAN_POINT('Ctrl Pts',(-23.306916352152,26.763804658643,-37.0102435969431));
#24715=CARTESIAN_POINT('Ctrl Pts',(-23.3124886367667,26.7642205274396,-37.0098957000135));
#24716=CARTESIAN_POINT('Ctrl Pts',(-23.3145770047589,26.7643743391979,-37.0097654408376));
#24717=CARTESIAN_POINT('Ctrl Pts',(-23.3183404813911,26.7646478377678,-37.0095309257412));
#24718=CARTESIAN_POINT('Ctrl Pts',(-23.3200155219303,26.7647682498288,-37.0094266293434));
#24719=CARTESIAN_POINT('Ctrl Pts',(-23.3239938779852,26.7650511125879,-37.0091791087641));
#24720=CARTESIAN_POINT('Ctrl Pts',(-23.3262972721948,26.7652123970623,-37.0090359514058));
#24721=CARTESIAN_POINT('Ctrl Pts',(-23.3321266006297,26.7656142735079,-37.0086740363678));
#24722=CARTESIAN_POINT('Ctrl Pts',(-23.3356527711888,26.7658515420788,-37.0084554662953));
#24723=CARTESIAN_POINT('Ctrl Pts',(-23.3547156750614,26.7671027485429,-37.007275723378));
#24724=CARTESIAN_POINT('Ctrl Pts',(-23.3702595606717,26.7680099080888,-37.0063204866648));
#24725=CARTESIAN_POINT('Ctrl Pts',(-23.6806216219765,26.7838669749509,-36.9873707650317));
#24726=CARTESIAN_POINT('Ctrl Pts',(-23.9761605115232,26.7583558899041,-36.9714544347291));
#24727=CARTESIAN_POINT('Ctrl Pts',(-24.4583366237232,26.64882672026,-36.9436049451794));
#24728=CARTESIAN_POINT('Ctrl Pts',(-24.6480019491708,26.5868142071439,-36.9321405980765));
#24729=CARTESIAN_POINT('Ctrl Pts',(-24.8383934972394,26.5043819107216,-36.9195291295822));
#24730=CARTESIAN_POINT('Ctrl Pts',(-24.8460568316879,26.5010284888284,-36.9190196418501));
#24731=CARTESIAN_POINT('Ctrl Pts',(-24.8582549540482,26.4956339934286,-36.9182056411506));
#24732=CARTESIAN_POINT('Ctrl Pts',(-24.8627982589755,26.4936121776381,-36.9179017877882));
#24733=CARTESIAN_POINT('Ctrl Pts',(-24.8714246283814,26.4897494127858,-36.9173235765552));
#24734=CARTESIAN_POINT('Ctrl Pts',(-24.8755085738406,26.4879104500785,-36.9170492874142));
#24735=CARTESIAN_POINT('Ctrl Pts',(-24.8826343016327,26.4846839177423,-36.9165697387077));
#24736=CARTESIAN_POINT('Ctrl Pts',(-24.8856777900358,26.4833001139089,-36.9163646092205));
#24737=CARTESIAN_POINT('Ctrl Pts',(-24.8915918674088,26.4806000062993,-36.9159654015663));
#24738=CARTESIAN_POINT('Ctrl Pts',(-24.8944626869059,26.4792842136612,-36.915771341228));
#24739=CARTESIAN_POINT('Ctrl Pts',(-24.9012339848637,26.4761686495352,-36.9153129629919));
#24740=CARTESIAN_POINT('Ctrl Pts',(-24.9051328013706,26.47436529799,-36.9150485214087));
#24741=CARTESIAN_POINT('Ctrl Pts',(-24.9186646541965,26.468073425422,-36.9141289130843));
#24742=CARTESIAN_POINT('Ctrl Pts',(-24.9282790055222,26.4635450913197,-36.9134723671469));
#24743=CARTESIAN_POINT('Ctrl Pts',(-25.0443425518691,26.4081763855203,-36.9055078073928));
#24744=CARTESIAN_POINT('Ctrl Pts',(-25.1479324417981,26.3515820047791,-36.897998072312));
#24745=CARTESIAN_POINT('Ctrl Pts',(-25.3288058286702,26.2394651356141,-36.8841218240613));
#24746=CARTESIAN_POINT('Ctrl Pts',(-25.4071822001974,26.1859547482682,-36.8778271556853));
#24747=CARTESIAN_POINT('Ctrl Pts',(-25.5392938429364,26.0869368599996,-36.8667524966644));
#24748=CARTESIAN_POINT('Ctrl Pts',(-25.5941139480393,26.0429785117665,-36.862006474762));
#24749=CARTESIAN_POINT('Ctrl Pts',(-25.7625151588359,25.8986510766886,-36.8469970142875));
#24750=CARTESIAN_POINT('Ctrl Pts',(-25.8704851319537,25.7920391618229,-36.836713848836));
#24751=CARTESIAN_POINT('Ctrl Pts',(-26.0046725470339,25.6394173201056,-36.8233723851675));
#24752=CARTESIAN_POINT('Ctrl Pts',(-26.0378526915846,25.5997971729503,-36.8200220751652));
#24753=CARTESIAN_POINT('Ctrl Pts',(-26.0854536892766,25.5400971853763,-36.8151584874253));
#24754=CARTESIAN_POINT('Ctrl Pts',(-26.1006180932762,25.5206236256763,-36.8136000076198));
#24755=CARTESIAN_POINT('Ctrl Pts',(-26.118150586085,25.4975674760254,-36.8117892564834));
#24756=CARTESIAN_POINT('Ctrl Pts',(-26.1207365479845,25.4941526918522,-36.8115219473492));
#24757=CARTESIAN_POINT('Ctrl Pts',(-26.1246808693452,25.4889225493197,-36.8111138834123));
#24758=CARTESIAN_POINT('Ctrl Pts',(-26.1260441212917,25.4871109131912,-36.8109727839044));
#24759=CARTESIAN_POINT('Ctrl Pts',(-26.1285140162168,25.4838214310551,-36.8107170326233));
#24760=CARTESIAN_POINT('Ctrl Pts',(-26.1296212968025,25.4823440783813,-36.8106023358032));
#24761=CARTESIAN_POINT('Ctrl Pts',(-26.1318647930798,25.4793454013391,-36.8103698622046));
#24762=CARTESIAN_POINT('Ctrl Pts',(-26.1330009293625,25.4778240303005,-36.8102520910679));
#24763=CARTESIAN_POINT('Ctrl Pts',(-26.1362647748683,25.4734454319254,-36.809913635124));
#24764=CARTESIAN_POINT('Ctrl Pts',(-26.1383891005508,25.4705856680496,-36.8096931890154));
#24765=CARTESIAN_POINT('Ctrl Pts',(-26.1476724996088,25.4580449849555,-36.8087291132581));
#24766=CARTESIAN_POINT('Ctrl Pts',(-26.154782150923,25.4483273478671,-36.8079889075632));
#24767=CARTESIAN_POINT('Ctrl Pts',(-26.276580515528,25.27987751124,-36.7952712207404));
#24768=CARTESIAN_POINT('Ctrl Pts',(-26.3766402942151,25.1110292659042,-36.7842407998931));
#24769=CARTESIAN_POINT('Ctrl Pts',(-26.5312661324533,24.7858241499196,-36.7640897792709));
#24770=CARTESIAN_POINT('Ctrl Pts',(-26.5903367750714,24.6323636279976,-36.7549764918937));
#24771=CARTESIAN_POINT('Ctrl Pts',(-26.6778332932944,24.3402872989219,-36.7375080872787));
#24772=CARTESIAN_POINT('Ctrl Pts',(-26.7093362909639,24.2030145175265,-36.7292521282823));
#24773=CARTESIAN_POINT('Ctrl Pts',(-26.7334530381549,24.0537043420488,-36.7200473415056));
#24774=CARTESIAN_POINT('Ctrl Pts',(-26.7350864177421,24.0432660241913,-36.7194027218723));
#24775=CARTESIAN_POINT('Ctrl Pts',(-26.7373626346129,24.028236054932,-36.7184728873856));
#24776=CARTESIAN_POINT('Ctrl Pts',(-26.7380469499211,24.0236506763662,-36.718188989758));
#24777=CARTESIAN_POINT('Ctrl Pts',(-26.7392181017893,24.0156854651227,-36.7176954439549));
#24778=CARTESIAN_POINT('Ctrl Pts',(-26.739709466716,24.012306297254,-36.7174859397762));
#24779=CARTESIAN_POINT('Ctrl Pts',(-26.7406444071193,24.0058040590447,-36.7170825722484));
#24780=CARTESIAN_POINT('Ctrl Pts',(-26.7410887699729,24.0026811041993,-36.7168887341169));
#24781=CARTESIAN_POINT('Ctrl Pts',(-26.7421254813436,23.9953176600328,-36.716431443899));
#24782=CARTESIAN_POINT('Ctrl Pts',(-26.7427139645895,23.9910766398913,-36.7161678695544));
#24783=CARTESIAN_POINT('Ctrl Pts',(-26.7444289284822,23.9785338609437,-36.7153877666544));
#24784=CARTESIAN_POINT('Ctrl Pts',(-26.7455314843335,23.9702289161191,-36.7148704811516));
#24785=CARTESIAN_POINT('Ctrl Pts',(-26.7549960068543,23.8967425880009,-36.7102864490859));
#24786=CARTESIAN_POINT('Ctrl Pts',(-26.7613943232522,23.8313280861149,-36.7061579510891));
#24787=CARTESIAN_POINT('Ctrl Pts',(-26.7671925918538,23.7448164684998,-36.7006289009842));
#24788=CARTESIAN_POINT('Ctrl Pts',(-26.768391966971,23.7238527012756,-36.6992837976909));
#24789=CARTESIAN_POINT('Ctrl Pts',(-26.7718346929764,23.6512402018618,-36.6946063877606));
#24790=CARTESIAN_POINT('Ctrl Pts',(-26.773040024557,23.5995522001169,-36.6912445666056));
#24791=CARTESIAN_POINT('Ctrl Pts',(-26.7728811535608,23.3855807961895,-36.6771997083351));
#24792=CARTESIAN_POINT('Ctrl Pts',(-26.7605037255032,23.2235558296569,-36.6662440056536));
#24793=CARTESIAN_POINT('Ctrl Pts',(-26.710004465697,22.8932709800689,-36.643626532723));
#24794=CARTESIAN_POINT('Ctrl Pts',(-26.6704762752376,22.7257093204273,-36.6319979907716));
#24795=CARTESIAN_POINT('Ctrl Pts',(-26.6057679240138,22.5248380811497,-36.6184114810434));
#24796=CARTESIAN_POINT('Ctrl Pts',(-26.5930900990038,22.4878077135424,-36.6159228844713));
#24797=CARTESIAN_POINT('Ctrl Pts',(-26.578114432191,22.4465349081901,-36.6131744992035));
#24798=CARTESIAN_POINT('Ctrl Pts',(-26.5764787318163,22.4420579335742,-36.6128767115571));
#24799=CARTESIAN_POINT('Ctrl Pts',(-26.5740014261304,22.4353238395941,-36.6124293167212));
#24800=CARTESIAN_POINT('Ctrl Pts',(-26.5731672217961,22.4330640330372,-36.6122792706444));
#24801=CARTESIAN_POINT('Ctrl Pts',(-26.5717184664743,22.429152950119,-36.6120197408775));
#24802=CARTESIAN_POINT('Ctrl Pts',(-26.5711050951413,22.4275012427643,-36.6119101863107));
#24803=CARTESIAN_POINT('Ctrl Pts',(-26.5698246799165,22.4240619418755,-36.6116821667021));
#24804=CARTESIAN_POINT('Ctrl Pts',(-26.5691574037859,22.4222744396219,-36.6115637163916));
#24805=CARTESIAN_POINT('Ctrl Pts',(-26.5675687387622,22.418030224266,-36.6112826054622));
#24806=CARTESIAN_POINT('Ctrl Pts',(-26.5666459336376,22.4155740346287,-36.6111200303186));
#24807=CARTESIAN_POINT('Ctrl Pts',(-26.5635588286077,22.4073876039012,-36.6105785218236));
#24808=CARTESIAN_POINT('Ctrl Pts',(-26.5613811746054,22.4016623613128,-36.6102003879903));
#24809=CARTESIAN_POINT('Ctrl Pts',(-26.5048478548731,22.2542971134466,-36.6004813482129));
#24810=CARTESIAN_POINT('Ctrl Pts',(-26.4405655351955,22.1166421818956,-36.5917321658582));
#24811=CARTESIAN_POINT('Ctrl Pts',(-26.19973517029,21.6835585904831,-36.5637208328264));
#24812=CARTESIAN_POINT('Ctrl Pts',(-25.9856858714323,21.4118035905615,-36.5450819728289));
#24813=CARTESIAN_POINT('Ctrl Pts',(-25.7175259722023,21.1649913424366,-36.5230454433827));
#24814=CARTESIAN_POINT('Ctrl Pts',(-25.7021778644842,21.1511355195344,-36.5217891244063));
#24815=CARTESIAN_POINT('Ctrl Pts',(-25.681989747927,21.133259865776,-36.5201425684659));
#24816=CARTESIAN_POINT('Ctrl Pts',(-25.6772695716875,21.1291049490659,-36.5197580060562));
#24817=CARTESIAN_POINT('Ctrl Pts',(-25.6699868931765,21.122732133314,-36.5191653002192));
#24818=CARTESIAN_POINT('Ctrl Pts',(-25.6674329839928,21.1205044007008,-36.5189575669462));
#24819=CARTESIAN_POINT('Ctrl Pts',(-25.6623772689153,21.1161084075038,-36.5185465696615));
#24820=CARTESIAN_POINT('Ctrl Pts',(-25.6598756261027,21.1139399650641,-36.5183433135708));
#24821=CARTESIAN_POINT('Ctrl Pts',(-25.6543223106103,21.109141276776,-36.5178923562123));
#24822=CARTESIAN_POINT('Ctrl Pts',(-25.6512690418472,21.1065128939125,-36.5176445782382));
#24823=CARTESIAN_POINT('Ctrl Pts',(-25.6425297714073,21.099018245474,-36.5169358306412));
#24824=CARTESIAN_POINT('Ctrl Pts',(-25.6368317641626,21.0941660757891,-36.5164742804625));
#24825=CARTESIAN_POINT('Ctrl Pts',(-25.6003389124298,21.0633090318379,-36.5135217323594));
#24826=CARTESIAN_POINT('Ctrl Pts',(-25.5690765561086,21.037864930152,-36.511007914727));
#24827=CARTESIAN_POINT('Ctrl Pts',(-25.4747252378456,20.9639716121331,-36.5034624939613));
#24828=CARTESIAN_POINT('Ctrl Pts',(-25.4103147885434,20.9172673753464,-36.4983641267141));
#24829=CARTESIAN_POINT('Ctrl Pts',(-25.218329737443,20.7886206919643,-36.4833136717069));
#24830=CARTESIAN_POINT('Ctrl Pts',(-25.0866289468455,20.713241588343,-36.4731572694925));
#24831=CARTESIAN_POINT('Ctrl Pts',(-24.7405448296714,20.5463448226812,-36.4471811271523));
#24832=CARTESIAN_POINT('Ctrl Pts',(-24.5206131289831,20.4682597647843,-36.4312873780352));
#24833=CARTESIAN_POINT('Ctrl Pts',(-24.2812336024695,20.4114691590066,-36.415757384098));
#24834=CARTESIAN_POINT('Ctrl Pts',(-24.2682760643001,20.4084796869861,-36.4149222209012));
#24835=CARTESIAN_POINT('Ctrl Pts',(-24.2517311926241,20.404770274817,-36.413863131888));
#24836=CARTESIAN_POINT('Ctrl Pts',(-24.248160876087,20.4039761796849,-36.4136350167718));
#24837=CARTESIAN_POINT('Ctrl Pts',(-24.2424877415917,20.4027245162911,-36.4132732426204));
#24838=CARTESIAN_POINT('Ctrl Pts',(-24.2403858175467,20.4022629762171,-36.4131393548287));
#24839=CARTESIAN_POINT('Ctrl Pts',(-24.2364960206088,20.4014129384777,-36.4128918654882));
#24840=CARTESIAN_POINT('Ctrl Pts',(-24.2347082908126,20.4010238604602,-36.4127782310411));
#24841=CARTESIAN_POINT('Ctrl Pts',(-24.2307179688395,20.4001589729111,-36.4125248374552));
#24842=CARTESIAN_POINT('Ctrl Pts',(-24.2285152134083,20.3996839520717,-36.4123851245607));
#24843=CARTESIAN_POINT('Ctrl Pts',(-24.2239253542042,20.3986991926628,-36.4120943497092));
#24844=CARTESIAN_POINT('Ctrl Pts',(-24.2215381645779,20.3981898546958,-36.4119433108896));
#24845=CARTESIAN_POINT('Ctrl Pts',(-24.2153568129213,20.3968783235349,-36.4115527085137));
#24846=CARTESIAN_POINT('Ctrl Pts',(-24.2115617635832,20.396080262813,-36.4113133803604));
#24847=CARTESIAN_POINT('Ctrl Pts',(-24.2004375837291,20.393761919072,-36.4106132426767));
#24848=CARTESIAN_POINT('Ctrl Pts',(-24.1931045254415,20.3922603046339,-36.4101534776245));
#24849=CARTESIAN_POINT('Ctrl Pts',(-24.1155988486123,20.3766703655162,-36.4053120563063));
#24850=CARTESIAN_POINT('Ctrl Pts',(-24.0449745415904,20.3648966421247,-36.4010560734304));
#24851=CARTESIAN_POINT('Ctrl Pts',(-23.8948817735102,20.3449881405634,-36.3922274650721));
#24852=CARTESIAN_POINT('Ctrl Pts',(-23.8153855835391,20.3374352335586,-36.3876777045289));
#24853=CARTESIAN_POINT('Ctrl Pts',(-23.6049510279843,20.3253069033151,-36.3757839736858));
#24854=CARTESIAN_POINT('Ctrl Pts',(-23.4738759926402,20.3257473208416,-36.3685241584834));
#24855=CARTESIAN_POINT('Ctrl Pts',(-23.1280552780243,20.3480124141352,-36.3490714349759));
#24856=CARTESIAN_POINT('Ctrl Pts',(-22.9148893781597,20.3834110551393,-36.3367367952457));
#24857=CARTESIAN_POINT('Ctrl Pts',(-22.6941767811211,20.44325642323,-36.3228456656794));
#24858=CARTESIAN_POINT('Ctrl Pts',(-22.6815055205312,20.4467755894092,-36.3220443369211));
#24859=CARTESIAN_POINT('Ctrl Pts',(-22.6643319584784,20.4516585884706,-36.320952962587));
#24860=CARTESIAN_POINT('Ctrl Pts',(-22.6598104583247,20.452954903015,-36.3206651205604));
#24861=CARTESIAN_POINT('Ctrl Pts',(-22.6521529254497,20.4551684721242,-36.3201767789445));
#24862=CARTESIAN_POINT('Ctrl Pts',(-22.6490154101578,20.456080608677,-36.3199764467883));
#24863=CARTESIAN_POINT('Ctrl Pts',(-22.6429754669886,20.4578465034749,-36.3195903200391));
#24864=CARTESIAN_POINT('Ctrl Pts',(-22.640072842781,20.4586995806194,-36.3194045479381));
#24865=CARTESIAN_POINT('Ctrl Pts',(-22.6332275488409,20.4607218788149,-36.3189659401813));
#24866=CARTESIAN_POINT('Ctrl Pts',(-22.6292859142401,20.4618945596411,-36.3187129914275));
#24867=CARTESIAN_POINT('Ctrl Pts',(-22.6178007378814,20.4653354720753,-36.3179747997104));
#24868=CARTESIAN_POINT('Ctrl Pts',(-22.6102632945252,20.4676238085501,-36.3174888979873));
#24869=CARTESIAN_POINT('Ctrl Pts',(-22.5561859923934,20.48425823154,-36.3139923162312));
#24870=CARTESIAN_POINT('Ctrl Pts',(-22.5099703623347,20.4996293295247,-36.3109480518948));
#24871=CARTESIAN_POINT('Ctrl Pts',(-22.3627238818848,20.5523378481134,-36.3010604485225));
#24872=CARTESIAN_POINT('Ctrl Pts',(-22.263218618272,20.5936909739957,-36.2940866565933));
#24873=CARTESIAN_POINT('Ctrl Pts',(-22.0124998480304,20.7129441289156,-36.2757662955648));
#24874=CARTESIAN_POINT('Ctrl Pts',(-21.865046638002,20.79796707663,-36.2642393396158));
#24875=CARTESIAN_POINT('Ctrl Pts',(-21.5771313945329,20.9958249234009,-36.2406128838094));
#24876=CARTESIAN_POINT('Ctrl Pts',(-21.4379889557836,21.1096241579081,-36.2285601998589));
#24877=CARTESIAN_POINT('Ctrl Pts',(-21.3009066345182,21.2422905762718,-36.2165404980373));
#24878=CARTESIAN_POINT('Ctrl Pts',(-21.2928246975247,21.2501949377664,-36.2158313324793));
#24879=CARTESIAN_POINT('Ctrl Pts',(-21.2823124365462,21.2605850084326,-36.2149084326304));
#24880=CARTESIAN_POINT('Ctrl Pts',(-21.2798444355367,21.263032227606,-36.2146917252203));
#24881=CARTESIAN_POINT('Ctrl Pts',(-21.2760466545972,21.2668102332616,-36.2143582071955));
#24882=CARTESIAN_POINT('Ctrl Pts',(-21.2747140827435,21.2681381898866,-36.2142411729082));
#24883=CARTESIAN_POINT('Ctrl Pts',(-21.2720885595176,21.2707592059578,-36.2140105678852));
#24884=CARTESIAN_POINT('Ctrl Pts',(-21.2707955532921,21.2720521915476,-36.2138969930042));
#24885=CARTESIAN_POINT('Ctrl Pts',(-21.2679203003728,21.2749322969241,-36.2136444195745));
#24886=CARTESIAN_POINT('Ctrl Pts',(-21.2663386120602,21.276519963282,-36.2135054659078));
#24887=CARTESIAN_POINT('Ctrl Pts',(-21.2630509578281,21.2798269351842,-36.2132166122395));
#24888=CARTESIAN_POINT('Ctrl Pts',(-21.2613452705144,21.2815465175545,-36.2130667344238));
#24889=CARTESIAN_POINT('Ctrl Pts',(-21.2569452490941,21.2859923959956,-36.2126800604422));
#24890=CARTESIAN_POINT('Ctrl Pts',(-21.2542538276504,21.2887215887428,-36.2124434931255));
#24891=CARTESIAN_POINT('Ctrl Pts',(-21.2464046053484,21.2967094212702,-36.2117534158122));
#24892=CARTESIAN_POINT('Ctrl Pts',(-21.2412599140774,21.3019809928191,-36.2113009144788));
#24893=CARTESIAN_POINT('Ctrl Pts',(-21.1876611514674,21.3572796580724,-36.2065839626036));
#24894=CARTESIAN_POINT('Ctrl Pts',(-21.1408186402256,21.4088515801244,-36.2024385803005));
#24895=CARTESIAN_POINT('Ctrl Pts',(-21.0488727828079,21.5169216021941,-36.1941548209046));
#24896=CARTESIAN_POINT('Ctrl Pts',(-21.0039254065023,21.5734989868452,-36.1900246960718));
#24897=CARTESIAN_POINT('Ctrl Pts',(-20.7543536877596,21.9103008554172,-36.1663062696027));
#24898=CARTESIAN_POINT('Ctrl Pts',(-20.5941768677858,22.2205512124119,-36.1475232007051));
#24899=CARTESIAN_POINT('Ctrl Pts',(-20.480085290229,22.5701388501849,-36.125289718227));
#24900=CARTESIAN_POINT('Ctrl Pts',(-20.4738270685922,22.589962961953,-36.1240266902884));
#24901=CARTESIAN_POINT('Ctrl Pts',(-20.465922369438,22.615873206881,-36.1223725560634));
#24902=CARTESIAN_POINT('Ctrl Pts',(-20.4641012442419,22.621905881726,-36.1219871894567));
#24903=CARTESIAN_POINT('Ctrl Pts',(-20.4613271866338,22.6311936225473,-36.1213935152513));
#24904=CARTESIAN_POINT('Ctrl Pts',(-20.4603616726461,22.6344449400733,-36.1211856199719));
#24905=CARTESIAN_POINT('Ctrl Pts',(-20.4584638951982,22.6408727710267,-36.1207744709013));
#24906=CARTESIAN_POINT('Ctrl Pts',(-20.4575313900382,22.6440492091991,-36.1205712253105));
#24907=CARTESIAN_POINT('Ctrl Pts',(-20.455476058479,22.6510905099913,-36.120120531337));
#24908=CARTESIAN_POINT('Ctrl Pts',(-20.4543555756043,22.6549560458985,-36.1198730067142));
#24909=CARTESIAN_POINT('Ctrl Pts',(-20.4511774820414,22.6659974070521,-36.1191656892814));
#24910=CARTESIAN_POINT('Ctrl Pts',(-20.4491375690422,22.6731782613215,-36.1187053195935));
#24911=CARTESIAN_POINT('Ctrl Pts',(-20.4363405771439,22.7188287350196,-36.115776281397));
#24912=CARTESIAN_POINT('Ctrl Pts',(-20.4262749658969,22.7574870385782,-36.1132852095718));
#24913=CARTESIAN_POINT('Ctrl Pts',(-20.3985070496801,22.8728898581411,-36.1058133343364));
#24914=CARTESIAN_POINT('Ctrl Pts',(-20.3828975020265,22.9501023987676,-36.1007671010837));
#24915=CARTESIAN_POINT('Ctrl Pts',(-20.3456661051738,23.176728242369,-36.0858170493578));
#24916=CARTESIAN_POINT('Ctrl Pts',(-20.3316936141314,23.3271725279076,-36.0757090336739));
#24917=CARTESIAN_POINT('Ctrl Pts',(-20.3238595866909,23.6766461001868,-36.0520800270863));
#24918=CARTESIAN_POINT('Ctrl Pts',(-20.3377822527856,23.8752634143697,-36.0385308482383));
#24919=CARTESIAN_POINT('Ctrl Pts',(-20.377356291198,24.1167929639755,-36.0227036340477));
#24920=CARTESIAN_POINT('Ctrl Pts',(-20.3857768522575,24.1620799896511,-36.0197662173081));
#24921=CARTESIAN_POINT('Ctrl Pts',(-20.3961827088941,24.2120576402219,-36.0165696893483));
#24922=CARTESIAN_POINT('Ctrl Pts',(-20.3972109282809,24.2169391872608,-36.0162579500095));
#24923=CARTESIAN_POINT('Ctrl Pts',(-20.3987641224817,24.224229122287,-36.0157931473617));
#24924=CARTESIAN_POINT('Ctrl Pts',(-20.3992805261228,24.2266392984727,-36.0156395963978));
#24925=CARTESIAN_POINT('Ctrl Pts',(-20.4001738928163,24.2307856224774,-36.0153756469721));
#24926=CARTESIAN_POINT('Ctrl Pts',(-20.4005495262702,24.2325220505968,-36.0152651718622));
#24927=CARTESIAN_POINT('Ctrl Pts',(-20.4013213784783,24.2360758431869,-36.01503920373));
#24928=CARTESIAN_POINT('Ctrl Pts',(-20.4017177340066,24.237893171887,-36.0149237193506));
#24929=CARTESIAN_POINT('Ctrl Pts',(-20.4026336844178,24.2420754988927,-36.0146581089266));
#24930=CARTESIAN_POINT('Ctrl Pts',(-20.4031543730134,24.2444402623517,-36.0145080462252));
#24931=CARTESIAN_POINT('Ctrl Pts',(-20.40426861698,24.2494737019514,-36.01418888265));
#24932=CARTESIAN_POINT('Ctrl Pts',(-20.4048629044418,24.2521422163872,-36.0140198239693));
#24933=CARTESIAN_POINT('Ctrl Pts',(-20.4064623333718,24.2592812668691,-36.0135679317684));
#24934=CARTESIAN_POINT('Ctrl Pts',(-20.4074736193994,24.2637504415804,-36.0132854473559));
#24935=CARTESIAN_POINT('Ctrl Pts',(-20.4105895559033,24.2773855344817,-36.0124248146525));
#24936=CARTESIAN_POINT('Ctrl Pts',(-20.4127248210161,24.286544508467,-36.0118483729121));
#24937=CARTESIAN_POINT('Ctrl Pts',(-20.4206701283094,24.3199627371146,-36.0097507603115));
#24938=CARTESIAN_POINT('Ctrl Pts',(-20.4267218518816,24.344164363953,-36.0082425398103));
#24939=CARTESIAN_POINT('Ctrl Pts',(-20.4594867013519,24.4690168634999,-36.0005067682971));
#24940=CARTESIAN_POINT('Ctrl Pts',(-20.4907881235879,24.5684091604007,-35.9944992791286));
#24941=CARTESIAN_POINT('Ctrl Pts',(-20.650077498447,24.9999980464501,-35.9683945667708));
#24942=CARTESIAN_POINT('Ctrl Pts',(-20.8277370423855,25.3111303006099,-35.9492060091754));
#24943=CARTESIAN_POINT('Ctrl Pts',(-21.0658790383776,25.6031635684743,-35.9264248461005));
#24944=CARTESIAN_POINT('Ctrl Pts',(-21.0792598747683,25.6192500272361,-35.925153634662));
#24945=CARTESIAN_POINT('Ctrl Pts',(-21.0968833364993,25.6400221522051,-35.9234902607903));
#24946=CARTESIAN_POINT('Ctrl Pts',(-21.100984638481,25.644827491231,-35.9231039179832));
#24947=CARTESIAN_POINT('Ctrl Pts',(-21.1075572341329,25.6524826509628,-35.9224859665967));
#24948=CARTESIAN_POINT('Ctrl Pts',(-21.110019462058,25.6553402630607,-35.9222547336004));
#24949=CARTESIAN_POINT('Ctrl Pts',(-21.1144616208505,25.660477476546,-35.9218380326047));
#24950=CARTESIAN_POINT('Ctrl Pts',(-21.1164397520709,25.6627586341387,-35.9216526395398));
#24951=CARTESIAN_POINT('Ctrl Pts',(-21.121083602554,25.6680986873764,-35.9212178015333));
#24952=CARTESIAN_POINT('Ctrl Pts',(-21.1237518942601,25.6711553304408,-35.9209682495042));
#24953=CARTESIAN_POINT('Ctrl Pts',(-21.1314466149519,25.6799364364569,-35.9202494556394));
#24954=CARTESIAN_POINT('Ctrl Pts',(-21.1364875530162,25.6856480976688,-35.9197796071069));
#24955=CARTESIAN_POINT('Ctrl Pts',(-21.1700857386549,25.7234457183815,-35.9166548617271));
#24956=CARTESIAN_POINT('Ctrl Pts',(-21.1992606143772,25.7549745790322,-35.9139739724777));
#24957=CARTESIAN_POINT('Ctrl Pts',(-21.2859458969972,25.8449765666889,-35.9060960928963));
#24958=CARTESIAN_POINT('Ctrl Pts',(-21.3450653380683,25.9018457059962,-35.9008300521178));
#24959=CARTESIAN_POINT('Ctrl Pts',(-21.5332913752687,26.0695625167543,-35.8843785522713));
#24960=CARTESIAN_POINT('Ctrl Pts',(-21.6690463963951,26.1724858591445,-35.8729222430422));
#24961=CARTESIAN_POINT('Ctrl Pts',(-21.8974531629939,26.3187544587974,-35.8545633502822));
#24962=CARTESIAN_POINT('Ctrl Pts',(-21.9851387481169,26.3692523867793,-35.8477131871593));
#24963=CARTESIAN_POINT('Ctrl Pts',(-22.0750360716487,26.4155368035442,-35.8409625058884));
#24964=CARTESIAN_POINT('Origin',(-23.5502525316942,23.5502525316942,-77.3107734492734));
#24965=CARTESIAN_POINT('',(-22.0750360068226,26.4155367701679,-34.3432429022327));
#24966=CARTESIAN_POINT('',(-22.0750360449252,26.4155367897853,-34.591474087242));
#24967=CARTESIAN_POINT('',(-22.0750360153461,26.4155367745563,-77.3107734492734));
#24968=CARTESIAN_POINT('Ctrl Pts',(-22.0750360068226,26.4155367701679,-34.3432429022327));
#24969=CARTESIAN_POINT('Ctrl Pts',(-22.0007070613304,26.3772678657451,-34.3484601301553));
#24970=CARTESIAN_POINT('Ctrl Pts',(-21.9278958678129,26.3361214753991,-34.3537789974476));
#24971=CARTESIAN_POINT('Ctrl Pts',(-21.6840503105524,26.1855166433196,-34.3723350494374));
#24972=CARTESIAN_POINT('Ctrl Pts',(-21.5218199711374,26.0627749939037,-34.3860246494312));
#24973=CARTESIAN_POINT('Ctrl Pts',(-21.3480496407231,25.9034410773503,-34.4019830935093));
#24974=CARTESIAN_POINT('Ctrl Pts',(-21.32420829208,25.8809007179502,-34.4042031017999));
#24975=CARTESIAN_POINT('Ctrl Pts',(-21.2730049423748,25.8309889135581,-34.4090328186539));
#24976=CARTESIAN_POINT('Ctrl Pts',(-21.2457830416468,25.8034803249169,-34.4116405938142));
#24977=CARTESIAN_POINT('Ctrl Pts',(-21.1576217685169,25.7111212547255,-34.4202052703184));
#24978=CARTESIAN_POINT('Ctrl Pts',(-21.0988680152868,25.6442324726953,-34.4261083234741));
#24979=CARTESIAN_POINT('Ctrl Pts',(-21.0135340926948,25.538560847403,-34.4348911343555));
#24980=CARTESIAN_POINT('Ctrl Pts',(-20.9849094514715,25.5014895385991,-34.4378769243289));
#24981=CARTESIAN_POINT('Ctrl Pts',(-20.9541522088457,25.4598088526623,-34.4411181652541));
#24982=CARTESIAN_POINT('Ctrl Pts',(-20.9512124616709,25.4558057176336,-34.4414283047594));
#24983=CARTESIAN_POINT('Ctrl Pts',(-20.9468613481896,25.4498518854977,-34.4418878353512));
#24984=CARTESIAN_POINT('Ctrl Pts',(-20.9454429126368,25.447906401049,-34.4420377178228));
#24985=CARTESIAN_POINT('Ctrl Pts',(-20.9430263346966,25.4445840792636,-34.4422932028219));
#24986=CARTESIAN_POINT('Ctrl Pts',(-20.9420271019281,25.4432080414735,-34.4423988819344));
#24987=CARTESIAN_POINT('Ctrl Pts',(-20.9399776514924,25.4403810512575,-34.4426157105413));
#24988=CARTESIAN_POINT('Ctrl Pts',(-20.9389275565582,25.4389300173834,-34.4427268514098));
#24989=CARTESIAN_POINT('Ctrl Pts',(-20.9364033023714,25.4354358427831,-34.4429941200044));
#24990=CARTESIAN_POINT('Ctrl Pts',(-20.9349303254307,25.4333918434727,-34.4431501650312));
#24991=CARTESIAN_POINT('Ctrl Pts',(-20.9304189952879,25.4271161236867,-34.4436283597811));
#24992=CARTESIAN_POINT('Ctrl Pts',(-20.9273884853667,25.4228787348662,-34.4439499679695));
#24993=CARTESIAN_POINT('Ctrl Pts',(-20.8929677935398,25.3745027707147,-34.4476073694678));
#24994=CARTESIAN_POINT('Ctrl Pts',(-20.862682553646,25.3295837488004,-34.45086875531));
#24995=CARTESIAN_POINT('Ctrl Pts',(-20.8317322380585,25.2810836304513,-34.4542738180806));
#24996=CARTESIAN_POINT('Ctrl Pts',(-20.8299269940291,25.2782449647298,-34.4544726975441));
#24997=CARTESIAN_POINT('Ctrl Pts',(-20.8237610995519,25.268515761665,-34.455152931108));
#24998=CARTESIAN_POINT('Ctrl Pts',(-20.8194221267253,25.2616114533222,-34.4556332520465));
#24999=CARTESIAN_POINT('Ctrl Pts',(-20.6471027308161,24.985087359384,-34.47477775252));
#25000=CARTESIAN_POINT('Ctrl Pts',(-20.519865127747,24.692106104075,-34.49171133187));
#25001=CARTESIAN_POINT('Ctrl Pts',(-20.4078696954906,24.2745906162874,-34.5166057051041));
#25002=CARTESIAN_POINT('Ctrl Pts',(-20.3841170084978,24.1624755286081,-34.5233394322785));
#25003=CARTESIAN_POINT('Ctrl Pts',(-20.3643995472534,24.0366909339388,-34.531045497961));
#25004=CARTESIAN_POINT('Ctrl Pts',(-20.3624917911599,24.0240278069181,-34.531822924568));
#25005=CARTESIAN_POINT('Ctrl Pts',(-20.3596950511249,24.0046818124729,-34.5330132473564));
#25006=CARTESIAN_POINT('Ctrl Pts',(-20.3587514647754,23.9980068692688,-34.5334244183703));
#25007=CARTESIAN_POINT('Ctrl Pts',(-20.3572411559676,23.9870755560331,-34.5340985722942));
#25008=CARTESIAN_POINT('Ctrl Pts',(-20.356661981368,23.982820903975,-34.534361161105));
#25009=CARTESIAN_POINT('Ctrl Pts',(-20.3555611067497,23.9746110799345,-34.5348682399654));
#25010=CARTESIAN_POINT('Ctrl Pts',(-20.3550382441824,23.9706560696495,-34.5351126927685));
#25011=CARTESIAN_POINT('Ctrl Pts',(-20.3540990298016,23.9634487390712,-34.5355584833958));
#25012=CARTESIAN_POINT('Ctrl Pts',(-20.3536802944851,23.960196729889,-34.5357597455015));
#25013=CARTESIAN_POINT('Ctrl Pts',(-20.3528437746979,23.95362088154,-34.5361669550568));
#25014=CARTESIAN_POINT('Ctrl Pts',(-20.3524262086116,23.9502970195201,-34.536372909126));
#25015=CARTESIAN_POINT('Ctrl Pts',(-20.3512634741268,23.9409233995366,-34.5369540723475));
#25016=CARTESIAN_POINT('Ctrl Pts',(-20.3505302887072,23.9348721936124,-34.5373296600194));
#25017=CARTESIAN_POINT('Ctrl Pts',(-20.3475695185783,23.909841549475,-34.5388850052883));
#25018=CARTESIAN_POINT('Ctrl Pts',(-20.345493636209,23.8908448696746,-34.5400695456273));
#25019=CARTESIAN_POINT('Ctrl Pts',(-20.3043252140318,23.4803282855601,-34.5657602552088));
#25020=CARTESIAN_POINT('Ctrl Pts',(-20.3371107642028,23.0849936398098,-34.5929304633547));
#25021=CARTESIAN_POINT('Ctrl Pts',(-20.447889439639,22.6771401084044,-34.6210306599174));
#25022=CARTESIAN_POINT('Ctrl Pts',(-20.455984439751,22.6488718552089,-34.6229754463904));
#25023=CARTESIAN_POINT('Ctrl Pts',(-20.4796015916718,22.5704697376549,-34.6283546355779));
#25024=CARTESIAN_POINT('Ctrl Pts',(-20.4959638763564,22.5205957816201,-34.6317596995402));
#25025=CARTESIAN_POINT('Ctrl Pts',(-20.5220038048327,22.4473171555432,-34.6367155914255));
#25026=CARTESIAN_POINT('Ctrl Pts',(-20.530750016865,22.4235931085398,-34.6383126122323));
#25027=CARTESIAN_POINT('Ctrl Pts',(-20.5413136857066,22.3959461722155,-34.6401629004444));
#25028=CARTESIAN_POINT('Ctrl Pts',(-20.5428606115146,22.3919218408371,-34.6404319615473));
#25029=CARTESIAN_POINT('Ctrl Pts',(-20.5452354656427,22.3857804786619,-34.6408421386363));
#25030=CARTESIAN_POINT('Ctrl Pts',(-20.5460575580257,22.3836612194446,-34.6409836048683));
#25031=CARTESIAN_POINT('Ctrl Pts',(-20.5475514847994,22.3798221003069,-34.6412397334357));
#25032=CARTESIAN_POINT('Ctrl Pts',(-20.548222552607,22.3781019541438,-34.6413544415352));
#25033=CARTESIAN_POINT('Ctrl Pts',(-20.5496896773327,22.3743508018939,-34.6416044734099));
#25034=CARTESIAN_POINT('Ctrl Pts',(-20.5504863160596,22.3723200324708,-34.6417397610191));
#25035=CARTESIAN_POINT('Ctrl Pts',(-20.5526705971863,22.3667685100034,-34.642109402514));
#25036=CARTESIAN_POINT('Ctrl Pts',(-20.5540623856115,22.3632493756113,-34.6423435054442));
#25037=CARTESIAN_POINT('Ctrl Pts',(-20.5608395694614,22.3462011449741,-34.6434766003094));
#25038=CARTESIAN_POINT('Ctrl Pts',(-20.5663105294902,22.3327059219045,-34.6443704842288));
#25039=CARTESIAN_POINT('Ctrl Pts',(-20.5752425792796,22.311095088351,-34.6457977035683));
#25040=CARTESIAN_POINT('Ctrl Pts',(-20.5786457694912,22.3029559987285,-34.6463342572363));
#25041=CARTESIAN_POINT('Ctrl Pts',(-20.5841268726297,22.2899971281019,-34.6471871585642));
#25042=CARTESIAN_POINT('Ctrl Pts',(-20.5861831842435,22.2851683400622,-34.6475046618648));
#25043=CARTESIAN_POINT('Ctrl Pts',(-20.5900432745282,22.2761648591229,-34.6480961230076));
#25044=CARTESIAN_POINT('Ctrl Pts',(-20.5918441079075,22.2719889273544,-34.6483702340477));
#25045=CARTESIAN_POINT('Ctrl Pts',(-20.7187095768812,21.9795062117621,-34.6675547678833));
#25046=CARTESIAN_POINT('Ctrl Pts',(-20.885281299253,21.7109931078188,-34.6843320588523));
#25047=CARTESIAN_POINT('Ctrl Pts',(-21.1846121611122,21.3565741653778,-34.7107036559407));
#25048=CARTESIAN_POINT('Ctrl Pts',(-21.288921514363,21.2491978969512,-34.7193927242447));
#25049=CARTESIAN_POINT('Ctrl Pts',(-21.4114337467225,21.1394860133782,-34.7293273802282));
#25050=CARTESIAN_POINT('Ctrl Pts',(-21.4226382767905,21.1295917600281,-34.7302335402359));
#25051=CARTESIAN_POINT('Ctrl Pts',(-21.4396042541796,21.1148186076509,-34.7316022234323));
#25052=CARTESIAN_POINT('Ctrl Pts',(-21.4453147804074,21.1098813280773,-34.7320623261927));
#25053=CARTESIAN_POINT('Ctrl Pts',(-21.4545581187579,21.1019461869807,-34.7328061663514));
#25054=CARTESIAN_POINT('Ctrl Pts',(-21.4580801640693,21.0989357806865,-34.7330893856879));
#25055=CARTESIAN_POINT('Ctrl Pts',(-21.4648362951719,21.0931862637637,-34.7336322726783));
#25056=CARTESIAN_POINT('Ctrl Pts',(-21.4680693185103,21.090445915105,-34.7338918886557));
#25057=CARTESIAN_POINT('Ctrl Pts',(-21.473832642943,21.0855803573383,-34.7343543887707));
#25058=CARTESIAN_POINT('Ctrl Pts',(-21.4763608294608,21.0834526434339,-34.734557169713));
#25059=CARTESIAN_POINT('Ctrl Pts',(-21.4813703605777,21.0792497822283,-34.7349587730184));
#25060=CARTESIAN_POINT('Ctrl Pts',(-21.4838515663761,21.0771744746477,-34.7351575884958));
#25061=CARTESIAN_POINT('Ctrl Pts',(-21.4905751321485,21.0715679936455,-34.7356960776725));
#25062=CARTESIAN_POINT('Ctrl Pts',(-21.4948234321514,21.0680439897889,-34.7360360433035));
#25063=CARTESIAN_POINT('Ctrl Pts',(-21.5106382774997,21.054993869995,-34.7373005899759));
#25064=CARTESIAN_POINT('Ctrl Pts',(-21.5222620254094,21.0455376599134,-34.7382280019356));
#25065=CARTESIAN_POINT('Ctrl Pts',(-21.7236658190774,20.8840116914442,-34.7542641705081));
#25066=CARTESIAN_POINT('Ctrl Pts',(-21.9299506997231,20.7538558993812,-34.7702790478333));
#25067=CARTESIAN_POINT('Ctrl Pts',(-22.3002996017339,20.5750184727055,-34.7980339945754));
#25068=CARTESIAN_POINT('Ctrl Pts',(-22.4572358536001,20.5138537552655,-34.809503254034));
#25069=CARTESIAN_POINT('Ctrl Pts',(-22.6941778985265,20.4422711913237,-34.8258774608988));
#25070=CARTESIAN_POINT('Ctrl Pts',(-22.7709526250061,20.4221371593679,-34.8310411096143));
#25071=CARTESIAN_POINT('Ctrl Pts',(-22.8634935673152,20.4014878722634,-34.8370362593162));
#25072=CARTESIAN_POINT('Ctrl Pts',(-22.8786126342737,20.3982283206955,-34.8380084971034));
#25073=CARTESIAN_POINT('Ctrl Pts',(-22.8973957773432,20.3943201099858,-34.8392068985248));
#25074=CARTESIAN_POINT('Ctrl Pts',(-22.9010379470199,20.393568858047,-34.8394388360333));
#25075=CARTESIAN_POINT('Ctrl Pts',(-22.9067821638133,20.3923943895788,-34.8398039318364));
#25076=CARTESIAN_POINT('Ctrl Pts',(-22.908883332392,20.391966966658,-34.8399373316242));
#25077=CARTESIAN_POINT('Ctrl Pts',(-22.9128150729242,20.3911712514396,-34.8401866724768));
#25078=CARTESIAN_POINT('Ctrl Pts',(-22.9146455259582,20.3908024555917,-34.8403026417883));
#25079=CARTESIAN_POINT('Ctrl Pts',(-22.9187602749238,20.3899771452007,-34.8405630801412));
#25080=CARTESIAN_POINT('Ctrl Pts',(-22.9210447410607,20.3895215173342,-34.840707497394));
#25081=CARTESIAN_POINT('Ctrl Pts',(-22.9268608490722,20.38836807272,-34.84107473288));
#25082=CARTESIAN_POINT('Ctrl Pts',(-22.9303931804206,20.3876736936584,-34.8412973537434));
#25083=CARTESIAN_POINT('Ctrl Pts',(-22.9500060562038,20.3838523529132,-34.842531168888));
#25084=CARTESIAN_POINT('Ctrl Pts',(-22.9661094790974,20.3808420432346,-34.8435357724718));
#25085=CARTESIAN_POINT('Ctrl Pts',(-23.2954234300031,20.321876612571,-34.8639207198055));
#25086=CARTESIAN_POINT('Ctrl Pts',(-23.6152476167728,20.3124748506111,-34.8809142840806));
#25087=CARTESIAN_POINT('Ctrl Pts',(-24.0912524206191,20.3691550261273,-34.9080681707626));
#25088=CARTESIAN_POINT('Ctrl Pts',(-24.2495220094252,20.4001614242365,-34.9173911876216));
#25089=CARTESIAN_POINT('Ctrl Pts',(-24.4197797009324,20.4469830502476,-34.9280526331369));
#25090=CARTESIAN_POINT('Ctrl Pts',(-24.4347307075587,20.4512111773565,-34.9289941738301));
#25091=CARTESIAN_POINT('Ctrl Pts',(-24.4571085370988,20.4577147274604,-34.9304116353184));
#25092=CARTESIAN_POINT('Ctrl Pts',(-24.4645588061848,20.4599091980298,-34.9308849233698));
#25093=CARTESIAN_POINT('Ctrl Pts',(-24.4765279614739,20.4634817741447,-34.9316475150072));
#25094=CARTESIAN_POINT('Ctrl Pts',(-24.4810519081484,20.4648429313501,-34.9319362643678));
#25095=CARTESIAN_POINT('Ctrl Pts',(-24.489687509176,20.4674619171001,-34.9324884387447));
#25096=CARTESIAN_POINT('Ctrl Pts',(-24.4937996742933,20.4687180373627,-34.9327518073116));
#25097=CARTESIAN_POINT('Ctrl Pts',(-24.5010769097955,20.4709569063961,-34.9332186532455));
#25098=CARTESIAN_POINT('Ctrl Pts',(-24.5042430074497,20.471936316942,-34.9334220206767));
#25099=CARTESIAN_POINT('Ctrl Pts',(-24.5104731382611,20.4738740998323,-34.9338227088392));
#25100=CARTESIAN_POINT('Ctrl Pts',(-24.5135372620037,20.4748321705845,-34.9340200194574));
#25101=CARTESIAN_POINT('Ctrl Pts',(-24.5208886265292,20.4771428128864,-34.9344939874453));
#25102=CARTESIAN_POINT('Ctrl Pts',(-24.5251744705691,20.4784997771241,-34.9347707892889));
#25103=CARTESIAN_POINT('Ctrl Pts',(-24.5407169959546,20.4834565848637,-34.9357763531983));
#25104=CARTESIAN_POINT('Ctrl Pts',(-24.5519565872076,20.487109339865,-34.9365068587834));
#25105=CARTESIAN_POINT('Ctrl Pts',(-24.5684619984128,20.4925739919557,-34.9375845858127));
#25106=CARTESIAN_POINT('Ctrl Pts',(-24.5737437111569,20.4943378772204,-34.9379302092753));
#25107=CARTESIAN_POINT('Ctrl Pts',(-24.8212023356703,20.5776928715304,-34.9541588400366));
#25108=CARTESIAN_POINT('Ctrl Pts',(-25.0527674979565,20.6877677715634,-34.9710531016189));
#25109=CARTESIAN_POINT('Ctrl Pts',(-25.3438339885319,20.8712531007473,-34.9943074855896));
#25110=CARTESIAN_POINT('Ctrl Pts',(-25.416826391595,20.9215885100657,-35.0003205387278));
#25111=CARTESIAN_POINT('Ctrl Pts',(-25.5736540245098,21.0395661349323,-35.0135462940109));
#25112=CARTESIAN_POINT('Ctrl Pts',(-25.6563690687709,21.1085366119362,-35.0207325778132));
#25113=CARTESIAN_POINT('Ctrl Pts',(-25.7728937280232,21.2160343936901,-35.0310091404875));
#25114=CARTESIAN_POINT('Ctrl Pts',(-25.8094840205728,21.2514306556499,-35.0342599627752));
#25115=CARTESIAN_POINT('Ctrl Pts',(-25.8487638998067,21.2912730071509,-35.037761145719));
#25116=CARTESIAN_POINT('Ctrl Pts',(-25.8522965001119,21.2948730580924,-35.0380761250755));
#25117=CARTESIAN_POINT('Ctrl Pts',(-25.857513573421,21.3002147723891,-35.0385414311324));
#25118=CARTESIAN_POINT('Ctrl Pts',(-25.8592045354802,21.3019500437548,-35.0386922672959));
#25119=CARTESIAN_POINT('Ctrl Pts',(-25.8620806909837,21.304908231908,-35.0389488571369));
#25120=CARTESIAN_POINT('Ctrl Pts',(-25.8632668721975,21.3061301813426,-35.0390546891388));
#25121=CARTESIAN_POINT('Ctrl Pts',(-25.8656950077818,21.308635505552,-35.0392713478928));
#25122=CARTESIAN_POINT('Ctrl Pts',(-25.8669368613937,21.3099189698054,-35.0393821667457));
#25123=CARTESIAN_POINT('Ctrl Pts',(-25.8699145708484,21.3130015764623,-35.0396479140008));
#25124=CARTESIAN_POINT('Ctrl Pts',(-25.8716494045566,21.3148017110894,-35.0398027617657));
#25125=CARTESIAN_POINT('Ctrl Pts',(-25.8779228914398,21.3213265166366,-35.040362807074));
#25126=CARTESIAN_POINT('Ctrl Pts',(-25.8824492698307,21.3260630477092,-35.040767049165));
#25127=CARTESIAN_POINT('Ctrl Pts',(-25.9552488809461,21.4027092063204,-35.0472719542793));
#25128=CARTESIAN_POINT('Ctrl Pts',(-26.0201901213056,21.4777268717888,-35.0531222631274));
#25129=CARTESIAN_POINT('Ctrl Pts',(-26.261188018089,21.7835706489239,-35.0755737946021));
#25130=CARTESIAN_POINT('Ctrl Pts',(-26.4091955186267,22.0347318964159,-35.091192604325));
#25131=CARTESIAN_POINT('Ctrl Pts',(-26.5524904703607,22.3759205460712,-35.1125630636644));
#25132=CARTESIAN_POINT('Ctrl Pts',(-26.5806507470381,22.4506283064672,-35.1172412866173));
#25133=CARTESIAN_POINT('Ctrl Pts',(-26.6198092890893,22.5674881632556,-35.1246057655479));
#25134=CARTESIAN_POINT('Ctrl Pts',(-26.6327762319027,22.6089492607536,-35.1272272637293));
#25135=CARTESIAN_POINT('Ctrl Pts',(-26.6470337324432,22.6579957608249,-35.1303425716459));
#25136=CARTESIAN_POINT('Ctrl Pts',(-26.6491405704215,22.6653407438188,-35.1308094748594));
#25137=CARTESIAN_POINT('Ctrl Pts',(-26.6523274107163,22.6766018524368,-35.1315259048349));
#25138=CARTESIAN_POINT('Ctrl Pts',(-26.6534261734689,22.6805126779563,-35.1317748193054));
#25139=CARTESIAN_POINT('Ctrl Pts',(-26.6553288187353,22.6873342661966,-35.1322091893514));
#25140=CARTESIAN_POINT('Ctrl Pts',(-26.6561360116098,22.6902441071061,-35.132394536813));
#25141=CARTESIAN_POINT('Ctrl Pts',(-26.6578145979914,22.6963284114237,-35.132782216677));
#25142=CARTESIAN_POINT('Ctrl Pts',(-26.6586852193673,22.6995030825916,-35.1329845739717));
#25143=CARTESIAN_POINT('Ctrl Pts',(-26.6610781248953,22.7082813865251,-35.1335443195804));
#25144=CARTESIAN_POINT('Ctrl Pts',(-26.6625901250463,22.7138877877499,-35.1339020418571));
#25145=CARTESIAN_POINT('Ctrl Pts',(-26.668456001228,22.7358742726036,-35.1353058433818));
#25146=CARTESIAN_POINT('Ctrl Pts',(-26.6726957229336,22.7522842828809,-35.1363556203747));
#25147=CARTESIAN_POINT('Ctrl Pts',(-26.7409505708434,23.0253429737005,-35.1538592873905));
#25148=CARTESIAN_POINT('Ctrl Pts',(-26.7732447749159,23.2888228325633,-35.1713988181561));
#25149=CARTESIAN_POINT('Ctrl Pts',(-26.772793207378,23.7789236503551,-35.204549075384));
#25150=CARTESIAN_POINT('Ctrl Pts',(-26.7488758700027,24.0040026005548,-35.2199369079335));
#25151=CARTESIAN_POINT('Ctrl Pts',(-26.6987903335703,24.2380105592995,-35.2350465306056));
#25152=CARTESIAN_POINT('Ctrl Pts',(-26.6958689391363,24.2512509818375,-35.2358982074512));
#25153=CARTESIAN_POINT('Ctrl Pts',(-26.6920474792217,24.2680656306222,-35.2369753193334));
#25154=CARTESIAN_POINT('Ctrl Pts',(-26.6912247834463,24.2716570308128,-35.2372051169407));
#25155=CARTESIAN_POINT('Ctrl Pts',(-26.6899104170286,24.277349900225,-35.2375689568062));
#25156=CARTESIAN_POINT('Ctrl Pts',(-26.6894227944469,24.2794522860702,-35.237703232253));
#25157=CARTESIAN_POINT('Ctrl Pts',(-26.6885096552618,24.2833713968149,-35.2379533663661));
#25158=CARTESIAN_POINT('Ctrl Pts',(-26.6880846755762,24.2851882301525,-35.2380692550396));
#25159=CARTESIAN_POINT('Ctrl Pts',(-26.6871299196235,24.2892539889667,-35.2383284395581));
#25160=CARTESIAN_POINT('Ctrl Pts',(-26.6865993038172,24.2915027093179,-35.2384716858026));
#25161=CARTESIAN_POINT('Ctrl Pts',(-26.6850306586588,24.2981187013265,-35.2388928273668));
#25162=CARTESIAN_POINT('Ctrl Pts',(-26.6839859169533,24.3024843999823,-35.2391703346865));
#25163=CARTESIAN_POINT('Ctrl Pts',(-26.6759971432169,24.33556187814,-35.2412700459277));
#25164=CARTESIAN_POINT('Ctrl Pts',(-26.6686674798507,24.3641803586769,-35.2430702961006));
#25165=CARTESIAN_POINT('Ctrl Pts',(-26.6424579619655,24.4609581587167,-35.249114825901));
#25166=CARTESIAN_POINT('Ctrl Pts',(-26.6217274525139,24.5285993442453,-35.2532663110832));
#25167=CARTESIAN_POINT('Ctrl Pts',(-26.5457432739953,24.7502104834999,-35.2667887112144));
#25168=CARTESIAN_POINT('Ctrl Pts',(-26.4809982209221,24.9006599313651,-35.2758495961854));
#25169=CARTESIAN_POINT('Ctrl Pts',(-26.3268836477632,25.1948986463688,-35.2944304041234));
#25170=CARTESIAN_POINT('Ctrl Pts',(-26.2370685923919,25.337863538251,-35.3039316651154));
#25171=CARTESIAN_POINT('Ctrl Pts',(-26.1293323375663,25.4827661252396,-35.3145301944914));
#25172=CARTESIAN_POINT('Ctrl Pts',(-26.1221219819609,25.492351643448,-35.3152360457092));
#25173=CARTESIAN_POINT('Ctrl Pts',(-26.0734315999069,25.5563344356934,-35.3199801803744));
#25174=CARTESIAN_POINT('Ctrl Pts',(-26.0302846707244,25.6094360464178,-35.3240770040704));
#25175=CARTESIAN_POINT('Ctrl Pts',(-25.9793159503632,25.6682367448302,-35.3288167679961));
#25176=CARTESIAN_POINT('Ctrl Pts',(-25.9731176227499,25.675324522614,-35.3293915621143));
#25177=CARTESIAN_POINT('Ctrl Pts',(-25.963994148034,25.6856653980409,-35.3302353124002));
#25178=CARTESIAN_POINT('Ctrl Pts',(-25.9610932562936,25.6889399096257,-35.3305032525866));
#25179=CARTESIAN_POINT('Ctrl Pts',(-25.9559364178062,25.6947370981578,-35.3309789698046));
#25180=CARTESIAN_POINT('Ctrl Pts',(-25.9536831433146,25.6972621522331,-35.3311866342528));
#25181=CARTESIAN_POINT('Ctrl Pts',(-25.9489913528764,25.7025032032666,-35.3316186235982));
#25182=CARTESIAN_POINT('Ctrl Pts',(-25.9465521928283,25.7052186148157,-35.331842975524));
#25183=CARTESIAN_POINT('Ctrl Pts',(-25.940243519563,25.7122178331288,-35.3324226534303));
#25184=CARTESIAN_POINT('Ctrl Pts',(-25.9363671123541,25.716495383724,-35.3327782712085));
#25185=CARTESIAN_POINT('Ctrl Pts',(-25.9200847484293,25.7343659687307,-35.3342696459927));
#25186=CARTESIAN_POINT('Ctrl Pts',(-25.9075741612623,25.747862814132,-35.3354098555917));
#25187=CARTESIAN_POINT('Ctrl Pts',(-25.8225516701534,25.8380265464535,-35.3431218734403));
#25188=CARTESIAN_POINT('Ctrl Pts',(-25.7464350338262,25.9111912373882,-35.3498507788165));
#25189=CARTESIAN_POINT('Ctrl Pts',(-25.5522071166439,26.0803548767304,-35.3666304963467));
#25190=CARTESIAN_POINT('Ctrl Pts',(-25.4306267117162,26.1719742093008,-35.3768231084262));
#25191=CARTESIAN_POINT('Ctrl Pts',(-25.1090873148588,26.3803717305367,-35.4027306334987));
#25192=CARTESIAN_POINT('Ctrl Pts',(-24.902148397357,26.4848632156532,-35.4185125111137));
#25193=CARTESIAN_POINT('Ctrl Pts',(-24.6732284693989,26.5710509133089,-35.4339548712004));
#25194=CARTESIAN_POINT('Ctrl Pts',(-24.6606338391312,26.5757031074226,-35.4347981624847));
#25195=CARTESIAN_POINT('Ctrl Pts',(-24.6445590105154,26.5815269117716,-35.4358661222886));
#25196=CARTESIAN_POINT('Ctrl Pts',(-24.6411056236721,26.5827713805962,-35.4360950649816));
#25197=CARTESIAN_POINT('Ctrl Pts',(-24.635621471982,26.584737079355,-35.4364578529398));
#25198=CARTESIAN_POINT('Ctrl Pts',(-24.6335921103004,26.5854621725633,-35.4365919291411));
#25199=CARTESIAN_POINT('Ctrl Pts',(-24.6298386752978,26.5867990351575,-35.4368395949772));
#25200=CARTESIAN_POINT('Ctrl Pts',(-24.6281148194717,26.5874113681351,-35.4369532178803));
#25201=CARTESIAN_POINT('Ctrl Pts',(-24.6242698576531,26.5887734559585,-35.4372063724033));
#25202=CARTESIAN_POINT('Ctrl Pts',(-24.6221484923312,26.5895224560834,-35.4373458581969));
#25203=CARTESIAN_POINT('Ctrl Pts',(-24.6177289696364,26.5910776743824,-35.437636070281));
#25204=CARTESIAN_POINT('Ctrl Pts',(-24.6154306779065,26.5918835104441,-35.4377867736952));
#25205=CARTESIAN_POINT('Ctrl Pts',(-24.60948259095,26.5939614835027,-35.4381762478616));
#25206=CARTESIAN_POINT('Ctrl Pts',(-24.6058314033714,26.5952296658916,-35.4384147850919));
#25207=CARTESIAN_POINT('Ctrl Pts',(-24.5951349559917,26.5989233568611,-35.4391120477866));
#25208=CARTESIAN_POINT('Ctrl Pts',(-24.5880834972502,26.6013310246709,-35.4395697390501));
#25209=CARTESIAN_POINT('Ctrl Pts',(-24.5137318223007,26.6264302621811,-35.4443756338971));
#25210=CARTESIAN_POINT('Ctrl Pts',(-24.445701495991,26.6469176209216,-35.4486000670434));
#25211=CARTESIAN_POINT('Ctrl Pts',(-24.3007011453494,26.6854053665977,-35.4573508684769));
#25212=CARTESIAN_POINT('Ctrl Pts',(-24.2236347675704,26.7028568755086,-35.4618552314217));
#25213=CARTESIAN_POINT('Ctrl Pts',(-23.8120524852248,26.7802751058987,-35.4854956806251));
#25214=CARTESIAN_POINT('Ctrl Pts',(-23.470311643524,26.7898800181453,-35.5039590711322));
#25215=CARTESIAN_POINT('Ctrl Pts',(-23.1137147143978,26.7433615719101,-35.5257141041009));
#25216=CARTESIAN_POINT('Ctrl Pts',(-23.0940803238998,26.7406157552393,-35.5269190354536));
#25217=CARTESIAN_POINT('Ctrl Pts',(-23.0683555791806,26.7367758949315,-35.5285074249098));
#25218=CARTESIAN_POINT('Ctrl Pts',(-23.0622409811886,26.7358451834671,-35.5288856948257));
#25219=CARTESIAN_POINT('Ctrl Pts',(-23.0528009056605,26.7343804791909,-35.5294708158884));
#25220=CARTESIAN_POINT('Ctrl Pts',(-23.0494734991666,26.7338588620555,-35.5296772736403));
#25221=CARTESIAN_POINT('Ctrl Pts',(-23.0428441129958,26.7328089634501,-35.5300890449534));
#25222=CARTESIAN_POINT('Ctrl Pts',(-23.0395421255566,26.7322807568371,-35.5302943558999));
#25223=CARTESIAN_POINT('Ctrl Pts',(-23.0322171070506,26.7310973055674,-35.530750289477));
#25224=CARTESIAN_POINT('Ctrl Pts',(-23.0281944898826,26.7304395666653,-35.5310009911626));
#25225=CARTESIAN_POINT('Ctrl Pts',(-23.0165705046972,26.728516277686,-35.5317263660063));
#25226=CARTESIAN_POINT('Ctrl Pts',(-23.0089724530998,26.7272310994357,-35.5322016633369));
#25227=CARTESIAN_POINT('Ctrl Pts',(-22.9572207793516,26.7182864826373,-35.5354469557434));
#25228=CARTESIAN_POINT('Ctrl Pts',(-22.9132283329123,26.7097343905958,-35.5382452937435));
#25229=CARTESIAN_POINT('Ctrl Pts',(-22.8163890395407,26.6888042241506,-35.544497113407));
#25230=CARTESIAN_POINT('Ctrl Pts',(-22.7636486034597,26.6760030091301,-35.5479632841837));
#25231=CARTESIAN_POINT('Ctrl Pts',(-22.6342331843538,26.641108466781,-35.5566226176568));
#25232=CARTESIAN_POINT('Ctrl Pts',(-22.5580103071176,26.6174883683902,-35.5618589955983));
#25233=CARTESIAN_POINT('Ctrl Pts',(-22.3428831416392,26.54196597949,-35.5770063263489));
#25234=CARTESIAN_POINT('Ctrl Pts',(-22.2066622590385,26.4833057049606,-35.5870567917328));
#25235=CARTESIAN_POINT('Ctrl Pts',(-22.0750357765539,26.4155366516121,-35.5970690335682));
#25236=CARTESIAN_POINT('',(-26.773002305904,23.5490461609309,-35.4331262776897));
#25237=CARTESIAN_POINT('Ctrl Pts',(-22.0750360716487,26.4155368035442,-35.8409625058884));
#25238=CARTESIAN_POINT('Ctrl Pts',(-22.1102710601675,26.4336778430016,-35.8383165964471));
#25239=CARTESIAN_POINT('Ctrl Pts',(-22.1458458370451,26.4511716035792,-35.8356862541541));
#25240=CARTESIAN_POINT('Ctrl Pts',(-22.251482879974,26.5007183571307,-35.8280127797491));
#25241=CARTESIAN_POINT('Ctrl Pts',(-22.3223804309384,26.5309208493099,-35.8230368370741));
#25242=CARTESIAN_POINT('Ctrl Pts',(-22.4000755463446,26.5607755364305,-35.817820286076));
#25243=CARTESIAN_POINT('Ctrl Pts',(-22.4058586657744,26.5629786295714,-35.8174333947282));
#25244=CARTESIAN_POINT('Ctrl Pts',(-22.4139306478428,26.5660270742643,-35.8168953569739));
#25245=CARTESIAN_POINT('Ctrl Pts',(-22.416214130997,26.5668864871443,-35.816743371817));
#25246=CARTESIAN_POINT('Ctrl Pts',(-22.4201558521784,26.5683648871744,-35.8164813996653));
#25247=CARTESIAN_POINT('Ctrl Pts',(-22.4218136237979,26.5689851012564,-35.8163713386144));
#25248=CARTESIAN_POINT('Ctrl Pts',(-22.425218250789,26.5702556614475,-35.8161455429463));
#25249=CARTESIAN_POINT('Ctrl Pts',(-22.426965156706,26.5709058567447,-35.8160298179407));
#25250=CARTESIAN_POINT('Ctrl Pts',(-22.4310705455282,26.5724298213702,-35.8157581574488));
#25251=CARTESIAN_POINT('Ctrl Pts',(-22.4334294954344,26.5733023483818,-35.8156022971143));
#25252=CARTESIAN_POINT('Ctrl Pts',(-22.4384200396872,26.5751416093315,-35.8152730549435));
#25253=CARTESIAN_POINT('Ctrl Pts',(-22.4410518811418,26.5761076735091,-35.8150997132645));
#25254=CARTESIAN_POINT('Ctrl Pts',(-22.4481475888601,26.5787017774224,-35.814633137517));
#25255=CARTESIAN_POINT('Ctrl Pts',(-22.4526138219289,26.580323389359,-35.8143402830806));
#25256=CARTESIAN_POINT('Ctrl Pts',(-22.4663785782171,26.5852867068029,-35.8134401962355));
#25257=CARTESIAN_POINT('Ctrl Pts',(-22.47568900116,26.5885955695641,-35.8128348596844));
#25258=CARTESIAN_POINT('Ctrl Pts',(-22.5101965692175,26.6006808732127,-35.8106036145321));
#25259=CARTESIAN_POINT('Ctrl Pts',(-22.5354879749682,26.6091873903452,-35.8089925511983));
#25260=CARTESIAN_POINT('Ctrl Pts',(-22.6250410973573,26.6380747305811,-35.8033636111943));
#25261=CARTESIAN_POINT('Ctrl Pts',(-22.6898372002171,26.6567535884842,-35.7994269386415));
#25262=CARTESIAN_POINT('Ctrl Pts',(-23.1353794936148,26.770178206605,-35.7729834020887));
#25263=CARTESIAN_POINT('Ctrl Pts',(-23.5300430090044,26.7967389386153,-35.7521744414144));
#25264=CARTESIAN_POINT('Ctrl Pts',(-23.9389670105545,26.7495320474123,-35.7272640303427));
#25265=CARTESIAN_POINT('Ctrl Pts',(-23.9580757106773,26.7471523730092,-35.7260934507402));
#25266=CARTESIAN_POINT('Ctrl Pts',(-23.9832220495494,26.7437916881667,-35.7245440337353));
#25267=CARTESIAN_POINT('Ctrl Pts',(-23.9892801281293,26.7429645005491,-35.7241700715772));
#25268=CARTESIAN_POINT('Ctrl Pts',(-23.9986575567256,26.7416568847585,-35.7235901304561));
#25269=CARTESIAN_POINT('Ctrl Pts',(-24.0019785951039,26.7411885032755,-35.7233845335682));
#25270=CARTESIAN_POINT('Ctrl Pts',(-24.0086109207714,26.7402425539957,-35.7229735226799));
#25271=CARTESIAN_POINT('Ctrl Pts',(-24.0119222076893,26.7397650125216,-35.7227681097491));
#25272=CARTESIAN_POINT('Ctrl Pts',(-24.0192906216346,26.7386906523412,-35.7223105469557));
#25273=CARTESIAN_POINT('Ctrl Pts',(-24.023347360047,26.7380912450151,-35.7220583152393));
#25274=CARTESIAN_POINT('Ctrl Pts',(-24.0351389005028,26.7363259706419,-35.7213242368148));
#25275=CARTESIAN_POINT('Ctrl Pts',(-24.0428705751676,26.7351396899056,-35.7208417425549));
#25276=CARTESIAN_POINT('Ctrl Pts',(-24.097428146185,26.7265654347395,-35.7174287829519));
#25277=CARTESIAN_POINT('Ctrl Pts',(-24.1440882455517,26.7181735485475,-35.7144665292356));
#25278=CARTESIAN_POINT('Ctrl Pts',(-24.2904466673276,26.688503768653,-35.7050312468401));
#25279=CARTESIAN_POINT('Ctrl Pts',(-24.3893221687627,26.6635252045523,-35.6984430715252));
#25280=CARTESIAN_POINT('Ctrl Pts',(-24.6284224582453,26.5909040938203,-35.6819927431484));
#25281=CARTESIAN_POINT('Ctrl Pts',(-24.7668648740075,26.5382050817035,-35.6720093853569));
#25282=CARTESIAN_POINT('Ctrl Pts',(-24.9665288773683,26.4460181806787,-35.6571229153511));
#25283=CARTESIAN_POINT('Ctrl Pts',(-25.0308432890317,26.413668094698,-35.6522499022575));
#25284=CARTESIAN_POINT('Ctrl Pts',(-25.1987209230725,26.3220562659645,-35.6393937959507));
#25285=CARTESIAN_POINT('Ctrl Pts',(-25.3001795653451,26.2591462882303,-35.6314789242579));
#25286=CARTESIAN_POINT('Ctrl Pts',(-25.4002781557176,26.1891028491708,-35.6236839281037));
#25287=CARTESIAN_POINT('Ctrl Pts',(-25.4026286123673,26.1874534462055,-35.6235009004112));
#25288=CARTESIAN_POINT('Ctrl Pts',(-25.4244144518681,26.1721220156394,-35.6218045739079));
#25289=CARTESIAN_POINT('Ctrl Pts',(-25.4437008155392,26.1582280245069,-35.6203037122082));
#25290=CARTESIAN_POINT('Ctrl Pts',(-25.4661264770231,26.1416925442678,-35.618561251092));
#25291=CARTESIAN_POINT('Ctrl Pts',(-25.46941597309,26.1392573595785,-35.6183057280522));
#25292=CARTESIAN_POINT('Ctrl Pts',(-25.4746698179196,26.1353524696976,-35.6178977397995));
#25293=CARTESIAN_POINT('Ctrl Pts',(-25.4766371292445,26.1338867866548,-35.6177449954255));
#25294=CARTESIAN_POINT('Ctrl Pts',(-25.4800846194524,26.1313122164113,-35.6174773793935));
#25295=CARTESIAN_POINT('Ctrl Pts',(-25.4815655184702,26.1302043006607,-35.6173624392838));
#25296=CARTESIAN_POINT('Ctrl Pts',(-25.4846446890758,26.1278965214748,-35.6171234849175));
#25297=CARTESIAN_POINT('Ctrl Pts',(-25.4862427953862,26.126696448323,-35.616999486122));
#25298=CARTESIAN_POINT('Ctrl Pts',(-25.4903536107411,26.1236035108993,-35.6166805716164));
#25299=CARTESIAN_POINT('Ctrl Pts',(-25.4928646739391,26.1217084469489,-35.6164858112233));
#25300=CARTESIAN_POINT('Ctrl Pts',(-25.5031164000837,26.1139480272504,-35.6156908490718));
#25301=CARTESIAN_POINT('Ctrl Pts',(-25.5108334105347,26.1080512934506,-35.6150928392398));
#25302=CARTESIAN_POINT('Ctrl Pts',(-25.5304873217621,26.0928921076946,-35.6135704978678));
#25303=CARTESIAN_POINT('Ctrl Pts',(-25.5423861053713,26.0835803197966,-35.6126495022508));
#25304=CARTESIAN_POINT('Ctrl Pts',(-25.5913610248482,26.0446949261278,-35.6088593843651));
#25305=CARTESIAN_POINT('Ctrl Pts',(-25.6278494990012,26.014386882081,-35.6060371482327));
#25306=CARTESIAN_POINT('Ctrl Pts',(-25.7307068847924,25.9250417818928,-35.5980423371901));
#25307=CARTESIAN_POINT('Ctrl Pts',(-25.7953244459871,25.8640501281224,-35.5929704918099));
#25308=CARTESIAN_POINT('Ctrl Pts',(-26.0948797477136,25.5569227432061,-35.5687497110011));
#25309=CARTESIAN_POINT('Ctrl Pts',(-26.292333685706,25.2773414137618,-35.5502689330145));
#25310=CARTESIAN_POINT('Ctrl Pts',(-26.4512012453136,24.9541794048019,-35.5284858410977));
#25311=CARTESIAN_POINT('Ctrl Pts',(-26.4598205427123,24.9362280241387,-35.5272756019372));
#25312=CARTESIAN_POINT('Ctrl Pts',(-26.4709027943603,24.9125880252599,-35.5256811838719));
#25313=CARTESIAN_POINT('Ctrl Pts',(-26.4735166138941,24.9069702837387,-35.5253022423404));
#25314=CARTESIAN_POINT('Ctrl Pts',(-26.4775271931732,24.8982851642112,-35.5247163051081));
#25315=CARTESIAN_POINT('Ctrl Pts',(-26.4789353788422,24.8952230528402,-35.5245097045662));
#25316=CARTESIAN_POINT('Ctrl Pts',(-26.4817311405975,24.8891184362096,-35.524097790502));
#25317=CARTESIAN_POINT('Ctrl Pts',(-26.4831187899893,24.8860759689611,-35.5238924798248));
#25318=CARTESIAN_POINT('Ctrl Pts',(-26.4861859744864,24.8793232479665,-35.5234367533396));
#25319=CARTESIAN_POINT('Ctrl Pts',(-26.4878632147489,24.8756119636666,-35.523186258876));
#25320=CARTESIAN_POINT('Ctrl Pts',(-26.4926868982587,24.8648843017093,-35.5224621049292));
#25321=CARTESIAN_POINT('Ctrl Pts',(-26.495815254209,24.8578598650942,-35.5219878245647));
#25322=CARTESIAN_POINT('Ctrl Pts',(-26.5168579384732,24.8101517381909,-35.5187658258118));
#25323=CARTESIAN_POINT('Ctrl Pts',(-26.5339532387647,24.7691140584656,-35.5159902273843));
#25324=CARTESIAN_POINT('Ctrl Pts',(-26.5527607584845,24.7211971406555,-35.512742594729));
#25325=CARTESIAN_POINT('Ctrl Pts',(-26.5553064642967,24.7146484223127,-35.5122986046544));
#25326=CARTESIAN_POINT('Ctrl Pts',(-26.5997588381729,24.5991798668501,-35.504467495601));
#25327=CARTESIAN_POINT('Ctrl Pts',(-26.635735585645,24.4880831732943,-35.4968877360105));
#25328=CARTESIAN_POINT('Ctrl Pts',(-26.7370147295979,24.1056518915583,-35.470687784072));
#25329=CARTESIAN_POINT('Ctrl Pts',(-26.7731066982184,23.8279241956221,-35.4513695415814));
#25330=CARTESIAN_POINT('Ctrl Pts',(-26.773002305904,23.5490461609309,-35.4331262776897));
#25331=CARTESIAN_POINT('Ctrl Pts',(-26.7730023043127,23.5490419171598,-35.4331260000766));
#25332=CARTESIAN_POINT('Ctrl Pts',(-26.7729772287911,23.4822889340426,-35.4287592473437));
#25333=CARTESIAN_POINT('Ctrl Pts',(-26.7708781614745,23.4155458727867,-35.4244662071997));
#25334=CARTESIAN_POINT('Ctrl Pts',(-26.7664586286456,23.3449437509865,-35.4200355072642));
#25335=CARTESIAN_POINT('Ctrl Pts',(-26.7662030275764,23.3409781616955,-35.4197870141426));
#25336=CARTESIAN_POINT('Ctrl Pts',(-26.765775929236,23.3345374468629,-35.419384037734));
#25337=CARTESIAN_POINT('Ctrl Pts',(-26.7656089083806,23.3320620439012,-35.4192293064516));
#25338=CARTESIAN_POINT('Ctrl Pts',(-26.7653110094593,23.3277215389382,-35.4189582536014));
#25339=CARTESIAN_POINT('Ctrl Pts',(-26.7651813668746,23.3258563575859,-35.4188418626807));
#25340=CARTESIAN_POINT('Ctrl Pts',(-26.7649255672512,23.3222218686168,-35.4186152298821));
#25341=CARTESIAN_POINT('Ctrl Pts',(-26.7647995723652,23.3204525486392,-35.4185049787189));
#25342=CARTESIAN_POINT('Ctrl Pts',(-26.7645459770347,23.316932383729,-35.4182857816497));
#25343=CARTESIAN_POINT('Ctrl Pts',(-26.7644184069459,23.3151815411187,-35.4181768341698));
#25344=CARTESIAN_POINT('Ctrl Pts',(-26.7641142346499,23.3110534530344,-35.417920137494));
#25345=CARTESIAN_POINT('Ctrl Pts',(-26.7639364250196,23.3086762935752,-35.4177724568808));
#25346=CARTESIAN_POINT('Ctrl Pts',(-26.7634025997687,23.3016444151936,-35.4173360056764));
#25347=CARTESIAN_POINT('Ctrl Pts',(-26.7630391056958,23.296990244488,-35.4170476553558));
#25348=CARTESIAN_POINT('Ctrl Pts',(-26.7597522742334,23.2560518271307,-35.4145157738777));
#25349=CARTESIAN_POINT('Ctrl Pts',(-26.7562243361318,23.2198168870903,-35.4123056700737));
#25350=CARTESIAN_POINT('Ctrl Pts',(-26.7508322708735,23.1727240080317,-35.409464540639));
#25351=CARTESIAN_POINT('Ctrl Pts',(-26.749525617909,23.161806680405,-35.4088080873048));
#25352=CARTESIAN_POINT('Ctrl Pts',(-26.7478631325033,23.1484940620951,-35.4080100514496));
#25353=CARTESIAN_POINT('Ctrl Pts',(-26.7475604569788,23.14609234896,-35.4078661759724));
#25354=CARTESIAN_POINT('Ctrl Pts',(-26.7458586310083,23.1327100165865,-35.4070650330177));
#25355=CARTESIAN_POINT('Ctrl Pts',(-26.7444056038027,23.1217361937076,-35.4064100676666));
#25356=CARTESIAN_POINT('Ctrl Pts',(-26.7412587244769,23.0988755296853,-35.4050493938619));
#25357=CARTESIAN_POINT('Ctrl Pts',(-26.7395549243022,23.0869902128819,-35.4043440936909));
#25358=CARTESIAN_POINT('Ctrl Pts',(-26.6899075509956,22.7539235962406,-35.3846317756214));
#25359=CARTESIAN_POINT('Ctrl Pts',(-26.5937600794297,22.4417934065153,-35.3673435633832));
#25360=CARTESIAN_POINT('Ctrl Pts',(-26.4186385468106,22.0790053562045,-35.3440268468972));
#25361=CARTESIAN_POINT('Ctrl Pts',(-26.382178021969,22.0099917746236,-35.3394427555385));
#25362=CARTESIAN_POINT('Ctrl Pts',(-26.3234807842531,21.9080305979578,-35.3323991552882));
#25363=CARTESIAN_POINT('Ctrl Pts',(-26.3030795179905,21.8740570806548,-35.3300050819726));
#25364=CARTESIAN_POINT('Ctrl Pts',(-26.2781062722816,21.8341560876949,-35.3271335975027));
#25365=CARTESIAN_POINT('Ctrl Pts',(-26.2741329988635,21.8278564581246,-35.3266784491115));
#25366=CARTESIAN_POINT('Ctrl Pts',(-26.2679810834712,21.8181771147889,-35.3259763256984));
#25367=CARTESIAN_POINT('Ctrl Pts',(-26.2658178757311,21.814787581595,-35.3257299252481));
#25368=CARTESIAN_POINT('Ctrl Pts',(-26.2620210750723,21.8088628494251,-35.3252982985042));
#25369=CARTESIAN_POINT('Ctrl Pts',(-26.2603902529755,21.8063258732707,-35.325113175787));
#25370=CARTESIAN_POINT('Ctrl Pts',(-26.2566971850662,21.8005984709031,-35.3246945683901));
#25371=CARTESIAN_POINT('Ctrl Pts',(-26.2546328571561,21.7974093985914,-35.3244610060081));
#25372=CARTESIAN_POINT('Ctrl Pts',(-26.2490551403864,21.7888259834855,-35.3238310774499));
#25373=CARTESIAN_POINT('Ctrl Pts',(-26.2455312326205,21.7834385265459,-35.323434317128));
#25374=CARTESIAN_POINT('Ctrl Pts',(-26.2299135711976,21.7597172304439,-35.3216812232514));
#25375=CARTESIAN_POINT('Ctrl Pts',(-26.2176489510915,21.7414970880346,-35.3203184627856));
#25376=CARTESIAN_POINT('Ctrl Pts',(-26.1979493648319,21.7128678096268,-35.3181509062968));
#25377=CARTESIAN_POINT('Ctrl Pts',(-26.1906368642594,21.7023749097116,-35.3173508118052));
#25378=CARTESIAN_POINT('Ctrl Pts',(-26.1757047245593,21.6812179892695,-35.3157259779533));
#25379=CARTESIAN_POINT('Ctrl Pts',(-26.1680821070627,21.6705563743447,-35.3149011346751));
#25380=CARTESIAN_POINT('Ctrl Pts',(-26.1563518490074,21.6543592278252,-35.3136387239792));
#25381=CARTESIAN_POINT('Ctrl Pts',(-26.1522910672432,21.6487897974573,-35.3132029465036));
#25382=CARTESIAN_POINT('Ctrl Pts',(-26.1447758475971,21.6385517038732,-35.3123987354935));
#25383=CARTESIAN_POINT('Ctrl Pts',(-26.1413265891683,21.6338792591201,-35.3120304997206));
#25384=CARTESIAN_POINT('Ctrl Pts',(-26.1354508134646,21.6259646618885,-35.3114046865719));
#25385=CARTESIAN_POINT('Ctrl Pts',(-26.1330307716773,21.6227177006777,-35.3111473547322));
#25386=CARTESIAN_POINT('Ctrl Pts',(-26.1268553438013,21.6144646623879,-35.3104917648633));
#25387=CARTESIAN_POINT('Ctrl Pts',(-26.1230914966107,21.609464963195,-35.3100931883706));
#25388=CARTESIAN_POINT('Ctrl Pts',(-26.1046789443896,21.5851543763156,-35.3081482062688));
#25389=CARTESIAN_POINT('Ctrl Pts',(-26.0898275629079,21.56599859903,-35.3065942185389));
#25390=CARTESIAN_POINT('Ctrl Pts',(-25.8882963309084,21.3120262959302,-35.28570179583));
#25391=CARTESIAN_POINT('Ctrl Pts',(-25.6699470611983,21.1042472797076,-35.2650663614345));
#25392=CARTESIAN_POINT('Ctrl Pts',(-25.3698430332791,20.8894266154983,-35.2403994929138));
#25393=CARTESIAN_POINT('Ctrl Pts',(-25.3122997712607,20.8509758007019,-35.2358226826034));
#25394=CARTESIAN_POINT('Ctrl Pts',(-25.2229634706317,20.7953560384084,-35.2289930548825));
#25395=CARTESIAN_POINT('Ctrl Pts',(-25.1920480787276,20.7768206858367,-35.2266779127681));
#25396=CARTESIAN_POINT('Ctrl Pts',(-25.1501596179288,20.7526523911278,-35.2236117789459));
#25397=CARTESIAN_POINT('Ctrl Pts',(-25.1394570294634,20.7465588418231,-35.2228344721761));
#25398=CARTESIAN_POINT('Ctrl Pts',(-25.1214967785109,20.7364690089506,-35.2215405593965));
#25399=CARTESIAN_POINT('Ctrl Pts',(-25.1142582661286,20.732439148541,-35.2210219063457));
#25400=CARTESIAN_POINT('Ctrl Pts',(-25.1044169892618,20.727009869037,-35.220320678601));
#25401=CARTESIAN_POINT('Ctrl Pts',(-25.1018278041891,20.7255860969865,-35.2201365560972));
#25402=CARTESIAN_POINT('Ctrl Pts',(-25.0977046983941,20.7233262139067,-35.2198439406262));
#25403=CARTESIAN_POINT('Ctrl Pts',(-25.0961720576621,20.7224877901201,-35.2197352985571));
#25404=CARTESIAN_POINT('Ctrl Pts',(-25.0929827772985,20.7207464773732,-35.2195094939903));
#25405=CARTESIAN_POINT('Ctrl Pts',(-25.0913260306343,20.7198437991928,-35.2193923456736));
#25406=CARTESIAN_POINT('Ctrl Pts',(-25.0875137868304,20.7177710381644,-35.219123128286));
#25407=CARTESIAN_POINT('Ctrl Pts',(-25.0853577407189,20.7166019577784,-35.2189711240067));
#25408=CARTESIAN_POINT('Ctrl Pts',(-25.0786768277215,20.712989205944,-35.2185008893086));
#25409=CARTESIAN_POINT('Ctrl Pts',(-25.0741474163586,20.7105538875253,-35.2181831929319));
#25410=CARTESIAN_POINT('Ctrl Pts',(-25.036998327253,20.6906944994713,-35.2155864094124));
#25411=CARTESIAN_POINT('Ctrl Pts',(-25.0040850920372,20.6738213446743,-35.2133417191707));
#25412=CARTESIAN_POINT('Ctrl Pts',(-24.9636240488202,20.6539507535484,-35.2106410446163));
#25413=CARTESIAN_POINT('Ctrl Pts',(-24.9563476162302,20.6504112168324,-35.210157649367));
#25414=CARTESIAN_POINT('Ctrl Pts',(-24.8096683027272,20.5797426575786,-35.2004577434593));
#25415=CARTESIAN_POINT('Ctrl Pts',(-24.6656073222198,20.522703824847,-35.1917311718961));
#25416=CARTESIAN_POINT('Ctrl Pts',(-24.5025675691141,20.4713769063217,-35.1821603804128));
#25417=CARTESIAN_POINT('Ctrl Pts',(-24.4871069909883,20.4666373203632,-35.1812558327212));
#25418=CARTESIAN_POINT('Ctrl Pts',(-24.454095136893,20.4567884159491,-35.1793297560321));
#25419=CARTESIAN_POINT('Ctrl Pts',(-24.4365347497474,20.4517116619209,-35.1783083894944));
#25420=CARTESIAN_POINT('Ctrl Pts',(-24.3987638234237,20.4411393496812,-35.1761168222705));
#25421=CARTESIAN_POINT('Ctrl Pts',(-24.3785410076821,20.4356908627473,-35.1749466799054));
#25422=CARTESIAN_POINT('Ctrl Pts',(-24.334635900298,20.4243196856882,-35.1724109795536));
#25423=CARTESIAN_POINT('Ctrl Pts',(-24.3109365743327,20.4184681832578,-35.1710452212981));
#25424=CARTESIAN_POINT('Ctrl Pts',(-24.1904826768414,20.3901753541152,-35.1641107875761));
#25425=CARTESIAN_POINT('Ctrl Pts',(-24.0927979376789,20.3719471053991,-35.1585083961151));
#25426=CARTESIAN_POINT('Ctrl Pts',(-23.9056804910848,20.3459089518649,-35.1476476806953));
#25427=CARTESIAN_POINT('Ctrl Pts',(-23.8164595480765,20.3372665966226,-35.1424143933045));
#25428=CARTESIAN_POINT('Ctrl Pts',(-23.6813569010971,20.329845919941,-35.1343384349252));
#25429=CARTESIAN_POINT('Ctrl Pts',(-23.6356679660651,20.3283104188919,-35.1315815822287));
#25430=CARTESIAN_POINT('Ctrl Pts',(-23.5822167247633,20.3276517380722,-35.1283214795438));
#25431=CARTESIAN_POINT('Ctrl Pts',(-23.5744696488246,20.3275842095927,-35.1278481159485));
#25432=CARTESIAN_POINT('Ctrl Pts',(-23.5626375397355,20.3275237405816,-35.1271238199217));
#25433=CARTESIAN_POINT('Ctrl Pts',(-23.5585526008213,20.3275106310607,-35.1268735209531));
#25434=CARTESIAN_POINT('Ctrl Pts',(-23.5511230347141,20.3275009137005,-35.1264178409445));
#25435=CARTESIAN_POINT('Ctrl Pts',(-23.5477784118435,20.327501745851,-35.1262125405728));
#25436=CARTESIAN_POINT('Ctrl Pts',(-23.5410707265129,20.3275138567011,-35.1258004776397));
#25437=CARTESIAN_POINT('Ctrl Pts',(-23.5377076684354,20.3275251930705,-35.125593713523));
#25438=CARTESIAN_POINT('Ctrl Pts',(-23.528184908038,20.3275721991508,-35.1250077699927));
#25439=CARTESIAN_POINT('Ctrl Pts',(-23.5220253060965,20.3276202646386,-35.1246282018288));
#25440=CARTESIAN_POINT('Ctrl Pts',(-23.4962473305034,20.3278953302995,-35.1230373233066));
#25441=CARTESIAN_POINT('Ctrl Pts',(-23.4766314273234,20.3282838166514,-35.1218209540399));
#25442=CARTESIAN_POINT('Ctrl Pts',(-23.0687695973218,20.3400879134943,-35.0964055382194));
#25443=CARTESIAN_POINT('Ctrl Pts',(-22.6858002567252,20.4214309025551,-35.069623226068));
#25444=CARTESIAN_POINT('Ctrl Pts',(-22.2619159494658,20.5953907963724,-35.0391127391074));
#25445=CARTESIAN_POINT('Ctrl Pts',(-22.1980262642422,20.6240767824526,-35.0345060840688));
#25446=CARTESIAN_POINT('Ctrl Pts',(-22.1105750395999,20.6668183800062,-35.0282362718396));
#25447=CARTESIAN_POINT('Ctrl Pts',(-22.0861849470184,20.6791255736755,-35.0264916429329));
#25448=CARTESIAN_POINT('Ctrl Pts',(-22.0530367481557,20.6963843638634,-35.0241290368914));
#25449=CARTESIAN_POINT('Ctrl Pts',(-22.0441417376591,20.701068630269,-35.0234959003547));
#25450=CARTESIAN_POINT('Ctrl Pts',(-22.0310213396206,20.7080566720482,-35.0225634237095));
#25451=CARTESIAN_POINT('Ctrl Pts',(-22.0267790629514,20.7103283583577,-35.0222621421862));
#25452=CARTESIAN_POINT('Ctrl Pts',(-22.0191110044989,20.7144566348325,-35.0217179868206));
#25453=CARTESIAN_POINT('Ctrl Pts',(-22.0156834817916,20.7163099464567,-35.021474909191));
#25454=CARTESIAN_POINT('Ctrl Pts',(-22.0103520847799,20.7192052190653,-35.0210970582408));
#25455=CARTESIAN_POINT('Ctrl Pts',(-22.0084459023188,20.7202428867582,-35.0209620112815));
#25456=CARTESIAN_POINT('Ctrl Pts',(-22.0050664683966,20.7220869755354,-35.0207226789908));
#25457=CARTESIAN_POINT('Ctrl Pts',(-22.0035928052966,20.7228926193332,-35.0206183443167));
#25458=CARTESIAN_POINT('Ctrl Pts',(-22.0004661013168,20.7246051478809,-35.0203970398053));
#25459=CARTESIAN_POINT('Ctrl Pts',(-21.9988132312426,20.7255123286859,-35.0202800897926));
#25460=CARTESIAN_POINT('Ctrl Pts',(-21.9940976224202,20.7281058868451,-35.0199465399138));
#25461=CARTESIAN_POINT('Ctrl Pts',(-21.9910368184786,20.7297958050934,-35.0197301678666));
#25462=CARTESIAN_POINT('Ctrl Pts',(-21.9779407853439,20.7370541654883,-35.018804916382));
#25463=CARTESIAN_POINT('Ctrl Pts',(-21.9679324286924,20.742671299328,-35.0180991313007));
#25464=CARTESIAN_POINT('Ctrl Pts',(-21.7009309084297,20.8944056514917,-34.9992998452728));
#25465=CARTESIAN_POINT('Ctrl Pts',(-21.4651766638632,21.0751685348301,-34.9833461707932));
#25466=CARTESIAN_POINT('Ctrl Pts',(-21.2313806859363,21.3118787927702,-34.9646243229777));
#25467=CARTESIAN_POINT('Ctrl Pts',(-21.205862805503,21.338619568004,-34.9625369789373));
#25468=CARTESIAN_POINT('Ctrl Pts',(-21.147885086423,21.4015068943849,-34.957680125195));
#25469=CARTESIAN_POINT('Ctrl Pts',(-21.1157718935573,21.4379597179199,-34.9549029970278));
#25470=CARTESIAN_POINT('Ctrl Pts',(-21.0315754825357,21.5380054843777,-34.9473567351631));
#25471=CARTESIAN_POINT('Ctrl Pts',(-20.9810836477019,21.6028845899669,-34.9425411697672));
#25472=CARTESIAN_POINT('Ctrl Pts',(-20.9081159774944,21.7044277003997,-34.9350672818862));
#25473=CARTESIAN_POINT('Ctrl Pts',(-20.8838006839266,21.739730741519,-34.9324800478644));
#25474=CARTESIAN_POINT('Ctrl Pts',(-20.8560047646456,21.7818621618579,-34.9294014082383));
#25475=CARTESIAN_POINT('Ctrl Pts',(-20.85183453684,21.7882321419558,-34.9289361804053));
#25476=CARTESIAN_POINT('Ctrl Pts',(-20.8454771057194,21.7980185539106,-34.9282217808261));
#25477=CARTESIAN_POINT('Ctrl Pts',(-20.843273695402,21.8014244676805,-34.9279732159145));
#25478=CARTESIAN_POINT('Ctrl Pts',(-20.8394415001117,21.8073726650068,-34.9275392215435));
#25479=CARTESIAN_POINT('Ctrl Pts',(-20.8378098428642,21.809913099753,-34.9273538995561));
#25480=CARTESIAN_POINT('Ctrl Pts',(-20.8341473935797,21.8156330706004,-34.9269367084173));
#25481=CARTESIAN_POINT('Ctrl Pts',(-20.8321186124971,21.8188138832824,-34.9267047647537));
#25482=CARTESIAN_POINT('Ctrl Pts',(-20.8267059096458,21.8273331169293,-34.9260836792575));
#25483=CARTESIAN_POINT('Ctrl Pts',(-20.8233321122456,21.8326779227388,-34.925694162187));
#25484=CARTESIAN_POINT('Ctrl Pts',(-20.8088439040152,21.8557805871537,-34.9240110655563));
#25485=CARTESIAN_POINT('Ctrl Pts',(-20.7978872662342,21.8736363422054,-34.9227116708748));
#25486=CARTESIAN_POINT('Ctrl Pts',(-20.6049696973395,22.1950169192351,-34.8993459391184));
#25487=CARTESIAN_POINT('Ctrl Pts',(-20.4740912964217,22.5263137615742,-34.8752016316414));
#25488=CARTESIAN_POINT('Ctrl Pts',(-20.3857128622535,22.936900134127,-34.8469817843743));
#25489=CARTESIAN_POINT('Ctrl Pts',(-20.3737649936119,23.0021282267358,-34.8425601506712));
#25490=CARTESIAN_POINT('Ctrl Pts',(-20.355974417955,23.1195993131637,-34.8347545633238));
#25491=CARTESIAN_POINT('Ctrl Pts',(-20.3493811837904,23.1717050819643,-34.8313472464132));
#25492=CARTESIAN_POINT('Ctrl Pts',(-20.3423694219911,23.2406017471819,-34.8269337702772));
#25493=CARTESIAN_POINT('Ctrl Pts',(-20.3408046029275,23.2572650336904,-34.8258733933838));
#25494=CARTESIAN_POINT('Ctrl Pts',(-20.3387687088946,23.2809231032737,-34.8243786282739));
#25495=CARTESIAN_POINT('Ctrl Pts',(-20.3381905664341,23.2879080661663,-34.8239386293022));
#25496=CARTESIAN_POINT('Ctrl Pts',(-20.3373422496122,23.298580618528,-34.8232684216144));
#25497=CARTESIAN_POINT('Ctrl Pts',(-20.3370556310825,23.3022668248324,-34.8230373167542));
#25498=CARTESIAN_POINT('Ctrl Pts',(-20.3365960711801,23.3083118159932,-34.8226589595125));
#25499=CARTESIAN_POINT('Ctrl Pts',(-20.336419382582,23.3106702997338,-34.8225114988373));
#25500=CARTESIAN_POINT('Ctrl Pts',(-20.3360833331101,23.3152232433623,-34.8222271392617));
#25501=CARTESIAN_POINT('Ctrl Pts',(-20.3359236230253,23.3174176750563,-34.8220902207626));
#25502=CARTESIAN_POINT('Ctrl Pts',(-20.3356354306693,23.3214342783161,-34.8218398639653));
#25503=CARTESIAN_POINT('Ctrl Pts',(-20.3355062508854,23.3232563877852,-34.8217263866737));
#25504=CARTESIAN_POINT('Ctrl Pts',(-20.3352453232688,23.3269817278382,-34.8214945755224));
#25505=CARTESIAN_POINT('Ctrl Pts',(-20.3351137167087,23.328884958408,-34.8213762501168));
#25506=CARTESIAN_POINT('Ctrl Pts',(-20.3347381610182,23.3343870510235,-34.8210344784404));
#25507=CARTESIAN_POINT('Ctrl Pts',(-20.3344985629005,23.3379862219352,-34.8208112783485));
#25508=CARTESIAN_POINT('Ctrl Pts',(-20.3334599073399,23.3539940610067,-34.8198201715079));
#25509=CARTESIAN_POINT('Ctrl Pts',(-20.3327266114931,23.3664071071806,-34.8190559287683));
#25510=CARTESIAN_POINT('Ctrl Pts',(-20.3319161041495,23.3816225989949,-34.8181240698352));
#25511=CARTESIAN_POINT('Ctrl Pts',(-20.3317706932313,23.3844210790239,-34.8179528834798));
#25512=CARTESIAN_POINT('Ctrl Pts',(-20.3142344698232,23.7306244914373,-34.7968000507418));
#25513=CARTESIAN_POINT('Ctrl Pts',(-20.3519034369753,24.0746657812167,-34.778616175727));
#25514=CARTESIAN_POINT('Ctrl Pts',(-20.4803306509189,24.5407864827825,-34.7510381268298));
#25515=CARTESIAN_POINT('Ctrl Pts',(-20.5260739330218,24.6727115785153,-34.7429048886946));
#25516=CARTESIAN_POINT('Ctrl Pts',(-20.5886929379442,24.8213777837415,-34.7331551081335));
#25517=CARTESIAN_POINT('Ctrl Pts',(-20.5973757248957,24.8414198954033,-34.7318282207098));
#25518=CARTESIAN_POINT('Ctrl Pts',(-20.6087619989247,24.8669866687115,-34.7301189833596));
#25519=CARTESIAN_POINT('Ctrl Pts',(-20.6112786387176,24.8725943171394,-34.7297430609305));
#25520=CARTESIAN_POINT('Ctrl Pts',(-20.615349798928,24.8815967594228,-34.7291378904619));
#25521=CARTESIAN_POINT('Ctrl Pts',(-20.6168942122411,24.8849961299234,-34.7289089910469));
#25522=CARTESIAN_POINT('Ctrl Pts',(-20.6198404107847,24.8914511247411,-34.728473605495));
#25523=CARTESIAN_POINT('Ctrl Pts',(-20.6212410775153,24.8945072566315,-34.7282671582107));
#25524=CARTESIAN_POINT('Ctrl Pts',(-20.6244360282961,24.9014496577748,-34.7277974715753));
#25525=CARTESIAN_POINT('Ctrl Pts',(-20.6262332755181,24.9053345492541,-34.7275341299656));
#25526=CARTESIAN_POINT('Ctrl Pts',(-20.6317043343149,24.9170991098769,-34.7267351015627));
#25527=CARTESIAN_POINT('Ctrl Pts',(-20.6354022742847,24.9249674560404,-34.7261985790288));
#25528=CARTESIAN_POINT('Ctrl Pts',(-20.6712529042939,25.0004541551198,-34.7210307564238));
#25529=CARTESIAN_POINT('Ctrl Pts',(-20.7057186181147,25.0669426451405,-34.716319048056));
#25530=CARTESIAN_POINT('Ctrl Pts',(-20.7623389405108,25.1674397520354,-34.7089372048993));
#25531=CARTESIAN_POINT('Ctrl Pts',(-20.7828741488684,25.2023340546415,-34.7063239463006));
#25532=CARTESIAN_POINT('Ctrl Pts',(-20.9502315849255,25.4748358270205,-34.6855175868048));
#25533=CARTESIAN_POINT('Ctrl Pts',(-21.1267174429531,25.6928135061553,-34.6662983157725));
#25534=CARTESIAN_POINT('Ctrl Pts',(-21.3607907075178,25.9154788250315,-34.6447288517958));
#25535=CARTESIAN_POINT('Ctrl Pts',(-21.3931604229004,25.9450369510754,-34.6418223086919));
#25536=CARTESIAN_POINT('Ctrl Pts',(-21.4765051668817,26.0180809874363,-34.6345479490649));
#25537=CARTESIAN_POINT('Ctrl Pts',(-21.5282551540125,26.0606575881064,-34.6302209951882));
#25538=CARTESIAN_POINT('Ctrl Pts',(-21.5869984647487,26.1059917322859,-34.6255486880487));
#25539=CARTESIAN_POINT('Ctrl Pts',(-21.5927127125243,26.1103711327569,-34.6250966272968));
#25540=CARTESIAN_POINT('Ctrl Pts',(-21.6014415316638,26.1170145894063,-34.6244098463555));
#25541=CARTESIAN_POINT('Ctrl Pts',(-21.6044454340026,26.1192925301499,-34.6241741762029));
#25542=CARTESIAN_POINT('Ctrl Pts',(-21.609364676905,26.1230093481,-34.6237893523476));
#25543=CARTESIAN_POINT('Ctrl Pts',(-21.6112776262543,26.1244513618925,-34.6236399802311));
#25544=CARTESIAN_POINT('Ctrl Pts',(-21.6149669941101,26.1272260243948,-34.6233524285916));
#25545=CARTESIAN_POINT('Ctrl Pts',(-21.6167431847448,26.1285589718589,-34.6232142280549));
#25546=CARTESIAN_POINT('Ctrl Pts',(-21.6199838046169,26.1309856726019,-34.6229625179809));
#25547=CARTESIAN_POINT('Ctrl Pts',(-21.6214477812819,26.1320800120164,-34.6228489670848));
#25548=CARTESIAN_POINT('Ctrl Pts',(-21.6244297155514,26.1343050903757,-34.6226180063433));
#25549=CARTESIAN_POINT('Ctrl Pts',(-21.625947732553,26.1354357331815,-34.6225006033263));
#25550=CARTESIAN_POINT('Ctrl Pts',(-21.6303018593628,26.1386727948636,-34.6221643475704));
#25551=CARTESIAN_POINT('Ctrl Pts',(-21.6331404491474,26.1407758970027,-34.6219457286227));
#25552=CARTESIAN_POINT('Ctrl Pts',(-21.6454631027971,26.1498743649823,-34.6209992339244));
#25553=CARTESIAN_POINT('Ctrl Pts',(-21.6549821956541,26.1568224632323,-34.6202746306601));
#25554=CARTESIAN_POINT('Ctrl Pts',(-21.7949119147841,26.2577869817221,-34.6097151306432));
#25555=CARTESIAN_POINT('Ctrl Pts',(-21.9321291746763,26.3419599464169,-34.6005212020825));
#25556=CARTESIAN_POINT('Ctrl Pts',(-22.0750360449252,26.4155367897853,-34.591474087242));
#25557=CARTESIAN_POINT('Origin',(-23.5502525316942,23.5502525316942,-77.3107734492734));
#25558=CARTESIAN_POINT('',(-22.0750360001986,26.4155367667575,-33.0962096862788));
#25559=CARTESIAN_POINT('',(-22.0750360407426,26.4155367876319,-33.3457833635692));
#25560=CARTESIAN_POINT('',(-22.0750360153461,26.4155367745563,-77.3107734492734));
#25561=CARTESIAN_POINT('',(-26.7730025308237,23.5501776283632,-33.9361574895006));
#25562=CARTESIAN_POINT('Ctrl Pts',(-22.0750360001986,26.4155367667575,-33.0962096862788));
#25563=CARTESIAN_POINT('Ctrl Pts',(-21.8563691433369,26.3029542319481,-33.1099615826865));
#25564=CARTESIAN_POINT('Ctrl Pts',(-21.6513097234616,26.1657136843064,-33.1238651265134));
#25565=CARTESIAN_POINT('Ctrl Pts',(-21.4610347210246,26.0040862784072,-33.1390039367681));
#25566=CARTESIAN_POINT('Ctrl Pts',(-21.458232861277,26.0016979859802,-33.139227381038));
#25567=CARTESIAN_POINT('Ctrl Pts',(-21.4454577522704,25.9907706896878,-33.1402485665619));
#25568=CARTESIAN_POINT('Ctrl Pts',(-21.4355327586255,25.98217568352,-33.141048590918));
#25569=CARTESIAN_POINT('Ctrl Pts',(-21.422126419754,25.9704217213913,-33.1421384460553));
#25570=CARTESIAN_POINT('Ctrl Pts',(-21.4185989616122,25.9673153591477,-33.1424260810886));
#25571=CARTESIAN_POINT('Ctrl Pts',(-21.4126317063929,25.9620372316407,-33.1429141511737));
#25572=CARTESIAN_POINT('Ctrl Pts',(-21.41018838457,25.9598694468353,-33.1431144191584));
#25573=CARTESIAN_POINT('Ctrl Pts',(-21.4052881021335,25.9555084443362,-33.143516930587));
#25574=CARTESIAN_POINT('Ctrl Pts',(-21.4028312000315,25.9533151679095,-33.1437191763518));
#25575=CARTESIAN_POINT('Ctrl Pts',(-21.3972792591422,25.9483436367564,-33.1441771851765));
#25576=CARTESIAN_POINT('Ctrl Pts',(-21.3941862323565,25.9455631531174,-33.1444330421825));
#25577=CARTESIAN_POINT('Ctrl Pts',(-21.3877398969916,25.9397456025662,-33.1449677489944));
#25578=CARTESIAN_POINT('Ctrl Pts',(-21.3843875860916,25.9367074481065,-33.1452466446443));
#25579=CARTESIAN_POINT('Ctrl Pts',(-21.3756512876778,25.9287562876458,-33.1459756400078));
#25580=CARTESIAN_POINT('Ctrl Pts',(-21.3702775726531,25.9238320783085,-33.1464262164091));
#25581=CARTESIAN_POINT('Ctrl Pts',(-21.2571524504909,25.8194615404176,-33.155957739489));
#25582=CARTESIAN_POINT('Ctrl Pts',(-21.1563115625081,25.7128096071311,-33.1653543985603));
#25583=CARTESIAN_POINT('Ctrl Pts',(-20.9567632727159,25.4706398307789,-33.1860228294603));
#25584=CARTESIAN_POINT('Ctrl Pts',(-20.860646518114,25.3335318316986,-33.1973454138663));
#25585=CARTESIAN_POINT('Ctrl Pts',(-20.6802635049344,25.028228141126,-33.2213400399107));
#25586=CARTESIAN_POINT('Ctrl Pts',(-20.5991667660968,24.8588241884184,-33.2339646060946));
#25587=CARTESIAN_POINT('Ctrl Pts',(-20.5291905543973,24.6724982782971,-33.2465080515665));
#25588=CARTESIAN_POINT('Ctrl Pts',(-20.5251875538291,24.6616628410653,-33.2472327864698));
#25589=CARTESIAN_POINT('Ctrl Pts',(-20.520045867269,24.6475115798543,-33.2481729616063));
#25590=CARTESIAN_POINT('Ctrl Pts',(-20.5188542771561,24.644215268975,-33.2483915134105));
#25591=CARTESIAN_POINT('Ctrl Pts',(-20.5170293989265,24.6391412085909,-33.248727238891));
#25592=CARTESIAN_POINT('Ctrl Pts',(-20.516392295446,24.6373648491599,-33.2488446410119));
#25593=CARTESIAN_POINT('Ctrl Pts',(-20.5151287059076,24.6338319715404,-33.2490778724776));
#25594=CARTESIAN_POINT('Ctrl Pts',(-20.5145021877954,24.6320754792531,-33.2491937029656));
#25595=CARTESIAN_POINT('Ctrl Pts',(-20.5131084018173,24.6281571466912,-33.2494518082576));
#25596=CARTESIAN_POINT('Ctrl Pts',(-20.5123419191119,24.6259950356032,-33.2495940353704));
#25597=CARTESIAN_POINT('Ctrl Pts',(-20.5101086582739,24.6196739825514,-33.2500092833688));
#25598=CARTESIAN_POINT('Ctrl Pts',(-20.5086480999534,24.6155128247743,-33.2502819325762));
#25599=CARTESIAN_POINT('Ctrl Pts',(-20.4981266829518,24.5853390589097,-33.2522539461489));
#25600=CARTESIAN_POINT('Ctrl Pts',(-20.4893907575546,24.5592132037144,-33.2539342641068));
#25601=CARTESIAN_POINT('Ctrl Pts',(-20.4626942376948,24.4758342157061,-33.2592205597368));
#25602=CARTESIAN_POINT('Ctrl Pts',(-20.4459960859557,24.4181871849207,-33.2627620246941));
#25603=CARTESIAN_POINT('Ctrl Pts',(-20.4039763335248,24.2563380369206,-33.272477228195));
#25604=CARTESIAN_POINT('Ctrl Pts',(-20.3822291417035,24.1512860302444,-33.2785255360439));
#25605=CARTESIAN_POINT('Ctrl Pts',(-20.3305533520322,23.8188976170506,-33.2973760650303));
#25606=CARTESIAN_POINT('Ctrl Pts',(-20.3196031291299,23.5893648384889,-33.3100296851615));
#25607=CARTESIAN_POINT('Ctrl Pts',(-20.3356199569554,23.3176406636581,-33.3259475145926));
#25608=CARTESIAN_POINT('Ctrl Pts',(-20.3390139194764,23.274721766108,-33.3284876399393));
#25609=CARTESIAN_POINT('Ctrl Pts',(-20.3435644573659,23.2288831854638,-33.331233243591));
#25610=CARTESIAN_POINT('Ctrl Pts',(-20.3438666796838,23.2258817089097,-33.331413173534));
#25611=CARTESIAN_POINT('Ctrl Pts',(-20.3487237541363,23.1783144981107,-33.3342670892068));
#25612=CARTESIAN_POINT('Ctrl Pts',(-20.3542029487011,23.1338498771441,-33.3369683206224));
#25613=CARTESIAN_POINT('Ctrl Pts',(-20.3617678339112,23.081478778588,-33.3401940811659));
#25614=CARTESIAN_POINT('Ctrl Pts',(-20.3629590867119,23.0734464985223,-33.3406900538544));
#25615=CARTESIAN_POINT('Ctrl Pts',(-20.3648204958809,23.0612142965102,-33.3414472648864));
#25616=CARTESIAN_POINT('Ctrl Pts',(-20.365468636815,23.0570110159026,-33.3417078038659));
#25617=CARTESIAN_POINT('Ctrl Pts',(-20.3666328507282,23.0495589020947,-33.3421703336049));
#25618=CARTESIAN_POINT('Ctrl Pts',(-20.367145582272,23.046309546657,-33.3423722179013));
#25619=CARTESIAN_POINT('Ctrl Pts',(-20.3682380853729,23.0394541708399,-33.3427985852264));
#25620=CARTESIAN_POINT('Ctrl Pts',(-20.3688190134011,23.0358483418249,-33.343023104774));
#25621=CARTESIAN_POINT('Ctrl Pts',(-20.3700195596786,23.0284763593021,-33.3434826542821));
#25622=CARTESIAN_POINT('Ctrl Pts',(-20.3706397411729,23.0247103045379,-33.3437177018581));
#25623=CARTESIAN_POINT('Ctrl Pts',(-20.3721875351231,23.0154143501939,-33.3442985825956));
#25624=CARTESIAN_POINT('Ctrl Pts',(-20.373122889533,23.0098857682043,-33.3446446620109));
#25625=CARTESIAN_POINT('Ctrl Pts',(-20.3825415490207,22.9550849831333,-33.3480812172106));
#25626=CARTESIAN_POINT('Ctrl Pts',(-20.3921555295228,22.9060164325008,-33.3512075851869));
#25627=CARTESIAN_POINT('Ctrl Pts',(-20.427173596164,22.7469910612913,-33.3615087445516));
#25628=CARTESIAN_POINT('Ctrl Pts',(-20.4572092184017,22.6381509536648,-33.3688281669958));
#25629=CARTESIAN_POINT('Ctrl Pts',(-20.5750435148632,22.2846519901156,-33.3934676448708));
#25630=CARTESIAN_POINT('Ctrl Pts',(-20.6866906506669,22.0490497753747,-33.4113898685815));
#25631=CARTESIAN_POINT('Ctrl Pts',(-20.873256927838,21.7536318750307,-33.4344967022571));
#25632=CARTESIAN_POINT('Ctrl Pts',(-20.9242628469046,21.6798694394627,-33.4403153220695));
#25633=CARTESIAN_POINT('Ctrl Pts',(-20.9821442319796,21.6032090350653,-33.4463371357854));
#25634=CARTESIAN_POINT('Ctrl Pts',(-20.9860203934933,21.5981070043533,-33.4467377807296));
#25635=CARTESIAN_POINT('Ctrl Pts',(-20.9914159621467,21.5910488395923,-33.4472918152884));
#25636=CARTESIAN_POINT('Ctrl Pts',(-20.9929224135749,21.5890828899089,-33.4474461099586));
#25637=CARTESIAN_POINT('Ctrl Pts',(-20.9955152272929,21.5857072827187,-33.447710995998));
#25638=CARTESIAN_POINT('Ctrl Pts',(-20.9966004906228,21.5842967888202,-33.4478216652609));
#25639=CARTESIAN_POINT('Ctrl Pts',(-20.9988443152639,21.5813855300486,-33.4480500582407));
#25640=CARTESIAN_POINT('Ctrl Pts',(-21.0000030303393,21.5798848914072,-33.4481677699938));
#25641=CARTESIAN_POINT('Ctrl Pts',(-21.002725924987,21.5763649272631,-33.4484438447483));
#25642=CARTESIAN_POINT('Ctrl Pts',(-21.0042911863621,21.574346431954,-33.4486021305158));
#25643=CARTESIAN_POINT('Ctrl Pts',(-21.0093797040153,21.5678005786252,-33.4491153610684));
#25644=CARTESIAN_POINT('Ctrl Pts',(-21.0129126750462,21.5632807337739,-33.4494696167201));
#25645=CARTESIAN_POINT('Ctrl Pts',(-21.1113438648524,21.4380451509746,-33.4592825933531));
#25646=CARTESIAN_POINT('Ctrl Pts',(-21.2147521873465,21.3242363460958,-33.4681333878435));
#25647=CARTESIAN_POINT('Ctrl Pts',(-21.4055294426812,21.142267750801,-33.483030971068));
#25648=CARTESIAN_POINT('Ctrl Pts',(-21.4890004342668,21.0704403289412,-33.4891509524939));
#25649=CARTESIAN_POINT('Ctrl Pts',(-21.5829023043167,20.9976602670516,-33.4957978756344));
#25650=CARTESIAN_POINT('Ctrl Pts',(-21.5898428124929,20.9923260434801,-33.4962878113997));
#25651=CARTESIAN_POINT('Ctrl Pts',(-21.6775652021031,20.9254725299975,-33.5024640968307));
#25652=CARTESIAN_POINT('Ctrl Pts',(-21.7611859506289,20.8677784600446,-33.5081824841757));
#25653=CARTESIAN_POINT('Ctrl Pts',(-21.9614576917328,20.7431364532308,-33.5217229239747));
#25654=CARTESIAN_POINT('Ctrl Pts',(-22.0798423872788,20.6793542897056,-33.5296175284711));
#25655=CARTESIAN_POINT('Ctrl Pts',(-22.211787265767,20.6185724728253,-33.5384551188689));
#25656=CARTESIAN_POINT('Ctrl Pts',(-22.2217463673485,20.6140460331101,-33.539122349422));
#25657=CARTESIAN_POINT('Ctrl Pts',(-22.235696797289,20.6077910282131,-33.540057298118));
#25658=CARTESIAN_POINT('Ctrl Pts',(-22.2396689504383,20.6060196681852,-33.5403235442553));
#25659=CARTESIAN_POINT('Ctrl Pts',(-22.2465439899483,20.6029704514811,-33.5407844308286));
#25660=CARTESIAN_POINT('Ctrl Pts',(-22.2494452070051,20.6016888260753,-33.5409789416953));
#25661=CARTESIAN_POINT('Ctrl Pts',(-22.2554004527121,20.5990685701119,-33.541378251856));
#25662=CARTESIAN_POINT('Ctrl Pts',(-22.2584546751475,20.5977303930413,-33.5415830663621));
#25663=CARTESIAN_POINT('Ctrl Pts',(-22.265574740991,20.5946239700525,-33.5420605910396));
#25664=CARTESIAN_POINT('Ctrl Pts',(-22.2696421601395,20.5928593728006,-33.5423334256436));
#25665=CARTESIAN_POINT('Ctrl Pts',(-22.2782159273906,20.5891607588091,-33.5429086337005));
#25666=CARTESIAN_POINT('Ctrl Pts',(-22.282723070723,20.5872286243859,-33.5432110707151));
#25667=CARTESIAN_POINT('Ctrl Pts',(-22.2947771836881,20.5820937712283,-33.544020080544));
#25668=CARTESIAN_POINT('Ctrl Pts',(-22.3023319571902,20.5789095668862,-33.5445272834179));
#25669=CARTESIAN_POINT('Ctrl Pts',(-22.4648403612685,20.5111442177498,-33.5554414300634));
#25670=CARTESIAN_POINT('Ctrl Pts',(-22.624566872141,20.4587498784554,-33.5662651477506));
#25671=CARTESIAN_POINT('Ctrl Pts',(-23.0510544832198,20.3548760843953,-33.5953898869025));
#25672=CARTESIAN_POINT('Ctrl Pts',(-23.3215040707769,20.3242192657087,-33.6141478595023));
#25673=CARTESIAN_POINT('Ctrl Pts',(-23.6027828106135,20.327914546034,-33.6325635426624));
#25674=CARTESIAN_POINT('Ctrl Pts',(-23.6129775065822,20.3280968703002,-33.6332293528822));
#25675=CARTESIAN_POINT('Ctrl Pts',(-23.6269571924176,20.328413259163,-33.6341399499521));
#25676=CARTESIAN_POINT('Ctrl Pts',(-23.6307429668876,20.3285056153361,-33.6343863022404));
#25677=CARTESIAN_POINT('Ctrl Pts',(-23.6887480650497,20.3300229881183,-33.6381570791507));
#25678=CARTESIAN_POINT('Ctrl Pts',(-23.7429272447251,20.3328099671841,-33.6416283943474));
#25679=CARTESIAN_POINT('Ctrl Pts',(-23.8022101889767,20.3373625460055,-33.6453525066291));
#25680=CARTESIAN_POINT('Ctrl Pts',(-23.8074053589227,20.3377741822644,-33.6456782367516));
#25681=CARTESIAN_POINT('Ctrl Pts',(-23.8151110842944,20.3384035533805,-33.6461604223376));
#25682=CARTESIAN_POINT('Ctrl Pts',(-23.8176223870372,20.3386116313225,-33.6463174168352));
#25683=CARTESIAN_POINT('Ctrl Pts',(-23.8219184263796,20.3389726602417,-33.646585724408));
#25684=CARTESIAN_POINT('Ctrl Pts',(-23.8237032789949,20.3391241536987,-33.6466971199233));
#25685=CARTESIAN_POINT('Ctrl Pts',(-23.8271823139483,20.3394223664628,-33.6469141011146));
#25686=CARTESIAN_POINT('Ctrl Pts',(-23.8288765018063,20.3395689381976,-33.6470196946127));
#25687=CARTESIAN_POINT('Ctrl Pts',(-23.8329687540999,20.3399262406164,-33.6472745843194));
#25688=CARTESIAN_POINT('Ctrl Pts',(-23.8353667051238,20.3401383178698,-33.647423803846));
#25689=CARTESIAN_POINT('Ctrl Pts',(-23.8427093881134,20.3407960047309,-33.647880304045));
#25690=CARTESIAN_POINT('Ctrl Pts',(-23.8476533596564,20.3412503566181,-33.6481870914634));
#25691=CARTESIAN_POINT('Ctrl Pts',(-23.8991286391414,20.3461009264995,-33.6513753883521));
#25692=CARTESIAN_POINT('Ctrl Pts',(-23.9455631103241,20.3514977492686,-33.6542013405379));
#25693=CARTESIAN_POINT('Ctrl Pts',(-24.0797102778871,20.3700550183086,-33.6622623549987));
#25694=CARTESIAN_POINT('Ctrl Pts',(-24.1670220117896,20.385828477111,-33.6673810797301));
#25695=CARTESIAN_POINT('Ctrl Pts',(-24.4595869022026,20.4512542135287,-33.6844254629808));
#25696=CARTESIAN_POINT('Ctrl Pts',(-24.6605722014291,20.517452757095,-33.6959852887159));
#25697=CARTESIAN_POINT('Ctrl Pts',(-25.0021907254882,20.6685214525579,-33.7172273695192));
#25698=CARTESIAN_POINT('Ctrl Pts',(-25.1455374519714,20.7453366397997,-33.7266900189917));
#25699=CARTESIAN_POINT('Ctrl Pts',(-25.2920499245774,20.8387237399306,-33.7372566753492));
#25700=CARTESIAN_POINT('Ctrl Pts',(-25.3015945470176,20.8448786783058,-33.7379492432885));
#25701=CARTESIAN_POINT('Ctrl Pts',(-25.3148079174917,20.8534986708749,-33.7389139443849));
#25702=CARTESIAN_POINT('Ctrl Pts',(-25.3185045074394,20.8559210663123,-33.7391844785292));
#25703=CARTESIAN_POINT('Ctrl Pts',(-25.3248607686757,20.8601050738654,-33.7396507825216));
#25704=CARTESIAN_POINT('Ctrl Pts',(-25.3275228359763,20.8618630500468,-33.7398464155035));
#25705=CARTESIAN_POINT('Ctrl Pts',(-25.3329533086972,20.8654608170367,-33.7402461934387));
#25706=CARTESIAN_POINT('Ctrl Pts',(-25.3357214856984,20.8673009433165,-33.7404503508605));
#25707=CARTESIAN_POINT('Ctrl Pts',(-25.3421223107855,20.871570140324,-33.7409232843133));
#25708=CARTESIAN_POINT('Ctrl Pts',(-25.3457528686692,20.8740023194234,-33.7411921776042));
#25709=CARTESIAN_POINT('Ctrl Pts',(-25.3533735968306,20.8791300757595,-33.7417579607111));
#25710=CARTESIAN_POINT('Ctrl Pts',(-25.3573626919273,20.8818272247923,-33.7420549097481));
#25711=CARTESIAN_POINT('Ctrl Pts',(-25.3679508446266,20.889020829745,-33.7428452003928));
#25712=CARTESIAN_POINT('Ctrl Pts',(-25.3745392294246,20.8935328680983,-33.7433391342962));
#25713=CARTESIAN_POINT('Ctrl Pts',(-25.5153070280779,20.9907078582783,-33.7539397125554));
#25714=CARTESIAN_POINT('Ctrl Pts',(-25.6422567166878,21.09338224976,-33.7644389256691));
#25715=CARTESIAN_POINT('Ctrl Pts',(-25.9895662079937,21.4207834984232,-33.7960580255962));
#25716=CARTESIAN_POINT('Ctrl Pts',(-26.185470304081,21.668630730991,-33.8179760209795));
#25717=CARTESIAN_POINT('Ctrl Pts',(-26.3451220011464,21.9456180217913,-33.8384547718852));
#25718=CARTESIAN_POINT('Ctrl Pts',(-26.3478314730971,21.9503464940923,-33.8388032263949));
#25719=CARTESIAN_POINT('Ctrl Pts',(-26.3528853098807,21.9592183597707,-33.8394548545913));
#25720=CARTESIAN_POINT('Ctrl Pts',(-26.3552325098241,21.9633601129969,-33.839758181165));
#25721=CARTESIAN_POINT('Ctrl Pts',(-26.3608358495007,21.9732987650764,-33.8404839161433));
#25722=CARTESIAN_POINT('Ctrl Pts',(-26.3640832599876,21.979100596782,-33.8409058391203));
#25723=CARTESIAN_POINT('Ctrl Pts',(-26.3753322015171,21.9993447255904,-33.8423718962414));
#25724=CARTESIAN_POINT('Ctrl Pts',(-26.3832408587141,22.0138387428455,-33.8434106793214));
#25725=CARTESIAN_POINT('Ctrl Pts',(-26.392742758226,22.0315755062785,-33.8446680972323));
#25726=CARTESIAN_POINT('Ctrl Pts',(-26.3944422040401,22.0347606302013,-33.8448933631846));
#25727=CARTESIAN_POINT('Ctrl Pts',(-26.3972309081421,22.0400084694065,-33.8452636200412));
#25728=CARTESIAN_POINT('Ctrl Pts',(-26.3983232791431,22.0420695118871,-33.8454088087808));
#25729=CARTESIAN_POINT('Ctrl Pts',(-26.4002861671601,22.0457827491069,-33.8456699753775));
#25730=CARTESIAN_POINT('Ctrl Pts',(-26.4011574838513,22.0474345108309,-33.845786004319));
#25731=CARTESIAN_POINT('Ctrl Pts',(-26.4030250904985,22.050982416565,-33.8460349153433));
#25732=CARTESIAN_POINT('Ctrl Pts',(-26.4040209232339,22.0528787914746,-33.8461677678749));
#25733=CARTESIAN_POINT('Ctrl Pts',(-26.406735822555,22.0580613490185,-33.8465303177134));
#25734=CARTESIAN_POINT('Ctrl Pts',(-26.4084511152392,22.0613495214307,-33.8467597743161));
#25735=CARTESIAN_POINT('Ctrl Pts',(-26.4172315678012,22.078252515367,-33.8479364185784));
#25736=CARTESIAN_POINT('Ctrl Pts',(-26.4242052938448,22.0919149903348,-33.8488778769539));
#25737=CARTESIAN_POINT('Ctrl Pts',(-26.4888348947098,22.2207974037022,-33.8576738508968));
#25738=CARTESIAN_POINT('Ctrl Pts',(-26.5396376523674,22.3393428356898,-33.8651296980488));
#25739=CARTESIAN_POINT('Ctrl Pts',(-26.6985628855833,22.7817085554313,-33.8917933600327));
#25740=CARTESIAN_POINT('Ctrl Pts',(-26.7621954688444,23.119040749908,-33.9102126580092));
#25741=CARTESIAN_POINT('Ctrl Pts',(-26.7723407741092,23.4815171997508,-33.9319943926306));
#25742=CARTESIAN_POINT('Ctrl Pts',(-26.7727267181171,23.5029527245104,-33.933288605986));
#25743=CARTESIAN_POINT('Ctrl Pts',(-26.7729677403501,23.5329858601504,-33.9351110803763));
#25744=CARTESIAN_POINT('Ctrl Pts',(-26.7730023310382,23.5415817653069,-33.9356337488379));
#25745=CARTESIAN_POINT('Ctrl Pts',(-26.7730025308237,23.5501776283632,-33.9361574895006));
#25746=CARTESIAN_POINT('Ctrl Pts',(-26.7730025308395,23.550178309149,-33.9361575309805));
#25747=CARTESIAN_POINT('Ctrl Pts',(-26.7730026748028,23.5564292106473,-33.9365383946152));
#25748=CARTESIAN_POINT('Ctrl Pts',(-26.7729846322319,23.5626800735835,-33.936919824221));
#25749=CARTESIAN_POINT('Ctrl Pts',(-26.7729246733282,23.5730252035013,-33.9375520422594));
#25750=CARTESIAN_POINT('Ctrl Pts',(-26.7728931401916,23.5771195237905,-33.9378025044864));
#25751=CARTESIAN_POINT('Ctrl Pts',(-26.7728227214832,23.5844490596819,-33.9382513222316));
#25752=CARTESIAN_POINT('Ctrl Pts',(-26.7727867662673,23.587684303309,-33.9384495856059));
#25753=CARTESIAN_POINT('Ctrl Pts',(-26.7727045033626,23.594202906064,-33.9388493776558));
#25754=CARTESIAN_POINT('Ctrl Pts',(-26.7726580493122,23.5974862591902,-33.9390509106868));
#25755=CARTESIAN_POINT('Ctrl Pts',(-26.7725550984058,23.6040532427504,-33.9394543198279));
#25756=CARTESIAN_POINT('Ctrl Pts',(-26.772498600233,23.6073368693641,-33.9396561957481));
#25757=CARTESIAN_POINT('Ctrl Pts',(-26.7723290392965,23.6163873244561,-33.9402130662241));
#25758=CARTESIAN_POINT('Ctrl Pts',(-26.7722055140904,23.6221539238401,-33.9405683889328));
#25759=CARTESIAN_POINT('Ctrl Pts',(-26.7716646389071,23.6445905543983,-33.9419528676441));
#25760=CARTESIAN_POINT('Ctrl Pts',(-26.7711333957747,23.6612573496447,-33.9429855938912));
#25761=CARTESIAN_POINT('Ctrl Pts',(-26.7673121293714,23.7576437976958,-33.9489834629668));
#25762=CARTESIAN_POINT('Ctrl Pts',(-26.7611921072332,23.8372173575544,-33.9540369670017));
#25763=CARTESIAN_POINT('Ctrl Pts',(-26.7160170114568,24.2321804174524,-33.9796545483204));
#25764=CARTESIAN_POINT('Ctrl Pts',(-26.633410184405,24.540788258247,-34.0016150782062));
#25765=CARTESIAN_POINT('Ctrl Pts',(-26.4697526943507,24.9182538998597,-34.0289546906226));
#25766=CARTESIAN_POINT('Ctrl Pts',(-26.4287144057312,25.0026195295785,-34.0350797575828));
#25767=CARTESIAN_POINT('Ctrl Pts',(-26.3777406275214,25.0967337583122,-34.0418341268903));
#25768=CARTESIAN_POINT('Ctrl Pts',(-26.3713585680126,25.1083455528806,-34.0426660560792));
#25769=CARTESIAN_POINT('Ctrl Pts',(-26.3631864848201,25.1229993601418,-34.0437138016294));
#25770=CARTESIAN_POINT('Ctrl Pts',(-26.3614629547836,25.1260780196333,-34.0439338057856));
#25771=CARTESIAN_POINT('Ctrl Pts',(-26.3587047030692,25.1309860261931,-34.0442843381788));
#25772=CARTESIAN_POINT('Ctrl Pts',(-26.3576732480507,25.1328171910255,-34.0444150766871));
#25773=CARTESIAN_POINT('Ctrl Pts',(-26.3557189380392,25.136278797346,-34.0446621371332));
#25774=CARTESIAN_POINT('Ctrl Pts',(-26.3547964593768,25.1379094310856,-34.0447784818508));
#25775=CARTESIAN_POINT('Ctrl Pts',(-26.3526914965804,25.1416227420244,-34.0450433429258));
#25776=CARTESIAN_POINT('Ctrl Pts',(-26.3515081143427,25.1437049028126,-34.045191799973));
#25777=CARTESIAN_POINT('Ctrl Pts',(-26.3484350510253,25.1490979538069,-34.0455761760316));
#25778=CARTESIAN_POINT('Ctrl Pts',(-26.3465418081482,25.1524068245231,-34.0458118647498));
#25779=CARTESIAN_POINT('Ctrl Pts',(-26.3350489188892,25.1724108235579,-34.0472359206745));
#25780=CARTESIAN_POINT('Ctrl Pts',(-26.3253053869441,25.1890234539341,-34.0484151055922));
#25781=CARTESIAN_POINT('Ctrl Pts',(-26.3131335552557,25.2093564197911,-34.0498553703653));
#25782=CARTESIAN_POINT('Ctrl Pts',(-26.3108459915708,25.2131599288851,-34.0501246581064));
#25783=CARTESIAN_POINT('Ctrl Pts',(-26.3067079486234,25.2200081399085,-34.0506092983583));
#25784=CARTESIAN_POINT('Ctrl Pts',(-26.3048602691497,25.2230545132971,-34.0508248109953));
#25785=CARTESIAN_POINT('Ctrl Pts',(-26.299939908391,25.2311367316886,-34.0513963951882));
#25786=CARTESIAN_POINT('Ctrl Pts',(-26.2968584294008,25.2361672410247,-34.0517519684595));
#25787=CARTESIAN_POINT('Ctrl Pts',(-26.1289376339257,25.5086153246693,-34.0710007669192));
#25788=CARTESIAN_POINT('Ctrl Pts',(-25.9258736091611,25.7505463979685,-34.0877711919136));
#25789=CARTESIAN_POINT('Ctrl Pts',(-25.5795725474262,26.058277027856,-34.1141110341939));
#25790=CARTESIAN_POINT('Ctrl Pts',(-25.4614555783776,26.1494102511916,-34.1227719060809));
#25791=CARTESIAN_POINT('Ctrl Pts',(-25.3250524106673,26.2403130448343,-34.1326742769969));
#25792=CARTESIAN_POINT('Ctrl Pts',(-25.3125795402053,26.2485007927453,-34.1335787766699));
#25793=CARTESIAN_POINT('Ctrl Pts',(-25.2937196724821,26.2606946956066,-34.1349451683691));
#25794=CARTESIAN_POINT('Ctrl Pts',(-25.2873746209282,26.264765607828,-34.1354046497046));
#25795=CARTESIAN_POINT('Ctrl Pts',(-25.2771105719835,26.2713001789964,-34.1361476057685));
#25796=CARTESIAN_POINT('Ctrl Pts',(-25.273200422461,26.2737777391324,-34.1364305641104));
#25797=CARTESIAN_POINT('Ctrl Pts',(-25.2657028320924,26.2785057757598,-34.136972990861));
#25798=CARTESIAN_POINT('Ctrl Pts',(-25.2621162641396,26.280757623826,-34.1372324077716));
#25799=CARTESIAN_POINT('Ctrl Pts',(-25.2557236603312,26.2847537125509,-34.1376946836892));
#25800=CARTESIAN_POINT('Ctrl Pts',(-25.2529193558775,26.2865007229983,-34.1378974398654));
#25801=CARTESIAN_POINT('Ctrl Pts',(-25.2473632567401,26.2899501829263,-34.1382990891161));
#25802=CARTESIAN_POINT('Ctrl Pts',(-25.2446115742029,26.2916528067677,-34.1384979754543));
#25803=CARTESIAN_POINT('Ctrl Pts',(-25.2379510153503,26.2957602175558,-34.1389793125636));
#25804=CARTESIAN_POINT('Ctrl Pts',(-25.2340395652403,26.2981607998471,-34.1392619178657));
#25805=CARTESIAN_POINT('Ctrl Pts',(-25.2195356375732,26.3070197300616,-34.1403096170406));
#25806=CARTESIAN_POINT('Ctrl Pts',(-25.2089111273498,26.3134251882087,-34.1410766496949));
#25807=CARTESIAN_POINT('Ctrl Pts',(-25.0239503714321,26.4234858634406,-34.1544232022468));
#25808=CARTESIAN_POINT('Ctrl Pts',(-24.8402839014482,26.5104967788181,-34.1676195293596));
#25809=CARTESIAN_POINT('Ctrl Pts',(-24.3728094877983,26.6801534362199,-34.2009236013512));
#25810=CARTESIAN_POINT('Ctrl Pts',(-24.0834569296122,26.7422086947903,-34.2213678720136));
#25811=CARTESIAN_POINT('Ctrl Pts',(-23.7767855565863,26.7650570357422,-34.2407691063148));
#25812=CARTESIAN_POINT('Ctrl Pts',(-23.7638675013172,26.7659412400283,-34.2415819518618));
#25813=CARTESIAN_POINT('Ctrl Pts',(-23.747451102101,26.766965533445,-34.2426090353967));
#25814=CARTESIAN_POINT('Ctrl Pts',(-23.7439576219611,26.7671777950607,-34.2428272645952));
#25815=CARTESIAN_POINT('Ctrl Pts',(-23.7383721105015,26.7675080355294,-34.2431756291451));
#25816=CARTESIAN_POINT('Ctrl Pts',(-23.7362803104675,26.7676296650862,-34.2433059702763));
#25817=CARTESIAN_POINT('Ctrl Pts',(-23.7323167027201,26.7678562541523,-34.2435527097234));
#25818=CARTESIAN_POINT('Ctrl Pts',(-23.730444935898,26.7679616196375,-34.2436691299855));
#25819=CARTESIAN_POINT('Ctrl Pts',(-23.7261708599775,26.7681984747732,-34.2439347432902));
#25820=CARTESIAN_POINT('Ctrl Pts',(-23.7237684984537,26.7683289074465,-34.2440838757663));
#25821=CARTESIAN_POINT('Ctrl Pts',(-23.7164153258074,26.7687198791526,-34.2445398499783));
#25822=CARTESIAN_POINT('Ctrl Pts',(-23.7114640279032,26.7689716861206,-34.244846200119));
#25823=CARTESIAN_POINT('Ctrl Pts',(-23.6923081619518,26.7699015791108,-34.2460288530424));
#25824=CARTESIAN_POINT('Ctrl Pts',(-23.6780994798894,26.7704970823297,-34.2469006047019));
#25825=CARTESIAN_POINT('Ctrl Pts',(-23.33974970073,26.782434752341,-34.2675392045379));
#25826=CARTESIAN_POINT('Ctrl Pts',(-23.0156821232511,26.7448780214831,-34.2848212851987));
#25827=CARTESIAN_POINT('Ctrl Pts',(-22.5521582334988,26.6185178297042,-34.3120772832817));
#25828=CARTESIAN_POINT('Ctrl Pts',(-22.4048753521352,26.5666320858267,-34.3211204643152));
#25829=CARTESIAN_POINT('Ctrl Pts',(-22.2479278794801,26.4981842970364,-34.3314608809321));
#25830=CARTESIAN_POINT('Ctrl Pts',(-22.233961182635,26.4919745214214,-34.3323872762318));
#25831=CARTESIAN_POINT('Ctrl Pts',(-22.2130498014579,26.4824983104864,-34.3337838692999));
#25832=CARTESIAN_POINT('Ctrl Pts',(-22.2060716142644,26.4793059809532,-34.3342515263368));
#25833=CARTESIAN_POINT('Ctrl Pts',(-22.1948511522685,26.4741243853716,-34.3350061115167));
#25834=CARTESIAN_POINT('Ctrl Pts',(-22.1906016691858,26.4721507242724,-34.3352925010232));
#25835=CARTESIAN_POINT('Ctrl Pts',(-22.1824824919245,26.4683582466141,-34.3358408559628));
#25836=CARTESIAN_POINT('Ctrl Pts',(-22.1786120809899,26.4665409808796,-34.3361027672922));
#25837=CARTESIAN_POINT('Ctrl Pts',(-22.171752231356,26.4633034132402,-34.336567885651));
#25838=CARTESIAN_POINT('Ctrl Pts',(-22.1687613366919,26.4618861958949,-34.3367709853125));
#25839=CARTESIAN_POINT('Ctrl Pts',(-22.162864093755,26.4590806907645,-34.3371720539694));
#25840=CARTESIAN_POINT('Ctrl Pts',(-22.1599576324459,26.4576926479692,-34.337370014267));
#25841=CARTESIAN_POINT('Ctrl Pts',(-22.1529644565345,26.4543400232102,-34.3378470315061));
#25842=CARTESIAN_POINT('Ctrl Pts',(-22.1488798057749,26.4523711726333,-34.3381262370635));
#25843=CARTESIAN_POINT('Ctrl Pts',(-22.1363532599769,26.4463006151483,-34.3389842902274));
#25844=CARTESIAN_POINT('Ctrl Pts',(-22.127925173531,26.4421706729057,-34.3395641235328));
#25845=CARTESIAN_POINT('Ctrl Pts',(-22.1046298374322,26.4306289926365,-34.3411738468377));
#25846=CARTESIAN_POINT('Ctrl Pts',(-22.0898029703684,26.4231396698567,-34.3422063933191));
#25847=CARTESIAN_POINT('Ctrl Pts',(-22.0750360068226,26.4155367701679,-34.3432429022327));
#25848=CARTESIAN_POINT('Ctrl Pts',(-22.0750360449252,26.4155367897853,-34.591474087242));
#25849=CARTESIAN_POINT('Ctrl Pts',(-22.0989250851324,26.4278362696248,-34.5899617254513));
#25850=CARTESIAN_POINT('Ctrl Pts',(-22.1229731237522,26.4398396576589,-34.5884536415116));
#25851=CARTESIAN_POINT('Ctrl Pts',(-22.3062474010362,26.5284719415273,-34.5770499000293));
#25852=CARTESIAN_POINT('Ctrl Pts',(-22.4713701982389,26.5921844381592,-34.5672641465516));
#25853=CARTESIAN_POINT('Ctrl Pts',(-22.7597642822913,26.6770083710693,-34.550017748628));
#25854=CARTESIAN_POINT('Ctrl Pts',(-22.8805536989833,26.7050856179438,-34.5427550083098));
#25855=CARTESIAN_POINT('Ctrl Pts',(-23.0226937761657,26.72959413185,-34.5340299418283));
#25856=CARTESIAN_POINT('Ctrl Pts',(-23.0427692406262,26.7328602566257,-34.5327937048404));
#25857=CARTESIAN_POINT('Ctrl Pts',(-23.0687953944981,26.7368420051045,-34.5311855281455));
#25858=CARTESIAN_POINT('Ctrl Pts',(-23.0747193465569,26.7377314157142,-34.5308191148241));
#25859=CARTESIAN_POINT('Ctrl Pts',(-23.0843050369607,26.7391432754798,-34.5302256063493));
#25860=CARTESIAN_POINT('Ctrl Pts',(-23.087965274411,26.739675949057,-34.5299988359311));
#25861=CARTESIAN_POINT('Ctrl Pts',(-23.0949620081948,26.7406818849192,-34.5295650764876));
#25862=CARTESIAN_POINT('Ctrl Pts',(-23.0982983476938,26.7411562178206,-34.5293581217229));
#25863=CARTESIAN_POINT('Ctrl Pts',(-23.1059391575518,26.7422303004553,-34.5288838814356));
#25864=CARTESIAN_POINT('Ctrl Pts',(-23.1102441025622,26.742826576678,-34.5286164861885));
#25865=CARTESIAN_POINT('Ctrl Pts',(-23.1234908646271,26.7446340783052,-34.5277930566887));
#25866=CARTESIAN_POINT('Ctrl Pts',(-23.1324365157674,26.745816450627,-34.5272361097632));
#25867=CARTESIAN_POINT('Ctrl Pts',(-23.199968826983,26.7544539715437,-34.5230248422883));
#25868=CARTESIAN_POINT('Ctrl Pts',(-23.258742200012,26.7603345431485,-34.519321007381));
#25869=CARTESIAN_POINT('Ctrl Pts',(-23.3243875765316,26.7650850840569,-34.5151371017011));
#25870=CARTESIAN_POINT('Ctrl Pts',(-23.3311356722392,26.7655520696067,-34.5147064640942));
#25871=CARTESIAN_POINT('Ctrl Pts',(-23.3551633488956,26.7671388541319,-34.5131711522595));
#25872=CARTESIAN_POINT('Ctrl Pts',(-23.3724501966957,26.7681406142995,-34.5120629585708));
#25873=CARTESIAN_POINT('Ctrl Pts',(-23.6489381739423,26.7819281614863,-34.4942805394447));
#25874=CARTESIAN_POINT('Ctrl Pts',(-23.9087114015202,26.7634955842362,-34.4766456071947));
#25875=CARTESIAN_POINT('Ctrl Pts',(-24.3227598611288,26.6832538237465,-34.4481740192113));
#25876=CARTESIAN_POINT('Ctrl Pts',(-24.4795746337458,26.6403721360618,-34.4373335505124));
#25877=CARTESIAN_POINT('Ctrl Pts',(-24.6392758716538,26.583435244152,-34.4266578296124));
#25878=CARTESIAN_POINT('Ctrl Pts',(-24.6460366139479,26.580999378516,-34.4262066079734));
#25879=CARTESIAN_POINT('Ctrl Pts',(-24.6563269305794,26.5772528886365,-34.4255209790797));
#25880=CARTESIAN_POINT('Ctrl Pts',(-24.6598623953732,26.5759586786235,-34.4252856256551));
#25881=CARTESIAN_POINT('Ctrl Pts',(-24.665641751141,26.5738315665879,-34.4249012503849));
#25882=CARTESIAN_POINT('Ctrl Pts',(-24.6678869840237,26.5730023596095,-34.4247520108348));
#25883=CARTESIAN_POINT('Ctrl Pts',(-24.6722120584686,26.5713995501179,-34.4244646960888));
#25884=CARTESIAN_POINT('Ctrl Pts',(-24.6742920277781,26.5706262996185,-34.4243265999491));
#25885=CARTESIAN_POINT('Ctrl Pts',(-24.6780981935649,26.5692068411864,-34.4240740376632));
#25886=CARTESIAN_POINT('Ctrl Pts',(-24.6798246278335,26.568561303088,-34.4239595318808));
#25887=CARTESIAN_POINT('Ctrl Pts',(-24.6833279853606,26.5672479215162,-34.4237272806032));
#25888=CARTESIAN_POINT('Ctrl Pts',(-24.6851048654437,26.5665799917916,-34.4236095409975));
#25889=CARTESIAN_POINT('Ctrl Pts',(-24.6902122849053,26.5646549594251,-34.4232712735655));
#25890=CARTESIAN_POINT('Ctrl Pts',(-24.6935413463131,26.5633939027402,-34.4230509840151));
#25891=CARTESIAN_POINT('Ctrl Pts',(-24.7081002806333,26.5578513403004,-34.422088425583));
#25892=CARTESIAN_POINT('Ctrl Pts',(-24.7193084323723,26.5535124796627,-34.4213495674383));
#25893=CARTESIAN_POINT('Ctrl Pts',(-24.9156620868752,26.4762349454548,-34.4084393356143));
#25894=CARTESIAN_POINT('Ctrl Pts',(-25.0937164261527,26.3863522313999,-34.3972459753073));
#25895=CARTESIAN_POINT('Ctrl Pts',(-25.3344371059875,26.2354043869343,-34.3813505390078));
#25896=CARTESIAN_POINT('Ctrl Pts',(-25.4046942725536,26.187372321764,-34.3766105042888));
#25897=CARTESIAN_POINT('Ctrl Pts',(-25.5501366417981,26.0792497867285,-34.3664324978558));
#25898=CARTESIAN_POINT('Ctrl Pts',(-25.6246955804839,26.0184599922566,-34.360988736405));
#25899=CARTESIAN_POINT('Ctrl Pts',(-25.7577443043866,25.8996896161691,-34.3506961002328));
#25900=CARTESIAN_POINT('Ctrl Pts',(-25.8169453570041,25.842626099165,-34.3458797196644));
#25901=CARTESIAN_POINT('Ctrl Pts',(-25.9035930747008,25.752465617683,-34.3384054537156));
#25902=CARTESIAN_POINT('Ctrl Pts',(-25.932668357607,25.7209779289634,-34.3358187005202));
#25903=CARTESIAN_POINT('Ctrl Pts',(-25.9661583935953,25.683225665798,-34.3327405758421));
#25904=CARTESIAN_POINT('Ctrl Pts',(-25.9711904492846,25.6775125350743,-34.3322753719789));
#25905=CARTESIAN_POINT('Ctrl Pts',(-25.9788725227825,25.6687281525263,-34.3315610015756));
#25906=CARTESIAN_POINT('Ctrl Pts',(-25.9815370883529,25.6656696114891,-34.3313124417928));
#25907=CARTESIAN_POINT('Ctrl Pts',(-25.9863871806123,25.660081129468,-34.3308585844646));
#25908=CARTESIAN_POINT('Ctrl Pts',(-25.9885745616518,25.6575527992717,-34.3306533643299));
#25909=CARTESIAN_POINT('Ctrl Pts',(-25.9929656964886,25.6524612234814,-34.3302403148355));
#25910=CARTESIAN_POINT('Ctrl Pts',(-25.9951693593398,25.6498979053328,-34.3300324820844));
#25911=CARTESIAN_POINT('Ctrl Pts',(-26.0014329777226,25.6425887832263,-34.3294401827105));
#25912=CARTESIAN_POINT('Ctrl Pts',(-26.005483159725,25.6378346572087,-34.3290553135174));
#25913=CARTESIAN_POINT('Ctrl Pts',(-26.0226514817313,25.6175633125344,-34.3274158523154));
#25914=CARTESIAN_POINT('Ctrl Pts',(-26.035636304759,25.6019342572194,-34.3261558100426));
#25915=CARTESIAN_POINT('Ctrl Pts',(-26.2795487272023,25.3026378881133,-34.3020968676183));
#25916=CARTESIAN_POINT('Ctrl Pts',(-26.4606222534033,24.9818635050336,-34.2770537867059));
#25917=CARTESIAN_POINT('Ctrl Pts',(-26.6271094795409,24.517415795489,-34.243989226576));
#25918=CARTESIAN_POINT('Ctrl Pts',(-26.6630483763629,24.3946244915293,-34.2355668452985));
#25919=CARTESIAN_POINT('Ctrl Pts',(-26.6933822471434,24.2622334149278,-34.2270389650358));
#25920=CARTESIAN_POINT('Ctrl Pts',(-26.695134826019,24.2544517537131,-34.2265397250902));
#25921=CARTESIAN_POINT('Ctrl Pts',(-26.6974891578114,24.2438141358053,-34.2258600779689));
#25922=CARTESIAN_POINT('Ctrl Pts',(-26.6981159301609,24.2409638347914,-34.2256782457209));
#25923=CARTESIAN_POINT('Ctrl Pts',(-26.6991586035824,24.2361912905079,-34.2253742523619));
#25924=CARTESIAN_POINT('Ctrl Pts',(-26.6995766167567,24.2342695181156,-34.2252519691377));
#25925=CARTESIAN_POINT('Ctrl Pts',(-26.7003967722442,24.2304822487735,-34.2250112344558));
#25926=CARTESIAN_POINT('Ctrl Pts',(-26.7007990167872,24.2286167771921,-34.2248927772435));
#25927=CARTESIAN_POINT('Ctrl Pts',(-26.7016826671531,24.2245009722181,-34.2246316865424));
#25928=CARTESIAN_POINT('Ctrl Pts',(-26.7021633209419,24.2222504743462,-34.2244890966266));
#25929=CARTESIAN_POINT('Ctrl Pts',(-26.7038361053311,24.2143769523061,-34.2239908346009));
#25930=CARTESIAN_POINT('Ctrl Pts',(-26.7050156117136,24.2087512121186,-34.2236358870092));
#25931=CARTESIAN_POINT('Ctrl Pts',(-26.7168820613318,24.1513896106907,-34.2200273371504));
#25932=CARTESIAN_POINT('Ctrl Pts',(-26.7263111805505,24.0993978854145,-34.2168443442268));
#25933=CARTESIAN_POINT('Ctrl Pts',(-26.7351634506009,24.0426760408111,-34.213443655824));
#25934=CARTESIAN_POINT('Ctrl Pts',(-26.7358589654859,24.0381563368825,-34.2131731762908));
#25935=CARTESIAN_POINT('Ctrl Pts',(-26.7375660709119,24.0269036836461,-34.2125009612454));
#25936=CARTESIAN_POINT('Ctrl Pts',(-26.7385659534925,24.0201689537097,-34.212099703183));
#25937=CARTESIAN_POINT('Ctrl Pts',(-26.7616769467061,23.8610344063721,-34.2026424515854));
#25938=CARTESIAN_POINT('Ctrl Pts',(-26.7728598453331,23.7072329408698,-34.1940161951904));
#25939=CARTESIAN_POINT('Ctrl Pts',(-26.773259724431,23.2714384287349,-34.1696554103458));
#25940=CARTESIAN_POINT('Ctrl Pts',(-26.7365681547528,22.9908963587475,-34.1539526948197));
#25941=CARTESIAN_POINT('Ctrl Pts',(-26.6594149078566,22.7020037985452,-34.1358363150405));
#25942=CARTESIAN_POINT('Ctrl Pts',(-26.6548187164703,22.685333240201,-34.1347843480911));
#25943=CARTESIAN_POINT('Ctrl Pts',(-26.6484871384135,22.6630692571995,-34.1333703569692));
#25944=CARTESIAN_POINT('Ctrl Pts',(-26.6468702889653,22.6574421904381,-34.1330122030452));
#25945=CARTESIAN_POINT('Ctrl Pts',(-26.6443176924442,22.6486488246929,-34.1324512916259));
#25946=CARTESIAN_POINT('Ctrl Pts',(-26.6433923923402,22.6454794851254,-34.1322488759086));
#25947=CARTESIAN_POINT('Ctrl Pts',(-26.6416119411351,22.6394157334218,-34.131861122603));
#25948=CARTESIAN_POINT('Ctrl Pts',(-26.6407575907768,22.6365210880454,-34.1316758113937));
#25949=CARTESIAN_POINT('Ctrl Pts',(-26.6387488631193,22.6297503153698,-34.1312418624257));
#25950=CARTESIAN_POINT('Ctrl Pts',(-26.6375912549009,22.6258751588442,-34.1309931190225));
#25951=CARTESIAN_POINT('Ctrl Pts',(-26.6342497521079,22.6147655926262,-34.1302789112706));
#25952=CARTESIAN_POINT('Ctrl Pts',(-26.6320477134568,22.6075367077089,-34.1298128522302));
#25953=CARTESIAN_POINT('Ctrl Pts',(-26.6175229815779,22.5604494765876,-34.1267682854441));
#25954=CARTESIAN_POINT('Ctrl Pts',(-26.6044532094046,22.5208274217603,-34.1241652894908));
#25955=CARTESIAN_POINT('Ctrl Pts',(-26.5634079707793,22.4040658371974,-34.116367397045));
#25956=CARTESIAN_POINT('Ctrl Pts',(-26.5332535193816,22.3277334834705,-34.1111017298354));
#25957=CARTESIAN_POINT('Ctrl Pts',(-26.3824442598128,21.9848864414576,-34.0866719699426));
#25958=CARTESIAN_POINT('Ctrl Pts',(-26.2287880226529,21.7344642084472,-34.0664604335202));
#25959=CARTESIAN_POINT('Ctrl Pts',(-26.0355998160522,21.4985894427246,-34.0462405615771));
#25960=CARTESIAN_POINT('Ctrl Pts',(-26.0276555567921,21.4890036839052,-34.045416869602));
#25961=CARTESIAN_POINT('Ctrl Pts',(-25.9975336278598,21.4530834563791,-34.0423235185648));
#25962=CARTESIAN_POINT('Ctrl Pts',(-25.9749892492306,21.4270580240375,-34.0400684419946));
#25963=CARTESIAN_POINT('Ctrl Pts',(-25.9502649669392,21.3994236470138,-34.0376632217024));
#25964=CARTESIAN_POINT('Ctrl Pts',(-25.9484961347917,21.3974515188744,-34.0374915133806));
#25965=CARTESIAN_POINT('Ctrl Pts',(-25.9433351138718,21.391711584531,-34.036991582895));
#25966=CARTESIAN_POINT('Ctrl Pts',(-25.9399364477877,21.3879495817102,-34.0366637119617));
#25967=CARTESIAN_POINT('Ctrl Pts',(-25.9348891704817,21.3823891560721,-34.0361788075853));
#25968=CARTESIAN_POINT('Ctrl Pts',(-25.9332473879307,21.3805845779198,-34.0360213907168));
#25969=CARTESIAN_POINT('Ctrl Pts',(-25.9287595720053,21.3756629986525,-34.035591949596));
#25970=CARTESIAN_POINT('Ctrl Pts',(-25.9259094512927,21.3725497101926,-34.0353201600074));
#25971=CARTESIAN_POINT('Ctrl Pts',(-25.897736460393,21.3418964777066,-34.032642890099));
#25972=CARTESIAN_POINT('Ctrl Pts',(-25.8719405791128,21.3147923621143,-34.0302656269705));
#25973=CARTESIAN_POINT('Ctrl Pts',(-25.8420088417417,21.2844198170474,-34.0275965287039));
#25974=CARTESIAN_POINT('Ctrl Pts',(-25.8383314087343,21.2807063372392,-34.0272701035406));
#25975=CARTESIAN_POINT('Ctrl Pts',(-25.8329293583653,21.2752778103493,-34.026792812293));
#25976=CARTESIAN_POINT('Ctrl Pts',(-25.8312118308432,21.2735557680694,-34.0266413894239));
#25977=CARTESIAN_POINT('Ctrl Pts',(-25.828160674771,21.2705035099383,-34.0263729720201));
#25978=CARTESIAN_POINT('Ctrl Pts',(-25.8268278288881,21.269172518461,-34.02625591518));
#25979=CARTESIAN_POINT('Ctrl Pts',(-25.824034723487,21.2663881856165,-34.0260110240449));
#25980=CARTESIAN_POINT('Ctrl Pts',(-25.8225742403267,21.264935079012,-34.0258832085064));
#25981=CARTESIAN_POINT('Ctrl Pts',(-25.8187403266074,21.2611278383023,-34.0255482931015));
#25982=CARTESIAN_POINT('Ctrl Pts',(-25.8163646169872,21.2587759870408,-34.0253413754972));
#25983=CARTESIAN_POINT('Ctrl Pts',(-25.8058782996316,21.2484272365452,-34.0244307290252));
#25984=CARTESIAN_POINT('Ctrl Pts',(-25.7977288594532,21.2404695419517,-34.0237300744063));
#25985=CARTESIAN_POINT('Ctrl Pts',(-25.7374045912891,21.1821861744517,-34.0185937615034));
#25986=CARTESIAN_POINT('Ctrl Pts',(-25.6835826396592,21.1335860457188,-34.0142851969908));
#25987=CARTESIAN_POINT('Ctrl Pts',(-25.5664369233721,21.0347726575465,-34.005353924082));
#25988=CARTESIAN_POINT('Ctrl Pts',(-25.5027726338303,20.9850419801022,-34.000754298886));
#25989=CARTESIAN_POINT('Ctrl Pts',(-25.2863692716015,20.8287302467345,-33.9856988285744));
#25990=CARTESIAN_POINT('Ctrl Pts',(-25.12627248535,20.7329938256092,-33.9754464430601));
#25991=CARTESIAN_POINT('Ctrl Pts',(-24.8140903485896,20.5812932963824,-33.9556989004152));
#25992=CARTESIAN_POINT('Ctrl Pts',(-24.6643334649044,20.5219167657888,-33.9463207751583));
#25993=CARTESIAN_POINT('Ctrl Pts',(-24.4999585228515,20.470592697566,-33.9358478357833));
#25994=CARTESIAN_POINT('Ctrl Pts',(-24.489116027262,20.4672699668533,-33.9351562911843));
#25995=CARTESIAN_POINT('Ctrl Pts',(-24.4736504825037,20.4626196327263,-33.9341687730128));
#25996=CARTESIAN_POINT('Ctrl Pts',(-24.4690415624383,20.4612450194121,-33.9338743405505));
#25997=CARTESIAN_POINT('Ctrl Pts',(-24.4611606937386,20.4589137434578,-33.933370640069));
#25998=CARTESIAN_POINT('Ctrl Pts',(-24.4578902630499,20.4579519428427,-33.9331615405289));
#25999=CARTESIAN_POINT('Ctrl Pts',(-24.4515883598676,20.4561094754065,-33.9327584782415));
#26000=CARTESIAN_POINT('Ctrl Pts',(-24.4485571059619,20.4552280698104,-33.9325645399227));
#26001=CARTESIAN_POINT('Ctrl Pts',(-24.4422618004233,20.453407594841,-33.9321616364375));
#26002=CARTESIAN_POINT('Ctrl Pts',(-24.4389975508576,20.4524692292047,-33.9319526485436));
#26003=CARTESIAN_POINT('Ctrl Pts',(-24.4275532764302,20.4491989500023,-33.9312196858708));
#26004=CARTESIAN_POINT('Ctrl Pts',(-24.4193655621167,20.4468942779046,-33.9306948231258));
#26005=CARTESIAN_POINT('Ctrl Pts',(-24.3462253711468,20.4266189789094,-33.9260019181378));
#26006=CARTESIAN_POINT('Ctrl Pts',(-24.2807374823834,20.4106586150428,-33.921768908817));
#26007=CARTESIAN_POINT('Ctrl Pts',(-24.1090165060227,20.3744710932078,-33.9105760508808));
#26008=CARTESIAN_POINT('Ctrl Pts',(-24.0021873925231,20.3575176940976,-33.9035192247818));
#26009=CARTESIAN_POINT('Ctrl Pts',(-23.5723489085688,20.3113095479474,-33.8748149336144));
#26010=CARTESIAN_POINT('Ctrl Pts',(-23.2466207461023,20.3254985094682,-33.8521583126289));
#26011=CARTESIAN_POINT('Ctrl Pts',(-22.9141283549771,20.3908731429603,-33.8307190678589));
#26012=CARTESIAN_POINT('Ctrl Pts',(-22.8997758614409,20.3937968911151,-33.8297974240534));
#26013=CARTESIAN_POINT('Ctrl Pts',(-22.8809036405921,20.3977755451565,-33.828591020595));
#26014=CARTESIAN_POINT('Ctrl Pts',(-22.8763658390729,20.3987424468587,-33.8283013601534));
#26015=CARTESIAN_POINT('Ctrl Pts',(-22.8695099129511,20.4002187727558,-33.8278643756535));
#26016=CARTESIAN_POINT('Ctrl Pts',(-22.8671902618453,20.4007209584248,-33.8277166375054));
#26017=CARTESIAN_POINT('Ctrl Pts',(-22.8630426885942,20.4016236720595,-33.8274526828081));
#26018=CARTESIAN_POINT('Ctrl Pts',(-22.8612145629831,20.4020232290674,-33.827336410379));
#26019=CARTESIAN_POINT('Ctrl Pts',(-22.8573209593397,20.4028777729977,-33.8270889210192));
#26020=CARTESIAN_POINT('Ctrl Pts',(-22.8552555864449,20.403333199744,-33.8269577302005));
#26021=CARTESIAN_POINT('Ctrl Pts',(-22.849688166731,20.4045665965518,-33.8266043328559));
#26022=CARTESIAN_POINT('Ctrl Pts',(-22.846186955032,20.4053483843368,-33.8263823469187));
#26023=CARTESIAN_POINT('Ctrl Pts',(-22.8291260887385,20.4091878350311,-33.8253018637408));
#26024=CARTESIAN_POINT('Ctrl Pts',(-22.8155847381095,20.4123274170791,-33.8244480345528));
#26025=CARTESIAN_POINT('Ctrl Pts',(-22.702288799366,20.4393688551679,-33.817332637962));
#26026=CARTESIAN_POINT('Ctrl Pts',(-22.6036961517975,20.4679359609417,-33.8113243182266));
#26027=CARTESIAN_POINT('Ctrl Pts',(-22.1430373343921,20.6256080320322,-33.7834093715236));
#26028=CARTESIAN_POINT('Ctrl Pts',(-21.8046557563379,20.8140647491773,-33.7629530372165));
#26029=CARTESIAN_POINT('Ctrl Pts',(-21.4920140997596,21.0702993370409,-33.7385002728303));
#26030=CARTESIAN_POINT('Ctrl Pts',(-21.4767457391084,21.0830511122999,-33.7372912672248));
#26031=CARTESIAN_POINT('Ctrl Pts',(-21.4569742189052,21.0998769871235,-33.7357058089206));
#26032=CARTESIAN_POINT('Ctrl Pts',(-21.4523629121682,21.1038237982725,-33.7353346041626));
#26033=CARTESIAN_POINT('Ctrl Pts',(-21.4449592670849,21.1101968937309,-33.7347363022266));
#26034=CARTESIAN_POINT('Ctrl Pts',(-21.4421598930686,21.1126150128746,-33.7345095436871));
#26035=CARTESIAN_POINT('Ctrl Pts',(-21.4368660551116,21.1172038068843,-33.7340797054491));
#26036=CARTESIAN_POINT('Ctrl Pts',(-21.4343707547595,21.1193735131893,-33.733876666203));
#26037=CARTESIAN_POINT('Ctrl Pts',(-21.4294505454255,21.1236650348486,-33.7334754611075));
#26038=CARTESIAN_POINT('Ctrl Pts',(-21.4270254701923,21.1257866544351,-33.733277303564));
#26039=CARTESIAN_POINT('Ctrl Pts',(-21.4195096468657,21.1323819291521,-33.7326618897988));
#26040=CARTESIAN_POINT('Ctrl Pts',(-21.4144298500582,21.1368679864196,-33.7322441145748));
#26041=CARTESIAN_POINT('Ctrl Pts',(-21.3876270925961,21.1606888694077,-33.7300300358509));
#26042=CARTESIAN_POINT('Ctrl Pts',(-21.3661530007074,21.1803005416068,-33.7282220846225));
#26043=CARTESIAN_POINT('Ctrl Pts',(-21.3070410851465,21.2357715425962,-33.7231476532436));
#26044=CARTESIAN_POINT('Ctrl Pts',(-21.2700024810063,21.2722536194351,-33.7198545779762));
#26045=CARTESIAN_POINT('Ctrl Pts',(-21.1817407988725,21.3634991863666,-33.7117201275055));
#26046=CARTESIAN_POINT('Ctrl Pts',(-21.1315171952111,21.4191833107751,-33.7068402480703));
#26047=CARTESIAN_POINT('Ctrl Pts',(-20.974648270876,21.6058028850584,-33.690764910758));
#26048=CARTESIAN_POINT('Ctrl Pts',(-20.8763439000876,21.7433695455611,-33.6793212401047));
#26049=CARTESIAN_POINT('Ctrl Pts',(-20.6945525037141,22.0453205366658,-33.6554792276729));
#26050=CARTESIAN_POINT('Ctrl Pts',(-20.6134386447165,22.2104820855729,-33.6431294467934));
#26051=CARTESIAN_POINT('Ctrl Pts',(-20.5429793028093,22.3915730568911,-33.6308941634161));
#26052=CARTESIAN_POINT('Ctrl Pts',(-20.539176480956,22.401491711204,-33.6302280575105));
#26053=CARTESIAN_POINT('Ctrl Pts',(-20.5342245208832,22.4146011337601,-33.6293531628402));
#26054=CARTESIAN_POINT('Ctrl Pts',(-20.5330313345554,22.417775023125,-33.6291417677605));
#26055=CARTESIAN_POINT('Ctrl Pts',(-20.5311899254078,22.4226967606199,-33.6288146207904));
#26056=CARTESIAN_POINT('Ctrl Pts',(-20.5305382108163,22.4244432859128,-33.628698658716));
#26057=CARTESIAN_POINT('Ctrl Pts',(-20.5292427416423,22.4279242225583,-33.6284677975111));
#26058=CARTESIAN_POINT('Ctrl Pts',(-20.5285989692078,22.4296586117499,-33.6283528981228));
#26059=CARTESIAN_POINT('Ctrl Pts',(-20.5271488963663,22.4335755925932,-33.6280936950383));
#26060=CARTESIAN_POINT('Ctrl Pts',(-20.5263434675872,22.4357584992534,-33.6279494444835));
#26061=CARTESIAN_POINT('Ctrl Pts',(-20.5239641549762,22.4422285787449,-33.6275224810836));
#26062=CARTESIAN_POINT('Ctrl Pts',(-20.5223970108164,22.4465182499633,-33.6272401726775));
#26063=CARTESIAN_POINT('Ctrl Pts',(-20.5100282925595,22.4805991636035,-33.6250032573602));
#26064=CARTESIAN_POINT('Ctrl Pts',(-20.4996570483137,22.5105462591293,-33.6230739679818));
#26065=CARTESIAN_POINT('Ctrl Pts',(-20.4600280880389,22.6306772103861,-33.6154606117935));
#26066=CARTESIAN_POINT('Ctrl Pts',(-20.4343120097873,22.7219869591672,-33.6099540842873));
#26067=CARTESIAN_POINT('Ctrl Pts',(-20.3454608025972,23.1007901843353,-33.5877542339657));
#26068=CARTESIAN_POINT('Ctrl Pts',(-20.3178151731128,23.3951199466005,-33.5718637579957));
#26069=CARTESIAN_POINT('Ctrl Pts',(-20.3344206511219,23.7801174801264,-33.5493579025877));
#26070=CARTESIAN_POINT('Ctrl Pts',(-20.3422003858697,23.8708950177142,-33.5439386155613));
#26071=CARTESIAN_POINT('Ctrl Pts',(-20.3550843030089,23.9711052124267,-33.5377879411271));
#26072=CARTESIAN_POINT('Ctrl Pts',(-20.3564017116921,23.9809890225315,-33.5371794886299));
#26073=CARTESIAN_POINT('Ctrl Pts',(-20.3583871955912,23.9953749329228,-33.5362912002658));
#26074=CARTESIAN_POINT('Ctrl Pts',(-20.359018981669,23.9998820511298,-33.5360125145795));
#26075=CARTESIAN_POINT('Ctrl Pts',(-20.3601332891304,24.0077107774697,-33.535527772931));
#26076=CARTESIAN_POINT('Ctrl Pts',(-20.3606114574496,24.0110330062804,-33.5353218552954));
#26077=CARTESIAN_POINT('Ctrl Pts',(-20.3615468750801,24.017460892261,-33.5349230331689));
#26078=CARTESIAN_POINT('Ctrl Pts',(-20.3620034738697,24.0205666414935,-33.5347301495402));
#26079=CARTESIAN_POINT('Ctrl Pts',(-20.3629742052434,24.0271031019756,-33.5343238077794));
#26080=CARTESIAN_POINT('Ctrl Pts',(-20.3634893406181,24.0305336582159,-33.5341103180113));
#26081=CARTESIAN_POINT('Ctrl Pts',(-20.3653902792497,24.0430552952626,-33.5333302371743));
#26082=CARTESIAN_POINT('Ctrl Pts',(-20.3668094438403,24.052141199039,-33.5327625870518));
#26083=CARTESIAN_POINT('Ctrl Pts',(-20.3844673139956,24.1621031661328,-33.5258728293296));
#26084=CARTESIAN_POINT('Ctrl Pts',(-20.4054538206304,24.262147530655,-33.5193997821666));
#26085=CARTESIAN_POINT('Ctrl Pts',(-20.4406702743354,24.3976288743335,-33.510336315347));
#26086=CARTESIAN_POINT('Ctrl Pts',(-20.4508302979962,24.4340681947827,-33.5078688015035));
#26087=CARTESIAN_POINT('Ctrl Pts',(-20.5416273151462,24.7388698104988,-33.4869829225475));
#26088=CARTESIAN_POINT('Ctrl Pts',(-20.6562932973689,24.9958000372653,-33.4676183517231));
#26089=CARTESIAN_POINT('Ctrl Pts',(-20.8498139941704,25.3114644951791,-33.4431268721492));
#26090=CARTESIAN_POINT('Ctrl Pts',(-20.9001124645207,25.3862800472435,-33.4372766156257));
#26091=CARTESIAN_POINT('Ctrl Pts',(-20.957285261597,25.4640653366161,-33.4312247337822));
#26092=CARTESIAN_POINT('Ctrl Pts',(-20.9611000124356,25.4692230759633,-33.4308236024124));
#26093=CARTESIAN_POINT('Ctrl Pts',(-20.9664097146433,25.4763574095024,-33.4302689986703));
#26094=CARTESIAN_POINT('Ctrl Pts',(-20.9678915503622,25.4783436772932,-33.4301146188623));
#26095=CARTESIAN_POINT('Ctrl Pts',(-20.9704417728123,25.4817538078126,-33.4298496211275));
#26096=CARTESIAN_POINT('Ctrl Pts',(-20.9715090479577,25.4831784941697,-33.4297389251703));
#26097=CARTESIAN_POINT('Ctrl Pts',(-20.973715424886,25.4861186670378,-33.4295105104022));
#26098=CARTESIAN_POINT('Ctrl Pts',(-20.9748546813497,25.4876340297954,-33.4293928035086));
#26099=CARTESIAN_POINT('Ctrl Pts',(-20.9775313935578,25.4911878801958,-33.4291167956924));
#26100=CARTESIAN_POINT('Ctrl Pts',(-20.9790699398956,25.4932255529728,-33.4289585718772));
#26101=CARTESIAN_POINT('Ctrl Pts',(-20.9840695703234,25.4998307970993,-33.4284457720489));
#26102=CARTESIAN_POINT('Ctrl Pts',(-20.9875404415114,25.5043909986914,-33.4280918835224));
#26103=CARTESIAN_POINT('Ctrl Pts',(-21.0825663294083,25.6285520875382,-33.4184597173937));
#26104=CARTESIAN_POINT('Ctrl Pts',(-21.1823965282736,25.7416164691065,-33.4097663298791));
#26105=CARTESIAN_POINT('Ctrl Pts',(-21.5214864338104,26.0753070640255,-33.3828610859152));
#26106=CARTESIAN_POINT('Ctrl Pts',(-21.7862386107151,26.2668469218924,-33.365236529596));
#26107=CARTESIAN_POINT('Ctrl Pts',(-22.0750360407425,26.4155367876319,-33.3457833635692));
#26108=CARTESIAN_POINT('Origin',(-23.5502525316942,23.5502525316942,-77.3107734492734));
#26109=CARTESIAN_POINT('',(-22.0750360153402,26.4155367745532,-31.8492183260801));
#26110=CARTESIAN_POINT('',(-22.0750360188393,26.4155367763548,-32.0936416103654));
#26111=CARTESIAN_POINT('',(-22.0750360153461,26.4155367745563,-77.3107734492734));
#26112=CARTESIAN_POINT('Ctrl Pts',(-22.0750360153402,26.4155367745532,-31.8492183260801));
#26113=CARTESIAN_POINT('Ctrl Pts',(-22.0738944921894,26.4149490514294,-31.8493005742725));
#26114=CARTESIAN_POINT('Ctrl Pts',(-22.0727533154471,26.414360643657,-31.8493827878888));
#26115=CARTESIAN_POINT('Ctrl Pts',(-22.0672699001479,26.411529163442,-31.8497777814017));
#26116=CARTESIAN_POINT('Ctrl Pts',(-22.0629323917442,26.4092768846506,-31.8500900877478));
#26117=CARTESIAN_POINT('Ctrl Pts',(-22.042973497031,26.398855388619,-31.8515264395472));
#26118=CARTESIAN_POINT('Ctrl Pts',(-22.0274138030302,26.3905677542308,-31.8526441799446));
#26119=CARTESIAN_POINT('Ctrl Pts',(-22.005523084465,26.3786763921286,-31.8542130139914));
#26120=CARTESIAN_POINT('Ctrl Pts',(-21.9991353961047,26.3751784127566,-31.8546703492278));
#26121=CARTESIAN_POINT('Ctrl Pts',(-21.9879855904546,26.369023416774,-31.8554677748243));
#26122=CARTESIAN_POINT('Ctrl Pts',(-21.9832182875004,26.3663759268647,-31.8558084524994));
#26123=CARTESIAN_POINT('Ctrl Pts',(-21.9762821996464,26.3625009499911,-31.8563036855365));
#26124=CARTESIAN_POINT('Ctrl Pts',(-21.9741081150861,26.3612830456652,-31.8564588524827));
#26125=CARTESIAN_POINT('Ctrl Pts',(-21.9703858958006,26.3591922131341,-31.8567244031774));
#26126=CARTESIAN_POINT('Ctrl Pts',(-21.9688370690047,26.3583205251025,-31.8568348673953));
#26127=CARTESIAN_POINT('Ctrl Pts',(-21.9657550741822,26.3565826032586,-31.857054613735));
#26128=CARTESIAN_POINT('Ctrl Pts',(-21.9642218972916,26.3557163953365,-31.8571638972305));
#26129=CARTESIAN_POINT('Ctrl Pts',(-21.9605961698484,26.353664024762,-31.8574222618296));
#26130=CARTESIAN_POINT('Ctrl Pts',(-21.9585042322179,26.3524767731539,-31.8575712721461));
#26131=CARTESIAN_POINT('Ctrl Pts',(-21.9522826605605,26.3489365873753,-31.8580142714327));
#26132=CARTESIAN_POINT('Ctrl Pts',(-21.9481568771009,26.3465768452873,-31.8583078221464));
#26133=CARTESIAN_POINT('Ctrl Pts',(-21.9104392548507,26.3248933723161,-31.8609895620944));
#26134=CARTESIAN_POINT('Ctrl Pts',(-21.8771914845096,26.3049732866924,-31.8633398248362));
#26135=CARTESIAN_POINT('Ctrl Pts',(-21.6094054099348,26.1378944182269,-31.8822251423793));
#26136=CARTESIAN_POINT('Ctrl Pts',(-21.3943349555691,25.961651090485,-31.8971909469708));
#26137=CARTESIAN_POINT('Ctrl Pts',(-21.1781705267215,25.7321807832313,-31.914974747874));
#26138=CARTESIAN_POINT('Ctrl Pts',(-21.1524126513311,25.7038420339421,-31.9171442098866));
#26139=CARTESIAN_POINT('Ctrl Pts',(-21.0635867614361,25.6025464314741,-31.9248238993856));
#26140=CARTESIAN_POINT('Ctrl Pts',(-21.0032981092715,25.5272294637784,-31.9304028332972));
#26141=CARTESIAN_POINT('Ctrl Pts',(-20.909347088567,25.3984156320949,-31.939839795394));
#26142=CARTESIAN_POINT('Ctrl Pts',(-20.8737177100792,25.3464287252652,-31.9436217478048));
#26143=CARTESIAN_POINT('Ctrl Pts',(-20.835103380396,25.2863841205163,-31.9479734280845));
#26144=CARTESIAN_POINT('Ctrl Pts',(-20.830597536065,25.2793171661598,-31.9484853402299));
#26145=CARTESIAN_POINT('Ctrl Pts',(-20.8238661677569,25.2686682960818,-31.949256359588));
#26146=CARTESIAN_POINT('Ctrl Pts',(-20.8216199990823,25.2650994188721,-31.9495146999878));
#26147=CARTESIAN_POINT('Ctrl Pts',(-20.8177672124186,25.2589510941145,-31.9499596598908));
#26148=CARTESIAN_POINT('Ctrl Pts',(-20.8161572224185,25.2563737574476,-31.9501461542553));
#26149=CARTESIAN_POINT('Ctrl Pts',(-20.8128474380097,25.2510586054515,-31.9505306954989));
#26150=CARTESIAN_POINT('Ctrl Pts',(-20.8111481002759,25.2483205106389,-31.950728758998));
#26151=CARTESIAN_POINT('Ctrl Pts',(-20.8070643168476,25.2417183448566,-31.9512062591381));
#26152=CARTESIAN_POINT('Ctrl Pts',(-20.8046839295779,25.2378517820837,-31.9514858450529));
#26153=CARTESIAN_POINT('Ctrl Pts',(-20.7973950915188,25.2259559775145,-31.9523458317469));
#26154=CARTESIAN_POINT('Ctrl Pts',(-20.792513665359,25.2179103102419,-31.9529272242997));
#26155=CARTESIAN_POINT('Ctrl Pts',(-20.735423768802,25.1228774396715,-31.9597917212386));
#26156=CARTESIAN_POINT('Ctrl Pts',(-20.6873209365657,25.033502008427,-31.9662235328316));
#26157=CARTESIAN_POINT('Ctrl Pts',(-20.5185056972325,24.6809264254587,-31.9915452865556));
#26158=CARTESIAN_POINT('Ctrl Pts',(-20.4292535129324,24.4042015975014,-32.0114653686875));
#26159=CARTESIAN_POINT('Ctrl Pts',(-20.362656743404,24.0330031812092,-32.0366528381726));
#26160=CARTESIAN_POINT('Ctrl Pts',(-20.350694977246,23.9460418892281,-32.0424342360964));
#26161=CARTESIAN_POINT('Ctrl Pts',(-20.3402134011377,23.8370278803283,-32.0494509881381));
#26162=CARTESIAN_POINT('Ctrl Pts',(-20.3383497153814,23.8153405885105,-32.0508355272982));
#26163=CARTESIAN_POINT('Ctrl Pts',(-20.3360633767315,23.785152533171,-32.0527454214404));
#26164=CARTESIAN_POINT('Ctrl Pts',(-20.3354544953238,23.77666702709,-32.0532803668208));
#26165=CARTESIAN_POINT('Ctrl Pts',(-20.3345913191728,23.7639313904858,-32.0540802945212));
#26166=CARTESIAN_POINT('Ctrl Pts',(-20.334311840174,23.7596830870683,-32.0543466380783));
#26167=CARTESIAN_POINT('Ctrl Pts',(-20.3338752870159,23.7528401399555,-32.0547748427269));
#26168=CARTESIAN_POINT('Ctrl Pts',(-20.333712933087,23.7502458561104,-32.0549369958535));
#26169=CARTESIAN_POINT('Ctrl Pts',(-20.3334086408069,23.7452872827178,-32.0552465656321));
#26170=CARTESIAN_POINT('Ctrl Pts',(-20.3332661699112,23.7429230292651,-32.0553940120786));
#26171=CARTESIAN_POINT('Ctrl Pts',(-20.3330175817601,23.7387206440339,-32.055655812217));
#26172=CARTESIAN_POINT('Ctrl Pts',(-20.3329104333136,23.7368825788505,-32.0557702242812));
#26173=CARTESIAN_POINT('Ctrl Pts',(-20.3327006061954,23.733229237687,-32.0559974389361));
#26174=CARTESIAN_POINT('Ctrl Pts',(-20.3325978888635,23.7314139727516,-32.0561102434532));
#26175=CARTESIAN_POINT('Ctrl Pts',(-20.3323207209375,23.7264411365231,-32.056419012715));
#26176=CARTESIAN_POINT('Ctrl Pts',(-20.3321493811051,23.7232833830596,-32.0566148012797));
#26177=CARTESIAN_POINT('Ctrl Pts',(-20.3315113630982,23.7111960230365,-32.0573631931802));
#26178=CARTESIAN_POINT('Ctrl Pts',(-20.3310771957264,23.7022646318452,-32.0579139801095));
#26179=CARTESIAN_POINT('Ctrl Pts',(-20.3243945682708,23.5518916312754,-32.0671519488671));
#26180=CARTESIAN_POINT('Ctrl Pts',(-20.3274353481881,23.4101702750807,-32.075334800481));
#26181=CARTESIAN_POINT('Ctrl Pts',(-20.3494043449505,23.1593159930794,-32.0895950084584));
#26182=CARTESIAN_POINT('Ctrl Pts',(-20.3646422121306,23.0501040211017,-32.0957271416361));
#26183=CARTESIAN_POINT('Ctrl Pts',(-20.4130198373575,22.7984372168493,-32.1100571274531));
#26184=CARTESIAN_POINT('Ctrl Pts',(-20.4503141307594,22.6570376743474,-32.1182659413323));
#26185=CARTESIAN_POINT('Ctrl Pts',(-20.5282390690473,22.4264039314636,-32.1323903339225));
#26186=CARTESIAN_POINT('Ctrl Pts',(-20.5635739952306,22.3356128585726,-32.1381485448151));
#26187=CARTESIAN_POINT('Ctrl Pts',(-20.6100416882379,22.2305616441219,-32.1451086628262));
#26188=CARTESIAN_POINT('Ctrl Pts',(-20.6172513823092,22.2146148257375,-32.1461734460391));
#26189=CARTESIAN_POINT('Ctrl Pts',(-20.6269659676147,22.1935855452764,-32.1475887946829));
#26190=CARTESIAN_POINT('Ctrl Pts',(-20.6293549820729,22.1884496268168,-32.1479353509995));
#26191=CARTESIAN_POINT('Ctrl Pts',(-20.6332954911716,22.1800363683645,-32.1485045238402));
#26192=CARTESIAN_POINT('Ctrl Pts',(-20.6348390057779,22.1767552862517,-32.1487268633484));
#26193=CARTESIAN_POINT('Ctrl Pts',(-20.6378376489551,22.1704088350346,-32.1491576408878));
#26194=CARTESIAN_POINT('Ctrl Pts',(-20.639292088475,22.1673431441044,-32.1493660547535));
#26195=CARTESIAN_POINT('Ctrl Pts',(-20.6426568797261,22.1602796113165,-32.1498470035502));
#26196=CARTESIAN_POINT('Ctrl Pts',(-20.6445706366749,22.156283407441,-32.1501196567699));
#26197=CARTESIAN_POINT('Ctrl Pts',(-20.6505519696393,22.1438593480508,-32.1509690655069));
#26198=CARTESIAN_POINT('Ctrl Pts',(-20.6546479901376,22.1354453107157,-32.1515468126199));
#26199=CARTESIAN_POINT('Ctrl Pts',(-20.6897042913362,22.06422265597,-32.1564587019866));
#26200=CARTESIAN_POINT('Ctrl Pts',(-20.7226653006145,22.0024249459316,-32.1608628475315));
#26201=CARTESIAN_POINT('Ctrl Pts',(-20.7618678909811,21.9343622476178,-32.1658815178235));
#26202=CARTESIAN_POINT('Ctrl Pts',(-20.7661543193358,21.926988087279,-32.1664275136878));
#26203=CARTESIAN_POINT('Ctrl Pts',(-20.7971646554925,21.8741235841165,-32.1703579458718));
#26204=CARTESIAN_POINT('Ctrl Pts',(-20.8249715891385,21.829280597049,-32.1737789202992));
#26205=CARTESIAN_POINT('Ctrl Pts',(-20.9631020303543,21.6182721797139,-32.1902929045161));
#26206=CARTESIAN_POINT('Ctrl Pts',(-21.0875844071843,21.4619167346764,-32.2038320553028));
#26207=CARTESIAN_POINT('Ctrl Pts',(-21.3459930509058,21.1928129195055,-32.2290492470429));
#26208=CARTESIAN_POINT('Ctrl Pts',(-21.4762336897309,21.0774518288264,-32.2406900247347));
#26209=CARTESIAN_POINT('Ctrl Pts',(-21.6207619097685,20.9689287081519,-32.2520673428584));
#26210=CARTESIAN_POINT('Ctrl Pts',(-21.6263835880648,20.9647361360828,-32.2525075988885));
#26211=CARTESIAN_POINT('Ctrl Pts',(-21.6349911982024,20.9583603140136,-32.2531781564823));
#26212=CARTESIAN_POINT('Ctrl Pts',(-21.6379672339975,20.9561638315572,-32.253409355333));
#26213=CARTESIAN_POINT('Ctrl Pts',(-21.6428528656709,20.9525709359393,-32.2537878428392));
#26214=CARTESIAN_POINT('Ctrl Pts',(-21.6447602191429,20.9511715006826,-32.2539353400084));
#26215=CARTESIAN_POINT('Ctrl Pts',(-21.6483608226076,20.9485358129148,-32.2542132761647));
#26216=CARTESIAN_POINT('Ctrl Pts',(-21.6500537397969,20.947299111212,-32.2543437464643));
#26217=CARTESIAN_POINT('Ctrl Pts',(-21.6532258410472,20.9449865869545,-32.2545878228032));
#26218=CARTESIAN_POINT('Ctrl Pts',(-21.654704730162,20.9439103745695,-32.2547014559994));
#26219=CARTESIAN_POINT('Ctrl Pts',(-21.6577038084725,20.9417317978579,-32.2549315725779));
#26220=CARTESIAN_POINT('Ctrl Pts',(-21.659224039156,20.9406295073716,-32.2550480507664));
#26221=CARTESIAN_POINT('Ctrl Pts',(-21.663547097536,20.9375007008111,-32.2553788044352));
#26222=CARTESIAN_POINT('Ctrl Pts',(-21.6663522362212,20.9354773593231,-32.2555928581835));
#26223=CARTESIAN_POINT('Ctrl Pts',(-21.6782275153922,20.9269407716948,-32.2564966720176));
#26224=CARTESIAN_POINT('Ctrl Pts',(-21.6873283589735,20.9204700716531,-32.257183512027));
#26225=CARTESIAN_POINT('Ctrl Pts',(-21.8417568821177,20.8118753613712,-32.2687436664392));
#26226=CARTESIAN_POINT('Ctrl Pts',(-21.9952732946475,20.7218738024144,-32.2788334421321));
#26227=CARTESIAN_POINT('Ctrl Pts',(-22.3343548446947,20.5590828974625,-32.2999369969224));
#26228=CARTESIAN_POINT('Ctrl Pts',(-22.5208049917386,20.4899032728678,-32.3108918663511));
#26229=CARTESIAN_POINT('Ctrl Pts',(-22.8226886985239,20.4086277445212,-32.328898755521));
#26230=CARTESIAN_POINT('Ctrl Pts',(-22.9344347631091,20.3848268816883,-32.3356126739721));
#26231=CARTESIAN_POINT('Ctrl Pts',(-23.0662960922209,20.3639886529421,-32.3436927811906));
#26232=CARTESIAN_POINT('Ctrl Pts',(-23.08541887836,20.361142782923,-32.3448682847374));
#26233=CARTESIAN_POINT('Ctrl Pts',(-23.1103889015759,20.3576560775315,-32.3464084159436));
#26234=CARTESIAN_POINT('Ctrl Pts',(-23.1162141924825,20.3568589055336,-32.3467680825904));
#26235=CARTESIAN_POINT('Ctrl Pts',(-23.1256829326285,20.3555895266754,-32.3473533118936));
#26236=CARTESIAN_POINT('Ctrl Pts',(-23.129325083379,20.3551075986491,-32.3475785663422));
#26237=CARTESIAN_POINT('Ctrl Pts',(-23.1363161862689,20.3541946996649,-32.3480112251396));
#26238=CARTESIAN_POINT('Ctrl Pts',(-23.1396650090683,20.3537627616706,-32.3482185985687));
#26239=CARTESIAN_POINT('Ctrl Pts',(-23.1473033010481,20.3527897606273,-32.3486918811889));
#26240=CARTESIAN_POINT('Ctrl Pts',(-23.1515931859479,20.352252065685,-32.3489578965885));
#26241=CARTESIAN_POINT('Ctrl Pts',(-23.1649636418193,20.3506035314565,-32.3497876474889));
#26242=CARTESIAN_POINT('Ctrl Pts',(-23.1740478098553,20.3495227308705,-32.3503523316397));
#26243=CARTESIAN_POINT('Ctrl Pts',(-23.2446340338875,20.3414292927383,-32.3547474831137));
#26244=CARTESIAN_POINT('Ctrl Pts',(-23.3063183171339,20.3361516489869,-32.3586324261187));
#26245=CARTESIAN_POINT('Ctrl Pts',(-23.3731385183356,20.3323691395817,-32.3628926225131));
#26246=CARTESIAN_POINT('Ctrl Pts',(-23.3781646436171,20.3320964358403,-32.3632133823488));
#26247=CARTESIAN_POINT('Ctrl Pts',(-23.4057085146813,20.330666692207,-32.3649729135784));
#26248=CARTESIAN_POINT('Ctrl Pts',(-23.4282368536426,20.3297342372304,-32.3664183604982));
#26249=CARTESIAN_POINT('Ctrl Pts',(-23.7063524398426,20.3211452726332,-32.3843406913961));
#26250=CARTESIAN_POINT('Ctrl Pts',(-23.9619326367737,20.3436996992466,-32.4017322505713));
#26251=CARTESIAN_POINT('Ctrl Pts',(-24.2472883519581,20.4035795680835,-32.421408368598));
#26252=CARTESIAN_POINT('Ctrl Pts',(-24.282342709261,20.4115499767024,-32.4238280008759));
#26253=CARTESIAN_POINT('Ctrl Pts',(-24.4418859928224,20.4506441107599,-32.4348345355536));
#26254=CARTESIAN_POINT('Ctrl Pts',(-24.5645973727856,20.4886033338312,-32.4432871457373));
#26255=CARTESIAN_POINT('Ctrl Pts',(-24.6892746159681,20.5354938664154,-32.4516433691759));
#26256=CARTESIAN_POINT('Ctrl Pts',(-24.6938135609635,20.5372126561868,-32.4519472507496));
#26257=CARTESIAN_POINT('Ctrl Pts',(-24.7010072225706,20.539955320554,-32.4524283191608));
#26258=CARTESIAN_POINT('Ctrl Pts',(-24.7036644732938,20.5409724598006,-32.4526059015662));
#26259=CARTESIAN_POINT('Ctrl Pts',(-24.7086943357708,20.5429054255215,-32.4529418150293));
#26260=CARTESIAN_POINT('Ctrl Pts',(-24.7110672149856,20.5438205431735,-32.4531001882837));
#26261=CARTESIAN_POINT('Ctrl Pts',(-24.7151824372747,20.5454132061463,-32.4533746798818));
#26262=CARTESIAN_POINT('Ctrl Pts',(-24.7169252763667,20.5460894595254,-32.4534908766082));
#26263=CARTESIAN_POINT('Ctrl Pts',(-24.7203095556865,20.547406010912,-32.4537164048956));
#26264=CARTESIAN_POINT('Ctrl Pts',(-24.721951056291,20.5480461373464,-32.4538257466579));
#26265=CARTESIAN_POINT('Ctrl Pts',(-24.7258357204919,20.549564688532,-32.4540843961509));
#26266=CARTESIAN_POINT('Ctrl Pts',(-24.7280784295514,20.5504442844373,-32.4542336327187));
#26267=CARTESIAN_POINT('Ctrl Pts',(-24.7347563757129,20.5530720344145,-32.4546777471464));
#26268=CARTESIAN_POINT('Ctrl Pts',(-24.7391887474357,20.5548275258967,-32.4549721836515));
#26269=CARTESIAN_POINT('Ctrl Pts',(-24.7800003394468,20.5710962801882,-32.4576802801949));
#26270=CARTESIAN_POINT('Ctrl Pts',(-24.8161180324508,20.5862625664614,-32.4600551922295));
#26271=CARTESIAN_POINT('Ctrl Pts',(-24.9395728826377,20.6407713765239,-32.468127346537));
#26272=CARTESIAN_POINT('Ctrl Pts',(-25.0254332322613,20.6833488495696,-32.4736622282515));
#26273=CARTESIAN_POINT('Ctrl Pts',(-25.1628325562598,20.7592942998411,-32.4825877250237));
#26274=CARTESIAN_POINT('Ctrl Pts',(-25.2155364877084,20.790417048588,-32.486028669322));
#26275=CARTESIAN_POINT('Ctrl Pts',(-25.350890996741,20.8756365801258,-32.4949885575412));
#26276=CARTESIAN_POINT('Ctrl Pts',(-25.431995712337,20.9320638626509,-32.5004831381294));
#26277=CARTESIAN_POINT('Ctrl Pts',(-25.6068369566286,21.0660335188971,-32.5128574011248));
#26278=CARTESIAN_POINT('Ctrl Pts',(-25.6990292764379,21.1453328370731,-32.5197562740335));
#26279=CARTESIAN_POINT('Ctrl Pts',(-25.832996411724,21.2744309134998,-32.5306092668335));
#26280=CARTESIAN_POINT('Ctrl Pts',(-25.8781150764888,21.3206026033689,-32.5344242374469));
#26281=CARTESIAN_POINT('Ctrl Pts',(-25.9449690559482,21.3932593340023,-32.5403519247257));
#26282=CARTESIAN_POINT('Ctrl Pts',(-25.9677204057971,21.4187892254526,-32.5424211957393));
#26283=CARTESIAN_POINT('Ctrl Pts',(-25.9947195720186,21.4500741340144,-32.5449427360589));
#26284=CARTESIAN_POINT('Ctrl Pts',(-25.9993606192261,21.4554881087556,-32.5453785932236));
#26285=CARTESIAN_POINT('Ctrl Pts',(-26.0065458234289,21.4639264673529,-32.5460571678793));
#26286=CARTESIAN_POINT('Ctrl Pts',(-26.0091024701993,21.4669402263825,-32.5462993702967));
#26287=CARTESIAN_POINT('Ctrl Pts',(-26.0135969057829,21.4722580367943,-32.5467264779922));
#26288=CARTESIAN_POINT('Ctrl Pts',(-26.0155370255143,21.4745601193603,-32.5469112872427));
#26289=CARTESIAN_POINT('Ctrl Pts',(-26.0196331029982,21.4794342344749,-32.5473023975595));
#26290=CARTESIAN_POINT('Ctrl Pts',(-26.0217882732762,21.4820069215261,-32.5475087305625));
#26291=CARTESIAN_POINT('Ctrl Pts',(-26.0278658715866,21.4892849854746,-32.548092147139));
#26292=CARTESIAN_POINT('Ctrl Pts',(-26.0317788922787,21.4939981676919,-32.5484696140535));
#26293=CARTESIAN_POINT('Ctrl Pts',(-26.0479959472624,21.5136451077219,-32.5500416793535));
#26294=CARTESIAN_POINT('Ctrl Pts',(-26.0601785977775,21.5286781239875,-32.5512411894322));
#26295=CARTESIAN_POINT('Ctrl Pts',(-26.3158295101706,21.8500168329163,-32.5768142654837));
#26296=CARTESIAN_POINT('Ctrl Pts',(-26.5015927998284,22.1979864031684,-32.6038166739562));
#26297=CARTESIAN_POINT('Ctrl Pts',(-26.6499297077645,22.66283580488,-32.6362805901247));
#26298=CARTESIAN_POINT('Ctrl Pts',(-26.6752124291342,22.7564410164609,-32.6426185368125));
#26299=CARTESIAN_POINT('Ctrl Pts',(-26.6981695169157,22.8597343840643,-32.6492974718204));
#26300=CARTESIAN_POINT('Ctrl Pts',(-26.7000631243058,22.8684241859521,-32.6498569400747));
#26301=CARTESIAN_POINT('Ctrl Pts',(-26.7032662444742,22.8834215291061,-32.6508182123991));
#26302=CARTESIAN_POINT('Ctrl Pts',(-26.7045928509369,22.8897253096225,-32.6512209568453));
#26303=CARTESIAN_POINT('Ctrl Pts',(-26.7064442304517,22.8986554968719,-32.6517896146392));
#26304=CARTESIAN_POINT('Ctrl Pts',(-26.706984633214,22.9012785919598,-32.6519564183613));
#26305=CARTESIAN_POINT('Ctrl Pts',(-26.7079064211033,22.9057813100117,-32.6522423496674));
#26306=CARTESIAN_POINT('Ctrl Pts',(-26.7082893986772,22.9076606022992,-32.6523615693166));
#26307=CARTESIAN_POINT('Ctrl Pts',(-26.7090185778951,22.9112551219252,-32.6525893715429));
#26308=CARTESIAN_POINT('Ctrl Pts',(-26.7093650597716,22.9129702870776,-32.6526979703629));
#26309=CARTESIAN_POINT('Ctrl Pts',(-26.7101758934343,22.9170010114908,-32.6529529509841));
#26310=CARTESIAN_POINT('Ctrl Pts',(-26.7106390979575,22.9193168045582,-32.6530992664441));
#26311=CARTESIAN_POINT('Ctrl Pts',(-26.7119936293792,22.9261277091575,-32.6535290668989));
#26312=CARTESIAN_POINT('Ctrl Pts',(-26.712877919357,22.9306242392305,-32.6538121494546));
#26313=CARTESIAN_POINT('Ctrl Pts',(-26.7202770964689,22.9686768506077,-32.6562022343197));
#26314=CARTESIAN_POINT('Ctrl Pts',(-26.7262676317525,23.002334356276,-32.6582797953842));
#26315=CARTESIAN_POINT('Ctrl Pts',(-26.732688692665,23.0420651920247,-32.6606962001471));
#26316=CARTESIAN_POINT('Ctrl Pts',(-26.7336387208964,23.0480507172951,-32.6610592764642));
#26317=CARTESIAN_POINT('Ctrl Pts',(-26.736122052057,23.063986837241,-32.6620234787032));
#26318=CARTESIAN_POINT('Ctrl Pts',(-26.7376256315328,23.0739420723073,-32.6626232543491));
#26319=CARTESIAN_POINT('Ctrl Pts',(-26.7397098639901,23.0881937896272,-32.6634784331918));
#26320=CARTESIAN_POINT('Ctrl Pts',(-26.7403285234067,23.0924845521119,-32.6637354552184));
#26321=CARTESIAN_POINT('Ctrl Pts',(-26.7621486069362,23.2460120617907,-32.6729163913047));
#26322=CARTESIAN_POINT('Ctrl Pts',(-26.7728646033546,23.3965673596197,-32.6813997023904));
#26323=CARTESIAN_POINT('Ctrl Pts',(-26.7730983081691,23.6544965668712,-32.6958333340991));
#26324=CARTESIAN_POINT('Ctrl Pts',(-26.7678501364995,23.7615982352801,-32.7017964825508));
#26325=CARTESIAN_POINT('Ctrl Pts',(-26.7506351306255,23.9352193070715,-32.7116318662049));
#26326=CARTESIAN_POINT('Ctrl Pts',(-26.7418971322367,24.0019740988081,-32.7154538829357));
#26327=CARTESIAN_POINT('Ctrl Pts',(-26.7272066053712,24.0921561186822,-32.7207080397753));
#26328=CARTESIAN_POINT('Ctrl Pts',(-26.7230716017257,24.1158635265889,-32.7220978152095));
#26329=CARTESIAN_POINT('Ctrl Pts',(-26.6992670649057,24.2438571607339,-32.7296528838007));
#26330=CARTESIAN_POINT('Ctrl Pts',(-26.6747228249882,24.3471600573904,-32.7359402965192));
#26331=CARTESIAN_POINT('Ctrl Pts',(-26.6422408818053,24.4590060418438,-32.743028451979));
#26332=CARTESIAN_POINT('Ctrl Pts',(-26.6393035127819,24.4689412339944,-32.7436605290631));
#26333=CARTESIAN_POINT('Ctrl Pts',(-26.6350940429976,24.4829306462483,-32.7445540395965));
#26334=CARTESIAN_POINT('Ctrl Pts',(-26.6338617307538,24.4869968524253,-32.7448141686529));
#26335=CARTESIAN_POINT('Ctrl Pts',(-26.6317029885174,24.4940695382372,-32.7452673657088));
#26336=CARTESIAN_POINT('Ctrl Pts',(-26.6307801884695,24.4970771276101,-32.7454603143725));
#26337=CARTESIAN_POINT('Ctrl Pts',(-26.6288447772025,24.5033522381762,-32.7458633720861));
#26338=CARTESIAN_POINT('Ctrl Pts',(-26.6278313649448,24.5066195060229,-32.7460735072353));
#26339=CARTESIAN_POINT('Ctrl Pts',(-26.6254216518884,24.5143449910082,-32.7465710268662));
#26340=CARTESIAN_POINT('Ctrl Pts',(-26.6240208580881,24.5188017886722,-32.7468585589017));
#26341=CARTESIAN_POINT('Ctrl Pts',(-26.6193600234842,24.5335188575532,-32.7478097499679));
#26342=CARTESIAN_POINT('Ctrl Pts',(-26.6160582874658,24.5437657561116,-32.7484747818853));
#26343=CARTESIAN_POINT('Ctrl Pts',(-26.5624116192098,24.7074434511631,-32.7591423102099));
#26344=CARTESIAN_POINT('Ctrl Pts',(-26.5006647601484,24.8568688694441,-32.7695288225766));
#26345=CARTESIAN_POINT('Ctrl Pts',(-26.2897734951666,25.2751922328451,-32.8005351340332));
#26346=CARTESIAN_POINT('Ctrl Pts',(-26.1131001464262,25.5281771266788,-32.8219155330127));
#26347=CARTESIAN_POINT('Ctrl Pts',(-25.9002539487991,25.7556166851122,-32.8419988580087));
#26348=CARTESIAN_POINT('Ctrl Pts',(-25.8971800871024,25.758887576175,-32.8422878495362));
#26349=CARTESIAN_POINT('Ctrl Pts',(-25.8686389259693,25.7891313146573,-32.8449614133608));
#26350=CARTESIAN_POINT('Ctrl Pts',(-25.8427131489051,25.8156704383487,-32.8473182379716));
#26351=CARTESIAN_POINT('Ctrl Pts',(-25.8126738666521,25.845376440473,-32.8499625221209));
#26352=CARTESIAN_POINT('Ctrl Pts',(-25.809005488428,25.8489867779354,-32.8502840034902));
#26353=CARTESIAN_POINT('Ctrl Pts',(-25.8035757308584,25.8543050792307,-32.850757705815));
#26354=CARTESIAN_POINT('Ctrl Pts',(-25.8018210483055,25.8560198219475,-32.8509104592977));
#26355=CARTESIAN_POINT('Ctrl Pts',(-25.7987135074864,25.8590496996146,-32.8511804024676));
#26356=CARTESIAN_POINT('Ctrl Pts',(-25.7973614515446,25.8603656511454,-32.8512976569204));
#26357=CARTESIAN_POINT('Ctrl Pts',(-25.7945380250747,25.8631088585408,-32.8515421060299));
#26358=CARTESIAN_POINT('Ctrl Pts',(-25.7930664513423,25.8645358951399,-32.8516692833866));
#26359=CARTESIAN_POINT('Ctrl Pts',(-25.7892244627109,25.8682544999243,-32.8520007226058));
#26360=CARTESIAN_POINT('Ctrl Pts',(-25.7868518833875,25.8705438437574,-32.852204809072));
#26361=CARTESIAN_POINT('Ctrl Pts',(-25.7765702746411,25.8804343270815,-32.8530866926373));
#26362=CARTESIAN_POINT('Ctrl Pts',(-25.7686258563344,25.8879988166541,-32.8537616503768));
#26363=CARTESIAN_POINT('Ctrl Pts',(-25.7110509021562,25.9422625517316,-32.858608236146));
#26364=CARTESIAN_POINT('Ctrl Pts',(-25.6599846933156,25.9874216482024,-32.862667468548));
#26365=CARTESIAN_POINT('Ctrl Pts',(-25.5736481366165,26.0590219997102,-32.8692219328439));
#26366=CARTESIAN_POINT('Ctrl Pts',(-25.539202555839,26.0864173723997,-32.8717609163356));
#26367=CARTESIAN_POINT('Ctrl Pts',(-25.2722679819864,26.289932287134,-32.8909561791572));
#26368=CARTESIAN_POINT('Ctrl Pts',(-25.0174044632498,26.4344614285616,-32.9066944801757));
#26369=CARTESIAN_POINT('Ctrl Pts',(-24.6546546661541,26.5794786291965,-32.9294330246753));
#26370=CARTESIAN_POINT('Ctrl Pts',(-24.5611101796028,26.6119642424164,-32.9353093113016));
#26371=CARTESIAN_POINT('Ctrl Pts',(-24.4564622976942,26.6429867795241,-32.9419529435307));
#26372=CARTESIAN_POINT('Ctrl Pts',(-24.4466851313176,26.645834844973,-32.942574287992));
#26373=CARTESIAN_POINT('Ctrl Pts',(-24.4328399272386,26.649796827138,-32.9434551090364));
#26374=CARTESIAN_POINT('Ctrl Pts',(-24.4287828782563,26.6509491921378,-32.9437133304078));
#26375=CARTESIAN_POINT('Ctrl Pts',(-24.4217031938542,26.6529450968397,-32.9441641402112));
#26376=CARTESIAN_POINT('Ctrl Pts',(-24.4186815595877,26.6537921937244,-32.9443566124584));
#26377=CARTESIAN_POINT('Ctrl Pts',(-24.412462212064,26.6555259562327,-32.9447529086426));
#26378=CARTESIAN_POINT('Ctrl Pts',(-24.4092643583715,26.656412098678,-32.9449567493252));
#26379=CARTESIAN_POINT('Ctrl Pts',(-24.401684330326,26.6584999643181,-32.9454401002292));
#26380=CARTESIAN_POINT('Ctrl Pts',(-24.3973009802778,26.6596973592401,-32.9457197509294));
#26381=CARTESIAN_POINT('Ctrl Pts',(-24.3880341363292,26.6622077238328,-32.9463112630458));
#26382=CARTESIAN_POINT('Ctrl Pts',(-24.3831500594962,26.6635184764309,-32.9466231957879));
#26383=CARTESIAN_POINT('Ctrl Pts',(-24.3699818299296,26.6670192640124,-32.94746470178));
#26384=CARTESIAN_POINT('Ctrl Pts',(-24.3616920375857,26.6691877525778,-32.9479949734354));
#26385=CARTESIAN_POINT('Ctrl Pts',(-24.2135519161788,26.7073084662701,-32.9574805693437));
#26386=CARTESIAN_POINT('Ctrl Pts',(-24.0714703429511,26.7338495096319,-32.9667414510033));
#26387=CARTESIAN_POINT('Ctrl Pts',(-23.761737303224,26.7704164516937,-32.9872886600487));
#26388=CARTESIAN_POINT('Ctrl Pts',(-23.5941031360689,26.7770543971564,-32.998635131657));
#26389=CARTESIAN_POINT('Ctrl Pts',(-23.2402316804886,26.7634809317805,-33.0225962090429));
#26390=CARTESIAN_POINT('Ctrl Pts',(-23.0546837852011,26.7401395627148,-33.0351630026068));
#26391=CARTESIAN_POINT('Ctrl Pts',(-22.8610286743464,26.698461255551,-33.0476453019769));
#26392=CARTESIAN_POINT('Ctrl Pts',(-22.8498891122367,26.6960018517268,-33.0483609794725));
#26393=CARTESIAN_POINT('Ctrl Pts',(-22.8353607991941,26.6927132774818,-33.0492911047388));
#26394=CARTESIAN_POINT('Ctrl Pts',(-22.8319601846165,26.691937721591,-33.0495085831789));
#26395=CARTESIAN_POINT('Ctrl Pts',(-22.8267249640257,26.6907348146592,-33.0498430216029));
#26396=CARTESIAN_POINT('Ctrl Pts',(-22.8248894759949,26.6903113764076,-33.0499602072532));
#26397=CARTESIAN_POINT('Ctrl Pts',(-22.8212372389396,26.6894654496845,-33.0501932419281));
#26398=CARTESIAN_POINT('Ctrl Pts',(-22.8194204960659,26.6890429957548,-33.0503090917033));
#26399=CARTESIAN_POINT('Ctrl Pts',(-22.8153645231524,26.688096133036,-33.050567578188));
#26400=CARTESIAN_POINT('Ctrl Pts',(-22.8131254923378,26.6875709056418,-33.0507101665289));
#26401=CARTESIAN_POINT('Ctrl Pts',(-22.8065674786844,26.6860251317832,-33.0511274991716));
#26402=CARTESIAN_POINT('Ctrl Pts',(-22.80225001707,26.6849980550526,-33.0514018660614));
#26403=CARTESIAN_POINT('Ctrl Pts',(-22.77048408867,26.6773719252353,-33.0534178007276));
#26404=CARTESIAN_POINT('Ctrl Pts',(-22.7431201570533,26.6704211149257,-33.0551393464126));
#26405=CARTESIAN_POINT('Ctrl Pts',(-22.6534129253988,26.6463750698616,-33.060744148782));
#26406=CARTESIAN_POINT('Ctrl Pts',(-22.5914890045306,26.6277628467614,-33.0645508962943));
#26407=CARTESIAN_POINT('Ctrl Pts',(-22.3842433140677,26.5586081210394,-33.0772088376499));
#26408=CARTESIAN_POINT('Ctrl Pts',(-22.2419874796715,26.4995286688493,-33.0857651520371));
#26409=CARTESIAN_POINT('Ctrl Pts',(-22.0946437916706,26.4255685299444,-33.0949784066172));
#26410=CARTESIAN_POINT('Ctrl Pts',(-22.0848262603312,26.4205773674136,-33.0955939796048));
#26411=CARTESIAN_POINT('Ctrl Pts',(-22.0750360001986,26.4155367667575,-33.0962096862788));
#26412=CARTESIAN_POINT('',(-26.7730025278725,23.5500955840177,-32.9388531742191));
#26413=CARTESIAN_POINT('Ctrl Pts',(-22.0750360407425,26.4155367876319,-33.3457833635692));
#26414=CARTESIAN_POINT('Ctrl Pts',(-22.0934975599687,26.4250418611875,-33.3445398102641));
#26415=CARTESIAN_POINT('Ctrl Pts',(-22.112057404666,26.4343718359091,-33.3432898004641));
#26416=CARTESIAN_POINT('Ctrl Pts',(-22.1489865025916,26.4524905249892,-33.3408021499824));
#26417=CARTESIAN_POINT('Ctrl Pts',(-22.1673439408664,26.4612825304923,-33.3395653147227));
#26418=CARTESIAN_POINT('Ctrl Pts',(-22.1913318126899,26.4724930341881,-33.3379484153733));
#26419=CARTESIAN_POINT('Ctrl Pts',(-22.1968878667446,26.475070330772,-33.3375738612578));
#26420=CARTESIAN_POINT('Ctrl Pts',(-22.2058231341918,26.4791842375785,-33.3369714106402));
#26421=CARTESIAN_POINT('Ctrl Pts',(-22.2091977331234,26.4807308833716,-33.3367438611689));
#26422=CARTESIAN_POINT('Ctrl Pts',(-22.2155902487557,26.4836473461102,-33.3363127707687));
#26423=CARTESIAN_POINT('Ctrl Pts',(-22.2186076231808,26.4850183459017,-33.336109270969));
#26424=CARTESIAN_POINT('Ctrl Pts',(-22.2245590236632,26.4877114065796,-33.3357078550636));
#26425=CARTESIAN_POINT('Ctrl Pts',(-22.2274929262389,26.489033732283,-33.3355099483746));
#26426=CARTESIAN_POINT('Ctrl Pts',(-22.2365709503581,26.4931088981848,-33.33489753076));
#26427=CARTESIAN_POINT('Ctrl Pts',(-22.2427216921104,26.4958468678803,-33.3344825092304));
#26428=CARTESIAN_POINT('Ctrl Pts',(-22.2749532048219,26.5100737072113,-33.3323072071324));
#26429=CARTESIAN_POINT('Ctrl Pts',(-22.3011762800028,26.5212352306522,-33.3305357575639));
#26430=CARTESIAN_POINT('Ctrl Pts',(-22.609118704902,26.6475095361506,-33.309707762113));
#26431=CARTESIAN_POINT('Ctrl Pts',(-22.9055735821883,26.7224815967412,-33.2891878761496));
#26432=CARTESIAN_POINT('Ctrl Pts',(-23.3588341836674,26.7708850918646,-33.2583693139221));
#26433=CARTESIAN_POINT('Ctrl Pts',(-23.5105910648775,26.7763262353634,-33.2481853320502));
#26434=CARTESIAN_POINT('Ctrl Pts',(-23.6694572013835,26.7708054078662,-33.2379986315153));
#26435=CARTESIAN_POINT('Ctrl Pts',(-23.6767334181999,26.7705278567195,-33.2375331354797));
#26436=CARTESIAN_POINT('Ctrl Pts',(-23.686994732268,26.7701016065472,-33.2368782269043));
#26437=CARTESIAN_POINT('Ctrl Pts',(-23.6899805990014,26.7699734142563,-33.2366878459587));
#26438=CARTESIAN_POINT('Ctrl Pts',(-23.7051621395935,26.7693004665252,-33.2357208218588));
#26439=CARTESIAN_POINT('Ctrl Pts',(-23.7173550338048,26.7686905624561,-33.2349473217719));
#26440=CARTESIAN_POINT('Ctrl Pts',(-23.7418179867142,26.7673274994166,-33.2334021530993));
#26441=CARTESIAN_POINT('Ctrl Pts',(-23.754087812286,26.7665733896745,-33.2326305457675));
#26442=CARTESIAN_POINT('Ctrl Pts',(-23.7699363465307,26.7655082727707,-33.2316385410066));
#26443=CARTESIAN_POINT('Ctrl Pts',(-23.7735190531659,26.7652614772053,-33.2314145968123));
#26444=CARTESIAN_POINT('Ctrl Pts',(-23.7790011998562,26.7648746302738,-33.2310724028891));
#26445=CARTESIAN_POINT('Ctrl Pts',(-23.7809009256648,26.7647388838606,-33.2309539105454));
#26446=CARTESIAN_POINT('Ctrl Pts',(-23.7844735270852,26.7644804174183,-33.2307312421432));
#26447=CARTESIAN_POINT('Ctrl Pts',(-23.7861464203984,26.7643580759092,-33.2306270452211));
#26448=CARTESIAN_POINT('Ctrl Pts',(-23.790000794754,26.7640731735606,-33.2303871325266));
#26449=CARTESIAN_POINT('Ctrl Pts',(-23.7921822023698,26.7639096979523,-33.2302514693569));
#26450=CARTESIAN_POINT('Ctrl Pts',(-23.7982668146116,26.7634474840974,-33.229873385367));
#26451=CARTESIAN_POINT('Ctrl Pts',(-23.802169660645,26.7631438537291,-33.2296312410973));
#26452=CARTESIAN_POINT('Ctrl Pts',(-23.8241538716531,26.7613932397491,-33.2282693092708));
#26453=CARTESIAN_POINT('Ctrl Pts',(-23.8422237931861,26.7598006945302,-33.2271576244526));
#26454=CARTESIAN_POINT('Ctrl Pts',(-23.8946149664489,26.7547372003608,-33.2239544766026));
#26455=CARTESIAN_POINT('Ctrl Pts',(-23.9288961922194,26.7508675772511,-33.2218835248355));
#26456=CARTESIAN_POINT('Ctrl Pts',(-24.0637070796941,26.7334538410463,-33.213814867673));
#26457=CARTESIAN_POINT('Ctrl Pts',(-24.1636431018701,26.7157164090414,-33.207998293565));
#26458=CARTESIAN_POINT('Ctrl Pts',(-24.3350497976686,26.6768692232602,-33.1980603507916));
#26459=CARTESIAN_POINT('Ctrl Pts',(-24.406928029046,26.6579439916959,-33.1939050691083));
#26460=CARTESIAN_POINT('Ctrl Pts',(-24.5557749688265,26.6131960086862,-33.1852193643978));
#26461=CARTESIAN_POINT('Ctrl Pts',(-24.6325506385452,26.5869165973926,-33.1806924514923));
#26462=CARTESIAN_POINT('Ctrl Pts',(-24.8947824507328,26.4859481403797,-33.1648687780428));
#26463=CARTESIAN_POINT('Ctrl Pts',(-25.0741970084934,26.3969426085533,-33.1533661924852));
#26464=CARTESIAN_POINT('Ctrl Pts',(-25.2546006401569,26.2854791351249,-33.1404768623262));
#26465=CARTESIAN_POINT('Ctrl Pts',(-25.2649650808094,26.2789936176864,-33.1397315731207));
#26466=CARTESIAN_POINT('Ctrl Pts',(-25.2794874153284,26.2697909017924,-33.138680459494));
#26467=CARTESIAN_POINT('Ctrl Pts',(-25.2836764058192,26.2671227717664,-33.1383764589223));
#26468=CARTESIAN_POINT('Ctrl Pts',(-25.2907595637828,26.2625881845202,-33.1378610523619));
#26469=CARTESIAN_POINT('Ctrl Pts',(-25.2936569469994,26.2607267460871,-33.1376498337871));
#26470=CARTESIAN_POINT('Ctrl Pts',(-25.2992164416482,26.2571424185173,-33.1372437950153));
#26471=CARTESIAN_POINT('Ctrl Pts',(-25.3018790061255,26.2554202365997,-33.137049001431));
#26472=CARTESIAN_POINT('Ctrl Pts',(-25.3073590406735,26.2518641950922,-33.1366473932997));
#26473=CARTESIAN_POINT('Ctrl Pts',(-25.3101761908232,26.250029851698,-33.1364405607687));
#26474=CARTESIAN_POINT('Ctrl Pts',(-25.3198341616743,26.2437196741262,-33.135730186922));
#26475=CARTESIAN_POINT('Ctrl Pts',(-25.3266607765907,26.2392222485213,-33.1352258348168));
#26476=CARTESIAN_POINT('Ctrl Pts',(-25.3805809713667,26.2034042706858,-33.131224345914));
#26477=CARTESIAN_POINT('Ctrl Pts',(-25.4268572011357,26.1708766186661,-33.1276816819474));
#26478=CARTESIAN_POINT('Ctrl Pts',(-25.5830425041545,26.0548349136855,-33.115334003637));
#26479=CARTESIAN_POINT('Ctrl Pts',(-25.6884173178196,25.965498047776,-33.1063052792513));
#26480=CARTESIAN_POINT('Ctrl Pts',(-25.9920850967049,25.6725608507018,-33.078148817936));
#26481=CARTESIAN_POINT('Ctrl Pts',(-26.1694835395828,25.4492962584218,-33.0584568692416));
#26482=CARTESIAN_POINT('Ctrl Pts',(-26.3335683822166,25.1752234889727,-33.0379419277616));
#26483=CARTESIAN_POINT('Ctrl Pts',(-26.3512995679964,25.1444650320273,-33.0356881699773));
#26484=CARTESIAN_POINT('Ctrl Pts',(-26.3707675269096,25.1093658051939,-33.0331761749419));
#26485=CARTESIAN_POINT('Ctrl Pts',(-26.3730065522511,25.1053084078306,-33.0328866870299));
#26486=CARTESIAN_POINT('Ctrl Pts',(-26.3763798428218,25.0991642865995,-33.0324496814402));
#26487=CARTESIAN_POINT('Ctrl Pts',(-26.3775205538046,25.0970811370757,-33.0323017527223));
#26488=CARTESIAN_POINT('Ctrl Pts',(-26.3794993398527,25.0934580056666,-33.032044880958));
#26489=CARTESIAN_POINT('Ctrl Pts',(-26.3803384609108,25.0919186011326,-33.0319358704661));
#26490=CARTESIAN_POINT('Ctrl Pts',(-26.3820915109339,25.0886962991249,-33.0317079609219));
#26491=CARTESIAN_POINT('Ctrl Pts',(-26.38300519554,25.0870132727936,-33.0315890780516));
#26492=CARTESIAN_POINT('Ctrl Pts',(-26.3851855519611,25.0829884585597,-33.0313051491347));
#26493=CARTESIAN_POINT('Ctrl Pts',(-26.3864508268256,25.0806459065231,-33.0311401932215));
#26494=CARTESIAN_POINT('Ctrl Pts',(-26.3907233234603,25.0727122347591,-33.0305825267814));
#26495=CARTESIAN_POINT('Ctrl Pts',(-26.3937169515039,25.0671137518563,-33.0301906827581));
#26496=CARTESIAN_POINT('Ctrl Pts',(-26.4007886855405,25.053794164906,-33.0292623257062));
#26497=CARTESIAN_POINT('Ctrl Pts',(-26.4048520181897,25.0460652147992,-33.0287267258366));
#26498=CARTESIAN_POINT('Ctrl Pts',(-26.4521185598003,24.9552644636975,-33.0224695368331));
#26499=CARTESIAN_POINT('Ctrl Pts',(-26.4917176430043,24.8703554270289,-33.0169616360652));
#26500=CARTESIAN_POINT('Ctrl Pts',(-26.6501299219583,24.4880190416136,-32.9931300871853));
#26501=CARTESIAN_POINT('Ctrl Pts',(-26.7279281297272,24.1755919286179,-32.9759853056577));
#26502=CARTESIAN_POINT('Ctrl Pts',(-26.7613682438287,23.8256322036592,-32.9554157090191));
#26503=CARTESIAN_POINT('Ctrl Pts',(-26.7638922506264,23.7944199831725,-32.9535715425229));
#26504=CARTESIAN_POINT('Ctrl Pts',(-26.7697429750524,23.7060588179885,-32.9483184815699));
#26505=CARTESIAN_POINT('Ctrl Pts',(-26.7720022991397,23.648853342671,-32.9448793374993));
#26506=CARTESIAN_POINT('Ctrl Pts',(-26.7728495196694,23.5828567386286,-32.9408577584136));
#26507=CARTESIAN_POINT('Ctrl Pts',(-26.7729262718921,23.5740924785577,-32.9403226086109));
#26508=CARTESIAN_POINT('Ctrl Pts',(-26.7729869265949,23.5611262650312,-32.9395292387437));
#26509=CARTESIAN_POINT('Ctrl Pts',(-26.7729983646242,23.5569244294693,-32.9392718832151));
#26510=CARTESIAN_POINT('Ctrl Pts',(-26.7730022562627,23.5518469269387,-32.9389605824208));
#26511=CARTESIAN_POINT('Ctrl Pts',(-26.7730025705176,23.5509712551186,-32.9389068839172));
#26512=CARTESIAN_POINT('Ctrl Pts',(-26.7730025278725,23.5500955840177,-32.9388531742191));
#26513=CARTESIAN_POINT('Ctrl Pts',(-26.7730025278685,23.5500955013274,-32.9388531691472));
#26514=CARTESIAN_POINT('Ctrl Pts',(-26.7730024448801,23.5483923217316,-32.9387487038255));
#26515=CARTESIAN_POINT('Ctrl Pts',(-26.7730010117309,23.5466891448804,-32.9386441961556));
#26516=CARTESIAN_POINT('Ctrl Pts',(-26.772992709127,23.5416085639561,-32.9383323222094));
#26517=CARTESIAN_POINT('Ctrl Pts',(-26.7729818806004,23.5382311766048,-32.9381248318214));
#26518=CARTESIAN_POINT('Ctrl Pts',(-26.7729435256734,23.53020407965,-32.9376312840049));
#26519=CARTESIAN_POINT('Ctrl Pts',(-26.7729112454758,23.5255544097048,-32.937345077671));
#26520=CARTESIAN_POINT('Ctrl Pts',(-26.7727734305524,23.5104212021922,-32.9364125139594));
#26521=CARTESIAN_POINT('Ctrl Pts',(-26.7726268024879,23.4999381883714,-32.9357648679799));
#26522=CARTESIAN_POINT('Ctrl Pts',(-26.7722380264066,23.4793332504897,-32.9344885898365));
#26523=CARTESIAN_POINT('Ctrl Pts',(-26.7719993249735,23.4692113766779,-32.9338600736771));
#26524=CARTESIAN_POINT('Ctrl Pts',(-26.7612907049837,23.0907913105067,-32.9103027448846));
#26525=CARTESIAN_POINT('Ctrl Pts',(-26.6877808583376,22.7270685989479,-32.885084236381));
#26526=CARTESIAN_POINT('Ctrl Pts',(-26.5081357901743,22.264385823112,-32.8518196064956));
#26527=CARTESIAN_POINT('Ctrl Pts',(-26.4546867999505,22.1478272357721,-32.8433775225756));
#26528=CARTESIAN_POINT('Ctrl Pts',(-26.3906799218286,22.0277041755948,-32.8348313886617));
#26529=CARTESIAN_POINT('Ctrl Pts',(-26.3869007472472,22.0206747599834,-32.8343318763894));
#26530=CARTESIAN_POINT('Ctrl Pts',(-26.3817036798259,22.0110935149354,-32.8336519194398));
#26531=CARTESIAN_POINT('Ctrl Pts',(-26.3803084160115,22.008529542656,-32.8334700480098));
#26532=CARTESIAN_POINT('Ctrl Pts',(-26.377967191008,22.0042411357324,-32.8331660071871));
#26533=CARTESIAN_POINT('Ctrl Pts',(-26.3770231348408,22.0025156715728,-32.8330437155999));
#26534=CARTESIAN_POINT('Ctrl Pts',(-26.375160036499,21.9991178524422,-32.832802978814));
#26535=CARTESIAN_POINT('Ctrl Pts',(-26.374241088537,21.9974454494284,-32.832684527838));
#26536=CARTESIAN_POINT('Ctrl Pts',(-26.3722108462576,21.9937583533224,-32.8324234673793));
#26537=CARTESIAN_POINT('Ctrl Pts',(-26.3710988767487,21.9917440286347,-32.8322809014323));
#26538=CARTESIAN_POINT('Ctrl Pts',(-26.3672025955125,21.9847037740034,-32.831782809551));
#26539=CARTESIAN_POINT('Ctrl Pts',(-26.3644069798813,21.979684062092,-32.831428007475));
#26540=CARTESIAN_POINT('Ctrl Pts',(-26.3358112527086,21.9286600398056,-32.8278247092542));
#26541=CARTESIAN_POINT('Ctrl Pts',(-26.308897036284,21.8832849595732,-32.8246465990569));
#26542=CARTESIAN_POINT('Ctrl Pts',(-26.2014680084607,21.7119029247497,-32.8126641634843));
#26543=CARTESIAN_POINT('Ctrl Pts',(-26.1133285652527,21.5908845319508,-32.8042430819917));
#26544=CARTESIAN_POINT('Ctrl Pts',(-25.9110167258903,21.3502333460017,-32.7866458254143));
#26545=CARTESIAN_POINT('Ctrl Pts',(-25.7954145153002,21.2323791317175,-32.7775002353527));
#26546=CARTESIAN_POINT('Ctrl Pts',(-25.606450882027,21.0671924849104,-32.7631272586304));
#26547=CARTESIAN_POINT('Ctrl Pts',(-25.5393491364183,21.0131219001765,-32.7581226245599));
#26548=CARTESIAN_POINT('Ctrl Pts',(-25.4224763846164,20.9264345351844,-32.7494949431218));
#26549=CARTESIAN_POINT('Ctrl Pts',(-25.3738212384152,20.8923888211743,-32.7459277758914));
#26550=CARTESIAN_POINT('Ctrl Pts',(-25.3173524649615,20.8551562880726,-32.7418043631227));
#26551=CARTESIAN_POINT('Ctrl Pts',(-25.3104316852225,20.8506312097284,-32.741299283889));
#26552=CARTESIAN_POINT('Ctrl Pts',(-25.3006646363791,20.8442986529883,-32.7405868543038));
#26553=CARTESIAN_POINT('Ctrl Pts',(-25.2978327870509,20.8424689028085,-32.7403803367974));
#26554=CARTESIAN_POINT('Ctrl Pts',(-25.2921745512692,20.8388255055654,-32.7399677847452));
#26555=CARTESIAN_POINT('Ctrl Pts',(-25.2893481908711,20.8370118257493,-32.7397617517658));
#26556=CARTESIAN_POINT('Ctrl Pts',(-25.2838747350031,20.8335115667915,-32.7393628324769));
#26557=CARTESIAN_POINT('Ctrl Pts',(-25.2812279991285,20.8318244297908,-32.7391699672304));
#26558=CARTESIAN_POINT('Ctrl Pts',(-25.2744888667233,20.8275424655377,-32.7386789806575));
#26559=CARTESIAN_POINT('Ctrl Pts',(-25.2703930854803,20.8249530035332,-32.7383806604875));
#26560=CARTESIAN_POINT('Ctrl Pts',(-25.2565231158068,20.8162277624099,-32.7373706942528));
#26561=CARTESIAN_POINT('Ctrl Pts',(-25.2467219008516,20.8101353044184,-32.7366574473003));
#26562=CARTESIAN_POINT('Ctrl Pts',(-25.0840016412879,20.7101957083805,-32.7248227451569));
#26563=CARTESIAN_POINT('Ctrl Pts',(-24.9235684379159,20.6292436815508,-32.7132238326056));
#26564=CARTESIAN_POINT('Ctrl Pts',(-24.6404389462193,20.5148803099678,-32.6928995698178));
#26565=CARTESIAN_POINT('Ctrl Pts',(-24.5209578058768,20.4745868465639,-32.6843706171678));
#26566=CARTESIAN_POINT('Ctrl Pts',(-24.3692103295671,20.4331373367921,-32.6737237044016));
#26567=CARTESIAN_POINT('Ctrl Pts',(-24.3388704104149,20.4253235925019,-32.6716043753079));
#26568=CARTESIAN_POINT('Ctrl Pts',(-24.2080795937979,20.3936658543684,-32.6625180722159));
#26569=CARTESIAN_POINT('Ctrl Pts',(-24.1066219995136,20.3742122802831,-32.6555931572272));
#26570=CARTESIAN_POINT('Ctrl Pts',(-23.962112668255,20.3536428876116,-32.6460414567569));
#26571=CARTESIAN_POINT('Ctrl Pts',(-23.9197078361218,20.3484647264754,-32.6432763534145));
#26572=CARTESIAN_POINT('Ctrl Pts',(-23.8505028150485,20.3414072492971,-32.6388381056639));
#26573=CARTESIAN_POINT('Ctrl Pts',(-23.8237610920042,20.3390173390903,-32.6371411308387));
#26574=CARTESIAN_POINT('Ctrl Pts',(-23.7926236343889,20.3366263862805,-32.6351885805348));
#26575=CARTESIAN_POINT('Ctrl Pts',(-23.788254982577,20.3362998892579,-32.6349151680174));
#26576=CARTESIAN_POINT('Ctrl Pts',(-23.7816037929846,20.3358164395047,-32.6344997301326));
#26577=CARTESIAN_POINT('Ctrl Pts',(-23.7793217535862,20.3356530094316,-32.634357340617));
#26578=CARTESIAN_POINT('Ctrl Pts',(-23.7751794865671,20.3353607909874,-32.634099152264));
#26579=CARTESIAN_POINT('Ctrl Pts',(-23.7733193275193,20.3352311874189,-32.6339833076684));
#26580=CARTESIAN_POINT('Ctrl Pts',(-23.7695725095829,20.3349734014089,-32.6337501686745));
#26581=CARTESIAN_POINT('Ctrl Pts',(-23.767685857983,20.3348452655748,-32.6336328773225));
#26582=CARTESIAN_POINT('Ctrl Pts',(-23.7622831977847,20.3344831095852,-32.6332972887105));
#26583=CARTESIAN_POINT('Ctrl Pts',(-23.7587669026956,20.3342531944893,-32.6330792237633));
#26584=CARTESIAN_POINT('Ctrl Pts',(-23.7435657184972,20.3332842918002,-32.6321380050906));
#26585=CARTESIAN_POINT('Ctrl Pts',(-23.7318770359504,20.3326032043024,-32.6314180791118));
#26586=CARTESIAN_POINT('Ctrl Pts',(-23.5315262038528,20.3220242024919,-32.6191393906247));
#26587=CARTESIAN_POINT('Ctrl Pts',(-23.3423248994838,20.3286694074378,-32.6084640003419));
#26588=CARTESIAN_POINT('Ctrl Pts',(-22.9894404253086,20.3723035744781,-32.588549400399));
#26589=CARTESIAN_POINT('Ctrl Pts',(-22.8259454551091,20.4055352459347,-32.579316486071));
#26590=CARTESIAN_POINT('Ctrl Pts',(-22.5244372085474,20.4915895526733,-32.5613824465345));
#26591=CARTESIAN_POINT('Ctrl Pts',(-22.3860584891629,20.5415385895365,-32.5527696868908));
#26592=CARTESIAN_POINT('Ctrl Pts',(-22.2427341036593,20.6046445157459,-32.5432328128197));
#26593=CARTESIAN_POINT('Ctrl Pts',(-22.2339039198737,20.6085799883571,-32.5426427231619));
#26594=CARTESIAN_POINT('Ctrl Pts',(-22.2218846027218,20.6140017614471,-32.541836020847));
#26595=CARTESIAN_POINT('Ctrl Pts',(-22.2186799344322,20.6154536700064,-32.5416205926686));
#26596=CARTESIAN_POINT('Ctrl Pts',(-22.2123383413912,20.6183393205256,-32.5411936136187));
#26597=CARTESIAN_POINT('Ctrl Pts',(-22.2092013276468,20.619772856553,-32.5409820700677));
#26598=CARTESIAN_POINT('Ctrl Pts',(-22.2030012036241,20.622618197052,-32.5405633135635));
#26599=CARTESIAN_POINT('Ctrl Pts',(-22.19993799602,20.624029779925,-32.5403561084788));
#26600=CARTESIAN_POINT('Ctrl Pts',(-22.1926742368548,20.6273908891914,-32.5398640115575));
#26601=CARTESIAN_POINT('Ctrl Pts',(-22.1884756686862,20.6293446620667,-32.5395789729213));
#26602=CARTESIAN_POINT('Ctrl Pts',(-22.174877681297,20.635708077134,-32.5386538597012));
#26603=CARTESIAN_POINT('Ctrl Pts',(-22.1654954290017,20.6401540592701,-32.5380125249133));
#26604=CARTESIAN_POINT('Ctrl Pts',(-22.0596522341203,20.6909378882987,-32.530742791405));
#26605=CARTESIAN_POINT('Ctrl Pts',(-21.9655456909224,20.7420023059026,-32.5239489342222));
#26606=CARTESIAN_POINT('Ctrl Pts',(-21.7250115949532,20.8884661623284,-32.5056650793883));
#26607=CARTESIAN_POINT('Ctrl Pts',(-21.583506544014,20.9912471509419,-32.493936398287));
#26608=CARTESIAN_POINT('Ctrl Pts',(-21.4269881206853,21.1256143325353,-32.4799772255557));
#26609=CARTESIAN_POINT('Ctrl Pts',(-21.4032449580152,21.1466134917307,-32.4778310510643));
#26610=CARTESIAN_POINT('Ctrl Pts',(-21.354467102715,21.1910535601611,-32.4733659870379));
#26611=CARTESIAN_POINT('Ctrl Pts',(-21.3294887965583,21.2145509442134,-32.4710476107752));
#26612=CARTESIAN_POINT('Ctrl Pts',(-21.274714305742,21.2677510737375,-32.4658983630617));
#26613=CARTESIAN_POINT('Ctrl Pts',(-21.2451146244644,21.297648150091,-32.4630709088906));
#26614=CARTESIAN_POINT('Ctrl Pts',(-21.1706952015629,21.3758187445105,-32.4558609967869));
#26615=CARTESIAN_POINT('Ctrl Pts',(-21.1267524101377,21.4249046598426,-32.4515049641448));
#26616=CARTESIAN_POINT('Ctrl Pts',(-21.0657346745248,21.4974194034751,-32.4453489385222));
#26617=CARTESIAN_POINT('Ctrl Pts',(-21.0474245075924,21.5197834132823,-32.443486805763));
#26618=CARTESIAN_POINT('Ctrl Pts',(-21.0127552722545,21.5633100515964,-32.4399367798627));
#26619=CARTESIAN_POINT('Ctrl Pts',(-20.9963538856645,21.5844360140202,-32.4382463935143));
#26620=CARTESIAN_POINT('Ctrl Pts',(-20.977576189165,21.6092545533601,-32.4363005695847));
#26621=CARTESIAN_POINT('Ctrl Pts',(-20.9749427294391,21.612749979888,-32.4360274333464));
#26622=CARTESIAN_POINT('Ctrl Pts',(-20.9709439626368,21.6180801537199,-32.4356123289803));
#26623=CARTESIAN_POINT('Ctrl Pts',(-20.9695734882036,21.6199109901045,-32.4354699975957));
#26624=CARTESIAN_POINT('Ctrl Pts',(-20.9670891588567,21.6232372155766,-32.4352118703271));
#26625=CARTESIAN_POINT('Ctrl Pts',(-20.9659746566322,21.6247321075389,-32.4350960287873));
#26626=CARTESIAN_POINT('Ctrl Pts',(-20.9635617626,21.6279744126945,-32.434845140499));
#26627=CARTESIAN_POINT('Ctrl Pts',(-20.9622638473796,21.6297221696251,-32.4347101276146));
#26628=CARTESIAN_POINT('Ctrl Pts',(-20.9587261818786,21.6344960454671,-32.4343419667466));
#26629=CARTESIAN_POINT('Ctrl Pts',(-20.9564899527783,21.6375247881644,-32.4341090663784));
#26630=CARTESIAN_POINT('Ctrl Pts',(-20.9457494194838,21.6521252105784,-32.4329895551772));
#26631=CARTESIAN_POINT('Ctrl Pts',(-20.9373170430352,21.6637499637321,-32.4321079066826));
#26632=CARTESIAN_POINT('Ctrl Pts',(-20.7854078230201,21.8761425095127,-32.4161672995348));
#26633=CARTESIAN_POINT('Ctrl Pts',(-20.6653543271839,22.0927148868873,-32.402584711569));
#26634=CARTESIAN_POINT('Ctrl Pts',(-20.5157421235767,22.4552672554377,-32.3806514408196));
#26635=CARTESIAN_POINT('Ctrl Pts',(-20.4694512672832,22.593223081863,-32.3724796837955));
#26636=CARTESIAN_POINT('Ctrl Pts',(-20.4081303995654,22.8273833972928,-32.3584314549032));
#26637=CARTESIAN_POINT('Ctrl Pts',(-20.387855446206,22.9219905029053,-32.3527115057707));
#26638=CARTESIAN_POINT('Ctrl Pts',(-20.368984280358,23.0345456970131,-32.3457961172374));
#26639=CARTESIAN_POINT('Ctrl Pts',(-20.3662423233057,23.0517545873036,-32.3447358629701));
#26640=CARTESIAN_POINT('Ctrl Pts',(-20.363011548495,23.0731464704354,-32.3434139987673));
#26641=CARTESIAN_POINT('Ctrl Pts',(-20.3623911469561,23.0773095434755,-32.3431565683048));
#26642=CARTESIAN_POINT('Ctrl Pts',(-20.36120745584,23.0853606082667,-32.3426583597296));
#26643=CARTESIAN_POINT('Ctrl Pts',(-20.3606431161796,23.0892484400211,-32.3424176153482));
#26644=CARTESIAN_POINT('Ctrl Pts',(-20.3596368733398,23.0962709192129,-32.3419824711307));
#26645=CARTESIAN_POINT('Ctrl Pts',(-20.3591924765587,23.0994052091849,-32.3417881506289));
#26646=CARTESIAN_POINT('Ctrl Pts',(-20.3582861849751,23.1058656724,-32.3413873929794));
#26647=CARTESIAN_POINT('Ctrl Pts',(-20.3578248696292,23.1091919217463,-32.3411809377242));
#26648=CARTESIAN_POINT('Ctrl Pts',(-20.3565688157848,23.1183537348506,-32.3406119436688));
#26649=CARTESIAN_POINT('Ctrl Pts',(-20.3557848764421,23.1241907441664,-32.3402490631975));
#26650=CARTESIAN_POINT('Ctrl Pts',(-20.3526121809303,23.1483148806608,-32.3387477260275));
#26651=CARTESIAN_POINT('Ctrl Pts',(-20.3503644586864,23.1666199136702,-32.3376048154102));
#26652=CARTESIAN_POINT('Ctrl Pts',(-20.3032741230911,23.5793718432674,-32.3117465916405));
#26653=CARTESIAN_POINT('Ctrl Pts',(-20.3315604187292,23.9786734206678,-32.2843093577868));
#26654=CARTESIAN_POINT('Ctrl Pts',(-20.4392175007159,24.3919768048705,-32.2559392313534));
#26655=CARTESIAN_POINT('Ctrl Pts',(-20.4472826421083,24.4212385718692,-32.253934274045));
#26656=CARTESIAN_POINT('Ctrl Pts',(-20.4697908015396,24.4986177343839,-32.2486492499378));
#26657=CARTESIAN_POINT('Ctrl Pts',(-20.4849481944475,24.5465210535561,-32.2453948329886));
#26658=CARTESIAN_POINT('Ctrl Pts',(-20.5090014674843,24.6167827500001,-32.2406666758664));
#26659=CARTESIAN_POINT('Ctrl Pts',(-20.5170368694584,24.6394254161046,-32.2391500367616));
#26660=CARTESIAN_POINT('Ctrl Pts',(-20.5267917606022,24.665967821038,-32.2373823008174));
#26661=CARTESIAN_POINT('Ctrl Pts',(-20.5282664109006,24.6699558528619,-32.2371169664158));
#26662=CARTESIAN_POINT('Ctrl Pts',(-20.5305371508951,24.6760596606071,-32.236711290985));
#26663=CARTESIAN_POINT('Ctrl Pts',(-20.5313275741362,24.6781775173447,-32.236570611438));
#26664=CARTESIAN_POINT('Ctrl Pts',(-20.5327675149939,24.6820233318838,-32.236315297225));
#26665=CARTESIAN_POINT('Ctrl Pts',(-20.5334162863201,24.6837515563149,-32.2362006183124));
#26666=CARTESIAN_POINT('Ctrl Pts',(-20.534736934515,24.6872603890066,-32.2359678935264));
#26667=CARTESIAN_POINT('Ctrl Pts',(-20.5354089011075,24.6890409525952,-32.2358498537634));
#26668=CARTESIAN_POINT('Ctrl Pts',(-20.5373508916225,24.6941730338864,-32.2355097913419));
#26669=CARTESIAN_POINT('Ctrl Pts',(-20.5386249348863,24.6975230431797,-32.235288010993));
#26670=CARTESIAN_POINT('Ctrl Pts',(-20.5442710332671,24.7122948568668,-32.2343109200981));
#26671=CARTESIAN_POINT('Ctrl Pts',(-20.5487025708757,24.7236940421205,-32.2335591480033));
#26672=CARTESIAN_POINT('Ctrl Pts',(-20.5547533042494,24.738999693843,-32.2325524044189));
#26673=CARTESIAN_POINT('Ctrl Pts',(-20.5563153774292,24.7429284113427,-32.2322942259462));
#26674=CARTESIAN_POINT('Ctrl Pts',(-20.678673881811,25.0489129699255,-32.2122038405596));
#26675=CARTESIAN_POINT('Ctrl Pts',(-20.8445229843576,25.3309994501408,-32.1948762701202));
#26676=CARTESIAN_POINT('Ctrl Pts',(-21.0997007465806,25.6448067668107,-32.1719248236123));
#26677=CARTESIAN_POINT('Ctrl Pts',(-21.1517893618659,25.7042568936529,-32.1673917865189));
#26678=CARTESIAN_POINT('Ctrl Pts',(-21.264216841234,25.8234340142811,-32.1578302418444));
#26679=CARTESIAN_POINT('Ctrl Pts',(-21.3248350630511,25.8828108690017,-32.1527934724041));
#26680=CARTESIAN_POINT('Ctrl Pts',(-21.3996273160094,25.9504997317078,-32.1466760200205));
#26681=CARTESIAN_POINT('Ctrl Pts',(-21.4116139476544,25.9611860504339,-32.1456984676126));
#26682=CARTESIAN_POINT('Ctrl Pts',(-21.4267636816768,25.9744904555619,-32.1444663326936));
#26683=CARTESIAN_POINT('Ctrl Pts',(-21.4298527449872,25.9771928177238,-32.1442152725309));
#26684=CARTESIAN_POINT('Ctrl Pts',(-21.435388514586,25.9820169610702,-32.1437656670329));
#26685=CARTESIAN_POINT('Ctrl Pts',(-21.4378332770202,25.9841409726871,-32.1435672147236));
#26686=CARTESIAN_POINT('Ctrl Pts',(-21.442768759651,25.9884158861818,-32.1431667927152));
#26687=CARTESIAN_POINT('Ctrl Pts',(-21.4452595808544,25.9905666650337,-32.1429648182638));
#26688=CARTESIAN_POINT('Ctrl Pts',(-21.4502401611088,25.9948540063139,-32.1425611707035));
#26689=CARTESIAN_POINT('Ctrl Pts',(-21.45272989724,25.9969905896301,-32.1423594987949));
#26690=CARTESIAN_POINT('Ctrl Pts',(-21.4594261472661,26.0027192880005,-32.1418173777458));
#26691=CARTESIAN_POINT('Ctrl Pts',(-21.4636386401292,26.0063043689985,-32.141476639139));
#26692=CARTESIAN_POINT('Ctrl Pts',(-21.4799286346328,26.020095960544,-32.1401601164727));
#26693=CARTESIAN_POINT('Ctrl Pts',(-21.492071805969,26.0302242427611,-32.1391811315167));
#26694=CARTESIAN_POINT('Ctrl Pts',(-21.6808000738247,26.1852963789888,-32.1240010788068));
#26695=CARTESIAN_POINT('Ctrl Pts',(-21.8721373965565,26.3110726560551,-32.1090129910853));
#26696=CARTESIAN_POINT('Ctrl Pts',(-22.0750360188393,26.4155367763548,-32.0936416103654));
#26697=CARTESIAN_POINT('Origin',(-23.5502525316942,23.5502525316942,-77.3107734492734));
#26698=CARTESIAN_POINT('',(-22.0750360141079,26.4155367739188,-30.5945512678406));
#26699=CARTESIAN_POINT('',(-22.0750360153473,26.4155367745569,-30.8398067994259));
#26700=CARTESIAN_POINT('',(-22.0750360153461,26.4155367745563,-77.3107734492734));
#26701=CARTESIAN_POINT('',(-26.7730022123545,23.5516872106683,-31.4417267961338));
#26702=CARTESIAN_POINT('Ctrl Pts',(-22.0750360141079,26.4155367739188,-30.5945512678406));
#26703=CARTESIAN_POINT('Ctrl Pts',(-22.0688193424089,26.4123360664149,-30.5950155140757));
#26704=CARTESIAN_POINT('Ctrl Pts',(-22.062612960042,26.4091150613421,-30.5954802403181));
#26705=CARTESIAN_POINT('Ctrl Pts',(-21.899720217809,26.3239024409474,-30.6077100556798));
#26706=CARTESIAN_POINT('Ctrl Pts',(-21.7500411724996,26.2291746960651,-30.6197661635553));
#26707=CARTESIAN_POINT('Ctrl Pts',(-21.5169744860561,26.0532828368445,-30.6394290545501));
#26708=CARTESIAN_POINT('Ctrl Pts',(-21.4288260479307,25.9790248359596,-30.6471016274814));
#26709=CARTESIAN_POINT('Ctrl Pts',(-21.3166967554925,25.873791936247,-30.6569980997168));
#26710=CARTESIAN_POINT('Ctrl Pts',(-21.2890327311311,25.8468787778165,-30.6594514707787));
#26711=CARTESIAN_POINT('Ctrl Pts',(-21.2585147040126,25.8161028858665,-30.6621644779852));
#26712=CARTESIAN_POINT('Ctrl Pts',(-21.255179510802,25.812724615011,-30.6624610609334));
#26713=CARTESIAN_POINT('Ctrl Pts',(-21.2501666828563,25.8076245500372,-30.6629069451011));
#26714=CARTESIAN_POINT('Ctrl Pts',(-21.2484835085805,25.8059082469019,-30.6630566811204));
#26715=CARTESIAN_POINT('Ctrl Pts',(-21.245570936239,25.8029316934211,-30.6633158170107));
#26716=CARTESIAN_POINT('Ctrl Pts',(-21.2443406507547,25.8016723191805,-30.6634252872606));
#26717=CARTESIAN_POINT('Ctrl Pts',(-21.2418053389746,25.7990728046313,-30.663650897408));
#26718=CARTESIAN_POINT('Ctrl Pts',(-21.2405004489038,25.7977325377478,-30.6637670262256));
#26719=CARTESIAN_POINT('Ctrl Pts',(-21.2374183707592,25.7945613823296,-30.664041342683));
#26720=CARTESIAN_POINT('Ctrl Pts',(-21.2356421837266,25.7927295126724,-30.6641994509686));
#26721=CARTESIAN_POINT('Ctrl Pts',(-21.2318835565197,25.7888438310577,-30.6645340769204));
#26722=CARTESIAN_POINT('Ctrl Pts',(-21.2299016639369,25.7867894889755,-30.6647105517354));
#26723=CARTESIAN_POINT('Ctrl Pts',(-21.2245417167,25.7812188118585,-30.6651879093344));
#26724=CARTESIAN_POINT('Ctrl Pts',(-21.2211688918846,25.777697421632,-30.6654883892477));
#26725=CARTESIAN_POINT('Ctrl Pts',(-21.1100184276691,25.6611225368121,-30.6753943383473));
#26726=CARTESIAN_POINT('Ctrl Pts',(-21.0105765751098,25.5403720102892,-30.6843764975585));
#26727=CARTESIAN_POINT('Ctrl Pts',(-20.877547983966,25.3525380594509,-30.6973657461954));
#26728=CARTESIAN_POINT('Ctrl Pts',(-20.8369091959534,25.2907556286848,-30.7014960095386));
#26729=CARTESIAN_POINT('Ctrl Pts',(-20.6589738741963,24.9988436939193,-30.7205980272287));
#26730=CARTESIAN_POINT('Ctrl Pts',(-20.548613374255,24.7535998448811,-30.735610210697));
#26731=CARTESIAN_POINT('Ctrl Pts',(-20.4648314815904,24.4811598058575,-30.7528808069889));
#26732=CARTESIAN_POINT('Ctrl Pts',(-20.4599236733617,24.4647354124297,-30.7539236727784));
#26733=CARTESIAN_POINT('Ctrl Pts',(-20.4535215918402,24.4426700812377,-30.7553272176433));
#26734=CARTESIAN_POINT('Ctrl Pts',(-20.4519112059637,24.4370628976378,-30.7556840987633));
#26735=CARTESIAN_POINT('Ctrl Pts',(-20.4494144678361,24.4282797161752,-30.7562434714147));
#26736=CARTESIAN_POINT('Ctrl Pts',(-20.4485177442805,24.4251066586071,-30.7564456243198));
#26737=CARTESIAN_POINT('Ctrl Pts',(-20.4468094100747,24.4190260728576,-30.756833151735));
#26738=CARTESIAN_POINT('Ctrl Pts',(-20.4459970113297,24.4161187679806,-30.7570185003342));
#26739=CARTESIAN_POINT('Ctrl Pts',(-20.4441037279792,24.4093064236934,-30.7574529494429));
#26740=CARTESIAN_POINT('Ctrl Pts',(-20.4430261225694,24.4054004851967,-30.7577021564311));
#26741=CARTESIAN_POINT('Ctrl Pts',(-20.4399504322976,24.3941696247325,-30.7584190316677));
#26742=CARTESIAN_POINT('Ctrl Pts',(-20.4379708730884,24.3868396971216,-30.758887301615));
#26743=CARTESIAN_POINT('Ctrl Pts',(-20.4250967562733,24.338491175706,-30.7619787102857));
#26744=CARTESIAN_POINT('Ctrl Pts',(-20.4149879066645,24.2972694215607,-30.7646272107363));
#26745=CARTESIAN_POINT('Ctrl Pts',(-20.3876267492122,24.175334061134,-30.772503631982));
#26746=CARTESIAN_POINT('Ctrl Pts',(-20.3726584837218,24.0941485426546,-30.7778025121034));
#26747=CARTESIAN_POINT('Ctrl Pts',(-20.3180199506583,23.7171385062734,-30.8026613816379));
#26748=CARTESIAN_POINT('Ctrl Pts',(-20.3164514857571,23.4173368954558,-30.8233146469624));
#26749=CARTESIAN_POINT('Ctrl Pts',(-20.3642743761263,23.0609594223086,-30.8470940150785));
#26750=CARTESIAN_POINT('Ctrl Pts',(-20.3741430726408,23.0005305293944,-30.8510914733854));
#26751=CARTESIAN_POINT('Ctrl Pts',(-20.3865311623377,22.9362470909539,-30.8552819171807));
#26752=CARTESIAN_POINT('Ctrl Pts',(-20.3873427156918,22.9320801605561,-30.8555532656844));
#26753=CARTESIAN_POINT('Ctrl Pts',(-20.38912763034,22.9230110318233,-30.8561432129615));
#26754=CARTESIAN_POINT('Ctrl Pts',(-20.3901041687273,22.918109457786,-30.8564616593882));
#26755=CARTESIAN_POINT('Ctrl Pts',(-20.3929137783052,22.9041763074973,-30.8573656916613));
#26756=CARTESIAN_POINT('Ctrl Pts',(-20.3947742096878,22.895150207601,-30.8579499264987));
#26757=CARTESIAN_POINT('Ctrl Pts',(-20.3996015829667,22.872227401869,-30.8594298547032));
#26758=CARTESIAN_POINT('Ctrl Pts',(-20.4026218030166,22.8583419225298,-30.8603227612037));
#26759=CARTESIAN_POINT('Ctrl Pts',(-20.4065550468342,22.8408177230264,-30.8614447563083));
#26760=CARTESIAN_POINT('Ctrl Pts',(-20.4073826525067,22.8371602887824,-30.861678654897));
#26761=CARTESIAN_POINT('Ctrl Pts',(-20.4087000209977,22.8313852916403,-30.8620475385581));
#26762=CARTESIAN_POINT('Ctrl Pts',(-20.4091855422439,22.8292667800049,-30.8621827677511));
#26763=CARTESIAN_POINT('Ctrl Pts',(-20.4100833454658,22.825367447266,-30.8624314975878));
#26764=CARTESIAN_POINT('Ctrl Pts',(-20.410494996931,22.8235864965073,-30.8625450338012));
#26765=CARTESIAN_POINT('Ctrl Pts',(-20.4114117765175,22.8196355045837,-30.8627967633902));
#26766=CARTESIAN_POINT('Ctrl Pts',(-20.4119176386763,22.8174656418001,-30.8629349133568));
#26767=CARTESIAN_POINT('Ctrl Pts',(-20.4133738798484,22.8112483565606,-30.8633304751454));
#26768=CARTESIAN_POINT('Ctrl Pts',(-20.4143298456853,22.8072022271339,-30.8635875640133));
#26769=CARTESIAN_POINT('Ctrl Pts',(-20.4165018556151,22.798088037533,-30.864165936676));
#26770=CARTESIAN_POINT('Ctrl Pts',(-20.4177223729979,22.7930210401099,-30.8644869657952));
#26771=CARTESIAN_POINT('Ctrl Pts',(-20.4216052914896,22.7770710947,-30.8654959461207));
#26772=CARTESIAN_POINT('Ctrl Pts',(-20.4243121893018,22.7661989159458,-30.8661814234864));
#26773=CARTESIAN_POINT('Ctrl Pts',(-20.4348882757984,22.7246458854925,-30.8687932994691));
#26774=CARTESIAN_POINT('Ctrl Pts',(-20.4431531922583,22.6940664281832,-30.8706987091507));
#26775=CARTESIAN_POINT('Ctrl Pts',(-20.4763521434528,22.5780519023696,-30.8778810748318));
#26776=CARTESIAN_POINT('Ctrl Pts',(-20.5043719285262,22.4935352122634,-30.883017142151));
#26777=CARTESIAN_POINT('Ctrl Pts',(-20.6638256231471,22.0718961832287,-30.9086423038742));
#26778=CARTESIAN_POINT('Ctrl Pts',(-20.8478374017651,21.7575008613413,-30.9281001657211));
#26779=CARTESIAN_POINT('Ctrl Pts',(-21.0933477263073,21.4645502289282,-30.9512144363502));
#26780=CARTESIAN_POINT('Ctrl Pts',(-21.1066246449303,21.4490105086031,-30.9524563951814));
#26781=CARTESIAN_POINT('Ctrl Pts',(-21.1241595226107,21.4288781051536,-30.9540867064273));
#26782=CARTESIAN_POINT('Ctrl Pts',(-21.1282845189385,21.4241698214925,-30.9544695223864));
#26783=CARTESIAN_POINT('Ctrl Pts',(-21.1346599792993,21.4169354833713,-30.9550601177974));
#26784=CARTESIAN_POINT('Ctrl Pts',(-21.136900763485,21.4144008864263,-30.9552674917682));
#26785=CARTESIAN_POINT('Ctrl Pts',(-21.1413635894362,21.4093688821453,-30.9556801054323));
#26786=CARTESIAN_POINT('Ctrl Pts',(-21.1435855342923,21.4068713942104,-30.9558853409126));
#26787=CARTESIAN_POINT('Ctrl Pts',(-21.1485090576894,21.4013546136284,-30.9563396843252));
#26788=CARTESIAN_POINT('Ctrl Pts',(-21.15121244896,21.3983369528698,-30.9565888685124));
#26789=CARTESIAN_POINT('Ctrl Pts',(-21.1589972090813,21.3896801155723,-30.9573056143887));
#26790=CARTESIAN_POINT('Ctrl Pts',(-21.1640927952532,21.3840538118536,-30.9577737774453));
#26791=CARTESIAN_POINT('Ctrl Pts',(-21.1977854299399,21.3471151427167,-30.960862918915));
#26792=CARTESIAN_POINT('Ctrl Pts',(-21.2269771102778,21.3163530579887,-30.9635092164275));
#26793=CARTESIAN_POINT('Ctrl Pts',(-21.3147468184241,21.227443200642,-30.9713833876034));
#26794=CARTESIAN_POINT('Ctrl Pts',(-21.3749576129802,21.1709629224028,-30.9766822698665));
#26795=CARTESIAN_POINT('Ctrl Pts',(-21.5628069315596,21.0078478194128,-30.9929165435534));
#26796=CARTESIAN_POINT('Ctrl Pts',(-21.6965842494174,20.908725455064,-31.0041053059787));
#26797=CARTESIAN_POINT('Ctrl Pts',(-22.0177484779828,20.7072115974436,-31.0297668914548));
#26798=CARTESIAN_POINT('Ctrl Pts',(-22.2088928401764,20.6121876235452,-31.044227353144));
#26799=CARTESIAN_POINT('Ctrl Pts',(-22.4202854353151,20.5320637313955,-31.0584951313363));
#26800=CARTESIAN_POINT('Ctrl Pts',(-22.4325671010641,20.5274940952138,-31.0593180401287));
#26801=CARTESIAN_POINT('Ctrl Pts',(-22.4482929948901,20.5217519175124,-31.0603637199532));
#26802=CARTESIAN_POINT('Ctrl Pts',(-22.4517115739019,20.5205102068063,-31.0605905539662));
#26803=CARTESIAN_POINT('Ctrl Pts',(-22.4571516406263,20.5185446607647,-31.0609507467402));
#26804=CARTESIAN_POINT('Ctrl Pts',(-22.4591717493049,20.5178170585019,-31.061084330922));
#26805=CARTESIAN_POINT('Ctrl Pts',(-22.4629376066325,20.516464923129,-31.0613330389747));
#26806=CARTESIAN_POINT('Ctrl Pts',(-22.4646831553819,20.5158398818747,-31.0614481927496));
#26807=CARTESIAN_POINT('Ctrl Pts',(-22.4685693130123,20.5144521198096,-31.0617042800127));
#26808=CARTESIAN_POINT('Ctrl Pts',(-22.4707101848415,20.513690158252,-31.0618451673615));
#26809=CARTESIAN_POINT('Ctrl Pts',(-22.4769689536497,20.511470044118,-31.0622564959152));
#26810=CARTESIAN_POINT('Ctrl Pts',(-22.4810890325076,20.5100179916889,-31.0625265724818));
#26811=CARTESIAN_POINT('Ctrl Pts',(-22.4904360282522,20.5067451508924,-31.0631377296184));
#26812=CARTESIAN_POINT('Ctrl Pts',(-22.4956647253006,20.5049294359247,-31.0634785128338));
#26813=CARTESIAN_POINT('Ctrl Pts',(-22.5123915937022,20.4991691172093,-31.0645652697315));
#26814=CARTESIAN_POINT('Ctrl Pts',(-22.5239075780579,20.4952760382373,-31.0653083063372));
#26815=CARTESIAN_POINT('Ctrl Pts',(-22.5690511218993,20.4802989495067,-31.0682019070743));
#26816=CARTESIAN_POINT('Ctrl Pts',(-22.6028397255656,20.4697038130985,-31.070326222368));
#26817=CARTESIAN_POINT('Ctrl Pts',(-22.7431133018594,20.4282444850772,-31.0790012601664));
#26818=CARTESIAN_POINT('Ctrl Pts',(-22.8509892320622,20.4023257435799,-31.0853339075474));
#26819=CARTESIAN_POINT('Ctrl Pts',(-23.1894211283398,20.339274232726,-31.1047429962862));
#26820=CARTESIAN_POINT('Ctrl Pts',(-23.4228011284631,20.3215785353226,-31.1175322274701));
#26821=CARTESIAN_POINT('Ctrl Pts',(-23.6977092200726,20.3306078702418,-31.1334451469605));
#26822=CARTESIAN_POINT('Ctrl Pts',(-23.7393402189706,20.3327844487018,-31.1358759734865));
#26823=CARTESIAN_POINT('Ctrl Pts',(-23.7923435688999,20.3365878399093,-31.1390037574374));
#26824=CARTESIAN_POINT('Ctrl Pts',(-23.803766462553,20.3374687693223,-31.1396797831305));
#26825=CARTESIAN_POINT('Ctrl Pts',(-23.8257221586846,20.3392798054361,-31.1409830735552));
#26826=CARTESIAN_POINT('Ctrl Pts',(-23.8362555695916,20.340200877478,-31.1416100723895));
#26827=CARTESIAN_POINT('Ctrl Pts',(-23.8995834695129,20.3460526272284,-31.1453904816775));
#26828=CARTESIAN_POINT('Ctrl Pts',(-23.9522517610108,20.3522335748746,-31.1485800592518));
#26829=CARTESIAN_POINT('Ctrl Pts',(-24.0133907474882,20.3609427497327,-31.152343516821));
#26830=CARTESIAN_POINT('Ctrl Pts',(-24.0220350087488,20.3622099999483,-31.1528770400366));
#26831=CARTESIAN_POINT('Ctrl Pts',(-24.0349149274915,20.3641517298804,-31.1536741395037));
#26832=CARTESIAN_POINT('Ctrl Pts',(-24.039154614404,20.3647995481361,-31.1539368689923));
#26833=CARTESIAN_POINT('Ctrl Pts',(-24.0467160222195,20.3659703720155,-31.1544060681523));
#26834=CARTESIAN_POINT('Ctrl Pts',(-24.0500382476838,20.3664901178466,-31.1546124339637));
#26835=CARTESIAN_POINT('Ctrl Pts',(-24.0570426464262,20.3675971552116,-31.1550479818217));
#26836=CARTESIAN_POINT('Ctrl Pts',(-24.0607246238067,20.3681856391177,-31.1552772015041));
#26837=CARTESIAN_POINT('Ctrl Pts',(-24.0704516824326,20.3697576147968,-31.1558834641308));
#26838=CARTESIAN_POINT('Ctrl Pts',(-24.0764949742184,20.3707519476879,-31.1562608515199));
#26839=CARTESIAN_POINT('Ctrl Pts',(-24.1038653751817,20.3753355074606,-31.1579733744937));
#26840=CARTESIAN_POINT('Ctrl Pts',(-24.1251584599197,20.379122066354,-31.1593147809428));
#26841=CARTESIAN_POINT('Ctrl Pts',(-24.281225190003,20.4084990001218,-31.1692155659));
#26842=CARTESIAN_POINT('Ctrl Pts',(-24.414262639076,20.4424536514726,-31.1780434244342));
#26843=CARTESIAN_POINT('Ctrl Pts',(-24.6778484949909,20.5279630428011,-31.1963246044052));
#26844=CARTESIAN_POINT('Ctrl Pts',(-24.8080148772339,20.5797752720373,-31.2057678805051));
#26845=CARTESIAN_POINT('Ctrl Pts',(-24.996123189273,20.6692373938036,-31.2198674738231));
#26846=CARTESIAN_POINT('Ctrl Pts',(-25.05690510107,20.7005528205261,-31.2244963167398));
#26847=CARTESIAN_POINT('Ctrl Pts',(-25.2073646350865,20.7842314678988,-31.2360817681565));
#26848=CARTESIAN_POINT('Ctrl Pts',(-25.2956007694072,20.8390431807035,-31.2429954405808));
#26849=CARTESIAN_POINT('Ctrl Pts',(-25.4187194192767,20.9240299779544,-31.2526681127528));
#26850=CARTESIAN_POINT('Ctrl Pts',(-25.4558394432219,20.950838660306,-31.2555876826491));
#26851=CARTESIAN_POINT('Ctrl Pts',(-25.4963522876585,20.9814321592773,-31.258766466337));
#26852=CARTESIAN_POINT('Ctrl Pts',(-25.5003197417942,20.9844426706967,-31.2590776837455));
#26853=CARTESIAN_POINT('Ctrl Pts',(-25.5062386342304,20.9889555957295,-31.2595418320974));
#26854=CARTESIAN_POINT('Ctrl Pts',(-25.508195331449,20.9904510510155,-31.2596952488355));
#26855=CARTESIAN_POINT('Ctrl Pts',(-25.5115601203913,20.9930287911824,-31.2599590246219));
#26856=CARTESIAN_POINT('Ctrl Pts',(-25.512969031341,20.994109996825,-31.2600694601017));
#26857=CARTESIAN_POINT('Ctrl Pts',(-25.5157939672834,20.9962815801149,-31.2602908608919));
#26858=CARTESIAN_POINT('Ctrl Pts',(-25.5172099761744,20.9973719688506,-31.2604018245894));
#26859=CARTESIAN_POINT('Ctrl Pts',(-25.5205647300228,20.9999597241063,-31.2606646834562));
#26860=CARTESIAN_POINT('Ctrl Pts',(-25.5225026810649,21.0014581281143,-31.2608165045997));
#26861=CARTESIAN_POINT('Ctrl Pts',(-25.5285788433304,21.0061672342897,-31.2612924446229));
#26862=CARTESIAN_POINT('Ctrl Pts',(-25.5327109638382,21.0093858367416,-31.2616160032855));
#26863=CARTESIAN_POINT('Ctrl Pts',(-25.5422877550396,21.0168830005951,-31.262365698121));
#26864=CARTESIAN_POINT('Ctrl Pts',(-25.547726543163,21.0211690835444,-31.2627913094226));
#26865=CARTESIAN_POINT('Ctrl Pts',(-25.5660502501383,21.0357052161835,-31.2642248797058));
#26866=CARTESIAN_POINT('Ctrl Pts',(-25.5788706710938,21.0460366636189,-31.2652273123123));
#26867=CARTESIAN_POINT('Ctrl Pts',(-25.6319483017241,21.0894848540732,-31.2693777004017));
#26868=CARTESIAN_POINT('Ctrl Pts',(-25.6714804064031,21.1234794045677,-31.2724694932406));
#26869=CARTESIAN_POINT('Ctrl Pts',(-25.7477148101706,21.1923221139306,-31.2784727668281));
#26870=CARTESIAN_POINT('Ctrl Pts',(-25.784455094727,21.2271047441308,-31.2813860179371));
#26871=CARTESIAN_POINT('Ctrl Pts',(-26.0323249684477,21.4730888533598,-31.3013051740137));
#26872=CARTESIAN_POINT('Ctrl Pts',(-26.2140185972063,21.7118690631205,-31.3174240420115));
#26873=CARTESIAN_POINT('Ctrl Pts',(-26.3706122565698,21.9907215525603,-31.3361418853286));
#26874=CARTESIAN_POINT('Ctrl Pts',(-26.3807970178109,22.0092840906525,-31.3373865927799));
#26875=CARTESIAN_POINT('Ctrl Pts',(-26.3934396085583,22.0328745025783,-31.3389675424852));
#26876=CARTESIAN_POINT('Ctrl Pts',(-26.39606839776,22.0378105019966,-31.3392982867036));
#26877=CARTESIAN_POINT('Ctrl Pts',(-26.4005547620264,22.0462875229302,-31.3398662341788));
#26878=CARTESIAN_POINT('Ctrl Pts',(-26.4024186242787,22.0498252152498,-31.3401032338228));
#26879=CARTESIAN_POINT('Ctrl Pts',(-26.4069810209009,22.0585240640669,-31.3406859521046));
#26880=CARTESIAN_POINT('Ctrl Pts',(-26.4096721510493,22.0636890712292,-31.341031909874));
#26881=CARTESIAN_POINT('Ctrl Pts',(-26.4155028921337,22.074954255483,-31.3417864096778));
#26882=CARTESIAN_POINT('Ctrl Pts',(-26.4186370490116,22.0810572105897,-31.3421951281142));
#26883=CARTESIAN_POINT('Ctrl Pts',(-26.4275684606248,22.098586325928,-31.3433690117569));
#26884=CARTESIAN_POINT('Ctrl Pts',(-26.4333170482685,22.1100370220811,-31.3441357760886));
#26885=CARTESIAN_POINT('Ctrl Pts',(-26.4442730895558,22.13218899199,-31.3456191995758));
#26886=CARTESIAN_POINT('Ctrl Pts',(-26.4494898562437,22.1428854430591,-31.3463355301751));
#26887=CARTESIAN_POINT('Ctrl Pts',(-26.4567367310608,22.1579557210437,-31.347344925897));
#26888=CARTESIAN_POINT('Ctrl Pts',(-26.4588164938705,22.1623056711631,-31.3476363001456));
#26889=CARTESIAN_POINT('Ctrl Pts',(-26.46932465279,22.1844114638629,-31.3491171350276));
#26890=CARTESIAN_POINT('Ctrl Pts',(-26.4776001108408,22.2022391805111,-31.3503117667081));
#26891=CARTESIAN_POINT('Ctrl Pts',(-26.4882558587278,22.225755643396,-31.351888476839));
#26892=CARTESIAN_POINT('Ctrl Pts',(-26.4907837513214,22.2313773661323,-31.3522654619498));
#26893=CARTESIAN_POINT('Ctrl Pts',(-26.4946662090913,22.240078125747,-31.3528490358458));
#26894=CARTESIAN_POINT('Ctrl Pts',(-26.4960321172405,22.2431521105773,-31.3530552346233));
#26895=CARTESIAN_POINT('Ctrl Pts',(-26.4987464359722,22.2492865660927,-31.3534667713633));
#26896=CARTESIAN_POINT('Ctrl Pts',(-26.5000949003736,22.2523470085423,-31.3536721071679));
#26897=CARTESIAN_POINT('Ctrl Pts',(-26.5030791519212,22.2591486683573,-31.3541285072096));
#26898=CARTESIAN_POINT('Ctrl Pts',(-26.5047125956162,22.2628909020463,-31.3543796513159));
#26899=CARTESIAN_POINT('Ctrl Pts',(-26.5094216332757,22.2737355149928,-31.3551075499871));
#26900=CARTESIAN_POINT('Ctrl Pts',(-26.5124787434192,22.2808458456486,-31.3555849354727));
#26901=CARTESIAN_POINT('Ctrl Pts',(-26.5333507493752,22.3298766531758,-31.3588778662293));
#26902=CARTESIAN_POINT('Ctrl Pts',(-26.5503000239454,22.37215789966,-31.3617227125035));
#26903=CARTESIAN_POINT('Ctrl Pts',(-26.5971043802589,22.4964820530526,-31.3701083297386));
#26904=CARTESIAN_POINT('Ctrl Pts',(-26.6245270168094,22.5793907976896,-31.3757273694872));
#26905=CARTESIAN_POINT('Ctrl Pts',(-26.7312608791712,22.9522346532994,-31.4011103371355));
#26906=CARTESIAN_POINT('Ctrl Pts',(-26.773135959949,23.251247164315,-31.4219442594993));
#26907=CARTESIAN_POINT('Ctrl Pts',(-26.7730022123545,23.5516872106683,-31.4417267961338));
#26908=CARTESIAN_POINT('Ctrl Pts',(-26.7730022103292,23.5516917530075,-31.4417270952249));
#26909=CARTESIAN_POINT('Ctrl Pts',(-26.7729671701148,23.6301549043037,-31.4468935140642));
#26910=CARTESIAN_POINT('Ctrl Pts',(-26.7700666504897,23.7085998482106,-31.4519687193417));
#26911=CARTESIAN_POINT('Ctrl Pts',(-26.7639460041217,23.7917389120325,-31.4571986492526));
#26912=CARTESIAN_POINT('Ctrl Pts',(-26.763576417344,23.7966079928911,-31.4575043968517));
#26913=CARTESIAN_POINT('Ctrl Pts',(-26.7629730222354,23.8043249163732,-31.4579880854355));
#26914=CARTESIAN_POINT('Ctrl Pts',(-26.7627464924713,23.8071732959786,-31.4581664275246));
#26915=CARTESIAN_POINT('Ctrl Pts',(-26.7623537222974,23.8120302345219,-31.4584701983748));
#26916=CARTESIAN_POINT('Ctrl Pts',(-26.76218938594,23.8140389391592,-31.4585957336956));
#26917=CARTESIAN_POINT('Ctrl Pts',(-26.7618790954275,23.817788377989,-31.45882987556));
#26918=CARTESIAN_POINT('Ctrl Pts',(-26.7617336101885,23.819529148648,-31.4589385086088));
#26919=CARTESIAN_POINT('Ctrl Pts',(-26.7614280364084,23.823149949312,-31.4591643117892));
#26920=CARTESIAN_POINT('Ctrl Pts',(-26.761267712553,23.8250299523968,-31.4592814677161));
#26921=CARTESIAN_POINT('Ctrl Pts',(-26.7608950755778,23.8293547350151,-31.4595507778698));
#26922=CARTESIAN_POINT('Ctrl Pts',(-26.760681620535,23.8317994196452,-31.4597028671405));
#26923=CARTESIAN_POINT('Ctrl Pts',(-26.7599946254918,23.8395651505979,-31.4601855378776));
#26924=CARTESIAN_POINT('Ctrl Pts',(-26.7595106442483,23.8448852999507,-31.4605155308063));
#26925=CARTESIAN_POINT('Ctrl Pts',(-26.7552520026556,23.8904425048174,-31.463335710523));
#26926=CARTESIAN_POINT('Ctrl Pts',(-26.7507338025173,23.9306087227669,-31.4657847612494));
#26927=CARTESIAN_POINT('Ctrl Pts',(-26.744956905583,23.9745124232755,-31.4684310361837));
#26928=CARTESIAN_POINT('Ctrl Pts',(-26.7444459440973,23.9783424014542,-31.4686616299177));
#26929=CARTESIAN_POINT('Ctrl Pts',(-26.7426260008648,23.9917993437584,-31.4694709675826));
#26930=CARTESIAN_POINT('Ctrl Pts',(-26.7412803627848,24.001421390797,-31.4700480944473));
#26931=CARTESIAN_POINT('Ctrl Pts',(-26.739568855722,24.0132687636727,-31.4707569216899));
#26932=CARTESIAN_POINT('Ctrl Pts',(-26.7392441515003,24.0154998794983,-31.4708903315642));
#26933=CARTESIAN_POINT('Ctrl Pts',(-26.7378330467221,24.0251250139474,-31.4714655400248));
#26934=CARTESIAN_POINT('Ctrl Pts',(-26.736723261678,24.0325156372822,-31.4719063769354));
#26935=CARTESIAN_POINT('Ctrl Pts',(-26.7340278152987,24.0500504125977,-31.4729504517365));
#26936=CARTESIAN_POINT('Ctrl Pts',(-26.7324193588308,24.060191024947,-31.473552790028));
#26937=CARTESIAN_POINT('Ctrl Pts',(-26.7287638285546,24.0825465157908,-31.474877777624));
#26938=CARTESIAN_POINT('Ctrl Pts',(-26.726694741267,24.0947576704901,-31.4755996082634));
#26939=CARTESIAN_POINT('Ctrl Pts',(-26.6708967325278,24.4129154496872,-31.4943637072343));
#26940=CARTESIAN_POINT('Ctrl Pts',(-26.5732867784656,24.7095217629079,-31.5109806629215));
#26941=CARTESIAN_POINT('Ctrl Pts',(-26.3998230380398,25.0576306333022,-31.5334894702754));
#26942=CARTESIAN_POINT('Ctrl Pts',(-26.3623861692889,25.1263692166543,-31.5380859597871));
#26943=CARTESIAN_POINT('Ctrl Pts',(-26.302231018629,25.2278430109924,-31.5451480538195));
#26944=CARTESIAN_POINT('Ctrl Pts',(-26.2813457101815,25.2616336242055,-31.547547838486));
#26945=CARTESIAN_POINT('Ctrl Pts',(-26.2558069777853,25.3012945775034,-31.5504254386768));
#26946=CARTESIAN_POINT('Ctrl Pts',(-26.2517503749817,25.3075466186917,-31.5508808803033));
#26947=CARTESIAN_POINT('Ctrl Pts',(-26.2454713079989,25.3171507987376,-31.5515833526639));
#26948=CARTESIAN_POINT('Ctrl Pts',(-26.2432641755925,25.3205129712401,-31.5518298078829));
#26949=CARTESIAN_POINT('Ctrl Pts',(-26.2392290095888,25.3266348163798,-31.552279539537));
#26950=CARTESIAN_POINT('Ctrl Pts',(-26.2374030043203,25.3293958247852,-31.5524827394345));
#26951=CARTESIAN_POINT('Ctrl Pts',(-26.2336966534207,25.334981284565,-31.5528945542364));
#26952=CARTESIAN_POINT('Ctrl Pts',(-26.2318160948289,25.3378055889431,-31.5531031770062));
#26953=CARTESIAN_POINT('Ctrl Pts',(-26.2264259250756,25.3458731319475,-31.5537002141623));
#26954=CARTESIAN_POINT('Ctrl Pts',(-26.2229053862977,25.3511090194161,-31.5540890415846));
#26955=CARTESIAN_POINT('Ctrl Pts',(-26.2076811182781,25.373608193274,-31.5557657151199));
#26956=CARTESIAN_POINT('Ctrl Pts',(-26.1958255408818,25.3907676719544,-31.5570593220089));
#26957=CARTESIAN_POINT('Ctrl Pts',(-25.9783852742474,25.6990434990484,-31.5805739475404));
#26958=CARTESIAN_POINT('Ctrl Pts',(-25.7261111862444,25.9541309542022,-31.6049071370198));
#26959=CARTESIAN_POINT('Ctrl Pts',(-25.3912798682883,26.1959979080524,-31.6326461065456));
#26960=CARTESIAN_POINT('Ctrl Pts',(-25.3443152646014,26.2280668805358,-31.636439443643));
#26961=CARTESIAN_POINT('Ctrl Pts',(-25.2482199101226,26.2900203305189,-31.6439750669341));
#26962=CARTESIAN_POINT('Ctrl Pts',(-25.1990870411787,26.3198673881172,-31.6477150910901));
#26963=CARTESIAN_POINT('Ctrl Pts',(-25.1334960367396,26.3573477978747,-31.6525365582984));
#26964=CARTESIAN_POINT('Ctrl Pts',(-25.1177375760591,26.3661776904649,-31.6536822439895));
#26965=CARTESIAN_POINT('Ctrl Pts',(-25.0954066340541,26.3784447704623,-31.6552870626515));
#26966=CARTESIAN_POINT('Ctrl Pts',(-25.088895592973,26.3819922923328,-31.6557527560709));
#26967=CARTESIAN_POINT('Ctrl Pts',(-25.0775080763461,26.3881458759834,-31.6565632799256));
#26968=CARTESIAN_POINT('Ctrl Pts',(-25.0726370612939,26.3907619010414,-31.6569087251532));
#26969=CARTESIAN_POINT('Ctrl Pts',(-25.0655463515619,26.3945465555632,-31.6574097366201));
#26970=CARTESIAN_POINT('Ctrl Pts',(-25.0633320207231,26.3957251312335,-31.6575659338356));
#26971=CARTESIAN_POINT('Ctrl Pts',(-25.0595494071545,26.3977327600747,-31.6578323069753));
#26972=CARTESIAN_POINT('Ctrl Pts',(-25.057981814435,26.3985631045279,-31.6579425658475));
#26973=CARTESIAN_POINT('Ctrl Pts',(-25.0548613333531,26.4002127066934,-31.6581617864368));
#26974=CARTESIAN_POINT('Ctrl Pts',(-25.0533084629692,26.4010319887212,-31.6582707497144));
#26975=CARTESIAN_POINT('Ctrl Pts',(-25.0496445403041,26.4029612191554,-31.65852754045));
#26976=CARTESIAN_POINT('Ctrl Pts',(-25.0475329203326,26.404070095745,-31.6586752991903));
#26977=CARTESIAN_POINT('Ctrl Pts',(-25.0412799644029,26.4073448646553,-31.6591121494404));
#26978=CARTESIAN_POINT('Ctrl Pts',(-25.0371351231144,26.4095041058193,-31.6594008195763));
#26979=CARTESIAN_POINT('Ctrl Pts',(-25.0005370548299,26.4284686443872,-31.6619419082835));
#26980=CARTESIAN_POINT('Ctrl Pts',(-24.9678031840086,26.4447306564743,-31.6641606311909));
#26981=CARTESIAN_POINT('Ctrl Pts',(-24.9250026665692,26.4650934017123,-31.667001268736));
#26982=CARTESIAN_POINT('Ctrl Pts',(-24.9151836461309,26.4697042422017,-31.6676488799276));
#26983=CARTESIAN_POINT('Ctrl Pts',(-24.9041223353676,26.4748304367094,-31.6683740683415));
#26984=CARTESIAN_POINT('Ctrl Pts',(-24.902902913269,26.4753946330368,-31.6684539552863));
#26985=CARTESIAN_POINT('Ctrl Pts',(-24.8949734676219,26.4790573719504,-31.668973046763));
#26986=CARTESIAN_POINT('Ctrl Pts',(-24.888253100853,26.4821336115829,-31.6694112031724));
#26987=CARTESIAN_POINT('Ctrl Pts',(-24.8779851799299,26.4867910826827,-31.6700780242888));
#26988=CARTESIAN_POINT('Ctrl Pts',(-24.8744452929799,26.4883890461963,-31.6703074369775));
#26989=CARTESIAN_POINT('Ctrl Pts',(-24.8674443493263,26.4915341656879,-31.6707602315558));
#26990=CARTESIAN_POINT('Ctrl Pts',(-24.8639834350638,26.4930816209663,-31.670983626237));
#26991=CARTESIAN_POINT('Ctrl Pts',(-24.7185394613715,26.5578052961059,-31.6803534140283));
#26992=CARTESIAN_POINT('Ctrl Pts',(-24.5721613300134,26.6106412801705,-31.6890580758463));
#26993=CARTESIAN_POINT('Ctrl Pts',(-24.4056671135617,26.657452284008,-31.6987258234761));
#26994=CARTESIAN_POINT('Ctrl Pts',(-24.3887655649884,26.6620559158255,-31.6997045351701));
#26995=CARTESIAN_POINT('Ctrl Pts',(-24.3523996410172,26.6716434469892,-31.7018059127665));
#26996=CARTESIAN_POINT('Ctrl Pts',(-24.3329245163827,26.6765835752178,-31.7029285479905));
#26997=CARTESIAN_POINT('Ctrl Pts',(-24.2906526495927,26.686886655365,-31.7053613799287));
#26998=CARTESIAN_POINT('Ctrl Pts',(-24.2678411222388,26.6921838751518,-31.7066717832037));
#26999=CARTESIAN_POINT('Ctrl Pts',(-24.2176883076366,26.7032555190323,-31.7095504538854));
#27000=CARTESIAN_POINT('Ctrl Pts',(-24.190325665609,26.7089238841405,-31.7111194988788));
#27001=CARTESIAN_POINT('Ctrl Pts',(-24.0695755187937,26.7323046739457,-31.7180466004763));
#27002=CARTESIAN_POINT('Ctrl Pts',(-23.9755090541764,26.7462355450478,-31.7234524754065));
#27003=CARTESIAN_POINT('Ctrl Pts',(-23.7841016460363,26.7659818857433,-31.7346167739771));
#27004=CARTESIAN_POINT('Ctrl Pts',(-23.6868396602599,26.771578627305,-31.7403748797362));
#27005=CARTESIAN_POINT('Ctrl Pts',(-23.5719807043389,26.7729768019354,-31.7473348747763));
#27006=CARTESIAN_POINT('Ctrl Pts',(-23.5544801755576,26.7730472728566,-31.7483996454995));
#27007=CARTESIAN_POINT('Ctrl Pts',(-23.5313158936095,26.7729518740491,-31.7498149800078));
#27008=CARTESIAN_POINT('Ctrl Pts',(-23.5256516816213,26.7729136130064,-31.7501615347802));
#27009=CARTESIAN_POINT('Ctrl Pts',(-23.516361776207,26.7728263674901,-31.7507307057313));
#27010=CARTESIAN_POINT('Ctrl Pts',(-23.5127359959132,26.7727861963494,-31.7509530448978));
#27011=CARTESIAN_POINT('Ctrl Pts',(-23.5057173616474,26.7726965878503,-31.7513838222347));
#27012=CARTESIAN_POINT('Ctrl Pts',(-23.5023245013513,26.7726479109414,-31.7515922362406));
#27013=CARTESIAN_POINT('Ctrl Pts',(-23.4945014558309,26.7725233167755,-31.7520731860221));
#27014=CARTESIAN_POINT('Ctrl Pts',(-23.4900713451068,26.7724436215143,-31.752345840088));
#27015=CARTESIAN_POINT('Ctrl Pts',(-23.4762851409093,26.7721671741008,-31.7531952538741));
#27016=CARTESIAN_POINT('Ctrl Pts',(-23.4669297932438,26.7719388069461,-31.7537730052068));
#27017=CARTESIAN_POINT('Ctrl Pts',(-23.3875781151358,26.7696559402467,-31.7586850076445));
#27018=CARTESIAN_POINT('Ctrl Pts',(-23.3176696867381,26.7653614335192,-31.7630892655988));
#27019=CARTESIAN_POINT('Ctrl Pts',(-23.2394771357738,26.7579945454056,-31.7681075218243));
#27020=CARTESIAN_POINT('Ctrl Pts',(-23.2309967787604,26.7571616253986,-31.7686529859288));
#27021=CARTESIAN_POINT('Ctrl Pts',(-23.167436973454,26.7506643245458,-31.7727502982384));
#27022=CARTESIAN_POINT('Ctrl Pts',(-23.1125110255552,26.7436152119414,-31.7763424882658));
#27023=CARTESIAN_POINT('Ctrl Pts',(-22.8633872303512,26.7050951771669,-31.7928643244734));
#27024=CARTESIAN_POINT('Ctrl Pts',(-22.6721543961242,26.6573002418126,-31.8062188117439));
#27025=CARTESIAN_POINT('Ctrl Pts',(-22.3835125292605,26.5563691939994,-31.8268870325203));
#27026=CARTESIAN_POINT('Ctrl Pts',(-22.2824186403182,26.5151504775598,-31.8342215566646));
#27027=CARTESIAN_POINT('Ctrl Pts',(-22.147086342378,26.4517811304981,-31.8440175553199));
#27028=CARTESIAN_POINT('Ctrl Pts',(-22.1108903054392,26.4339966676922,-31.8466349789575));
#27029=CARTESIAN_POINT('Ctrl Pts',(-22.0750360153402,26.4155367745532,-31.8492183260801));
#27030=CARTESIAN_POINT('Ctrl Pts',(-22.0750360188393,26.4155367763548,-32.0936416103654));
#27031=CARTESIAN_POINT('Ctrl Pts',(-22.099508153078,26.4281364675027,-32.0917876278781));
#27032=CARTESIAN_POINT('Ctrl Pts',(-22.1241485350163,26.4404261539109,-32.0899290872953));
#27033=CARTESIAN_POINT('Ctrl Pts',(-22.3021405079941,26.5263694585511,-32.0765701184169));
#27034=CARTESIAN_POINT('Ctrl Pts',(-22.4609515178144,26.5880945217143,-32.0649839042452));
#27035=CARTESIAN_POINT('Ctrl Pts',(-22.672592506279,26.6516095084807,-32.0504662776571));
#27036=CARTESIAN_POINT('Ctrl Pts',(-22.7216285051253,26.6650695515949,-32.0471658601115));
#27037=CARTESIAN_POINT('Ctrl Pts',(-22.7971629712594,26.6838930052114,-32.0421987407113));
#27038=CARTESIAN_POINT('Ctrl Pts',(-22.8234427352679,26.6900923589496,-32.0404919919648));
#27039=CARTESIAN_POINT('Ctrl Pts',(-22.8540807623507,26.6969145215607,-32.0385294665726));
#27040=CARTESIAN_POINT('Ctrl Pts',(-22.8583651546385,26.6978593478192,-32.0382556466428));
#27041=CARTESIAN_POINT('Ctrl Pts',(-22.8648880253284,26.6992838583967,-32.0378397169844));
#27042=CARTESIAN_POINT('Ctrl Pts',(-22.8671250856603,26.6997699067365,-32.0376972417929));
#27043=CARTESIAN_POINT('Ctrl Pts',(-22.8711853150902,26.7006475474158,-32.0374389633542));
#27044=CARTESIAN_POINT('Ctrl Pts',(-22.8730083001809,26.7010399397377,-32.0373231141769));
#27045=CARTESIAN_POINT('Ctrl Pts',(-22.8769584286894,26.7018866069624,-32.0370723342303));
#27046=CARTESIAN_POINT('Ctrl Pts',(-22.8790856858302,26.7023403094398,-32.0369374370961));
#27047=CARTESIAN_POINT('Ctrl Pts',(-22.8848882932016,26.7035717520788,-32.0365698912813));
#27048=CARTESIAN_POINT('Ctrl Pts',(-22.8885645612441,26.7043452230422,-32.0363374888414));
#27049=CARTESIAN_POINT('Ctrl Pts',(-22.9062194276443,26.7080275054709,-32.0352235627163));
#27050=CARTESIAN_POINT('Ctrl Pts',(-22.9202161845924,26.7108498871461,-32.0343469421178));
#27051=CARTESIAN_POINT('Ctrl Pts',(-22.9432036681648,26.7153264315599,-32.0329171872676));
#27052=CARTESIAN_POINT('Ctrl Pts',(-22.9521833053234,26.7170354922394,-32.0323611644874));
#27053=CARTESIAN_POINT('Ctrl Pts',(-22.9661359248567,26.7196295781824,-32.0315008964205));
#27054=CARTESIAN_POINT('Ctrl Pts',(-22.9711038374556,26.7205411406121,-32.0311953167347));
#27055=CARTESIAN_POINT('Ctrl Pts',(-22.9811219353428,26.722355027642,-32.0305805178028));
#27056=CARTESIAN_POINT('Ctrl Pts',(-22.9861721747632,26.7232569805009,-32.0302713175148));
#27057=CARTESIAN_POINT('Ctrl Pts',(-23.3006925612394,26.7786544411731,-32.0110588758788));
#27058=CARTESIAN_POINT('Ctrl Pts',(-23.6165153703464,26.7876180436505,-31.9942836676612));
#27059=CARTESIAN_POINT('Ctrl Pts',(-24.0051908355359,26.7416604620454,-31.9720327086367));
#27060=CARTESIAN_POINT('Ctrl Pts',(-24.0813495013313,26.7298733216919,-31.9676034726495));
#27061=CARTESIAN_POINT('Ctrl Pts',(-24.2364518921627,26.7001399949314,-31.9583694496124));
#27062=CARTESIAN_POINT('Ctrl Pts',(-24.3152870336579,26.6819263847318,-31.9535602268042));
#27063=CARTESIAN_POINT('Ctrl Pts',(-24.4083988206492,26.6566886966496,-31.9477081244511));
#27064=CARTESIAN_POINT('Ctrl Pts',(-24.4234186455926,26.6525003658251,-31.9467587520726));
#27065=CARTESIAN_POINT('Ctrl Pts',(-24.4423168605814,26.6470824167095,-31.9455572709253));
#27066=CARTESIAN_POINT('Ctrl Pts',(-24.4462243005283,26.645954179594,-31.9453084733732));
#27067=CARTESIAN_POINT('Ctrl Pts',(-24.4532285327579,26.643917400355,-31.9448618148281));
#27068=CARTESIAN_POINT('Ctrl Pts',(-24.4563261209214,26.6430115958419,-31.9446640434848));
#27069=CARTESIAN_POINT('Ctrl Pts',(-24.4625755027005,26.6411739414436,-31.9442645556436));
#27070=CARTESIAN_POINT('Ctrl Pts',(-24.4657272415048,26.6402419200644,-31.9440628337363));
#27071=CARTESIAN_POINT('Ctrl Pts',(-24.4720409092905,26.6383643563047,-31.9436582362708));
#27072=CARTESIAN_POINT('Ctrl Pts',(-24.4752028225904,26.6374187749689,-31.9434553596357));
#27073=CARTESIAN_POINT('Ctrl Pts',(-24.4837471465164,26.6348492596578,-31.9429064477829));
#27074=CARTESIAN_POINT('Ctrl Pts',(-24.4891267509622,26.6332161010247,-31.9425601102259));
#27075=CARTESIAN_POINT('Ctrl Pts',(-24.5102331235181,26.6267481894661,-31.9411983733315));
#27076=CARTESIAN_POINT('Ctrl Pts',(-24.5259268319407,26.6218071726948,-31.9401794866225));
#27077=CARTESIAN_POINT('Ctrl Pts',(-24.7960124758728,26.534494488316,-31.9225326301285));
#27078=CARTESIAN_POINT('Ctrl Pts',(-25.0391605311647,26.4209161073131,-31.9047925280574));
#27079=CARTESIAN_POINT('Ctrl Pts',(-25.3342556629352,26.2354074398297,-31.881212746759));
#27080=CARTESIAN_POINT('Ctrl Pts',(-25.4014077988599,26.1895608608288,-31.8757019961106));
#27081=CARTESIAN_POINT('Ctrl Pts',(-25.5892536727295,26.0506141001433,-31.8599698365334));
#27082=CARTESIAN_POINT('Ctrl Pts',(-25.7051902539378,25.9514168619256,-31.8498567385606));
#27083=CARTESIAN_POINT('Ctrl Pts',(-25.8177666183684,25.8403464848335,-31.8399519287678));
#27084=CARTESIAN_POINT('Ctrl Pts',(-25.8218380447533,25.8363080221709,-31.8395935993931));
#27085=CARTESIAN_POINT('Ctrl Pts',(-25.8277071462057,25.8304552779514,-31.8390769213745));
#27086=CARTESIAN_POINT('Ctrl Pts',(-25.8295134483037,25.8286497225553,-31.8389178877137));
#27087=CARTESIAN_POINT('Ctrl Pts',(-25.8326569320553,25.8255000589626,-31.8386410945821));
#27088=CARTESIAN_POINT('Ctrl Pts',(-25.8339950754361,25.8241569164711,-31.8385232579414));
#27089=CARTESIAN_POINT('Ctrl Pts',(-25.8365871690197,25.8215505431322,-31.838294982161));
#27090=CARTESIAN_POINT('Ctrl Pts',(-25.8378412546809,25.8202874576588,-31.8381845319204));
#27091=CARTESIAN_POINT('Ctrl Pts',(-25.8408383405488,25.8172638576927,-31.837920551206));
#27092=CARTESIAN_POINT('Ctrl Pts',(-25.8425803616032,25.8155023678608,-31.8377670989777));
#27093=CARTESIAN_POINT('Ctrl Pts',(-25.8488228842705,25.8091755037698,-31.8372171365467));
#27094=CARTESIAN_POINT('Ctrl Pts',(-25.8533118314653,25.8045986725801,-31.8368215374142));
#27095=CARTESIAN_POINT('Ctrl Pts',(-25.9204921765884,25.7356929876222,-31.8308986482986));
#27096=CARTESIAN_POINT('Ctrl Pts',(-25.9804878180238,25.6687769911317,-31.825576660699));
#27097=CARTESIAN_POINT('Ctrl Pts',(-26.2272038826552,25.3693051862334,-31.8030981683612));
#27098=CARTESIAN_POINT('Ctrl Pts',(-26.3839477802576,25.1139725137947,-31.787094809092));
#27099=CARTESIAN_POINT('Ctrl Pts',(-26.5364078101719,24.7650802226755,-31.7651202686616));
#27100=CARTESIAN_POINT('Ctrl Pts',(-26.5665370044784,24.6882138758409,-31.7602836583404));
#27101=CARTESIAN_POINT('Ctrl Pts',(-26.6076296514555,24.5702334173207,-31.7528145787027));
#27102=CARTESIAN_POINT('Ctrl Pts',(-26.6207856268887,24.5299168157773,-31.7502546265053));
#27103=CARTESIAN_POINT('Ctrl Pts',(-26.6353538752722,24.4820920501767,-31.7472052100246));
#27104=CARTESIAN_POINT('Ctrl Pts',(-26.6375402435065,24.4748225784133,-31.7467413507094));
#27105=CARTESIAN_POINT('Ctrl Pts',(-26.6408541345635,24.4636613729258,-31.7460286169164));
#27106=CARTESIAN_POINT('Ctrl Pts',(-26.6420000463417,24.459775090144,-31.7457803448455));
#27107=CARTESIAN_POINT('Ctrl Pts',(-26.643986948663,24.4529894994882,-31.7453466723294));
#27108=CARTESIAN_POINT('Ctrl Pts',(-26.6448312017001,24.4500911454493,-31.7451613788289));
#27109=CARTESIAN_POINT('Ctrl Pts',(-26.6465891875138,24.4440241755646,-31.7447733919892));
#27110=CARTESIAN_POINT('Ctrl Pts',(-26.6475021312051,24.4408553364066,-31.7445706731151));
#27111=CARTESIAN_POINT('Ctrl Pts',(-26.6500170264353,24.4320754672165,-31.7440088067331));
#27112=CARTESIAN_POINT('Ctrl Pts',(-26.6516085989866,24.4264614997047,-31.7436493209781));
#27113=CARTESIAN_POINT('Ctrl Pts',(-26.6578179067946,24.4043304783406,-31.7422312874853));
#27114=CARTESIAN_POINT('Ctrl Pts',(-26.6623189449261,24.3877812301906,-31.741168946694));
#27115=CARTESIAN_POINT('Ctrl Pts',(-26.7375347627839,24.1022501202929,-31.7228040984325));
#27116=CARTESIAN_POINT('Ctrl Pts',(-26.7732536883996,23.8253238402451,-31.7042898690192));
#27117=CARTESIAN_POINT('Ctrl Pts',(-26.7729665957051,23.5092218944626,-31.6828951409107));
#27118=CARTESIAN_POINT('Ctrl Pts',(-26.7722562232377,23.4711217833702,-31.6803149608563));
#27119=CARTESIAN_POINT('Ctrl Pts',(-26.7644303207503,23.2560857020112,-31.6657657622672));
#27120=CARTESIAN_POINT('Ctrl Pts',(-26.7434157378901,23.0799352991948,-31.6538820381171));
#27121=CARTESIAN_POINT('Ctrl Pts',(-26.7058780190909,22.8958358037867,-31.6420498464673));
#27122=CARTESIAN_POINT('Ctrl Pts',(-26.7036742033385,22.8852974662144,-31.6413746745486));
#27123=CARTESIAN_POINT('Ctrl Pts',(-26.7007030161701,22.8714367023745,-31.6404896323586));
#27124=CARTESIAN_POINT('Ctrl Pts',(-26.6999831573655,22.8681043284166,-31.6402770805511));
#27125=CARTESIAN_POINT('Ctrl Pts',(-26.6988607096658,22.8629479463126,-31.6399485462579));
#27126=CARTESIAN_POINT('Ctrl Pts',(-26.698461823381,22.8611231481565,-31.6398323506808));
#27127=CARTESIAN_POINT('Ctrl Pts',(-26.697661010985,22.857474851877,-31.6396001833679));
#27128=CARTESIAN_POINT('Ctrl Pts',(-26.6972590890948,22.8556513678103,-31.6394842127192));
#27129=CARTESIAN_POINT('Ctrl Pts',(-26.6963524134703,22.851554801634,-31.6392238358332));
#27130=CARTESIAN_POINT('Ctrl Pts',(-26.6958467820369,22.8492819214714,-31.6390794812575));
#27131=CARTESIAN_POINT('Ctrl Pts',(-26.6943403469148,22.8425447501263,-31.6386519102628));
#27132=CARTESIAN_POINT('Ctrl Pts',(-26.6933324942288,22.8380820158505,-31.6383691000201));
#27133=CARTESIAN_POINT('Ctrl Pts',(-26.6852159230003,22.8024949834775,-31.6361170968028));
#27134=CARTESIAN_POINT('Ctrl Pts',(-26.677654249942,22.7714743239807,-31.6341736065395));
#27135=CARTESIAN_POINT('Ctrl Pts',(-26.6494075755702,22.6626513238917,-31.6274082600648));
#27136=CARTESIAN_POINT('Ctrl Pts',(-26.626268577755,22.5855114800766,-31.6227076184188));
#27137=CARTESIAN_POINT('Ctrl Pts',(-26.4754428656927,22.1435836564873,-31.5959084979339));
#27138=CARTESIAN_POINT('Ctrl Pts',(-26.2858780751226,21.8032999665366,-31.5753607361601));
#27139=CARTESIAN_POINT('Ctrl Pts',(-26.0278316041391,21.4891553492079,-31.550770459468));
#27140=CARTESIAN_POINT('Ctrl Pts',(-26.014959557988,21.4737798248807,-31.5495518380616));
#27141=CARTESIAN_POINT('Ctrl Pts',(-25.9979124874068,21.453799120331,-31.5479479241696));
#27142=CARTESIAN_POINT('Ctrl Pts',(-25.9938662510642,21.4490842484604,-31.5475679472693));
#27143=CARTESIAN_POINT('Ctrl Pts',(-25.9876018397336,21.4418272198131,-31.5469807632382));
#27144=CARTESIAN_POINT('Ctrl Pts',(-25.9853932489911,21.4392767781608,-31.5467739540099));
#27145=CARTESIAN_POINT('Ctrl Pts',(-25.9809878159776,21.4342055755476,-31.5463618491365));
#27146=CARTESIAN_POINT('Ctrl Pts',(-25.9787910473817,21.431684755916,-31.5461565567016));
#27147=CARTESIAN_POINT('Ctrl Pts',(-25.9739136021094,21.426105380699,-31.5457011974784));
#27148=CARTESIAN_POINT('Ctrl Pts',(-25.9712310540105,21.4230484752933,-31.5454510526797));
#27149=CARTESIAN_POINT('Ctrl Pts',(-25.9634774421054,21.4142464886248,-31.5447288893735));
#27150=CARTESIAN_POINT('Ctrl Pts',(-25.958391690382,21.4085144349542,-31.544256255268));
#27151=CARTESIAN_POINT('Ctrl Pts',(-25.9240405623118,21.3700749731657,-31.5410708341378));
#27152=CARTESIAN_POINT('Ctrl Pts',(-25.8941313316755,21.3379515429586,-31.5383308851528));
#27153=CARTESIAN_POINT('Ctrl Pts',(-25.8124474623153,21.2537367921335,-31.5309310567334));
#27154=CARTESIAN_POINT('Ctrl Pts',(-25.7595351166022,21.2027901733812,-31.5262224063497));
#27155=CARTESIAN_POINT('Ctrl Pts',(-25.5931411847298,21.0531897174514,-31.5116626298826));
#27156=CARTESIAN_POINT('Ctrl Pts',(-25.4744656083958,20.9606362568154,-31.501598282119));
#27157=CARTESIAN_POINT('Ctrl Pts',(-25.1540162765927,20.7449462415519,-31.4754912088065));
#27158=CARTESIAN_POINT('Ctrl Pts',(-24.944357773292,20.635069194381,-31.4593569162729));
#27159=CARTESIAN_POINT('Ctrl Pts',(-24.7120466367349,20.5441699177788,-31.443607863754));
#27160=CARTESIAN_POINT('Ctrl Pts',(-24.6994988870679,20.5393504984236,-31.4427636179599));
#27161=CARTESIAN_POINT('Ctrl Pts',(-24.6834846601421,20.5333143499677,-31.4416946078555));
#27162=CARTESIAN_POINT('Ctrl Pts',(-24.6800459954441,20.5320249427118,-31.4414655593854));
#27163=CARTESIAN_POINT('Ctrl Pts',(-24.6745855759095,20.5299880707178,-31.4411026366636));
#27164=CARTESIAN_POINT('Ctrl Pts',(-24.6725652755543,20.5292367565639,-31.4409685312059));
#27165=CARTESIAN_POINT('Ctrl Pts',(-24.6688288471521,20.5278515100017,-31.4407208313979));
#27166=CARTESIAN_POINT('Ctrl Pts',(-24.6671129441123,20.5272170160854,-31.4406072037327));
#27167=CARTESIAN_POINT('Ctrl Pts',(-24.6632865415761,20.5258058198558,-31.4403540960606));
#27168=CARTESIAN_POINT('Ctrl Pts',(-24.6611757737163,20.5250298671101,-31.4402146617738));
#27169=CARTESIAN_POINT('Ctrl Pts',(-24.656778072143,20.5234184234391,-31.4399245441745));
#27170=CARTESIAN_POINT('Ctrl Pts',(-24.6544909991105,20.5225833130157,-31.4397738837476));
#27171=CARTESIAN_POINT('Ctrl Pts',(-24.6485724780854,20.5204298003499,-31.4393845618823));
#27172=CARTESIAN_POINT('Ctrl Pts',(-24.6449395886151,20.5191153299518,-31.4391461337008));
#27173=CARTESIAN_POINT('Ctrl Pts',(-24.6342978316785,20.5152865029144,-31.4384492782468));
#27174=CARTESIAN_POINT('Ctrl Pts',(-24.6272825454265,20.5127898800189,-31.4379918836948));
#27175=CARTESIAN_POINT('Ctrl Pts',(-24.5533416179106,20.4867639152512,-31.4331912368279));
#27176=CARTESIAN_POINT('Ctrl Pts',(-24.4856592661558,20.4654241404961,-31.4289714742513));
#27177=CARTESIAN_POINT('Ctrl Pts',(-24.3413968316429,20.4251248968509,-31.4202339904514));
#27178=CARTESIAN_POINT('Ctrl Pts',(-24.2647146840019,20.4067072037797,-31.4157380672096));
#27179=CARTESIAN_POINT('Ctrl Pts',(-23.8541433891334,20.3238974740217,-31.3920938532711));
#27180=CARTESIAN_POINT('Ctrl Pts',(-23.5123593490702,20.3098401169598,-31.3736219133235));
#27181=CARTESIAN_POINT('Ctrl Pts',(-23.1549569878328,20.3517757514882,-31.3518531529117));
#27182=CARTESIAN_POINT('Ctrl Pts',(-23.1352470274782,20.3542733883821,-31.3506456799688));
#27183=CARTESIAN_POINT('Ctrl Pts',(-23.1094278848446,20.3577880424927,-31.3490543967694));
#27184=CARTESIAN_POINT('Ctrl Pts',(-23.1032964649168,20.3586406885014,-31.3486757982039));
#27185=CARTESIAN_POINT('Ctrl Pts',(-23.0938317763761,20.3599846732642,-31.3480902739741));
#27186=CARTESIAN_POINT('Ctrl Pts',(-23.0904967344325,20.3604635855156,-31.3478837425613));
#27187=CARTESIAN_POINT('Ctrl Pts',(-23.0838530841978,20.3614282498084,-31.3474718914821));
#27188=CARTESIAN_POINT('Ctrl Pts',(-23.0805444686026,20.3619139234685,-31.347266574539));
#27189=CARTESIAN_POINT('Ctrl Pts',(-23.0732061684528,20.3630027874709,-31.3468107253183));
#27190=CARTESIAN_POINT('Ctrl Pts',(-23.0691768647877,20.3636084713698,-31.3465601141707));
#27191=CARTESIAN_POINT('Ctrl Pts',(-23.0575379845299,20.3653806027337,-31.3458352954368));
#27192=CARTESIAN_POINT('Ctrl Pts',(-23.0499314639139,20.3665666715071,-31.345360465199));
#27193=CARTESIAN_POINT('Ctrl Pts',(-22.9982436229178,20.3748160605633,-31.3421261273462));
#27194=CARTESIAN_POINT('Ctrl Pts',(-22.9543107943938,20.3827671347366,-31.3393384952434));
#27195=CARTESIAN_POINT('Ctrl Pts',(-22.9007946020738,20.393605384121,-31.3358932618598));
#27196=CARTESIAN_POINT('Ctrl Pts',(-22.8910395103731,20.3956281474638,-31.3352632347512));
#27197=CARTESIAN_POINT('Ctrl Pts',(-22.7562148393406,20.4242373445125,-31.3265275360768));
#27198=CARTESIAN_POINT('Ctrl Pts',(-22.632840817412,20.4581956537457,-31.3181915046303));
#27199=CARTESIAN_POINT('Ctrl Pts',(-22.210310530093,20.6020134004645,-31.288508791225));
#27200=CARTESIAN_POINT('Ctrl Pts',(-21.9256952333279,20.7487587908881,-31.2662788654909));
#27201=CARTESIAN_POINT('Ctrl Pts',(-21.6542858115567,20.9441669564894,-31.2451184715937));
#27202=CARTESIAN_POINT('Ctrl Pts',(-21.6414141517445,20.9535800661338,-31.2441155302391));
#27203=CARTESIAN_POINT('Ctrl Pts',(-21.6257506293052,20.9652142921887,-31.2428963222445));
#27204=CARTESIAN_POINT('Ctrl Pts',(-21.6228921940158,20.9673447902036,-31.2426738812911));
#27205=CARTESIAN_POINT('Ctrl Pts',(-21.6181804980262,20.9708687689621,-31.2423073157127));
#27206=CARTESIAN_POINT('Ctrl Pts',(-21.6163252057177,20.972259506754,-31.2421629999459));
#27207=CARTESIAN_POINT('Ctrl Pts',(-21.6130126149994,20.97474823216,-31.2419053725884));
#27208=CARTESIAN_POINT('Ctrl Pts',(-21.6115547515364,20.9758454525745,-31.2417920074192));
#27209=CARTESIAN_POINT('Ctrl Pts',(-21.6084271104004,20.9782035481762,-31.2415488331755));
#27210=CARTESIAN_POINT('Ctrl Pts',(-21.6067576331428,20.9794648081037,-31.2414190522702));
#27211=CARTESIAN_POINT('Ctrl Pts',(-21.6033227858814,20.9820650313965,-31.2411520766157));
#27212=CARTESIAN_POINT('Ctrl Pts',(-21.6015575653926,20.9834041917648,-31.2410148958836));
#27213=CARTESIAN_POINT('Ctrl Pts',(-21.5971337313606,20.9867674664976,-31.2406711577194));
#27214=CARTESIAN_POINT('Ctrl Pts',(-21.594476874384,20.9887939030586,-31.2404647630279));
#27215=CARTESIAN_POINT('Ctrl Pts',(-21.5869862659899,20.994525584977,-31.2398829814991));
#27216=CARTESIAN_POINT('Ctrl Pts',(-21.5821598278555,20.998240430091,-31.2395082592389));
#27217=CARTESIAN_POINT('Ctrl Pts',(-21.5375901287719,21.0327467719972,-31.2360488699788));
#27218=CARTESIAN_POINT('Ctrl Pts',(-21.4985593411228,21.0644526761777,-31.2330266140962));
#27219=CARTESIAN_POINT('Ctrl Pts',(-21.4103840409328,21.1395726183558,-31.226173877576));
#27220=CARTESIAN_POINT('Ctrl Pts',(-21.3617898444017,21.1835994364965,-31.2223782813598));
#27221=CARTESIAN_POINT('Ctrl Pts',(-21.1000448549493,21.4357042791965,-31.2016080923626));
#27222=CARTESIAN_POINT('Ctrl Pts',(-20.9152016390504,21.6710633347323,-31.1855464329415));
#27223=CARTESIAN_POINT('Ctrl Pts',(-20.7191388197885,22.0077453333449,-31.162798688452));
#27224=CARTESIAN_POINT('Ctrl Pts',(-20.6763836762828,22.0889487800925,-31.1573411403017));
#27225=CARTESIAN_POINT('Ctrl Pts',(-20.6332280755213,22.1801539651271,-31.1511987777575));
#27226=CARTESIAN_POINT('Ctrl Pts',(-20.6293389435296,22.1884648948877,-31.1506389702535));
#27227=CARTESIAN_POINT('Ctrl Pts',(-20.6236027006337,22.2008606592959,-31.1498038352257));
#27228=CARTESIAN_POINT('Ctrl Pts',(-20.621728510578,22.2049329724979,-31.1495294438701));
#27229=CARTESIAN_POINT('Ctrl Pts',(-20.6185280839479,22.2119253628992,-31.149058243651));
#27230=CARTESIAN_POINT('Ctrl Pts',(-20.6171976944573,22.2148435419469,-31.1488615782981));
#27231=CARTESIAN_POINT('Ctrl Pts',(-20.6146125865771,22.220536415976,-31.148477883503));
#27232=CARTESIAN_POINT('Ctrl Pts',(-20.6133574404032,22.2233109133766,-31.1482908690904));
#27233=CARTESIAN_POINT('Ctrl Pts',(-20.6103562353584,22.2299701870663,-31.147841962428));
#27234=CARTESIAN_POINT('Ctrl Pts',(-20.6086139450114,22.2338566460266,-31.1475799409189));
#27235=CARTESIAN_POINT('Ctrl Pts',(-20.6033817501196,22.2455901558354,-31.1467887737845));
#27236=CARTESIAN_POINT('Ctrl Pts',(-20.5999155239155,22.2534476672209,-31.1462588164598));
#27237=CARTESIAN_POINT('Ctrl Pts',(-20.5682748950425,22.3259565941175,-31.1413669215099));
#27238=CARTESIAN_POINT('Ctrl Pts',(-20.5422002916347,22.3914981919462,-31.1369337551516));
#27239=CARTESIAN_POINT('Ctrl Pts',(-20.4787304662932,22.5676563085786,-31.1249744274318));
#27240=CARTESIAN_POINT('Ctrl Pts',(-20.4451626688475,22.679531529205,-31.1173310898589));
#27241=CARTESIAN_POINT('Ctrl Pts',(-20.3531744804519,23.060042885716,-31.0912524807817));
#27242=CARTESIAN_POINT('Ctrl Pts',(-20.3230315876301,23.3342594172357,-31.0722239809687));
#27243=CARTESIAN_POINT('Ctrl Pts',(-20.3289571149693,23.6594370364511,-31.051135404293));
#27244=CARTESIAN_POINT('Ctrl Pts',(-20.3310623846339,23.7098800000633,-31.0479099357925));
#27245=CARTESIAN_POINT('Ctrl Pts',(-20.3346852960567,23.7653596522754,-31.044428020615));
#27246=CARTESIAN_POINT('Ctrl Pts',(-20.3350307202184,23.7704624862737,-31.0441083786154));
#27247=CARTESIAN_POINT('Ctrl Pts',(-20.335562804414,23.7780545300027,-31.0436337463751));
#27248=CARTESIAN_POINT('Ctrl Pts',(-20.3357402090904,23.7805443488446,-31.0434782397668));
#27249=CARTESIAN_POINT('Ctrl Pts',(-20.3360494333168,23.7848142311195,-31.043211815167));
#27250=CARTESIAN_POINT('Ctrl Pts',(-20.3361798389581,23.7865943906608,-31.0431008172558));
#27251=CARTESIAN_POINT('Ctrl Pts',(-20.3364487973374,23.7902245324426,-31.0428746268244));
#27252=CARTESIAN_POINT('Ctrl Pts',(-20.3365874682379,23.7920744993528,-31.0427594417227));
#27253=CARTESIAN_POINT('Ctrl Pts',(-20.336913973075,23.7963804194966,-31.0424915356239));
#27254=CARTESIAN_POINT('Ctrl Pts',(-20.3371030257961,23.7988362848051,-31.042338883861));
#27255=CARTESIAN_POINT('Ctrl Pts',(-20.3375076276058,23.8040146290227,-31.0420173146262));
#27256=CARTESIAN_POINT('Ctrl Pts',(-20.3377238222434,23.8067370572855,-31.0418484336281));
#27257=CARTESIAN_POINT('Ctrl Pts',(-20.3383114561585,23.8140195150221,-31.0413971495107));
#27258=CARTESIAN_POINT('Ctrl Pts',(-20.3386891473511,23.818579055089,-31.0411150942539));
#27259=CARTESIAN_POINT('Ctrl Pts',(-20.3398712056426,23.8324889194978,-31.0402560870281));
#27260=CARTESIAN_POINT('Ctrl Pts',(-20.3407067156359,23.8418366480163,-31.0396808340372));
#27261=CARTESIAN_POINT('Ctrl Pts',(-20.3439057351248,23.8759464335914,-31.0375886768354));
#27262=CARTESIAN_POINT('Ctrl Pts',(-20.3465151394298,23.9006852692491,-31.0360846485061));
#27263=CARTESIAN_POINT('Ctrl Pts',(-20.3614725686483,24.0283080230706,-31.028383288618));
#27264=CARTESIAN_POINT('Ctrl Pts',(-20.3784920495251,24.1305922333574,-31.0224039191853));
#27265=CARTESIAN_POINT('Ctrl Pts',(-20.4758542060815,24.5805036920593,-30.9962779180317));
#27266=CARTESIAN_POINT('Ctrl Pts',(-20.6086304496797,24.9141463597551,-30.9770522312961));
#27267=CARTESIAN_POINT('Ctrl Pts',(-20.8041219539098,25.2370591183088,-30.9542295987389));
#27268=CARTESIAN_POINT('Ctrl Pts',(-20.8150582393367,25.2547353748124,-30.9529667279983));
#27269=CARTESIAN_POINT('Ctrl Pts',(-20.8295315910889,25.2776305539875,-30.9513127713045));
#27270=CARTESIAN_POINT('Ctrl Pts',(-20.8329142233263,25.2829469033408,-30.9509274235007));
#27271=CARTESIAN_POINT('Ctrl Pts',(-20.8381414640695,25.2911093960815,-30.9503337719367));
#27272=CARTESIAN_POINT('Ctrl Pts',(-20.8399750233767,25.2939626260578,-30.950125880445));
#27273=CARTESIAN_POINT('Ctrl Pts',(-20.8436071932945,25.2995951322218,-30.949714734929));
#27274=CARTESIAN_POINT('Ctrl Pts',(-20.8454055893282,25.3023745423272,-30.9495114890991));
#27275=CARTESIAN_POINT('Ctrl Pts',(-20.8493998811444,25.3085268906114,-30.9490607889974));
#27276=CARTESIAN_POINT('Ctrl Pts',(-20.8515978166765,25.3118984921771,-30.9488132584748));
#27277=CARTESIAN_POINT('Ctrl Pts',(-20.8578906809884,25.3215122417096,-30.9481059077528));
#27278=CARTESIAN_POINT('Ctrl Pts',(-20.8620009715116,25.327744259701,-30.9476455105892));
#27279=CARTESIAN_POINT('Ctrl Pts',(-20.8882461781951,25.3672379558742,-30.9447159278817));
#27280=CARTESIAN_POINT('Ctrl Pts',(-20.9109755451346,25.4000986372219,-30.942224329423));
#27281=CARTESIAN_POINT('Ctrl Pts',(-20.9803170051858,25.4964678571596,-30.9347507268733));
#27282=CARTESIAN_POINT('Ctrl Pts',(-21.0286502156223,25.5586953994385,-30.9297032613071));
#27283=CARTESIAN_POINT('Ctrl Pts',(-21.1117901697997,25.6579988339002,-30.9212725220757));
#27284=CARTESIAN_POINT('Ctrl Pts',(-21.145282527071,25.6961351128577,-30.9179372410419));
#27285=CARTESIAN_POINT('Ctrl Pts',(-21.2054707436818,25.7614891919763,-30.9120515975798));
#27286=CARTESIAN_POINT('Ctrl Pts',(-21.231775711509,25.7890545112767,-30.9095132581886));
#27287=CARTESIAN_POINT('Ctrl Pts',(-21.4649912632757,26.0249251064988,-30.8873144693889));
#27288=CARTESIAN_POINT('Ctrl Pts',(-21.6989790627461,26.2045159984836,-30.866934320563));
#27289=CARTESIAN_POINT('Ctrl Pts',(-21.9679152640053,26.3578459892651,-30.8473466964458));
#27290=CARTESIAN_POINT('Ctrl Pts',(-21.9818381270953,26.3656474475507,-30.8463429150488));
#27291=CARTESIAN_POINT('Ctrl Pts',(-21.9989425455034,26.3750653761334,-30.8451228128778));
#27292=CARTESIAN_POINT('Ctrl Pts',(-22.0020692552626,26.3767802287538,-30.8449003072546));
#27293=CARTESIAN_POINT('Ctrl Pts',(-22.007233933754,26.379601670035,-30.8445336570458));
#27294=CARTESIAN_POINT('Ctrl Pts',(-22.0092702507424,26.3807112489488,-30.8443893211667));
#27295=CARTESIAN_POINT('Ctrl Pts',(-22.0128516768031,26.3826577395739,-30.8441358662157));
#27296=CARTESIAN_POINT('Ctrl Pts',(-22.014396269705,26.383495583888,-30.844026687041));
#27297=CARTESIAN_POINT('Ctrl Pts',(-22.0177623447085,26.3853179059365,-30.8437890415365));
#27298=CARTESIAN_POINT('Ctrl Pts',(-22.0195840863143,26.3863018894825,-30.8436606073366));
#27299=CARTESIAN_POINT('Ctrl Pts',(-22.0244495363387,26.3889238280697,-30.8433180690589));
#27300=CARTESIAN_POINT('Ctrl Pts',(-22.0274949444745,26.3905586490577,-30.8431041662688));
#27301=CARTESIAN_POINT('Ctrl Pts',(-22.0342064433436,26.3941475858544,-30.8426338534958));
#27302=CARTESIAN_POINT('Ctrl Pts',(-22.0378737014702,26.3960995225607,-30.8423775812223));
#27303=CARTESIAN_POINT('Ctrl Pts',(-22.0488140436608,26.4018955147988,-30.8416151501708));
#27304=CARTESIAN_POINT('Ctrl Pts',(-22.0560981499387,26.4057188549625,-30.841110272455));
#27305=CARTESIAN_POINT('Ctrl Pts',(-22.0672725156933,26.4115296795246,-30.8403398323904));
#27306=CARTESIAN_POINT('Ctrl Pts',(-22.0711522263205,26.413537171993,-30.8400730875419));
#27307=CARTESIAN_POINT('Ctrl Pts',(-22.0750360153473,26.4155367745569,-30.8398067994259));
#27308=CARTESIAN_POINT('Origin',(-23.5502525316942,23.5502525316942,-77.3107734492734));
#27309=CARTESIAN_POINT('',(-22.0750360135777,26.4155367736458,-29.3439103255379));
#27310=CARTESIAN_POINT('',(-22.0750360153461,26.4155367745563,-29.5927618641105));
#27311=CARTESIAN_POINT('',(-22.0750360153461,26.4155367745563,-77.3107734492734));
#27312=CARTESIAN_POINT('Ctrl Pts',(-22.0750360135777,26.4155367736458,-29.3439103255379));
#27313=CARTESIAN_POINT('Ctrl Pts',(-22.0178680196052,26.3861033346239,-29.3476546934872));
#27314=CARTESIAN_POINT('Ctrl Pts',(-21.9615946141282,26.3549660488702,-29.3514478427651));
#27315=CARTESIAN_POINT('Ctrl Pts',(-21.8847349755201,26.3093822712396,-29.3568014974043));
#27316=CARTESIAN_POINT('Ctrl Pts',(-21.8633295656043,26.2963473047052,-29.3583116634764));
#27317=CARTESIAN_POINT('Ctrl Pts',(-21.8326932487767,26.2771977414827,-29.3605019039041));
#27318=CARTESIAN_POINT('Ctrl Pts',(-21.8233380687557,26.2712829432223,-29.3611746482961));
#27319=CARTESIAN_POINT('Ctrl Pts',(-21.8067732576553,26.2606900322315,-29.3623729386914));
#27320=CARTESIAN_POINT('Ctrl Pts',(-21.7995514877892,26.2560310288995,-29.3628977725897));
#27321=CARTESIAN_POINT('Ctrl Pts',(-21.7887921416467,26.2490287101577,-29.3636833449846));
#27322=CARTESIAN_POINT('Ctrl Pts',(-21.7852403766333,26.246707177959,-29.3639432671455));
#27323=CARTESIAN_POINT('Ctrl Pts',(-21.7789872810581,26.2426023328506,-29.3644019340346));
#27324=CARTESIAN_POINT('Ctrl Pts',(-21.7762840274648,26.2408219483375,-29.364600568507));
#27325=CARTESIAN_POINT('Ctrl Pts',(-21.7708981957186,26.237263151053,-29.3649970187144));
#27326=CARTESIAN_POINT('Ctrl Pts',(-21.7682155900993,26.2354847861122,-29.3651948325027));
#27327=CARTESIAN_POINT('Ctrl Pts',(-21.761767325518,26.231196155021,-29.3656711635234));
#27328=CARTESIAN_POINT('Ctrl Pts',(-21.7580042887569,26.2286819743959,-29.3659498284372));
#27329=CARTESIAN_POINT('Ctrl Pts',(-21.7464831292812,26.2209492436591,-29.3668051362848));
#27330=CARTESIAN_POINT('Ctrl Pts',(-21.7387424626994,26.2157048856773,-29.3673827563272));
#27331=CARTESIAN_POINT('Ctrl Pts',(-21.7101508074189,26.1961517571963,-29.3695274202732));
#27332=CARTESIAN_POINT('Ctrl Pts',(-21.6894460663366,26.1816316960969,-29.3711025028214));
#27333=CARTESIAN_POINT('Ctrl Pts',(-21.6640209969043,26.1633511693042,-29.3730646011676));
#27334=CARTESIAN_POINT('Ctrl Pts',(-21.6591370896011,26.1598188321732,-29.3734427924499));
#27335=CARTESIAN_POINT('Ctrl Pts',(-21.648714880122,26.1522362363972,-29.3742526237282));
#27336=CARTESIAN_POINT('Ctrl Pts',(-21.6431795531629,26.1481819559223,-29.37468441725));
#27337=CARTESIAN_POINT('Ctrl Pts',(-21.6363407950832,26.1431393595879,-29.3752199848165));
#27338=CARTESIAN_POINT('Ctrl Pts',(-21.6350250815671,26.1421676638052,-29.375323119516));
#27339=CARTESIAN_POINT('Ctrl Pts',(-21.6314837665997,26.1395481226425,-29.3756009723261));
#27340=CARTESIAN_POINT('Ctrl Pts',(-21.6292595520746,26.1378984122934,-29.3757757620028));
#27341=CARTESIAN_POINT('Ctrl Pts',(-21.6215065602348,26.1321324767796,-29.3763859985233));
#27342=CARTESIAN_POINT('Ctrl Pts',(-21.6159888937043,26.128001404417,-29.3768220143343));
#27343=CARTESIAN_POINT('Ctrl Pts',(-21.6075922613752,26.1216727140609,-29.3774881687768));
#27344=CARTESIAN_POINT('Ctrl Pts',(-21.6047036525534,26.1194878729702,-29.377717817731));
#27345=CARTESIAN_POINT('Ctrl Pts',(-21.5985003974116,26.1147794908042,-29.3782120175689));
#27346=CARTESIAN_POINT('Ctrl Pts',(-21.5951869518569,26.1122543849245,-29.3784766279318));
#27347=CARTESIAN_POINT('Ctrl Pts',(-21.5802653414545,26.1008371416732,-29.379671133859));
#27348=CARTESIAN_POINT('Ctrl Pts',(-21.5687130228502,26.0918725949951,-29.3806037805596));
#27349=CARTESIAN_POINT('Ctrl Pts',(-21.5237318913766,26.0564743641618,-29.384266207618));
#27350=CARTESIAN_POINT('Ctrl Pts',(-21.4907688772662,26.0294581693593,-29.3870177915576));
#27351=CARTESIAN_POINT('Ctrl Pts',(-21.2445470582561,25.8193573905688,-29.4080911069868));
#27352=CARTESIAN_POINT('Ctrl Pts',(-21.0555397480742,25.6097386112236,-29.4274458762233));
#27353=CARTESIAN_POINT('Ctrl Pts',(-20.8373662174436,25.2929815670697,-29.4530975145878));
#27354=CARTESIAN_POINT('Ctrl Pts',(-20.7827271599645,25.2048415278285,-29.4598936185849));
#27355=CARTESIAN_POINT('Ctrl Pts',(-20.7256455166144,25.1019960620047,-29.4673212103159));
#27356=CARTESIAN_POINT('Ctrl Pts',(-20.7189445487789,25.0897355281373,-29.4681988265762));
#27357=CARTESIAN_POINT('Ctrl Pts',(-20.7106204621924,25.0742670284856,-29.4692958628696));
#27358=CARTESIAN_POINT('Ctrl Pts',(-20.7089228237139,25.0710996533412,-29.4695199599921));
#27359=CARTESIAN_POINT('Ctrl Pts',(-20.7062338593202,25.0660624908859,-29.4698754899475));
#27360=CARTESIAN_POINT('Ctrl Pts',(-20.7052390775139,25.0641945671737,-29.4700071435581));
#27361=CARTESIAN_POINT('Ctrl Pts',(-20.7033683078661,25.0606734263678,-29.4702549637882));
#27362=CARTESIAN_POINT('Ctrl Pts',(-20.702491926048,25.0590204382652,-29.4703711550892));
#27363=CARTESIAN_POINT('Ctrl Pts',(-20.7005081999307,25.0552709460492,-29.4706343809338));
#27364=CARTESIAN_POINT('Ctrl Pts',(-20.699401731423,25.0531739862772,-29.4707813589195));
#27365=CARTESIAN_POINT('Ctrl Pts',(-20.696141954228,25.0469795609016,-29.4712148445495));
#27366=CARTESIAN_POINT('Ctrl Pts',(-20.6939951463143,25.0428786528182,-29.4715009385304));
#27367=CARTESIAN_POINT('Ctrl Pts',(-20.6797915815371,25.0156036493566,-29.4733979461197));
#27368=CARTESIAN_POINT('Ctrl Pts',(-20.6680076885269,24.9922874595808,-29.4749918691834));
#27369=CARTESIAN_POINT('Ctrl Pts',(-20.6536477416588,24.9629947168081,-29.4769631282619));
#27370=CARTESIAN_POINT('Ctrl Pts',(-20.6508049473055,24.9571510703622,-29.477354839241));
#27371=CARTESIAN_POINT('Ctrl Pts',(-20.6440280852471,24.9431127748106,-29.4782922640567));
#27372=CARTESIAN_POINT('Ctrl Pts',(-20.6401109531268,24.9349099573782,-29.4788370940603));
#27373=CARTESIAN_POINT('Ctrl Pts',(-20.5485036108483,24.7409702492367,-29.491652241233));
#27374=CARTESIAN_POINT('Ctrl Pts',(-20.4787227531851,24.5472639593954,-29.5030407899759));
#27375=CARTESIAN_POINT('Ctrl Pts',(-20.3847622922454,24.1795985552876,-29.524248206233));
#27376=CARTESIAN_POINT('Ctrl Pts',(-20.3554027693371,24.0077815706142,-29.5340068344254));
#27377=CARTESIAN_POINT('Ctrl Pts',(-20.3345864680789,23.7726456518554,-29.5477977963679));
#27378=CARTESIAN_POINT('Ctrl Pts',(-20.3309013420733,23.7107022381336,-29.5514690400063));
#27379=CARTESIAN_POINT('Ctrl Pts',(-20.3283426521953,23.626975527394,-29.5565006900676));
#27380=CARTESIAN_POINT('Ctrl Pts',(-20.3278986134397,23.6052514403914,-29.5578124777193));
#27381=CARTESIAN_POINT('Ctrl Pts',(-20.3275715248233,23.5735714598629,-29.5597351966069));
#27382=CARTESIAN_POINT('Ctrl Pts',(-20.3275148733939,23.5636176640317,-29.5603407145013));
#27383=CARTESIAN_POINT('Ctrl Pts',(-20.3274959959025,23.5457836877933,-29.5614281862632));
#27384=CARTESIAN_POINT('Ctrl Pts',(-20.3275165572314,23.5379035755246,-29.5619095984465));
#27385=CARTESIAN_POINT('Ctrl Pts',(-20.3275917209395,23.5259291449268,-29.562642538152));
#27386=CARTESIAN_POINT('Ctrl Pts',(-20.3276252255884,23.5218346849459,-29.5628934030969));
#27387=CARTESIAN_POINT('Ctrl Pts',(-20.3276971372912,23.5147068521127,-29.5633305569627));
#27388=CARTESIAN_POINT('Ctrl Pts',(-20.3277320245295,23.5116734423643,-29.5635167351411));
#27389=CARTESIAN_POINT('Ctrl Pts',(-20.3278130012697,23.5054025759249,-29.5639019011689));
#27390=CARTESIAN_POINT('Ctrl Pts',(-20.327859686684,23.5021651313347,-29.5641009075339));
#27391=CARTESIAN_POINT('Ctrl Pts',(-20.3279844528735,23.4943318896531,-29.5645828024794));
#27392=CARTESIAN_POINT('Ctrl Pts',(-20.328067487074,23.4897361877984,-29.5648658463594));
#27393=CARTESIAN_POINT('Ctrl Pts',(-20.3284119160133,23.472691946768,-29.5659167782128));
#27394=CARTESIAN_POINT('Ctrl Pts',(-20.328735619331,23.4602449011797,-29.5666866204059));
#27395=CARTESIAN_POINT('Ctrl Pts',(-20.3355574378041,23.2457656474243,-29.5799937603329));
#27396=CARTESIAN_POINT('Ctrl Pts',(-20.3609750653052,23.0448238380425,-29.5931434484847));
#27397=CARTESIAN_POINT('Ctrl Pts',(-20.4695336815122,22.5588805452749,-29.6264839085009));
#27398=CARTESIAN_POINT('Ctrl Pts',(-20.5734868528602,22.2804003586288,-29.6470235236238));
#27399=CARTESIAN_POINT('Ctrl Pts',(-20.7198542289663,22.0091112912566,-29.6664610660877));
#27400=CARTESIAN_POINT('Ctrl Pts',(-20.7257963594688,21.9982479511263,-29.6672381357626));
#27401=CARTESIAN_POINT('Ctrl Pts',(-20.7334716707122,21.984406111499,-29.6682263614525));
#27402=CARTESIAN_POINT('Ctrl Pts',(-20.7351471143684,21.9813959671733,-29.668441152554));
#27403=CARTESIAN_POINT('Ctrl Pts',(-20.7378433631286,21.976570044646,-29.6687853172609));
#27404=CARTESIAN_POINT('Ctrl Pts',(-20.7388611017096,21.974752570113,-29.6689148880571));
#27405=CARTESIAN_POINT('Ctrl Pts',(-20.7407994797359,21.9712988794009,-29.6691610219957));
#27406=CARTESIAN_POINT('Ctrl Pts',(-20.7417197800179,21.9696624931244,-29.6692776054535));
#27407=CARTESIAN_POINT('Ctrl Pts',(-20.7438336168351,21.9659115543129,-29.6695447561175));
#27408=CARTESIAN_POINT('Ctrl Pts',(-20.7450281120055,21.9637975485434,-29.669695260203));
#27409=CARTESIAN_POINT('Ctrl Pts',(-20.7487242609105,21.9572733672647,-29.6701595612308));
#27410=CARTESIAN_POINT('Ctrl Pts',(-20.7512339494578,21.9528677166186,-29.6704728399794));
#27411=CARTESIAN_POINT('Ctrl Pts',(-20.770526498855,21.9191855432891,-29.6728661176289));
#27412=CARTESIAN_POINT('Ctrl Pts',(-20.7877586611584,21.8901669393629,-29.6749175545129));
#27413=CARTESIAN_POINT('Ctrl Pts',(-20.8093909820106,21.8550085227891,-29.6773968778175));
#27414=CARTESIAN_POINT('Ctrl Pts',(-20.8133601924533,21.8486078537924,-29.6778479909058));
#27415=CARTESIAN_POINT('Ctrl Pts',(-20.8181976230589,21.8408678220982,-29.6783932675793));
#27416=CARTESIAN_POINT('Ctrl Pts',(-20.819044410989,21.8395151729472,-29.678488551549));
#27417=CARTESIAN_POINT('Ctrl Pts',(-20.8233726044137,21.8326127718551,-29.6789747325476));
#27418=CARTESIAN_POINT('Ctrl Pts',(-20.8268699477001,21.8270729749063,-29.679364800089));
#27419=CARTESIAN_POINT('Ctrl Pts',(-20.8318244887076,21.8192777348539,-29.6799135416402));
#27420=CARTESIAN_POINT('Ctrl Pts',(-20.8332676266793,21.8170134257934,-29.6800729201709));
#27421=CARTESIAN_POINT('Ctrl Pts',(-20.8403392056938,21.8059485279323,-29.6808516821647));
#27422=CARTESIAN_POINT('Ctrl Pts',(-20.846007644706,21.797173443852,-29.6814690798452));
#27423=CARTESIAN_POINT('Ctrl Pts',(-20.9285584498409,21.6707329957657,-29.6903645643389));
#27424=CARTESIAN_POINT('Ctrl Pts',(-21.013022656774,21.5581819596051,-29.6982795084682));
#27425=CARTESIAN_POINT('Ctrl Pts',(-21.2408970703335,21.2926398740057,-29.7178652504914));
#27426=CARTESIAN_POINT('Ctrl Pts',(-21.3923631804421,21.1474532628132,-29.7294602028303));
#27427=CARTESIAN_POINT('Ctrl Pts',(-21.6272380310684,20.9625583051563,-29.7468655659453));
#27428=CARTESIAN_POINT('Ctrl Pts',(-21.6999182033129,20.9100997314028,-29.7521774371936));
#27429=CARTESIAN_POINT('Ctrl Pts',(-21.7839123618448,20.8546482895322,-29.7582790555064));
#27430=CARTESIAN_POINT('Ctrl Pts',(-21.7931713010991,20.8486038923756,-29.7589511416509));
#27431=CARTESIAN_POINT('Ctrl Pts',(-21.809680239358,20.8379473332529,-29.760148670272));
#27432=CARTESIAN_POINT('Ctrl Pts',(-21.816917956813,20.8333162711962,-29.7606734037356));
#27433=CARTESIAN_POINT('Ctrl Pts',(-21.8277546186596,20.8264433461016,-29.7614586800626));
#27434=CARTESIAN_POINT('Ctrl Pts',(-21.8313396483493,20.8241795247618,-29.7617184066143));
#27435=CARTESIAN_POINT('Ctrl Pts',(-21.8376702830193,20.8201994025288,-29.7621769409948));
#27436=CARTESIAN_POINT('Ctrl Pts',(-21.8404140321721,20.8184801487952,-29.7623756390624));
#27437=CARTESIAN_POINT('Ctrl Pts',(-21.8458915249443,20.8150593959817,-29.7627722440192));
#27438=CARTESIAN_POINT('Ctrl Pts',(-21.8486252371749,20.8133578531583,-29.7629701490033));
#27439=CARTESIAN_POINT('Ctrl Pts',(-21.8552118826738,20.8092718145734,-29.7634469072589));
#27440=CARTESIAN_POINT('Ctrl Pts',(-21.8590672961273,20.806891346554,-29.7637259087937));
#27441=CARTESIAN_POINT('Ctrl Pts',(-21.8709126337061,20.7996120777616,-29.7645829255367));
#27442=CARTESIAN_POINT('Ctrl Pts',(-21.8789188640216,20.7947400261683,-29.7651619231961));
#27443=CARTESIAN_POINT('Ctrl Pts',(-21.9724172570428,20.7384006129698,-29.7719208478736));
#27444=CARTESIAN_POINT('Ctrl Pts',(-22.0602255887921,20.6909009412967,-29.7782445824907));
#27445=CARTESIAN_POINT('Ctrl Pts',(-22.3819606330559,20.5357067558023,-29.8013675934019));
#27446=CARTESIAN_POINT('Ctrl Pts',(-22.6263770501641,20.4520579569957,-29.8189404587776));
#27447=CARTESIAN_POINT('Ctrl Pts',(-22.9533205482786,20.382334018617,-29.8414493446333));
#27448=CARTESIAN_POINT('Ctrl Pts',(-23.0291113477924,20.3689872783488,-29.8465917825679));
#27449=CARTESIAN_POINT('Ctrl Pts',(-23.1572388236527,20.3511266032592,-29.8550899336988));
#27450=CARTESIAN_POINT('Ctrl Pts',(-23.2093391404665,20.345155772925,-29.8584916769161));
#27451=CARTESIAN_POINT('Ctrl Pts',(-23.2866758290401,20.3382001449357,-29.8634397232182));
#27452=CARTESIAN_POINT('Ctrl Pts',(-23.3118131919861,20.3362363539057,-29.8650322106239));
#27453=CARTESIAN_POINT('Ctrl Pts',(-23.3412706070281,20.334282588203,-29.8668778505859));
#27454=CARTESIAN_POINT('Ctrl Pts',(-23.3455698655681,20.334006096954,-29.8671467070072));
#27455=CARTESIAN_POINT('Ctrl Pts',(-23.3521377209585,20.3335969318248,-29.8675566367083));
#27456=CARTESIAN_POINT('Ctrl Pts',(-23.3544059038064,20.3334580364201,-29.8676980595864));
#27457=CARTESIAN_POINT('Ctrl Pts',(-23.3585172869121,20.3332106346201,-29.8679541427334));
#27458=CARTESIAN_POINT('Ctrl Pts',(-23.3603604268506,20.3331013135838,-29.8680688486836));
#27459=CARTESIAN_POINT('Ctrl Pts',(-23.3643819693845,20.3328662543343,-29.8683189145969));
#27460=CARTESIAN_POINT('Ctrl Pts',(-23.3665604002292,20.3327411448328,-29.8684542383228));
#27461=CARTESIAN_POINT('Ctrl Pts',(-23.3725198130563,20.3324049617285,-29.8688240719535));
#27462=CARTESIAN_POINT('Ctrl Pts',(-23.3763010579012,20.3321983388747,-29.8690583304702));
#27463=CARTESIAN_POINT('Ctrl Pts',(-23.3946494961498,20.331228138621,-29.8701931602841));
#27464=CARTESIAN_POINT('Ctrl Pts',(-23.4092216979807,20.3305567897318,-29.8710886048444));
#27465=CARTESIAN_POINT('Ctrl Pts',(-23.4325845243015,20.3296393727334,-29.8725155990318));
#27466=CARTESIAN_POINT('Ctrl Pts',(-23.4413722550516,20.3293303083371,-29.8730503965846));
#27467=CARTESIAN_POINT('Ctrl Pts',(-23.4552246608118,20.3288998764988,-29.8738904909778));
#27468=CARTESIAN_POINT('Ctrl Pts',(-23.4602884691847,20.32875448055,-29.8741969752191));
#27469=CARTESIAN_POINT('Ctrl Pts',(-23.4692961088083,20.3285171015429,-29.8747410953382));
#27470=CARTESIAN_POINT('Ctrl Pts',(-23.4732397926475,20.3284204189589,-29.8749789573932));
#27471=CARTESIAN_POINT('Ctrl Pts',(-23.5803222991823,20.3259919310898,-29.8814280122492));
#27472=CARTESIAN_POINT('Ctrl Pts',(-23.6835242716581,20.3286064585765,-29.8874025397333));
#27473=CARTESIAN_POINT('Ctrl Pts',(-24.0285862726569,20.353962550305,-29.9070860077399));
#27474=CARTESIAN_POINT('Ctrl Pts',(-24.2679519370511,20.3990644558192,-29.9203144092884));
#27475=CARTESIAN_POINT('Ctrl Pts',(-24.5505743434249,20.4862231225292,-29.9372986458494));
#27476=CARTESIAN_POINT('Ctrl Pts',(-24.6007670061799,20.5030671259447,-29.9403667958796));
#27477=CARTESIAN_POINT('Ctrl Pts',(-24.7210768166272,20.5467673770786,-29.9478724683544));
#27478=CARTESIAN_POINT('Ctrl Pts',(-24.7907115036365,20.5748512547966,-29.9523441954129));
#27479=CARTESIAN_POINT('Ctrl Pts',(-24.868407917047,20.6093881481318,-29.9575042744246));
#27480=CARTESIAN_POINT('Ctrl Pts',(-24.8774985147824,20.6134796362641,-29.9581106953332));
#27481=CARTESIAN_POINT('Ctrl Pts',(-24.8937548436343,20.6208871665473,-29.9592000183315));
#27482=CARTESIAN_POINT('Ctrl Pts',(-24.9009276764422,20.6241875022867,-29.9596823779508));
#27483=CARTESIAN_POINT('Ctrl Pts',(-24.9118019608451,20.6292394398509,-29.9604162867224));
#27484=CARTESIAN_POINT('Ctrl Pts',(-24.9155123577214,20.6309718089936,-29.9606671697497));
#27485=CARTESIAN_POINT('Ctrl Pts',(-24.921965761614,20.6339998711249,-29.9611043425421));
#27486=CARTESIAN_POINT('Ctrl Pts',(-24.9247102655843,20.6352923770674,-29.9612905215306));
#27487=CARTESIAN_POINT('Ctrl Pts',(-24.9303801549335,20.6379723616087,-29.9616756857563));
#27488=CARTESIAN_POINT('Ctrl Pts',(-24.9333052816768,20.6393603770194,-29.9618746895022));
#27489=CARTESIAN_POINT('Ctrl Pts',(-24.9412253582447,20.643133202324,-29.9624143161514));
#27490=CARTESIAN_POINT('Ctrl Pts',(-24.9462162471045,20.6455264681822,-29.9627552331826));
#27491=CARTESIAN_POINT('Ctrl Pts',(-24.9647861974285,20.6544901738789,-29.9640269622098));
#27492=CARTESIAN_POINT('Ctrl Pts',(-24.9783250739995,20.6611429931159,-29.9649606468073));
#27493=CARTESIAN_POINT('Ctrl Pts',(-25.0089915469142,20.676480304755,-29.9670905329614));
#27494=CARTESIAN_POINT('Ctrl Pts',(-25.0260891053785,20.6852232632828,-29.9682887668945));
#27495=CARTESIAN_POINT('Ctrl Pts',(-25.0464773044485,20.6958798418967,-29.969730731327));
#27496=CARTESIAN_POINT('Ctrl Pts',(-25.0498442633546,20.6976472906906,-29.9699692921683));
#27497=CARTESIAN_POINT('Ctrl Pts',(-25.0572871008995,20.7015711467992,-29.970497600275));
#27498=CARTESIAN_POINT('Ctrl Pts',(-25.0613614899503,20.7037303481606,-29.9707874454732));
#27499=CARTESIAN_POINT('Ctrl Pts',(-25.0711318546157,20.7089349910903,-29.9714840264801));
#27500=CARTESIAN_POINT('Ctrl Pts',(-25.0768233194982,20.7119888176816,-29.9718910560287));
#27501=CARTESIAN_POINT('Ctrl Pts',(-25.0841663774437,20.7159573035311,-29.9724178296406));
#27502=CARTESIAN_POINT('Ctrl Pts',(-25.085826430652,20.7168563491271,-29.9725370258026));
#27503=CARTESIAN_POINT('Ctrl Pts',(-25.0935890551594,20.7210692289107,-29.9730949078344));
#27504=CARTESIAN_POINT('Ctrl Pts',(-25.0996816595853,20.7244013038612,-29.9735342314657));
#27505=CARTESIAN_POINT('Ctrl Pts',(-25.1100426696915,20.7301113717904,-29.974283841551));
#27506=CARTESIAN_POINT('Ctrl Pts',(-25.1143165425432,20.7324794382877,-29.9745937808011));
#27507=CARTESIAN_POINT('Ctrl Pts',(-25.1220899392833,20.7368096544886,-29.9751588337431));
#27508=CARTESIAN_POINT('Ctrl Pts',(-25.1255912220107,20.7387686406224,-29.9754138371047));
#27509=CARTESIAN_POINT('Ctrl Pts',(-25.133468711454,20.7431954727536,-29.9759886783919));
#27510=CARTESIAN_POINT('Ctrl Pts',(-25.137842816619,20.7456670202929,-29.9763086439246));
#27511=CARTESIAN_POINT('Ctrl Pts',(-25.1573788527386,20.7567660240735,-29.9777411800791));
#27512=CARTESIAN_POINT('Ctrl Pts',(-25.172476144904,20.7655061500406,-29.9788576187743));
#27513=CARTESIAN_POINT('Ctrl Pts',(-25.2071090662918,20.7859330518737,-29.981440477589));
#27514=CARTESIAN_POINT('Ctrl Pts',(-25.2265931529087,20.7977050126855,-29.9829097270072));
#27515=CARTESIAN_POINT('Ctrl Pts',(-25.3325497949153,20.8632645283129,-29.9909884532556));
#27516=CARTESIAN_POINT('Ctrl Pts',(-25.4165538316109,20.9209171537859,-29.9977228300741));
#27517=CARTESIAN_POINT('Ctrl Pts',(-25.555793132434,21.0265164871294,-30.0094254298211));
#27518=CARTESIAN_POINT('Ctrl Pts',(-25.6123897533205,21.0725466813383,-30.0143486467559));
#27519=CARTESIAN_POINT('Ctrl Pts',(-25.7843945942848,21.2224173576041,-30.0297844763344));
#27520=CARTESIAN_POINT('Ctrl Pts',(-25.8939017044282,21.3327041494442,-30.0403263721104));
#27521=CARTESIAN_POINT('Ctrl Pts',(-26.0396786864498,21.5024319866593,-30.0550241421539));
#27522=CARTESIAN_POINT('Ctrl Pts',(-26.0826536977781,21.5558209040924,-30.0594523360189));
#27523=CARTESIAN_POINT('Ctrl Pts',(-26.1305212028653,21.619332474965,-30.0644608289943));
#27524=CARTESIAN_POINT('Ctrl Pts',(-26.1371001740058,21.6281552488437,-30.0651509600491));
#27525=CARTESIAN_POINT('Ctrl Pts',(-26.1455936015387,21.6396680164257,-30.0660440282673));
#27526=CARTESIAN_POINT('Ctrl Pts',(-26.1475491984386,21.6423273539272,-30.0662498027954));
#27527=CARTESIAN_POINT('Ctrl Pts',(-26.1507131027957,21.6466436994435,-30.0665829521676));
#27528=CARTESIAN_POINT('Ctrl Pts',(-26.1519239142178,21.648298855736,-30.0667105023748));
#27529=CARTESIAN_POINT('Ctrl Pts',(-26.1542454935481,21.6514787758734,-30.0669551688019));
#27530=CARTESIAN_POINT('Ctrl Pts',(-26.1553564992659,21.6530033547712,-30.0670723014382));
#27531=CARTESIAN_POINT('Ctrl Pts',(-26.157908217494,21.6565114203862,-30.0673414352144));
#27532=CARTESIAN_POINT('Ctrl Pts',(-26.1593480094013,21.6584955809613,-30.0674933716782));
#27533=CARTESIAN_POINT('Ctrl Pts',(-26.163798106624,21.6646429526951,-30.0679632281952));
#27534=CARTESIAN_POINT('Ctrl Pts',(-26.1668007407994,21.6688117468322,-30.0682806154101));
#27535=CARTESIAN_POINT('Ctrl Pts',(-26.1912655746108,21.7029500488124,-30.0708697227064));
#27536=CARTESIAN_POINT('Ctrl Pts',(-26.2122232150547,21.7332801264855,-30.0731072706912));
#27537=CARTESIAN_POINT('Ctrl Pts',(-26.401834456812,22.0180125257273,-30.0936045308531));
#27538=CARTESIAN_POINT('Ctrl Pts',(-26.5340888704572,22.2948407039127,-30.1099427983761));
#27539=CARTESIAN_POINT('Ctrl Pts',(-26.656866147206,22.68647214118,-30.1332533022025));
#27540=CARTESIAN_POINT('Ctrl Pts',(-26.683380540385,22.7882349637176,-30.1393122610416));
#27541=CARTESIAN_POINT('Ctrl Pts',(-26.7184296737575,22.9559771439133,-30.1494398378854));
#27542=CARTESIAN_POINT('Ctrl Pts',(-26.7299793276157,23.0212476397247,-30.1534137343236));
#27543=CARTESIAN_POINT('Ctrl Pts',(-26.7407269052554,23.095211152118,-30.1579693586841));
#27544=CARTESIAN_POINT('Ctrl Pts',(-26.7419124831522,23.1036026267634,-30.158486962878));
#27545=CARTESIAN_POINT('Ctrl Pts',(-26.7436409838326,23.116195277371,-30.1592648597348));
#27546=CARTESIAN_POINT('Ctrl Pts',(-26.7442087515706,23.1203930528824,-30.1595243648907));
#27547=CARTESIAN_POINT('Ctrl Pts',(-26.745169978138,23.1276069065558,-30.1599706576229));
#27548=CARTESIAN_POINT('Ctrl Pts',(-26.7455674473661,23.1306224521967,-30.160157317942));
#27549=CARTESIAN_POINT('Ctrl Pts',(-26.7463762991624,23.1368268868681,-30.1605415767201));
#27550=CARTESIAN_POINT('Ctrl Pts',(-26.7467871795949,23.1400158373105,-30.1607391908765));
#27551=CARTESIAN_POINT('Ctrl Pts',(-26.7477633900233,23.1476829759905,-30.1612145855562));
#27552=CARTESIAN_POINT('Ctrl Pts',(-26.7483240844621,23.152161738826,-30.1614925124879));
#27553=CARTESIAN_POINT('Ctrl Pts',(-26.7500113936267,23.1658734166126,-30.1623440788993));
#27554=CARTESIAN_POINT('Ctrl Pts',(-26.751107439879,23.175109982171,-30.1629186838432));
#27555=CARTESIAN_POINT('Ctrl Pts',(-26.7631557277501,23.2805415000219,-30.1694888280347));
#27556=CARTESIAN_POINT('Ctrl Pts',(-26.7698068178985,23.3771689334649,-30.1756196284918));
#27557=CARTESIAN_POINT('Ctrl Pts',(-26.7727190415123,23.5001227090048,-30.1835710666304));
#27558=CARTESIAN_POINT('Ctrl Pts',(-26.773019992036,23.5263099891905,-30.1852730874953));
#27559=CARTESIAN_POINT('Ctrl Pts',(-26.7727881413319,23.8591445991835,-30.2070111173044));
#27560=CARTESIAN_POINT('Ctrl Pts',(-26.7288145915301,24.1641331308318,-30.2282816487434));
#27561=CARTESIAN_POINT('Ctrl Pts',(-26.6200796999562,24.5344139073553,-30.2536889018559));
#27562=CARTESIAN_POINT('Ctrl Pts',(-26.5949190042235,24.609696273329,-30.2588187780465));
#27563=CARTESIAN_POINT('Ctrl Pts',(-26.5648100570725,24.6898135548397,-30.2641831682948));
#27564=CARTESIAN_POINT('Ctrl Pts',(-26.5626008004105,24.69564081031,-30.2645727891766));
#27565=CARTESIAN_POINT('Ctrl Pts',(-26.5595004538812,24.7037474359697,-30.2651140049904));
#27566=CARTESIAN_POINT('Ctrl Pts',(-26.5586236682179,24.7060322063748,-30.2652664516389));
#27567=CARTESIAN_POINT('Ctrl Pts',(-26.5571075767115,24.7099694972708,-30.265529002119));
#27568=CARTESIAN_POINT('Ctrl Pts',(-26.5564695106695,24.7116224888342,-30.2656391807735));
#27569=CARTESIAN_POINT('Ctrl Pts',(-26.5551441303917,24.7150476448031,-30.2658673810035));
#27570=CARTESIAN_POINT('Ctrl Pts',(-26.5544566126293,24.7168197245953,-30.2659853894375));
#27571=CARTESIAN_POINT('Ctrl Pts',(-26.5528310619855,24.7209986205535,-30.266263545387));
#27572=CARTESIAN_POINT('Ctrl Pts',(-26.551891699791,24.7234049258035,-30.2664236122652));
#27573=CARTESIAN_POINT('Ctrl Pts',(-26.5487986489507,24.7313001648601,-30.2669484756866));
#27574=CARTESIAN_POINT('Ctrl Pts',(-26.5466327734298,24.7367843590633,-30.2673125387166));
#27575=CARTESIAN_POINT('Ctrl Pts',(-26.5000259625355,24.8538555828179,-30.2750737539433));
#27576=CARTESIAN_POINT('Ctrl Pts',(-26.4493901276216,24.9628929750652,-30.282100310551));
#27577=CARTESIAN_POINT('Ctrl Pts',(-26.2525711616475,25.3312978359722,-30.3059732692979));
#27578=CARTESIAN_POINT('Ctrl Pts',(-26.0767028823639,25.5730501660351,-30.3220187358018));
#27579=CARTESIAN_POINT('Ctrl Pts',(-25.8062139033024,25.8535635513256,-30.3447669706851));
#27580=CARTESIAN_POINT('Ctrl Pts',(-25.7394636572377,25.9170975895764,-30.3502465928779));
#27581=CARTESIAN_POINT('Ctrl Pts',(-25.6624018828405,25.9843944398709,-30.3564747648856));
#27582=CARTESIAN_POINT('Ctrl Pts',(-25.6546833073551,25.9910705948392,-30.3570975201256));
#27583=CARTESIAN_POINT('Ctrl Pts',(-25.6438091903555,26.0003862018332,-30.3579734393602));
#27584=CARTESIAN_POINT('Ctrl Pts',(-25.6406800497583,26.0030564937015,-30.3582253288853));
#27585=CARTESIAN_POINT('Ctrl Pts',(-25.6349368787238,26.0079385288728,-30.3586873443334));
#27586=CARTESIAN_POINT('Ctrl Pts',(-25.6323244157136,26.0101521144245,-30.35889739407));
#27587=CARTESIAN_POINT('Ctrl Pts',(-25.6270299040134,26.0146237700862,-30.3593228634635));
#27588=CARTESIAN_POINT('Ctrl Pts',(-25.6243476892283,26.0168816347677,-30.3595382910953));
#27589=CARTESIAN_POINT('Ctrl Pts',(-25.6177480198142,26.022418802283,-30.3600680749249));
#27590=CARTESIAN_POINT('Ctrl Pts',(-25.613826451375,26.0256931672915,-30.3603826324934));
#27591=CARTESIAN_POINT('Ctrl Pts',(-25.5995684669787,26.0375406331669,-30.3615254288376));
#27592=CARTESIAN_POINT('Ctrl Pts',(-25.5891863872528,26.0460583386876,-30.3623559179686));
#27593=CARTESIAN_POINT('Ctrl Pts',(-25.437248566063,26.1691309932815,-30.3744868818276));
#27594=CARTESIAN_POINT('Ctrl Pts',(-25.286311467082,26.2715311269103,-30.3862789528047));
#27595=CARTESIAN_POINT('Ctrl Pts',(-24.8570945016134,26.512426752707,-30.4190829565415));
#27596=CARTESIAN_POINT('Ctrl Pts',(-24.5661446532548,26.6243825795122,-30.4406920981083));
#27597=CARTESIAN_POINT('Ctrl Pts',(-24.2479013163498,26.6966259625061,-30.4613445472688));
#27598=CARTESIAN_POINT('Ctrl Pts',(-24.2320884196013,26.7000905340298,-30.4623628158075));
#27599=CARTESIAN_POINT('Ctrl Pts',(-24.2127426893788,26.7041766273685,-30.4635983697762));
#27600=CARTESIAN_POINT('Ctrl Pts',(-24.2092344245252,26.7049115109712,-30.4638220229564));
#27601=CARTESIAN_POINT('Ctrl Pts',(-24.2034488875219,26.7061133472418,-30.4641901703862));
#27602=CARTESIAN_POINT('Ctrl Pts',(-24.2011723359378,26.7065836890492,-30.4643348586425));
#27603=CARTESIAN_POINT('Ctrl Pts',(-24.1971080543292,26.7074187966109,-30.4645928544933));
#27604=CARTESIAN_POINT('Ctrl Pts',(-24.1953205273345,26.7077845065994,-30.464706216421));
#27605=CARTESIAN_POINT('Ctrl Pts',(-24.1917008116831,26.7085218618142,-30.4649355532503));
#27606=CARTESIAN_POINT('Ctrl Pts',(-24.189868616906,26.7088934294631,-30.4650515233761));
#27607=CARTESIAN_POINT('Ctrl Pts',(-24.184797483288,26.7099172580589,-30.4653721930844));
#27608=CARTESIAN_POINT('Ctrl Pts',(-24.1815578514779,26.7105661351317,-30.4655766975536));
#27609=CARTESIAN_POINT('Ctrl Pts',(-24.1744627206393,26.7119758981761,-30.4660238257275));
#27610=CARTESIAN_POINT('Ctrl Pts',(-24.1706068094036,26.7127347176761,-30.4662663318913));
#27611=CARTESIAN_POINT('Ctrl Pts',(-24.1592671837969,26.7149447485685,-30.4669780911508));
#27612=CARTESIAN_POINT('Ctrl Pts',(-24.151779633724,26.7163764746666,-30.4674462575447));
#27613=CARTESIAN_POINT('Ctrl Pts',(-23.8706312918523,26.7691026838073,-30.4849599311715));
#27614=CARTESIAN_POINT('Ctrl Pts',(-23.5914249828275,26.7847545344439,-30.5000963244803));
#27615=CARTESIAN_POINT('Ctrl Pts',(-23.2212777852796,26.7575053768555,-30.520917584913));
#27616=CARTESIAN_POINT('Ctrl Pts',(-23.129251950374,26.7467275321325,-30.5261491574218));
#27617=CARTESIAN_POINT('Ctrl Pts',(-23.0198448949343,26.7291071748471,-30.5325202795852));
#27618=CARTESIAN_POINT('Ctrl Pts',(-23.0018933449354,26.7260597189684,-30.5335705176079));
#27619=CARTESIAN_POINT('Ctrl Pts',(-22.9441085196505,26.7157456147818,-30.5369683054403));
#27620=CARTESIAN_POINT('Ctrl Pts',(-22.904387082252,26.7078805429485,-30.5393303430552));
#27621=CARTESIAN_POINT('Ctrl Pts',(-22.7936632030015,26.6837799593381,-30.5460008612745));
#27622=CARTESIAN_POINT('Ctrl Pts',(-22.7230511849288,26.6658838028677,-30.5503555532915));
#27623=CARTESIAN_POINT('Ctrl Pts',(-22.643480072533,26.6428213331935,-30.5553994666403));
#27624=CARTESIAN_POINT('Ctrl Pts',(-22.6338634750866,26.6399853968554,-30.55601133696));
#27625=CARTESIAN_POINT('Ctrl Pts',(-22.6199611895901,26.6358149970042,-30.5568992565498));
#27626=CARTESIAN_POINT('Ctrl Pts',(-22.6156647431757,26.6345163618087,-30.5571741311988));
#27627=CARTESIAN_POINT('Ctrl Pts',(-22.6081157370842,26.6322173923887,-30.5576579216964));
#27628=CARTESIAN_POINT('Ctrl Pts',(-22.6048620155102,26.6312208720186,-30.5578667120766));
#27629=CARTESIAN_POINT('Ctrl Pts',(-22.5981661591933,26.6291585202097,-30.5582969425794));
#27630=CARTESIAN_POINT('Ctrl Pts',(-22.5947242227068,26.6280920657462,-30.558518402933));
#27631=CARTESIAN_POINT('Ctrl Pts',(-22.585974182157,26.6253648485503,-30.5590821754393));
#27632=CARTESIAN_POINT('Ctrl Pts',(-22.5806685912022,26.6236961180295,-30.559424749439));
#27633=CARTESIAN_POINT('Ctrl Pts',(-22.5594669748747,26.6169673588041,-30.5607966490888));
#27634=CARTESIAN_POINT('Ctrl Pts',(-22.5436062447099,26.6117977439168,-30.561829582323));
#27635=CARTESIAN_POINT('Ctrl Pts',(-22.4422558208104,26.5778910734511,-30.5684733855978));
#27636=CARTESIAN_POINT('Ctrl Pts',(-22.3579716391042,26.5457016635174,-30.5741984001336));
#27637=CARTESIAN_POINT('Ctrl Pts',(-22.2073804094754,26.4808254844909,-30.5848078846483));
#27638=CARTESIAN_POINT('Ctrl Pts',(-22.1406353433465,26.4493111592343,-30.5896524661825));
#27639=CARTESIAN_POINT('Ctrl Pts',(-22.0750360141079,26.4155367739188,-30.5945512678406));
#27640=CARTESIAN_POINT('',(-26.7730022627907,23.5515690488782,-30.4357734492251));
#27641=CARTESIAN_POINT('Ctrl Pts',(-22.0750360153473,26.4155367745569,-30.8398067994259));
#27642=CARTESIAN_POINT('Ctrl Pts',(-22.0896415646513,26.4230565686636,-30.8388053845237));
#27643=CARTESIAN_POINT('Ctrl Pts',(-22.1043047924991,26.4304647802139,-30.8378104288188));
#27644=CARTESIAN_POINT('Ctrl Pts',(-22.1562909130468,26.4562323249972,-30.8343173602465));
#27645=CARTESIAN_POINT('Ctrl Pts',(-22.1939133292558,26.4739816325899,-30.8318515798414));
#27646=CARTESIAN_POINT('Ctrl Pts',(-22.271427038284,26.5087322291368,-30.8268761304353));
#27647=CARTESIAN_POINT('Ctrl Pts',(-22.3113387733486,26.5256667448064,-30.8243695128954));
#27648=CARTESIAN_POINT('Ctrl Pts',(-22.4738574150107,26.5907858705176,-30.8143381125657));
#27649=CARTESIAN_POINT('Ctrl Pts',(-22.5990278524788,26.6322395860278,-30.8070055666797));
#27650=CARTESIAN_POINT('Ctrl Pts',(-22.8937240215838,26.7101649942925,-30.7899699113415));
#27651=CARTESIAN_POINT('Ctrl Pts',(-23.0643419887723,26.7408575560767,-30.7802623955911));
#27652=CARTESIAN_POINT('Ctrl Pts',(-23.2645785093251,26.7604392800701,-30.7685091963496));
#27653=CARTESIAN_POINT('Ctrl Pts',(-23.2926045056041,26.7628100852407,-30.7668565829421));
#27654=CARTESIAN_POINT('Ctrl Pts',(-23.331741746087,26.7656054033468,-30.7645363181845));
#27655=CARTESIAN_POINT('Ctrl Pts',(-23.3428300446381,26.7663397444739,-30.7638775544502));
#27656=CARTESIAN_POINT('Ctrl Pts',(-23.407200966481,26.7702685337694,-30.7600447307454));
#27657=CARTESIAN_POINT('Ctrl Pts',(-23.4605500761491,26.7721960073218,-30.7568341862726));
#27658=CARTESIAN_POINT('Ctrl Pts',(-23.5226744088817,26.7728964239378,-30.7530481043858));
#27659=CARTESIAN_POINT('Ctrl Pts',(-23.5314289522968,26.772959449729,-30.7525134800927));
#27660=CARTESIAN_POINT('Ctrl Pts',(-23.5444762355346,26.7730002140307,-30.7517150453256));
#27661=CARTESIAN_POINT('Ctrl Pts',(-23.5487689006376,26.7730050490555,-30.7514520857702));
#27662=CARTESIAN_POINT('Ctrl Pts',(-23.5564247971283,26.7729983760178,-30.7509826194275));
#27663=CARTESIAN_POINT('Ctrl Pts',(-23.5597880312251,26.7729901797316,-30.7507762169138));
#27664=CARTESIAN_POINT('Ctrl Pts',(-23.5668781877368,26.7729618019281,-30.7503407396844));
#27665=CARTESIAN_POINT('Ctrl Pts',(-23.5706050980211,26.7729404200489,-30.7501116275816));
#27666=CARTESIAN_POINT('Ctrl Pts',(-23.5804479922134,26.772866874851,-30.7495059882894));
#27667=CARTESIAN_POINT('Ctrl Pts',(-23.5865638575088,26.7728037659414,-30.7491291179597));
#27668=CARTESIAN_POINT('Ctrl Pts',(-23.6142202505335,26.7724396428028,-30.747422331667));
#27669=CARTESIAN_POINT('Ctrl Pts',(-23.6357572087454,26.7719400649529,-30.7460861963887));
#27670=CARTESIAN_POINT('Ctrl Pts',(-23.793485220148,26.7666986802268,-30.7362477508896));
#27671=CARTESIAN_POINT('Ctrl Pts',(-23.9292405103811,26.7535394864115,-30.7274805953845));
#27672=CARTESIAN_POINT('Ctrl Pts',(-24.1033085259862,26.7254459097807,-30.7158523677548));
#27673=CARTESIAN_POINT('Ctrl Pts',(-24.1427522735887,26.7183225768443,-30.7131920352082));
#27674=CARTESIAN_POINT('Ctrl Pts',(-24.2128996231742,26.7042985062799,-30.7084186982923));
#27675=CARTESIAN_POINT('Ctrl Pts',(-24.2436548780747,26.6976801005883,-30.7063112961726));
#27676=CARTESIAN_POINT('Ctrl Pts',(-24.2996732027336,26.6847642680805,-30.7024483376437));
#27677=CARTESIAN_POINT('Ctrl Pts',(-24.3249665393735,26.6786088650635,-30.7006949379456));
#27678=CARTESIAN_POINT('Ctrl Pts',(-24.371673866749,26.6666409487333,-30.6974415540267));
#27679=CARTESIAN_POINT('Ctrl Pts',(-24.3931078930697,26.6609123660805,-30.6959424745147));
#27680=CARTESIAN_POINT('Ctrl Pts',(-24.4330530342956,26.6497932208371,-30.6931384441911));
#27681=CARTESIAN_POINT('Ctrl Pts',(-24.4515783206892,26.6444569577199,-30.6918338530952));
#27682=CARTESIAN_POINT('Ctrl Pts',(-24.4863444610054,26.6341037530824,-30.6893785057667));
#27683=CARTESIAN_POINT('Ctrl Pts',(-24.5025957205963,26.6291239006293,-30.6882278505086));
#27684=CARTESIAN_POINT('Ctrl Pts',(-24.6745433977778,26.5749425435578,-30.6760257244682));
#27685=CARTESIAN_POINT('Ctrl Pts',(-24.8263400034613,26.5140997215737,-30.6649999976738));
#27686=CARTESIAN_POINT('Ctrl Pts',(-25.008685592226,26.4243928804284,-30.6519102651671));
#27687=CARTESIAN_POINT('Ctrl Pts',(-25.0441613391181,26.4061143238229,-30.6493720376264));
#27688=CARTESIAN_POINT('Ctrl Pts',(-25.0839761424602,26.3846550758923,-30.6465406795878));
#27689=CARTESIAN_POINT('Ctrl Pts',(-25.0886556539219,26.3821179471519,-30.6462081795906));
#27690=CARTESIAN_POINT('Ctrl Pts',(-25.0954802137077,26.3783959117298,-30.645723690707));
#27691=CARTESIAN_POINT('Ctrl Pts',(-25.0976301994596,26.3772201510165,-30.6455711209473));
#27692=CARTESIAN_POINT('Ctrl Pts',(-25.1014328647216,26.3751349531954,-30.6453013844033));
#27693=CARTESIAN_POINT('Ctrl Pts',(-25.1030860878248,26.3742265166853,-30.6451841532012));
#27694=CARTESIAN_POINT('Ctrl Pts',(-25.1064994497403,26.3723469903577,-30.6449421884633));
#27695=CARTESIAN_POINT('Ctrl Pts',(-25.1082594737742,26.3713757073161,-30.6448174679982));
#27696=CARTESIAN_POINT('Ctrl Pts',(-25.1127694359319,26.3688813416591,-30.6444979868244));
#27697=CARTESIAN_POINT('Ctrl Pts',(-25.1155180646345,26.3673558766183,-30.6443033797757));
#27698=CARTESIAN_POINT('Ctrl Pts',(-25.1215271747893,26.3640093629202,-30.6438781415758));
#27699=CARTESIAN_POINT('Ctrl Pts',(-25.1247867371966,26.3621866606058,-30.6436476160705));
#27700=CARTESIAN_POINT('Ctrl Pts',(-25.1342395880614,26.356879166635,-30.6429794667181));
#27701=CARTESIAN_POINT('Ctrl Pts',(-25.1404245762917,26.3533795237318,-30.642542775759));
#27702=CARTESIAN_POINT('Ctrl Pts',(-25.1614114643989,26.3414127279415,-30.6410624502854));
#27703=CARTESIAN_POINT('Ctrl Pts',(-25.1761580135121,26.3328483953251,-30.6400247576722));
#27704=CARTESIAN_POINT('Ctrl Pts',(-25.2354706131042,26.2977689871749,-30.6358581440697));
#27705=CARTESIAN_POINT('Ctrl Pts',(-25.2794640673054,26.2702956878254,-30.6327840256834));
#27706=CARTESIAN_POINT('Ctrl Pts',(-25.3822358234883,26.202614360581,-30.6255948593987));
#27707=CARTESIAN_POINT('Ctrl Pts',(-25.4403831712318,26.161496158141,-30.6215208040603));
#27708=CARTESIAN_POINT('Ctrl Pts',(-25.7757914055035,25.9072368850689,-30.5976899544582));
#27709=CARTESIAN_POINT('Ctrl Pts',(-26.0181963368405,25.652073300597,-30.5787784602397));
#27710=CARTESIAN_POINT('Ctrl Pts',(-26.2263704658291,25.3460608378841,-30.5563966807607));
#27711=CARTESIAN_POINT('Ctrl Pts',(-26.2376968839226,25.3290660390078,-30.5551556795549));
#27712=CARTESIAN_POINT('Ctrl Pts',(-26.2522817390364,25.3067248166451,-30.5535264381184));
#27713=CARTESIAN_POINT('Ctrl Pts',(-26.2556873804691,25.3014746773092,-30.5531437251543));
#27714=CARTESIAN_POINT('Ctrl Pts',(-26.2609104028558,25.2933712631271,-30.552553246362));
#27715=CARTESIAN_POINT('Ctrl Pts',(-26.2627386323656,25.2905249701039,-30.5523458857275));
#27716=CARTESIAN_POINT('Ctrl Pts',(-26.2663646508542,25.2848601803131,-30.5519332719248));
#27717=CARTESIAN_POINT('Ctrl Pts',(-26.268162542628,25.282041754096,-30.5517280229265));
#27718=CARTESIAN_POINT('Ctrl Pts',(-26.272130102672,25.2758006976413,-30.551273611167));
#27719=CARTESIAN_POINT('Ctrl Pts',(-26.2742977047105,25.2723767663307,-30.5510243720673));
#27720=CARTESIAN_POINT('Ctrl Pts',(-26.2805089075306,25.2625245190747,-30.5503073544005));
#27721=CARTESIAN_POINT('Ctrl Pts',(-26.2845362312402,25.2560860186964,-30.5498389737924));
#27722=CARTESIAN_POINT('Ctrl Pts',(-26.3109358254074,25.2135471746394,-30.546745604233));
#27723=CARTESIAN_POINT('Ctrl Pts',(-26.3326144774095,25.1770232721595,-30.5440952171019));
#27724=CARTESIAN_POINT('Ctrl Pts',(-26.3942783487156,25.0682927778022,-30.5362166880143));
#27725=CARTESIAN_POINT('Ctrl Pts',(-26.4322164859861,24.9949707910128,-30.5309176222556));
#27726=CARTESIAN_POINT('Ctrl Pts',(-26.6041806500607,24.6288266619948,-30.5045205254442));
#27727=CARTESIAN_POINT('Ctrl Pts',(-26.6965903755075,24.3185668852515,-30.4821115131693));
#27728=CARTESIAN_POINT('Ctrl Pts',(-26.7431534170635,23.9880228588051,-30.4602696852952));
#27729=CARTESIAN_POINT('Ctrl Pts',(-26.7447467514788,23.9762403370877,-30.4594940394283));
#27730=CARTESIAN_POINT('Ctrl Pts',(-26.7464584706982,23.9630323747509,-30.4586280200418));
#27731=CARTESIAN_POINT('Ctrl Pts',(-26.7466411350313,23.9616155099008,-30.4585351636877));
#27732=CARTESIAN_POINT('Ctrl Pts',(-26.7475863015471,23.9542455360234,-30.4580523949869));
#27733=CARTESIAN_POINT('Ctrl Pts',(-26.7483331201726,23.9482903866946,-30.4576630965287));
#27734=CARTESIAN_POINT('Ctrl Pts',(-26.7492392382619,23.9408977734967,-30.4571808391253));
#27735=CARTESIAN_POINT('Ctrl Pts',(-26.7494142067891,23.939462282803,-30.4570872420964));
#27736=CARTESIAN_POINT('Ctrl Pts',(-26.7504927256297,23.9305639488393,-30.4565073467545));
#27737=CARTESIAN_POINT('Ctrl Pts',(-26.7513711365737,23.9230980124563,-30.4560220845911));
#27738=CARTESIAN_POINT('Ctrl Pts',(-26.7567164489198,23.8762544524727,-30.4529857364108));
#27739=CARTESIAN_POINT('Ctrl Pts',(-26.7604830691188,23.8367980929405,-30.4504651099382));
#27740=CARTESIAN_POINT('Ctrl Pts',(-26.7639283268978,23.7919831049697,-30.4476514652907));
#27741=CARTESIAN_POINT('Ctrl Pts',(-26.7643224524585,23.7866850424314,-30.447319614519));
#27742=CARTESIAN_POINT('Ctrl Pts',(-26.7648790846507,23.7789437706466,-30.4468358942514));
#27743=CARTESIAN_POINT('Ctrl Pts',(-26.7650519081915,23.7765013476353,-30.4466834464799));
#27744=CARTESIAN_POINT('Ctrl Pts',(-26.7653529280629,23.7721772059014,-30.4464138505772));
#27745=CARTESIAN_POINT('Ctrl Pts',(-26.7654822561327,23.7702955704694,-30.4462966382534));
#27746=CARTESIAN_POINT('Ctrl Pts',(-26.7657282010927,23.7666707248699,-30.4460710328125));
#27747=CARTESIAN_POINT('Ctrl Pts',(-26.7658450518867,23.7649275394335,-30.4459626265691));
#27748=CARTESIAN_POINT('Ctrl Pts',(-26.7660938256411,23.7611705429245,-30.4457291706014));
#27749=CARTESIAN_POINT('Ctrl Pts',(-26.766225274738,23.7591566995994,-30.4456041477784));
#27750=CARTESIAN_POINT('Ctrl Pts',(-26.7665386882908,23.7542846946977,-30.4453019616243));
#27751=CARTESIAN_POINT('Ctrl Pts',(-26.7667187350782,23.7514264049812,-30.4451249060969));
#27752=CARTESIAN_POINT('Ctrl Pts',(-26.7671964395218,23.7436781166658,-30.4446455557152));
#27753=CARTESIAN_POINT('Ctrl Pts',(-26.7674867590106,23.7387876487219,-30.4443436680854));
#27754=CARTESIAN_POINT('Ctrl Pts',(-26.7712280359402,23.6732390291014,-30.4403060186204));
#27755=CARTESIAN_POINT('Ctrl Pts',(-26.7729743898063,23.612491610421,-30.4366633785719));
#27756=CARTESIAN_POINT('Ctrl Pts',(-26.7730021943074,23.5517271931927,-30.4330867142687));
#27757=CARTESIAN_POINT('Ctrl Pts',(-26.7730022627907,23.5515690488782,-30.4357734492251));
#27758=CARTESIAN_POINT('Ctrl Pts',(-26.77304247429,23.4531338744264,-30.4296632602288));
#27759=CARTESIAN_POINT('Ctrl Pts',(-26.7685685722269,23.3545143288027,-30.4235530712325));
#27760=CARTESIAN_POINT('Ctrl Pts',(-26.7595561131448,23.2561639658024,-30.4174428822362));
#27761=CARTESIAN_POINT('Ctrl Pts',(-26.7505553265621,23.1579409814163,-30.4113406068599));
#27762=CARTESIAN_POINT('Ctrl Pts',(-26.7370277015207,23.0599869250309,-30.4052383314836));
#27763=CARTESIAN_POINT('Ctrl Pts',(-26.7190008029838,22.9627561864298,-30.3991360561074));
#27764=CARTESIAN_POINT('Ctrl Pts',(-26.7006986159141,22.8640406384855,-30.3929405929633));
#27765=CARTESIAN_POINT('Ctrl Pts',(-26.6777585735126,22.7660711481936,-30.3867451298192));
#27766=CARTESIAN_POINT('Ctrl Pts',(-26.6502643952142,22.6693189311685,-30.3805496666752));
#27767=CARTESIAN_POINT('Ctrl Pts',(-26.6232272244863,22.5741749271682,-30.3744571843705));
#27768=CARTESIAN_POINT('Ctrl Pts',(-26.5917862856016,22.4802084820841,-30.3683647020658));
#27769=CARTESIAN_POINT('Ctrl Pts',(-26.5560725534804,22.3878569195513,-30.3622722197611));
#27770=CARTESIAN_POINT('Ctrl Pts',(-26.5203688660586,22.2955313314444,-30.3561814510033));
#27771=CARTESIAN_POINT('Ctrl Pts',(-26.4803949324917,22.2048201373144,-30.3500906822455));
#27772=CARTESIAN_POINT('Ctrl Pts',(-26.4363308136407,22.1161431519826,-30.3439999134877));
#27773=CARTESIAN_POINT('Ctrl Pts',(-26.3922667373225,22.027466252246,-30.337909150609));
#27774=CARTESIAN_POINT('Ctrl Pts',(-26.3441126820331,21.940823954374,-30.3318183877303));
#27775=CARTESIAN_POINT('Ctrl Pts',(-26.2920953441146,21.8566127959538,-30.3257276248516));
#27776=CARTESIAN_POINT('Ctrl Pts',(-26.2385168775424,21.7698743176509,-30.3194540678348));
#27777=CARTESIAN_POINT('Ctrl Pts',(-26.1808398076691,21.6857156553139,-30.313180510818));
#27778=CARTESIAN_POINT('Ctrl Pts',(-26.11935980296,21.6045379094464,-30.3069069538011));
#27779=CARTESIAN_POINT('Ctrl Pts',(-26.0595866822292,21.525613920625,-30.3008075710383));
#27780=CARTESIAN_POINT('Ctrl Pts',(-25.9962193630557,21.4495078018546,-30.2947081882755));
#27781=CARTESIAN_POINT('Ctrl Pts',(-25.9295693813819,21.3765531754601,-30.2886088055127));
#27782=CARTESIAN_POINT('Ctrl Pts',(-25.8600645098058,21.3004736055775,-30.2822481613689));
#27783=CARTESIAN_POINT('Ctrl Pts',(-25.7869898592751,21.2278219288648,-30.275887517225));
#27784=CARTESIAN_POINT('Ctrl Pts',(-25.7107384781269,21.1589311317634,-30.2695268730812));
#27785=CARTESIAN_POINT('Ctrl Pts',(-25.6344870969787,21.0900403346621,-30.2631662289373));
#27786=CARTESIAN_POINT('Ctrl Pts',(-25.5550594510845,21.024910698303,-30.2568055847935));
#27787=CARTESIAN_POINT('Ctrl Pts',(-25.4728825618927,20.9638242358625,-30.2504449406496));
#27788=CARTESIAN_POINT('Ctrl Pts',(-25.3931416972281,20.9045486003132,-30.2442728493373));
#27789=CARTESIAN_POINT('Ctrl Pts',(-25.310516577792,20.8488596986913,-30.238100758025));
#27790=CARTESIAN_POINT('Ctrl Pts',(-25.2253636729472,20.7970507179962,-30.2319286667126));
#27791=CARTESIAN_POINT('Ctrl Pts',(-25.1403261418701,20.745311933348,-30.2257649379739));
#27792=CARTESIAN_POINT('Ctrl Pts',(-25.0527680005755,20.6974428447619,-30.2196012092351));
#27793=CARTESIAN_POINT('Ctrl Pts',(-24.963077241254,20.6536952816891,-30.2134374804963));
#27794=CARTESIAN_POINT('Ctrl Pts',(-24.8734815008737,20.6099940650533,-30.2072802816496));
#27795=CARTESIAN_POINT('Ctrl Pts',(-24.7817580224552,20.5704058825787,-30.2011230828029));
#27796=CARTESIAN_POINT('Ctrl Pts',(-24.6883212883984,20.5351377631466,-30.1949658839562));
#27797=CARTESIAN_POINT('Ctrl Pts',(-24.5949528509282,20.4998954225712,-30.1888131856485));
#27798=CARTESIAN_POINT('Ctrl Pts',(-24.4998740527622,20.4689670199309,-30.1826604873408));
#27799=CARTESIAN_POINT('Ctrl Pts',(-24.4035205023671,20.4425119806308,-30.1765077890331));
#27800=CARTESIAN_POINT('Ctrl Pts',(-24.3072034893753,20.4160669731193,-30.1703574238374));
#27801=CARTESIAN_POINT('Ctrl Pts',(-24.2096131030746,20.394092073292,-30.1642070586416));
#27802=CARTESIAN_POINT('Ctrl Pts',(-24.111200453139,20.3766969560147,-30.1580566934459));
#27803=CARTESIAN_POINT('Ctrl Pts',(-24.0127987931402,20.3593037812847,-30.1519070150737));
#27804=CARTESIAN_POINT('Ctrl Pts',(-23.9135754798358,20.346489447917,-30.1457573367014));
#27805=CARTESIAN_POINT('Ctrl Pts',(-23.8139911698563,20.3383123869779,-30.1396076583292));
#27806=CARTESIAN_POINT('Ctrl Pts',(-23.7143913391297,20.3301340516,-30.1334570214968));
#27807=CARTESIAN_POINT('Ctrl Pts',(-23.6144308329609,20.3265944597579,-30.1273063846643));
#27808=CARTESIAN_POINT('Ctrl Pts',(-23.5145737635325,20.3277000359228,-30.1211557478318));
#27809=CARTESIAN_POINT('Ctrl Pts',(-23.4146098680168,20.3288067948219,-30.11499853111));
#27810=CARTESIAN_POINT('Ctrl Pts',(-23.3147500654339,20.3345686402192,-30.1088413143882));
#27811=CARTESIAN_POINT('Ctrl Pts',(-23.2154566783019,20.3449398637862,-30.1026840976664));
#27812=CARTESIAN_POINT('Ctrl Pts',(-23.116107895796,20.3553168734164,-30.0965234458586));
#27813=CARTESIAN_POINT('Ctrl Pts',(-23.0173265875522,20.3703083172426,-30.0903627940508));
#27814=CARTESIAN_POINT('Ctrl Pts',(-22.919566093302,20.3898170903463,-30.084202142243));
#27815=CARTESIAN_POINT('Ctrl Pts',(-22.8216420109809,20.4093585085647,-30.0780311814739));
#27816=CARTESIAN_POINT('Ctrl Pts',(-22.7247425764993,20.433432250389,-30.0718602207049));
#27817=CARTESIAN_POINT('Ctrl Pts',(-22.6293072918812,20.4618909227232,-30.0656892599359));
#27818=CARTESIAN_POINT('Ctrl Pts',(-22.5564597472485,20.4836139616532,-30.0609788497155));
#27819=CARTESIAN_POINT('Ctrl Pts',(-22.4844650125374,20.5078908642717,-30.0562684394952));
#27820=CARTESIAN_POINT('Ctrl Pts',(-22.4135100480725,20.5346374885513,-30.0515580292748));
#27821=CARTESIAN_POINT('Ctrl Pts',(-22.3205371435372,20.5696838220186,-30.0453859379625));
#27822=CARTESIAN_POINT('Ctrl Pts',(-22.2290227564579,20.6090955091581,-30.0392138466501));
#27823=CARTESIAN_POINT('Ctrl Pts',(-22.1394062367787,20.6527311263163,-30.0330417553378));
#27824=CARTESIAN_POINT('Ctrl Pts',(-22.0499111386242,20.696307621527,-30.026878026599));
#27825=CARTESIAN_POINT('Ctrl Pts',(-21.9623091840145,20.7440964831748,-30.0207142978602));
#27826=CARTESIAN_POINT('Ctrl Pts',(-21.8770219675195,20.795907411414,-30.0145505691215));
#27827=CARTESIAN_POINT('Ctrl Pts',(-21.7918251048255,20.8476634508375,-30.0083933702748));
#27828=CARTESIAN_POINT('Ctrl Pts',(-21.70893847417,20.9034328613005,-30.0022361714281));
#27829=CARTESIAN_POINT('Ctrl Pts',(-21.6287602977326,20.9629788396923,-29.9960789725814));
#27830=CARTESIAN_POINT('Ctrl Pts',(-21.5486407266801,21.0224812935848,-29.9899262742737));
#27831=CARTESIAN_POINT('Ctrl Pts',(-21.4712260215294,21.0857545689622,-29.983773575966));
#27832=CARTESIAN_POINT('Ctrl Pts',(-21.3968857743915,21.152518357303,-29.9776208776583));
#27833=CARTESIAN_POINT('Ctrl Pts',(-21.3225737171811,21.2192568287201,-29.9714705124626));
#27834=CARTESIAN_POINT('Ctrl Pts',(-21.2513341243105,21.2894828931717,-29.9653201472668));
#27835=CARTESIAN_POINT('Ctrl Pts',(-21.1835031109869,21.3628763084345,-29.9591697820711));
#27836=CARTESIAN_POINT('Ctrl Pts',(-21.1156796724878,21.4362615277083,-29.9530201036988));
#27837=CARTESIAN_POINT('Ctrl Pts',(-21.0512643516077,21.5128130755611,-29.9468704253266));
#27838=CARTESIAN_POINT('Ctrl Pts',(-20.9905553118204,21.5921749783091,-29.9407207469544));
#27839=CARTESIAN_POINT('Ctrl Pts',(-20.9298368102049,21.6715492500337,-29.934570110122));
#27840=CARTESIAN_POINT('Ctrl Pts',(-20.8728260009893,21.7537344015906,-29.9284194732895));
#27841=CARTESIAN_POINT('Ctrl Pts',(-20.819779161499,21.8383434403127,-29.9222688364571));
#27842=CARTESIAN_POINT('Ctrl Pts',(-20.7666755730337,21.9230429929327,-29.9161116197353));
#27843=CARTESIAN_POINT('Ctrl Pts',(-20.7175446535865,22.0101712420173,-29.9099544030134));
#27844=CARTESIAN_POINT('Ctrl Pts',(-20.672597852894,22.0993145205857,-29.9037971862916));
#27845=CARTESIAN_POINT('Ctrl Pts',(-20.6276259765656,22.1885075318241,-29.8976365344838));
#27846=CARTESIAN_POINT('Ctrl Pts',(-20.5868430450439,22.2797174147473,-29.891475882676));
#27847=CARTESIAN_POINT('Ctrl Pts',(-20.5504124116753,22.3725102777079,-29.8853152308682));
#27848=CARTESIAN_POINT('Ctrl Pts',(-20.5139208169021,22.4654584161258,-29.8791442700992));
#27849=CARTESIAN_POINT('Ctrl Pts',(-20.481796207618,22.5599944141723,-29.8729733093301));
#27850=CARTESIAN_POINT('Ctrl Pts',(-20.4541521490144,22.6556688392038,-29.8668023485611));
#27851=CARTESIAN_POINT('Ctrl Pts',(-20.4330509200399,22.7286989242045,-29.8620919383407));
#27852=CARTESIAN_POINT('Ctrl Pts',(-20.4145592793517,22.8023919974991,-29.8573815281203));
#27853=CARTESIAN_POINT('Ctrl Pts',(-20.3987074968319,22.8765452838969,-29.8526711178999));
#27854=CARTESIAN_POINT('Ctrl Pts',(-20.3779367688915,22.9737089773633,-29.8464990265876));
#27855=CARTESIAN_POINT('Ctrl Pts',(-20.3616270767543,23.0720052543431,-29.8403269352752));
#27856=CARTESIAN_POINT('Ctrl Pts',(-20.3498969255981,23.1709880368763,-29.8341548439629));
#27857=CARTESIAN_POINT('Ctrl Pts',(-20.3381826676371,23.269836707525,-29.8279911152241));
#27858=CARTESIAN_POINT('Ctrl Pts',(-20.3310356685776,23.3693696073798,-29.8218273864853));
#27859=CARTESIAN_POINT('Ctrl Pts',(-20.3285237157046,23.4691291767217,-29.8156636577466));
#27860=CARTESIAN_POINT('Ctrl Pts',(-20.3260144240098,23.5687830601628,-29.8095064588999));
#27861=CARTESIAN_POINT('Ctrl Pts',(-20.3281304270622,23.6686627038138,-29.8033492600532));
#27862=CARTESIAN_POINT('Ctrl Pts',(-20.3348877544018,23.7683050745538,-29.7971920612065));
#27863=CARTESIAN_POINT('Ctrl Pts',(-20.3416401425449,23.8678746127632,-29.7910393628988));
#27864=CARTESIAN_POINT('Ctrl Pts',(-20.3530270807583,23.9672067907756,-29.7848866645911));
#27865=CARTESIAN_POINT('Ctrl Pts',(-20.369012520984,24.0658391459078,-29.7787339662834));
#27866=CARTESIAN_POINT('Ctrl Pts',(-20.3849918995079,24.1644340995105,-29.7725836010876));
#27867=CARTESIAN_POINT('Ctrl Pts',(-20.405566245794,24.2623293291983,-29.7664332358919));
#27868=CARTESIAN_POINT('Ctrl Pts',(-20.4306478192053,24.3590689511101,-29.7602828706961));
#27869=CARTESIAN_POINT('Ctrl Pts',(-20.4557265917072,24.4557977699156,-29.7541331923239));
#27870=CARTESIAN_POINT('Ctrl Pts',(-20.4853114816216,24.551370817013,-29.7479835139517));
#27871=CARTESIAN_POINT('Ctrl Pts',(-20.5192641723132,24.6453448236024,-29.7418338355795));
#27872=CARTESIAN_POINT('Ctrl Pts',(-20.5532221547131,24.7393334765431,-29.7356831987471));
#27873=CARTESIAN_POINT('Ctrl Pts',(-20.5915491424,24.8317221853703,-29.7295325619146));
#27874=CARTESIAN_POINT('Ctrl Pts',(-20.6340580807087,24.9220861537277,-29.7233819250821));
#27875=CARTESIAN_POINT('Ctrl Pts',(-20.6766124946516,25.0125467925487,-29.7172247083603));
#27876=CARTESIAN_POINT('Ctrl Pts',(-20.7233576076971,25.1009779716693,-29.7110674916385));
#27877=CARTESIAN_POINT('Ctrl Pts',(-20.7740596924203,25.1869781903385,-29.7049102749167));
#27878=CARTESIAN_POINT('Ctrl Pts',(-20.824790063629,25.2730263881774,-29.6987496231089));
#27879=CARTESIAN_POINT('Ctrl Pts',(-20.8794815650756,25.3566405611141,-29.692588971301));
#27880=CARTESIAN_POINT('Ctrl Pts',(-20.9378574558461,25.4374487404083,-29.6864283194932));
#27881=CARTESIAN_POINT('Ctrl Pts',(-20.9963310302405,25.5183921405221,-29.6802573587242));
#27882=CARTESIAN_POINT('Ctrl Pts',(-21.0585010383686,25.5965198279169,-29.6740863979551));
#27883=CARTESIAN_POINT('Ctrl Pts',(-21.1240507518066,25.6714933208953,-29.6679154371861));
#27884=CARTESIAN_POINT('Ctrl Pts',(-21.174086078829,25.7287219957807,-29.6632050269657));
#27885=CARTESIAN_POINT('Ctrl Pts',(-21.2260897821239,25.7841135535356,-29.6584946167454));
#27886=CARTESIAN_POINT('Ctrl Pts',(-21.2799076256754,25.8375329190133,-29.653784206525));
#27887=CARTESIAN_POINT('Ctrl Pts',(-21.3504158686518,25.9075191048615,-29.6476129680208));
#27888=CARTESIAN_POINT('Ctrl Pts',(-21.4242874215632,25.9743652245237,-29.6414417295167));
#27889=CARTESIAN_POINT('Ctrl Pts',(-21.5012111803779,26.0377305925212,-29.6352704910125));
#27890=CARTESIAN_POINT('Ctrl Pts',(-21.5780433761809,26.1010205361762,-29.6291065981866));
#27891=CARTESIAN_POINT('Ctrl Pts',(-21.6579202304885,26.1608376828121,-29.6229427053607));
#27892=CARTESIAN_POINT('Ctrl Pts',(-21.7404934092444,26.2168776424305,-29.6167788125348));
#27893=CARTESIAN_POINT('Ctrl Pts',(-21.8229734022357,26.2728543596432,-29.6106218758062));
#27894=CARTESIAN_POINT('Ctrl Pts',(-21.9081433105631,26.3250621247924,-29.6044649390776));
#27895=CARTESIAN_POINT('Ctrl Pts',(-21.9956222941264,26.3732371910468,-29.598308002349));
#27896=CARTESIAN_POINT('Ctrl Pts',(-22.021889173106,26.387702478406,-29.5964592896028));
#27897=CARTESIAN_POINT('Ctrl Pts',(-22.0483640244497,26.4018044680348,-29.5946105768567));
#27898=CARTESIAN_POINT('Ctrl Pts',(-22.0750360153461,26.4155367745563,-29.5927618641105));
#27899=CARTESIAN_POINT('Origin',(-23.5502525316942,23.5502525316942,-77.3107734492734));
#27900=CARTESIAN_POINT('',(-22.0750360120315,26.4155367728497,-28.0986394360247));
#27901=CARTESIAN_POINT('',(-22.0750360250495,26.4155367795522,-28.3456357132216));
#27902=CARTESIAN_POINT('',(-22.0750360153461,26.4155367745563,-77.3107734492734));
#27903=CARTESIAN_POINT('',(-26.7730017233255,23.5479699147772,-28.9373019452253));
#27904=CARTESIAN_POINT('Ctrl Pts',(-22.0750360120315,26.4155367728497,-28.0986394360247));
#27905=CARTESIAN_POINT('Ctrl Pts',(-22.0457737676643,26.4004708517544,-28.1005328265967));
#27906=CARTESIAN_POINT('Ctrl Pts',(-22.0167408821415,26.3849559218225,-28.1024119499114));
#27907=CARTESIAN_POINT('Ctrl Pts',(-21.6748533170991,26.1954628496327,-28.1246044605303));
#27908=CARTESIAN_POINT('Ctrl Pts',(-21.3928839179396,25.9710015176139,-28.1438902681475));
#27909=CARTESIAN_POINT('Ctrl Pts',(-21.1398241737672,25.6894988982981,-28.1667794881155));
#27910=CARTESIAN_POINT('Ctrl Pts',(-21.1262321418025,25.6740851533254,-28.1680281683821));
#27911=CARTESIAN_POINT('Ctrl Pts',(-21.108684928598,25.6537982414884,-28.1696660787883));
#27912=CARTESIAN_POINT('Ctrl Pts',(-21.1045950464036,25.6490417963526,-28.170049708029));
#27913=CARTESIAN_POINT('Ctrl Pts',(-21.0983191428002,25.6416998015274,-28.1706412827738));
#27914=CARTESIAN_POINT('Ctrl Pts',(-21.0961232492827,25.6391226787204,-28.170848820618));
#27915=CARTESIAN_POINT('Ctrl Pts',(-21.091788234588,25.6340187908414,-28.1712596231423));
#27916=CARTESIAN_POINT('Ctrl Pts',(-21.0896489373911,25.6314921801919,-28.1714628802191));
#27917=CARTESIAN_POINT('Ctrl Pts',(-21.0849647354103,25.62594259982,-28.1719090968935));
#27918=CARTESIAN_POINT('Ctrl Pts',(-21.0824214924024,25.6229182400776,-28.172152124204));
#27919=CARTESIAN_POINT('Ctrl Pts',(-21.0752520114677,25.6143605732085,-28.1728393777775));
#27920=CARTESIAN_POINT('Ctrl Pts',(-21.0706387987971,25.6088164283073,-28.1732841353436));
#27921=CARTESIAN_POINT('Ctrl Pts',(-21.060349706979,25.5963662613294,-28.1742818439563));
#27922=CARTESIAN_POINT('Ctrl Pts',(-21.0546838890198,25.5894520359693,-28.1748351998737));
#27923=CARTESIAN_POINT('Ctrl Pts',(-20.940071239815,25.448392557348,-28.1861101217549));
#27924=CARTESIAN_POINT('Ctrl Pts',(-20.8420786467419,25.3057463143876,-28.1972739626629));
#27925=CARTESIAN_POINT('Ctrl Pts',(-20.5967514026887,24.878826739896,-28.2300056570019));
#27926=CARTESIAN_POINT('Ctrl Pts',(-20.4796206664047,24.5795689191511,-28.2523197625039));
#27927=CARTESIAN_POINT('Ctrl Pts',(-20.40481865564,24.2521269563646,-28.2735771100213));
#27928=CARTESIAN_POINT('Ctrl Pts',(-20.4013172076754,24.2362469400368,-28.2746000397125));
#27929=CARTESIAN_POINT('Ctrl Pts',(-20.3971895140062,24.2168289031897,-28.2758405644299));
#27930=CARTESIAN_POINT('Ctrl Pts',(-20.3964488736767,24.2133158314876,-28.2760645865919));
#27931=CARTESIAN_POINT('Ctrl Pts',(-20.3952379829243,24.2075242958414,-28.2764332167125));
#27932=CARTESIAN_POINT('Ctrl Pts',(-20.394764328944,24.2052465601175,-28.2765780195515));
#27933=CARTESIAN_POINT('Ctrl Pts',(-20.3939150078018,24.2011399900831,-28.2768387700104));
#27934=CARTESIAN_POINT('Ctrl Pts',(-20.3935384643245,24.199311346555,-28.2769547679846));
#27935=CARTESIAN_POINT('Ctrl Pts',(-20.3927324527901,24.1953797444401,-28.2772039206444));
#27936=CARTESIAN_POINT('Ctrl Pts',(-20.3923034976272,24.1932766895667,-28.277337045227));
#27937=CARTESIAN_POINT('Ctrl Pts',(-20.3911351383668,24.1875191630919,-28.2777010940057));
#27938=CARTESIAN_POINT('Ctrl Pts',(-20.390399971814,24.1838638198422,-28.2779317741339));
#27939=CARTESIAN_POINT('Ctrl Pts',(-20.3866241110558,24.164919733748,-28.2791250121446));
#27940=CARTESIAN_POINT('Ctrl Pts',(-20.3836879595922,24.1496100101691,-28.2800816458943));
#27941=CARTESIAN_POINT('Ctrl Pts',(-20.3688848404305,24.0692766066483,-28.2850639507176));
#27942=CARTESIAN_POINT('Ctrl Pts',(-20.3589083696421,24.0039156259955,-28.288989741447));
#27943=CARTESIAN_POINT('Ctrl Pts',(-20.3414055106743,23.8596071438143,-28.2974681633333));
#27944=CARTESIAN_POINT('Ctrl Pts',(-20.3347676558959,23.7805954683339,-28.3019873584115));
#27945=CARTESIAN_POINT('Ctrl Pts',(-20.3176104769489,23.415212041599,-28.3226327839373));
#27946=CARTESIAN_POINT('Ctrl Pts',(-20.3423956066103,23.1285168796791,-28.3382485084046));
#27947=CARTESIAN_POINT('Ctrl Pts',(-20.4061312790621,22.8426796651111,-28.3555398922522));
#27948=CARTESIAN_POINT('Ctrl Pts',(-20.407530293231,22.8364915465942,-28.3559150095668));
#27949=CARTESIAN_POINT('Ctrl Pts',(-20.4098390087808,22.8264180262352,-28.3565269417755));
#27950=CARTESIAN_POINT('Ctrl Pts',(-20.4107376743249,22.8225300939839,-28.3567634329744));
#27951=CARTESIAN_POINT('Ctrl Pts',(-20.4131624841209,22.812127634291,-28.3573970294207));
#27952=CARTESIAN_POINT('Ctrl Pts',(-20.4147016935437,22.8056161968533,-28.3577945193885));
#27953=CARTESIAN_POINT('Ctrl Pts',(-20.4178650969972,22.7924175376324,-28.3586020675221));
#27954=CARTESIAN_POINT('Ctrl Pts',(-20.4194904543843,22.7857306330608,-28.3590121587173));
#27955=CARTESIAN_POINT('Ctrl Pts',(-20.4318543410835,22.7355648507611,-28.3620960318187));
#27956=CARTESIAN_POINT('Ctrl Pts',(-20.4434762945637,22.6923105764136,-28.3647965182208));
#27957=CARTESIAN_POINT('Ctrl Pts',(-20.458080002252,22.6421543994694,-28.3679810907144));
#27958=CARTESIAN_POINT('Ctrl Pts',(-20.4601894839292,22.6350020037225,-28.3684364875575));
#27959=CARTESIAN_POINT('Ctrl Pts',(-20.4635945384035,22.6236028091302,-28.3691643299522));
#27960=CARTESIAN_POINT('Ctrl Pts',(-20.4648741054659,22.6193512251498,-28.3694362509177));
#27961=CARTESIAN_POINT('Ctrl Pts',(-20.4671475010851,22.6118536522862,-28.3699165875322));
#27962=CARTESIAN_POINT('Ctrl Pts',(-20.4681376822445,22.6086065571885,-28.3701248832217));
#27963=CARTESIAN_POINT('Ctrl Pts',(-20.4701735865106,22.6019678431212,-28.3705512976928));
#27964=CARTESIAN_POINT('Ctrl Pts',(-20.4712197852755,22.5985763759219,-28.3707694318627));
#27965=CARTESIAN_POINT('Ctrl Pts',(-20.4737868247455,22.5903033355186,-28.3713022658019));
#27966=CARTESIAN_POINT('Ctrl Pts',(-20.4753136806577,22.5854236519577,-28.3716171631319));
#27967=CARTESIAN_POINT('Ctrl Pts',(-20.481322679037,22.5663786226375,-28.3728486068638));
#27968=CARTESIAN_POINT('Ctrl Pts',(-20.4858910908008,22.5522408798928,-28.3737679923199));
#27969=CARTESIAN_POINT('Ctrl Pts',(-20.497417591397,22.5173955230455,-28.3760472034784));
#27970=CARTESIAN_POINT('Ctrl Pts',(-20.5044887021416,22.4967263432852,-28.3774107401984));
#27971=CARTESIAN_POINT('Ctrl Pts',(-20.532596483792,22.4172148300085,-28.3827017580308));
#27972=CARTESIAN_POINT('Ctrl Pts',(-20.55513161223,22.3589203926956,-28.3866784342014));
#27973=CARTESIAN_POINT('Ctrl Pts',(-20.6410761734975,22.1544790325411,-28.4009806201322));
#27974=CARTESIAN_POINT('Ctrl Pts',(-20.7136011081862,22.012433146819,-28.4115913252341));
#27975=CARTESIAN_POINT('Ctrl Pts',(-20.9252502708133,21.6642252786945,-28.4390916016061));
#27976=CARTESIAN_POINT('Ctrl Pts',(-21.0782666922542,21.4676958156449,-28.4561251040388));
#27977=CARTESIAN_POINT('Ctrl Pts',(-21.2625359049252,21.2803006108625,-28.4727335983485));
#27978=CARTESIAN_POINT('Ctrl Pts',(-21.2728034451685,21.2699993078989,-28.4736476745489));
#27979=CARTESIAN_POINT('Ctrl Pts',(-21.285829001022,21.2571066696766,-28.474792652779));
#27980=CARTESIAN_POINT('Ctrl Pts',(-21.288522101492,21.2544504208411,-28.4750286027276));
#27981=CARTESIAN_POINT('Ctrl Pts',(-21.2927753915277,21.2502700793659,-28.4754000079284));
#27982=CARTESIAN_POINT('Ctrl Pts',(-21.2943324513777,21.2487428291979,-28.4755357128491));
#27983=CARTESIAN_POINT('Ctrl Pts',(-21.2972105638743,21.2459255446815,-28.475786071016));
#27984=CARTESIAN_POINT('Ctrl Pts',(-21.2985311669445,21.2446350726616,-28.475900758895));
#27985=CARTESIAN_POINT('Ctrl Pts',(-21.3014803658126,21.241758113757,-28.4761564652177));
#27986=CARTESIAN_POINT('Ctrl Pts',(-21.3031095279273,21.2401722187204,-28.476297436621));
#27987=CARTESIAN_POINT('Ctrl Pts',(-21.3078344902041,21.2355824695181,-28.4767054737042));
#27988=CARTESIAN_POINT('Ctrl Pts',(-21.3109346600731,21.232583090232,-28.476972187209));
#27989=CARTESIAN_POINT('Ctrl Pts',(-21.3322816495003,21.2120129364058,-28.4788018597472));
#27990=CARTESIAN_POINT('Ctrl Pts',(-21.3507297219677,21.1946509641895,-28.4803487599328));
#27991=CARTESIAN_POINT('Ctrl Pts',(-21.4080343618453,21.1419803023754,-28.4850568093903));
#27992=CARTESIAN_POINT('Ctrl Pts',(-21.4475522187311,21.1074005328722,-28.4881693969901));
#27993=CARTESIAN_POINT('Ctrl Pts',(-21.6076210183211,20.9740976309633,-28.5003382679784));
#27994=CARTESIAN_POINT('Ctrl Pts',(-21.734424714907,20.8832001422886,-28.5090316179169));
#27995=CARTESIAN_POINT('Ctrl Pts',(-22.0235578813535,20.7061558996501,-28.5279753231044));
#27996=CARTESIAN_POINT('Ctrl Pts',(-22.1876604078382,20.6239890641521,-28.5382073089231));
#27997=CARTESIAN_POINT('Ctrl Pts',(-22.4460779480476,20.5210718888121,-28.5544251766118));
#27998=CARTESIAN_POINT('Ctrl Pts',(-22.5358107410767,20.4898535339552,-28.5600698241396));
#27999=CARTESIAN_POINT('Ctrl Pts',(-22.6366378218943,20.4596973238734,-28.5664760012072));
#28000=CARTESIAN_POINT('Ctrl Pts',(-22.6465048792214,20.4567975849806,-28.5671035574248));
#28001=CARTESIAN_POINT('Ctrl Pts',(-22.6603503177924,20.4528005721681,-28.5679850933276));
#28002=CARTESIAN_POINT('Ctrl Pts',(-22.6643172574638,20.451663613897,-28.5682377764442));
#28003=CARTESIAN_POINT('Ctrl Pts',(-22.6715830818834,20.4495962610382,-28.5687007930918));
#28004=CARTESIAN_POINT('Ctrl Pts',(-22.6748812929801,20.4486635026506,-28.5689110492092));
#28005=CARTESIAN_POINT('Ctrl Pts',(-22.6812116091347,20.4468841443079,-28.5693147471649));
#28006=CARTESIAN_POINT('Ctrl Pts',(-22.6842434799975,20.4460367216741,-28.5695081618755));
#28007=CARTESIAN_POINT('Ctrl Pts',(-22.6918359285543,20.443926584322,-28.5699926803283));
#28008=CARTESIAN_POINT('Ctrl Pts',(-22.6963980438696,20.4426694726105,-28.5702839661719));
#28009=CARTESIAN_POINT('Ctrl Pts',(-22.7117232073031,20.4384828486854,-28.5712629763721));
#28010=CARTESIAN_POINT('Ctrl Pts',(-22.7224986013104,20.435599194055,-28.5719521897182));
#28011=CARTESIAN_POINT('Ctrl Pts',(-22.7480732931222,20.4288971163325,-28.5735901035087));
#28012=CARTESIAN_POINT('Ctrl Pts',(-22.762885109827,20.4251279438093,-28.5745403868792));
#28013=CARTESIAN_POINT('Ctrl Pts',(-22.8152588299014,20.4121963408617,-28.5779067108225));
#28014=CARTESIAN_POINT('Ctrl Pts',(-22.8529570386473,20.4036049212294,-28.5803409959292));
#28015=CARTESIAN_POINT('Ctrl Pts',(-22.9717341059481,20.3787748510699,-28.5880485090311));
#28016=CARTESIAN_POINT('Ctrl Pts',(-23.0532837118726,20.3649779230921,-28.5933960546017));
#28017=CARTESIAN_POINT('Ctrl Pts',(-23.2243120047308,20.3427702129441,-28.6047206496569));
#28018=CARTESIAN_POINT('Ctrl Pts',(-23.3137948937588,20.3349351179556,-28.6107075828226));
#28019=CARTESIAN_POINT('Ctrl Pts',(-23.651213964546,20.3195525459553,-28.6334266896517));
#28020=CARTESIAN_POINT('Ctrl Pts',(-23.8994266878082,20.33688921321,-28.6504978698463));
#28021=CARTESIAN_POINT('Ctrl Pts',(-24.1774287343905,20.3889268521848,-28.6686534037139));
#28022=CARTESIAN_POINT('Ctrl Pts',(-24.2115506383187,20.39588807887,-28.6708634308689));
#28023=CARTESIAN_POINT('Ctrl Pts',(-24.2500539190637,20.404395444659,-28.6733312249766));
#28024=CARTESIAN_POINT('Ctrl Pts',(-24.2545510434342,20.4053992122527,-28.6736190557927));
#28025=CARTESIAN_POINT('Ctrl Pts',(-24.2613561901461,20.4069334646038,-28.6740539798745));
#28026=CARTESIAN_POINT('Ctrl Pts',(-24.2636657819565,20.4074568487017,-28.6742014787334));
#28027=CARTESIAN_POINT('Ctrl Pts',(-24.2676825072062,20.408371747787,-28.6744578080761));
#28028=CARTESIAN_POINT('Ctrl Pts',(-24.2693898981495,20.4087621086226,-28.6745667053214));
#28029=CARTESIAN_POINT('Ctrl Pts',(-24.2729648554991,20.4095825184256,-28.6747945872698));
#28030=CARTESIAN_POINT('Ctrl Pts',(-24.2748323556039,20.4100128411563,-28.6749135554974));
#28031=CARTESIAN_POINT('Ctrl Pts',(-24.279301046538,20.4110467474254,-28.6751980574347));
#28032=CARTESIAN_POINT('Ctrl Pts',(-24.281901880967,20.4116519003913,-28.6753635000455));
#28033=CARTESIAN_POINT('Ctrl Pts',(-24.2907291271696,20.4137173613854,-28.675924543295));
#28034=CARTESIAN_POINT('Ctrl Pts',(-24.2969519949127,20.4151929826077,-28.6763192630331));
#28035=CARTESIAN_POINT('Ctrl Pts',(-24.3117396132708,20.4187460801285,-28.6772554492345));
#28036=CARTESIAN_POINT('Ctrl Pts',(-24.3203003678685,20.4208401961633,-28.6777959817824));
#28037=CARTESIAN_POINT('Ctrl Pts',(-24.4212888938915,20.4459833202594,-28.6841566350594));
#28038=CARTESIAN_POINT('Ctrl Pts',(-24.5126695466553,20.4730867865112,-28.6897556859943));
#28039=CARTESIAN_POINT('Ctrl Pts',(-24.7260409289243,20.5468108767779,-28.7027445753374));
#28040=CARTESIAN_POINT('Ctrl Pts',(-24.8466632624847,20.596870925378,-28.7100224867177));
#28041=CARTESIAN_POINT('Ctrl Pts',(-25.0222118266607,20.6825600099545,-28.7209374163615));
#28042=CARTESIAN_POINT('Ctrl Pts',(-25.0796271686613,20.712764624056,-28.7245613534846));
#28043=CARTESIAN_POINT('Ctrl Pts',(-25.2137529162196,20.7885786949616,-28.7332265286045));
#28044=CARTESIAN_POINT('Ctrl Pts',(-25.2895548991831,20.8356803928689,-28.738285974307));
#28045=CARTESIAN_POINT('Ctrl Pts',(-25.4617414420578,20.9528490235168,-28.7503097824543));
#28046=CARTESIAN_POINT('Ctrl Pts',(-25.5563820560106,21.0252309277073,-28.7573375949468));
#28047=CARTESIAN_POINT('Ctrl Pts',(-25.6548829332698,21.1096046956223,-28.7652293067485));
#28048=CARTESIAN_POINT('Ctrl Pts',(-25.6629368686961,21.1165730386487,-28.7658789716184));
#28049=CARTESIAN_POINT('Ctrl Pts',(-25.6741934702381,21.1264103467309,-28.7667932378602));
#28050=CARTESIAN_POINT('Ctrl Pts',(-25.6774252222514,21.1292460483723,-28.7670564522302));
#28051=CARTESIAN_POINT('Ctrl Pts',(-25.6830214968313,21.1341763569442,-28.7675135214894));
#28052=CARTESIAN_POINT('Ctrl Pts',(-25.6853886381995,21.1362679941637,-28.7677072519067));
#28053=CARTESIAN_POINT('Ctrl Pts',(-25.6901450071799,21.1404832535143,-28.7680973218956));
#28054=CARTESIAN_POINT('Ctrl Pts',(-25.6925341575451,21.1426069564222,-28.7682936647256));
#28055=CARTESIAN_POINT('Ctrl Pts',(-25.6973962959695,21.1469418520064,-28.7686940759141));
#28056=CARTESIAN_POINT('Ctrl Pts',(-25.6998690367107,21.1491533149193,-28.7688981555311));
#28057=CARTESIAN_POINT('Ctrl Pts',(-25.7055712828378,21.1542689117148,-28.7693697970876));
#28058=CARTESIAN_POINT('Ctrl Pts',(-25.708798335423,21.1571757591795,-28.7696374736355));
#28059=CARTESIAN_POINT('Ctrl Pts',(-25.7260470158395,21.1727762101977,-28.7710723125631));
#28060=CARTESIAN_POINT('Ctrl Pts',(-25.7399623349701,21.1855863291616,-28.7722444173748));
#28061=CARTESIAN_POINT('Ctrl Pts',(-25.8184708034618,21.259146629123,-28.778941702782));
#28062=CARTESIAN_POINT('Ctrl Pts',(-25.8806422236163,21.3224146156167,-28.7845758035015));
#28063=CARTESIAN_POINT('Ctrl Pts',(-25.9834335687823,21.4360350660689,-28.794494905584));
#28064=CARTESIAN_POINT('Ctrl Pts',(-26.0252946668328,21.4851977972338,-28.7987276692833));
#28065=CARTESIAN_POINT('Ctrl Pts',(-26.2620045503497,21.7807395581866,-28.8238093022325));
#28066=CARTESIAN_POINT('Ctrl Pts',(-26.4214492098276,22.0532594467184,-28.8457136511841));
#28067=CARTESIAN_POINT('Ctrl Pts',(-26.5415064264269,22.3508509004986,-28.8662754692804));
#28068=CARTESIAN_POINT('Ctrl Pts',(-26.5440395804668,22.3571878880069,-28.8667117733235));
#28069=CARTESIAN_POINT('Ctrl Pts',(-26.5560983834144,22.3876346694204,-28.8688004823148));
#28070=CARTESIAN_POINT('Ctrl Pts',(-26.5653533788868,22.4118516517457,-28.8704391043862));
#28071=CARTESIAN_POINT('Ctrl Pts',(-26.5759117200941,22.4405114090173,-28.8723494948835));
#28072=CARTESIAN_POINT('Ctrl Pts',(-26.5774986402483,22.4448476816115,-28.8726377669867));
#28073=CARTESIAN_POINT('Ctrl Pts',(-26.5798854598636,22.4514133747103,-28.8730730637447));
#28074=CARTESIAN_POINT('Ctrl Pts',(-26.5806922216405,22.4536402674668,-28.8732204977814));
#28075=CARTESIAN_POINT('Ctrl Pts',(-26.5821317838291,22.4576275903347,-28.8734841119724));
#28076=CARTESIAN_POINT('Ctrl Pts',(-26.5827655055024,22.4593876794983,-28.8736003474431));
#28077=CARTESIAN_POINT('Ctrl Pts',(-26.5841134085846,22.4631415771758,-28.8738479766281));
#28078=CARTESIAN_POINT('Ctrl Pts',(-26.5848271553455,22.4651355327885,-28.8739793438489));
#28079=CARTESIAN_POINT('Ctrl Pts',(-26.5867490358632,22.4705213120552,-28.8743337297367));
#28080=CARTESIAN_POINT('Ctrl Pts',(-26.5879534563827,22.4739144719093,-28.8745565256626));
#28081=CARTESIAN_POINT('Ctrl Pts',(-26.5938300578524,22.4905587898351,-28.8756471023783));
#28082=CARTESIAN_POINT('Ctrl Pts',(-26.5984213256531,22.5038386533231,-28.8765101090521));
#28083=CARTESIAN_POINT('Ctrl Pts',(-26.636521800248,22.6164200410221,-28.8837696013276));
#28084=CARTESIAN_POINT('Ctrl Pts',(-26.6652594053402,22.7172829949885,-28.8899018075406));
#28085=CARTESIAN_POINT('Ctrl Pts',(-26.744656370487,23.0582574373607,-28.9099530865801));
#28086=CARTESIAN_POINT('Ctrl Pts',(-26.7728280024169,23.3026992723123,-28.923287335281));
#28087=CARTESIAN_POINT('Ctrl Pts',(-26.7730017233255,23.5479699147772,-28.9373019452253));
#28088=CARTESIAN_POINT('Ctrl Pts',(-26.7730017261855,23.5479739563721,-28.9373021761595));
#28089=CARTESIAN_POINT('Ctrl Pts',(-26.77310750083,23.6975784688127,-28.9458504874898));
#28090=CARTESIAN_POINT('Ctrl Pts',(-26.7627962705988,23.8469938290537,-28.95460972371));
#28091=CARTESIAN_POINT('Ctrl Pts',(-26.741199785725,24.0019385244878,-28.9641350168917));
#28092=CARTESIAN_POINT('Ctrl Pts',(-26.7402311793074,24.0087291840131,-28.9645533451948));
#28093=CARTESIAN_POINT('Ctrl Pts',(-26.7386138167336,24.0198148236502,-28.9652376989888));
#28094=CARTESIAN_POINT('Ctrl Pts',(-26.7379780403255,24.0241116999024,-28.9655033132474));
#28095=CARTESIAN_POINT('Ctrl Pts',(-26.7368413629611,24.031688081907,-28.9659722812069));
#28096=CARTESIAN_POINT('Ctrl Pts',(-26.7363440803388,24.0349681308747,-28.9661755199251));
#28097=CARTESIAN_POINT('Ctrl Pts',(-26.7353577173884,24.0414070247902,-28.9665748982821));
#28098=CARTESIAN_POINT('Ctrl Pts',(-26.7348690002649,24.0445659221799,-28.9667710261764));
#28099=CARTESIAN_POINT('Ctrl Pts',(-26.7338880026587,24.05084490862,-28.9671612610362));
#28100=CARTESIAN_POINT('Ctrl Pts',(-26.7333958330707,24.0539650117883,-28.9673553642859));
#28101=CARTESIAN_POINT('Ctrl Pts',(-26.7322230130486,24.0613297258003,-28.967813980105));
#28102=CARTESIAN_POINT('Ctrl Pts',(-26.7315384563999,24.0655737010028,-28.9680786166914));
#28103=CARTESIAN_POINT('Ctrl Pts',(-26.7291290238785,24.0803234289836,-28.9689995929475));
#28104=CARTESIAN_POINT('Ctrl Pts',(-26.7273605963087,24.0908219075442,-28.9696573173102));
#28105=CARTESIAN_POINT('Ctrl Pts',(-26.7052103282031,24.2184552440559,-28.9776806382628));
#28106=CARTESIAN_POINT('Ctrl Pts',(-26.6784160768633,24.3343701443852,-28.9852512008797));
#28107=CARTESIAN_POINT('Ctrl Pts',(-26.6409941573877,24.4633081625523,-28.9940089287639));
#28108=CARTESIAN_POINT('Ctrl Pts',(-26.6365990521609,24.4780561349063,-28.9950156244242));
#28109=CARTESIAN_POINT('Ctrl Pts',(-26.6264426625231,24.5112654569427,-28.9972936394615));
#28110=CARTESIAN_POINT('Ctrl Pts',(-26.6206205161857,24.5297074730995,-28.9985665023647));
#28111=CARTESIAN_POINT('Ctrl Pts',(-26.528013106308,24.814105188315,-29.0183145735201));
#28112=CARTESIAN_POINT('Ctrl Pts',(-26.4071385078111,25.0676723411625,-29.0376800869498));
#28113=CARTESIAN_POINT('Ctrl Pts',(-26.2177285793629,25.3600599865555,-29.0605674288933));
#28114=CARTESIAN_POINT('Ctrl Pts',(-26.1785644887213,25.4164811813935,-29.0650052950319));
#28115=CARTESIAN_POINT('Ctrl Pts',(-26.1310546949927,25.4804595640769,-29.0700239003928));
#28116=CARTESIAN_POINT('Ctrl Pts',(-26.1244395149726,25.4892730002468,-29.0707149285074));
#28117=CARTESIAN_POINT('Ctrl Pts',(-26.1157831302581,25.5006835653382,-29.0716089842846));
#28118=CARTESIAN_POINT('Ctrl Pts',(-26.1137830614142,25.5033115918857,-29.0718148570516));
#28119=CARTESIAN_POINT('Ctrl Pts',(-26.1105342614802,25.5075668226656,-29.0721481264205));
#28120=CARTESIAN_POINT('Ctrl Pts',(-26.1092880169629,25.5091959088007,-29.0722756986184));
#28121=CARTESIAN_POINT('Ctrl Pts',(-26.1068926580093,25.5123209263377,-29.0725203799484));
#28122=CARTESIAN_POINT('Ctrl Pts',(-26.1057437888333,25.5138170341852,-29.0726375055454));
#28123=CARTESIAN_POINT('Ctrl Pts',(-26.1030992701564,25.5172545903056,-29.0729065858502));
#28124=CARTESIAN_POINT('Ctrl Pts',(-26.1016027155292,25.519195346557,-29.0730584759672));
#28125=CARTESIAN_POINT('Ctrl Pts',(-26.0968474818594,25.5253474855905,-29.0735398880642));
#28126=CARTESIAN_POINT('Ctrl Pts',(-26.0935805566796,25.529552528006,-29.0738688258547));
#28127=CARTESIAN_POINT('Ctrl Pts',(-26.0819098674858,25.544497921155,-29.0750376022537));
#28128=CARTESIAN_POINT('Ctrl Pts',(-26.0734482253182,25.5551931907378,-29.075873413166));
#28129=CARTESIAN_POINT('Ctrl Pts',(-25.8818857597726,25.7941889934861,-29.0945452236154));
#28130=CARTESIAN_POINT('Ctrl Pts',(-25.6685672168057,25.9965910085693,-29.1103398070627));
#28131=CARTESIAN_POINT('Ctrl Pts',(-25.3874961015267,26.1985536749705,-29.1298247459396));
#28132=CARTESIAN_POINT('Ctrl Pts',(-25.3434127134965,26.2285988847945,-29.132843821961));
#28133=CARTESIAN_POINT('Ctrl Pts',(-25.2093666288013,26.315165306086,-29.1419562739163));
#28134=CARTESIAN_POINT('Ctrl Pts',(-25.1173409524393,26.3683428325062,-29.1481261796362));
#28135=CARTESIAN_POINT('Ctrl Pts',(-24.9945922910384,26.431399944741,-29.1563520597774));
#28136=CARTESIAN_POINT('Ctrl Pts',(-24.9661084387559,26.4455037640826,-29.1582603601898));
#28137=CARTESIAN_POINT('Ctrl Pts',(-24.9254978612916,26.4648695470193,-29.1609824763531));
#28138=CARTESIAN_POINT('Ctrl Pts',(-24.9135396301744,26.4704820332343,-29.1617841962552));
#28139=CARTESIAN_POINT('Ctrl Pts',(-24.8924822323475,26.4802075994966,-29.1631963986441));
#28140=CARTESIAN_POINT('Ctrl Pts',(-24.8833977688225,26.4843522303837,-29.163805786847));
#28141=CARTESIAN_POINT('Ctrl Pts',(-24.8710533577024,26.4899149913908,-29.164634095819));
#28142=CARTESIAN_POINT('Ctrl Pts',(-24.8678100415018,26.4913700756089,-29.1648517446707));
#28143=CARTESIAN_POINT('Ctrl Pts',(-24.8617043644207,26.4940972056145,-29.1652615229575));
#28144=CARTESIAN_POINT('Ctrl Pts',(-24.858842541338,26.4953704512827,-29.1654536109171));
#28145=CARTESIAN_POINT('Ctrl Pts',(-24.8528765790236,26.4980143382492,-29.1658540922756));
#28146=CARTESIAN_POINT('Ctrl Pts',(-24.8497721235563,26.4993842525726,-29.1660625103156));
#28147=CARTESIAN_POINT('Ctrl Pts',(-24.8426086295729,26.5025318061895,-29.1665434884385));
#28148=CARTESIAN_POINT('Ctrl Pts',(-24.8385480835539,26.5043059789229,-29.166816166856));
#28149=CARTESIAN_POINT('Ctrl Pts',(-24.8258990503452,26.5098016753919,-29.1676657259697));
#28150=CARTESIAN_POINT('Ctrl Pts',(-24.8172980579573,26.5134941360726,-29.1682435987626));
#28151=CARTESIAN_POINT('Ctrl Pts',(-24.744167543798,26.5445129239736,-29.1731588563472));
#28152=CARTESIAN_POINT('Ctrl Pts',(-24.6787830639527,26.5697634102216,-29.1775663504581));
#28153=CARTESIAN_POINT('Ctrl Pts',(-24.6048937059054,26.5955631446181,-29.1825671672736));
#28154=CARTESIAN_POINT('Ctrl Pts',(-24.5971456932678,26.5982353797177,-29.1830917848841));
#28155=CARTESIAN_POINT('Ctrl Pts',(-24.5373087534623,26.6186176470773,-29.1871451528167));
#28156=CARTESIAN_POINT('Ctrl Pts',(-24.4847867009972,26.6350199136976,-29.1907138161595));
#28157=CARTESIAN_POINT('Ctrl Pts',(-24.2781412461083,26.693792047651,-29.2047915390161));
#28158=CARTESIAN_POINT('Ctrl Pts',(-24.1213830391341,26.7260144948076,-29.2155646733074));
#28159=CARTESIAN_POINT('Ctrl Pts',(-23.9441831418336,26.7488916604126,-29.2276587873675));
#28160=CARTESIAN_POINT('Ctrl Pts',(-23.925448596786,26.7511432694058,-29.228936183964));
#28161=CARTESIAN_POINT('Ctrl Pts',(-23.8849509625642,26.7556500416624,-29.2316937821234));
#28162=CARTESIAN_POINT('Ctrl Pts',(-23.8631824172781,26.7578483806063,-29.2331737678876));
#28163=CARTESIAN_POINT('Ctrl Pts',(-23.815533891302,26.7621705823165,-29.2364065824248));
#28164=CARTESIAN_POINT('Ctrl Pts',(-23.7896470491529,26.7642036905725,-29.2381586321875));
#28165=CARTESIAN_POINT('Ctrl Pts',(-23.7316354157073,26.7680550344347,-29.2420722144512));
#28166=CARTESIAN_POINT('Ctrl Pts',(-23.6995018850785,26.7697054976405,-29.2442313072394));
#28167=CARTESIAN_POINT('Ctrl Pts',(-23.54952267875,26.7751584691819,-29.2542546933018));
#28168=CARTESIAN_POINT('Ctrl Pts',(-23.4315345725427,26.772973742257,-29.2619875291052));
#28169=CARTESIAN_POINT('Ctrl Pts',(-23.3076494984088,26.7638643378415,-29.2697725269664));
#28170=CARTESIAN_POINT('Ctrl Pts',(-23.3013820339088,26.7633850451904,-29.2701654658527));
#28171=CARTESIAN_POINT('Ctrl Pts',(-23.2924727293388,26.7626774983935,-29.2707226998974));
#28172=CARTESIAN_POINT('Ctrl Pts',(-23.2898297581368,26.7624643199034,-29.2708878378797));
#28173=CARTESIAN_POINT('Ctrl Pts',(-23.2852804824809,26.7620917298774,-29.2711717942256));
#28174=CARTESIAN_POINT('Ctrl Pts',(-23.2833740543012,26.7619338826732,-29.2712907014308));
#28175=CARTESIAN_POINT('Ctrl Pts',(-23.2797184055553,26.761627927185,-29.2715185402341));
#28176=CARTESIAN_POINT('Ctrl Pts',(-23.2779691683028,26.7614800873536,-29.2716274870229));
#28177=CARTESIAN_POINT('Ctrl Pts',(-23.2738446755678,26.7611281043468,-29.2718841963246));
#28178=CARTESIAN_POINT('Ctrl Pts',(-23.2714695201314,26.7609227543324,-29.2720318902262));
#28179=CARTESIAN_POINT('Ctrl Pts',(-23.2644429821229,26.7603074015115,-29.2724684228279));
#28180=CARTESIAN_POINT('Ctrl Pts',(-23.2597922347245,26.7598899228019,-29.2727568410163));
#28181=CARTESIAN_POINT('Ctrl Pts',(-23.2188591733074,26.7561258304405,-29.2752909141835));
#28182=CARTESIAN_POINT('Ctrl Pts',(-23.1826332768724,26.7521740678932,-29.2775030777286));
#28183=CARTESIAN_POINT('Ctrl Pts',(-22.9025418799797,26.7168032448063,-29.2944242968928));
#28184=CARTESIAN_POINT('Ctrl Pts',(-22.662894899956,26.6581784939642,-29.3078710662029));
#28185=CARTESIAN_POINT('Ctrl Pts',(-22.3199191577746,26.5313152572039,-29.3283726114739));
#28186=CARTESIAN_POINT('Ctrl Pts',(-22.2100241677656,26.4835510573287,-29.3351413443454));
#28187=CARTESIAN_POINT('Ctrl Pts',(-22.0936865702591,26.4250817291775,-29.3426915969777));
#28188=CARTESIAN_POINT('Ctrl Pts',(-22.0843494206542,26.4203318622999,-29.3433003194745));
#28189=CARTESIAN_POINT('Ctrl Pts',(-22.0750360135777,26.4155367736458,-29.3439103255379));
#28190=CARTESIAN_POINT('',(-26.7730017063021,23.5525590581545,-29.1857734493121));
#28191=CARTESIAN_POINT('Ctrl Pts',(-22.0750360153461,26.4155367745563,-29.5927618641105));
#28192=CARTESIAN_POINT('Ctrl Pts',(-22.1637904272254,26.4612327555499,-29.5866100394058));
#28193=CARTESIAN_POINT('Ctrl Pts',(-22.2547296296025,26.5028317038812,-29.5804582147011));
#28194=CARTESIAN_POINT('Ctrl Pts',(-22.3474377521427,26.5401278081217,-29.5743063899964));
#28195=CARTESIAN_POINT('Ctrl Pts',(-22.4401181667825,26.5774127655855,-29.5681564039025));
#28196=CARTESIAN_POINT('Ctrl Pts',(-22.5345660482642,26.6103972724394,-29.5620064178085));
#28197=CARTESIAN_POINT('Ctrl Pts',(-22.6303447948988,26.6389233329101,-29.5558564317145));
#28198=CARTESIAN_POINT('Ctrl Pts',(-22.7261205394837,26.6674484992718,-29.5497066383832));
#28199=CARTESIAN_POINT('Ctrl Pts',(-22.8232266497658,26.6915153735237,-29.5435568450518));
#28200=CARTESIAN_POINT('Ctrl Pts',(-22.9212115556172,26.7110158909029,-29.5374070517205));
#28201=CARTESIAN_POINT('Ctrl Pts',(-23.0192196038505,26.7305210139753,-29.5312558059117));
#28202=CARTESIAN_POINT('Ctrl Pts',(-23.1181064339784,26.7454575528111,-29.5251045601029));
#28203=CARTESIAN_POINT('Ctrl Pts',(-23.2174114836804,26.7557687770527,-29.5189533142941));
#28204=CARTESIAN_POINT('Ctrl Pts',(-23.3168270587088,26.7660914775628,-29.5127952222227));
#28205=CARTESIAN_POINT('Ctrl Pts',(-23.4166613497563,26.7717785427884,-29.5066371301513));
#28206=CARTESIAN_POINT('Ctrl Pts',(-23.5164500562438,26.7728252547143,-29.5004790380799));
#28207=CARTESIAN_POINT('Ctrl Pts',(-23.6163016224669,26.7738726259938,-29.4943170668517));
#28208=CARTESIAN_POINT('Ctrl Pts',(-23.7161071133172,26.7702738400485,-29.4881550956234));
#28209=CARTESIAN_POINT('Ctrl Pts',(-23.8154056779686,26.7620762148251,-29.4819931243952));
#28210=CARTESIAN_POINT('Ctrl Pts',(-23.9148615618508,26.7538656020616,-29.475821390724));
#28211=CARTESIAN_POINT('Ctrl Pts',(-24.0138084862309,26.7410416609189,-29.4696496570529));
#28212=CARTESIAN_POINT('Ctrl Pts',(-24.1117942094486,26.7237030995532,-29.4634779233817));
#28213=CARTESIAN_POINT('Ctrl Pts',(-24.1572044138707,26.7156677696078,-29.4606177139711));
#28214=CARTESIAN_POINT('Ctrl Pts',(-24.2024083687602,26.706663527161,-29.4577575045606));
#28215=CARTESIAN_POINT('Ctrl Pts',(-24.2473622296468,26.6967038075795,-29.45489729515));
#28216=CARTESIAN_POINT('Ctrl Pts',(-24.3443688800026,26.6752115705164,-29.4487252038377));
#28217=CARTESIAN_POINT('Ctrl Pts',(-24.4405515237555,26.6491911330412,-29.4425531125254));
#28218=CARTESIAN_POINT('Ctrl Pts',(-24.53545518344,26.6187201129948,-29.436381021213));
#28219=CARTESIAN_POINT('Ctrl Pts',(-24.6302302580479,26.5882903781682,-29.4302172924743));
#28220=CARTESIAN_POINT('Ctrl Pts',(-24.7237293829445,26.5534221778618,-29.4240535637355));
#28221=CARTESIAN_POINT('Ctrl Pts',(-24.8155082173733,26.5142440317422,-29.4178898349967));
#28222=CARTESIAN_POINT('Ctrl Pts',(-24.9071898207412,26.4751073911913,-29.41173263615));
#28223=CARTESIAN_POINT('Ctrl Pts',(-24.9971543595918,26.431670052021,-29.4055754373033));
#28224=CARTESIAN_POINT('Ctrl Pts',(-25.0849740268791,26.3841098842646,-29.3994182384567));
#28225=CARTESIAN_POINT('Ctrl Pts',(-25.172729503315,26.3365844801069,-29.3932655401489));
#28226=CARTESIAN_POINT('Ctrl Pts',(-25.2583428443512,26.2849424450272,-29.3871128418412));
#28227=CARTESIAN_POINT('Ctrl Pts',(-25.3414084066746,26.2294087783553,-29.3809601435335));
#28228=CARTESIAN_POINT('Ctrl Pts',(-25.4244424704185,26.1738961701289,-29.3748097783378));
#28229=CARTESIAN_POINT('Ctrl Pts',(-25.5049303143946,26.1144951037006,-29.368659413142));
#28230=CARTESIAN_POINT('Ctrl Pts',(-25.5824937638322,26.0514748602564,-29.3625090479463));
#28231=CARTESIAN_POINT('Ctrl Pts',(-25.6600485516049,25.9884616544084,-29.3563593695741));
#28232=CARTESIAN_POINT('Ctrl Pts',(-25.7346792569647,25.9218303490014,-29.3502096912019));
#28233=CARTESIAN_POINT('Ctrl Pts',(-25.8060401997706,25.8518909826796,-29.3440600128297));
#28234=CARTESIAN_POINT('Ctrl Pts',(-25.8774122645609,25.7819407159336,-29.3379093759972));
#28235=CARTESIAN_POINT('Ctrl Pts',(-25.9455132443089,25.7086816682928,-29.3317587391648));
#28236=CARTESIAN_POINT('Ctrl Pts',(-26.0100345170859,25.6324605296719,-29.3256081023323));
#28237=CARTESIAN_POINT('Ctrl Pts',(-26.0746248140709,25.5561578504443,-29.3194508856105));
#28238=CARTESIAN_POINT('Ctrl Pts',(-26.1356274756683,25.476887084633,-29.3132936688887));
#28239=CARTESIAN_POINT('Ctrl Pts',(-26.1927744666104,25.3950276903482,-29.3071364521669));
#28240=CARTESIAN_POINT('Ctrl Pts',(-26.2499533396248,25.3131226270425,-29.300975800359));
#28241=CARTESIAN_POINT('Ctrl Pts',(-26.3032720263459,25.2286264265793,-29.2948151485512));
#28242=CARTESIAN_POINT('Ctrl Pts',(-26.3525072295006,25.1419453950072,-29.2886544967434));
#28243=CARTESIAN_POINT('Ctrl Pts',(-26.4018248206584,25.0551193152454,-29.2824835359744));
#28244=CARTESIAN_POINT('Ctrl Pts',(-26.4470450824199,24.9661014890839,-29.2763125752054));
#28245=CARTESIAN_POINT('Ctrl Pts',(-26.4879917950637,24.8753206744542,-29.2701416144363));
#28246=CARTESIAN_POINT('Ctrl Pts',(-26.519247189636,24.8060259741559,-29.265431204216));
#28247=CARTESIAN_POINT('Ctrl Pts',(-26.5480135503193,24.7357045242288,-29.2607207939956));
#28248=CARTESIAN_POINT('Ctrl Pts',(-26.5742321263537,24.6645527486836,-29.2560103837753));
#28249=CARTESIAN_POINT('Ctrl Pts',(-26.6138607220893,24.5570089619713,-29.2488907392101));
#28250=CARTESIAN_POINT('Ctrl Pts',(-26.647783099162,24.447255320658,-29.2417710946449));
#28251=CARTESIAN_POINT('Ctrl Pts',(-26.6757817560599,24.3358635233027,-29.2346514500797));
#28252=CARTESIAN_POINT('Ctrl Pts',(-26.7036600285425,24.2249506716497,-29.2275624174918));
#28253=CARTESIAN_POINT('Ctrl Pts',(-26.7256653011929,24.1124138660151,-29.2204733849039));
#28254=CARTESIAN_POINT('Ctrl Pts',(-26.7416295934255,23.9988392149064,-29.2133843523159));
#28255=CARTESIAN_POINT('Ctrl Pts',(-26.7574726370541,23.8861271618817,-29.2063491608437));
#28256=CARTESIAN_POINT('Ctrl Pts',(-26.7673660173076,23.7723931300587,-29.1993139693714));
#28257=CARTESIAN_POINT('Ctrl Pts',(-26.7711931727418,23.6582291465142,-29.1922787778991));
#28258=CARTESIAN_POINT('Ctrl Pts',(-26.7723728091336,23.6230406123812,-29.1901103350368));
#28259=CARTESIAN_POINT('Ctrl Pts',(-26.7729764761766,23.5878113596244,-29.1879418921745));
#28260=CARTESIAN_POINT('Ctrl Pts',(-26.7730017063021,23.5525590581545,-29.1857734493121));
#28261=CARTESIAN_POINT('Ctrl Pts',(-26.7730017875139,23.5524426489476,-29.1878050506611));
#28262=CARTESIAN_POINT('Ctrl Pts',(-26.7730978322047,23.4111132496054,-29.1797069801023));
#28263=CARTESIAN_POINT('Ctrl Pts',(-26.7638973695217,23.2699447972146,-29.1714120560357));
#28264=CARTESIAN_POINT('Ctrl Pts',(-26.744572087701,23.1230677348811,-29.1623918435185));
#28265=CARTESIAN_POINT('Ctrl Pts',(-26.7436589419758,23.1162942685426,-29.1619750092687));
#28266=CARTESIAN_POINT('Ctrl Pts',(-26.7421316500873,23.1052311455476,-29.1612927794928));
#28267=CARTESIAN_POINT('Ctrl Pts',(-26.7415303834496,23.1009397084099,-29.1610277915846));
#28268=CARTESIAN_POINT('Ctrl Pts',(-26.7404540131282,23.0933684618979,-29.1605596629691));
#28269=CARTESIAN_POINT('Ctrl Pts',(-26.7399825013429,23.0900881415331,-29.1603566362779));
#28270=CARTESIAN_POINT('Ctrl Pts',(-26.7390458587803,23.0836425069241,-29.1599572952329));
#28271=CARTESIAN_POINT('Ctrl Pts',(-26.7385810726079,23.0804771458343,-29.1597609920217));
#28272=CARTESIAN_POINT('Ctrl Pts',(-26.7376474138155,23.0741838055142,-29.1593703190914));
#28273=CARTESIAN_POINT('Ctrl Pts',(-26.7371786481747,23.0710558136392,-29.1591759529613));
#28274=CARTESIAN_POINT('Ctrl Pts',(-26.7360595035004,23.0636622325974,-29.1587160834287));
#28275=CARTESIAN_POINT('Ctrl Pts',(-26.735405162214,23.0593972568973,-29.1584504543809));
#28276=CARTESIAN_POINT('Ctrl Pts',(-26.7334352255732,23.0467270823126,-29.1576602775376));
#28277=CARTESIAN_POINT('Ctrl Pts',(-26.7320949185329,23.0383258144043,-29.1571349449975));
#28278=CARTESIAN_POINT('Ctrl Pts',(-26.7195282007226,22.9615118130368,-29.1523189045252));
#28279=CARTESIAN_POINT('Ctrl Pts',(-26.7061310172942,22.8934773202314,-29.147959382976));
#28280=CARTESIAN_POINT('Ctrl Pts',(-26.6774694265848,22.7692147556738,-29.1398137491908));
#28281=CARTESIAN_POINT('Ctrl Pts',(-26.6628540108267,22.7128655940036,-29.1360493975091));
#28282=CARTESIAN_POINT('Ctrl Pts',(-26.6414100372519,22.6385343577541,-29.1309907238798));
#28283=CARTESIAN_POINT('Ctrl Pts',(-26.6359344826545,22.6201710142091,-29.1297333745749));
#28284=CARTESIAN_POINT('Ctrl Pts',(-26.5623348694739,22.3811460790395,-29.1132691276442));
#28285=CARTESIAN_POINT('Ctrl Pts',(-26.4708490317124,22.1683884474793,-29.0974506762419));
#28286=CARTESIAN_POINT('Ctrl Pts',(-26.2920295268063,21.8512804912174,-29.0730389994483));
#28287=CARTESIAN_POINT('Ctrl Pts',(-26.219491580603,21.7394461910802,-29.0642607777098));
#28288=CARTESIAN_POINT('Ctrl Pts',(-26.1367677658436,21.627730648971,-29.0555536027452));
#28289=CARTESIAN_POINT('Ctrl Pts',(-26.1332910408018,21.6230619578884,-29.0551898483074));
#28290=CARTESIAN_POINT('Ctrl Pts',(-26.1282612931955,21.6163458660896,-29.0546667867535));
#28291=CARTESIAN_POINT('Ctrl Pts',(-26.1267184672577,21.6142908976119,-29.0545067709204));
#28292=CARTESIAN_POINT('Ctrl Pts',(-26.1240314701585,21.6107208503455,-29.0542288327711));
#28293=CARTESIAN_POINT('Ctrl Pts',(-26.1228884166142,21.6092049354887,-29.0541108314192));
#28294=CARTESIAN_POINT('Ctrl Pts',(-26.1206737563305,21.6062732511622,-29.053882658039));
#28295=CARTESIAN_POINT('Ctrl Pts',(-26.1196023218151,21.6048573607219,-29.0537724742252));
#28296=CARTESIAN_POINT('Ctrl Pts',(-26.1170430173746,21.6014810668913,-29.0535097670928));
#28297=CARTESIAN_POINT('Ctrl Pts',(-26.1155540682241,21.5995214774018,-29.053357320312));
#28298=CARTESIAN_POINT('Ctrl Pts',(-26.1110494180498,21.5936070337708,-29.0528972814162));
#28299=CARTESIAN_POINT('Ctrl Pts',(-26.1080267874823,21.5896574294555,-29.0525901761172));
#28300=CARTESIAN_POINT('Ctrl Pts',(-26.0772325074866,21.5496116446586,-29.0494772548016));
#28301=CARTESIAN_POINT('Ctrl Pts',(-26.0487060704095,21.5140987572732,-29.0467239433665));
#28302=CARTESIAN_POINT('Ctrl Pts',(-26.0175118019993,21.4769078405047,-29.0438339126906));
#28303=CARTESIAN_POINT('Ctrl Pts',(-26.015585750564,21.4746180177553,-29.04365594797));
#28304=CARTESIAN_POINT('Ctrl Pts',(-26.0117202351808,21.4700353974643,-29.0432997250141));
#28305=CARTESIAN_POINT('Ctrl Pts',(-26.0097807499415,21.4677426218444,-29.0431214682556));
#28306=CARTESIAN_POINT('Ctrl Pts',(-26.0047167776538,21.4617731546945,-29.0426572673003));
#28307=CARTESIAN_POINT('Ctrl Pts',(-26.0015872231578,21.4581007509231,-29.0423716006928));
#28308=CARTESIAN_POINT('Ctrl Pts',(-25.9950613792114,21.4504776857515,-29.0417783993475));
#28309=CARTESIAN_POINT('Ctrl Pts',(-25.9916637312353,21.4465282009115,-29.041470938331));
#28310=CARTESIAN_POINT('Ctrl Pts',(-25.8155682578971,21.2428329530368,-29.0256060609946));
#28311=CARTESIAN_POINT('Ctrl Pts',(-25.6189684505117,21.0650389092865,-29.011311710947));
#28312=CARTESIAN_POINT('Ctrl Pts',(-25.3508928804503,20.8767071381769,-28.9927839516359));
#28313=CARTESIAN_POINT('Ctrl Pts',(-25.2978622993952,20.8417455230738,-28.9891641270716));
#28314=CARTESIAN_POINT('Ctrl Pts',(-25.1737167013367,20.7650642010329,-28.9807431975298));
#28315=CARTESIAN_POINT('Ctrl Pts',(-25.1019673969194,20.7244624990995,-28.9759140970834));
#28316=CARTESIAN_POINT('Ctrl Pts',(-24.9908675854954,20.667100962717,-28.9684399780985));
#28317=CARTESIAN_POINT('Ctrl Pts',(-24.9526074542006,20.6482988606401,-28.9658668952078));
#28318=CARTESIAN_POINT('Ctrl Pts',(-24.9071202726928,20.6270548078539,-28.9628048494863));
#28319=CARTESIAN_POINT('Ctrl Pts',(-24.9002423026352,20.6238720683855,-28.9623417722362));
#28320=CARTESIAN_POINT('Ctrl Pts',(-24.8903390209827,20.6193317277861,-28.9616748783384));
#28321=CARTESIAN_POINT('Ctrl Pts',(-24.8873227039497,20.617954471829,-28.9614717402185));
#28322=CARTESIAN_POINT('Ctrl Pts',(-24.8813931506945,20.6152580782002,-28.961072369919));
#28323=CARTESIAN_POINT('Ctrl Pts',(-24.8784800653019,20.613938616521,-28.9608761491836));
#28324=CARTESIAN_POINT('Ctrl Pts',(-24.8726837850013,20.6113236223774,-28.9604856849874));
#28325=CARTESIAN_POINT('Ctrl Pts',(-24.8698006381139,20.6100279912099,-28.9602914451794));
#28326=CARTESIAN_POINT('Ctrl Pts',(-24.8629844746599,20.6069769825097,-28.9598321908792));
#28327=CARTESIAN_POINT('Ctrl Pts',(-24.8590498428713,20.6052252465089,-28.9595670515512));
#28328=CARTESIAN_POINT('Ctrl Pts',(-24.845334809303,20.599152094943,-28.9586427205044));
#28329=CARTESIAN_POINT('Ctrl Pts',(-24.8355365031388,20.5948715068701,-28.9579821307434));
#28330=CARTESIAN_POINT('Ctrl Pts',(-24.714536864437,20.5427259140448,-28.949821262496));
#28331=CARTESIAN_POINT('Ctrl Pts',(-24.6007588445094,20.5011207606099,-28.9421083247538));
#28332=CARTESIAN_POINT('Ctrl Pts',(-24.3327012309122,20.4198866280059,-28.9238223284591));
#28333=CARTESIAN_POINT('Ctrl Pts',(-24.1772886262071,20.3850932526665,-28.9131300683707));
#28334=CARTESIAN_POINT('Ctrl Pts',(-24.0019307036954,20.3592595124698,-28.901136047765));
#28335=CARTESIAN_POINT('Ctrl Pts',(-23.9838806593071,20.3567566000239,-28.8999025020582));
#28336=CARTESIAN_POINT('Ctrl Pts',(-23.9450401234547,20.3517061403668,-28.8972511733862));
#28337=CARTESIAN_POINT('Ctrl Pts',(-23.9242439999695,20.3492079139723,-28.8958334595716));
#28338=CARTESIAN_POINT('Ctrl Pts',(-23.8790394740103,20.3442240555681,-28.892757217207));
#28339=CARTESIAN_POINT('Ctrl Pts',(-23.8546239296,20.3418140471437,-28.8910991318945));
#28340=CARTESIAN_POINT('Ctrl Pts',(-23.748166612865,20.3325319994976,-28.8838893005205));
#28341=CARTESIAN_POINT('Ctrl Pts',(-23.6659019234487,20.3285259790501,-28.8783682569127));
#28342=CARTESIAN_POINT('Ctrl Pts',(-23.5087905137374,20.3269016204149,-28.8680139259658));
#28343=CARTESIAN_POINT('Ctrl Pts',(-23.433999207243,20.328731553804,-28.8631671609071));
#28344=CARTESIAN_POINT('Ctrl Pts',(-23.3477463155057,20.3338502686176,-28.8577226574796));
#28345=CARTESIAN_POINT('Ctrl Pts',(-23.3361632639188,20.3346004857259,-28.8569945425464));
#28346=CARTESIAN_POINT('Ctrl Pts',(-23.3212266133829,20.335648975901,-28.8560597580245));
#28347=CARTESIAN_POINT('Ctrl Pts',(-23.3178692701128,20.3358899335792,-28.8558499143927));
#28348=CARTESIAN_POINT('Ctrl Pts',(-23.3124524438862,20.336287232171,-28.855511789468));
#28349=CARTESIAN_POINT('Ctrl Pts',(-23.3103927342609,20.3364402929451,-28.855383323093));
#28350=CARTESIAN_POINT('Ctrl Pts',(-23.3064563567602,20.3367366176271,-28.8551380060102));
#28351=CARTESIAN_POINT('Ctrl Pts',(-23.3045796810269,20.3368795444213,-28.8550211373786));
#28352=CARTESIAN_POINT('Ctrl Pts',(-23.3002884806279,20.3372101415671,-28.8547541028295));
#28353=CARTESIAN_POINT('Ctrl Pts',(-23.2978740442107,20.3373988894118,-28.8546039987214));
#28354=CARTESIAN_POINT('Ctrl Pts',(-23.2914856275526,20.3379055477404,-28.85420720605));
#28355=CARTESIAN_POINT('Ctrl Pts',(-23.2875120046881,20.338228112131,-28.8539607797343));
#28356=CARTESIAN_POINT('Ctrl Pts',(-23.2616566056573,20.340375260849,-28.8523597604061));
#28357=CARTESIAN_POINT('Ctrl Pts',(-23.2397926723898,20.3424161204473,-28.8510171683383));
#28358=CARTESIAN_POINT('Ctrl Pts',(-23.212129218147,20.3452838204643,-28.8493307999366));
#28359=CARTESIAN_POINT('Ctrl Pts',(-23.2063094478701,20.345903148232,-28.848976719384));
#28360=CARTESIAN_POINT('Ctrl Pts',(-23.1972182861481,20.3468956635614,-28.8484246431366));
#28361=CARTESIAN_POINT('Ctrl Pts',(-23.19394575607,20.3472580132822,-28.8482261236804));
#28362=CARTESIAN_POINT('Ctrl Pts',(-22.9372563832404,20.3760781168246,-28.8326708500973));
#28363=CARTESIAN_POINT('Ctrl Pts',(-22.688072301185,20.4345129588063,-28.8187512422246));
#28364=CARTESIAN_POINT('Ctrl Pts',(-22.3377715968158,20.5619661320368,-28.7978450164624));
#28365=CARTESIAN_POINT('Ctrl Pts',(-22.2294787618548,20.6082261051504,-28.7911886111177));
#28366=CARTESIAN_POINT('Ctrl Pts',(-22.0572184094176,20.6932424326598,-28.780047070728));
#28367=CARTESIAN_POINT('Ctrl Pts',(-21.9916385807724,20.7284837749121,-28.7756673038632));
#28368=CARTESIAN_POINT('Ctrl Pts',(-21.9057698650325,20.7785350649673,-28.7697122790831));
#28369=CARTESIAN_POINT('Ctrl Pts',(-21.8843462381465,20.7913583466394,-28.768207687774));
#28370=CARTESIAN_POINT('Ctrl Pts',(-21.8536701141095,20.8102073697275,-28.7660249302696));
#28371=CARTESIAN_POINT('Ctrl Pts',(-21.8442958509804,20.8160339617762,-28.7653540360045));
#28372=CARTESIAN_POINT('Ctrl Pts',(-21.8276914572692,20.8264730885345,-28.7641587096565));
#28373=CARTESIAN_POINT('Ctrl Pts',(-21.8204494252323,20.8310665651339,-28.7636349843473));
#28374=CARTESIAN_POINT('Ctrl Pts',(-21.8096553014972,20.8379736349204,-28.7628507796498));
#28375=CARTESIAN_POINT('Ctrl Pts',(-21.8060892591045,20.8402654450218,-28.7625911125401));
#28376=CARTESIAN_POINT('Ctrl Pts',(-21.7998068596887,20.8443205296667,-28.7621326025134));
#28377=CARTESIAN_POINT('Ctrl Pts',(-21.7970886138773,20.8460808789732,-28.7619338691828));
#28378=CARTESIAN_POINT('Ctrl Pts',(-21.791672304423,20.8496001068204,-28.7615371833804));
#28379=CARTESIAN_POINT('Ctrl Pts',(-21.7889742146708,20.851358938834,-28.7613392327984));
#28380=CARTESIAN_POINT('Ctrl Pts',(-21.7824847433342,20.8556031740254,-28.7608622866739));
#28381=CARTESIAN_POINT('Ctrl Pts',(-21.7786959680197,20.8580925335286,-28.7605831426332));
#28382=CARTESIAN_POINT('Ctrl Pts',(-21.767083188397,20.8657576705535,-28.7597254339427));
#28383=CARTESIAN_POINT('Ctrl Pts',(-21.7592765729207,20.870959587936,-28.7591458847152));
#28384=CARTESIAN_POINT('Ctrl Pts',(-21.668391809895,20.9320951000328,-28.7523638350446));
#28385=CARTESIAN_POINT('Ctrl Pts',(-21.5879501309053,20.9918323543447,-28.7460164624855));
#28386=CARTESIAN_POINT('Ctrl Pts',(-21.3073057961999,21.2212738091584,-28.7225475816191));
#28387=CARTESIAN_POINT('Ctrl Pts',(-21.1252441958995,21.4115033235543,-28.7046161273414));
#28388=CARTESIAN_POINT('Ctrl Pts',(-20.9468391219765,21.6503473015461,-28.6845635052697));
#28389=CARTESIAN_POINT('Ctrl Pts',(-20.9258775914347,21.679408458616,-28.6821622980976));
#28390=CARTESIAN_POINT('Ctrl Pts',(-20.8759840157796,21.7510703115994,-28.6763440716493));
#28391=CARTESIAN_POINT('Ctrl Pts',(-20.8475789100175,21.794028015299,-28.6729424642591));
#28392=CARTESIAN_POINT('Ctrl Pts',(-20.7981253501123,21.8728613128955,-28.6668769919587));
#28393=CARTESIAN_POINT('Ctrl Pts',(-20.7767186442866,21.9084987533439,-28.6641978893532));
#28394=CARTESIAN_POINT('Ctrl Pts',(-20.7456497249463,21.9625646759178,-28.6602378257455));
#28395=CARTESIAN_POINT('Ctrl Pts',(-20.735467407305,21.9806874998422,-28.6589276349974));
#28396=CARTESIAN_POINT('Ctrl Pts',(-20.7234969515208,22.0024841068837,-28.6573734971663));
#28397=CARTESIAN_POINT('Ctrl Pts',(-20.7215398484717,22.0060638246068,-28.6571189501576));
#28398=CARTESIAN_POINT('Ctrl Pts',(-20.7185265993363,22.0116002803441,-28.6567263448873));
#28399=CARTESIAN_POINT('Ctrl Pts',(-20.7174656808087,22.0135543947478,-28.6565879810183));
#28400=CARTESIAN_POINT('Ctrl Pts',(-20.7156071445307,22.016986112899,-28.6563453598468));
#28401=CARTESIAN_POINT('Ctrl Pts',(-20.714808662411,22.0184632360818,-28.6562410469593));
#28402=CARTESIAN_POINT('Ctrl Pts',(-20.7131188323505,22.0215951249323,-28.6560201287088));
#28403=CARTESIAN_POINT('Ctrl Pts',(-20.7122277801546,22.0232500415547,-28.6559035426119));
#28404=CARTESIAN_POINT('Ctrl Pts',(-20.7096972042968,22.0279598479969,-28.6555721655314));
#28405=CARTESIAN_POINT('Ctrl Pts',(-20.7080611554445,22.0310166172015,-28.6553575976185));
#28406=CARTESIAN_POINT('Ctrl Pts',(-20.7011449269301,22.0439890688454,-28.6544491112207));
#28407=CARTESIAN_POINT('Ctrl Pts',(-20.6959115969542,22.0539298391925,-28.6537581502749));
#28408=CARTESIAN_POINT('Ctrl Pts',(-20.6050295978417,22.228773111704,-28.6416927508709));
#28409=CARTESIAN_POINT('Ctrl Pts',(-20.5337346761073,22.400779568126,-28.6311755735118));
#28410=CARTESIAN_POINT('Ctrl Pts',(-20.389182143201,22.8576051345413,-28.6043264995181));
#28411=CARTESIAN_POINT('Ctrl Pts',(-20.3392943206521,23.147941418624,-28.5881471858314));
#28412=CARTESIAN_POINT('Ctrl Pts',(-20.3287100462353,23.4600136944735,-28.5693493968427));
#28413=CARTESIAN_POINT('Ctrl Pts',(-20.3282337608482,23.4790201658713,-28.5681997495099));
#28414=CARTESIAN_POINT('Ctrl Pts',(-20.3277795947686,23.5070436185374,-28.5664972167989));
#28415=CARTESIAN_POINT('Ctrl Pts',(-20.3276713315218,23.516058305461,-28.5659484005843));
#28416=CARTESIAN_POINT('Ctrl Pts',(-20.3275441137625,23.5323406855082,-28.5649550188217));
#28417=CARTESIAN_POINT('Ctrl Pts',(-20.3275119155594,23.5396082378426,-28.5645108702719));
#28418=CARTESIAN_POINT('Ctrl Pts',(-20.3275001498358,23.5508373964193,-28.5638234208343));
#28419=CARTESIAN_POINT('Ctrl Pts',(-20.3275033037355,23.5547989927359,-28.5635806626337));
#28420=CARTESIAN_POINT('Ctrl Pts',(-20.3275217297088,23.5617785305081,-28.5631525640811));
#28421=CARTESIAN_POINT('Ctrl Pts',(-20.3275339364467,23.564796481065,-28.5629673201907));
#28422=CARTESIAN_POINT('Ctrl Pts',(-20.3275709938322,23.5715967200886,-28.5625496125246));
#28423=CARTESIAN_POINT('Ctrl Pts',(-20.3275982638655,23.5753789859878,-28.5623170730586));
#28424=CARTESIAN_POINT('Ctrl Pts',(-20.3276892751585,23.5855245596403,-28.5616927342797));
#28425=CARTESIAN_POINT('Ctrl Pts',(-20.3277652053051,23.5918877170724,-28.5613005528182));
#28426=CARTESIAN_POINT('Ctrl Pts',(-20.3281774760633,23.6195658935915,-28.5595919943545));
#28427=CARTESIAN_POINT('Ctrl Pts',(-20.3287064500831,23.6408771152084,-28.5582695834757));
#28428=CARTESIAN_POINT('Ctrl Pts',(-20.3299018714579,23.6752760136589,-28.5561235542816));
#28429=CARTESIAN_POINT('Ctrl Pts',(-20.3304367923625,23.68836785485,-28.5553041093124));
#28430=CARTESIAN_POINT('Ctrl Pts',(-20.3313207361289,23.707187490914,-28.554122219375));
#28431=CARTESIAN_POINT('Ctrl Pts',(-20.3316052489282,23.7129183067775,-28.5537617947625));
#28432=CARTESIAN_POINT('Ctrl Pts',(-20.3323601474497,23.7273457816071,-28.5528530887614));
#28433=CARTESIAN_POINT('Ctrl Pts',(-20.3328504829972,23.7360413106617,-28.5523041906726));
#28434=CARTESIAN_POINT('Ctrl Pts',(-20.3334693737092,23.7462782142428,-28.5516565524522));
#28435=CARTESIAN_POINT('Ctrl Pts',(-20.3335638018583,23.7478216817356,-28.55155886629));
#28436=CARTESIAN_POINT('Ctrl Pts',(-20.3532645815474,24.0660808513355,-28.5314082498986));
#28437=CARTESIAN_POINT('Ctrl Pts',(-20.4195393688342,24.3781153774592,-28.5097640448727));
#28438=CARTESIAN_POINT('Ctrl Pts',(-20.5820092018874,24.8142198702219,-28.478450090031));
#28439=CARTESIAN_POINT('Ctrl Pts',(-20.6432743851476,24.9493851986291,-28.4686253341562));
#28440=CARTESIAN_POINT('Ctrl Pts',(-20.7165361692649,25.08524649767,-28.4589536416341));
#28441=CARTESIAN_POINT('Ctrl Pts',(-20.7194516232791,25.0906164876008,-28.4585717185055));
#28442=CARTESIAN_POINT('Ctrl Pts',(-20.7236395539426,25.0982782120599,-28.458027347838));
#28443=CARTESIAN_POINT('Ctrl Pts',(-20.7248995581056,25.1005766938669,-28.457864109409));
#28444=CARTESIAN_POINT('Ctrl Pts',(-20.7270813490224,25.1045451921739,-28.4575823910894));
#28445=CARTESIAN_POINT('Ctrl Pts',(-20.728001815516,25.1062159297837,-28.4574638260143));
#28446=CARTESIAN_POINT('Ctrl Pts',(-20.7297756467799,25.1094288561361,-28.4572358935095));
#28447=CARTESIAN_POINT('Ctrl Pts',(-20.7306287916589,25.1109711590266,-28.4571265121238));
#28448=CARTESIAN_POINT('Ctrl Pts',(-20.7326520855379,25.1146217663981,-28.456867684811));
#28449=CARTESIAN_POINT('Ctrl Pts',(-20.7338233382753,25.1167294626494,-28.45671831027));
#28450=CARTESIAN_POINT('Ctrl Pts',(-20.737321466759,25.1230078194232,-28.4562735318395));
#28451=CARTESIAN_POINT('Ctrl Pts',(-20.7396552621872,25.1271746478721,-28.4559785711346));
#28452=CARTESIAN_POINT('Ctrl Pts',(-20.7613322996444,25.1656764860252,-28.4532550994881));
#28453=CARTESIAN_POINT('Ctrl Pts',(-20.7812956043339,25.1996610595797,-28.4508658195019));
#28454=CARTESIAN_POINT('Ctrl Pts',(-20.803234317856,25.2354870070532,-28.4483534852167));
#28455=CARTESIAN_POINT('Ctrl Pts',(-20.8045929490365,25.2376996450414,-28.4481983479061));
#28456=CARTESIAN_POINT('Ctrl Pts',(-20.8066545361579,25.2410480206287,-28.4479636154648));
#28457=CARTESIAN_POINT('Ctrl Pts',(-20.8073555233706,25.242184961862,-28.4478839183709));
#28458=CARTESIAN_POINT('Ctrl Pts',(-20.809763756394,25.2460854795346,-28.4476105211679));
#28459=CARTESIAN_POINT('Ctrl Pts',(-20.8114744791637,25.2488469193212,-28.4474170002688));
#28460=CARTESIAN_POINT('Ctrl Pts',(-20.8181204991471,25.259538747383,-28.4466678385315));
#28461=CARTESIAN_POINT('Ctrl Pts',(-20.8230861360351,25.2674503259406,-28.4461137380288));
#28462=CARTESIAN_POINT('Ctrl Pts',(-20.9067392098813,25.3994538047281,-28.4368709550051));
#28463=CARTESIAN_POINT('Ctrl Pts',(-20.9937964206793,25.5180555047688,-28.4285955642676));
#28464=CARTESIAN_POINT('Ctrl Pts',(-21.2232943471133,25.7896499278746,-28.4086932174755));
#28465=CARTESIAN_POINT('Ctrl Pts',(-21.3730785653031,25.9355285963084,-28.3971377995706));
#28466=CARTESIAN_POINT('Ctrl Pts',(-21.6062643214353,26.1222463147299,-28.3797478217694));
#28467=CARTESIAN_POINT('Ctrl Pts',(-21.6789512606303,26.1756042134507,-28.3744052371149));
#28468=CARTESIAN_POINT('Ctrl Pts',(-21.7629865289072,26.2320282364482,-28.3682690981738));
#28469=CARTESIAN_POINT('Ctrl Pts',(-21.7722308742147,26.2381661605273,-28.3675946460266));
#28470=CARTESIAN_POINT('Ctrl Pts',(-21.7887106377258,26.2489859358252,-28.3663932032738));
#28471=CARTESIAN_POINT('Ctrl Pts',(-21.7959335169198,26.2536867592846,-28.3658669280088));
#28472=CARTESIAN_POINT('Ctrl Pts',(-21.8067422644647,26.2606597946396,-28.3650797949164));
#28473=CARTESIAN_POINT('Ctrl Pts',(-21.8103139494466,26.2629540104226,-28.3648197591482));
#28474=CARTESIAN_POINT('Ctrl Pts',(-21.8166167627524,26.2669849547422,-28.3643609986512));
#28475=CARTESIAN_POINT('Ctrl Pts',(-21.8193459995205,26.268724642007,-28.3641623844399));
#28476=CARTESIAN_POINT('Ctrl Pts',(-21.8247940363646,26.272185833388,-28.3637659885104));
#28477=CARTESIAN_POINT('Ctrl Pts',(-21.8275128036597,26.2739073826803,-28.3635682087591));
#28478=CARTESIAN_POINT('Ctrl Pts',(-21.8340592725838,26.2780389455092,-28.3630920629843));
#28479=CARTESIAN_POINT('Ctrl Pts',(-21.8378894710184,26.2804449736511,-28.3628135495515));
#28480=CARTESIAN_POINT('Ctrl Pts',(-21.8496437075298,26.2877942054343,-28.3619590420407));
#28481=CARTESIAN_POINT('Ctrl Pts',(-21.8575841259507,26.2927110005755,-28.3613820733927));
#28482=CARTESIAN_POINT('Ctrl Pts',(-21.9338952363816,26.339506015508,-28.3558396228713));
#28483=CARTESIAN_POINT('Ctrl Pts',(-22.0037740529195,26.3788469336282,-28.3507823253816));
#28484=CARTESIAN_POINT('Ctrl Pts',(-22.0750360250495,26.4155367795522,-28.3456357132216));
#28485=CARTESIAN_POINT('Origin',(-23.5502525316942,23.5502525316942,-77.3107734492734));
#28486=CARTESIAN_POINT('',(-22.0750359193537,26.4155367251338,-26.8471666088699));
#28487=CARTESIAN_POINT('',(-22.075036065511,26.4155368003841,-27.0910469152906));
#28488=CARTESIAN_POINT('',(-22.0750360153461,26.4155367745563,-77.3107734492734));
#28489=CARTESIAN_POINT('Ctrl Pts',(-22.0750359193537,26.4155367251338,-26.8471666088699));
#28490=CARTESIAN_POINT('Ctrl Pts',(-22.0260367658724,26.390309082664,-26.8508920404459));
#28491=CARTESIAN_POINT('Ctrl Pts',(-21.9776797507882,26.3638219780101,-26.8546086240552));
#28492=CARTESIAN_POINT('Ctrl Pts',(-21.8781595643101,26.3059413752287,-26.8623136408831));
#28493=CARTESIAN_POINT('Ctrl Pts',(-21.8271551177872,26.2743398862597,-26.8662947903275));
#28494=CARTESIAN_POINT('Ctrl Pts',(-21.738688681582,26.2160480245785,-26.8732220726755));
#28495=CARTESIAN_POINT('Ctrl Pts',(-21.7008600709887,26.189945166315,-26.8761915947194));
#28496=CARTESIAN_POINT('Ctrl Pts',(-21.6516467702822,26.1544090410951,-26.8800514157724));
#28497=CARTESIAN_POINT('Ctrl Pts',(-21.6397520395683,26.1456952398626,-26.8809840513181));
#28498=CARTESIAN_POINT('Ctrl Pts',(-21.620268116247,26.1312152481546,-26.8825107149833));
#28499=CARTESIAN_POINT('Ctrl Pts',(-21.612644096435,26.1254965870606,-26.8831078348526));
#28500=CARTESIAN_POINT('Ctrl Pts',(-21.6031705806084,26.118324759632,-26.8838493652823));
#28501=CARTESIAN_POINT('Ctrl Pts',(-21.6012972651902,26.1169033574592,-26.8839959755264));
#28502=CARTESIAN_POINT('Ctrl Pts',(-21.5976569202388,26.1141349154017,-26.88428083274));
#28503=CARTESIAN_POINT('Ctrl Pts',(-21.5958897253786,26.1127880964664,-26.8844190951337));
#28504=CARTESIAN_POINT('Ctrl Pts',(-21.5927896310873,26.1104203726923,-26.8846616028622));
#28505=CARTESIAN_POINT('Ctrl Pts',(-21.5914561420157,26.1094002580186,-26.8847659036036));
#28506=CARTESIAN_POINT('Ctrl Pts',(-21.5886308242752,26.1072353973833,-26.8849868629702));
#28507=CARTESIAN_POINT('Ctrl Pts',(-21.5871392046254,26.1060903911004,-26.8851035022259));
#28508=CARTESIAN_POINT('Ctrl Pts',(-21.5828965887288,26.1028277428331,-26.8854352174195));
#28509=CARTESIAN_POINT('Ctrl Pts',(-21.5801480001898,26.1007069520001,-26.8856500695361));
#28510=CARTESIAN_POINT('Ctrl Pts',(-21.5684890295062,26.09168088228,-26.8865612413888));
#28511=CARTESIAN_POINT('Ctrl Pts',(-21.5596113436682,26.0847332100937,-26.8872545818093));
#28512=CARTESIAN_POINT('Ctrl Pts',(-21.41087107141,25.9670654949637,-26.8988666419973));
#28513=CARTESIAN_POINT('Ctrl Pts',(-21.2803791194128,25.8449491498019,-26.9089956370651));
#28514=CARTESIAN_POINT('Ctrl Pts',(-21.0456744101102,25.5855828122911,-26.928618496798));
#28515=CARTESIAN_POINT('Ctrl Pts',(-20.9410178326508,25.4495612646637,-26.9380960457788));
#28516=CARTESIAN_POINT('Ctrl Pts',(-20.8092052211597,25.2466497277178,-26.9519072738813));
#28517=CARTESIAN_POINT('Ctrl Pts',(-20.7726966531897,25.1861884320487,-26.955982907929));
#28518=CARTESIAN_POINT('Ctrl Pts',(-20.7002369447813,25.0567615842695,-26.9646796958136));
#28519=CARTESIAN_POINT('Ctrl Pts',(-20.6647375153548,24.9875972882442,-26.9693116594756));
#28520=CARTESIAN_POINT('Ctrl Pts',(-20.62625933619,24.9054464025964,-26.974823299408));
#28521=CARTESIAN_POINT('Ctrl Pts',(-20.6208154210256,24.8936381211498,-26.9756157458324));
#28522=CARTESIAN_POINT('Ctrl Pts',(-20.6133390157772,24.8771596491318,-26.9767220076204));
#28523=CARTESIAN_POINT('Ctrl Pts',(-20.6112458609511,24.8725169860069,-26.977033731123));
#28524=CARTESIAN_POINT('Ctrl Pts',(-20.6077316579981,24.8646728370825,-26.9775604945887));
#28525=CARTESIAN_POINT('Ctrl Pts',(-20.6063048038795,24.861473949722,-26.9777753345429));
#28526=CARTESIAN_POINT('Ctrl Pts',(-20.6034922756459,24.8551407643858,-26.978200724581));
#28527=CARTESIAN_POINT('Ctrl Pts',(-20.6021063800053,24.8520065693578,-26.978411266713));
#28528=CARTESIAN_POINT('Ctrl Pts',(-20.5990636132989,24.8450955877511,-26.9788755714642));
#28529=CARTESIAN_POINT('Ctrl Pts',(-20.5974089894626,24.8413178231235,-26.9791294107488));
#28530=CARTESIAN_POINT('Ctrl Pts',(-20.5916595658092,24.8281221219862,-26.9800162000431));
#28531=CARTESIAN_POINT('Ctrl Pts',(-20.5876025676836,24.8186878727369,-26.9806504412069));
#28532=CARTESIAN_POINT('Ctrl Pts',(-20.5467000557884,24.7223053009467,-26.9871326715368));
#28533=CARTESIAN_POINT('Ctrl Pts',(-20.5136514437285,24.6338050129039,-26.9931089683476));
#28534=CARTESIAN_POINT('Ctrl Pts',(-20.4700071163023,24.4991605575395,-27.0022507094504));
#28535=CARTESIAN_POINT('Ctrl Pts',(-20.456461892712,24.4540209799194,-27.0053231697352));
#28536=CARTESIAN_POINT('Ctrl Pts',(-20.4362526953945,24.3808845304795,-27.0103115760106));
#28537=CARTESIAN_POINT('Ctrl Pts',(-20.4289651590741,24.3530660650558,-27.0122113264497));
#28538=CARTESIAN_POINT('Ctrl Pts',(-20.3862460394477,24.180613230437,-27.0239992133313));
#28539=CARTESIAN_POINT('Ctrl Pts',(-20.3605039071274,24.0337714989359,-27.0340954346083));
#28540=CARTESIAN_POINT('Ctrl Pts',(-20.3330041524413,23.7709970912481,-27.0519681521743));
#28541=CARTESIAN_POINT('Ctrl Pts',(-20.3271653359956,23.6557389800221,-27.0597386029792));
#28542=CARTESIAN_POINT('Ctrl Pts',(-20.3276739831064,23.4891930462134,-27.0706769641778));
#28543=CARTESIAN_POINT('Ctrl Pts',(-20.3290513344615,23.4379838597281,-27.0740001600598));
#28544=CARTESIAN_POINT('Ctrl Pts',(-20.3329625754352,23.3609537968624,-27.0789177859605));
#28545=CARTESIAN_POINT('Ctrl Pts',(-20.3345882289384,23.3350970764512,-27.0805546623936));
#28546=CARTESIAN_POINT('Ctrl Pts',(-20.3368491931666,23.3049460358877,-27.0824450548671));
#28547=CARTESIAN_POINT('Ctrl Pts',(-20.3371815178791,23.3006309107382,-27.0827151631127));
#28548=CARTESIAN_POINT('Ctrl Pts',(-20.3377033941646,23.2940282747255,-27.083127774201));
#28549=CARTESIAN_POINT('Ctrl Pts',(-20.3378866970975,23.2917402965951,-27.0832706282321));
#28550=CARTESIAN_POINT('Ctrl Pts',(-20.338208834002,23.2877726522134,-27.0835181343936));
#28551=CARTESIAN_POINT('Ctrl Pts',(-20.3383465409453,23.2860929025797,-27.0836228503175));
#28552=CARTESIAN_POINT('Ctrl Pts',(-20.3386372136275,23.2825811081201,-27.0838416321398));
#28553=CARTESIAN_POINT('Ctrl Pts',(-20.3387904288674,23.2807490912958,-27.0839556834204));
#28554=CARTESIAN_POINT('Ctrl Pts',(-20.3392199648168,23.2756654483533,-27.0842719384555));
#28555=CARTESIAN_POINT('Ctrl Pts',(-20.3394996578835,23.2724140976612,-27.0844739509926));
#28556=CARTESIAN_POINT('Ctrl Pts',(-20.3406266450549,23.2595421896845,-27.0852727167983));
#28557=CARTESIAN_POINT('Ctrl Pts',(-20.3415122555193,23.2499249092361,-27.0858673265037));
#28558=CARTESIAN_POINT('Ctrl Pts',(-20.3576985785761,23.082400492013,-27.0961889709261));
#28559=CARTESIAN_POINT('Ctrl Pts',(-20.3845980169538,22.9258065010839,-27.1052850566293));
#28560=CARTESIAN_POINT('Ctrl Pts',(-20.4804163682251,22.5408641719855,-27.1276378505912));
#28561=CARTESIAN_POINT('Ctrl Pts',(-20.5633040467645,22.3170065845988,-27.1406808360339));
#28562=CARTESIAN_POINT('Ctrl Pts',(-20.7033516195836,22.038045098057,-27.1587878107292));
#28563=CARTESIAN_POINT('Ctrl Pts',(-20.7388964210788,21.9729473214874,-27.1631517063108));
#28564=CARTESIAN_POINT('Ctrl Pts',(-20.7959756707622,21.8764794275465,-27.1698679657483));
#28565=CARTESIAN_POINT('Ctrl Pts',(-20.8158732438125,21.8441672018477,-27.1721615386944));
#28566=CARTESIAN_POINT('Ctrl Pts',(-20.8402917118767,21.8060381767722,-27.1749237051255));
#28567=CARTESIAN_POINT('Ctrl Pts',(-20.8442684038102,21.7998750698024,-27.1753719389211));
#28568=CARTESIAN_POINT('Ctrl Pts',(-20.8504618681525,21.7903479417083,-27.176067590275));
#28569=CARTESIAN_POINT('Ctrl Pts',(-20.852663985154,21.786974383999,-27.1763144586388));
#28570=CARTESIAN_POINT('Ctrl Pts',(-20.8565259857495,21.7810821166994,-27.1767465856523));
#28571=CARTESIAN_POINT('Ctrl Pts',(-20.8581830941586,21.778561586577,-27.1769317398702));
#28572=CARTESIAN_POINT('Ctrl Pts',(-20.8619317185221,21.7728771766915,-27.1773499957243));
#28573=CARTESIAN_POINT('Ctrl Pts',(-20.8640252830125,21.7697146592105,-27.177583174327));
#28574=CARTESIAN_POINT('Ctrl Pts',(-20.8696724100461,21.7612167948402,-27.1782110418472));
#28575=CARTESIAN_POINT('Ctrl Pts',(-20.8732363033976,21.7558883633043,-27.1786061205019));
#28576=CARTESIAN_POINT('Ctrl Pts',(-20.8889486863455,21.7325475397031,-27.1803428628922));
#28577=CARTESIAN_POINT('Ctrl Pts',(-20.9012630200807,21.7146479649917,-27.1816908078596));
#28578=CARTESIAN_POINT('Ctrl Pts',(-20.9211790226122,21.686316749822,-27.1838505169198));
#28579=CARTESIAN_POINT('Ctrl Pts',(-20.9286641508296,21.6758036877424,-27.184657774807));
#28580=CARTESIAN_POINT('Ctrl Pts',(-20.9439858421571,21.6545552562208,-27.1863013473081));
#28581=CARTESIAN_POINT('Ctrl Pts',(-20.9518260710226,21.6438228484408,-27.1871377928967));
#28582=CARTESIAN_POINT('Ctrl Pts',(-20.9606726219819,21.6318688495237,-27.1880765539643));
#28583=CARTESIAN_POINT('Ctrl Pts',(-20.9616138061386,21.6305990188582,-27.1881763654606));
#28584=CARTESIAN_POINT('Ctrl Pts',(-20.9667366158092,21.623698024057,-27.1887192902085));
#28585=CARTESIAN_POINT('Ctrl Pts',(-20.9709356567675,21.6180798644611,-27.1891630702296));
#28586=CARTESIAN_POINT('Ctrl Pts',(-20.9771903562164,21.6097680342387,-27.1898222764186));
#28587=CARTESIAN_POINT('Ctrl Pts',(-20.979231996512,21.6070637988966,-27.1900371660716));
#28588=CARTESIAN_POINT('Ctrl Pts',(-20.9837670935096,21.6010765381762,-27.190513867766));
#28589=CARTESIAN_POINT('Ctrl Pts',(-20.9862625896019,21.597795071282,-27.1907757573389));
#28590=CARTESIAN_POINT('Ctrl Pts',(-20.9936778277722,21.5880830942577,-27.1915527036022));
#28591=CARTESIAN_POINT('Ctrl Pts',(-20.9986154877599,21.581666360853,-27.1920684404946));
#28592=CARTESIAN_POINT('Ctrl Pts',(-21.0258601365433,21.5465353078924,-27.194905322363));
#28593=CARTESIAN_POINT('Ctrl Pts',(-21.0486269763962,21.5181823820836,-27.1972437804498));
#28594=CARTESIAN_POINT('Ctrl Pts',(-21.1137718757252,21.4398077761736,-27.20384668455));
#28595=CARTESIAN_POINT('Ctrl Pts',(-21.1572020062041,21.3906869782413,-27.2081486075978));
#28596=CARTESIAN_POINT('Ctrl Pts',(-21.3604878269591,21.1744313400374,-27.2278261083055));
#28597=CARTESIAN_POINT('Ctrl Pts',(-21.5365383283496,21.0234879716498,-27.2437097035072));
#28598=CARTESIAN_POINT('Ctrl Pts',(-21.7936281069791,20.8471294510117,-27.2644792212185));
#28599=CARTESIAN_POINT('Ctrl Pts',(-21.8617311438462,20.8040731091805,-27.2697723757969));
#28600=CARTESIAN_POINT('Ctrl Pts',(-21.9589654034866,20.7475858510543,-27.2769731829047));
#28601=CARTESIAN_POINT('Ctrl Pts',(-21.9867873873434,20.7319707535634,-27.2789943272813));
#28602=CARTESIAN_POINT('Ctrl Pts',(-22.0188469036213,20.7145982586971,-27.2812748325742));
#28603=CARTESIAN_POINT('Ctrl Pts',(-22.0228605125205,20.7124343602754,-27.2815594750754));
#28604=CARTESIAN_POINT('Ctrl Pts',(-22.028944683598,20.7091707852351,-27.2819896447962));
#28605=CARTESIAN_POINT('Ctrl Pts',(-22.0310118539481,20.708064849308,-27.2821355707));
#28606=CARTESIAN_POINT('Ctrl Pts',(-22.0345724629695,20.7061649183253,-27.2823865244086));
#28607=CARTESIAN_POINT('Ctrl Pts',(-22.0360653183553,20.7053698440847,-27.2824916215947));
#28608=CARTESIAN_POINT('Ctrl Pts',(-22.0391620258546,20.7037237083264,-27.28270938069));
#28609=CARTESIAN_POINT('Ctrl Pts',(-22.0407659670959,20.7028728291535,-27.2828220307546));
#28610=CARTESIAN_POINT('Ctrl Pts',(-22.0446764378578,20.7008025856408,-27.2830963410143));
#28611=CARTESIAN_POINT('Ctrl Pts',(-22.0469837354505,20.6995846633257,-27.2832579087991));
#28612=CARTESIAN_POINT('Ctrl Pts',(-22.0557152412963,20.6949892289551,-27.2838682672576));
#28613=CARTESIAN_POINT('Ctrl Pts',(-22.0621494379016,20.6916305865929,-27.2843158641715));
#28614=CARTESIAN_POINT('Ctrl Pts',(-22.1720690493164,20.6347243806983,-27.2919264069866));
#28615=CARTESIAN_POINT('Ctrl Pts',(-22.278385902341,20.5867990869696,-27.2987445813672));
#28616=CARTESIAN_POINT('Ctrl Pts',(-22.6389719541953,20.4472476424409,-27.3208570302327));
#28617=CARTESIAN_POINT('Ctrl Pts',(-22.9021208458613,20.3818130722391,-27.3354823432333));
#28618=CARTESIAN_POINT('Ctrl Pts',(-23.2523011243991,20.3402444932921,-27.3558338489613));
#28619=CARTESIAN_POINT('Ctrl Pts',(-23.3345807846856,20.3336688280655,-27.3606691824551));
#28620=CARTESIAN_POINT('Ctrl Pts',(-23.4594236850669,20.3285031561878,-27.3681389531905));
#28621=CARTESIAN_POINT('Ctrl Pts',(-23.5018586590562,20.3275864476686,-27.3707009717934));
#28622=CARTESIAN_POINT('Ctrl Pts',(-23.5518681495668,20.327494045324,-27.3737512091903));
#28623=CARTESIAN_POINT('Ctrl Pts',(-23.559438394421,20.3275067319023,-27.3742137742785));
#28624=CARTESIAN_POINT('Ctrl Pts',(-23.5710884201954,20.3275673043312,-27.3749269297939));
#28625=CARTESIAN_POINT('Ctrl Pts',(-23.5751683077212,20.3275962650757,-27.375176925816));
#28626=CARTESIAN_POINT('Ctrl Pts',(-23.5825921627519,20.3276630613571,-27.375632275883));
#28627=CARTESIAN_POINT('Ctrl Pts',(-23.5859361521421,20.3276983544675,-27.3758375498092));
#28628=CARTESIAN_POINT('Ctrl Pts',(-23.5926455178866,20.3277796109207,-27.3762497475168));
#28629=CARTESIAN_POINT('Ctrl Pts',(-23.5960108891255,20.3278256414474,-27.3764566731538));
#28630=CARTESIAN_POINT('Ctrl Pts',(-23.6055488063937,20.3279710426286,-27.3770436139016));
#28631=CARTESIAN_POINT('Ctrl Pts',(-23.6117211230013,20.3280828769112,-27.377424019945));
#28632=CARTESIAN_POINT('Ctrl Pts',(-23.6376193444084,20.3286265600959,-27.3790226005423));
#28633=CARTESIAN_POINT('Ctrl Pts',(-23.6573410603169,20.3292218146726,-27.38024589515));
#28634=CARTESIAN_POINT('Ctrl Pts',(-23.6818738810518,20.3301878376917,-27.3817752713361));
#28635=CARTESIAN_POINT('Ctrl Pts',(-23.6866915886361,20.3303883736123,-27.3820759747956));
#28636=CARTESIAN_POINT('Ctrl Pts',(-23.7033529612528,20.3311193603287,-27.3831171954525));
#28637=CARTESIAN_POINT('Ctrl Pts',(-23.7151940279755,20.3317043476123,-27.3838594173286));
#28638=CARTESIAN_POINT('Ctrl Pts',(-23.7319041231595,20.3326223360048,-27.3849100416364));
#28639=CARTESIAN_POINT('Ctrl Pts',(-23.7367761392773,20.3329010867497,-27.3852167473408));
#28640=CARTESIAN_POINT('Ctrl Pts',(-23.7495874034398,20.3336632764585,-27.3860242645489));
#28641=CARTESIAN_POINT('Ctrl Pts',(-23.7575254910398,20.3341650412033,-27.3865256429478));
#28642=CARTESIAN_POINT('Ctrl Pts',(-23.7723101285133,20.3351545395856,-27.3874613822976));
#28643=CARTESIAN_POINT('Ctrl Pts',(-23.7791571494084,20.3356347705929,-27.3878955091363));
#28644=CARTESIAN_POINT('Ctrl Pts',(-23.7917113942758,20.3365556034639,-27.3886929141803));
#28645=CARTESIAN_POINT('Ctrl Pts',(-23.7974190914475,20.3369895452734,-27.3890559868144));
#28646=CARTESIAN_POINT('Ctrl Pts',(-23.8071130942556,20.3377525374955,-27.3896735499039));
#28647=CARTESIAN_POINT('Ctrl Pts',(-23.8111000133897,20.3380738080876,-27.3899278030432));
#28648=CARTESIAN_POINT('Ctrl Pts',(-23.8198832183645,20.3387980291236,-27.3904885063707));
#28649=CARTESIAN_POINT('Ctrl Pts',(-23.824679214045,20.3392043033286,-27.3907950564591));
#28650=CARTESIAN_POINT('Ctrl Pts',(-23.8502450560752,20.3414277099266,-27.3924312167005));
#28651=CARTESIAN_POINT('Ctrl Pts',(-23.8709974423327,20.3434355861917,-27.3937665279039));
#28652=CARTESIAN_POINT('Ctrl Pts',(-23.9169671777955,20.3483340202737,-27.3967404757581));
#28653=CARTESIAN_POINT('Ctrl Pts',(-23.9421726339419,20.3513214033321,-27.398381835098));
#28654=CARTESIAN_POINT('Ctrl Pts',(-24.2485422030417,20.3913079300507,-27.4184620976162));
#28655=CARTESIAN_POINT('Ctrl Pts',(-24.523653771292,20.4649669869097,-27.4379844135203));
#28656=CARTESIAN_POINT('Ctrl Pts',(-24.825809218905,20.5903579231332,-27.4598164802937));
#28657=CARTESIAN_POINT('Ctrl Pts',(-24.8657629177183,20.6078974098833,-27.4627082128863));
#28658=CARTESIAN_POINT('Ctrl Pts',(-24.9512979700198,20.6475376053584,-27.4688926788763));
#28659=CARTESIAN_POINT('Ctrl Pts',(-24.9967409844313,20.6699133064484,-27.4721743931875));
#28660=CARTESIAN_POINT('Ctrl Pts',(-25.063059387563,20.7045335054178,-27.4769379506344));
#28661=CARTESIAN_POINT('Ctrl Pts',(-25.0843527685705,20.7159558097657,-27.4784634019905));
#28662=CARTESIAN_POINT('Ctrl Pts',(-25.1091375065775,20.7296121273527,-27.4802324490357));
#28663=CARTESIAN_POINT('Ctrl Pts',(-25.1127547636655,20.7316143088887,-27.4804904718943));
#28664=CARTESIAN_POINT('Ctrl Pts',(-25.1183901304226,20.7347477126295,-27.4808921803111));
#28665=CARTESIAN_POINT('Ctrl Pts',(-25.1204108754696,20.7358741473479,-27.4810361720595));
#28666=CARTESIAN_POINT('Ctrl Pts',(-25.1240593781938,20.7379131043381,-27.481296052582));
#28667=CARTESIAN_POINT('Ctrl Pts',(-25.1256875518353,20.7388248619648,-27.4814119901711));
#28668=CARTESIAN_POINT('Ctrl Pts',(-25.1289508605464,20.740656000545,-27.4816442882008));
#28669=CARTESIAN_POINT('Ctrl Pts',(-25.130585978231,20.7415753912655,-27.481760647262));
#28670=CARTESIAN_POINT('Ctrl Pts',(-25.1352252685827,20.7441892960905,-27.4820906898222));
#28671=CARTESIAN_POINT('Ctrl Pts',(-25.1382275366147,20.7458872126071,-27.48230415313));
#28672=CARTESIAN_POINT('Ctrl Pts',(-25.150869962235,20.753063880138,-27.4832025557653));
#28673=CARTESIAN_POINT('Ctrl Pts',(-25.1604846858802,20.7585876289112,-27.4838846181772));
#28674=CARTESIAN_POINT('Ctrl Pts',(-25.1776116016297,20.7685451237803,-27.4850978198798));
#28675=CARTESIAN_POINT('Ctrl Pts',(-25.1851345962312,20.7729599139287,-27.4856301033665));
#28676=CARTESIAN_POINT('Ctrl Pts',(-25.197389025921,20.7802183438603,-27.486496305049));
#28677=CARTESIAN_POINT('Ctrl Pts',(-25.2021311835739,20.7830436576129,-27.4868312942811));
#28678=CARTESIAN_POINT('Ctrl Pts',(-25.3061752250288,20.8453944590595,-27.4941769651038));
#28679=CARTESIAN_POINT('Ctrl Pts',(-25.4022167629854,20.9102229560541,-27.5008772485788));
#28680=CARTESIAN_POINT('Ctrl Pts',(-25.5485161450003,21.0208977144942,-27.5112957396993));
#28681=CARTESIAN_POINT('Ctrl Pts',(-25.6011657139346,21.0633973242185,-27.5150923677892));
#28682=CARTESIAN_POINT('Ctrl Pts',(-25.7522718646537,21.1934377043465,-27.5262476922591));
#28683=CARTESIAN_POINT('Ctrl Pts',(-25.846742002686,21.2853904296058,-27.5335686083081));
#28684=CARTESIAN_POINT('Ctrl Pts',(-26.040334849408,21.4984262833477,-27.5498983373966));
#28685=CARTESIAN_POINT('Ctrl Pts',(-26.1368000453749,21.6214541580965,-27.5589515026325));
#28686=CARTESIAN_POINT('Ctrl Pts',(-26.232501659889,21.7636660968393,-27.5693033675074));
#28687=CARTESIAN_POINT('Ctrl Pts',(-26.2409499253896,21.7764151665385,-27.5702303163041));
#28688=CARTESIAN_POINT('Ctrl Pts',(-26.2554523816259,21.7986424686929,-27.5718447860026));
#28689=CARTESIAN_POINT('Ctrl Pts',(-26.2615483444967,21.8080932245922,-27.5725307361182));
#28690=CARTESIAN_POINT('Ctrl Pts',(-26.2701515405881,21.8215855420155,-27.5735093910273));
#28691=CARTESIAN_POINT('Ctrl Pts',(-26.2726995356101,21.8256011204601,-27.5738005779749));
#28692=CARTESIAN_POINT('Ctrl Pts',(-26.2770731718763,21.8325277092297,-27.5743027235192));
#28693=CARTESIAN_POINT('Ctrl Pts',(-26.278903068152,21.8354360344635,-27.5745135238498));
#28694=CARTESIAN_POINT('Ctrl Pts',(-26.2823900170519,21.8409976912398,-27.5749165687585));
#28695=CARTESIAN_POINT('Ctrl Pts',(-26.284047865499,21.8436505214804,-27.5751087835752));
#28696=CARTESIAN_POINT('Ctrl Pts',(-26.2879106457462,21.8498516773536,-27.5755580256911));
#28697=CARTESIAN_POINT('Ctrl Pts',(-26.2901125423047,21.8534018791974,-27.5758151647898));
#28698=CARTESIAN_POINT('Ctrl Pts',(-26.2976529273765,21.8656124721264,-27.5766993901535));
#28699=CARTESIAN_POINT('Ctrl Pts',(-26.3029572646633,21.8742937870422,-27.5773277324666));
#28700=CARTESIAN_POINT('Ctrl Pts',(-26.3578089267249,21.9650293629311,-27.5838921196927));
#28701=CARTESIAN_POINT('Ctrl Pts',(-26.4037083799335,22.049222229168,-27.5899604577764));
#28702=CARTESIAN_POINT('Ctrl Pts',(-26.4726995227722,22.1904072333082,-27.6001157597815));
#28703=CARTESIAN_POINT('Ctrl Pts',(-26.4980358290127,22.2462400455313,-27.6041261286337));
#28704=CARTESIAN_POINT('Ctrl Pts',(-26.5931479282226,22.472795605622,-27.6203635841559));
#28705=CARTESIAN_POINT('Ctrl Pts',(-26.6498017644445,22.6486366990462,-27.6329121172837));
#28706=CARTESIAN_POINT('Ctrl Pts',(-26.7097274841857,22.9093575789905,-27.6509692449815));
#28707=CARTESIAN_POINT('Ctrl Pts',(-26.7252084198942,22.991070298954,-27.6565486071451));
#28708=CARTESIAN_POINT('Ctrl Pts',(-26.7488938478758,23.1493473482492,-27.6671061356368));
#28709=CARTESIAN_POINT('Ctrl Pts',(-26.7575502042249,23.2257913095039,-27.6720946080847));
#28710=CARTESIAN_POINT('Ctrl Pts',(-26.7640638516621,23.3102623004044,-27.6774340442857));
#28711=CARTESIAN_POINT('Ctrl Pts',(-26.7646357955772,23.3180484247342,-27.677924591551));
#28712=CARTESIAN_POINT('Ctrl Pts',(-26.7655837712384,23.3316288913531,-27.6787772910222));
#28713=CARTESIAN_POINT('Ctrl Pts',(-26.7659724447151,23.3374222745436,-27.6791401278862));
#28714=CARTESIAN_POINT('Ctrl Pts',(-26.766510366941,23.3457783552546,-27.6796621050492));
#28715=CARTESIAN_POINT('Ctrl Pts',(-26.7666722115368,23.3483401872269,-27.6798219500412));
#28716=CARTESIAN_POINT('Ctrl Pts',(-26.7669484020376,23.352796605738,-27.6800996835761));
#28717=CARTESIAN_POINT('Ctrl Pts',(-26.7670641351845,23.3546911022024,-27.6802176508381));
#28718=CARTESIAN_POINT('Ctrl Pts',(-26.7672849326199,23.3583586841663,-27.6804458270211));
#28719=CARTESIAN_POINT('Ctrl Pts',(-26.7673902044812,23.3601317498259,-27.6805560476143));
#28720=CARTESIAN_POINT('Ctrl Pts',(-26.7676379901545,23.3643642765043,-27.6808189460489));
#28721=CARTESIAN_POINT('Ctrl Pts',(-26.7677791500136,23.3668238201183,-27.6809715470843));
#28722=CARTESIAN_POINT('Ctrl Pts',(-26.76819734492,23.3742594091091,-27.6814323748453));
#28723=CARTESIAN_POINT('Ctrl Pts',(-26.7684656594506,23.3792359673273,-27.6817401124202));
#28724=CARTESIAN_POINT('Ctrl Pts',(-26.771087071927,23.4300488404061,-27.6848753945718));
#28725=CARTESIAN_POINT('Ctrl Pts',(-26.7724724436299,23.4759327161919,-27.6876496112822));
#28726=CARTESIAN_POINT('Ctrl Pts',(-26.7728947536254,23.5238210516992,-27.6905001678976));
#28727=CARTESIAN_POINT('Ctrl Pts',(-26.7729104433794,23.5258087595122,-27.6906184057381));
#28728=CARTESIAN_POINT('Ctrl Pts',(-26.7729349638419,23.5293276960502,-27.6908275872599));
#28729=CARTESIAN_POINT('Ctrl Pts',(-26.7729445422572,23.5308589170087,-27.6909185627983));
#28730=CARTESIAN_POINT('Ctrl Pts',(-26.7729781551214,23.536923291716,-27.6912786850976));
#28731=CARTESIAN_POINT('Ctrl Pts',(-26.7729937162975,23.5414565081284,-27.6915474733269));
#28732=CARTESIAN_POINT('Ctrl Pts',(-26.7730009972145,23.5469610462477,-27.6918733737843));
#28733=CARTESIAN_POINT('Ctrl Pts',(-26.7730018428478,23.547932327846,-27.6919308611048));
#28734=CARTESIAN_POINT('Ctrl Pts',(-26.7730307965937,23.6171065457229,-27.6960237967814));
#28735=CARTESIAN_POINT('Ctrl Pts',(-26.7708942687391,23.685297442175,-27.6999698176733));
#28736=CARTESIAN_POINT('Ctrl Pts',(-26.7475149334412,24.0555011632254,-27.7211499751951));
#28737=CARTESIAN_POINT('Ctrl Pts',(-26.6859643129802,24.353425706689,-27.737471870038));
#28738=CARTESIAN_POINT('Ctrl Pts',(-26.5767465221006,24.6578991193774,-27.7564158227598));
#28739=CARTESIAN_POINT('Ctrl Pts',(-26.5695630873687,24.6773330873056,-27.7576345291315));
#28740=CARTESIAN_POINT('Ctrl Pts',(-26.5602633221964,24.701765460286,-27.7591794514905));
#28741=CARTESIAN_POINT('Ctrl Pts',(-26.5583209859049,24.7068298779789,-27.7595003834268));
#28742=CARTESIAN_POINT('Ctrl Pts',(-26.5549015267926,24.715678841402,-27.7600623753962));
#28743=CARTESIAN_POINT('Ctrl Pts',(-26.5534300124923,24.7194655515156,-27.7603032629522));
#28744=CARTESIAN_POINT('Ctrl Pts',(-26.5497758286131,24.7288166070759,-27.7608991089322));
#28745=CARTESIAN_POINT('Ctrl Pts',(-26.547584837468,24.734377667235,-27.7612543242227));
#28746=CARTESIAN_POINT('Ctrl Pts',(-26.5428223863458,24.7463675637165,-27.7620220811712));
#28747=CARTESIAN_POINT('Ctrl Pts',(-26.5402456567134,24.752794263218,-27.76243478686));
#28748=CARTESIAN_POINT('Ctrl Pts',(-26.5347268705365,24.766431437017,-27.7633130779086));
#28749=CARTESIAN_POINT('Ctrl Pts',(-26.5317793532091,24.773639641314,-27.7637788352832));
#28750=CARTESIAN_POINT('Ctrl Pts',(-26.5218520079364,24.7976681626849,-27.7653365908627));
#28751=CARTESIAN_POINT('Ctrl Pts',(-26.5147558308815,24.8144397695091,-27.7664323440683));
#28752=CARTESIAN_POINT('Ctrl Pts',(-26.4989374612271,24.8509603471575,-27.7688375173806));
#28753=CARTESIAN_POINT('Ctrl Pts',(-26.4901582497826,24.8706835099713,-27.7701488040181));
#28754=CARTESIAN_POINT('Ctrl Pts',(-26.4785227033803,24.8961322648778,-27.7718573461241));
#28755=CARTESIAN_POINT('Ctrl Pts',(-26.4758464137888,24.9019399551397,-27.7722483823615));
#28756=CARTESIAN_POINT('Ctrl Pts',(-26.4715567915688,24.9111762406691,-27.7728720813576));
#28757=CARTESIAN_POINT('Ctrl Pts',(-26.4699546570244,24.9146100433308,-27.7731043561075));
#28758=CARTESIAN_POINT('Ctrl Pts',(-26.4670660496595,24.920772712375,-27.773521943844));
#28759=CARTESIAN_POINT('Ctrl Pts',(-26.465781791869,24.9235026171493,-27.7737071797881));
#28760=CARTESIAN_POINT('Ctrl Pts',(-26.4627716175191,24.9298779900951,-27.7741403755748));
#28761=CARTESIAN_POINT('Ctrl Pts',(-26.461042689535,24.9335220237113,-27.7743884398804));
#28762=CARTESIAN_POINT('Ctrl Pts',(-26.4560766090705,24.943938413776,-27.7750988446037));
#28763=CARTESIAN_POINT('Ctrl Pts',(-26.4528226465237,24.9507026855894,-27.775561769883));
#28764=CARTESIAN_POINT('Ctrl Pts',(-26.4317574416837,24.9941038111393,-27.7785423666954));
#28765=CARTESIAN_POINT('Ctrl Pts',(-26.413277202109,25.0304101430023,-27.7810833604011));
#28766=CARTESIAN_POINT('Ctrl Pts',(-26.3562805936072,25.1373227500454,-27.7887131151413));
#28767=CARTESIAN_POINT('Ctrl Pts',(-26.3158065315181,25.206843797112,-27.7938701211423));
#28768=CARTESIAN_POINT('Ctrl Pts',(-26.1912799074142,25.4034356558246,-27.8090332427642));
#28769=CARTESIAN_POINT('Ctrl Pts',(-26.100772022104,25.5261460470135,-27.8192437448183));
#28770=CARTESIAN_POINT('Ctrl Pts',(-25.8523241743234,25.817347432618,-27.8451268344965));
#28771=CARTESIAN_POINT('Ctrl Pts',(-25.6843128591967,25.9761670819324,-27.8608631890206));
#28772=CARTESIAN_POINT('Ctrl Pts',(-25.4901365032949,26.123799971556,-27.8762617352713));
#28773=CARTESIAN_POINT('Ctrl Pts',(-25.4794450245147,26.1318242601176,-27.8771013171008));
#28774=CARTESIAN_POINT('Ctrl Pts',(-25.4657590848714,26.1419634795186,-27.8781652257692));
#28775=CARTESIAN_POINT('Ctrl Pts',(-25.46281072611,26.1441399898598,-27.8783937879586));
#28776=CARTESIAN_POINT('Ctrl Pts',(-25.4581238422539,26.1475875625996,-27.8787561076886));
#28777=CARTESIAN_POINT('Ctrl Pts',(-25.4563877559068,26.1488619112483,-27.8788900951662));
#28778=CARTESIAN_POINT('Ctrl Pts',(-25.45314479405,26.1512373612211,-27.8791399663272));
#28779=CARTESIAN_POINT('Ctrl Pts',(-25.4516382494196,26.1523388865296,-27.8792558794401));
#28780=CARTESIAN_POINT('Ctrl Pts',(-25.4482595072068,26.1548047868761,-27.8795154665618));
#28781=CARTESIAN_POINT('Ctrl Pts',(-25.4463867990182,26.156168449261,-27.8796590902643));
#28782=CARTESIAN_POINT('Ctrl Pts',(-25.4408571949992,26.1601858612588,-27.880082424326));
#28783=CARTESIAN_POINT('Ctrl Pts',(-25.4371961674776,26.1628339550473,-27.8803617405255));
#28784=CARTESIAN_POINT('Ctrl Pts',(-25.4089182331777,26.1831974987447,-27.8825118710273));
#28785=CARTESIAN_POINT('Ctrl Pts',(-25.3840568642563,26.2005731201463,-27.8843595243185));
#28786=CARTESIAN_POINT('Ctrl Pts',(-25.297705981302,26.2591268357333,-27.8906453675226));
#28787=CARTESIAN_POINT('Ctrl Pts',(-25.2350419812564,26.2985392286721,-27.8949815813351));
#28788=CARTESIAN_POINT('Ctrl Pts',(-24.8282243934108,26.5352563772553,-27.9220954164485));
#28789=CARTESIAN_POINT('Ctrl Pts',(-24.4515116493518,26.6697458561519,-27.9430971696385));
#28790=CARTESIAN_POINT('Ctrl Pts',(-24.0415267464132,26.735391284638,-27.968234994199));
#28791=CARTESIAN_POINT('Ctrl Pts',(-24.0232504909872,26.7381565669311,-27.9693589590303));
#28792=CARTESIAN_POINT('Ctrl Pts',(-23.9989970848315,26.7416130670694,-27.9708552936865));
#28793=CARTESIAN_POINT('Ctrl Pts',(-23.9930400876004,26.7424450259339,-27.9712231971251));
#28794=CARTESIAN_POINT('Ctrl Pts',(-23.9837778518436,26.7437121718227,-27.9717958357649));
#28795=CARTESIAN_POINT('Ctrl Pts',(-23.9804741864604,26.7441589179204,-27.9720002045456));
#28796=CARTESIAN_POINT('Ctrl Pts',(-23.9738515274216,26.745044021169,-27.9724101318888));
#28797=CARTESIAN_POINT('Ctrl Pts',(-23.9705325320732,26.745482334314,-27.9726156915776));
#28798=CARTESIAN_POINT('Ctrl Pts',(-23.9631933473753,26.7464399287122,-27.973070510139));
#28799=CARTESIAN_POINT('Ctrl Pts',(-23.9591728539711,26.7469567976377,-27.9733198450236));
#28800=CARTESIAN_POINT('Ctrl Pts',(-23.947509200345,26.7484338964333,-27.9740437053471));
#28801=CARTESIAN_POINT('Ctrl Pts',(-23.939863598296,26.7493743045691,-27.9745188570281));
#28802=CARTESIAN_POINT('Ctrl Pts',(-23.9226111110704,26.7514335941752,-27.9755925577239));
#28803=CARTESIAN_POINT('Ctrl Pts',(-23.913002445059,26.7525366545498,-27.9761916032309));
#28804=CARTESIAN_POINT('Ctrl Pts',(-23.8325928212801,26.761401008441,-27.9812136948862));
#28805=CARTESIAN_POINT('Ctrl Pts',(-23.7615623349881,26.7668559331855,-27.9857090673376));
#28806=CARTESIAN_POINT('Ctrl Pts',(-23.6169160821752,26.7731527285653,-27.9949924779138));
#28807=CARTESIAN_POINT('Ctrl Pts',(-23.5433351847723,26.7738344784115,-27.9997825785216));
#28808=CARTESIAN_POINT('Ctrl Pts',(-23.3009450046869,26.7677815484129,-28.0157712370068));
#28809=CARTESIAN_POINT('Ctrl Pts',(-23.1326943961955,26.7502969351834,-28.0272205050949));
#28810=CARTESIAN_POINT('Ctrl Pts',(-22.7869542469707,26.6866297101573,-28.051001373812));
#28811=CARTESIAN_POINT('Ctrl Pts',(-22.610417657927,26.638328612315,-28.063284995901));
#28812=CARTESIAN_POINT('Ctrl Pts',(-22.4283729664856,26.5714492742446,-28.0755037517968));
#28813=CARTESIAN_POINT('Ctrl Pts',(-22.4178585777924,26.5675240571047,-28.0762077678696));
#28814=CARTESIAN_POINT('Ctrl Pts',(-22.404124386863,26.5623149228752,-28.0771249362809));
#28815=CARTESIAN_POINT('Ctrl Pts',(-22.400886014703,26.5610806873069,-28.0773410166546));
#28816=CARTESIAN_POINT('Ctrl Pts',(-22.3958947294136,26.5591691404018,-28.0776737785532));
#28817=CARTESIAN_POINT('Ctrl Pts',(-22.3941404200447,26.5584955204141,-28.0777906821476));
#28818=CARTESIAN_POINT('Ctrl Pts',(-22.3908197462685,26.5572171137637,-28.0780118619361));
#28819=CARTESIAN_POINT('Ctrl Pts',(-22.3892532733171,26.5566126404994,-28.0781161561847));
#28820=CARTESIAN_POINT('Ctrl Pts',(-22.3856132045299,26.5552047352018,-28.0783584073007));
#28821=CARTESIAN_POINT('Ctrl Pts',(-22.3835399708013,26.5544003822618,-28.0784963074868));
#28822=CARTESIAN_POINT('Ctrl Pts',(-22.3776641046471,26.5521137210949,-28.0788869266434));
#28823=CARTESIAN_POINT('Ctrl Pts',(-22.3738634357685,26.5506263275901,-28.0791393384523));
#28824=CARTESIAN_POINT('Ctrl Pts',(-22.3506953780232,26.5415087080106,-28.0806765125242));
#28825=CARTESIAN_POINT('Ctrl Pts',(-22.3313988845291,26.5336979758403,-28.0819505231964));
#28826=CARTESIAN_POINT('Ctrl Pts',(-22.2737259380351,26.5097004610811,-28.0857432112327));
#28827=CARTESIAN_POINT('Ctrl Pts',(-22.2355848051969,26.4929555953082,-28.088231305606));
#28828=CARTESIAN_POINT('Ctrl Pts',(-22.156442735343,26.4563642927838,-28.0933731878603));
#28829=CARTESIAN_POINT('Ctrl Pts',(-22.1155198733829,26.4363802410779,-28.0960199595268));
#28830=CARTESIAN_POINT('Ctrl Pts',(-22.0750360120315,26.4155367728497,-28.0986394360247));
#28831=CARTESIAN_POINT('Ctrl Pts',(-22.0750360250495,26.4155367795522,-28.3456357132216));
#28832=CARTESIAN_POINT('Ctrl Pts',(-22.091222596573,26.4238705766319,-28.3444667025509));
#28833=CARTESIAN_POINT('Ctrl Pts',(-22.1074805334644,26.4320675962987,-28.3432931375839));
#28834=CARTESIAN_POINT('Ctrl Pts',(-22.3054080929832,26.5297648046258,-28.3290133416339));
#28835=CARTESIAN_POINT('Ctrl Pts',(-22.4950313262397,26.602074816926,-28.3153652355254));
#28836=CARTESIAN_POINT('Ctrl Pts',(-22.8186265216834,26.6916871270874,-28.2926363034063));
#28837=CARTESIAN_POINT('Ctrl Pts',(-22.9491881424434,26.7192608350467,-28.2836204738926));
#28838=CARTESIAN_POINT('Ctrl Pts',(-23.1487073223709,26.7486193460728,-28.2703736691822));
#28839=CARTESIAN_POINT('Ctrl Pts',(-23.2166313515898,26.7564164935814,-28.2659565325146));
#28840=CARTESIAN_POINT('Ctrl Pts',(-23.2957094283846,26.7629532859387,-28.2609595882052));
#28841=CARTESIAN_POINT('Ctrl Pts',(-23.3066661480529,26.7638025950668,-28.2602704704017));
#28842=CARTESIAN_POINT('Ctrl Pts',(-23.3209178774124,26.7648340074414,-28.2593785103852));
#28843=CARTESIAN_POINT('Ctrl Pts',(-23.3242089511216,26.765067106096,-28.2591728395609));
#28844=CARTESIAN_POINT('Ctrl Pts',(-23.3295459451123,26.765436876254,-28.2588398122093));
#28845=CARTESIAN_POINT('Ctrl Pts',(-23.3315916373522,26.7655766491363,-28.2587122805726));
#28846=CARTESIAN_POINT('Ctrl Pts',(-23.3355198921271,26.7658412827015,-28.2584676176437));
#28847=CARTESIAN_POINT('Ctrl Pts',(-23.3374024253794,26.7659664422211,-28.2583504699907));
#28848=CARTESIAN_POINT('Ctrl Pts',(-23.3417323384354,26.7662504959953,-28.2580812576323));
#28849=CARTESIAN_POINT('Ctrl Pts',(-23.3441797964861,26.766408250139,-28.2579292577104));
#28850=CARTESIAN_POINT('Ctrl Pts',(-23.3507095393682,26.766821649096,-28.2575241765232));
#28851=CARTESIAN_POINT('Ctrl Pts',(-23.3547921517343,26.7670723173074,-28.2572713753666));
#28852=CARTESIAN_POINT('Ctrl Pts',(-23.3825577015494,26.7687240399441,-28.2555552154814));
#28853=CARTESIAN_POINT('Ctrl Pts',(-23.4062558144183,26.7698713647319,-28.2541059046928));
#28854=CARTESIAN_POINT('Ctrl Pts',(-23.4328909733259,26.7708661997485,-28.2524921538547));
#28855=CARTESIAN_POINT('Ctrl Pts',(-23.435816843841,26.7709714898925,-28.2523150891112));
#28856=CARTESIAN_POINT('Ctrl Pts',(-23.4447895948412,26.7712821401018,-28.25177270529));
#28857=CARTESIAN_POINT('Ctrl Pts',(-23.4508369528162,26.7714744602716,-28.2514080181906));
#28858=CARTESIAN_POINT('Ctrl Pts',(-23.5565023923831,26.7745370243844,-28.2450503623923));
#28859=CARTESIAN_POINT('Ctrl Pts',(-23.6562100320388,26.772802192418,-28.2392759192138));
#28860=CARTESIAN_POINT('Ctrl Pts',(-23.9963589197518,26.7510753422953,-28.2198714685166));
#28861=CARTESIAN_POINT('Ctrl Pts',(-24.2345453410997,26.7087375037097,-28.2067323379703));
#28862=CARTESIAN_POINT('Ctrl Pts',(-24.5853653927134,26.6047923542932,-28.1857469774809));
#28863=CARTESIAN_POINT('Ctrl Pts',(-24.7027745884231,26.5624543105908,-28.1784394210376));
#28864=CARTESIAN_POINT('Ctrl Pts',(-24.8298160167241,26.5081261618088,-28.1700817451043));
#28865=CARTESIAN_POINT('Ctrl Pts',(-24.8421716834014,26.5027504607126,-28.1692641105389));
#28866=CARTESIAN_POINT('Ctrl Pts',(-24.8608909735119,26.494466074673,-28.1680179181634));
#28867=CARTESIAN_POINT('Ctrl Pts',(-24.8672795384414,26.4916138447798,-28.1675912896985));
#28868=CARTESIAN_POINT('Ctrl Pts',(-24.879047032239,26.4863141217649,-28.1668029860135));
#28869=CARTESIAN_POINT('Ctrl Pts',(-24.88442862512,26.4838725882732,-28.1664415166155));
#28870=CARTESIAN_POINT('Ctrl Pts',(-24.8931250226613,26.4798983076587,-28.1658558379112));
#28871=CARTESIAN_POINT('Ctrl Pts',(-24.8964440077816,26.4783746960102,-28.1656319442895));
#28872=CARTESIAN_POINT('Ctrl Pts',(-24.9028145511808,26.4754371168576,-28.1652014848227));
#28873=CARTESIAN_POINT('Ctrl Pts',(-24.9058665014971,26.4740240067883,-28.1649949488607));
#28874=CARTESIAN_POINT('Ctrl Pts',(-24.9128086315527,26.4707964644134,-28.1645244312726));
#28875=CARTESIAN_POINT('Ctrl Pts',(-24.916697403529,26.4689790348383,-28.1642603460209));
#28876=CARTESIAN_POINT('Ctrl Pts',(-24.9285057280637,26.4634316064408,-28.1634568710614));
#28877=CARTESIAN_POINT('Ctrl Pts',(-24.9364136756692,26.4596771269282,-28.1629166318499));
#28878=CARTESIAN_POINT('Ctrl Pts',(-24.9924176331645,26.4328078055491,-28.1590751908731));
#28879=CARTESIAN_POINT('Ctrl Pts',(-25.0399458663028,26.4085349361942,-28.1557337085104));
#28880=CARTESIAN_POINT('Ctrl Pts',(-25.1033799928596,26.3741268907081,-28.1511587815032));
#28881=CARTESIAN_POINT('Ctrl Pts',(-25.1198334462314,26.3650148724693,-28.1499614442918));
#28882=CARTESIAN_POINT('Ctrl Pts',(-25.1692292808915,26.3370914018397,-28.1463342854025));
#28883=CARTESIAN_POINT('Ctrl Pts',(-25.2019193243432,26.3178423174141,-28.1438896680594));
#28884=CARTESIAN_POINT('Ctrl Pts',(-25.3085456052629,26.2524949138342,-28.1357693187238));
#28885=CARTESIAN_POINT('Ctrl Pts',(-25.3809484801084,26.2039780023688,-28.1300168962215));
#28886=CARTESIAN_POINT('Ctrl Pts',(-25.5000638130591,26.1169627798335,-28.120164061873));
#28887=CARTESIAN_POINT('Ctrl Pts',(-25.5478224245145,26.0799718213193,-28.1161003258449));
#28888=CARTESIAN_POINT('Ctrl Pts',(-25.6814717108706,25.9703094477637,-28.1044255861544));
#28889=CARTESIAN_POINT('Ctrl Pts',(-25.7646361271542,25.8944530915306,-28.0967832329403));
#28890=CARTESIAN_POINT('Ctrl Pts',(-25.9092953044591,25.7479244000381,-28.0829489636283));
#28891=CARTESIAN_POINT('Ctrl Pts',(-25.9720099168832,25.6786177014701,-28.0767379976417));
#28892=CARTESIAN_POINT('Ctrl Pts',(-26.0529830675722,25.5809118788983,-28.0685199261794));
#28893=CARTESIAN_POINT('Ctrl Pts',(-26.0739357864591,25.5548124710593,-28.0663737895877));
#28894=CARTESIAN_POINT('Ctrl Pts',(-26.1053688146291,25.5143841721224,-28.0631296224353));
#28895=CARTESIAN_POINT('Ctrl Pts',(-26.1161430272316,25.5002879979052,-28.0620130314254));
#28896=CARTESIAN_POINT('Ctrl Pts',(-26.1291357384022,25.4829951636764,-28.0606615986522));
#28897=CARTESIAN_POINT('Ctrl Pts',(-26.1314652948904,25.4798828970271,-28.0604190944728));
#28898=CARTESIAN_POINT('Ctrl Pts',(-26.1350933375184,25.4750175382014,-28.0600411225277));
#28899=CARTESIAN_POINT('Ctrl Pts',(-26.1363956748274,25.4732673431353,-28.0599053841224));
#28900=CARTESIAN_POINT('Ctrl Pts',(-26.1386961029975,25.4701692626037,-28.0596655136418));
#28901=CARTESIAN_POINT('Ctrl Pts',(-26.1396949135333,25.4688219275229,-28.0595613308248));
#28902=CARTESIAN_POINT('Ctrl Pts',(-26.1418283757576,25.4659393149201,-28.0593387214288));
#28903=CARTESIAN_POINT('Ctrl Pts',(-26.1429627119285,25.4644038131545,-28.0592203172602));
#28904=CARTESIAN_POINT('Ctrl Pts',(-26.1462401832608,25.4599589836337,-28.0588780740737));
#28905=CARTESIAN_POINT('Ctrl Pts',(-26.1483797993858,25.4570470462781,-28.0586544823067));
#28906=CARTESIAN_POINT('Ctrl Pts',(-26.1578938713649,25.4440530061133,-28.0576594781602));
#28907=CARTESIAN_POINT('Ctrl Pts',(-26.1652147010318,25.4339315006875,-28.0568917651191));
#28908=CARTESIAN_POINT('Ctrl Pts',(-26.2891267691927,25.2605006933438,-28.0438568544211));
#28909=CARTESIAN_POINT('Ctrl Pts',(-26.3902940373637,25.0866676759173,-28.0325809763221));
#28910=CARTESIAN_POINT('Ctrl Pts',(-26.5429088041556,24.7571149001774,-28.0122675951485));
#28911=CARTESIAN_POINT('Ctrl Pts',(-26.5999296419002,24.6047547349596,-28.0032414775938));
#28912=CARTESIAN_POINT('Ctrl Pts',(-26.6834535120523,24.3170490310567,-27.9860561397293));
#28913=CARTESIAN_POINT('Ctrl Pts',(-26.7132381663515,24.1830555833076,-27.9780009853923));
#28914=CARTESIAN_POINT('Ctrl Pts',(-26.7360219800529,24.0371831240379,-27.9690153142882));
#28915=CARTESIAN_POINT('Ctrl Pts',(-26.7375955069498,24.0267744449488,-27.9683730257797));
#28916=CARTESIAN_POINT('Ctrl Pts',(-26.7397875255258,24.0117777377308,-27.9674459538917));
#28917=CARTESIAN_POINT('Ctrl Pts',(-26.7404471835827,24.0071957178688,-27.9671624768382));
#28918=CARTESIAN_POINT('Ctrl Pts',(-26.741576100555,23.9992325907365,-27.9666694249724));
#28919=CARTESIAN_POINT('Ctrl Pts',(-26.742049865516,23.995852121289,-27.9664599933422));
#28920=CARTESIAN_POINT('Ctrl Pts',(-26.7429513243097,23.9893447120259,-27.966056596909));
#28921=CARTESIAN_POINT('Ctrl Pts',(-26.7433797975567,23.9862178824784,-27.9658626570529));
#28922=CARTESIAN_POINT('Ctrl Pts',(-26.7443795968072,23.9788411948198,-27.9654048682809));
#28923=CARTESIAN_POINT('Ctrl Pts',(-26.7449470342126,23.974590823096,-27.9651408964531));
#28924=CARTESIAN_POINT('Ctrl Pts',(-26.7468855769549,23.9598459295181,-27.9642244593242));
#28925=CARTESIAN_POINT('Ctrl Pts',(-26.7482134557164,23.9493458813364,-27.9635706274052));
#28926=CARTESIAN_POINT('Ctrl Pts',(-26.7634633710269,23.823793334209,-27.9557375364648));
#28927=CARTESIAN_POINT('Ctrl Pts',(-26.7712197835639,23.7080907305508,-27.9483637133435));
#28928=CARTESIAN_POINT('Ctrl Pts',(-26.7729215282811,23.5774614639784,-27.9398519451178));
#28929=CARTESIAN_POINT('Ctrl Pts',(-26.773012390264,23.5626892989409,-27.9388867844921));
#28930=CARTESIAN_POINT('Ctrl Pts',(-26.7727575709933,23.2110422962226,-27.9158503389308));
#28931=CARTESIAN_POINT('Ctrl Pts',(-26.7197020955071,22.8763495411284,-27.8922909362946));
#28932=CARTESIAN_POINT('Ctrl Pts',(-26.6152955177309,22.5544455036829,-27.8704582810525));
#28933=CARTESIAN_POINT('Ctrl Pts',(-26.614798743827,22.552917754895,-27.870354689524));
#28934=CARTESIAN_POINT('Ctrl Pts',(-26.6119154340057,22.5440730905102,-27.8697551139629));
#28935=CARTESIAN_POINT('Ctrl Pts',(-26.6095038130355,22.5367643002632,-27.8692602551711));
#28936=CARTESIAN_POINT('Ctrl Pts',(-26.5964312181218,22.4976176123845,-27.8666132174146));
#28937=CARTESIAN_POINT('Ctrl Pts',(-26.5852988693888,22.4659376270967,-27.8644834212579));
#28938=CARTESIAN_POINT('Ctrl Pts',(-26.5719199947845,22.4296861849303,-27.8620652658687));
#28939=CARTESIAN_POINT('Ctrl Pts',(-26.5701558720947,22.4249405702942,-27.8617490864555));
#28940=CARTESIAN_POINT('Ctrl Pts',(-26.5675387330221,22.4179507585522,-27.8612839635613));
#28941=CARTESIAN_POINT('Ctrl Pts',(-26.566694391418,22.4157033555097,-27.8611345028287));
#28942=CARTESIAN_POINT('Ctrl Pts',(-26.5651846726073,22.4116985015733,-27.8608683249617));
#28943=CARTESIAN_POINT('Ctrl Pts',(-26.5645202696188,22.4099406892609,-27.8607515491336));
#28944=CARTESIAN_POINT('Ctrl Pts',(-26.5631185154367,22.4062418509251,-27.8605059430021));
#28945=CARTESIAN_POINT('Ctrl Pts',(-26.5623808275813,22.4043009607798,-27.8603771336885));
#28946=CARTESIAN_POINT('Ctrl Pts',(-26.5604249396263,22.3991698681239,-27.8600367782566));
#28947=CARTESIAN_POINT('Ctrl Pts',(-26.5592035396146,22.3959808756096,-27.8598254253746));
#28948=CARTESIAN_POINT('Ctrl Pts',(-26.5536383735634,22.381519464416,-27.8588677722455));
#28949=CARTESIAN_POINT('Ctrl Pts',(-26.5492362416556,22.370269389447,-27.8581249519048));
#28950=CARTESIAN_POINT('Ctrl Pts',(-26.4445438957539,22.1070886160616,-27.840792771029));
#28951=CARTESIAN_POINT('Ctrl Pts',(-26.3128995881329,21.8687409220148,-27.8260083971645));
#28952=CARTESIAN_POINT('Ctrl Pts',(-26.0642755729425,21.5282726740257,-27.8023801385226));
#28953=CARTESIAN_POINT('Ctrl Pts',(-25.9672458494466,21.4132331838796,-27.7938688589953));
#28954=CARTESIAN_POINT('Ctrl Pts',(-25.8524451970975,21.2949838244306,-27.7841991169555));
#28955=CARTESIAN_POINT('Ctrl Pts',(-25.8422701725874,21.2846437536349,-27.7833453307919));
#28956=CARTESIAN_POINT('Ctrl Pts',(-25.827942769408,21.270279248488,-27.7821473958473));
#28957=CARTESIAN_POINT('Ctrl Pts',(-25.8238487559985,21.266196665622,-27.7818055721336));
#28958=CARTESIAN_POINT('Ctrl Pts',(-25.8169190234892,21.2593233737513,-27.7812277782856));
#28959=CARTESIAN_POINT('Ctrl Pts',(-25.8140890731733,21.2565268495332,-27.780992042157));
#28960=CARTESIAN_POINT('Ctrl Pts',(-25.8036506780703,21.2462498836954,-27.7801233228417));
#28961=CARTESIAN_POINT('Ctrl Pts',(-25.7960103334599,21.2388020563469,-27.77948903373));
#28962=CARTESIAN_POINT('Ctrl Pts',(-25.7854158988804,21.2285766879859,-27.7786115635794));
#28963=CARTESIAN_POINT('Ctrl Pts',(-25.7824932875299,21.2257665220486,-27.7783697169762));
#28964=CARTESIAN_POINT('Ctrl Pts',(-25.7751554492186,21.2187376030999,-27.7777630385599));
#28965=CARTESIAN_POINT('Ctrl Pts',(-25.7707335324531,21.2145258826228,-27.7773979209094));
#28966=CARTESIAN_POINT('Ctrl Pts',(-25.7634265288417,21.2076057209109,-27.7767953487298));
#28967=CARTESIAN_POINT('Ctrl Pts',(-25.7605483641336,21.2048899681197,-27.7765581957637));
#28968=CARTESIAN_POINT('Ctrl Pts',(-25.741055508043,21.1865648233036,-27.7749533329978));
#28969=CARTESIAN_POINT('Ctrl Pts',(-25.7242809224244,21.1711271084033,-27.7735786103019));
#28970=CARTESIAN_POINT('Ctrl Pts',(-25.6954679031304,21.1451695605413,-27.7712271134602));
#28971=CARTESIAN_POINT('Ctrl Pts',(-25.6835122501118,21.1345588326975,-27.7702541946075));
#28972=CARTESIAN_POINT('Ctrl Pts',(-25.6672101433751,21.1203059941518,-27.7689311469195));
#28973=CARTESIAN_POINT('Ctrl Pts',(-25.662932150155,21.1165856411649,-27.7685842831046));
#28974=CARTESIAN_POINT('Ctrl Pts',(-25.656175391532,21.1107408739595,-27.7680369475192));
#28975=CARTESIAN_POINT('Ctrl Pts',(-25.6537031628454,21.1086088922591,-27.7678367898858));
#28976=CARTESIAN_POINT('Ctrl Pts',(-25.6489330379125,21.1045078899317,-27.7674507924296));
#28977=CARTESIAN_POINT('Ctrl Pts',(-25.6466355982512,21.1025383412616,-27.767264974716));
#28978=CARTESIAN_POINT('Ctrl Pts',(-25.6412048158433,21.0978958956884,-27.7668259427331));
#28979=CARTESIAN_POINT('Ctrl Pts',(-25.6380691221251,21.0952257682511,-27.7665726146914));
#28980=CARTESIAN_POINT('Ctrl Pts',(-25.6288988996428,21.0874473526808,-27.7658322430834));
#28981=CARTESIAN_POINT('Ctrl Pts',(-25.6228507127432,21.0823552787908,-27.7653445347762));
#28982=CARTESIAN_POINT('Ctrl Pts',(-25.5788725063078,21.0456049528063,-27.7618025009631));
#28983=CARTESIAN_POINT('Ctrl Pts',(-25.5402394498579,21.0148018571047,-27.7587135933616));
#28984=CARTESIAN_POINT('Ctrl Pts',(-25.4129275838536,20.9179954581738,-27.7485986818957));
#28985=CARTESIAN_POINT('Ctrl Pts',(-25.3215652991524,20.8556686671606,-27.7414344773991));
#28986=CARTESIAN_POINT('Ctrl Pts',(-24.9349558788092,20.6200949718609,-27.7115257856852));
#28987=CARTESIAN_POINT('Ctrl Pts',(-24.6162611888996,20.4897250687589,-27.6875263106363));
#28988=CARTESIAN_POINT('Ctrl Pts',(-24.2806172334618,20.4113528533177,-27.6657409453154));
#28989=CARTESIAN_POINT('Ctrl Pts',(-24.2781867339425,20.4107883121538,-27.6655833814341));
#28990=CARTESIAN_POINT('Ctrl Pts',(-24.2634287327331,20.407378475753,-27.6646278195998));
#28991=CARTESIAN_POINT('Ctrl Pts',(-24.2510849843588,20.4046029149767,-27.6638335165579));
#28992=CARTESIAN_POINT('Ctrl Pts',(-24.2351775371141,20.4011243212991,-27.6628165265227));
#28993=CARTESIAN_POINT('Ctrl Pts',(-24.2316287748377,20.4003545707842,-27.6625900720807));
#28994=CARTESIAN_POINT('Ctrl Pts',(-24.2262088589102,20.3991885424487,-27.6622448701653));
#28995=CARTESIAN_POINT('Ctrl Pts',(-24.2243386561576,20.3987879328969,-27.6621258733536));
#28996=CARTESIAN_POINT('Ctrl Pts',(-24.2206815633181,20.39800796426,-27.6618934148032));
#28997=CARTESIAN_POINT('Ctrl Pts',(-24.2188947155602,20.3976284612798,-27.661779945442));
#28998=CARTESIAN_POINT('Ctrl Pts',(-24.2149636146895,20.3967970395991,-27.6615305508119));
#28999=CARTESIAN_POINT('Ctrl Pts',(-24.2128192285021,20.3963457897579,-27.6613946647799));
#29000=CARTESIAN_POINT('Ctrl Pts',(-24.208369616088,20.3954141823495,-27.6611130228035));
#29001=CARTESIAN_POINT('Ctrl Pts',(-24.2060643191928,20.3949341631727,-27.6609672864054));
#29002=CARTESIAN_POINT('Ctrl Pts',(-24.2001621286091,20.393711930532,-27.660594615446));
#29003=CARTESIAN_POINT('Ctrl Pts',(-24.1965644763096,20.3929733356918,-27.6603678870672));
#29004=CARTESIAN_POINT('Ctrl Pts',(-24.1861607333994,20.3908559840969,-27.659713456821));
#29005=CARTESIAN_POINT('Ctrl Pts',(-24.179351387116,20.3894930631268,-27.6592866420208));
#29006=CARTESIAN_POINT('Ctrl Pts',(-24.0023717711687,20.3546643853969,-27.6482315259105));
#29007=CARTESIAN_POINT('Ctrl Pts',(-23.8297521528159,20.3349618556343,-27.6383561242275));
#29008=CARTESIAN_POINT('Ctrl Pts',(-23.4484967478153,20.3224021052908,-27.6169332664649));
#29009=CARTESIAN_POINT('Ctrl Pts',(-23.2404663162241,20.3356915897079,-27.6054720796417));
#29010=CARTESIAN_POINT('Ctrl Pts',(-22.9156572943151,20.3882810206372,-27.5864908625305));
#29011=CARTESIAN_POINT('Ctrl Pts',(-22.7973442730704,20.4143477497127,-27.5793492315649));
#29012=CARTESIAN_POINT('Ctrl Pts',(-22.6704907839253,20.4498894622086,-27.5713335535967));
#29013=CARTESIAN_POINT('Ctrl Pts',(-22.6602091364746,20.4528254307333,-27.57068130512));
#29014=CARTESIAN_POINT('Ctrl Pts',(-22.64580687572,20.4570156885087,-27.5697639853748));
#29015=CARTESIAN_POINT('Ctrl Pts',(-22.6416737968816,20.4582271768493,-27.5695003134372));
#29016=CARTESIAN_POINT('Ctrl Pts',(-22.6345116909567,20.4603421339048,-27.5690426616133));
#29017=CARTESIAN_POINT('Ctrl Pts',(-22.6314815338907,20.4612417827247,-27.5688488069542));
#29018=CARTESIAN_POINT('Ctrl Pts',(-22.6251851071931,20.4631212660621,-27.5684455108588));
#29019=CARTESIAN_POINT('Ctrl Pts',(-22.6219190611988,20.4641018291953,-27.5682360457735));
#29020=CARTESIAN_POINT('Ctrl Pts',(-22.6142420528619,20.4664199824469,-27.567743049977));
#29021=CARTESIAN_POINT('Ctrl Pts',(-22.6098324002864,20.4677618529782,-27.5674593791032));
#29022=CARTESIAN_POINT('Ctrl Pts',(-22.5954669524367,20.4721669965229,-27.5665336309416));
#29023=CARTESIAN_POINT('Ctrl Pts',(-22.5855232044507,20.4752690544612,-27.5658902802643));
#29024=CARTESIAN_POINT('Ctrl Pts',(-22.4288690561347,20.5249736341063,-27.5557141453052));
#29025=CARTESIAN_POINT('Ctrl Pts',(-22.285690421506,20.5819730215234,-27.5458333273703));
#29026=CARTESIAN_POINT('Ctrl Pts',(-21.9946440933085,20.7227276221636,-27.5244900953961));
#29027=CARTESIAN_POINT('Ctrl Pts',(-21.8482018975906,20.80838630508,-27.5129986719099));
#29028=CARTESIAN_POINT('Ctrl Pts',(-21.5626078206911,21.0071681203855,-27.4894673343863));
#29029=CARTESIAN_POINT('Ctrl Pts',(-21.4247465032278,21.1212093742254,-27.4774738837223));
#29030=CARTESIAN_POINT('Ctrl Pts',(-21.2889783856318,21.2539764858177,-27.4655095693023));
#29031=CARTESIAN_POINT('Ctrl Pts',(-21.280966154777,21.2618942138149,-27.4648029511396));
#29032=CARTESIAN_POINT('Ctrl Pts',(-21.2705396108174,21.2723063939006,-27.4638828823967));
#29033=CARTESIAN_POINT('Ctrl Pts',(-21.268087709431,21.2747628409691,-27.463666481054));
#29034=CARTESIAN_POINT('Ctrl Pts',(-21.264313586221,21.2785561973325,-27.4633333300623));
#29035=CARTESIAN_POINT('Ctrl Pts',(-21.2629885678664,21.2798903011676,-27.4632163575272));
#29036=CARTESIAN_POINT('Ctrl Pts',(-21.2603771441525,21.2825242374737,-27.4629858029898));
#29037=CARTESIAN_POINT('Ctrl Pts',(-21.2590906850647,21.2838239977544,-27.462872216964));
#29038=CARTESIAN_POINT('Ctrl Pts',(-21.2562289940121,21.2867202034551,-27.4626195284817));
#29039=CARTESIAN_POINT('Ctrl Pts',(-21.2546543254948,21.2883171948221,-27.4624804710883));
#29040=CARTESIAN_POINT('Ctrl Pts',(-21.2513809356743,21.2916439279018,-27.46219136977));
#29041=CARTESIAN_POINT('Ctrl Pts',(-21.2496824956679,21.2933739462267,-27.462041348131));
#29042=CARTESIAN_POINT('Ctrl Pts',(-21.2452999143994,21.2978480987988,-27.4616541875922));
#29043=CARTESIAN_POINT('Ctrl Pts',(-21.2426187111102,21.3005951249417,-27.4614172783475));
#29044=CARTESIAN_POINT('Ctrl Pts',(-21.2347966425239,21.3086379214079,-27.4607259564314));
#29045=CARTESIAN_POINT('Ctrl Pts',(-21.229669011587,21.3139466124558,-27.4602725568183));
#29046=CARTESIAN_POINT('Ctrl Pts',(-21.1761827372135,21.3697035767936,-27.4555402873246));
#29047=CARTESIAN_POINT('Ctrl Pts',(-21.1294547676214,21.4216987989674,-27.4513812887903));
#29048=CARTESIAN_POINT('Ctrl Pts',(-21.0363283071697,21.5323604847526,-27.4429387710752));
#29049=CARTESIAN_POINT('Ctrl Pts',(-20.9902068916258,21.5912040813125,-27.4386691064423));
#29050=CARTESIAN_POINT('Ctrl Pts',(-20.7433623807068,21.9297618533628,-27.4149813532217));
#29051=CARTESIAN_POINT('Ctrl Pts',(-20.5864467909286,22.238584460576,-27.3963216915705));
#29052=CARTESIAN_POINT('Ctrl Pts',(-20.4750288076411,22.5861228419328,-27.3742550090276));
#29053=CARTESIAN_POINT('Ctrl Pts',(-20.4688929050841,22.605916875279,-27.3729959150457));
#29054=CARTESIAN_POINT('Ctrl Pts',(-20.4611429728201,22.6317976834487,-27.3713462241427));
#29055=CARTESIAN_POINT('Ctrl Pts',(-20.4593551848093,22.6378322529165,-27.370961328668));
#29056=CARTESIAN_POINT('Ctrl Pts',(-20.4566316490513,22.647125248447,-27.3703682217717));
#29057=CARTESIAN_POINT('Ctrl Pts',(-20.4556833393844,22.6503800023115,-27.3701604214003));
#29058=CARTESIAN_POINT('Ctrl Pts',(-20.4538191165052,22.6568161166219,-27.3697493613167));
#29059=CARTESIAN_POINT('Ctrl Pts',(-20.4529029662033,22.6599974044978,-27.3695461096418));
#29060=CARTESIAN_POINT('Ctrl Pts',(-20.45088326008,22.6670515931156,-27.3690952616911));
#29061=CARTESIAN_POINT('Ctrl Pts',(-20.449782059596,22.6709251574218,-27.3688475889029));
#29062=CARTESIAN_POINT('Ctrl Pts',(-20.4466572488379,22.6819957864979,-27.368139435214));
#29063=CARTESIAN_POINT('Ctrl Pts',(-20.4446514279513,22.6891978073771,-27.3676783752861));
#29064=CARTESIAN_POINT('Ctrl Pts',(-20.432031698148,22.735127460427,-27.3647356193985));
#29065=CARTESIAN_POINT('Ctrl Pts',(-20.4221177325538,22.7740421918965,-27.3622312776528));
#29066=CARTESIAN_POINT('Ctrl Pts',(-20.3948148981791,22.8902477932376,-27.3547162184903));
#29067=CARTESIAN_POINT('Ctrl Pts',(-20.3795469005245,22.9680008883995,-27.3496392843041));
#29068=CARTESIAN_POINT('Ctrl Pts',(-20.3434960960042,23.195676434859,-27.3346300451783));
#29069=CARTESIAN_POINT('Ctrl Pts',(-20.3303887193855,23.346586899906,-27.3244934663298));
#29070=CARTESIAN_POINT('Ctrl Pts',(-20.3247602752572,23.6926575135823,-27.301095174387));
#29071=CARTESIAN_POINT('Ctrl Pts',(-20.3392647210968,23.8873678111172,-27.2878124174258));
#29072=CARTESIAN_POINT('Ctrl Pts',(-20.3730184054975,24.0900803510924,-27.2745017022544));
#29073=CARTESIAN_POINT('Ctrl Pts',(-20.3748179618797,24.1005670473554,-27.2738146778478));
#29074=CARTESIAN_POINT('Ctrl Pts',(-20.383380451811,24.1490230904487,-27.270647948827));
#29075=CARTESIAN_POINT('Ctrl Pts',(-20.3907730311557,24.1868800274762,-27.2681961000597));
#29076=CARTESIAN_POINT('Ctrl Pts',(-20.3998370119586,24.2292386473724,-27.2654846098623));
#29077=CARTESIAN_POINT('Ctrl Pts',(-20.4008404656162,24.2338779634932,-27.265188066928));
#29078=CARTESIAN_POINT('Ctrl Pts',(-20.4023675379607,24.2408634257542,-27.2647422285662));
#29079=CARTESIAN_POINT('Ctrl Pts',(-20.4028835323434,24.2432112049104,-27.2645924984833));
#29080=CARTESIAN_POINT('Ctrl Pts',(-20.4037820055221,24.2472775600696,-27.2643333660178));
#29081=CARTESIAN_POINT('Ctrl Pts',(-20.4041632657479,24.2489963996338,-27.2642238932724));
#29082=CARTESIAN_POINT('Ctrl Pts',(-20.4049525588973,24.2525410362477,-27.2639982647894));
#29083=CARTESIAN_POINT('Ctrl Pts',(-20.4053607726679,24.2543667884236,-27.2638821201531));
#29084=CARTESIAN_POINT('Ctrl Pts',(-20.4063277117511,24.2586738456541,-27.2636082932666));
#29085=CARTESIAN_POINT('Ctrl Pts',(-20.4068877866776,24.2611548536931,-27.2634506892497));
#29086=CARTESIAN_POINT('Ctrl Pts',(-20.4080817631305,24.2664149075113,-27.263116818007));
#29087=CARTESIAN_POINT('Ctrl Pts',(-20.408716416197,24.2691937827882,-27.2629405941249));
#29088=CARTESIAN_POINT('Ctrl Pts',(-20.4104444595008,24.276714168369,-27.2624641079194));
#29089=CARTESIAN_POINT('Ctrl Pts',(-20.4115449083338,24.281454074057,-27.2621642465351));
#29090=CARTESIAN_POINT('Ctrl Pts',(-20.414986669664,24.2961276522568,-27.2612373102804));
#29091=CARTESIAN_POINT('Ctrl Pts',(-20.4173644641279,24.3060528251512,-27.2606122661771));
#29092=CARTESIAN_POINT('Ctrl Pts',(-20.4264149244297,24.3430537504568,-27.2582887618035));
#29093=CARTESIAN_POINT('Ctrl Pts',(-20.4333919821465,24.3700547034005,-27.2566065343163));
#29094=CARTESIAN_POINT('Ctrl Pts',(-20.463100504303,24.4791589201139,-27.2498506205596));
#29095=CARTESIAN_POINT('Ctrl Pts',(-20.4887342817251,24.5604421301773,-27.2449130157355));
#29096=CARTESIAN_POINT('Ctrl Pts',(-20.6187277574231,24.9219992695622,-27.2229963851145));
#29097=CARTESIAN_POINT('Ctrl Pts',(-20.7585553201252,25.187922908098,-27.2068575406488));
#29098=CARTESIAN_POINT('Ctrl Pts',(-20.9453378837994,25.4478776582449,-27.1881204528247));
#29099=CARTESIAN_POINT('Ctrl Pts',(-20.9577988984852,25.4648662199832,-27.1868817434871));
#29100=CARTESIAN_POINT('Ctrl Pts',(-20.9756751268422,25.4887430464348,-27.1851197306153));
#29101=CARTESIAN_POINT('Ctrl Pts',(-20.9809533847627,25.4957334955659,-27.1846012754538));
#29102=CARTESIAN_POINT('Ctrl Pts',(-20.9923596098454,25.5107123575417,-27.1834846887523));
#29103=CARTESIAN_POINT('Ctrl Pts',(-20.998496631977,25.5186937305589,-27.1828862334092));
#29104=CARTESIAN_POINT('Ctrl Pts',(-21.0079814435464,25.5309101037726,-27.1819647670412));
#29105=CARTESIAN_POINT('Ctrl Pts',(-21.011302676566,25.5351657126906,-27.1816427452628));
#29106=CARTESIAN_POINT('Ctrl Pts',(-21.0159069862475,25.5410349076958,-27.181197191485));
#29107=CARTESIAN_POINT('Ctrl Pts',(-21.0171809547537,25.5426556531512,-27.181074002872));
#29108=CARTESIAN_POINT('Ctrl Pts',(-21.0226607669264,25.5496133308452,-27.1805445151488));
#29109=CARTESIAN_POINT('Ctrl Pts',(-21.026881906823,25.5549381486916,-27.1801376376653));
#29110=CARTESIAN_POINT('Ctrl Pts',(-21.0354179279221,25.565636358547,-27.1793168042112));
#29111=CARTESIAN_POINT('Ctrl Pts',(-21.0397332663463,25.5710093382107,-27.1789028319518));
#29112=CARTESIAN_POINT('Ctrl Pts',(-21.0619358400896,25.5984726224765,-27.1767779337644));
#29113=CARTESIAN_POINT('Ctrl Pts',(-21.0800970920959,25.6203388879972,-27.1750563413133));
#29114=CARTESIAN_POINT('Ctrl Pts',(-21.1030807607007,25.6472782177658,-27.1728967126854));
#29115=CARTESIAN_POINT('Ctrl Pts',(-21.1076340105721,25.6525800903421,-27.1724697864939));
#29116=CARTESIAN_POINT('Ctrl Pts',(-21.1150476112965,25.6611560014915,-27.1717761223117));
#29117=CARTESIAN_POINT('Ctrl Pts',(-21.117897421736,25.6644391558828,-27.1715098220131));
#29118=CARTESIAN_POINT('Ctrl Pts',(-21.1229681233152,25.6702570884826,-27.1710365991958));
#29119=CARTESIAN_POINT('Ctrl Pts',(-21.1251863678478,25.6727941734044,-27.1708297871987));
#29120=CARTESIAN_POINT('Ctrl Pts',(-21.1298470893764,25.6781079621941,-27.1703956851505));
#29121=CARTESIAN_POINT('Ctrl Pts',(-21.1322903730021,25.6808839491996,-27.1701683615188));
#29122=CARTESIAN_POINT('Ctrl Pts',(-21.1387018024524,25.6881431950954,-27.1695724772847));
#29123=CARTESIAN_POINT('Ctrl Pts',(-21.142677659514,25.6926195969837,-27.1692035932176));
#29124=CARTESIAN_POINT('Ctrl Pts',(-21.1601949872662,25.7122319408333,-27.1675810738168));
#29125=CARTESIAN_POINT('Ctrl Pts',(-21.1738666514183,25.7272504988128,-27.166321947949));
#29126=CARTESIAN_POINT('Ctrl Pts',(-21.2717601239595,25.8327671696733,-27.1573551654457));
#29127=CARTESIAN_POINT('Ctrl Pts',(-21.3609756864225,25.9184714850618,-27.1494305534831));
#29128=CARTESIAN_POINT('Ctrl Pts',(-21.5751204954169,26.1017256264431,-27.1309314082777));
#29129=CARTESIAN_POINT('Ctrl Pts',(-21.7027636106987,26.1956141639096,-27.1202558090638));
#29130=CARTESIAN_POINT('Ctrl Pts',(-21.9142445350118,26.3283746354195,-27.1033532466859));
#29131=CARTESIAN_POINT('Ctrl Pts',(-21.9937381269423,26.3736798513359,-27.0971618111161));
#29132=CARTESIAN_POINT('Ctrl Pts',(-22.075036065511,26.4155368003841,-27.0910469152906));
#29133=CARTESIAN_POINT('Origin',(-23.5502525316942,23.5502525316942,-77.3107734492734));
#29134=CARTESIAN_POINT('',(-22.0750360129136,26.4155367733039,-25.5932554334314));
#29135=CARTESIAN_POINT('',(-22.0750360153461,26.4155367745563,-25.8427499795855));
#29136=CARTESIAN_POINT('',(-22.0750360153461,26.4155367745563,-77.3107734492734));
#29137=CARTESIAN_POINT('',(-26.7730012222585,23.5532068148341,-26.4393797936538));
#29138=CARTESIAN_POINT('Ctrl Pts',(-22.0750360129136,26.4155367733039,-25.5932554334314));
#29139=CARTESIAN_POINT('Ctrl Pts',(-22.0466160857789,26.400904526575,-25.5952554284658));
#29140=CARTESIAN_POINT('Ctrl Pts',(-22.0184151274967,26.3858501008074,-25.5972702832576));
#29141=CARTESIAN_POINT('Ctrl Pts',(-21.8659511005368,26.3015223303977,-25.6083320059081));
#29142=CARTESIAN_POINT('Ctrl Pts',(-21.7461716184923,26.2245075153379,-25.6176508306857));
#29143=CARTESIAN_POINT('Ctrl Pts',(-21.4613038304606,26.0134772959779,-25.6413397160578));
#29144=CARTESIAN_POINT('Ctrl Pts',(-21.303635164313,25.8705735223199,-25.6559036723081));
#29145=CARTESIAN_POINT('Ctrl Pts',(-21.0944527268427,25.6395215795845,-25.6765955928807));
#29146=CARTESIAN_POINT('Ctrl Pts',(-21.0311771901896,25.5627787652145,-25.6830726758594));
#29147=CARTESIAN_POINT('Ctrl Pts',(-20.9676130371031,25.4779801495591,-25.6897174714637));
#29148=CARTESIAN_POINT('Ctrl Pts',(-20.9636975148505,25.4727232530088,-25.6901273803765));
#29149=CARTESIAN_POINT('Ctrl Pts',(-20.9583104462015,25.4654444387193,-25.6906921223488));
#29150=CARTESIAN_POINT('Ctrl Pts',(-20.956825208201,25.4634327461919,-25.6908479065927));
#29151=CARTESIAN_POINT('Ctrl Pts',(-20.9542831361505,25.4599812165819,-25.6911146791055));
#29152=CARTESIAN_POINT('Ctrl Pts',(-20.9532251579762,25.4585422300046,-25.6912257477665));
#29153=CARTESIAN_POINT('Ctrl Pts',(-20.9511607803285,25.4557295140885,-25.6914425498431));
#29154=CARTESIAN_POINT('Ctrl Pts',(-20.9501542760336,25.4543558701116,-25.6915482903905));
#29155=CARTESIAN_POINT('Ctrl Pts',(-20.9477186181656,25.4510262320079,-25.691804264714));
#29156=CARTESIAN_POINT('Ctrl Pts',(-20.9462905770222,25.4490694184909,-25.6919544201115));
#29157=CARTESIAN_POINT('Ctrl Pts',(-20.941956907097,25.4431170024411,-25.692410333838));
#29158=CARTESIAN_POINT('Ctrl Pts',(-20.939058241125,25.4391163032716,-25.6927156072367));
#29159=CARTESIAN_POINT('Ctrl Pts',(-20.9101819219358,25.3990680971417,-25.6957601621768));
#29160=CARTESIAN_POINT('Ctrl Pts',(-20.8849415955605,25.3624914566933,-25.6984493069875));
#29161=CARTESIAN_POINT('Ctrl Pts',(-20.8147579481775,25.2561459785098,-25.7060455061551));
#29162=CARTESIAN_POINT('Ctrl Pts',(-20.7717398914447,25.1851447816814,-25.7108506896358));
#29163=CARTESIAN_POINT('Ctrl Pts',(-20.6356006970802,24.9395194057876,-25.7268641983878));
#29164=CARTESIAN_POINT('Ctrl Pts',(-20.5558286481992,24.7580144686285,-25.7377197541403));
#29165=CARTESIAN_POINT('Ctrl Pts',(-20.4353490094598,24.3969530827771,-25.759239959292));
#29166=CARTESIAN_POINT('Ctrl Pts',(-20.3923577359698,24.2189910478363,-25.7698177668922));
#29167=CARTESIAN_POINT('Ctrl Pts',(-20.3628658909522,24.0265166909956,-25.7816551154909));
#29168=CARTESIAN_POINT('Ctrl Pts',(-20.3611171214491,24.0146623465175,-25.7823856273575));
#29169=CARTESIAN_POINT('Ctrl Pts',(-20.3587995697496,23.9983217230218,-25.783394695097));
#29170=CARTESIAN_POINT('Ctrl Pts',(-20.3581740435405,23.9938434847684,-25.7836714519002));
#29171=CARTESIAN_POINT('Ctrl Pts',(-20.3571195539444,23.9861764941586,-25.784145650055));
#29172=CARTESIAN_POINT('Ctrl Pts',(-20.3566859360818,23.9829883794347,-25.7843429437593));
#29173=CARTESIAN_POINT('Ctrl Pts',(-20.3558517992045,23.9767859643919,-25.7847269927303));
#29174=CARTESIAN_POINT('Ctrl Pts',(-20.3554507705869,23.9737717355901,-25.7849137316051));
#29175=CARTESIAN_POINT('Ctrl Pts',(-20.3545020456995,23.9665628592628,-25.7853605804908));
#29176=CARTESIAN_POINT('Ctrl Pts',(-20.3539583423078,23.9623677003015,-25.7856208165796));
#29177=CARTESIAN_POINT('Ctrl Pts',(-20.3523831134483,23.9500227526658,-25.7863871852772));
#29178=CARTESIAN_POINT('Ctrl Pts',(-20.3513744929227,23.9418701216849,-25.7868940416044));
#29179=CARTESIAN_POINT('Ctrl Pts',(-20.3433305143562,23.8747458198268,-25.7910734740989));
#29180=CARTESIAN_POINT('Ctrl Pts',(-20.3378957416415,23.8155972373785,-25.7947963390178));
#29181=CARTESIAN_POINT('Ctrl Pts',(-20.3285759293287,23.6701510508368,-25.8040577793937));
#29182=CARTESIAN_POINT('Ctrl Pts',(-20.3265203635264,23.5837865669375,-25.8096498790746));
#29183=CARTESIAN_POINT('Ctrl Pts',(-20.3312443887873,23.2955008810514,-25.8286127636319));
#29184=CARTESIAN_POINT('Ctrl Pts',(-20.3535312457334,23.0943235734584,-25.8423650085166));
#29185=CARTESIAN_POINT('Ctrl Pts',(-20.4268977295717,22.7401297703474,-25.8667698532619));
#29186=CARTESIAN_POINT('Ctrl Pts',(-20.4708981446793,22.5862844333187,-25.8774245470127));
#29187=CARTESIAN_POINT('Ctrl Pts',(-20.5293837507614,22.4275069688881,-25.8880659182035));
#29188=CARTESIAN_POINT('Ctrl Pts',(-20.5326689630047,22.4187070391859,-25.8886544743528));
#29189=CARTESIAN_POINT('Ctrl Pts',(-20.5371344159718,22.4069034181398,-25.8894421585468));
#29190=CARTESIAN_POINT('Ctrl Pts',(-20.5382807193698,22.4038870678297,-25.8896432916494));
#29191=CARTESIAN_POINT('Ctrl Pts',(-20.5400845987286,22.3991617747834,-25.889958129409));
#29192=CARTESIAN_POINT('Ctrl Pts',(-20.5407391001022,22.3974516727391,-25.8900720191904));
#29193=CARTESIAN_POINT('Ctrl Pts',(-20.5419994419277,22.3941669999518,-25.8902906728358));
#29194=CARTESIAN_POINT('Ctrl Pts',(-20.5426050573807,22.3925923574354,-25.890395449145));
#29195=CARTESIAN_POINT('Ctrl Pts',(-20.5440429341088,22.3888625216875,-25.8906435273757));
#29196=CARTESIAN_POINT('Ctrl Pts',(-20.5448762757092,22.3867077495736,-25.8907867630043));
#29197=CARTESIAN_POINT('Ctrl Pts',(-20.5473027640423,22.3804535752124,-25.8912022672793));
#29198=CARTESIAN_POINT('Ctrl Pts',(-20.5489019943193,22.3763565150168,-25.8914741690518));
#29199=CARTESIAN_POINT('Ctrl Pts',(-20.5596986649789,22.3488628679761,-25.8932969084707));
#29200=CARTESIAN_POINT('Ctrl Pts',(-20.5691615391037,22.3255704743457,-25.8948319705014));
#29201=CARTESIAN_POINT('Ctrl Pts',(-20.5992255527518,22.2539833284593,-25.8995285319187));
#29202=CARTESIAN_POINT('Ctrl Pts',(-20.6207358953281,22.2060773081627,-25.9026412468845));
#29203=CARTESIAN_POINT('Ctrl Pts',(-20.7266384798453,21.9848526626355,-25.9169691570747));
#29204=CARTESIAN_POINT('Ctrl Pts',(-20.8253061598993,21.8187926760373,-25.9276078750564));
#29205=CARTESIAN_POINT('Ctrl Pts',(-21.075301156244,21.4728763016167,-25.9514974228584));
#29206=CARTESIAN_POINT('Ctrl Pts',(-21.2325934954969,21.298739857563,-25.9647842345868));
#29207=CARTESIAN_POINT('Ctrl Pts',(-21.4188107304198,21.1329587006397,-25.9799075518166));
#29208=CARTESIAN_POINT('Ctrl Pts',(-21.4303589499629,21.1228249205734,-25.9808428965056));
#29209=CARTESIAN_POINT('Ctrl Pts',(-21.4461973801844,21.1091256221012,-25.9821224904774));
#29210=CARTESIAN_POINT('Ctrl Pts',(-21.4504251679843,21.1054879803865,-25.9824637443543));
#29211=CARTESIAN_POINT('Ctrl Pts',(-21.4571285021402,21.0997505633829,-25.9830043350012));
#29212=CARTESIAN_POINT('Ctrl Pts',(-21.4595978284044,21.0976435104106,-25.983203371009));
#29213=CARTESIAN_POINT('Ctrl Pts',(-21.4643789991388,21.0935762494489,-25.983588552876));
#29214=CARTESIAN_POINT('Ctrl Pts',(-21.4666904348543,21.0916155641702,-25.9837746788138));
#29215=CARTESIAN_POINT('Ctrl Pts',(-21.4721801403489,21.086972199082,-25.9842165239373));
#29216=CARTESIAN_POINT('Ctrl Pts',(-21.475360838293,21.0842924101387,-25.9844723613647));
#29217=CARTESIAN_POINT('Ctrl Pts',(-21.4819520062175,21.078761026196,-25.9850021822777));
#29218=CARTESIAN_POINT('Ctrl Pts',(-21.4853632051681,21.0759103172223,-25.9852762012896));
#29219=CARTESIAN_POINT('Ctrl Pts',(-21.5044794001666,21.0600021423594,-25.986810771898));
#29220=CARTESIAN_POINT('Ctrl Pts',(-21.5203020622721,21.0470873817229,-25.9880771181759));
#29221=CARTESIAN_POINT('Ctrl Pts',(-21.5618579938909,21.0138217640207,-25.9913936382917));
#29222=CARTESIAN_POINT('Ctrl Pts',(-21.5877806383283,20.9937123273048,-25.9934533155369));
#29223=CARTESIAN_POINT('Ctrl Pts',(-21.7038148360023,20.9065038095629,-26.0026352737741));
#29224=CARTESIAN_POINT('Ctrl Pts',(-21.797083216875,20.8437544101364,-26.0099213445031));
#29225=CARTESIAN_POINT('Ctrl Pts',(-22.0284305272443,20.7050902457756,-26.0277530298547));
#29226=CARTESIAN_POINT('Ctrl Pts',(-22.1691708408958,20.6341768044259,-26.0384172166561));
#29227=CARTESIAN_POINT('Ctrl Pts',(-22.4863892306049,20.5024755421486,-26.0616561809228));
#29228=CARTESIAN_POINT('Ctrl Pts',(-22.6641432575376,20.4461297931122,-26.0741841150298));
#29229=CARTESIAN_POINT('Ctrl Pts',(-22.8568016817507,20.4029726116038,-26.0866236460597));
#29230=CARTESIAN_POINT('Ctrl Pts',(-22.8678295755585,20.4005630399126,-26.0873317600395));
#29231=CARTESIAN_POINT('Ctrl Pts',(-22.8822673444627,20.3974878057661,-26.0882534838102));
#29232=CARTESIAN_POINT('Ctrl Pts',(-22.885665780598,20.3967696828498,-26.0884700575069));
#29233=CARTESIAN_POINT('Ctrl Pts',(-22.8909061585447,20.3956711870409,-26.0888034110007));
#29234=CARTESIAN_POINT('Ctrl Pts',(-22.8927472699457,20.3952869327319,-26.0889204141328));
#29235=CARTESIAN_POINT('Ctrl Pts',(-22.8962325141349,20.3945627183802,-26.0891416842019));
#29236=CARTESIAN_POINT('Ctrl Pts',(-22.8978765679066,20.3942224331177,-26.0892459693726));
#29237=CARTESIAN_POINT('Ctrl Pts',(-22.9016964896863,20.3934349004004,-26.0894880603117));
#29238=CARTESIAN_POINT('Ctrl Pts',(-22.903872551095,20.3929886184895,-26.0896258096721));
#29239=CARTESIAN_POINT('Ctrl Pts',(-22.9083523754007,20.3920746903083,-26.0899090652074));
#29240=CARTESIAN_POINT('Ctrl Pts',(-22.9106561928953,20.3916073138913,-26.0900545557954));
#29241=CARTESIAN_POINT('Ctrl Pts',(-22.9223004883275,20.3892582927471,-26.0907890267353));
#29242=CARTESIAN_POINT('Ctrl Pts',(-22.9316488971708,20.38741553049,-26.0913757932439));
#29243=CARTESIAN_POINT('Ctrl Pts',(-23.031887606566,20.3681178628545,-26.0976378217376));
#29244=CARTESIAN_POINT('Ctrl Pts',(-23.1234912616387,20.3545426362438,-26.1031002694851));
#29245=CARTESIAN_POINT('Ctrl Pts',(-23.36549370013,20.3292734116293,-26.1171488011011));
#29246=CARTESIAN_POINT('Ctrl Pts',(-23.5163487217757,20.3241560729969,-26.1255285187324));
#29247=CARTESIAN_POINT('Ctrl Pts',(-23.8323603099707,20.3356129472515,-26.1432025886247));
#29248=CARTESIAN_POINT('Ctrl Pts',(-23.9969887292421,20.3543312104419,-26.1524859298898));
#29249=CARTESIAN_POINT('Ctrl Pts',(-24.2533264134514,20.4036757062538,-26.1677018267937));
#29250=CARTESIAN_POINT('Ctrl Pts',(-24.3463526069307,20.4259157198697,-26.1733833970995));
#29251=CARTESIAN_POINT('Ctrl Pts',(-24.4480199986554,20.4550571408937,-26.1798212244726));
#29252=CARTESIAN_POINT('Ctrl Pts',(-24.4577801060651,20.4579047779642,-26.1804415992924));
#29253=CARTESIAN_POINT('Ctrl Pts',(-24.4715302085239,20.461987250421,-26.181318947267));
#29254=CARTESIAN_POINT('Ctrl Pts',(-24.4755315993695,20.4631837517677,-26.1815746650283));
#29255=CARTESIAN_POINT('Ctrl Pts',(-24.4825257580295,20.4652899746741,-26.1820223507182));
#29256=CARTESIAN_POINT('Ctrl Pts',(-24.4855195550988,20.4661962835715,-26.1822142065693));
#29257=CARTESIAN_POINT('Ctrl Pts',(-24.4917995457593,20.4681074034527,-26.1826171357466));
#29258=CARTESIAN_POINT('Ctrl Pts',(-24.4950854591017,20.4691131141441,-26.1828282383828));
#29259=CARTESIAN_POINT('Ctrl Pts',(-24.5029163974237,20.4715236134287,-26.1833319959671));
#29260=CARTESIAN_POINT('Ctrl Pts',(-24.5074599231468,20.4729332108256,-26.1836248086719));
#29261=CARTESIAN_POINT('Ctrl Pts',(-24.5170340081362,20.4759267593049,-26.1842429499482));
#29262=CARTESIAN_POINT('Ctrl Pts',(-24.5220638291835,20.4775130081565,-26.1845683535597));
#29263=CARTESIAN_POINT('Ctrl Pts',(-24.5631955841039,20.4905957771221,-26.1872347919139));
#29264=CARTESIAN_POINT('Ctrl Pts',(-24.5990948177383,20.5027153712128,-26.1895963136385));
#29265=CARTESIAN_POINT('Ctrl Pts',(-24.7044609709276,20.5403692459345,-26.1966327866888));
#29266=CARTESIAN_POINT('Ctrl Pts',(-24.7732675739397,20.5676651825905,-26.2013652384361));
#29267=CARTESIAN_POINT('Ctrl Pts',(-24.9350324553696,20.6383771541438,-26.2128267337714));
#29268=CARTESIAN_POINT('Ctrl Pts',(-25.0269740096375,20.6839091609418,-26.2196164624709));
#29269=CARTESIAN_POINT('Ctrl Pts',(-25.1924470295556,20.7759327578964,-26.2323069832667));
#29270=CARTESIAN_POINT('Ctrl Pts',(-25.2665739945196,20.8211697425376,-26.2381787127077));
#29271=CARTESIAN_POINT('Ctrl Pts',(-25.5088286091214,20.9827863629253,-26.2578918473817));
#29272=CARTESIAN_POINT('Ctrl Pts',(-25.6677170236228,21.1121657469431,-26.2717348321048));
#29273=CARTESIAN_POINT('Ctrl Pts',(-25.821858189922,21.2641925738402,-26.2853852131768));
#29274=CARTESIAN_POINT('Ctrl Pts',(-25.8303793546975,21.2726915381514,-26.2861405184911));
#29275=CARTESIAN_POINT('Ctrl Pts',(-25.8413604848419,21.2837674567762,-26.2871145266407));
#29276=CARTESIAN_POINT('Ctrl Pts',(-25.8438639208011,21.2863008882499,-26.2873366217572));
#29277=CARTESIAN_POINT('Ctrl Pts',(-25.8476953866011,21.2901911397318,-26.2876765952293));
#29278=CARTESIAN_POINT('Ctrl Pts',(-25.8490264155081,21.2915449813149,-26.2877947113037));
#29279=CARTESIAN_POINT('Ctrl Pts',(-25.8516493791459,21.2942176203209,-26.2880274949857));
#29280=CARTESIAN_POINT('Ctrl Pts',(-25.8529413702411,21.2955363447514,-26.2881421668035));
#29281=CARTESIAN_POINT('Ctrl Pts',(-25.8558175709315,21.298477109276,-26.288397468802));
#29282=CARTESIAN_POINT('Ctrl Pts',(-25.8574011985168,21.3000997074586,-26.2885380526686));
#29283=CARTESIAN_POINT('Ctrl Pts',(-25.8606679701239,21.3034539435115,-26.2888280899896));
#29284=CARTESIAN_POINT('Ctrl Pts',(-25.8623508835512,21.3051858054197,-26.2889775252629));
#29285=CARTESIAN_POINT('Ctrl Pts',(-25.8666881331037,21.3096592556299,-26.2893627090665));
#29286=CARTESIAN_POINT('Ctrl Pts',(-25.8693395588278,21.3124036795251,-26.2895982312024));
#29287=CARTESIAN_POINT('Ctrl Pts',(-25.9037394696299,21.3481369526412,-26.292654723985));
#29288=CARTESIAN_POINT('Ctrl Pts',(-25.93478833906,21.3817960983765,-26.2954223621426));
#29289=CARTESIAN_POINT('Ctrl Pts',(-26.0353763748323,21.4956149352642,-26.3044645540959));
#29290=CARTESIAN_POINT('Ctrl Pts',(-26.101678464393,21.578551275761,-26.3105516153088));
#29291=CARTESIAN_POINT('Ctrl Pts',(-26.1877841110832,21.6978948818709,-26.3188719448097));
#29292=CARTESIAN_POINT('Ctrl Pts',(-26.2111581172451,21.7316312805218,-26.3211782084304));
#29293=CARTESIAN_POINT('Ctrl Pts',(-26.2578370083805,21.8018316399261,-26.3259025378353));
#29294=CARTESIAN_POINT('Ctrl Pts',(-26.2810645145316,21.8383368609585,-26.3283193986257));
#29295=CARTESIAN_POINT('Ctrl Pts',(-26.4412065254279,22.1015791237185,-26.3455359781616));
#29296=CARTESIAN_POINT('Ctrl Pts',(-26.5504225488228,22.3439262135446,-26.3603971229294));
#29297=CARTESIAN_POINT('Ctrl Pts',(-26.6336827338814,22.612781136021,-26.3774560674618));
#29298=CARTESIAN_POINT('Ctrl Pts',(-26.6384817946835,22.6287133667779,-26.3784685467288));
#29299=CARTESIAN_POINT('Ctrl Pts',(-26.644776610432,22.6502128086864,-26.3798371630166));
#29300=CARTESIAN_POINT('Ctrl Pts',(-26.6463811801509,22.6557481055433,-26.3801897385123));
#29301=CARTESIAN_POINT('Ctrl Pts',(-26.6488765163352,22.6644434419306,-26.3807439323971));
#29302=CARTESIAN_POINT('Ctrl Pts',(-26.6497773216551,22.6676006082332,-26.3809452227713));
#29303=CARTESIAN_POINT('Ctrl Pts',(-26.6514978781004,22.673665973772,-26.3813320660291));
#29304=CARTESIAN_POINT('Ctrl Pts',(-26.6523183672854,22.6765739616839,-26.3815175946163));
#29305=CARTESIAN_POINT('Ctrl Pts',(-26.6542369828561,22.6834107176471,-26.3819539199041));
#29306=CARTESIAN_POINT('Ctrl Pts',(-26.6553317398057,22.6873404187035,-26.3822048260951));
#29307=CARTESIAN_POINT('Ctrl Pts',(-26.6575744862882,22.6954504341637,-26.3827228721671));
#29308=CARTESIAN_POINT('Ctrl Pts',(-26.658721507635,22.6996310055359,-26.3829900430241));
#29309=CARTESIAN_POINT('Ctrl Pts',(-26.661656323595,22.7104127977774,-26.3836794166359));
#29310=CARTESIAN_POINT('Ctrl Pts',(-26.6634315399716,22.7170173931024,-26.3841020278085));
#29311=CARTESIAN_POINT('Ctrl Pts',(-26.6776328213054,22.7705314330652,-26.3875289299324));
#29312=CARTESIAN_POINT('Ctrl Pts',(-26.6890183623401,22.8177082581051,-26.3905667834484));
#29313=CARTESIAN_POINT('Ctrl Pts',(-26.7485255020659,23.091222376041,-26.4082874827796));
#29314=CARTESIAN_POINT('Ctrl Pts',(-26.7732131713021,23.321914293925,-26.4237303520041));
#29315=CARTESIAN_POINT('Ctrl Pts',(-26.7730011780047,23.5532063773351,-26.4393798414846));
#29316=CARTESIAN_POINT('Ctrl Pts',(-26.7730011776085,23.5532068095779,-26.4393798707307));
#29317=CARTESIAN_POINT('Ctrl Pts',(-26.7728187939646,23.7521646139568,-26.4528415856483));
#29318=CARTESIAN_POINT('Ctrl Pts',(-26.7542127905816,23.9507015891791,-26.4663742124312));
#29319=CARTESIAN_POINT('Ctrl Pts',(-26.7116066042551,24.1771034647024,-26.4811392033754));
#29320=CARTESIAN_POINT('Ctrl Pts',(-26.7053548002584,24.2078477869537,-26.4831290045788));
#29321=CARTESIAN_POINT('Ctrl Pts',(-26.6978017852289,24.2423993461137,-26.4853442721287));
#29322=CARTESIAN_POINT('Ctrl Pts',(-26.6969415319832,24.2462998375609,-26.4855940493224));
#29323=CARTESIAN_POINT('Ctrl Pts',(-26.6955333286218,24.2526288330179,-26.4859988394831));
#29324=CARTESIAN_POINT('Ctrl Pts',(-26.6949898153863,24.2550583041157,-26.4861541035073));
#29325=CARTESIAN_POINT('Ctrl Pts',(-26.6939341498047,24.2597515333118,-26.4864538054994));
#29326=CARTESIAN_POINT('Ctrl Pts',(-26.6934223662965,24.2620153715993,-26.4865982645441));
#29327=CARTESIAN_POINT('Ctrl Pts',(-26.6924945752026,24.2660988746399,-26.4868586454711));
#29328=CARTESIAN_POINT('Ctrl Pts',(-26.692079433339,24.2679187262862,-26.4869746170569));
#29329=CARTESIAN_POINT('Ctrl Pts',(-26.6911826369063,24.2718343085429,-26.4872239906468));
#29330=CARTESIAN_POINT('Ctrl Pts',(-26.6907004671745,24.2739299122374,-26.4873573620492));
#29331=CARTESIAN_POINT('Ctrl Pts',(-26.6893940226746,24.279582080404,-26.4877168401273));
#29332=CARTESIAN_POINT('Ctrl Pts',(-26.6885657981603,24.2831377429326,-26.4879427182525));
#29333=CARTESIAN_POINT('Ctrl Pts',(-26.6847072690303,24.2995763701924,-26.4889858231773));
#29334=CARTESIAN_POINT('Ctrl Pts',(-26.6816036104003,24.3124422400324,-26.4897988653303));
#29335=CARTESIAN_POINT('Ctrl Pts',(-26.6259159983002,24.5372061696567,-26.5039495852026));
#29336=CARTESIAN_POINT('Ctrl Pts',(-26.5520031509013,24.7432775469653,-26.5161201670329));
#29337=CARTESIAN_POINT('Ctrl Pts',(-26.4375640099535,24.9826461329155,-26.530945810762));
#29338=CARTESIAN_POINT('Ctrl Pts',(-26.4164043658069,25.0245295185153,-26.5335660783988));
#29339=CARTESIAN_POINT('Ctrl Pts',(-26.3723481959893,25.1071981816068,-26.5388134831348));
#29340=CARTESIAN_POINT('Ctrl Pts',(-26.3494634076132,25.1479765534623,-26.5414399236056));
#29341=CARTESIAN_POINT('Ctrl Pts',(-26.2569383071893,25.3047532254069,-26.5517267163221));
#29342=CARTESIAN_POINT('Ctrl Pts',(-26.1809153902179,25.4168075921755,-26.5594982311706));
#29343=CARTESIAN_POINT('Ctrl Pts',(-26.0639810361362,25.5677727300214,-26.570840231124));
#29344=CARTESIAN_POINT('Ctrl Pts',(-26.0287459242314,25.6109050170868,-26.5741893002898));
#29345=CARTESIAN_POINT('Ctrl Pts',(-25.9886642750751,25.6574541673798,-26.577934422271));
#29346=CARTESIAN_POINT('Ctrl Pts',(-25.9849042592158,25.6617973521273,-26.5782851409547));
#29347=CARTESIAN_POINT('Ctrl Pts',(-25.9777882968403,25.669972706456,-26.5789477591288));
#29348=CARTESIAN_POINT('Ctrl Pts',(-25.9744348340489,25.6738070223618,-26.5792595548606));
#29349=CARTESIAN_POINT('Ctrl Pts',(-25.9687599733586,25.6802646414454,-26.5797864056087));
#29350=CARTESIAN_POINT('Ctrl Pts',(-25.9664433555826,25.6828921485719,-26.5800012604653));
#29351=CARTESIAN_POINT('Ctrl Pts',(-25.961852048035,25.6880825244253,-26.5804266527004));
#29352=CARTESIAN_POINT('Ctrl Pts',(-25.9595775450603,25.6906455528128,-26.5806371820813));
#29353=CARTESIAN_POINT('Ctrl Pts',(-25.954557091364,25.6962847191884,-26.5811014256582));
#29354=CARTESIAN_POINT('Ctrl Pts',(-25.9518093188138,25.6993592213221,-26.5813552164458));
#29355=CARTESIAN_POINT('Ctrl Pts',(-25.942200720708,25.7100689106365,-26.5822416627262));
#29356=CARTESIAN_POINT('Ctrl Pts',(-25.9353093782173,25.7176765245055,-26.5828756080392));
#29357=CARTESIAN_POINT('Ctrl Pts',(-25.8647669544663,25.7948071564964,-26.589346795019));
#29358=CARTESIAN_POINT('Ctrl Pts',(-25.79813719248,25.8615322686978,-26.5953118672348));
#29359=CARTESIAN_POINT('Ctrl Pts',(-25.603024202773,26.0404978431804,-26.6124106714986));
#29360=CARTESIAN_POINT('Ctrl Pts',(-25.4684291804516,26.1455903907483,-26.6238087826733));
#29361=CARTESIAN_POINT('Ctrl Pts',(-25.2306108965602,26.3026382741286,-26.6430725027435));
#29362=CARTESIAN_POINT('Ctrl Pts',(-25.1317542002661,26.3606056611473,-26.6508504791865));
#29363=CARTESIAN_POINT('Ctrl Pts',(-24.9445148763404,26.4573842054219,-26.664973187452));
#29364=CARTESIAN_POINT('Ctrl Pts',(-24.8570639945482,26.4977309699153,-26.6713408444356));
#29365=CARTESIAN_POINT('Ctrl Pts',(-24.7354057767133,26.5473783905949,-26.6797764110105));
#29366=CARTESIAN_POINT('Ctrl Pts',(-24.7026640372419,26.5601195723894,-26.6820060338804));
#29367=CARTESIAN_POINT('Ctrl Pts',(-24.6664360610661,26.5735395089644,-26.6844235475585));
#29368=CARTESIAN_POINT('Ctrl Pts',(-24.6631512467908,26.5747502203004,-26.6846423006544));
#29369=CARTESIAN_POINT('Ctrl Pts',(-24.6577215003067,26.576741463756,-26.6850031545402));
#29370=CARTESIAN_POINT('Ctrl Pts',(-24.6555777105048,26.5775250700522,-26.6851454373212));
#29371=CARTESIAN_POINT('Ctrl Pts',(-24.6513917103602,26.5790501135761,-26.6854228864567));
#29372=CARTESIAN_POINT('Ctrl Pts',(-24.6493495798175,26.5797917642642,-26.6855580655519));
#29373=CARTESIAN_POINT('Ctrl Pts',(-24.6457299551105,26.5811021797688,-26.6857973571994));
#29374=CARTESIAN_POINT('Ctrl Pts',(-24.6441527757854,26.5816717752915,-26.6859015194632));
#29375=CARTESIAN_POINT('Ctrl Pts',(-24.6407727611106,26.5828894802824,-26.6861245239524));
#29376=CARTESIAN_POINT('Ctrl Pts',(-24.638969797323,26.5835372114232,-26.6862433430584));
#29377=CARTESIAN_POINT('Ctrl Pts',(-24.633732624901,26.5854134422677,-26.6865880927255));
#29378=CARTESIAN_POINT('Ctrl Pts',(-24.6302968927519,26.5866377252935,-26.6868137702857));
#29379=CARTESIAN_POINT('Ctrl Pts',(-24.6147953716523,26.5921318716312,-26.6878298272367));
#29380=CARTESIAN_POINT('Ctrl Pts',(-24.6027060719757,26.596335743839,-26.6886163132033));
#29381=CARTESIAN_POINT('Ctrl Pts',(-24.3949020994769,26.6672116108374,-26.7020392121718));
#29382=CARTESIAN_POINT('Ctrl Pts',(-24.1932089191864,26.7149803551183,-26.713625383618));
#29383=CARTESIAN_POINT('Ctrl Pts',(-23.820618542259,26.7660986835303,-26.7346507693911));
#29384=CARTESIAN_POINT('Ctrl Pts',(-23.65138925435,26.7758581450546,-26.7440662802989));
#29385=CARTESIAN_POINT('Ctrl Pts',(-23.3723933857431,26.7699642270149,-26.760150770649));
#29386=CARTESIAN_POINT('Ctrl Pts',(-23.2628019955691,26.7620348366198,-26.7666084160437));
#29387=CARTESIAN_POINT('Ctrl Pts',(-23.1327263931029,26.7459123981048,-26.7745324639313));
#29388=CARTESIAN_POINT('Ctrl Pts',(-23.1116428156245,26.7430869372719,-26.775824918877));
#29389=CARTESIAN_POINT('Ctrl Pts',(-23.0861361291948,26.7394113186635,-26.7773987524319));
#29390=CARTESIAN_POINT('Ctrl Pts',(-23.081684485776,26.7387603001642,-26.7776738094763));
#29391=CARTESIAN_POINT('Ctrl Pts',(-23.0730819547546,26.7374838417917,-26.7782060779828));
#29392=CARTESIAN_POINT('Ctrl Pts',(-23.0689308950522,26.7368596090413,-26.7784632507013));
#29393=CARTESIAN_POINT('Ctrl Pts',(-23.061779539548,26.7357699020578,-26.7789068791562));
#29394=CARTESIAN_POINT('Ctrl Pts',(-23.0587786528486,26.7353082937263,-26.7790932118733));
#29395=CARTESIAN_POINT('Ctrl Pts',(-23.0525865793213,26.7343468449782,-26.7794780569912));
#29396=CARTESIAN_POINT('Ctrl Pts',(-23.0493954835156,26.7338464463134,-26.7796765869559));
#29397=CARTESIAN_POINT('Ctrl Pts',(-23.0416930972526,26.7326267606781,-26.7801562650638));
#29398=CARTESIAN_POINT('Ctrl Pts',(-23.0371825823272,26.7319026787693,-26.7804375654599));
#29399=CARTESIAN_POINT('Ctrl Pts',(-23.0205596711014,26.7291979023252,-26.7814757506057));
#29400=CARTESIAN_POINT('Ctrl Pts',(-23.0084571978714,26.7271576303038,-26.7822345291494));
#29401=CARTESIAN_POINT('Ctrl Pts',(-22.8131164048176,26.6930778076623,-26.7945296334222));
#29402=CARTESIAN_POINT('Ctrl Pts',(-22.6330120593938,26.6453079987484,-26.8065804500814));
#29403=CARTESIAN_POINT('Ctrl Pts',(-22.4105157107109,26.5651606632149,-26.8223531931913));
#29404=CARTESIAN_POINT('Ctrl Pts',(-22.3633844825301,26.5469198563805,-26.8257450715511));
#29405=CARTESIAN_POINT('Ctrl Pts',(-22.2346156750902,26.4935690587107,-26.8351384017386));
#29406=CARTESIAN_POINT('Ctrl Pts',(-22.153992098097,26.4561880039129,-26.8411635288059));
#29407=CARTESIAN_POINT('Ctrl Pts',(-22.0750359193537,26.4155367251338,-26.8471666088699));
#29408=CARTESIAN_POINT('',(-26.7730021969517,23.548783660454,-26.6857734492732));
#29409=CARTESIAN_POINT('Ctrl Pts',(-22.075036065511,26.4155368003841,-27.0910469152906));
#29410=CARTESIAN_POINT('Ctrl Pts',(-22.1117303554584,26.4344291739391,-27.0882869220563));
#29411=CARTESIAN_POINT('Ctrl Pts',(-22.148792243511,26.4526190695116,-27.085542761816));
#29412=CARTESIAN_POINT('Ctrl Pts',(-22.2594218474688,26.5043014372093,-27.0774983103592));
#29413=CARTESIAN_POINT('Ctrl Pts',(-22.3339104340851,26.5357446747267,-27.0722699745989));
#29414=CARTESIAN_POINT('Ctrl Pts',(-22.4153638470589,26.5665722126063,-27.0668111573741));
#29415=CARTESIAN_POINT('Ctrl Pts',(-22.4212246077583,26.5687708259081,-27.0664198027816));
#29416=CARTESIAN_POINT('Ctrl Pts',(-22.4293900709342,26.5718069195685,-27.0658765620758));
#29417=CARTESIAN_POINT('Ctrl Pts',(-22.4316893305083,26.5726588478394,-27.0657238159769));
#29418=CARTESIAN_POINT('Ctrl Pts',(-22.4356529918019,26.5741223325226,-27.065460883452));
#29419=CARTESIAN_POINT('Ctrl Pts',(-22.4373169255687,26.5747351392394,-27.0653506217124));
#29420=CARTESIAN_POINT('Ctrl Pts',(-22.4407290852288,26.5759885993234,-27.0651247527524));
#29421=CARTESIAN_POINT('Ctrl Pts',(-22.4424773575766,26.5766291098535,-27.0650091546586));
#29422=CARTESIAN_POINT('Ctrl Pts',(-22.4465774975758,26.5781272398572,-27.0647383491723));
#29423=CARTESIAN_POINT('Ctrl Pts',(-22.4489298174668,26.5789836370416,-27.0645832155842));
#29424=CARTESIAN_POINT('Ctrl Pts',(-22.453903179367,26.5807877035772,-27.0642557119632));
#29425=CARTESIAN_POINT('Ctrl Pts',(-22.4565244598306,26.5817347162575,-27.0640833812348));
#29426=CARTESIAN_POINT('Ctrl Pts',(-22.4635801570312,26.5842734462758,-27.0636202759859));
#29427=CARTESIAN_POINT('Ctrl Pts',(-22.4680168622465,26.5858588494513,-27.0633298737699));
#29428=CARTESIAN_POINT('Ctrl Pts',(-22.481662201955,26.5907011293495,-27.0624391472207));
#29429=CARTESIAN_POINT('Ctrl Pts',(-22.4908822818475,26.5939259121944,-27.0618406728729));
#29430=CARTESIAN_POINT('Ctrl Pts',(-22.5249495504638,26.6056676045646,-27.0596413416516));
#29431=CARTESIAN_POINT('Ctrl Pts',(-22.5498866831905,26.6139228368537,-27.0580548651704));
#29432=CARTESIAN_POINT('Ctrl Pts',(-22.6375646623112,26.6417631738311,-27.0525494658113));
#29433=CARTESIAN_POINT('Ctrl Pts',(-22.7008045695414,26.6597342420235,-27.0487076966726));
#29434=CARTESIAN_POINT('Ctrl Pts',(-23.1479267347048,26.7721330564597,-27.022162150229));
#29435=CARTESIAN_POINT('Ctrl Pts',(-23.545741737267,26.7971594833623,-27.0012211057315));
#29436=CARTESIAN_POINT('Ctrl Pts',(-23.9568305774995,26.7473079199282,-26.9761541515665));
#29437=CARTESIAN_POINT('Ctrl Pts',(-23.9754169173656,26.7448893005317,-26.975014559856));
#29438=CARTESIAN_POINT('Ctrl Pts',(-23.9999718579269,26.7414759141054,-26.9735004027993));
#29439=CARTESIAN_POINT('Ctrl Pts',(-24.0059605246826,26.7406262360074,-26.9731304388732));
#29440=CARTESIAN_POINT('Ctrl Pts',(-24.0152529528623,26.7392811190478,-26.9725553120215));
#29441=CARTESIAN_POINT('Ctrl Pts',(-24.0185584178081,26.7387973909586,-26.9723505208016));
#29442=CARTESIAN_POINT('Ctrl Pts',(-24.0251741908387,26.7378187166248,-26.9719402165293));
#29443=CARTESIAN_POINT('Ctrl Pts',(-24.0284844919059,26.7373237511269,-26.9717347030976));
#29444=CARTESIAN_POINT('Ctrl Pts',(-24.0358721948227,26.7362073519493,-26.9712755773411));
#29445=CARTESIAN_POINT('Ctrl Pts',(-24.0399491815204,26.7355832468351,-26.97102188047));
#29446=CARTESIAN_POINT('Ctrl Pts',(-24.0518660012482,26.7337356005694,-26.9702793863383));
#29447=CARTESIAN_POINT('Ctrl Pts',(-24.0597024852284,26.7324909366055,-26.9697899184823));
#29448=CARTESIAN_POINT('Ctrl Pts',(-24.116989443313,26.7231750538389,-26.9662028460948));
#29449=CARTESIAN_POINT('Ctrl Pts',(-24.1662479564414,26.7139809078823,-26.9630696557072));
#29450=CARTESIAN_POINT('Ctrl Pts',(-24.3260858397578,26.680272746659,-26.9527351699353));
#29451=CARTESIAN_POINT('Ctrl Pts',(-24.4355809342886,26.6510802658873,-26.945388088509));
#29452=CARTESIAN_POINT('Ctrl Pts',(-24.6742678469254,26.5737700654847,-26.9287949825337));
#29453=CARTESIAN_POINT('Ctrl Pts',(-24.8023721830723,26.5230055533087,-26.9194953408774));
#29454=CARTESIAN_POINT('Ctrl Pts',(-24.9889587135771,26.434860562369,-26.9055264108721));
#29455=CARTESIAN_POINT('Ctrl Pts',(-25.0501337969723,26.4035305480273,-26.9008757124831));
#29456=CARTESIAN_POINT('Ctrl Pts',(-25.207388667933,26.3165384928552,-26.8887966559881));
#29457=CARTESIAN_POINT('Ctrl Pts',(-25.301685132614,26.2578209571642,-26.8814262590562));
#29458=CARTESIAN_POINT('Ctrl Pts',(-25.420215464717,26.1752239871941,-26.8721611929508));
#29459=CARTESIAN_POINT('Ctrl Pts',(-25.4473619559212,26.1556723758847,-26.8700394180871));
#29460=CARTESIAN_POINT('Ctrl Pts',(-25.4782575644331,26.1326815688672,-26.8676294277858));
#29461=CARTESIAN_POINT('Ctrl Pts',(-25.4823076611297,26.1296528720743,-26.8673135998061));
#29462=CARTESIAN_POINT('Ctrl Pts',(-25.4882690212393,26.1251729978878,-26.8668488949387));
#29463=CARTESIAN_POINT('Ctrl Pts',(-25.4901857947329,26.1237292182056,-26.8666995021319));
#29464=CARTESIAN_POINT('Ctrl Pts',(-25.4935544277947,26.1211859458161,-26.8664369986447));
#29465=CARTESIAN_POINT('Ctrl Pts',(-25.4950069681579,26.1200873631877,-26.8663238236793));
#29466=CARTESIAN_POINT('Ctrl Pts',(-25.4978515093721,26.1179321921358,-26.8661022217772));
#29467=CARTESIAN_POINT('Ctrl Pts',(-25.4992435774488,26.1168757062371,-26.8659937881466));
#29468=CARTESIAN_POINT('Ctrl Pts',(-25.5030079675217,26.114013959205,-26.8657006020191));
#29469=CARTESIAN_POINT('Ctrl Pts',(-25.5053786526177,26.112206532218,-26.8655160031056));
#29470=CARTESIAN_POINT('Ctrl Pts',(-25.5144524502014,26.1052686755528,-26.864809588611));
#29471=CARTESIAN_POINT('Ctrl Pts',(-25.5211379817682,26.1001151479354,-26.8642893945366));
#29472=CARTESIAN_POINT('Ctrl Pts',(-25.5377733974908,26.0871872582246,-26.8629955173038));
#29473=CARTESIAN_POINT('Ctrl Pts',(-25.5476980835186,26.0793804996065,-26.8622240460002));
#29474=CARTESIAN_POINT('Ctrl Pts',(-25.5867509088847,26.0482882705484,-26.859189032477));
#29475=CARTESIAN_POINT('Ctrl Pts',(-25.6155210571724,26.0245553377063,-26.8569546066483));
#29476=CARTESIAN_POINT('Ctrl Pts',(-25.6894226469634,25.961405442039,-26.8511995436364));
#29477=CARTESIAN_POINT('Ctrl Pts',(-25.7338795117567,25.9212188201317,-26.8477218094315));
#29478=CARTESIAN_POINT('Ctrl Pts',(-26.0545500009983,25.6146744723364,-26.8222951215269));
#29479=CARTESIAN_POINT('Ctrl Pts',(-26.2823220011113,25.302157492601,-26.8018640436458));
#29480=CARTESIAN_POINT('Ctrl Pts',(-26.4584747066371,24.9390487663431,-26.7774497082871));
#29481=CARTESIAN_POINT('Ctrl Pts',(-26.466969304452,24.9211188418543,-26.7762438771411));
#29482=CARTESIAN_POINT('Ctrl Pts',(-26.4778949051428,24.8974963759323,-26.7746544548105));
#29483=CARTESIAN_POINT('Ctrl Pts',(-26.4804759586782,24.8918733834103,-26.7742760601043));
#29484=CARTESIAN_POINT('Ctrl Pts',(-26.4844372364744,24.8831775213704,-26.7736907813634));
#29485=CARTESIAN_POINT('Ctrl Pts',(-26.4858288717208,24.880109840434,-26.7734842910414));
#29486=CARTESIAN_POINT('Ctrl Pts',(-26.4885924524867,24.873992406304,-26.7730724773471));
#29487=CARTESIAN_POINT('Ctrl Pts',(-26.4899644658967,24.8709426882141,-26.7728671566262));
#29488=CARTESIAN_POINT('Ctrl Pts',(-26.4929981009611,24.8641713604134,-26.7724112341954));
#29489=CARTESIAN_POINT('Ctrl Pts',(-26.4946574124827,24.860448727555,-26.7721605534873));
#29490=CARTESIAN_POINT('Ctrl Pts',(-26.4994326782185,24.8496806265695,-26.77143533832));
#29491=CARTESIAN_POINT('Ctrl Pts',(-26.502530421322,24.8426271566261,-26.7709601801534));
#29492=CARTESIAN_POINT('Ctrl Pts',(-26.5234532658806,24.7945186638534,-26.7677184542764));
#29493=CARTESIAN_POINT('Ctrl Pts',(-26.5404459694104,24.7531090038476,-26.7649236151799));
#29494=CARTESIAN_POINT('Ctrl Pts',(-26.5727237170193,24.6695361042963,-26.7592705182487));
#29495=CARTESIAN_POINT('Ctrl Pts',(-26.588002015373,24.6273809067697,-26.7564127809705));
#29496=CARTESIAN_POINT('Ctrl Pts',(-26.7155422445852,24.2511536329094,-26.7308484582895));
#29497=CARTESIAN_POINT('Ctrl Pts',(-26.7731442464588,23.9012054539653,-26.7062883839866));
#29498=CARTESIAN_POINT('Ctrl Pts',(-26.7730022699222,23.5489535893969,-26.6831828372533));
#29499=CARTESIAN_POINT('Ctrl Pts',(-26.7730021969517,23.548783660454,-26.6857734492732));
#29500=CARTESIAN_POINT('Ctrl Pts',(-26.772964759865,23.4666455156343,-26.6806758114827));
#29501=CARTESIAN_POINT('Ctrl Pts',(-26.7697874348417,23.3845817953304,-26.6755781736922));
#29502=CARTESIAN_POINT('Ctrl Pts',(-26.7634854691912,23.3027618209907,-26.6704805359017));
#29503=CARTESIAN_POINT('Ctrl Pts',(-26.7558552080702,23.2036962589499,-26.6643084445893));
#29504=CARTESIAN_POINT('Ctrl Pts',(-26.7436258552823,23.1048094192993,-26.658136353277));
#29505=CARTESIAN_POINT('Ctrl Pts',(-26.7268102442853,23.0065626742592,-26.6519642619647));
#29506=CARTESIAN_POINT('Ctrl Pts',(-26.7100174167789,22.9084490438458,-26.6458005332259));
#29507=CARTESIAN_POINT('Ctrl Pts',(-26.6886507545427,22.8109742086628,-26.6396368044871));
#29508=CARTESIAN_POINT('Ctrl Pts',(-26.6627749830657,22.7145961715745,-26.6334730757483));
#29509=CARTESIAN_POINT('Ctrl Pts',(-26.6369266245401,22.6183202379713,-26.6273158769017));
#29510=CARTESIAN_POINT('Ctrl Pts',(-26.6065787658576,22.5231392096193,-26.621158678055));
#29511=CARTESIAN_POINT('Ctrl Pts',(-26.5718473181805,22.4295016634016,-26.6150014792083));
#29512=CARTESIAN_POINT('Ctrl Pts',(-26.5371412570854,22.3359325605517,-26.6088487809006));
#29513=CARTESIAN_POINT('Ctrl Pts',(-26.4980581279732,22.2439051028591,-26.6026960825929));
#29514=CARTESIAN_POINT('Ctrl Pts',(-26.4547636208086,22.1538525547136,-26.5965433842852));
#29515=CARTESIAN_POINT('Ctrl Pts',(-26.4114855309827,22.0638341546225,-26.5903930190894));
#29516=CARTESIAN_POINT('Ctrl Pts',(-26.3639994242631,21.9757895671151,-26.5842426538937));
#29517=CARTESIAN_POINT('Ctrl Pts',(-26.3125186966516,21.890131091428,-26.5780922886979));
#29518=CARTESIAN_POINT('Ctrl Pts',(-26.2610437179955,21.8044821813936,-26.5719426103257));
#29519=CARTESIAN_POINT('Ctrl Pts',(-26.2055752291014,21.7212192257498,-26.5657929319535));
#29520=CARTESIAN_POINT('Ctrl Pts',(-26.1463715498038,21.6407280866269,-26.5596432535813));
#29521=CARTESIAN_POINT('Ctrl Pts',(-26.0871586432963,21.5602244025297,-26.5534926167488));
#29522=CARTESIAN_POINT('Ctrl Pts',(-26.0242096475015,21.4824937429909,-26.5473419799164));
#29523=CARTESIAN_POINT('Ctrl Pts',(-25.9578243828091,21.4078904371315,-26.5411913430839));
#29524=CARTESIAN_POINT('Ctrl Pts',(-25.8913680998289,21.3332073214065,-26.5350341263621));
#29525=CARTESIAN_POINT('Ctrl Pts',(-25.8214684965082,21.2616585653733,-26.5288769096403));
#29526=CARTESIAN_POINT('Ctrl Pts',(-25.74846354577,21.1935629254678,-26.5227196929184));
#29527=CARTESIAN_POINT('Ctrl Pts',(-25.6754178658689,21.1254292952837,-26.5165590411106));
#29528=CARTESIAN_POINT('Ctrl Pts',(-25.5992637194991,21.060752898994,-26.5103983893028));
#29529=CARTESIAN_POINT('Ctrl Pts',(-25.5203719548123,20.9998119773678,-26.504237737495));
#29530=CARTESIAN_POINT('Ctrl Pts',(-25.4413481761488,20.9387690799088,-26.498066776726));
#29531=CARTESIAN_POINT('Ctrl Pts',(-25.3595779846455,20.8814743922859,-26.491895815957));
#29532=CARTESIAN_POINT('Ctrl Pts',(-25.2754610805144,20.8281627048189,-26.4857248551879));
#29533=CARTESIAN_POINT('Ctrl Pts',(-25.2112530682199,20.7874688928001,-26.4810144449675));
#29534=CARTESIAN_POINT('Ctrl Pts',(-25.1456783284721,20.7490948998627,-26.4763040347471));
#29535=CARTESIAN_POINT('Ctrl Pts',(-25.0789230656487,20.7131265279504,-26.4715936245267));
#29536=CARTESIAN_POINT('Ctrl Pts',(-24.9914530665518,20.6659968586837,-26.4654215332144));
#29537=CARTESIAN_POINT('Ctrl Pts',(-24.901647425585,20.6228330894294,-26.4592494419021));
#29538=CARTESIAN_POINT('Ctrl Pts',(-24.8099012399664,20.5838738144283,-26.4530773505898));
#29539=CARTESIAN_POINT('Ctrl Pts',(-24.7182793613591,20.5449673253932,-26.446913621851));
#29540=CARTESIAN_POINT('Ctrl Pts',(-24.6247225603269,20.5102541761597,-26.4407498931122));
#29541=CARTESIAN_POINT('Ctrl Pts',(-24.5296511492348,20.4799274820521,-26.4345861643734));
#29542=CARTESIAN_POINT('Ctrl Pts',(-24.43468045738,20.4496329162307,-26.4284289655267));
#29543=CARTESIAN_POINT('Ctrl Pts',(-24.3381987571015,20.4237156980897,-26.42227176668));
#29544=CARTESIAN_POINT('Ctrl Pts',(-24.2406460985544,20.4023207844452,-26.4161145678333));
#29545=CARTESIAN_POINT('Ctrl Pts',(-24.143164745085,20.3809415091852,-26.4099618695256));
#29546=CARTESIAN_POINT('Ctrl Pts',(-24.0446144127321,20.36407805925,-26.4038091712179));
#29547=CARTESIAN_POINT('Ctrl Pts',(-23.9454491765465,20.3518252346625,-26.3976564729102));
#29548=CARTESIAN_POINT('Ctrl Pts',(-23.8463215439594,20.3395770563635,-26.3915061077145));
#29549=CARTESIAN_POINT('Ctrl Pts',(-23.7465799014946,20.3319360826576,-26.3853557425187));
#29550=CARTESIAN_POINT('Ctrl Pts',(-23.646686473003,20.3289456451241,-26.3792053773229));
#29551=CARTESIAN_POINT('Ctrl Pts',(-23.5468041998097,20.3259555415388,-26.3730556989507));
#29552=CARTESIAN_POINT('Ctrl Pts',(-23.4467706084967,20.3276149546168,-26.3669060205785));
#29553=CARTESIAN_POINT('Ctrl Pts',(-23.34704996417,20.3339151303864,-26.3607563422063));
#29554=CARTESIAN_POINT('Ctrl Pts',(-23.2473137778478,20.340216288072,-26.3546057053739));
#29555=CARTESIAN_POINT('Ctrl Pts',(-23.1478910689693,20.3511596176907,-26.3484550685414));
#29556=CARTESIAN_POINT('Ctrl Pts',(-23.0492420061998,20.3666844052292,-26.342304431709));
#29557=CARTESIAN_POINT('Ctrl Pts',(-22.9504874096561,20.3822258010291,-26.3361472149872));
#29558=CARTESIAN_POINT('Ctrl Pts',(-22.8525085418933,20.4023583742926,-26.3299899982653));
#29559=CARTESIAN_POINT('Ctrl Pts',(-22.7557562667419,20.4269700840957,-26.3238327815435));
#29560=CARTESIAN_POINT('Ctrl Pts',(-22.6589500138924,20.4515955246709,-26.3176721297357));
#29561=CARTESIAN_POINT('Ctrl Pts',(-22.563372132021,20.4807049517233,-26.3115114779279));
#29562=CARTESIAN_POINT('Ctrl Pts',(-22.4694571689025,20.5141367654119,-26.3053508261201));
#29563=CARTESIAN_POINT('Ctrl Pts',(-22.3753850526541,20.5476245224133,-26.2991798653511));
#29564=CARTESIAN_POINT('Ctrl Pts',(-22.2829818156605,20.5854489489311,-26.293008904582));
#29565=CARTESIAN_POINT('Ctrl Pts',(-22.1926610458664,20.6274006845922,-26.286837943813));
#29566=CARTESIAN_POINT('Ctrl Pts',(-22.1237175064283,20.659423232104,-26.2821275335926));
#29567=CARTESIAN_POINT('Ctrl Pts',(-22.0559868955778,20.6938495909111,-26.2774171233723));
#29568=CARTESIAN_POINT('Ctrl Pts',(-21.9896420512896,20.7305694837345,-26.2727067131519));
#29569=CARTESIAN_POINT('Ctrl Pts',(-21.9027098271538,20.7786838773609,-26.2665346218396));
#29570=CARTESIAN_POINT('Ctrl Pts',(-21.8178516677939,20.8309070227635,-26.2603625305272));
#29571=CARTESIAN_POINT('Ctrl Pts',(-21.7354818733435,20.8870354883256,-26.2541904392149));
#29572=CARTESIAN_POINT('Ctrl Pts',(-21.6532236818211,20.9430879053658,-26.2480267104761));
#29573=CARTESIAN_POINT('Ctrl Pts',(-21.573447509833,21.0030348830378,-26.2418629817373));
#29574=CARTESIAN_POINT('Ctrl Pts',(-21.4965430251931,21.0666271925162,-26.2356992529985));
#29575=CARTESIAN_POINT('Ctrl Pts',(-21.4197200136369,21.1301521319111,-26.2295420541518));
#29576=CARTESIAN_POINT('Ctrl Pts',(-21.3457629740193,21.1973144500351,-26.2233848553052));
#29577=CARTESIAN_POINT('Ctrl Pts',(-21.2750317267056,21.2678222806137,-26.2172276564585));
#29578=CARTESIAN_POINT('Ctrl Pts',(-21.2043521796445,21.3382785742439,-26.2110749581508));
#29579=CARTESIAN_POINT('Ctrl Pts',(-21.1368940437931,21.4120752127719,-26.2049222598431));
#29580=CARTESIAN_POINT('Ctrl Pts',(-21.0729825228156,21.48888141867,-26.1987695615354));
#29581=CARTESIAN_POINT('Ctrl Pts',(-21.0090952371777,21.5656584995456,-26.1926191963396));
#29582=CARTESIAN_POINT('Ctrl Pts',(-20.9487521716963,21.6454425466293,-26.1864688311439));
#29583=CARTESIAN_POINT('Ctrl Pts',(-20.8922396335423,21.7278681057955,-26.1803184659481));
#29584=CARTESIAN_POINT('Ctrl Pts',(-20.8357334062562,21.8102844603352,-26.1741687875759));
#29585=CARTESIAN_POINT('Ctrl Pts',(-20.783057101491,21.8953413822114,-26.1680191092037));
#29586=CARTESIAN_POINT('Ctrl Pts',(-20.734454309355,21.982643545508,-26.1618694308314));
#29587=CARTESIAN_POINT('Ctrl Pts',(-20.6858439422141,22.0699593153134,-26.155718793999));
#29588=CARTESIAN_POINT('Ctrl Pts',(-20.6413085600557,22.1595206420112,-26.1495681571665));
#29589=CARTESIAN_POINT('Ctrl Pts',(-20.601045823833,22.2509075594846,-26.1434175203341));
#29590=CARTESIAN_POINT('Ctrl Pts',(-20.5607400149404,22.3423922417623,-26.1372603036123));
#29591=CARTESIAN_POINT('Ctrl Pts',(-20.5247161549714,22.4357060164541,-26.1311030868904));
#29592=CARTESIAN_POINT('Ctrl Pts',(-20.4931236930307,22.5304090013857,-26.1249458701686));
#29593=CARTESIAN_POINT('Ctrl Pts',(-20.4615136057849,22.6251648207246,-26.1187852183608));
#29594=CARTESIAN_POINT('Ctrl Pts',(-20.4343399581838,22.7213109757304,-26.112624566553));
#29595=CARTESIAN_POINT('Ctrl Pts',(-20.4117016850638,22.8183945225043,-26.1064639147452));
#29596=CARTESIAN_POINT('Ctrl Pts',(-20.3890255300626,22.9156405245753,-26.1002929539761));
#29597=CARTESIAN_POINT('Ctrl Pts',(-20.3708999878733,23.0138266242466,-26.0941219932071));
#29598=CARTESIAN_POINT('Ctrl Pts',(-20.3573724819186,23.1124916948837,-26.0879510324381));
#29599=CARTESIAN_POINT('Ctrl Pts',(-20.3470466826322,23.1878045958268,-26.0832406222177));
#29600=CARTESIAN_POINT('Ctrl Pts',(-20.3393988894415,23.2633964015082,-26.0785302119973));
#29601=CARTESIAN_POINT('Ctrl Pts',(-20.3344297504739,23.3390620908957,-26.073819801777));
#29602=CARTESIAN_POINT('Ctrl Pts',(-20.327918644643,23.4382074991004,-26.0676477104646));
#29603=CARTESIAN_POINT('Ctrl Pts',(-20.3259854205563,23.5378289163274,-26.0614756191523));
#29604=CARTESIAN_POINT('Ctrl Pts',(-20.3286828745671,23.6374678215102,-26.05530352784));
#29605=CARTESIAN_POINT('Ctrl Pts',(-20.3313766737943,23.736971725827,-26.0491397991012));
#29606=CARTESIAN_POINT('Ctrl Pts',(-20.3386886690033,23.8364926405893,-26.0429760703624));
#29607=CARTESIAN_POINT('Ctrl Pts',(-20.3506198117746,23.9355680129816,-26.0368123416236));
#29608=CARTESIAN_POINT('Ctrl Pts',(-20.3625383146199,24.0345384243155,-26.0306551427769));
#29609=CARTESIAN_POINT('Ctrl Pts',(-20.3790661845488,24.1330638027741,-26.0244979439303));
#29610=CARTESIAN_POINT('Ctrl Pts',(-20.4001523677289,24.2306836593522,-26.0183407450836));
#29611=CARTESIAN_POINT('Ctrl Pts',(-20.4212231381879,24.328232161735,-26.0121880467759));
#29612=CARTESIAN_POINT('Ctrl Pts',(-20.4468455061786,24.424876034842,-26.0060353484682));
#29613=CARTESIAN_POINT('Ctrl Pts',(-20.4769169693841,24.5201628800977,-25.9998826501605));
#29614=CARTESIAN_POINT('Ctrl Pts',(-20.506977029448,24.6154135924462,-25.9937322849647));
#29615=CARTESIAN_POINT('Ctrl Pts',(-20.5414827018791,24.7093078856211,-25.987581919769));
#29616=CARTESIAN_POINT('Ctrl Pts',(-20.5802812851532,24.801407341148,-25.9814315545732));
#29617=CARTESIAN_POINT('Ctrl Pts',(-20.6190755357121,24.8934965117452,-25.975281876201));
#29618=CARTESIAN_POINT('Ctrl Pts',(-20.66216157536,24.9837908428531,-25.9691321978288));
#29619=CARTESIAN_POINT('Ctrl Pts',(-20.7093384805505,25.0718717076099,-25.9629825194566));
#29620=CARTESIAN_POINT('Ctrl Pts',(-20.7565227385139,25.1599663002403,-25.9568318826241));
#29621=CARTESIAN_POINT('Ctrl Pts',(-20.8077989233013,25.2458463583302,-25.9506812457917));
#29622=CARTESIAN_POINT('Ctrl Pts',(-20.8629205544969,25.3291185769132,-25.9445306089592));
#29623=CARTESIAN_POINT('Ctrl Pts',(-20.9181011542587,25.4124798792774,-25.9383733922374));
#29624=CARTESIAN_POINT('Ctrl Pts',(-20.9771351750754,25.493227408159,-25.9322161755156));
#29625=CARTESIAN_POINT('Ctrl Pts',(-21.0397333202698,25.5709976545559,-25.9260589587937));
#29626=CARTESIAN_POINT('Ctrl Pts',(-21.1023663887131,25.6488112886546,-25.9198983069859));
#29627=CARTESIAN_POINT('Ctrl Pts',(-21.1685672535822,25.723644007013,-25.9137376551781));
#29628=CARTESIAN_POINT('Ctrl Pts',(-21.2380083240489,25.7951677387144,-25.9075770033703));
#29629=CARTESIAN_POINT('Ctrl Pts',(-21.30756559412,25.8668111550531,-25.9014060426013));
#29630=CARTESIAN_POINT('Ctrl Pts',(-21.3803735832145,25.9351342270883,-25.8952350818323));
#29631=CARTESIAN_POINT('Ctrl Pts',(-21.4560699721281,25.9998477982044,-25.8890641210632));
#29632=CARTESIAN_POINT('Ctrl Pts',(-21.5138504470547,26.0492448820937,-25.8843537108428));
#29633=CARTESIAN_POINT('Ctrl Pts',(-21.5733131450406,26.0965396743571,-25.8796433006224));
#29634=CARTESIAN_POINT('Ctrl Pts',(-21.6342859287919,26.1416208071547,-25.874932890402));
#29635=CARTESIAN_POINT('Ctrl Pts',(-21.714165212207,26.2006807411426,-25.8687618716318));
#29636=CARTESIAN_POINT('Ctrl Pts',(-21.7969185090282,26.2561477796076,-25.8625908528617));
#29637=CARTESIAN_POINT('Ctrl Pts',(-21.8821887856859,26.3077298029972,-25.8564198340915));
#29638=CARTESIAN_POINT('Ctrl Pts',(-21.9451515000021,26.3458174500629,-25.8518632159228));
#29639=CARTESIAN_POINT('Ctrl Pts',(-22.0094857164726,26.3817876329866,-25.8473065977542));
#29640=CARTESIAN_POINT('Ctrl Pts',(-22.0750360153461,26.4155367745563,-25.8427499795855));
#29641=CARTESIAN_POINT('Origin',(-23.5502525316942,23.5502525316942,-77.3107734492734));
#29642=CARTESIAN_POINT('',(-22.0750358381979,26.41553668335,-24.3461133775544));
#29643=CARTESIAN_POINT('',(-22.0750360162151,26.4155367750037,-24.595751509546));
#29644=CARTESIAN_POINT('',(-22.0750360153461,26.4155367745563,-77.3107734492734));
#29645=CARTESIAN_POINT('Ctrl Pts',(-22.0750358381979,26.41553668335,-24.3461133775544));
#29646=CARTESIAN_POINT('Ctrl Pts',(-21.9942420567666,26.3739392958695,-24.3511965660311));
#29647=CARTESIAN_POINT('Ctrl Pts',(-21.915210609006,26.3289261847787,-24.3563001168851));
#29648=CARTESIAN_POINT('Ctrl Pts',(-21.7437655782969,26.2214199815303,-24.3678324034171));
#29649=CARTESIAN_POINT('Ctrl Pts',(-21.6525150813945,26.1573811521374,-24.3742908593729));
#29650=CARTESIAN_POINT('Ctrl Pts',(-21.5390546616165,26.068638211058,-24.3828717168821));
#29651=CARTESIAN_POINT('Ctrl Pts',(-21.513648116224,26.0481367645602,-24.3848309001178));
#29652=CARTESIAN_POINT('Ctrl Pts',(-21.478200653001,26.0186326016083,-24.3876205875967));
#29653=CARTESIAN_POINT('Ctrl Pts',(-21.4678975313913,26.0099469846117,-24.3884382972418));
#29654=CARTESIAN_POINT('Ctrl Pts',(-21.4500025419448,25.9946683393774,-24.3898707498562));
#29655=CARTESIAN_POINT('Ctrl Pts',(-21.442386442401,25.9881038820229,-24.3904843155895));
#29656=CARTESIAN_POINT('Ctrl Pts',(-21.4313292993113,25.9784829735044,-24.391380879353));
#29657=CARTESIAN_POINT('Ctrl Pts',(-21.4278638338603,25.9754545765195,-24.3916627094949));
#29658=CARTESIAN_POINT('Ctrl Pts',(-21.4218429421456,25.9701702577748,-24.3921538211899));
#29659=CARTESIAN_POINT('Ctrl Pts',(-21.4192845797578,25.9679176800463,-24.3923629627279));
#29660=CARTESIAN_POINT('Ctrl Pts',(-21.4143596290804,25.963567486651,-24.3927664613728));
#29661=CARTESIAN_POINT('Ctrl Pts',(-21.4119925438389,25.9614704371255,-24.392960794596));
#29662=CARTESIAN_POINT('Ctrl Pts',(-21.4064042304386,25.9565049349294,-24.3934205316858));
#29663=CARTESIAN_POINT('Ctrl Pts',(-21.4031856723078,25.9536334977325,-24.3936860610432));
#29664=CARTESIAN_POINT('Ctrl Pts',(-21.3936403042452,25.9450831190102,-24.3944757773306));
#29665=CARTESIAN_POINT('Ctrl Pts',(-21.3873302283899,25.9393856274369,-24.3950007477598));
#29666=CARTESIAN_POINT('Ctrl Pts',(-21.3298854188692,25.8871034771742,-24.3998068246709));
#29667=CARTESIAN_POINT('Ctrl Pts',(-21.2802438219251,25.8389119027674,-24.4041564342965));
#29668=CARTESIAN_POINT('Ctrl Pts',(-21.2082531198804,25.7643762605397,-24.4107750023431));
#29669=CARTESIAN_POINT('Ctrl Pts',(-21.1847121261474,25.7392074376824,-24.4129923546755));
#29670=CARTESIAN_POINT('Ctrl Pts',(-21.0736178722476,25.6165458569963,-24.4237153959014));
#29671=CARTESIAN_POINT('Ctrl Pts',(-20.9916693985912,25.514160270632,-24.4324258250087));
#29672=CARTESIAN_POINT('Ctrl Pts',(-20.835900403239,25.2931889296636,-24.4506278352556));
#29673=CARTESIAN_POINT('Ctrl Pts',(-20.7630866643506,25.1742109531433,-24.460115482091));
#29674=CARTESIAN_POINT('Ctrl Pts',(-20.6560132643234,24.9707122163578,-24.4755478720504));
#29675=CARTESIAN_POINT('Ctrl Pts',(-20.6172210949921,24.8887799985957,-24.4815622660975));
#29676=CARTESIAN_POINT('Ctrl Pts',(-20.5694664188923,24.7758365227026,-24.4894937801904));
#29677=CARTESIAN_POINT('Ctrl Pts',(-20.5574412069163,24.7461716431143,-24.4915443729831));
#29678=CARTESIAN_POINT('Ctrl Pts',(-20.5396624058426,24.7003646965779,-24.4946556751766));
#29679=CARTESIAN_POINT('Ctrl Pts',(-20.5335925928887,24.6843485339007,-24.4957333046094));
#29680=CARTESIAN_POINT('Ctrl Pts',(-20.5263193641045,24.6646853404913,-24.4970431785866));
#29681=CARTESIAN_POINT('Ctrl Pts',(-20.5249945541802,24.6610839578005,-24.4972825492739));
#29682=CARTESIAN_POINT('Ctrl Pts',(-20.5230545161551,24.6557809172264,-24.4976342236286));
#29683=CARTESIAN_POINT('Ctrl Pts',(-20.5224342900949,24.6540811109485,-24.4977468266259));
#29684=CARTESIAN_POINT('Ctrl Pts',(-20.5212364104313,24.6507895673814,-24.4979646388119));
#29685=CARTESIAN_POINT('Ctrl Pts',(-20.5206585796359,24.6491978968028,-24.4980698585799));
#29686=CARTESIAN_POINT('Ctrl Pts',(-20.519465785293,24.6459041804562,-24.4982873742448));
#29687=CARTESIAN_POINT('Ctrl Pts',(-20.518851002486,24.6442020763938,-24.4983996590513));
#29688=CARTESIAN_POINT('Ctrl Pts',(-20.5171802155366,24.6395640675289,-24.4987052919356));
#29689=CARTESIAN_POINT('Ctrl Pts',(-20.516127037101,24.6366271357791,-24.4988984699946));
#29690=CARTESIAN_POINT('Ctrl Pts',(-20.5121678759728,24.6255358086718,-24.4996266723458));
#29691=CARTESIAN_POINT('Ctrl Pts',(-20.5092904535769,24.6173711495599,-24.5001600029783));
#29692=CARTESIAN_POINT('Ctrl Pts',(-20.4609195629319,24.4783346514528,-24.5091975069974));
#29693=CARTESIAN_POINT('Ctrl Pts',(-20.4238729202963,24.3446553899401,-24.517217845754));
#29694=CARTESIAN_POINT('Ctrl Pts',(-20.3551706346225,24.0156382555668,-24.536272362119));
#29695=CARTESIAN_POINT('Ctrl Pts',(-20.3326574356841,23.8189847521018,-24.547117070942));
#29696=CARTESIAN_POINT('Ctrl Pts',(-20.3256208212519,23.5007927607372,-24.5651899284967));
#29697=CARTESIAN_POINT('Ctrl Pts',(-20.3297372762626,23.3800377929015,-24.5721640598763));
#29698=CARTESIAN_POINT('Ctrl Pts',(-20.3453062312673,23.2079899305531,-24.5824427175599));
#29699=CARTESIAN_POINT('Ctrl Pts',(-20.3512490558342,23.156297253546,-24.585574812308));
#29700=CARTESIAN_POINT('Ctrl Pts',(-20.3595523592231,23.0968049578778,-24.5892373976859));
#29701=CARTESIAN_POINT('Ctrl Pts',(-20.3606943141009,23.0888409285247,-24.5897288943518));
#29702=CARTESIAN_POINT('Ctrl Pts',(-20.3624701296571,23.0767780109904,-24.5904751976016));
#29703=CARTESIAN_POINT('Ctrl Pts',(-20.3630821067939,23.072675891899,-24.5907293094634));
#29704=CARTESIAN_POINT('Ctrl Pts',(-20.3641547980022,23.0655794749389,-24.5911694720465));
#29705=CARTESIAN_POINT('Ctrl Pts',(-20.3646118197373,23.0625846172243,-24.591355405287));
#29706=CARTESIAN_POINT('Ctrl Pts',(-20.365568049112,23.0563771639102,-24.5917411526894));
#29707=CARTESIAN_POINT('Ctrl Pts',(-20.3660678964055,23.0531646714878,-24.5919409869918));
#29708=CARTESIAN_POINT('Ctrl Pts',(-20.3672937210695,23.0453640785457,-24.5924267181702));
#29709=CARTESIAN_POINT('Ctrl Pts',(-20.3680247572274,23.0407767900571,-24.5927127756552));
#29710=CARTESIAN_POINT('Ctrl Pts',(-20.3708020896542,23.0235880918394,-24.5937862042517));
#29711=CARTESIAN_POINT('Ctrl Pts',(-20.3729133193837,23.0109974269687,-24.5945756389425));
#29712=CARTESIAN_POINT('Ctrl Pts',(-20.4083844396729,22.8069025392743,-24.607424484363));
#29713=CARTESIAN_POINT('Ctrl Pts',(-20.458921985018,22.6188262768828,-24.6200478186325));
#29714=CARTESIAN_POINT('Ctrl Pts',(-20.5918336647267,22.2579389643895,-24.6457555550066));
#29715=CARTESIAN_POINT('Ctrl Pts',(-20.6732649491656,22.0855835023762,-24.6587700828748));
#29716=CARTESIAN_POINT('Ctrl Pts',(-20.8033175417523,21.8635505196032,-24.6759683258234));
#29717=CARTESIAN_POINT('Ctrl Pts',(-20.8390145422813,21.8067488291666,-24.6804064953374));
#29718=CARTESIAN_POINT('Ctrl Pts',(-20.8974319489932,21.7199324189762,-24.6872057762782));
#29719=CARTESIAN_POINT('Ctrl Pts',(-20.9189481274954,21.6891329305297,-24.6896211211219));
#29720=CARTESIAN_POINT('Ctrl Pts',(-20.952303431785,21.6431214416742,-24.6932258971368));
#29721=CARTESIAN_POINT('Ctrl Pts',(-20.9637478094435,21.6276288332772,-24.6944390438673));
#29722=CARTESIAN_POINT('Ctrl Pts',(-20.9777246859083,21.6090585967343,-24.6958914920005));
#29723=CARTESIAN_POINT('Ctrl Pts',(-20.980124553005,21.6058823035649,-24.6961398615071));
#29724=CARTESIAN_POINT('Ctrl Pts',(-20.9836324166107,21.6012573871763,-24.6965014075827));
#29725=CARTESIAN_POINT('Ctrl Pts',(-20.9847357549222,21.5998052607723,-24.6966149112888));
#29726=CARTESIAN_POINT('Ctrl Pts',(-20.9868704247937,21.5970007227452,-24.6968340959611));
#29727=CARTESIAN_POINT('Ctrl Pts',(-20.9879015953884,21.5956481895299,-24.6969397883115));
#29728=CARTESIAN_POINT('Ctrl Pts',(-20.9900206387922,21.5928733084553,-24.6971566012376));
#29729=CARTESIAN_POINT('Ctrl Pts',(-20.9911086239971,21.5914510540718,-24.6972677132519));
#29730=CARTESIAN_POINT('Ctrl Pts',(-20.9937291751688,21.5880312829964,-24.6975348458409));
#29731=CARTESIAN_POINT('Ctrl Pts',(-20.9952629005193,21.5860346501976,-24.6976907839008));
#29732=CARTESIAN_POINT('Ctrl Pts',(-21.0008616586123,21.5787637335637,-24.6982585552015));
#29733=CARTESIAN_POINT('Ctrl Pts',(-21.0049407326039,21.573500207242,-24.6986693984758));
#29734=CARTESIAN_POINT('Ctrl Pts',(-21.0751090713098,21.483534191825,-24.7056893985408));
#29735=CARTESIAN_POINT('Ctrl Pts',(-21.1453851673489,21.4021653774305,-24.7120045047514));
#29736=CARTESIAN_POINT('Ctrl Pts',(-21.3948660591346,21.1409325738133,-24.7327511290629));
#29737=CARTESIAN_POINT('Ctrl Pts',(-21.5911937752434,20.9787518385778,-24.7465189818075));
#29738=CARTESIAN_POINT('Ctrl Pts',(-21.8797832001963,20.7927780074297,-24.7661495306448));
#29739=CARTESIAN_POINT('Ctrl Pts',(-21.9570250919267,20.7474400199854,-24.7713438428092));
#29740=CARTESIAN_POINT('Ctrl Pts',(-22.0893259150182,20.6770220488164,-24.7802253492873));
#29741=CARTESIAN_POINT('Ctrl Pts',(-22.1433850086716,20.6501692530227,-24.7838499385904));
#29742=CARTESIAN_POINT('Ctrl Pts',(-22.2057877483621,20.6213273781261,-24.7880404125832));
#29743=CARTESIAN_POINT('Ctrl Pts',(-22.2134256682169,20.61783338638,-24.788553416586));
#29744=CARTESIAN_POINT('Ctrl Pts',(-22.224921991625,20.6126286048934,-24.7893257556589));
#29745=CARTESIAN_POINT('Ctrl Pts',(-22.2287702815314,20.6108954526734,-24.7895843199667));
#29746=CARTESIAN_POINT('Ctrl Pts',(-22.2353957090791,20.6079272035765,-24.7900295357289));
#29747=CARTESIAN_POINT('Ctrl Pts',(-22.2381712165852,20.6066884636131,-24.7902160616375));
#29748=CARTESIAN_POINT('Ctrl Pts',(-22.2438918075935,20.6041449985452,-24.7906005470091));
#29749=CARTESIAN_POINT('Ctrl Pts',(-22.2468371025105,20.6028407591064,-24.7907985229131));
#29750=CARTESIAN_POINT('Ctrl Pts',(-22.253934027402,20.5997108073271,-24.791275613205));
#29751=CARTESIAN_POINT('Ctrl Pts',(-22.2580875575324,20.5978894424005,-24.7915548763077));
#29752=CARTESIAN_POINT('Ctrl Pts',(-22.2708518277206,20.5923242766125,-24.7924132218858));
#29753=CARTESIAN_POINT('Ctrl Pts',(-22.279475037692,20.5886093591834,-24.7929932909782));
#29754=CARTESIAN_POINT('Ctrl Pts',(-22.3806125536874,20.5455618927602,-24.7997991666576));
#29755=CARTESIAN_POINT('Ctrl Pts',(-22.4748928168715,20.5105450851924,-24.8061709491154));
#29756=CARTESIAN_POINT('Ctrl Pts',(-22.7967502871049,20.4078523582729,-24.8280470430414));
#29757=CARTESIAN_POINT('Ctrl Pts',(-23.0301059990025,20.3609168026128,-24.8441755224214));
#29758=CARTESIAN_POINT('Ctrl Pts',(-23.4347770175042,20.325142173986,-24.8716094853957));
#29759=CARTESIAN_POINT('Ctrl Pts',(-23.6040338753196,20.3235212395249,-24.8829017911953));
#29760=CARTESIAN_POINT('Ctrl Pts',(-23.7802520709472,20.3357112361222,-24.8939887584956));
#29761=CARTESIAN_POINT('Ctrl Pts',(-23.7878456990397,20.3362635742414,-24.8944651904783));
#29762=CARTESIAN_POINT('Ctrl Pts',(-23.7982875002998,20.337060289193,-24.8951184239805));
#29763=CARTESIAN_POINT('Ctrl Pts',(-23.8011373335486,20.3372815468779,-24.8952965137058));
#29764=CARTESIAN_POINT('Ctrl Pts',(-23.8059470911408,20.3376614090711,-24.8955967492564));
#29765=CARTESIAN_POINT('Ctrl Pts',(-23.807907164663,20.3378180157784,-24.8957190081312));
#29766=CARTESIAN_POINT('Ctrl Pts',(-23.8117693411559,20.3381301549741,-24.8959597246975));
#29767=CARTESIAN_POINT('Ctrl Pts',(-23.8136714494186,20.33828558316,-24.8960781880952));
#29768=CARTESIAN_POINT('Ctrl Pts',(-23.8178675274861,20.3386322123916,-24.8963393266138));
#29769=CARTESIAN_POINT('Ctrl Pts',(-23.8201614367503,20.3388241821308,-24.8964819580899));
#29770=CARTESIAN_POINT('Ctrl Pts',(-23.8281871675072,20.3395044891259,-24.8969805444856));
#29771=CARTESIAN_POINT('Ctrl Pts',(-23.8339179294859,20.3400057190726,-24.8973357735987));
#29772=CARTESIAN_POINT('Ctrl Pts',(-23.8924304317722,20.3452813076583,-24.9009550037664));
#29773=CARTESIAN_POINT('Ctrl Pts',(-23.9450918740019,20.3513419424527,-24.9041479392798));
#29774=CARTESIAN_POINT('Ctrl Pts',(-24.3053621488696,20.4018377480508,-24.9256953060309));
#29775=CARTESIAN_POINT('Ctrl Pts',(-24.6053151435294,20.4892720706137,-24.9422885620987));
#29776=CARTESIAN_POINT('Ctrl Pts',(-25.0082028413813,20.6731155715469,-24.9676174329098));
#29777=CARTESIAN_POINT('Ctrl Pts',(-25.1247799959606,20.7352226792367,-24.9753316666834));
#29778=CARTESIAN_POINT('Ctrl Pts',(-25.2551571926593,20.8153190460711,-24.984583487794));
#29779=CARTESIAN_POINT('Ctrl Pts',(-25.2729923736557,20.826518242533,-24.985863138569));
#29780=CARTESIAN_POINT('Ctrl Pts',(-25.2958604313623,20.8411921812023,-24.9875225668843));
#29781=CARTESIAN_POINT('Ctrl Pts',(-25.300995243951,20.8445077402075,-24.9878964028895));
#29782=CARTESIAN_POINT('Ctrl Pts',(-25.3092449414227,20.8498679020947,-24.9884990060819));
#29783=CARTESIAN_POINT('Ctrl Pts',(-25.3123657839856,20.8519033454001,-24.9887274299295));
#29784=CARTESIAN_POINT('Ctrl Pts',(-25.3182969246568,20.8557863696564,-24.9891624280565));
#29785=CARTESIAN_POINT('Ctrl Pts',(-25.3211078760074,20.8576329478625,-24.9893689644735));
#29786=CARTESIAN_POINT('Ctrl Pts',(-25.327501034483,20.861847101054,-24.9898395684709));
#29787=CARTESIAN_POINT('Ctrl Pts',(-25.3310814052966,20.8642174383234,-24.9901037398517));
#29788=CARTESIAN_POINT('Ctrl Pts',(-25.3419530551118,20.8714461624883,-24.9909077750359));
#29789=CARTESIAN_POINT('Ctrl Pts',(-25.349229223334,20.8763271045706,-24.9914484901306));
#29790=CARTESIAN_POINT('Ctrl Pts',(-25.4008117339563,20.9112351234727,-24.9953003538391));
#29791=CARTESIAN_POINT('Ctrl Pts',(-25.4443816440976,20.9423306404437,-24.9986520302611));
#29792=CARTESIAN_POINT('Ctrl Pts',(-25.4955332093108,20.9807952869625,-25.0027096482574));
#29793=CARTESIAN_POINT('Ctrl Pts',(-25.5038804688768,20.987136200711,-25.0033757999959));
#29794=CARTESIAN_POINT('Ctrl Pts',(-25.7604356513508,21.1840071851929,-25.0239743455247));
#29795=CARTESIAN_POINT('Ctrl Pts',(-25.9795760202373,21.4096135289019,-25.0454125857946));
#29796=CARTESIAN_POINT('Ctrl Pts',(-26.2145839418957,21.7349565496501,-25.0723390774719));
#29797=CARTESIAN_POINT('Ctrl Pts',(-26.2634661549541,21.8088635518611,-25.0782164990782));
#29798=CARTESIAN_POINT('Ctrl Pts',(-26.3340400323854,21.9257690607955,-25.0870527925547));
#29799=CARTESIAN_POINT('Ctrl Pts',(-26.35791678203,21.9673938916192,-25.0901133549678));
#29800=CARTESIAN_POINT('Ctrl Pts',(-26.3832419160754,22.0139213161168,-25.0934280746687));
#29801=CARTESIAN_POINT('Ctrl Pts',(-26.3856170279805,22.0183091156466,-25.0937396425749));
#29802=CARTESIAN_POINT('Ctrl Pts',(-26.3891253037819,22.024826438771,-25.0942008785615));
#29803=CARTESIAN_POINT('Ctrl Pts',(-26.3902662676191,22.026951720652,-25.0943510433309));
#29804=CARTESIAN_POINT('Ctrl Pts',(-26.3922078700308,22.0305781219144,-25.0946068549077));
#29805=CARTESIAN_POINT('Ctrl Pts',(-26.3930097061134,22.0320785943001,-25.0947125788137));
#29806=CARTESIAN_POINT('Ctrl Pts',(-26.3946525539107,22.0351587132599,-25.0949293551341));
#29807=CARTESIAN_POINT('Ctrl Pts',(-26.395493436236,22.0367384220128,-25.0950403991395));
#29808=CARTESIAN_POINT('Ctrl Pts',(-26.3975122473545,22.0405386540711,-25.0953072109253));
#29809=CARTESIAN_POINT('Ctrl Pts',(-26.3986888971739,22.0427598608585,-25.0954628966264));
#29810=CARTESIAN_POINT('Ctrl Pts',(-26.4029620255938,22.0508492737995,-25.0960289372831));
#29811=CARTESIAN_POINT('Ctrl Pts',(-26.4060430064908,22.0567257149562,-25.0964383099897));
#29812=CARTESIAN_POINT('Ctrl Pts',(-26.4577959584851,22.1561812384885,-25.1033367305253));
#29813=CARTESIAN_POINT('Ctrl Pts',(-26.501868974304,22.2520964265145,-25.1095423662194));
#29814=CARTESIAN_POINT('Ctrl Pts',(-26.6470901888889,22.6139767095907,-25.1319578696367));
#29815=CARTESIAN_POINT('Ctrl Pts',(-26.7176115374808,22.8908052075387,-25.1472952514175));
#29816=CARTESIAN_POINT('Ctrl Pts',(-26.763440811863,23.2799435771829,-25.1699287516284));
#29817=CARTESIAN_POINT('Ctrl Pts',(-26.7706612529901,23.3871273484865,-25.176256398643));
#29818=CARTESIAN_POINT('Ctrl Pts',(-26.7728416733939,23.5130652031083,-25.1838833289959));
#29819=CARTESIAN_POINT('Ctrl Pts',(-26.773002644352,23.5316686044944,-25.1850147830875));
#29820=CARTESIAN_POINT('Ctrl Pts',(-26.7730024965163,23.5560682488993,-25.1865053929689));
#29821=CARTESIAN_POINT('Ctrl Pts',(-26.772986824523,23.5618643988586,-25.1868599786412));
#29822=CARTESIAN_POINT('Ctrl Pts',(-26.7729377463209,23.5709501786123,-25.1874165900529));
#29823=CARTESIAN_POINT('Ctrl Pts',(-26.7729149391584,23.5742398731262,-25.18761828284));
#29824=CARTESIAN_POINT('Ctrl Pts',(-26.7728615327684,23.5805495615121,-25.1880054422562));
#29825=CARTESIAN_POINT('Ctrl Pts',(-26.7728317253419,23.5835695602356,-25.1881908838321));
#29826=CARTESIAN_POINT('Ctrl Pts',(-26.7727518242488,23.5906555902458,-25.1886263190768));
#29827=CARTESIAN_POINT('Ctrl Pts',(-26.7726982801883,23.5947215706633,-25.1888764208102));
#29828=CARTESIAN_POINT('Ctrl Pts',(-26.7725216750178,23.606446944656,-25.1895983790682));
#29829=CARTESIAN_POINT('Ctrl Pts',(-26.7723790003642,23.6141059758931,-25.1900708506798));
#29830=CARTESIAN_POINT('Ctrl Pts',(-26.7712362172908,23.6655939150874,-25.1932531001028));
#29831=CARTESIAN_POINT('Ctrl Pts',(-26.7693692134111,23.7093971855818,-25.1959899785362));
#29832=CARTESIAN_POINT('Ctrl Pts',(-26.7619186212252,23.8275066412046,-25.2034541201707));
#29833=CARTESIAN_POINT('Ctrl Pts',(-26.7546509317697,23.901675869812,-25.2082324795851));
#29834=CARTESIAN_POINT('Ctrl Pts',(-26.724906397274,24.1251128121717,-25.2229054033648));
#29835=CARTESIAN_POINT('Ctrl Pts',(-26.6945118729874,24.2731054473815,-25.2330126697525));
#29836=CARTESIAN_POINT('Ctrl Pts',(-26.590672507125,24.6443251435024,-25.2590688590711));
#29837=CARTESIAN_POINT('Ctrl Pts',(-26.5029950011948,24.8626862556386,-25.2751013124365));
#29838=CARTESIAN_POINT('Ctrl Pts',(-26.3861254169185,25.0813039438851,-25.2907489502845));
#29839=CARTESIAN_POINT('Ctrl Pts',(-26.3798007370111,25.0929613234707,-25.2915818772712));
#29840=CARTESIAN_POINT('Ctrl Pts',(-26.3716419636381,25.1077802474873,-25.2926385140698));
#29841=CARTESIAN_POINT('Ctrl Pts',(-26.3698743296894,25.1109779491634,-25.2928663900156));
#29842=CARTESIAN_POINT('Ctrl Pts',(-26.3670574117202,25.1160534313222,-25.2932278652182));
#29843=CARTESIAN_POINT('Ctrl Pts',(-26.3660116859845,25.1179331670627,-25.2933616926141));
#29844=CARTESIAN_POINT('Ctrl Pts',(-26.3640550236922,25.1214420754794,-25.2936114184695));
#29845=CARTESIAN_POINT('Ctrl Pts',(-26.3631445598176,25.1230714928659,-25.2937273460361));
#29846=CARTESIAN_POINT('Ctrl Pts',(-26.3610992378097,25.1267244597029,-25.2939871610301));
#29847=CARTESIAN_POINT('Ctrl Pts',(-26.3599636123488,25.1287475707767,-25.2941309977533));
#29848=CARTESIAN_POINT('Ctrl Pts',(-26.3566017512803,25.1347215865861,-25.2945555715205));
#29849=CARTESIAN_POINT('Ctrl Pts',(-26.3543693480444,25.1386690416312,-25.2948359109001));
#29850=CARTESIAN_POINT('Ctrl Pts',(-26.3369167534398,25.1693781964003,-25.2970152998891));
#29851=CARTESIAN_POINT('Ctrl Pts',(-26.3213214519027,25.19592643981,-25.2988904724722));
#29852=CARTESIAN_POINT('Ctrl Pts',(-26.2659851992392,25.2871088638027,-25.3053143200299));
#29853=CARTESIAN_POINT('Ctrl Pts',(-26.2243416399564,25.350564477048,-25.3097556288964));
#29854=CARTESIAN_POINT('Ctrl Pts',(-25.9947049575678,25.6749044566902,-25.3326233146511));
#29855=CARTESIAN_POINT('Ctrl Pts',(-25.7706983366996,25.9080351566661,-25.3498404506165));
#29856=CARTESIAN_POINT('Ctrl Pts',(-25.4996794513211,26.1166254322822,-25.3698751400516));
#29857=CARTESIAN_POINT('Ctrl Pts',(-25.4833670027122,26.1289350627727,-25.371077468022));
#29858=CARTESIAN_POINT('Ctrl Pts',(-25.463399221677,26.1437071179424,-25.3725455591721));
#29859=CARTESIAN_POINT('Ctrl Pts',(-25.4598542611247,26.146318436677,-25.3728060564054));
#29860=CARTESIAN_POINT('Ctrl Pts',(-25.4530687889067,26.1512953900363,-25.3733044229119));
#29861=CARTESIAN_POINT('Ctrl Pts',(-25.4498291872766,26.153662255308,-25.3735422480229));
#29862=CARTESIAN_POINT('Ctrl Pts',(-25.4426371394999,26.1588962215782,-25.3740699915606));
#29863=CARTESIAN_POINT('Ctrl Pts',(-25.4386825853658,26.161760398167,-25.3743600131102));
#29864=CARTESIAN_POINT('Ctrl Pts',(-25.4290878115077,26.1686764438218,-25.3750633118715));
#29865=CARTESIAN_POINT('Ctrl Pts',(-25.4234409908385,26.1727190782331,-25.3754769175077));
#29866=CARTESIAN_POINT('Ctrl Pts',(-25.4162456212369,26.1778352425375,-25.3760035799283));
#29867=CARTESIAN_POINT('Ctrl Pts',(-25.4147091087239,26.1789257302666,-25.3761160231406));
#29868=CARTESIAN_POINT('Ctrl Pts',(-25.4078589152983,26.183778395495,-25.3766172326296));
#29869=CARTESIAN_POINT('Ctrl Pts',(-25.4025348237314,26.1875257942529,-25.3770065321166));
#29870=CARTESIAN_POINT('Ctrl Pts',(-25.3933405446863,26.1939556755297,-25.3776784155976));
#29871=CARTESIAN_POINT('Ctrl Pts',(-25.38947575301,26.1966458656836,-25.3779607172545));
#29872=CARTESIAN_POINT('Ctrl Pts',(-25.3760585976065,26.2059416426025,-25.3789403582186));
#29873=CARTESIAN_POINT('Ctrl Pts',(-25.3664765136131,26.2125040010901,-25.3796392704975));
#29874=CARTESIAN_POINT('Ctrl Pts',(-25.3529516299144,26.2216596123777,-25.3806248661675));
#29875=CARTESIAN_POINT('Ctrl Pts',(-25.3490382096055,26.2242962699358,-25.3809099423132));
#29876=CARTESIAN_POINT('Ctrl Pts',(-25.3283307484909,26.2381818454686,-25.3824178597072));
#29877=CARTESIAN_POINT('Ctrl Pts',(-25.3114372345221,26.2492809780931,-25.383646198793));
#29878=CARTESIAN_POINT('Ctrl Pts',(-25.2891999355987,26.2635933382306,-25.3852611017637));
#29879=CARTESIAN_POINT('Ctrl Pts',(-25.2839494047233,26.2669511821796,-25.3856422586221));
#29880=CARTESIAN_POINT('Ctrl Pts',(-25.2758384527454,26.2721052462623,-25.3862308561582));
#29881=CARTESIAN_POINT('Ctrl Pts',(-25.2729848725658,26.2739122483821,-25.3864378957839));
#29882=CARTESIAN_POINT('Ctrl Pts',(-25.2673011265986,26.2774989199629,-25.386850199858));
#29883=CARTESIAN_POINT('Ctrl Pts',(-25.2644710215902,26.2792786782073,-25.3870554606738));
#29884=CARTESIAN_POINT('Ctrl Pts',(-25.2581976393072,26.2832101892727,-25.3875103737555));
#29885=CARTESIAN_POINT('Ctrl Pts',(-25.25475305876,26.285359842519,-25.3877601032832));
#29886=CARTESIAN_POINT('Ctrl Pts',(-25.2449515517711,26.2914509447047,-25.3884705590168));
#29887=CARTESIAN_POINT('Ctrl Pts',(-25.2385849843963,26.295376761266,-25.3889318610918));
#29888=CARTESIAN_POINT('Ctrl Pts',(-25.1975301416009,26.320495564185,-25.3919055275477));
#29889=CARTESIAN_POINT('Ctrl Pts',(-25.1624584995583,26.3410519971134,-25.394441117158));
#29890=CARTESIAN_POINT('Ctrl Pts',(-25.0569090985583,26.4002637512238,-25.4020624068653));
#29891=CARTESIAN_POINT('Ctrl Pts',(-24.9853683382631,26.4369493933388,-25.4072163515426));
#29892=CARTESIAN_POINT('Ctrl Pts',(-24.7745449265404,26.5352834901584,-25.4223735829986));
#29893=CARTESIAN_POINT('Ctrl Pts',(-24.6321792707311,26.589780091718,-25.4325812533794));
#29894=CARTESIAN_POINT('Ctrl Pts',(-24.2856361981713,26.6949938428261,-25.4570697029826));
#29895=CARTESIAN_POINT('Ctrl Pts',(-24.0792687220177,26.7362129017849,-25.4713853704981));
#29896=CARTESIAN_POINT('Ctrl Pts',(-23.864664158185,26.7576339377859,-25.4852012007488));
#29897=CARTESIAN_POINT('Ctrl Pts',(-23.8589818607033,26.7581858784842,-25.4855662287531));
#29898=CARTESIAN_POINT('Ctrl Pts',(-23.8491217673299,26.7591171813321,-25.4861982364657));
#29899=CARTESIAN_POINT('Ctrl Pts',(-23.8449446599103,26.759503489428,-25.4864655432152));
#29900=CARTESIAN_POINT('Ctrl Pts',(-23.8246727901913,26.761338364082,-25.487760655175));
#29901=CARTESIAN_POINT('Ctrl Pts',(-23.808567676587,26.7626740501463,-25.4887829877595));
#29902=CARTESIAN_POINT('Ctrl Pts',(-23.7834862285339,26.7645643494126,-25.4903641880516));
#29903=CARTESIAN_POINT('Ctrl Pts',(-23.7745167244039,26.7652026083401,-25.4909274743598));
#29904=CARTESIAN_POINT('Ctrl Pts',(-23.7623816169219,26.7660150948552,-25.4916865131141));
#29905=CARTESIAN_POINT('Ctrl Pts',(-23.7592183669247,26.7662221974934,-25.4918840912387));
#29906=CARTESIAN_POINT('Ctrl Pts',(-23.75423882804,26.7665408372821,-25.4921946694891));
#29907=CARTESIAN_POINT('Ctrl Pts',(-23.7524227522241,26.7666555032961,-25.4923078463569));
#29908=CARTESIAN_POINT('Ctrl Pts',(-23.7489196819735,26.7668737065528,-25.4925259744105));
#29909=CARTESIAN_POINT('Ctrl Pts',(-23.7472327145148,26.7669774541484,-25.4926309366481));
#29910=CARTESIAN_POINT('Ctrl Pts',(-23.7432148351371,26.7672213790242,-25.4928807343515));
#29911=CARTESIAN_POINT('Ctrl Pts',(-23.7408838538725,26.7673603499573,-25.4930255007715));
#29912=CARTESIAN_POINT('Ctrl Pts',(-23.7340450090293,26.7677606166555,-25.4934497825451));
#29913=CARTESIAN_POINT('Ctrl Pts',(-23.7295367212226,26.7680149734371,-25.4937289067766));
#29914=CARTESIAN_POINT('Ctrl Pts',(-23.6968968366111,26.7697877000548,-25.4957457301195));
#29915=CARTESIAN_POINT('Ctrl Pts',(-23.6687458053862,26.7709466692085,-25.497463526227));
#29916=CARTESIAN_POINT('Ctrl Pts',(-23.5753301375406,26.7735660187263,-25.5031026907515));
#29917=CARTESIAN_POINT('Ctrl Pts',(-23.510032919845,26.7734128327498,-25.5069456578207));
#29918=CARTESIAN_POINT('Ctrl Pts',(-23.1813916093272,26.7626515615342,-25.5259887504925));
#29919=CARTESIAN_POINT('Ctrl Pts',(-22.9200420020355,26.7217539591146,-25.5402446042775));
#29920=CARTESIAN_POINT('Ctrl Pts',(-22.5195078414425,26.6075503236672,-25.5640006145775));
#29921=CARTESIAN_POINT('Ctrl Pts',(-22.3756324402608,26.5552088110836,-25.5729361593038));
#29922=CARTESIAN_POINT('Ctrl Pts',(-22.2257724556061,26.4882784400287,-25.5829187877678));
#29923=CARTESIAN_POINT('Ctrl Pts',(-22.2155413559588,26.483644728855,-25.5836037374406));
#29924=CARTESIAN_POINT('Ctrl Pts',(-22.201337443255,26.4771220188907,-25.5845595067221));
#29925=CARTESIAN_POINT('Ctrl Pts',(-22.1973438769779,26.475278186724,-25.5848287660469));
#29926=CARTESIAN_POINT('Ctrl Pts',(-22.19046550888,26.4720853395405,-25.5852934573601));
#29927=CARTESIAN_POINT('Ctrl Pts',(-22.1875789009828,26.4707402102292,-25.5854887546627));
#29928=CARTESIAN_POINT('Ctrl Pts',(-22.1816192627898,26.4679523213986,-25.5858925487251));
#29929=CARTESIAN_POINT('Ctrl Pts',(-22.1785465104716,26.4665089811164,-25.5861010654169));
#29930=CARTESIAN_POINT('Ctrl Pts',(-22.1713894614715,26.4631333413704,-25.5865874983815));
#29931=CARTESIAN_POINT('Ctrl Pts',(-22.1673069440084,26.4611973059852,-25.5868655442008));
#29932=CARTESIAN_POINT('Ctrl Pts',(-22.1545432197083,26.4551115064115,-25.5877366467598));
#29933=CARTESIAN_POINT('Ctrl Pts',(-22.1458765779327,26.4509314735687,-25.5883307567479));
#29934=CARTESIAN_POINT('Ctrl Pts',(-22.1163850462825,26.4365441768311,-25.5903615011968));
#29935=CARTESIAN_POINT('Ctrl Pts',(-22.0956529123993,26.426151563364,-25.591804560725));
#29936=CARTESIAN_POINT('Ctrl Pts',(-22.0750360129136,26.4155367733039,-25.5932554334314));
#29937=CARTESIAN_POINT('',(-26.7730012125181,23.5531684787983,-25.4357734492732));
#29938=CARTESIAN_POINT('Ctrl Pts',(-22.0750360153461,26.4155367745563,-25.8427499795855));
#29939=CARTESIAN_POINT('Ctrl Pts',(-22.1636338262233,26.4611521281618,-25.8365912525975));
#29940=CARTESIAN_POINT('Ctrl Pts',(-22.2544540515615,26.5027082272478,-25.8304325256094));
#29941=CARTESIAN_POINT('Ctrl Pts',(-22.3470880535136,26.5399871020105,-25.8242737986213));
#29942=CARTESIAN_POINT('Ctrl Pts',(-22.4399842542781,26.5773714939319,-25.8180976394716));
#29943=CARTESIAN_POINT('Ctrl Pts',(-22.5347041380959,26.6104541829362,-25.8119214803219));
#29944=CARTESIAN_POINT('Ctrl Pts',(-22.6308118557336,26.6390624005416,-25.8057453211721));
#29945=CARTESIAN_POINT('Ctrl Pts',(-22.7265250860868,26.6675531918013,-25.7995945129131));
#29946=CARTESIAN_POINT('Ctrl Pts',(-22.8236143597423,26.6916060486344,-25.7934437046541));
#29947=CARTESIAN_POINT('Ctrl Pts',(-22.921631680785,26.7110994733069,-25.7872928963952));
#29948=CARTESIAN_POINT('Ctrl Pts',(-23.0196313073245,26.7305893789435,-25.7811431985062));
#29949=CARTESIAN_POINT('Ctrl Pts',(-23.118558222282,26.7455214036659,-25.7749935006173));
#29950=CARTESIAN_POINT('Ctrl Pts',(-23.2179534647942,26.7558250067191,-25.7688438027283));
#29951=CARTESIAN_POINT('Ctrl Pts',(-23.3173573550546,26.7661295062234,-25.7626935697933));
#29952=CARTESIAN_POINT('Ctrl Pts',(-23.4172292216113,26.7718047397265,-25.7565433368582));
#29953=CARTESIAN_POINT('Ctrl Pts',(-23.5171052057916,26.7728320601598,-25.7503931039231));
#29954=CARTESIAN_POINT('Ctrl Pts',(-23.6177178214486,26.7738669575554,-25.7441975101818));
#29955=CARTESIAN_POINT('Ctrl Pts',(-23.7183341686747,26.77018508424,-25.7380019164405));
#29956=CARTESIAN_POINT('Ctrl Pts',(-23.8184818372402,26.7618207782283,-25.7318063226992));
#29957=CARTESIAN_POINT('Ctrl Pts',(-23.9180485167876,26.7535049962613,-25.7256466716011));
#29958=CARTESIAN_POINT('Ctrl Pts',(-24.0171515152515,26.7405610834495,-25.719487020503));
#29959=CARTESIAN_POINT('Ctrl Pts',(-24.1153348872376,26.7230745396161,-25.713327369405));
#29960=CARTESIAN_POINT('Ctrl Pts',(-24.2143776349878,26.7054349402126,-25.707113804342));
#29961=CARTESIAN_POINT('Ctrl Pts',(-24.3124841403336,26.6831729071579,-25.700900239279));
#29962=CARTESIAN_POINT('Ctrl Pts',(-24.4092014443937,26.6564277244147,-25.6946866742161));
#29963=CARTESIAN_POINT('Ctrl Pts',(-24.5059187484537,26.6296825416715,-25.6884731091531));
#29964=CARTESIAN_POINT('Ctrl Pts',(-24.6012464461555,26.5984544082594,-25.6822595440902));
#29965=CARTESIAN_POINT('Ctrl Pts',(-24.6947529679961,26.5629317900629,-25.6760459790272));
#29966=CARTESIAN_POINT('Ctrl Pts',(-24.7876353608333,26.5276462750743,-25.6698738877149));
#29967=CARTESIAN_POINT('Ctrl Pts',(-24.8790480053133,26.4879991748671,-25.6637017964026));
#29968=CARTESIAN_POINT('Ctrl Pts',(-24.9685519169491,26.444133043444,-25.6575297050903));
#29969=CARTESIAN_POINT('Ctrl Pts',(-25.0579345596333,26.4003263462923,-25.6513659763515));
#29970=CARTESIAN_POINT('Ctrl Pts',(-25.1454132230758,26.3523121693096,-25.6452022476127));
#29971=CARTESIAN_POINT('Ctrl Pts',(-25.2305668039053,26.300281896829,-25.639038518874));
#29972=CARTESIAN_POINT('Ctrl Pts',(-25.315630172508,26.2483067455388,-25.6328813200273));
#29973=CARTESIAN_POINT('Ctrl Pts',(-25.3983729869398,26.1923241826761,-25.6267241211806));
#29974=CARTESIAN_POINT('Ctrl Pts',(-25.478397635834,26.1325720355282,-25.6205669223339));
#29975=CARTESIAN_POINT('Ctrl Pts',(-25.5583637915627,26.0728635635764,-25.6144142240262));
#29976=CARTESIAN_POINT('Ctrl Pts',(-25.6356153848488,26.0093912445286,-25.6082615257185));
#29977=CARTESIAN_POINT('Ctrl Pts',(-25.7097835462753,25.9424363372498,-25.6021088274108));
#29978=CARTESIAN_POINT('Ctrl Pts',(-25.7839235830294,25.875506819367,-25.5959584622151));
#29979=CARTESIAN_POINT('Ctrl Pts',(-25.8549821891059,25.805097628041,-25.5898080970194));
#29980=CARTESIAN_POINT('Ctrl Pts',(-25.9226240746639,25.7315298695419,-25.5836577318236));
#29981=CARTESIAN_POINT('Ctrl Pts',(-25.9902584065176,25.657970326501,-25.5775080534514));
#29982=CARTESIAN_POINT('Ctrl Pts',(-26.0544764824102,25.5812532373267,-25.5713583750792));
#29983=CARTESIAN_POINT('Ctrl Pts',(-26.1149810560759,25.5017353419498,-25.565208696707));
#29984=CARTESIAN_POINT('Ctrl Pts',(-26.1754950597027,25.4222050532839,-25.5590580598746));
#29985=CARTESIAN_POINT('Ctrl Pts',(-26.2322941484489,25.3398734371122,-25.5529074230421));
#29986=CARTESIAN_POINT('Ctrl Pts',(-26.2851230418963,25.2551281444375,-25.5467567862097));
#29987=CARTESIAN_POINT('Ctrl Pts',(-26.338008451162,25.1702921921019,-25.5405995694879));
#29988=CARTESIAN_POINT('Ctrl Pts',(-26.3869149534866,25.0830377763704,-25.5344423527661));
#29989=CARTESIAN_POINT('Ctrl Pts',(-26.4316321645472,24.9937791070921,-25.5282851360443));
#29990=CARTESIAN_POINT('Ctrl Pts',(-26.4763743231567,24.9044706407677,-25.5221244842365));
#29991=CARTESIAN_POINT('Ctrl Pts',(-26.5169223597245,24.8131560911232,-25.5159638324287));
#29992=CARTESIAN_POINT('Ctrl Pts',(-26.5531140382146,24.7202697688142,-25.5098031806209));
#29993=CARTESIAN_POINT('Ctrl Pts',(-26.5893662782528,24.6272280146571,-25.5036322198519));
#29994=CARTESIAN_POINT('Ctrl Pts',(-26.6212474603662,24.5326096460635,-25.4974612590828));
#29995=CARTESIAN_POINT('Ctrl Pts',(-26.6486451765087,24.4368643864872,-25.4912902983138));
#29996=CARTESIAN_POINT('Ctrl Pts',(-26.6695583676576,24.3637802321472,-25.4865798880933));
#29997=CARTESIAN_POINT('Ctrl Pts',(-26.6878602727366,24.2900398083783,-25.4818694778729));
#29998=CARTESIAN_POINT('Ctrl Pts',(-26.7035211438753,24.2158459676096,-25.4771590676524));
#29999=CARTESIAN_POINT('Ctrl Pts',(-26.7324039533253,24.0790128025634,-25.4684718190552));
#30000=CARTESIAN_POINT('Ctrl Pts',(-26.7523885214649,23.9402409635565,-25.4597845704581));
#30001=CARTESIAN_POINT('Ctrl Pts',(-26.7632725917776,23.8004917292665,-25.451097321861));
#30002=CARTESIAN_POINT('Ctrl Pts',(-26.7696722438977,23.7183215063795,-25.4459893643317));
#30003=CARTESIAN_POINT('Ctrl Pts',(-26.7729264349836,23.6358137368479,-25.4408814068025));
#30004=CARTESIAN_POINT('Ctrl Pts',(-26.7730012125181,23.5531684787983,-25.4357734492732));
#30005=CARTESIAN_POINT('Ctrl Pts',(-26.7730011889102,23.5531944548989,-25.4353089034207));
#30006=CARTESIAN_POINT('Ctrl Pts',(-26.7731884018712,23.3481108152563,-25.4238407640643));
#30007=CARTESIAN_POINT('Ctrl Pts',(-26.7538000984645,23.1434866085334,-25.4124470511572));
#30008=CARTESIAN_POINT('Ctrl Pts',(-26.7031666390037,22.8799922622032,-25.3967826797724));
#30009=CARTESIAN_POINT('Ctrl Pts',(-26.6894092282985,22.8182616518643,-25.3930429563939));
#30010=CARTESIAN_POINT('Ctrl Pts',(-26.668420407663,22.7356161449482,-25.3879222863631));
#30011=CARTESIAN_POINT('Ctrl Pts',(-26.6627762856602,22.7143104346675,-25.3865919026157));
#30012=CARTESIAN_POINT('Ctrl Pts',(-26.6542383834634,22.6833669565597,-25.3846440141879));
#30013=CARTESIAN_POINT('Ctrl Pts',(-26.651517222446,22.6736818941095,-25.3840320896982));
#30014=CARTESIAN_POINT('Ctrl Pts',(-26.6465449289241,22.6562976690975,-25.3829295945767));
#30015=CARTESIAN_POINT('Ctrl Pts',(-26.6443103054599,22.6485938400208,-25.3824395640204));
#30016=CARTESIAN_POINT('Ctrl Pts',(-26.6408780439607,22.6369241860975,-25.3816950300408));
#30017=CARTESIAN_POINT('Ctrl Pts',(-26.6397014703825,22.6329521561756,-25.3814412162738));
#30018=CARTESIAN_POINT('Ctrl Pts',(-26.6375688243138,22.6258031392673,-25.3809836765325));
#30019=CARTESIAN_POINT('Ctrl Pts',(-26.636615496696,22.6226253339657,-25.3807800407724));
#30020=CARTESIAN_POINT('Ctrl Pts',(-26.6346975093471,22.6162676363982,-25.3803721224825));
#30021=CARTESIAN_POINT('Ctrl Pts',(-26.6337328351289,22.6130877526885,-25.3801678396835));
#30022=CARTESIAN_POINT('Ctrl Pts',(-26.6310239654322,22.6042078881229,-25.3795966552453));
#30023=CARTESIAN_POINT('Ctrl Pts',(-26.629268877884,22.5985112676431,-25.3792293961564));
#30024=CARTESIAN_POINT('Ctrl Pts',(-26.622128657541,22.5755621820864,-25.3777464935016));
#30025=CARTESIAN_POINT('Ctrl Pts',(-26.6166143242975,22.5583505478229,-25.3766266048381));
#30026=CARTESIAN_POINT('Ctrl Pts',(-26.5236614073807,22.2764053979661,-25.3581519600213));
#30027=CARTESIAN_POINT('Ctrl Pts',(-26.4023970181992,22.024130081821,-25.339579901343));
#30028=CARTESIAN_POINT('Ctrl Pts',(-26.2280885577321,21.7566644747549,-25.3179710301184));
#30029=CARTESIAN_POINT('Ctrl Pts',(-26.2052948315316,21.7230923563477,-25.3152235755487));
#30030=CARTESIAN_POINT('Ctrl Pts',(-26.1601961409055,21.6592945322985,-25.3099429938384));
#30031=CARTESIAN_POINT('Ctrl Pts',(-26.1379844457675,21.6290103779702,-25.3074095324303));
#30032=CARTESIAN_POINT('Ctrl Pts',(-26.0569976219313,21.5225435138002,-25.2984211826418));
#30033=CARTESIAN_POINT('Ctrl Pts',(-25.9953419616863,21.4486066427533,-25.2920253528034));
#30034=CARTESIAN_POINT('Ctrl Pts',(-25.8994727031881,21.3435818525894,-25.2828292845965));
#30035=CARTESIAN_POINT('Ctrl Pts',(-25.8677548923741,21.3102939930612,-25.2798969970652));
#30036=CARTESIAN_POINT('Ctrl Pts',(-25.832586026379,21.2749313314308,-25.2767737138878));
#30037=CARTESIAN_POINT('Ctrl Pts',(-25.8298333296033,21.272173487519,-25.2765300816771));
#30038=CARTESIAN_POINT('Ctrl Pts',(-25.8253426346145,21.2676906854283,-25.2761339842759));
#30039=CARTESIAN_POINT('Ctrl Pts',(-25.8236076704964,21.2659627139585,-25.2759812825055));
#30040=CARTESIAN_POINT('Ctrl Pts',(-25.8202452034551,21.26262142416,-25.2756859765076));
#30041=CARTESIAN_POINT('Ctrl Pts',(-25.8186179465947,21.2610078618156,-25.275543352924));
#30042=CARTESIAN_POINT('Ctrl Pts',(-25.8156633477755,21.2580843715041,-25.2752849182419));
#30043=CARTESIAN_POINT('Ctrl Pts',(-25.8143365942525,21.25677386427,-25.2751690609383));
#30044=CARTESIAN_POINT('Ctrl Pts',(-25.811663806379,21.2541383845913,-25.2749360489257));
#30045=CARTESIAN_POINT('Ctrl Pts',(-25.8103177502107,21.2528134491734,-25.2748188970151));
#30046=CARTESIAN_POINT('Ctrl Pts',(-25.8064650454706,21.2490278592123,-25.2744841413567));
#30047=CARTESIAN_POINT('Ctrl Pts',(-25.8039555277778,21.2465701086411,-25.2742667680802));
#30048=CARTESIAN_POINT('Ctrl Pts',(-25.7931318544871,21.2360043231496,-25.2733321011948));
#30049=CARTESIAN_POINT('Ctrl Pts',(-25.7847777897391,21.22793702595,-25.2726179802339));
#30050=CARTESIAN_POINT('Ctrl Pts',(-25.6405526593777,21.090161476115,-25.2604099510848));
#30051=CARTESIAN_POINT('Ctrl Pts',(-25.49361760892,20.9725098359525,-25.2497899061814));
#30052=CARTESIAN_POINT('Ctrl Pts',(-25.2622466463587,20.8183454987195,-25.2342159687254));
#30053=CARTESIAN_POINT('Ctrl Pts',(-25.1851835457418,20.7715405176478,-25.2291984533894));
#30054=CARTESIAN_POINT('Ctrl Pts',(-25.0162539603779,20.678402767604,-25.2183763682211));
#30055=CARTESIAN_POINT('Ctrl Pts',(-24.9239294038489,20.6331150134832,-25.2125658290094));
#30056=CARTESIAN_POINT('Ctrl Pts',(-24.7538664296068,20.5595602659388,-25.2018725575941));
#30057=CARTESIAN_POINT('Ctrl Pts',(-24.6769047411481,20.5297261173178,-25.1970372714229));
#30058=CARTESIAN_POINT('Ctrl Pts',(-24.5587347299776,20.4890625084898,-25.1895663204952));
#30059=CARTESIAN_POINT('Ctrl Pts',(-24.5183145227767,20.4760410195271,-25.1870030473364));
#30060=CARTESIAN_POINT('Ctrl Pts',(-24.4703397101177,20.4616257468752,-25.1839476773876));
#30061=CARTESIAN_POINT('Ctrl Pts',(-24.4630214341635,20.4594551004631,-25.1834812468426));
#30062=CARTESIAN_POINT('Ctrl Pts',(-24.4517983873074,20.4561696106459,-25.182765383559));
#30063=CARTESIAN_POINT('Ctrl Pts',(-24.4478990713153,20.4550361027895,-25.1825165615587));
#30064=CARTESIAN_POINT('Ctrl Pts',(-24.4410963574338,20.4530725305681,-25.1820822842363));
#30065=CARTESIAN_POINT('Ctrl Pts',(-24.4381939095448,20.4522391697741,-25.1818969368485));
#30066=CARTESIAN_POINT('Ctrl Pts',(-24.432123918381,20.4505055640145,-25.1815091892792));
#30067=CARTESIAN_POINT('Ctrl Pts',(-24.4289561594791,20.4496060925323,-25.1813067640991));
#30068=CARTESIAN_POINT('Ctrl Pts',(-24.4201940160148,20.447132625693,-25.1807466502201));
#30069=CARTESIAN_POINT('Ctrl Pts',(-24.414596764343,20.4455689111071,-25.1803886268379));
#30070=CARTESIAN_POINT('Ctrl Pts',(-24.3926270071581,20.4394951954414,-25.1789824537228));
#30071=CARTESIAN_POINT('Ctrl Pts',(-24.3762234175929,20.4350995595521,-25.1779305905217));
#30072=CARTESIAN_POINT('Ctrl Pts',(-24.1014736756122,20.3637980891094,-25.1602778818559));
#30073=CARTESIAN_POINT('Ctrl Pts',(-23.8358927386007,20.3291214756929,-25.1425701657684));
#30074=CARTESIAN_POINT('Ctrl Pts',(-23.4267889288459,20.3267234742127,-25.1148939772119));
#30075=CARTESIAN_POINT('Ctrl Pts',(-23.2845310373082,20.3353220345913,-25.1052250138841));
#30076=CARTESIAN_POINT('Ctrl Pts',(-23.0537308282695,20.3647012457331,-25.0898361327789));
#30077=CARTESIAN_POINT('Ctrl Pts',(-22.9646668409626,20.3798639494307,-25.0839740286218));
#30078=CARTESIAN_POINT('Ctrl Pts',(-22.8703647349686,20.4000291128422,-25.0779301917035));
#30079=CARTESIAN_POINT('Ctrl Pts',(-22.8643845959251,20.4013257016508,-25.077547634101));
#30080=CARTESIAN_POINT('Ctrl Pts',(-22.8563549101249,20.4030906240935,-25.0770349530157));
#30081=CARTESIAN_POINT('Ctrl Pts',(-22.8543021274838,20.4035439311385,-25.0769039734312));
#30082=CARTESIAN_POINT('Ctrl Pts',(-22.8502524039958,20.4044423706066,-25.0766457508542));
#30083=CARTESIAN_POINT('Ctrl Pts',(-22.8482554408431,20.4048873966308,-25.0765185017903));
#30084=CARTESIAN_POINT('Ctrl Pts',(-22.8444162806151,20.4057467971586,-25.0762740276297));
#30085=CARTESIAN_POINT('Ctrl Pts',(-22.8425740291365,20.4061608878491,-25.076156786799));
#30086=CARTESIAN_POINT('Ctrl Pts',(-22.8383302133378,20.4071187072685,-25.0758868747397));
#30087=CARTESIAN_POINT('Ctrl Pts',(-22.8359289013411,20.4076635708469,-25.0757342694022));
#30088=CARTESIAN_POINT('Ctrl Pts',(-22.8295079310855,20.4091282446274,-25.075326529862));
#30089=CARTESIAN_POINT('Ctrl Pts',(-22.8254893928949,20.4100530222373,-25.0750716816159));
#30090=CARTESIAN_POINT('Ctrl Pts',(-22.7977834246291,20.4164849546489,-25.0733168548771));
#30091=CARTESIAN_POINT('Ctrl Pts',(-22.77415638964,20.422252556085,-25.071831649577));
#30092=CARTESIAN_POINT('Ctrl Pts',(-22.7484894056022,20.4288268668199,-25.0702282693014));
#30093=CARTESIAN_POINT('Ctrl Pts',(-22.746383285551,20.4293685981214,-25.070096776972));
#30094=CARTESIAN_POINT('Ctrl Pts',(-22.7382730603912,20.4314634458349,-25.0695907071709));
#30095=CARTESIAN_POINT('Ctrl Pts',(-22.7322728484797,20.4330317722651,-25.0692168903105));
#30096=CARTESIAN_POINT('Ctrl Pts',(-22.5844514960315,20.4721252959915,-25.0600212488412));
#30097=CARTESIAN_POINT('Ctrl Pts',(-22.4453345871329,20.5192781823821,-25.0516745944945));
#30098=CARTESIAN_POINT('Ctrl Pts',(-22.1582736097082,20.6389811651494,-25.0342009114188));
#30099=CARTESIAN_POINT('Ctrl Pts',(-22.0117053170849,20.7137091718695,-25.0251191020992));
#30100=CARTESIAN_POINT('Ctrl Pts',(-21.7695005183071,20.8615147519106,-25.0089992574562));
#30101=CARTESIAN_POINT('Ctrl Pts',(-21.6710754504718,20.9293599697798,-25.0020956390491));
#30102=CARTESIAN_POINT('Ctrl Pts',(-21.5497127840613,21.0233731794041,-24.992959904933));
#30103=CARTESIAN_POINT('Ctrl Pts',(-21.523109659365,21.0446647392237,-24.9909165609518));
#30104=CARTESIAN_POINT('Ctrl Pts',(-21.4806407506145,21.0797734422604,-24.9875848521638));
#30105=CARTESIAN_POINT('Ctrl Pts',(-21.464563511104,21.0933314640759,-24.9863069476716));
#30106=CARTESIAN_POINT('Ctrl Pts',(-21.445220533953,21.1099701785289,-24.9847486842183));
#30107=CARTESIAN_POINT('Ctrl Pts',(-21.441826778509,21.1129018146924,-24.9844744992205));
#30108=CARTESIAN_POINT('Ctrl Pts',(-21.4352760529614,21.1185844639965,-24.983943732195));
#30109=CARTESIAN_POINT('Ctrl Pts',(-21.4321183020021,21.1213345664682,-24.9836871882893));
#30110=CARTESIAN_POINT('Ctrl Pts',(-21.4266811764424,21.126088454664,-24.9832442661499));
#30111=CARTESIAN_POINT('Ctrl Pts',(-21.4243992504586,21.1280893250199,-24.9830580097833));
#30112=CARTESIAN_POINT('Ctrl Pts',(-21.4196911427847,21.1322293322858,-24.9826729660928));
#30113=CARTESIAN_POINT('Ctrl Pts',(-21.4172653490884,21.1343689038037,-24.9824741606752));
#30114=CARTESIAN_POINT('Ctrl Pts',(-21.4107097925491,21.140168532973,-24.9819357701278));
#30115=CARTESIAN_POINT('Ctrl Pts',(-21.4065862163756,21.1438355392585,-24.9815958932823));
#30116=CARTESIAN_POINT('Ctrl Pts',(-21.3913082819028,21.1574923046487,-24.9803320893177));
#30117=CARTESIAN_POINT('Ctrl Pts',(-21.3802143044725,21.1675490549554,-24.9794053356684));
#30118=CARTESIAN_POINT('Ctrl Pts',(-21.1902825530019,21.3421499556484,-24.9633806528413));
#30119=CARTESIAN_POINT('Ctrl Pts',(-21.0305897911249,21.5262891007911,-24.9473779817701));
#30120=CARTESIAN_POINT('Ctrl Pts',(-20.7889154821981,21.8784123272978,-24.9185566004384));
#30121=CARTESIAN_POINT('Ctrl Pts',(-20.6979079543708,22.0389063857813,-24.9059825873275));
#30122=CARTESIAN_POINT('Ctrl Pts',(-20.5993018170917,22.2538186249941,-24.8904472403405));
#30123=CARTESIAN_POINT('Ctrl Pts',(-20.5786572175354,22.3018643835983,-24.8870542862236));
#30124=CARTESIAN_POINT('Ctrl Pts',(-20.5496435745144,22.3741909401787,-24.88208666226));
#30125=CARTESIAN_POINT('Ctrl Pts',(-20.540381470176,22.3981018144832,-24.8804667693281));
#30126=CARTESIAN_POINT('Ctrl Pts',(-20.5298946739763,22.4261641905469,-24.8785937825932));
#30127=CARTESIAN_POINT('Ctrl Pts',(-20.5283920803275,22.4302098537728,-24.8783244397983));
#30128=CARTESIAN_POINT('Ctrl Pts',(-20.5261036578797,22.4364094510798,-24.8779127509367));
#30129=CARTESIAN_POINT('Ctrl Pts',(-20.5253120008632,22.4385612057224,-24.877770056116));
#30130=CARTESIAN_POINT('Ctrl Pts',(-20.5239424562059,22.4422959759785,-24.8775227215581));
#30131=CARTESIAN_POINT('Ctrl Pts',(-20.523363515203,22.4438785966043,-24.8774180183248));
#30132=CARTESIAN_POINT('Ctrl Pts',(-20.5221550884941,22.4471900574534,-24.8771991593359));
#30133=CARTESIAN_POINT('Ctrl Pts',(-20.5215258436894,22.4489189777687,-24.8770850183594));
#30134=CARTESIAN_POINT('Ctrl Pts',(-20.5199783451464,22.4531822591119,-24.8768038699544));
#30135=CARTESIAN_POINT('Ctrl Pts',(-20.5190617877949,22.4557172408671,-24.8766369646318));
#30136=CARTESIAN_POINT('Ctrl Pts',(-20.5154912957184,22.4656312629952,-24.8759852525025));
#30137=CARTESIAN_POINT('Ctrl Pts',(-20.5128610878374,22.4730189099971,-24.8755018556955));
#30138=CARTESIAN_POINT('Ctrl Pts',(-20.464922702181,22.609238283189,-24.8666285242348));
#30139=CARTESIAN_POINT('Ctrl Pts',(-20.4278152121157,22.7408307611289,-24.8587112864988));
#30140=CARTESIAN_POINT('Ctrl Pts',(-20.3608247917679,23.0531649242651,-24.8405838914187));
#30141=CARTESIAN_POINT('Ctrl Pts',(-20.3377637587829,23.2348726545533,-24.8305242899372));
#30142=CARTESIAN_POINT('Ctrl Pts',(-20.3246922209086,23.5520743529381,-24.8125820225287));
#30143=CARTESIAN_POINT('Ctrl Pts',(-20.3275837454163,23.6867915274818,-24.8048470393509));
#30144=CARTESIAN_POINT('Ctrl Pts',(-20.3435642375,23.8763907146123,-24.7935457820398));
#30145=CARTESIAN_POINT('Ctrl Pts',(-20.3496752336241,23.9317237731833,-24.7901982811708));
#30146=CARTESIAN_POINT('Ctrl Pts',(-20.3583145021751,23.9949040326001,-24.7863105455624));
#30147=CARTESIAN_POINT('Ctrl Pts',(-20.3594436192301,24.0029354491905,-24.7858151272651));
#30148=CARTESIAN_POINT('Ctrl Pts',(-20.3612030984382,24.0151169144062,-24.7850618431574));
#30149=CARTESIAN_POINT('Ctrl Pts',(-20.3618112775774,24.0192701761881,-24.7848046812701));
#30150=CARTESIAN_POINT('Ctrl Pts',(-20.3628733623185,24.0264256223609,-24.7843610565323));
#30151=CARTESIAN_POINT('Ctrl Pts',(-20.3633234007789,24.0294283825726,-24.7841747166687));
#30152=CARTESIAN_POINT('Ctrl Pts',(-20.3642610108956,24.0356245825048,-24.7837898427399));
#30153=CARTESIAN_POINT('Ctrl Pts',(-20.3647491418694,24.038817933248,-24.7835912910878));
#30154=CARTESIAN_POINT('Ctrl Pts',(-20.3659392769527,24.0465261813377,-24.7831115372972));
#30155=CARTESIAN_POINT('Ctrl Pts',(-20.3666460815882,24.0510403212438,-24.7828301828225));
#30156=CARTESIAN_POINT('Ctrl Pts',(-20.3692875461222,24.0676789213714,-24.7817916611449));
#30157=CARTESIAN_POINT('Ctrl Pts',(-20.3712818692017,24.0797936806887,-24.7810325986286));
#30158=CARTESIAN_POINT('Ctrl Pts',(-20.4046183674197,24.2753223754761,-24.7687338081732));
#30159=CARTESIAN_POINT('Ctrl Pts',(-20.4517119208864,24.4556611035921,-24.7566792777236));
#30160=CARTESIAN_POINT('Ctrl Pts',(-20.5759333105863,24.8046694572859,-24.7319714021758));
#30161=CARTESIAN_POINT('Ctrl Pts',(-20.6525832623123,24.972801138048,-24.7193716503923));
#30162=CARTESIAN_POINT('Ctrl Pts',(-20.7759911050168,25.1916088990411,-24.7025156064405));
#30163=CARTESIAN_POINT('Ctrl Pts',(-20.8105990912414,25.2487451401518,-24.6980709847025));
#30164=CARTESIAN_POINT('Ctrl Pts',(-20.8812051224731,25.3575323700152,-24.6895770141447));
#30165=CARTESIAN_POINT('Ctrl Pts',(-20.9169914727159,25.4092877555646,-24.6855214791563));
#30166=CARTESIAN_POINT('Ctrl Pts',(-20.9604302225336,25.468336456842,-24.6809074436844));
#30167=CARTESIAN_POINT('Ctrl Pts',(-20.9666282369265,25.4766769520849,-24.6802560372837));
#30168=CARTESIAN_POINT('Ctrl Pts',(-20.9748071527373,25.4875726165946,-24.6794056436001));
#30169=CARTESIAN_POINT('Ctrl Pts',(-20.9767516202334,25.4901548669365,-24.6792041446733));
#30170=CARTESIAN_POINT('Ctrl Pts',(-20.9799357772215,25.4943702102052,-24.6788752875817));
#30171=CARTESIAN_POINT('Ctrl Pts',(-20.9811731398142,25.4960050453752,-24.6787477657336));
#30172=CARTESIAN_POINT('Ctrl Pts',(-20.9835521528349,25.4991420327842,-24.6785031094168));
#30173=CARTESIAN_POINT('Ctrl Pts',(-20.9846935589217,25.5006443588757,-24.6783859586087));
#30174=CARTESIAN_POINT('Ctrl Pts',(-20.9873218890374,25.5040974845918,-24.6781167223467));
#30175=CARTESIAN_POINT('Ctrl Pts',(-20.9888097250308,25.5060475944042,-24.6779647017149));
#30176=CARTESIAN_POINT('Ctrl Pts',(-20.9935411057226,25.5122343655977,-24.6774824922253));
#30177=CARTESIAN_POINT('Ctrl Pts',(-20.9967929678628,25.5164646995712,-24.6771528902814));
#30178=CARTESIAN_POINT('Ctrl Pts',(-21.0246578149761,25.5525282463149,-24.6743438678715));
#30179=CARTESIAN_POINT('Ctrl Pts',(-21.0498558660914,25.5839077607909,-24.671905224204));
#30180=CARTESIAN_POINT('Ctrl Pts',(-21.0799522337295,25.6199818344024,-24.6690973586096));
#30181=CARTESIAN_POINT('Ctrl Pts',(-21.0842842821854,25.6251413341401,-24.6686956564226));
#30182=CARTESIAN_POINT('Ctrl Pts',(-21.0895053122892,25.6313201695628,-24.6682144109145));
#30183=CARTESIAN_POINT('Ctrl Pts',(-21.090378763121,25.6323525374314,-24.6681339976959));
#30184=CARTESIAN_POINT('Ctrl Pts',(-21.0950344255599,25.6378482397424,-24.6677058919929));
#30185=CARTESIAN_POINT('Ctrl Pts',(-21.098828159937,25.6423018474209,-24.6673588428888));
#30186=CARTESIAN_POINT('Ctrl Pts',(-21.1049678416876,25.6494698186711,-24.666800034592));
#30187=CARTESIAN_POINT('Ctrl Pts',(-21.1073062145871,25.6521906195225,-24.6665878671274));
#30188=CARTESIAN_POINT('Ctrl Pts',(-21.113142139006,25.6589580835634,-24.6660599847067));
#30189=CARTESIAN_POINT('Ctrl Pts',(-21.1166452415063,25.6629999677221,-24.6657445653324));
#30190=CARTESIAN_POINT('Ctrl Pts',(-21.1438216464234,25.6941988655711,-24.6633086188658));
#30191=CARTESIAN_POINT('Ctrl Pts',(-21.1679395541954,25.720966824405,-24.6612112363208));
#30192=CARTESIAN_POINT('Ctrl Pts',(-21.3509471070143,25.9173581750506,-24.6457183651113));
#30193=CARTESIAN_POINT('Ctrl Pts',(-21.5273273903961,26.0697606774814,-24.6330541793684));
#30194=CARTESIAN_POINT('Ctrl Pts',(-21.8239570215381,26.2746653433132,-24.6126352561625));
#30195=CARTESIAN_POINT('Ctrl Pts',(-21.9335721904794,26.3411056280582,-24.6052582349024));
#30196=CARTESIAN_POINT('Ctrl Pts',(-22.0562160936962,26.4057883835446,-24.5970160069381));
#30197=CARTESIAN_POINT('Ctrl Pts',(-22.0656142246213,26.410685883649,-24.5963845258621));
#30198=CARTESIAN_POINT('Ctrl Pts',(-22.0750360162151,26.4155367750037,-24.595751509546));
#30199=CARTESIAN_POINT('Origin',(-23.5502525316942,23.5502525316942,-77.3107734492734));
#30200=CARTESIAN_POINT('',(-22.0750360144199,26.4155367740794,-23.0992549867839));
#30201=CARTESIAN_POINT('',(-22.0750361484425,26.4155368430821,-23.3437344129902));
#30202=CARTESIAN_POINT('',(-22.0750360153461,26.4155367745563,-77.3107734492734));
#30203=CARTESIAN_POINT('',(-26.7730011959272,23.5473183053636,-23.9397396857875));
#30204=CARTESIAN_POINT('Ctrl Pts',(-22.0750360144199,26.4155367740794,-23.0992549867839));
#30205=CARTESIAN_POINT('Ctrl Pts',(-22.0526720052502,26.4040224694141,-23.1008603458253));
#30206=CARTESIAN_POINT('Ctrl Pts',(-22.0304419422344,26.3922458895206,-23.1024518991583));
#30207=CARTESIAN_POINT('Ctrl Pts',(-22.0032929933772,26.3774537839156,-23.1043883274086));
#30208=CARTESIAN_POINT('Ctrl Pts',(-21.9982428631065,26.3746846380804,-23.1047482203538));
#30209=CARTESIAN_POINT('Ctrl Pts',(-21.9911837266924,26.3707892408664,-23.1052508151255));
#30210=CARTESIAN_POINT('Ctrl Pts',(-21.9891685018808,26.3696743728632,-23.1053942410843));
#30211=CARTESIAN_POINT('Ctrl Pts',(-21.9854852714282,26.3676315667143,-23.1056562805497));
#30212=CARTESIAN_POINT('Ctrl Pts',(-21.9838168929055,26.3667043057108,-23.1057749377895));
#30213=CARTESIAN_POINT('Ctrl Pts',(-21.9804318188111,26.3648189915202,-23.1060156104344));
#30214=CARTESIAN_POINT('Ctrl Pts',(-21.9787151754853,26.3638608494001,-23.1061376198625));
#30215=CARTESIAN_POINT('Ctrl Pts',(-21.9745064460719,26.3615066993986,-23.1064366553964));
#30216=CARTESIAN_POINT('Ctrl Pts',(-21.9720153311895,26.3601089445529,-23.1066135683252));
#30217=CARTESIAN_POINT('Ctrl Pts',(-21.9629028630669,26.3549800328295,-23.1072604185072));
#30218=CARTESIAN_POINT('Ctrl Pts',(-21.9562927882141,26.3512287302806,-23.1077290646005));
#30219=CARTESIAN_POINT('Ctrl Pts',(-21.8041224907108,26.2641570021886,-23.1185060047682));
#30220=CARTESIAN_POINT('Ctrl Pts',(-21.6652493783781,26.1696090175664,-23.1280982957044));
#30221=CARTESIAN_POINT('Ctrl Pts',(-21.3790799817679,25.9401759256473,-23.1487362799999));
#30222=CARTESIAN_POINT('Ctrl Pts',(-21.235677483171,25.8015777694774,-23.1596934586764));
#30223=CARTESIAN_POINT('Ctrl Pts',(-21.0702570794957,25.6090734412315,-23.1742394009387));
#30224=CARTESIAN_POINT('Ctrl Pts',(-21.0356070445344,25.566605336247,-23.1774093606516));
#30225=CARTESIAN_POINT('Ctrl Pts',(-20.9891845055225,25.5066498009376,-23.1818481530357));
#30226=CARTESIAN_POINT('Ctrl Pts',(-20.9764744656409,25.4898984139694,-23.1830845046559));
#30227=CARTESIAN_POINT('Ctrl Pts',(-20.956437147721,25.4629461860943,-23.1850685601107));
#30228=CARTESIAN_POINT('Ctrl Pts',(-20.9490038800524,25.4528246611588,-23.1858124946643));
#30229=CARTESIAN_POINT('Ctrl Pts',(-20.9098721462823,25.398882832957,-23.1897717415704));
#30230=CARTESIAN_POINT('Ctrl Pts',(-20.8792228444592,25.3543152930603,-23.1930240305316));
#30231=CARTESIAN_POINT('Ctrl Pts',(-20.8449141634396,25.3016345935273,-23.1968550702407));
#30232=CARTESIAN_POINT('Ctrl Pts',(-20.840147809869,25.2942500109331,-23.1973917880099));
#30233=CARTESIAN_POINT('Ctrl Pts',(-20.8330949964117,25.2832242498736,-23.1981927353129));
#30234=CARTESIAN_POINT('Ctrl Pts',(-20.8307854908379,25.2795978011429,-23.1984561059475));
#30235=CARTESIAN_POINT('Ctrl Pts',(-20.8266819636738,25.273125782778,-23.1989260223214));
#30236=CARTESIAN_POINT('Ctrl Pts',(-20.8248851241249,25.2702820000202,-23.1991324630038));
#30237=CARTESIAN_POINT('Ctrl Pts',(-20.8211090458313,25.2642849865661,-23.199567728883));
#30238=CARTESIAN_POINT('Ctrl Pts',(-20.8191308132183,25.2611311309716,-23.1997965909635));
#30239=CARTESIAN_POINT('Ctrl Pts',(-20.8139263454462,25.2528017262641,-23.2004009035254));
#30240=CARTESIAN_POINT('Ctrl Pts',(-20.810709340469,25.2476204529389,-23.2007766944757));
#30241=CARTESIAN_POINT('Ctrl Pts',(-20.7965075665723,25.2246016803702,-23.2024457171014));
#30242=CARTESIAN_POINT('Ctrl Pts',(-20.7856823631863,25.206666777778,-23.2037448036639));
#30243=CARTESIAN_POINT('Ctrl Pts',(-20.7085360894879,25.0759898615199,-23.2132023369311));
#30244=CARTESIAN_POINT('Ctrl Pts',(-20.6489669286855,24.9594227849635,-23.2216043350849));
#30245=CARTESIAN_POINT('Ctrl Pts',(-20.5061810561957,24.6323255162996,-23.2450942772063));
#30246=CARTESIAN_POINT('Ctrl Pts',(-20.4377823232886,24.4161423954807,-23.2605675407608));
#30247=CARTESIAN_POINT('Ctrl Pts',(-20.3820984467936,24.1432649662729,-23.2792669845356));
#30248=CARTESIAN_POINT('Ctrl Pts',(-20.3728737988561,24.0916662810255,-23.2827643168317));
#30249=CARTESIAN_POINT('Ctrl Pts',(-20.3519589038958,23.955596953829,-23.291851815795));
#30250=CARTESIAN_POINT('Ctrl Pts',(-20.3423540112512,23.8708400634492,-23.2973770419077));
#30251=CARTESIAN_POINT('Ctrl Pts',(-20.3356585118087,23.7794751077061,-23.3031195551253));
#30252=CARTESIAN_POINT('Ctrl Pts',(-20.3352140922839,23.7731550592039,-23.3035156891557));
#30253=CARTESIAN_POINT('Ctrl Pts',(-20.3346226657071,23.7643744657246,-23.304064485965));
#30254=CARTESIAN_POINT('Ctrl Pts',(-20.3344598433802,23.7619150544676,-23.3042180317759));
#30255=CARTESIAN_POINT('Ctrl Pts',(-20.3341845214919,23.7576826939507,-23.3044819707126));
#30256=CARTESIAN_POINT('Ctrl Pts',(-20.3340706664254,23.7559098389113,-23.3045924404842));
#30257=CARTESIAN_POINT('Ctrl Pts',(-20.3338382123986,23.7522428554611,-23.3048207510061));
#30258=CARTESIAN_POINT('Ctrl Pts',(-20.3337198208707,23.7503487197704,-23.3049385793195));
#30259=CARTESIAN_POINT('Ctrl Pts',(-20.3334880305208,23.7465869590227,-23.3051723845295));
#30260=CARTESIAN_POINT('Ctrl Pts',(-20.3333745847555,23.7447193358178,-23.3052883642054));
#30261=CARTESIAN_POINT('Ctrl Pts',(-20.3329978407276,23.7384265658923,-23.3056788159374));
#30262=CARTESIAN_POINT('Ctrl Pts',(-20.3327420447994,23.7340009493014,-23.3059528650489));
#30263=CARTESIAN_POINT('Ctrl Pts',(-20.330912618885,23.701173745058,-23.3079816498569));
#30264=CARTESIAN_POINT('Ctrl Pts',(-20.3297058779552,23.6727518077291,-23.3097160531707));
#30265=CARTESIAN_POINT('Ctrl Pts',(-20.3269511859043,23.5784127480245,-23.3154105682177));
#30266=CARTESIAN_POINT('Ctrl Pts',(-20.327049529715,23.5124606501146,-23.3192907359446));
#30267=CARTESIAN_POINT('Ctrl Pts',(-20.3352371621147,23.2581378676011,-23.334021231277));
#30268=CARTESIAN_POINT('Ctrl Pts',(-20.3578234590084,23.0706055463776,-23.3444091301467));
#30269=CARTESIAN_POINT('Ctrl Pts',(-20.4279196131496,22.7377635052762,-23.3634774543496));
#30270=CARTESIAN_POINT('Ctrl Pts',(-20.4695876885442,22.5918167582764,-23.3720671587884));
#30271=CARTESIAN_POINT('Ctrl Pts',(-20.5241750661265,22.4416316695437,-23.3814550155393));
#30272=CARTESIAN_POINT('Ctrl Pts',(-20.5270107178045,22.433921945941,-23.3819384688577));
#30273=CARTESIAN_POINT('Ctrl Pts',(-20.5543047109259,22.3605803176069,-23.3865524052256));
#30274=CARTESIAN_POINT('Ctrl Pts',(-20.5808655039735,22.2957554736422,-23.3907450756816));
#30275=CARTESIAN_POINT('Ctrl Pts',(-20.613344061928,22.2233110149212,-23.3955805924083));
#30276=CARTESIAN_POINT('Ctrl Pts',(-20.6172098019913,22.2147880089344,-23.3961518718639));
#30277=CARTESIAN_POINT('Ctrl Pts',(-20.6229604040299,22.202254758996,-23.3969955157115));
#30278=CARTESIAN_POINT('Ctrl Pts',(-20.6248165247868,22.1982313169702,-23.3972668870566));
#30279=CARTESIAN_POINT('Ctrl Pts',(-20.6281087067295,22.1911334998293,-23.39774658335));
#30280=CARTESIAN_POINT('Ctrl Pts',(-20.6295413398934,22.188057534454,-23.3979547893603));
#30281=CARTESIAN_POINT('Ctrl Pts',(-20.6325149081688,22.1816993283513,-23.3983858310079));
#30282=CARTESIAN_POINT('Ctrl Pts',(-20.6340565293918,22.1784174154723,-23.3986086902226));
#30283=CARTESIAN_POINT('Ctrl Pts',(-20.6380205131122,22.1700154814129,-23.3991801748325));
#30284=CARTESIAN_POINT('Ctrl Pts',(-20.6404508334848,22.1648992477027,-23.3995290764575));
#30285=CARTESIAN_POINT('Ctrl Pts',(-20.6502732736223,22.144361234189,-23.4009333280311));
#30286=CARTESIAN_POINT('Ctrl Pts',(-20.6577745040162,22.1289922181322,-23.401992475539));
#30287=CARTESIAN_POINT('Ctrl Pts',(-20.7004942582236,22.0432042588119,-23.4079520153094));
#30288=CARTESIAN_POINT('Ctrl Pts',(-20.7381591809437,21.9740399989937,-23.4129381228677));
#30289=CARTESIAN_POINT('Ctrl Pts',(-20.8172861502717,21.8406184110363,-23.4229307101639));
#30290=CARTESIAN_POINT('Ctrl Pts',(-20.8585779155171,21.7763189272092,-23.4279289919953));
#30291=CARTESIAN_POINT('Ctrl Pts',(-21.0025744920654,21.5687059696429,-23.4446634374616));
#30292=CARTESIAN_POINT('Ctrl Pts',(-21.1147460351111,21.4323548253059,-23.4566555367521));
#30293=CARTESIAN_POINT('Ctrl Pts',(-21.3513725353846,21.188519213391,-23.4795925760803));
#30294=CARTESIAN_POINT('Ctrl Pts',(-21.4740362523306,21.0799898051002,-23.4905119516601));
#30295=CARTESIAN_POINT('Ctrl Pts',(-21.6120169235371,20.9754805025922,-23.5013991362776));
#30296=CARTESIAN_POINT('Ctrl Pts',(-21.619634798213,20.9697635378817,-23.5019959719635));
#30297=CARTESIAN_POINT('Ctrl Pts',(-21.6298830023823,20.962143381919,-23.502793088914));
#30298=CARTESIAN_POINT('Ctrl Pts',(-21.6324909246131,20.9602103469244,-23.502995435553));
#30299=CARTESIAN_POINT('Ctrl Pts',(-21.636577585143,20.9571908030581,-23.503311727895));
#30300=CARTESIAN_POINT('Ctrl Pts',(-21.6380543290206,20.9561016179446,-23.5034258616197));
#30301=CARTESIAN_POINT('Ctrl Pts',(-21.6408898541461,20.9540139888709,-23.5036447024369));
#30302=CARTESIAN_POINT('Ctrl Pts',(-21.6422484799371,20.9530153565119,-23.5037494224437));
#30303=CARTESIAN_POINT('Ctrl Pts',(-21.6454640087084,20.9506557272755,-23.5039969471388));
#30304=CARTESIAN_POINT('Ctrl Pts',(-21.647321584708,20.9492956550959,-23.5041396864265));
#30305=CARTESIAN_POINT('Ctrl Pts',(-21.6527015468777,20.9453654256284,-23.50455236521));
#30306=CARTESIAN_POINT('Ctrl Pts',(-21.6562277113733,20.9428004121212,-23.5048219454728));
#30307=CARTESIAN_POINT('Ctrl Pts',(-21.6813580722248,20.9245978832095,-23.5067368871061));
#30308=CARTESIAN_POINT('Ctrl Pts',(-21.7031512656833,20.909221320502,-23.5083644142925));
#30309=CARTESIAN_POINT('Ctrl Pts',(-21.7406046323372,20.8834858746942,-23.5111101663504));
#30310=CARTESIAN_POINT('Ctrl Pts',(-21.7561685422695,20.8729903862415,-23.5122363947064));
#30311=CARTESIAN_POINT('Ctrl Pts',(-21.8399782720328,20.8175325562861,-23.5182274075555));
#30312=CARTESIAN_POINT('Ctrl Pts',(-21.9098290128302,20.7750391717824,-23.5229619072411));
#30313=CARTESIAN_POINT('Ctrl Pts',(-22.0940734020842,20.6723451183414,-23.5349951245099));
#30314=CARTESIAN_POINT('Ctrl Pts',(-22.2106064329151,20.6162860039805,-23.5421785095639));
#30315=CARTESIAN_POINT('Ctrl Pts',(-22.5588791986188,20.4738353558232,-23.5632159096264));
#30316=CARTESIAN_POINT('Ctrl Pts',(-22.7975225493418,20.4069205050357,-23.5771737610186));
#30317=CARTESIAN_POINT('Ctrl Pts',(-23.0432947225784,20.3676254979143,-23.5922640621125));
#30318=CARTESIAN_POINT('Ctrl Pts',(-23.0451407231895,20.3673319990299,-23.5923774403421));
#30319=CARTESIAN_POINT('Ctrl Pts',(-23.0615135198418,20.364743461565,-23.5933833390404));
#30320=CARTESIAN_POINT('Ctrl Pts',(-23.076055423014,20.3625463111515,-23.59427891268));
#30321=CARTESIAN_POINT('Ctrl Pts',(-23.0960326882598,20.3596676489539,-23.595512349508));
#30322=CARTESIAN_POINT('Ctrl Pts',(-23.101455662634,20.3589003214428,-23.59584749003));
#30323=CARTESIAN_POINT('Ctrl Pts',(-23.110076159562,20.3577029654525,-23.5963807472094));
#30324=CARTESIAN_POINT('Ctrl Pts',(-23.1132724342129,20.3572639056925,-23.5965785774332));
#30325=CARTESIAN_POINT('Ctrl Pts',(-23.1194792363821,20.3564207958164,-23.5969629591715));
#30326=CARTESIAN_POINT('Ctrl Pts',(-23.122489687642,20.356016200706,-23.5971494932159));
#30327=CARTESIAN_POINT('Ctrl Pts',(-23.1296713298563,20.3550613454243,-23.5975947225523));
#30328=CARTESIAN_POINT('Ctrl Pts',(-23.1338430272395,20.3545149973389,-23.5978535413942));
#30329=CARTESIAN_POINT('Ctrl Pts',(-23.1424909710813,20.3533996366139,-23.5983904772561));
#30330=CARTESIAN_POINT('Ctrl Pts',(-23.146967364325,20.3528318529995,-23.5986686326294));
#30331=CARTESIAN_POINT('Ctrl Pts',(-23.1727640578846,20.3496148469964,-23.6002728994812));
#30332=CARTESIAN_POINT('Ctrl Pts',(-23.1941088221092,20.3471695232961,-23.6016054439138));
#30333=CARTESIAN_POINT('Ctrl Pts',(-23.331948350839,20.3327729852343,-23.6102453931805));
#30334=CARTESIAN_POINT('Ctrl Pts',(-23.4489834350858,20.3269668961474,-23.6177457480732));
#30335=CARTESIAN_POINT('Ctrl Pts',(-23.5918469541447,20.3276678158969,-23.6271060223113));
#30336=CARTESIAN_POINT('Ctrl Pts',(-23.6176271013464,20.3281037201314,-23.6288030111484));
#30337=CARTESIAN_POINT('Ctrl Pts',(-23.7992293307109,20.3333547118536,-23.6408102743609));
#30338=CARTESIAN_POINT('Ctrl Pts',(-23.9545180558525,20.349161448779,-23.6513683593087));
#30339=CARTESIAN_POINT('Ctrl Pts',(-24.2933576937108,20.408705929475,-23.6746481218824));
#30340=CARTESIAN_POINT('Ctrl Pts',(-24.4754912276071,20.4574428319542,-23.6873247070297));
#30341=CARTESIAN_POINT('Ctrl Pts',(-24.6632907085622,20.5257857751049,-23.6999206682697));
#30342=CARTESIAN_POINT('Ctrl Pts',(-24.6742112107683,20.5298270579421,-23.700651282035));
#30343=CARTESIAN_POINT('Ctrl Pts',(-24.6884006392453,20.5351656655093,-23.701597973782));
#30344=CARTESIAN_POINT('Ctrl Pts',(-24.6916895019339,20.5364092098517,-23.7018172164006));
#30345=CARTESIAN_POINT('Ctrl Pts',(-24.6967425088693,20.5383292483968,-23.7021537701781));
#30346=CARTESIAN_POINT('Ctrl Pts',(-24.6985080910102,20.5390019106441,-23.7022713115765));
#30347=CARTESIAN_POINT('Ctrl Pts',(-24.7020150150549,20.5403415327603,-23.7025046706367));
#30348=CARTESIAN_POINT('Ctrl Pts',(-24.7037563597892,20.5410084475123,-23.7026204896939));
#30349=CARTESIAN_POINT('Ctrl Pts',(-24.7076351717219,20.5424978488391,-23.7028783543432));
#30350=CARTESIAN_POINT('Ctrl Pts',(-24.7097723364268,20.5433211007856,-23.7030203526736));
#30351=CARTESIAN_POINT('Ctrl Pts',(-24.7141909275168,20.5450285866354,-23.7033137702766));
#30352=CARTESIAN_POINT('Ctrl Pts',(-24.7164722291671,20.54591314232,-23.7034651700428));
#30353=CARTESIAN_POINT('Ctrl Pts',(-24.7288682872509,20.5507358572257,-23.7042873594953));
#30354=CARTESIAN_POINT('Ctrl Pts',(-24.7389642676682,20.5547225624952,-23.7049552490516));
#30355=CARTESIAN_POINT('Ctrl Pts',(-24.7652369262736,20.5652508651911,-23.7066892161213));
#30356=CARTESIAN_POINT('Ctrl Pts',(-24.7813811958475,20.5718730610906,-23.7077506745688));
#30357=CARTESIAN_POINT('Ctrl Pts',(-24.8338768826158,20.593905981155,-23.7111914285813));
#30358=CARTESIAN_POINT('Ctrl Pts',(-24.8700003717419,20.6098542019597,-23.7135421767373));
#30359=CARTESIAN_POINT('Ctrl Pts',(-24.9867121830484,20.6639658680672,-23.7211103545583));
#30360=CARTESIAN_POINT('Ctrl Pts',(-25.066015557521,20.7048120328583,-23.7262109146711));
#30361=CARTESIAN_POINT('Ctrl Pts',(-25.2100786963827,20.7867481608396,-23.7355775440997));
#30362=CARTESIAN_POINT('Ctrl Pts',(-25.2752610823137,20.8269594419621,-23.7398565314771));
#30363=CARTESIAN_POINT('Ctrl Pts',(-25.5637921702891,21.0194748815147,-23.7592381835299));
#30364=CARTESIAN_POINT('Ctrl Pts',(-25.7688317937022,21.1971572815913,-23.7743667659568));
#30365=CARTESIAN_POINT('Ctrl Pts',(-25.9609057437737,21.4112874541552,-23.7917933946624));
#30366=CARTESIAN_POINT('Ctrl Pts',(-25.9724225127965,21.4243378871351,-23.7928521842482));
#30367=CARTESIAN_POINT('Ctrl Pts',(-25.9876814368424,21.4419137643161,-23.7942740129781));
#30368=CARTESIAN_POINT('Ctrl Pts',(-25.991517904435,21.4463572384781,-23.7946331272622));
#30369=CARTESIAN_POINT('Ctrl Pts',(-25.9974950197168,21.4533184153263,-23.7951951868065));
#30370=CARTESIAN_POINT('Ctrl Pts',(-25.9996439855587,21.4558289859004,-23.7953977878822));
#30371=CARTESIAN_POINT('Ctrl Pts',(-26.0037476673929,21.4606381447685,-23.7957856801245));
#30372=CARTESIAN_POINT('Ctrl Pts',(-26.0057030253743,21.4629361829029,-23.7959709445524));
#30373=CARTESIAN_POINT('Ctrl Pts',(-26.0102677180874,21.4683161368726,-23.7964044640518));
#30374=CARTESIAN_POINT('Ctrl Pts',(-26.0128744890458,21.4714002126723,-23.7966528241015));
#30375=CARTESIAN_POINT('Ctrl Pts',(-26.0203245733942,21.4802480991828,-23.7973649012666));
#30376=CARTESIAN_POINT('Ctrl Pts',(-26.0251534714505,21.4860239642489,-23.797829207574));
#30377=CARTESIAN_POINT('Ctrl Pts',(-26.0557543723189,21.5228875587062,-23.8007892573681));
#30378=CARTESIAN_POINT('Ctrl Pts',(-26.0809594311276,21.5544392746789,-23.8033078989538));
#30379=CARTESIAN_POINT('Ctrl Pts',(-26.244414824835,21.7671289644243,-23.8201978888315));
#30380=CARTESIAN_POINT('Ctrl Pts',(-26.3636864802293,21.9619851869276,-23.8353240067263));
#30381=CARTESIAN_POINT('Ctrl Pts',(-26.4777808904536,22.2022343826553,-23.853299922116));
#30382=CARTESIAN_POINT('Ctrl Pts',(-26.493544964916,22.2370104166826,-23.8558846631623));
#30383=CARTESIAN_POINT('Ctrl Pts',(-26.5757446364894,22.427265028808,-23.8699136662745));
#30384=CARTESIAN_POINT('Ctrl Pts',(-26.6304903866062,22.587522776766,-23.8813450294571));
#30385=CARTESIAN_POINT('Ctrl Pts',(-26.6821308760925,22.7893365361344,-23.894757065339));
#30386=CARTESIAN_POINT('Ctrl Pts',(-26.6911576956937,22.8275006976044,-23.8972506216658));
#30387=CARTESIAN_POINT('Ctrl Pts',(-26.7004989772834,22.8704822495638,-23.900003971944));
#30388=CARTESIAN_POINT('Ctrl Pts',(-26.7015014226486,22.8751445904222,-23.9003019142834));
#30389=CARTESIAN_POINT('Ctrl Pts',(-26.7029947639759,22.8821658722308,-23.9007494982689));
#30390=CARTESIAN_POINT('Ctrl Pts',(-26.7034933638686,22.8845231405997,-23.9008995793385));
#30391=CARTESIAN_POINT('Ctrl Pts',(-26.7043520109571,22.8886052374062,-23.9011591490832));
#30392=CARTESIAN_POINT('Ctrl Pts',(-26.7047132871157,22.8903298016229,-23.9012687086991));
#30393=CARTESIAN_POINT('Ctrl Pts',(-26.7054627769787,22.8939221956383,-23.9014967181431));
#30394=CARTESIAN_POINT('Ctrl Pts',(-26.7058507460793,22.8957900718362,-23.9016151532709));
#30395=CARTESIAN_POINT('Ctrl Pts',(-26.7066195734819,22.8995081668616,-23.9018506688271));
#30396=CARTESIAN_POINT('Ctrl Pts',(-26.7070004645134,22.9013583804411,-23.901967751257));
#30397=CARTESIAN_POINT('Ctrl Pts',(-26.7078884691636,22.9056912316447,-23.9022416674573));
#30398=CARTESIAN_POINT('Ctrl Pts',(-26.7083942829245,22.9081741390036,-23.902398426545));
#30399=CARTESIAN_POINT('Ctrl Pts',(-26.7097109438724,22.9146764800406,-23.9028084193512));
#30400=CARTESIAN_POINT('Ctrl Pts',(-26.7105170524914,22.9186968850994,-23.9030613840234));
#30401=CARTESIAN_POINT('Ctrl Pts',(-26.7521445500613,23.1283862502783,-23.9162277483037));
#30402=CARTESIAN_POINT('Ctrl Pts',(-26.7728102336783,23.3375787477034,-23.9280086774442));
#30403=CARTESIAN_POINT('Ctrl Pts',(-26.7730011959272,23.5473183053636,-23.9397396857875));
#30404=CARTESIAN_POINT('Ctrl Pts',(-26.7730011946114,23.5473168605001,-23.9397396049744));
#30405=CARTESIAN_POINT('Ctrl Pts',(-26.7731913401487,23.7560566122004,-23.9514146933273));
#30406=CARTESIAN_POINT('Ctrl Pts',(-26.7531018191501,23.9643123818198,-23.9630020629255));
#30407=CARTESIAN_POINT('Ctrl Pts',(-26.7009884365783,24.2306218430946,-23.9788500787034));
#30408=CARTESIAN_POINT('Ctrl Pts',(-26.6871740276188,24.2917118419737,-23.9825546230068));
#30409=CARTESIAN_POINT('Ctrl Pts',(-26.6661438042863,24.3735494892528,-23.9876295540581));
#30410=CARTESIAN_POINT('Ctrl Pts',(-26.6604825235153,24.3946846870221,-23.9889503815506));
#30411=CARTESIAN_POINT('Ctrl Pts',(-26.6519194653666,24.4253981801862,-23.9908853337584));
#30412=CARTESIAN_POINT('Ctrl Pts',(-26.6491875112965,24.4350234976433,-23.9914939643327));
#30413=CARTESIAN_POINT('Ctrl Pts',(-26.6441945082637,24.4523081755506,-23.9925910053368));
#30414=CARTESIAN_POINT('Ctrl Pts',(-26.6419497195621,24.4599721784601,-23.9930788834171));
#30415=CARTESIAN_POINT('Ctrl Pts',(-26.6384994033316,24.4715917316363,-23.9938207979259));
#30416=CARTESIAN_POINT('Ctrl Pts',(-26.6373146991872,24.475553474798,-23.9940741520627));
#30417=CARTESIAN_POINT('Ctrl Pts',(-26.6351659572365,24.4826889753866,-23.9945311845607));
#30418=CARTESIAN_POINT('Ctrl Pts',(-26.6342046366951,24.4858635505183,-23.9947347735429));
#30419=CARTESIAN_POINT('Ctrl Pts',(-26.6322693770049,24.4922189823462,-23.9951428692646));
#30420=CARTESIAN_POINT('Ctrl Pts',(-26.6312954103363,24.495399826443,-23.9953473767017));
#30421=CARTESIAN_POINT('Ctrl Pts',(-26.6285569963222,24.5042939039249,-23.9959199348474));
#30422=CARTESIAN_POINT('Ctrl Pts',(-26.6267815775774,24.5100037212961,-23.9962883458997));
#30423=CARTESIAN_POINT('Ctrl Pts',(-26.6195334212119,24.5330873004436,-23.9977811819743));
#30424=CARTESIAN_POINT('Ctrl Pts',(-26.6139294050163,24.550419195487,-23.9989099238953));
#30425=CARTESIAN_POINT('Ctrl Pts',(-26.519397830105,24.8345320628341,-24.017545087222));
#30426=CARTESIAN_POINT('Ctrl Pts',(-26.3960942803446,25.0885346291411,-24.0362920090593));
#30427=CARTESIAN_POINT('Ctrl Pts',(-26.2192915525039,25.3568988811205,-24.0580453556523));
#30428=CARTESIAN_POINT('Ctrl Pts',(-26.1965005650715,25.3901198356431,-24.0607728054594));
#30429=CARTESIAN_POINT('Ctrl Pts',(-26.151527219039,25.4531095828278,-24.0660027638298));
#30430=CARTESIAN_POINT('Ctrl Pts',(-26.1294412712494,25.4829399032005,-24.0685057064869));
#30431=CARTESIAN_POINT('Ctrl Pts',(-26.048824160954,25.5879814055165,-24.0773992275354));
#30432=CARTESIAN_POINT('Ctrl Pts',(-25.9874740112576,25.6609759905915,-24.0837302108687));
#30433=CARTESIAN_POINT('Ctrl Pts',(-25.892135588897,25.7647000913621,-24.0928360104573));
#30434=CARTESIAN_POINT('Ctrl Pts',(-25.8605868521906,25.7975954316597,-24.0957412233313));
#30435=CARTESIAN_POINT('Ctrl Pts',(-25.825749706611,25.8324102111203,-24.098824215181));
#30436=CARTESIAN_POINT('Ctrl Pts',(-25.8231459242318,25.8350034356866,-24.0990539063354));
#30437=CARTESIAN_POINT('Ctrl Pts',(-25.8188658191795,25.8392516280609,-24.0994302579395));
#30438=CARTESIAN_POINT('Ctrl Pts',(-25.8171921163905,25.8409092128108,-24.0995771235987));
#30439=CARTESIAN_POINT('Ctrl Pts',(-25.813934097109,25.8441287887592,-24.099862418485));
#30440=CARTESIAN_POINT('Ctrl Pts',(-25.8123499781645,25.8456909767565,-24.1000008632961));
#30441=CARTESIAN_POINT('Ctrl Pts',(-25.8095674495811,25.8484293055243,-24.100243565293));
#30442=CARTESIAN_POINT('Ctrl Pts',(-25.8083697432332,25.8496061454182,-24.10034787822));
#30443=CARTESIAN_POINT('Ctrl Pts',(-25.8058301439159,25.85209760176,-24.1005687331212));
#30444=CARTESIAN_POINT('Ctrl Pts',(-25.8044880251404,25.8534119772111,-24.1006852559316));
#30445=CARTESIAN_POINT('Ctrl Pts',(-25.8006689998049,25.8571455222679,-24.1010162759714));
#30446=CARTESIAN_POINT('Ctrl Pts',(-25.7981893333185,25.8595618843087,-24.1012305508906));
#30447=CARTESIAN_POINT('Ctrl Pts',(-25.7876748376399,25.8697749683601,-24.1021363983417));
#30448=CARTESIAN_POINT('Ctrl Pts',(-25.779603177107,25.8775339108661,-24.1028250344881));
#30449=CARTESIAN_POINT('Ctrl Pts',(-25.6369681623953,26.0132198365096,-24.1148793439844));
#30450=CARTESIAN_POINT('Ctrl Pts',(-25.4916150674948,26.1293460963654,-24.1253889290192));
#30451=CARTESIAN_POINT('Ctrl Pts',(-25.2605723914126,26.2832669251856,-24.1409456774259));
#30452=CARTESIAN_POINT('Ctrl Pts',(-25.1819532705439,26.3309205124581,-24.1460606515053));
#30453=CARTESIAN_POINT('Ctrl Pts',(-25.0090674825753,26.4258522193989,-24.1571241608869));
#30454=CARTESIAN_POINT('Ctrl Pts',(-24.9143034855469,26.4719947646665,-24.1630791476204));
#30455=CARTESIAN_POINT('Ctrl Pts',(-24.742166867768,26.5456093841202,-24.1738904336621));
#30456=CARTESIAN_POINT('Ctrl Pts',(-24.6656844564941,26.5749231725428,-24.1786914958999));
#30457=CARTESIAN_POINT('Ctrl Pts',(-24.5488533596312,26.6146674686757,-24.1860723820432));
#30458=CARTESIAN_POINT('Ctrl Pts',(-24.5092802455146,26.6272816375021,-24.1885801440985));
#30459=CARTESIAN_POINT('Ctrl Pts',(-24.462204149314,26.6412910899979,-24.1915760180743));
#30460=CARTESIAN_POINT('Ctrl Pts',(-24.4549249562355,26.6434293653915,-24.1920396106293));
#30461=CARTESIAN_POINT('Ctrl Pts',(-24.4437478933156,26.6466698176789,-24.1927520112161));
#30462=CARTESIAN_POINT('Ctrl Pts',(-24.4398553484388,26.6477903923804,-24.1930002176856));
#30463=CARTESIAN_POINT('Ctrl Pts',(-24.4330583895921,26.6497332126272,-24.1934338089761));
#30464=CARTESIAN_POINT('Ctrl Pts',(-24.4301549075182,26.6505587235302,-24.1936190869576));
#30465=CARTESIAN_POINT('Ctrl Pts',(-24.4240767438306,26.6522776259771,-24.194007074424));
#30466=CARTESIAN_POINT('Ctrl Pts',(-24.4209018435775,26.6531702255538,-24.1942098094914));
#30467=CARTESIAN_POINT('Ctrl Pts',(-24.4121038877988,26.6556291392311,-24.194771809376));
#30468=CARTESIAN_POINT('Ctrl Pts',(-24.4064779591219,26.6571850464691,-24.1951314127393));
#30469=CARTESIAN_POINT('Ctrl Pts',(-24.3842907345081,26.6632563068459,-24.1965505160643));
#30470=CARTESIAN_POINT('Ctrl Pts',(-24.3676979352611,26.6676545304265,-24.1976138164549));
#30471=CARTESIAN_POINT('Ctrl Pts',(-24.091284638085,26.7385643546634,-24.215362586379));
#30472=CARTESIAN_POINT('Ctrl Pts',(-23.8242531776045,26.772504814028,-24.2331668575916));
#30473=CARTESIAN_POINT('Ctrl Pts',(-23.4214272906506,26.7732445289567,-24.2604203146326));
#30474=CARTESIAN_POINT('Ctrl Pts',(-23.2867965958626,26.7650413154186,-24.2695682297704));
#30475=CARTESIAN_POINT('Ctrl Pts',(-23.0924240080346,26.7409022095162,-24.2825541124644));
#30476=CARTESIAN_POINT('Ctrl Pts',(-23.0319996262432,26.7316464430765,-24.2865583138494));
#30477=CARTESIAN_POINT('Ctrl Pts',(-22.9349367916642,26.713939252274,-24.292900675658));
#30478=CARTESIAN_POINT('Ctrl Pts',(-22.8981207296166,26.7065559938886,-24.2952851960947));
#30479=CARTESIAN_POINT('Ctrl Pts',(-22.8568181674232,26.6975193984223,-24.2979300194087));
#30480=CARTESIAN_POINT('Ctrl Pts',(-22.8521983699295,26.6964979664753,-24.2982254208128));
#30481=CARTESIAN_POINT('Ctrl Pts',(-22.8457234806042,26.6950514124651,-24.2986388234941));
#30482=CARTESIAN_POINT('Ctrl Pts',(-22.8438665197796,26.6946348218338,-24.2987573136612));
#30483=CARTESIAN_POINT('Ctrl Pts',(-22.8401408995587,26.6937955492028,-24.2989948957758));
#30484=CARTESIAN_POINT('Ctrl Pts',(-22.838272243399,26.6933728447224,-24.2991139865327));
#30485=CARTESIAN_POINT('Ctrl Pts',(-22.8346953969855,26.6925603809119,-24.2993418000708));
#30486=CARTESIAN_POINT('Ctrl Pts',(-22.8329871501063,26.6921708954809,-24.2994505386666));
#30487=CARTESIAN_POINT('Ctrl Pts',(-22.8289682914225,26.6912511352162,-24.2997062161781));
#30488=CARTESIAN_POINT('Ctrl Pts',(-22.826657941614,26.690719702655,-24.2998530878346));
#30489=CARTESIAN_POINT('Ctrl Pts',(-22.8198492723732,26.6891456428286,-24.300285599877));
#30490=CARTESIAN_POINT('Ctrl Pts',(-22.8153525805544,26.6880958908815,-24.3005708305936));
#30491=CARTESIAN_POINT('Ctrl Pts',(-22.7767206179296,26.6789896669431,-24.3030178488451));
#30492=CARTESIAN_POINT('Ctrl Pts',(-22.7427150276733,26.6703857193908,-24.3051486259031));
#30493=CARTESIAN_POINT('Ctrl Pts',(-22.5714913024336,26.6240763784092,-24.3157910506227));
#30494=CARTESIAN_POINT('Ctrl Pts',(-22.4367224791473,26.5778632490605,-24.3238888879124));
#30495=CARTESIAN_POINT('Ctrl Pts',(-22.2272216684074,26.4901330316552,-24.336652316664));
#30496=CARTESIAN_POINT('Ctrl Pts',(-22.1503628003474,26.4543194309421,-24.3413741372416));
#30497=CARTESIAN_POINT('Ctrl Pts',(-22.0750358381979,26.41553668335,-24.3461133775544));
#30498=CARTESIAN_POINT('Ctrl Pts',(-22.0750360162151,26.4155367750037,-24.595751509546));
#30499=CARTESIAN_POINT('Ctrl Pts',(-22.1135901637226,26.4353867131996,-24.5931611949348));
#30500=CARTESIAN_POINT('Ctrl Pts',(-22.1525404942053,26.4544562058755,-24.5905450872213));
#30501=CARTESIAN_POINT('Ctrl Pts',(-22.1992285932744,26.4761571518567,-24.5874060765246));
#30502=CARTESIAN_POINT('Ctrl Pts',(-22.2066066639115,26.4795526714133,-24.5869099316408));
#30503=CARTESIAN_POINT('Ctrl Pts',(-22.2177862503386,26.4846465929852,-24.5861579857106));
#30504=CARTESIAN_POINT('Ctrl Pts',(-22.2215783899634,26.4863655953767,-24.5859028954903));
#30505=CARTESIAN_POINT('Ctrl Pts',(-22.2281375372298,26.4893235916303,-24.5854616203673));
#30506=CARTESIAN_POINT('Ctrl Pts',(-22.2309029882116,26.490566041501,-24.5852755547004));
#30507=CARTESIAN_POINT('Ctrl Pts',(-22.2366315793422,26.4931300491559,-24.5848900866926));
#30508=CARTESIAN_POINT('Ctrl Pts',(-22.2395949693015,26.4944510377824,-24.584690665037));
#30509=CARTESIAN_POINT('Ctrl Pts',(-22.246783399311,26.4976424164554,-24.5842068684607));
#30510=CARTESIAN_POINT('Ctrl Pts',(-22.2510104682009,26.4995081957512,-24.5839223356345));
#30511=CARTESIAN_POINT('Ctrl Pts',(-22.2667842902624,26.5064300851794,-24.5828603989528));
#30512=CARTESIAN_POINT('Ctrl Pts',(-22.2783565466571,26.5114274759495,-24.5820809878546));
#30513=CARTESIAN_POINT('Ctrl Pts',(-22.4759157260681,26.5953701807305,-24.5687684308176));
#30514=CARTESIAN_POINT('Ctrl Pts',(-22.6688550547314,26.6567057686386,-24.5556235351217));
#30515=CARTESIAN_POINT('Ctrl Pts',(-23.1550784418745,26.7623114966141,-24.5223063464347));
#30516=CARTESIAN_POINT('Ctrl Pts',(-23.4511820654088,26.7850140077257,-24.5017867825422));
#30517=CARTESIAN_POINT('Ctrl Pts',(-23.7544767040227,26.7665358265135,-24.4826244287114));
#30518=CARTESIAN_POINT('Ctrl Pts',(-23.762716842461,26.7660020034705,-24.4821053352034));
#30519=CARTESIAN_POINT('Ctrl Pts',(-23.7769695461287,26.7650236438852,-24.4812102187402));
#30520=CARTESIAN_POINT('Ctrl Pts',(-23.7829830373137,26.7645938983768,-24.4808333971234));
#30521=CARTESIAN_POINT('Ctrl Pts',(-23.7915880354677,26.7639546797248,-24.4802954290968));
#30522=CARTESIAN_POINT('Ctrl Pts',(-23.7941805030643,26.7637589447166,-24.4801335147024));
#30523=CARTESIAN_POINT('Ctrl Pts',(-23.7986804902654,26.7634137123425,-24.4798527489413));
#30524=CARTESIAN_POINT('Ctrl Pts',(-23.8005881163156,26.7632656531378,-24.4797338159228));
#30525=CARTESIAN_POINT('Ctrl Pts',(-23.8042454445681,26.7629785149475,-24.4795059672133));
#30526=CARTESIAN_POINT('Ctrl Pts',(-23.805995162196,26.7628397056464,-24.4793970362644));
#30527=CARTESIAN_POINT('Ctrl Pts',(-23.8101198885386,26.7625090900617,-24.4791404212831));
#30528=CARTESIAN_POINT('Ctrl Pts',(-23.8124948036043,26.7623160788299,-24.4789928057272));
#30529=CARTESIAN_POINT('Ctrl Pts',(-23.8195179552625,26.7617374606436,-24.4785566731242));
#30530=CARTESIAN_POINT('Ctrl Pts',(-23.8241655967816,26.7613443943819,-24.4782685754838));
#30531=CARTESIAN_POINT('Ctrl Pts',(-23.8649685290172,26.7578043253812,-24.4757437032973));
#30532=CARTESIAN_POINT('Ctrl Pts',(-23.9010709602227,26.7540567345328,-24.4735401528992));
#30533=CARTESIAN_POINT('Ctrl Pts',(-24.0850469088672,26.7318118287296,-24.4624316296644));
#30534=CARTESIAN_POINT('Ctrl Pts',(-24.2315888290129,26.7036817315449,-24.4539779292751));
#30535=CARTESIAN_POINT('Ctrl Pts',(-24.6727856904948,26.5867819606826,-24.4283674860072));
#30536=CARTESIAN_POINT('Ctrl Pts',(-24.9570698253272,26.4659750863626,-24.4114705710625));
#30537=CARTESIAN_POINT('Ctrl Pts',(-25.2408271966982,26.2940949345589,-24.3914493253635));
#30538=CARTESIAN_POINT('Ctrl Pts',(-25.2615680613305,26.2812071151483,-24.3899672347442));
#30539=CARTESIAN_POINT('Ctrl Pts',(-25.2875883956991,26.2646259568132,-24.3880834199653));
#30540=CARTESIAN_POINT('Ctrl Pts',(-25.2930063466631,26.2611505627554,-24.3876898176084));
#30541=CARTESIAN_POINT('Ctrl Pts',(-25.3016051047201,26.2555983797952,-24.3870629637952));
#30542=CARTESIAN_POINT('Ctrl Pts',(-25.3047927341906,26.2535321455169,-24.3868301071897));
#30543=CARTESIAN_POINT('Ctrl Pts',(-25.3107854499251,26.2496325782911,-24.38639143699));
#30544=CARTESIAN_POINT('Ctrl Pts',(-25.3135913467412,26.2478004951887,-24.3861856704558));
#30545=CARTESIAN_POINT('Ctrl Pts',(-25.3198864802833,26.2436761299926,-24.3857231837511));
#30546=CARTESIAN_POINT('Ctrl Pts',(-25.3233741257845,26.2413814405684,-24.3854663733113));
#30547=CARTESIAN_POINT('Ctrl Pts',(-25.3322207599491,26.2355361520196,-24.3848134706495));
#30548=CARTESIAN_POINT('Ctrl Pts',(-25.3375735834468,26.2319762954514,-24.3844170298212));
#30549=CARTESIAN_POINT('Ctrl Pts',(-25.3670114078132,26.2122715948748,-24.382229090642));
#30550=CARTESIAN_POINT('Ctrl Pts',(-25.3908876964281,26.1958187108771,-24.3804259489078));
#30551=CARTESIAN_POINT('Ctrl Pts',(-25.420547413654,26.1747846595952,-24.3781491998147));
#30552=CARTESIAN_POINT('Ctrl Pts',(-25.4265420342252,26.170502431438,-24.3776871251509));
#30553=CARTESIAN_POINT('Ctrl Pts',(-25.4379895582557,26.162265520645,-24.3768010469268));
#30554=CARTESIAN_POINT('Ctrl Pts',(-25.4434448555878,26.158314217993,-24.3763771745035));
#30555=CARTESIAN_POINT('Ctrl Pts',(-25.4506736422669,26.153043735412,-24.3758133496465));
#30556=CARTESIAN_POINT('Ctrl Pts',(-25.4524582489989,26.1517397710777,-24.3756739803957));
#30557=CARTESIAN_POINT('Ctrl Pts',(-25.4584959367463,26.1473186600229,-24.3752018724596));
#30558=CARTESIAN_POINT('Ctrl Pts',(-25.4627426913871,26.1441929235276,-24.374868805511));
#30559=CARTESIAN_POINT('Ctrl Pts',(-25.4789472584008,26.1322044582896,-24.3735940742485));
#30560=CARTESIAN_POINT('Ctrl Pts',(-25.4908511484174,26.1232694568167,-24.3726496569076));
#30561=CARTESIAN_POINT('Ctrl Pts',(-25.5466781651561,26.0807581829191,-24.3681824733048));
#30562=CARTESIAN_POINT('Ctrl Pts',(-25.5897923591412,26.0461393228307,-24.3646203905203));
#30563=CARTESIAN_POINT('Ctrl Pts',(-25.7922967131517,25.8747852472769,-24.3473423809893));
#30564=CARTESIAN_POINT('Ctrl Pts',(-25.9389431022739,25.723810072234,-24.3331035367328));
#30565=CARTESIAN_POINT('Ctrl Pts',(-26.1793091158038,25.4224169657331,-24.3070379786952));
#30566=CARTESIAN_POINT('Ctrl Pts',(-26.2773881017931,25.276429187255,-24.2952556664628));
#30567=CARTESIAN_POINT('Ctrl Pts',(-26.3690376809031,25.1125316842191,-24.2834169688822));
#30568=CARTESIAN_POINT('Ctrl Pts',(-26.3749211754069,25.1018687639936,-24.2826527823063));
#30569=CARTESIAN_POINT('Ctrl Pts',(-26.3823816985277,25.0881646467886,-24.2816785826214));
#30570=CARTESIAN_POINT('Ctrl Pts',(-26.3840144138419,25.0851541203736,-24.2814650587251));
#30571=CARTESIAN_POINT('Ctrl Pts',(-26.3866303491642,25.0803122558447,-24.2811224375034));
#30572=CARTESIAN_POINT('Ctrl Pts',(-26.3876165961152,25.0784825696448,-24.2809931461232));
#30573=CARTESIAN_POINT('Ctrl Pts',(-26.3894908597987,25.0749973654298,-24.2807472175548));
#30574=CARTESIAN_POINT('Ctrl Pts',(-26.3903791925085,25.0733420373796,-24.280630560662));
#30575=CARTESIAN_POINT('Ctrl Pts',(-26.3923975312072,25.0695731391579,-24.2803652904408));
#30576=CARTESIAN_POINT('Ctrl Pts',(-26.3935266257324,25.0674590874345,-24.2802167360947));
#30577=CARTESIAN_POINT('Ctrl Pts',(-26.397023599987,25.0608939405748,-24.2797561451968));
#30578=CARTESIAN_POINT('Ctrl Pts',(-26.3993834083641,25.0564385195183,-24.2794446232843));
#30579=CARTESIAN_POINT('Ctrl Pts',(-26.4171602356189,25.022683823262,-24.2770923519426));
#30580=CARTESIAN_POINT('Ctrl Pts',(-26.4321361119596,24.9931527117092,-24.2750790808188));
#30581=CARTESIAN_POINT('Ctrl Pts',(-26.579979590395,24.6901299695189,-24.2548187603384));
#30582=CARTESIAN_POINT('Ctrl Pts',(-26.6739828158323,24.3993323757024,-24.2385300908595));
#30583=CARTESIAN_POINT('Ctrl Pts',(-26.7554840368577,23.9282288769233,-24.2114155426187));
#30584=CARTESIAN_POINT('Ctrl Pts',(-26.7712071638657,23.7547343293672,-24.2013077227666));
#30585=CARTESIAN_POINT('Ctrl Pts',(-26.7729543698201,23.5706188576439,-24.1900992063219));
#30586=CARTESIAN_POINT('Ctrl Pts',(-26.7730027367683,23.5604032267184,-24.1894758147137));
#30587=CARTESIAN_POINT('Ctrl Pts',(-26.7730024481601,23.5460721172818,-24.1885991423379));
#30588=CARTESIAN_POINT('Ctrl Pts',(-26.7729944818974,23.5419566236212,-24.1883471389412));
#30589=CARTESIAN_POINT('Ctrl Pts',(-26.7729654429978,23.5344164006638,-24.1878849716837));
#30590=CARTESIAN_POINT('Ctrl Pts',(-26.7729467943467,23.5309916631083,-24.1876748841723));
#30591=CARTESIAN_POINT('Ctrl Pts',(-26.7728980092678,23.5240613418659,-24.1872493968364));
#30592=CARTESIAN_POINT('Ctrl Pts',(-26.7728676117933,23.5205557656606,-24.1870339891313));
#30593=CARTESIAN_POINT('Ctrl Pts',(-26.7727788835205,23.5119438898649,-24.1865043616412));
#30594=CARTESIAN_POINT('Ctrl Pts',(-26.7727141358576,23.5068376786332,-24.1861899407832));
#30595=CARTESIAN_POINT('Ctrl Pts',(-26.77243530426,23.4883198168534,-24.1850482512166));
#30596=CARTESIAN_POINT('Ctrl Pts',(-26.7721496286861,23.4749095251215,-24.1842187379668));
#30597=CARTESIAN_POINT('Ctrl Pts',(-26.766790052078,23.2803648806809,-24.1721444470134));
#30598=CARTESIAN_POINT('Ctrl Pts',(-26.7465330965104,23.1000046048152,-24.1604131008969));
#30599=CARTESIAN_POINT('Ctrl Pts',(-26.6505728266991,22.6169393471348,-24.1275965740543));
#30600=CARTESIAN_POINT('Ctrl Pts',(-26.5459786080223,22.3219673449654,-24.1058982575636));
#30601=CARTESIAN_POINT('Ctrl Pts',(-26.3932673462726,22.0324783221359,-24.0851894584158));
#30602=CARTESIAN_POINT('Ctrl Pts',(-26.385723253345,22.0184308714549,-24.0841866006848));
#30603=CARTESIAN_POINT('Ctrl Pts',(-26.3763650867354,22.0013115717109,-24.0829674816765));
#30604=CARTESIAN_POINT('Ctrl Pts',(-26.3746499423254,21.9981863158393,-24.0827450471344));
#30605=CARTESIAN_POINT('Ctrl Pts',(-26.3718107114501,21.9930330940964,-24.0823784899465));
#30606=CARTESIAN_POINT('Ctrl Pts',(-26.3706896220525,21.9910034951441,-24.0822341761736));
#30607=CARTESIAN_POINT('Ctrl Pts',(-26.3686620880612,21.9873422274789,-24.0819739450208));
#30608=CARTESIAN_POINT('Ctrl Pts',(-26.3677564186201,21.9857101405592,-24.0818579782231));
#30609=CARTESIAN_POINT('Ctrl Pts',(-26.3658033691769,21.9821977889061,-24.081608489898));
#30610=CARTESIAN_POINT('Ctrl Pts',(-26.3647555262799,21.9803177915336,-24.0814749992009));
#30611=CARTESIAN_POINT('Ctrl Pts',(-26.3618744257787,21.9751607925527,-24.0811089522741));
#30612=CARTESIAN_POINT('Ctrl Pts',(-26.3600373157019,21.9718859298215,-24.0808766446092));
#30613=CARTESIAN_POINT('Ctrl Pts',(-26.3503791746485,21.954739468497,-24.0796610486636));
#30614=CARTESIAN_POINT('Ctrl Pts',(-26.342460952926,21.9409224510512,-24.0786839524006));
#30615=CARTESIAN_POINT('Ctrl Pts',(-26.2425535918111,21.7695449051666,-24.0665881839196));
#30616=CARTESIAN_POINT('Ctrl Pts',(-26.1374328324067,21.6199875102982,-24.0562719498195));
#30617=CARTESIAN_POINT('Ctrl Pts',(-25.8787942388071,21.3113972672536,-24.0337156542308));
#30618=CARTESIAN_POINT('Ctrl Pts',(-25.7204834332987,21.1576242166834,-24.0215484534736));
#30619=CARTESIAN_POINT('Ctrl Pts',(-25.4736594461816,20.962679400865,-24.0032057382177));
#30620=CARTESIAN_POINT('Ctrl Pts',(-25.3970504099156,20.9074578362577,-23.997594077638));
#30621=CARTESIAN_POINT('Ctrl Pts',(-25.309547620996,20.8500481308872,-23.9912234706796));
#30622=CARTESIAN_POINT('Ctrl Pts',(-25.300934715666,20.8444559938398,-23.9905968397905));
#30623=CARTESIAN_POINT('Ctrl Pts',(-25.2888254725746,20.8366757957987,-23.9897163776854));
#30624=CARTESIAN_POINT('Ctrl Pts',(-25.2853513739022,20.8344530950889,-23.9894638387473));
#30625=CARTESIAN_POINT('Ctrl Pts',(-25.2789826769736,20.830395661883,-23.9890009958823));
#30626=CARTESIAN_POINT('Ctrl Pts',(-25.2760893962197,20.8285588633392,-23.9887907691329));
#30627=CARTESIAN_POINT('Ctrl Pts',(-25.2702328803411,20.8248539492092,-23.9883653138106));
#30628=CARTESIAN_POINT('Ctrl Pts',(-25.2672695191249,20.8229860434568,-23.9881500778712));
#30629=CARTESIAN_POINT('Ctrl Pts',(-25.2599899739694,20.8184140696937,-23.9876214465936));
#30630=CARTESIAN_POINT('Ctrl Pts',(-25.2556704244734,20.8157154018502,-23.9873078518885));
#30631=CARTESIAN_POINT('Ctrl Pts',(-25.2402792684196,20.8061503251487,-23.9861907599558));
#30632=CARTESIAN_POINT('Ctrl Pts',(-25.2291725577093,20.7993408956997,-23.9853851647965));
#30633=CARTESIAN_POINT('Ctrl Pts',(-25.0768004289212,20.7071893456473,-23.9743396876003));
#30634=CARTESIAN_POINT('Ctrl Pts',(-24.9292473700157,20.6327682584562,-23.9636990083846));
#30635=CARTESIAN_POINT('Ctrl Pts',(-24.5119950272348,20.461064647255,-23.9337742698664));
#30636=CARTESIAN_POINT('Ctrl Pts',(-24.2340204520156,20.3878992887072,-23.9139196522787));
#30637=CARTESIAN_POINT('Ctrl Pts',(-23.9470354765121,20.3520201929175,-23.8951205970291));
#30638=CARTESIAN_POINT('Ctrl Pts',(-23.9440193939772,20.3516474519105,-23.8949232288537));
#30639=CARTESIAN_POINT('Ctrl Pts',(-23.9323667444999,20.350224096708,-23.8941614849061));
#30640=CARTESIAN_POINT('Ctrl Pts',(-23.9237263824441,20.3492041811732,-23.8935983304071));
#30641=CARTESIAN_POINT('Ctrl Pts',(-23.9134437259337,20.3480326083604,-23.8929302063955));
#30642=CARTESIAN_POINT('Ctrl Pts',(-23.9118054007822,20.3478472163345,-23.8928238173666));
#30643=CARTESIAN_POINT('Ctrl Pts',(-23.9074597642698,20.3473588436667,-23.8925417887819));
#30644=CARTESIAN_POINT('Ctrl Pts',(-23.9047522037392,20.3470580376876,-23.8923662419409));
#30645=CARTESIAN_POINT('Ctrl Pts',(-23.8630352829491,20.3424768905867,-23.8896641713945));
#30646=CARTESIAN_POINT('Ctrl Pts',(-23.8239490751474,20.3389057483981,-23.8871685558398));
#30647=CARTESIAN_POINT('Ctrl Pts',(-23.7800477678339,20.3357021018247,-23.8844131272201));
#30648=CARTESIAN_POINT('Ctrl Pts',(-23.7752894778093,20.3353654900852,-23.8841151038464));
#30649=CARTESIAN_POINT('Ctrl Pts',(-23.7681262491319,20.3348747291761,-23.8836674143066));
#30650=CARTESIAN_POINT('Ctrl Pts',(-23.7657218828922,20.3347127125559,-23.8835173084496));
#30651=CARTESIAN_POINT('Ctrl Pts',(-23.7615590213966,20.3344368909703,-23.8832577034981));
#30652=CARTESIAN_POINT('Ctrl Pts',(-23.7598006148731,20.3343218314792,-23.8831481334284));
#30653=CARTESIAN_POINT('Ctrl Pts',(-23.7561382798192,20.3340852069241,-23.8829201098612));
#30654=CARTESIAN_POINT('Ctrl Pts',(-23.7542343397835,20.3339638903894,-23.8828016710548));
#30655=CARTESIAN_POINT('Ctrl Pts',(-23.7497654691771,20.3336831239949,-23.882523916806));
#30656=CARTESIAN_POINT('Ctrl Pts',(-23.7472004462455,20.3335250508786,-23.8823646794655));
#30657=CARTESIAN_POINT('Ctrl Pts',(-23.7387871980561,20.3330166736344,-23.8818429873877));
#30658=CARTESIAN_POINT('Ctrl Pts',(-23.7329381626823,20.3326792460775,-23.8814812562427));
#30659=CARTESIAN_POINT('Ctrl Pts',(-23.7191303365629,20.3319204530977,-23.8806295099922));
#30660=CARTESIAN_POINT('Ctrl Pts',(-23.7111707959164,20.3315126545934,-23.8801402386767));
#30661=CARTESIAN_POINT('Ctrl Pts',(-23.4323053348698,20.3182622931688,-23.8630560864631));
#30662=CARTESIAN_POINT('Ctrl Pts',(-23.16080701125,20.3396357480102,-23.8482691213606));
#30663=CARTESIAN_POINT('Ctrl Pts',(-22.7479223309423,20.4253530435576,-23.8246348929832));
#30664=CARTESIAN_POINT('Ctrl Pts',(-22.6030162188156,20.4661857497469,-23.8161204641292));
#30665=CARTESIAN_POINT('Ctrl Pts',(-22.4480413576374,20.5218119157592,-23.8064594158265));
#30666=CARTESIAN_POINT('Ctrl Pts',(-22.4346150897375,20.5267322116466,-23.8056178439904));
#30667=CARTESIAN_POINT('Ctrl Pts',(-22.4148446274654,20.5341270673599,-23.8043715685224));
#30668=CARTESIAN_POINT('Ctrl Pts',(-22.408474710319,20.536532682202,-23.8039689420992));
#30669=CARTESIAN_POINT('Ctrl Pts',(-22.3983656136364,20.5403870578628,-23.803328218135));
#30670=CARTESIAN_POINT('Ctrl Pts',(-22.3946214105764,20.5418226498031,-23.8030905238647));
#30671=CARTESIAN_POINT('Ctrl Pts',(-22.3861982872293,20.5450702653078,-23.8025549251685));
#30672=CARTESIAN_POINT('Ctrl Pts',(-22.381520906744,20.5468862325729,-23.8022568995735));
#30673=CARTESIAN_POINT('Ctrl Pts',(-22.3703978204451,20.5512346285788,-23.8015467164951));
#30674=CARTESIAN_POINT('Ctrl Pts',(-22.3639560170771,20.5537769183789,-23.8011342522416));
#30675=CARTESIAN_POINT('Ctrl Pts',(-22.3556000050665,20.557105828695,-23.8005976785059));
#30676=CARTESIAN_POINT('Ctrl Pts',(-22.353678257408,20.5578735698746,-23.8004741689376));
#30677=CARTESIAN_POINT('Ctrl Pts',(-22.3476820297402,20.5602757720516,-23.8000884617111));
#30678=CARTESIAN_POINT('Ctrl Pts',(-22.3436101607425,20.5619167032242,-23.7998260581191));
#30679=CARTESIAN_POINT('Ctrl Pts',(-22.3381046787364,20.5641484562573,-23.7994706115027));
#30680=CARTESIAN_POINT('Ctrl Pts',(-22.3366681078595,20.5647320053899,-23.7993778025879));
#30681=CARTESIAN_POINT('Ctrl Pts',(-22.331470850864,20.5668475530221,-23.7990418165322));
#30682=CARTESIAN_POINT('Ctrl Pts',(-22.3277126509722,20.5683856178107,-23.7987984439021));
#30683=CARTESIAN_POINT('Ctrl Pts',(-22.3142021397951,20.5739447069637,-23.7979220204694));
#30684=CARTESIAN_POINT('Ctrl Pts',(-22.3044667538371,20.5780064734786,-23.7972876482053));
#30685=CARTESIAN_POINT('Ctrl Pts',(-22.2709709904118,20.5921749464184,-23.7950950191172));
#30686=CARTESIAN_POINT('Ctrl Pts',(-22.2473127128763,20.6025191599446,-23.7935289351613));
#30687=CARTESIAN_POINT('Ctrl Pts',(-22.2176177406058,20.6159301530916,-23.7915402977232));
#30688=CARTESIAN_POINT('Ctrl Pts',(-22.2114624926143,20.6187333797618,-23.7911268341268));
#30689=CARTESIAN_POINT('Ctrl Pts',(-22.2017611015577,20.6231885199193,-23.7904731684279));
#30690=CARTESIAN_POINT('Ctrl Pts',(-22.1982090397507,20.6248275605389,-23.7902334114089));
#30691=CARTESIAN_POINT('Ctrl Pts',(-22.1916569267781,20.6278654078197,-23.7897903695151));
#30692=CARTESIAN_POINT('Ctrl Pts',(-22.1886560260014,20.629262378503,-23.789587148441));
#30693=CARTESIAN_POINT('Ctrl Pts',(-22.1820206347767,20.6323637138716,-23.7891371202448));
#30694=CARTESIAN_POINT('Ctrl Pts',(-22.1783871700797,20.6340702489337,-23.7888902380685));
#30695=CARTESIAN_POINT('Ctrl Pts',(-22.1681836681901,20.6388858336101,-23.7881956664484));
#30696=CARTESIAN_POINT('Ctrl Pts',(-22.1616209776259,20.6420103134738,-23.7877474411647));
#30697=CARTESIAN_POINT('Ctrl Pts',(-22.1219007421649,20.6610861127146,-23.7850254711747));
#30698=CARTESIAN_POINT('Ctrl Pts',(-22.0890089303692,20.6775815815664,-23.7827327932335));
#30699=CARTESIAN_POINT('Ctrl Pts',(-21.9932549035333,20.727672918416,-23.775940772644));
#30700=CARTESIAN_POINT('Ctrl Pts',(-21.931219655381,20.7627933742059,-23.7713883736102));
#30701=CARTESIAN_POINT('Ctrl Pts',(-21.7501365379864,20.8733961698955,-23.757634152848));
#30702=CARTESIAN_POINT('Ctrl Pts',(-21.6348297273714,20.9546551705515,-23.7482446119146));
#30703=CARTESIAN_POINT('Ctrl Pts',(-21.3604613216403,21.1762710365889,-23.7244600478107));
#30704=CARTESIAN_POINT('Ctrl Pts',(-21.2092161194307,21.325273779263,-23.7099592694294));
#30705=CARTESIAN_POINT('Ctrl Pts',(-21.0691689069866,21.493461026055,-23.6957428109769));
#30706=CARTESIAN_POINT('Ctrl Pts',(-21.0646760818302,21.4988927475438,-23.695285834948));
#30707=CARTESIAN_POINT('Ctrl Pts',(-21.0555852536157,21.5099570628334,-23.69435942076));
#30708=CARTESIAN_POINT('Ctrl Pts',(-21.0509884134667,21.515590570128,-23.6938900453711));
#30709=CARTESIAN_POINT('Ctrl Pts',(-21.0421924103202,21.5264450113449,-23.6929901874747));
#30710=CARTESIAN_POINT('Ctrl Pts',(-21.0379903899416,21.5316635729054,-23.6925595477772));
#30711=CARTESIAN_POINT('Ctrl Pts',(-21.012864403665,21.5630679519031,-23.6899801450836));
#30712=CARTESIAN_POINT('Ctrl Pts',(-20.9923327208649,21.5895670576824,-23.6878539924824));
#30713=CARTESIAN_POINT('Ctrl Pts',(-20.9691807075941,21.6204309316236,-23.6854395457123));
#30714=CARTESIAN_POINT('Ctrl Pts',(-20.9661536889331,21.6244861022082,-23.6851235257715));
#30715=CARTESIAN_POINT('Ctrl Pts',(-20.9617049419742,21.6304752791011,-23.6846585925624));
#30716=CARTESIAN_POINT('Ctrl Pts',(-20.9602758217878,21.6324037456707,-23.6845091626482));
#30717=CARTESIAN_POINT('Ctrl Pts',(-20.957731722874,21.6358448035968,-23.6842430197704));
#30718=CARTESIAN_POINT('Ctrl Pts',(-20.9566159126651,21.6373567734085,-23.6841262481696));
#30719=CARTESIAN_POINT('Ctrl Pts',(-20.9542697997638,21.6405416817682,-23.6838806299165));
#30720=CARTESIAN_POINT('Ctrl Pts',(-20.9530397944163,21.6422148297119,-23.6837518042901));
#30721=CARTESIAN_POINT('Ctrl Pts',(-20.9498312060558,21.6465882498758,-23.6834156044054));
#30722=CARTESIAN_POINT('Ctrl Pts',(-20.9478552051094,21.649290426987,-23.6832084113911));
#30723=CARTESIAN_POINT('Ctrl Pts',(-20.9391556064585,21.6612260964148,-23.682295551724));
#30724=CARTESIAN_POINT('Ctrl Pts',(-20.9324768054736,21.6704923654461,-23.6815929764616));
#30725=CARTESIAN_POINT('Ctrl Pts',(-20.7648079871324,21.9057453495876,-23.6639047990543));
#30726=CARTESIAN_POINT('Ctrl Pts',(-20.6335913016358,22.1515919264555,-23.6488142119931));
#30727=CARTESIAN_POINT('Ctrl Pts',(-20.4929026413639,22.5239732263405,-23.6264859908256));
#30728=CARTESIAN_POINT('Ctrl Pts',(-20.4566731781995,22.6389889467513,-23.6196667255412));
#30729=CARTESIAN_POINT('Ctrl Pts',(-20.4213715694493,22.7777648678965,-23.611349375747));
#30730=CARTESIAN_POINT('Ctrl Pts',(-20.4160060215637,22.7998312850777,-23.6100243919422));
#30731=CARTESIAN_POINT('Ctrl Pts',(-20.406786065273,22.8395744107522,-23.6076322084003));
#30732=CARTESIAN_POINT('Ctrl Pts',(-20.4028464228304,22.8572304648466,-23.6065674294376));
#30733=CARTESIAN_POINT('Ctrl Pts',(-20.3980831448805,22.8794565426786,-23.6052240434625));
#30734=CARTESIAN_POINT('Ctrl Pts',(-20.3971204060971,22.8839966497238,-23.6049494739503));
#30735=CARTESIAN_POINT('Ctrl Pts',(-20.3953438417585,22.892464714974,-23.6044370526568));
#30736=CARTESIAN_POINT('Ctrl Pts',(-20.3945275355068,22.8963921475972,-23.6041992737519));
#30737=CARTESIAN_POINT('Ctrl Pts',(-20.3927231901507,22.9051553447019,-23.6036684443759));
#30738=CARTESIAN_POINT('Ctrl Pts',(-20.3917389245447,22.9099918688072,-23.6033752837712));
#30739=CARTESIAN_POINT('Ctrl Pts',(-20.3893980467729,22.9216313356403,-23.6026693006691));
#30740=CARTESIAN_POINT('Ctrl Pts',(-20.3880522852024,22.9284364150007,-23.6022561582308));
#30741=CARTESIAN_POINT('Ctrl Pts',(-20.386356173301,22.9371610191565,-23.6017259640447));
#30742=CARTESIAN_POINT('Ctrl Pts',(-20.3859855739064,22.9390766247513,-23.6016095208772));
#30743=CARTESIAN_POINT('Ctrl Pts',(-20.3845509011245,22.9465286437605,-23.6011564127289));
#30744=CARTESIAN_POINT('Ctrl Pts',(-20.3834996210228,22.9520674860645,-23.6008193635447));
#30745=CARTESIAN_POINT('Ctrl Pts',(-20.3818845289956,22.9607004531195,-23.6002935988242));
#30746=CARTESIAN_POINT('Ctrl Pts',(-20.3813107001516,22.9637927103325,-23.6001051879877));
#30747=CARTESIAN_POINT('Ctrl Pts',(-20.3791000905458,22.9758032541401,-23.5993730464057));
#30748=CARTESIAN_POINT('Ctrl Pts',(-20.3774964349613,22.9847275317053,-23.5988283089596));
#30749=CARTESIAN_POINT('Ctrl Pts',(-20.371047878187,23.021504411815,-23.5965803086276));
#30750=CARTESIAN_POINT('Ctrl Pts',(-20.3665320274462,23.049412761456,-23.5948669746406));
#30751=CARTESIAN_POINT('Ctrl Pts',(-20.3614494646558,23.0836765682424,-23.5927532826252));
#30752=CARTESIAN_POINT('Ctrl Pts',(-20.360533583047,23.0899796151041,-23.592364035024));
#30753=CARTESIAN_POINT('Ctrl Pts',(-20.3590509169601,23.1004002314163,-23.5917197957695));
#30754=CARTESIAN_POINT('Ctrl Pts',(-20.3584733995894,23.1045162761006,-23.5914651446945));
#30755=CARTESIAN_POINT('Ctrl Pts',(-20.3574448583731,23.1119513305294,-23.5910048193579));
#30756=CARTESIAN_POINT('Ctrl Pts',(-20.3569910425335,23.1152699533436,-23.5907992338866));
#30757=CARTESIAN_POINT('Ctrl Pts',(-20.3560318986578,23.1223662892296,-23.5903593634743));
#30758=CARTESIAN_POINT('Ctrl Pts',(-20.3555280972335,23.1261442004075,-23.5901250305081));
#30759=CARTESIAN_POINT('Ctrl Pts',(-20.3542010158115,23.1362322828458,-23.5894988722143));
#30760=CARTESIAN_POINT('Ctrl Pts',(-20.3533897253129,23.1425439901125,-23.5891066679494));
#30761=CARTESIAN_POINT('Ctrl Pts',(-20.3495813288464,23.1728830685771,-23.5872192627774));
#30762=CARTESIAN_POINT('Ctrl Pts',(-20.3468364451308,23.196940792269,-23.5857161086511));
#30763=CARTESIAN_POINT('Ctrl Pts',(-20.3331476443629,23.3302376721122,-23.5773496685747));
#30764=CARTESIAN_POINT('Ctrl Pts',(-20.3275213050042,23.4399384600812,-23.5703199306854));
#30765=CARTESIAN_POINT('Ctrl Pts',(-20.3274657168425,23.7657667085965,-23.5490035681645));
#30766=CARTESIAN_POINT('Ctrl Pts',(-20.349157902338,23.9812695237662,-23.5342952087362));
#30767=CARTESIAN_POINT('Ctrl Pts',(-20.4242855499426,24.3504227763822,-23.5088742976067));
#30768=CARTESIAN_POINT('Ctrl Pts',(-20.4680713323199,24.5052996682065,-23.4981541099756));
#30769=CARTESIAN_POINT('Ctrl Pts',(-20.5264718386568,24.6651322124755,-23.4874519413867));
#30770=CARTESIAN_POINT('Ctrl Pts',(-20.529745103123,24.6739701392045,-23.4868614022524));
#30771=CARTESIAN_POINT('Ctrl Pts',(-20.5341928331809,24.6858193071609,-23.4860714414125));
#30772=CARTESIAN_POINT('Ctrl Pts',(-20.5353330843489,24.6888432100233,-23.4858700003323));
#30773=CARTESIAN_POINT('Ctrl Pts',(-20.5371268904546,24.6935787271738,-23.4855547892503));
#30774=CARTESIAN_POINT('Ctrl Pts',(-20.5377773556571,24.695291497392,-23.4854408333968));
#30775=CARTESIAN_POINT('Ctrl Pts',(-20.5390295541023,24.69858026695,-23.4852221218783));
#30776=CARTESIAN_POINT('Ctrl Pts',(-20.5396310602909,24.7001563382259,-23.4851173536515));
#30777=CARTESIAN_POINT('Ctrl Pts',(-20.5410586083286,24.7038880126808,-23.4848693978276));
#30778=CARTESIAN_POINT('Ctrl Pts',(-20.5418857280567,24.7060431988409,-23.4847262763112));
#30779=CARTESIAN_POINT('Ctrl Pts',(-20.5442921572474,24.7122934317031,-23.484311445562));
#30780=CARTESIAN_POINT('Ctrl Pts',(-20.5458775253894,24.716386163861,-23.4840401013514));
#30781=CARTESIAN_POINT('Ctrl Pts',(-20.5574004510024,24.745953879614,-23.482081816879));
#30782=CARTESIAN_POINT('Ctrl Pts',(-20.5676539074737,24.7713057071099,-23.4804136411855));
#30783=CARTESIAN_POINT('Ctrl Pts',(-20.6007665205555,24.8502703506694,-23.4752427358927));
#30784=CARTESIAN_POINT('Ctrl Pts',(-20.6247590735966,24.903398119426,-23.4718001964935));
#30785=CARTESIAN_POINT('Ctrl Pts',(-20.7324588542617,25.1256077120508,-23.45743864668));
#30786=CARTESIAN_POINT('Ctrl Pts',(-20.8294895028433,25.2878269320418,-23.4470296570714));
#30787=CARTESIAN_POINT('Ctrl Pts',(-21.0754982611935,25.6274963677508,-23.4235442770395));
#30788=CARTESIAN_POINT('Ctrl Pts',(-21.2304849904737,25.7992536462733,-23.4104254281309));
#30789=CARTESIAN_POINT('Ctrl Pts',(-21.4135859341381,25.9629265584005,-23.3955241237047));
#30790=CARTESIAN_POINT('Ctrl Pts',(-21.4247768227455,25.9727910984094,-23.3946157782963));
#30791=CARTESIAN_POINT('Ctrl Pts',(-21.4401940093273,25.98619197087,-23.3933674926352));
#30792=CARTESIAN_POINT('Ctrl Pts',(-21.4443616089297,25.9897957963171,-23.3930303611992));
#30793=CARTESIAN_POINT('Ctrl Pts',(-21.4509892080793,25.9954972049312,-23.3924947093769));
#30794=CARTESIAN_POINT('Ctrl Pts',(-21.4534431707852,25.9976018156644,-23.3922964800495));
#30795=CARTESIAN_POINT('Ctrl Pts',(-21.458207405974,26.0016753774308,-23.391911826622));
#30796=CARTESIAN_POINT('Ctrl Pts',(-21.4605173026228,26.003644764691,-23.3917254207921));
#30797=CARTESIAN_POINT('Ctrl Pts',(-21.4660234693189,26.0083258315441,-23.3912812916404));
#30798=CARTESIAN_POINT('Ctrl Pts',(-21.4692222480699,26.0110345395645,-23.3910234465167));
#30799=CARTESIAN_POINT('Ctrl Pts',(-21.4758587811278,26.0166321241154,-23.3904888387139));
#30800=CARTESIAN_POINT('Ctrl Pts',(-21.4792973052858,26.0195200700919,-23.3902120386211));
#30801=CARTESIAN_POINT('Ctrl Pts',(-21.498944167284,26.0359511626844,-23.3886315461787));
#30802=CARTESIAN_POINT('Ctrl Pts',(-21.5152789949966,26.0493416378965,-23.387321642926));
#30803=CARTESIAN_POINT('Ctrl Pts',(-21.5584549584209,26.0840311395242,-23.3838695119901));
#30804=CARTESIAN_POINT('Ctrl Pts',(-21.5855056430197,26.1050638992508,-23.3817167949403));
#30805=CARTESIAN_POINT('Ctrl Pts',(-21.7092023617559,26.1981155243112,-23.3719151217746));
#30806=CARTESIAN_POINT('Ctrl Pts',(-21.8094967939359,26.2651020372075,-23.3640769187142));
#30807=CARTESIAN_POINT('Ctrl Pts',(-21.9663631470339,26.3576013138764,-23.351998894681));
#30808=CARTESIAN_POINT('Ctrl Pts',(-22.0202990286664,26.3873549640467,-23.347877474289));
#30809=CARTESIAN_POINT('Ctrl Pts',(-22.0750361484425,26.4155368430821,-23.3437344129902));
#30810=CARTESIAN_POINT('Origin',(-23.5502525316942,23.5502525316942,-77.3107734492734));
#30811=CARTESIAN_POINT('',(-22.0750357083693,26.4155366165066,-21.8446295278275));
#30812=CARTESIAN_POINT('',(-22.0750360154714,26.4155367746208,-22.0897962101869));
#30813=CARTESIAN_POINT('',(-22.0750360153461,26.4155367745563,-77.3107734492734));
#30814=CARTESIAN_POINT('Ctrl Pts',(-22.0750357083693,26.4155366165066,-21.8446295278275));
#30815=CARTESIAN_POINT('Ctrl Pts',(-22.0175648871972,26.3859472565221,-21.8489280757192));
#30816=CARTESIAN_POINT('Ctrl Pts',(-21.9609748464247,26.3546239485576,-21.8532666299503));
#30817=CARTESIAN_POINT('Ctrl Pts',(-21.7998026708723,26.2589618161571,-21.8659034386297));
#30818=CARTESIAN_POINT('Ctrl Pts',(-21.6979264287397,26.1903412992165,-21.8742489937229));
#30819=CARTESIAN_POINT('Ctrl Pts',(-21.5244223507677,26.0584773150897,-21.8888979493505));
#30820=CARTESIAN_POINT('Ctrl Pts',(-21.4512157560001,25.9975422367158,-21.8952310941675));
#30821=CARTESIAN_POINT('Ctrl Pts',(-21.3558308332747,25.9107126436346,-21.9035866384558));
#30822=CARTESIAN_POINT('Ctrl Pts',(-21.3312099826078,25.8875819698615,-21.9057532493313));
#30823=CARTESIAN_POINT('Ctrl Pts',(-21.2941318082051,25.8516338354809,-21.9090251984061));
#30824=CARTESIAN_POINT('Ctrl Pts',(-21.2814105753201,25.8390934690216,-21.9101494660534));
#30825=CARTESIAN_POINT('Ctrl Pts',(-21.2660424491475,25.8236898054178,-21.9115089783301));
#30826=CARTESIAN_POINT('Ctrl Pts',(-21.2632959612886,25.8209269654747,-21.9117519931002));
#30827=CARTESIAN_POINT('Ctrl Pts',(-21.2590180584144,25.8166079578517,-21.9121305815918));
#30828=CARTESIAN_POINT('Ctrl Pts',(-21.2574832153539,25.8150552143436,-21.9122664274059));
#30829=CARTESIAN_POINT('Ctrl Pts',(-21.2547721363206,25.8123069363795,-21.9125064027904));
#30830=CARTESIAN_POINT('Ctrl Pts',(-21.2535952618458,25.8111120497052,-21.9126105833104));
#30831=CARTESIAN_POINT('Ctrl Pts',(-21.2510818220564,25.8085561536955,-21.9128330972335));
#30832=CARTESIAN_POINT('Ctrl Pts',(-21.2497455360575,25.8071948801547,-21.9129514083752));
#30833=CARTESIAN_POINT('Ctrl Pts',(-21.2458864310717,25.803256624501,-21.9132931155375));
#30834=CARTESIAN_POINT('Ctrl Pts',(-21.2433667176426,25.8006765826526,-21.9135162655098));
#30835=CARTESIAN_POINT('Ctrl Pts',(-21.2321827625733,25.7891863333612,-21.9145069439859));
#30836=CARTESIAN_POINT('Ctrl Pts',(-21.2235656232407,25.7802301245495,-21.9152708122574));
#30837=CARTESIAN_POINT('Ctrl Pts',(-21.213063906329,25.7691880394058,-21.9162027683702));
#30838=CARTESIAN_POINT('Ctrl Pts',(-21.2111301221775,25.7671494195417,-21.9163744217491));
#30839=CARTESIAN_POINT('Ctrl Pts',(-21.0368363059738,25.5829247099505,-21.9318498942574));
#30840=CARTESIAN_POINT('Ctrl Pts',(-20.8862975578017,25.3812101444086,-21.9456286065462));
#30841=CARTESIAN_POINT('Ctrl Pts',(-20.6817044623154,25.0275522702009,-21.9684852111726));
#30842=CARTESIAN_POINT('Ctrl Pts',(-20.6128721779985,24.8854578161312,-21.9773680046081));
#30843=CARTESIAN_POINT('Ctrl Pts',(-20.531997760293,24.6816458296823,-21.9901818120448));
#30844=CARTESIAN_POINT('Ctrl Pts',(-20.5109237958273,24.6237481151354,-21.9938278098427));
#30845=CARTESIAN_POINT('Ctrl Pts',(-20.4847155180432,24.5447712697004,-21.998826647149));
#30846=CARTESIAN_POINT('Ctrl Pts',(-20.4781148537225,24.5241902890543,-22.0001315745631));
#30847=CARTESIAN_POINT('Ctrl Pts',(-20.4687890124242,24.4940737252635,-22.0020450068197));
#30848=CARTESIAN_POINT('Ctrl Pts',(-20.4658999503546,24.484589203659,-22.0026481592239));
#30849=CARTESIAN_POINT('Ctrl Pts',(-20.4607996145595,24.4675638137298,-22.0037319302085));
#30850=CARTESIAN_POINT('Ctrl Pts',(-20.4585720599139,24.4600278743091,-22.004212013445));
#30851=CARTESIAN_POINT('Ctrl Pts',(-20.4552276040109,24.4485592567871,-22.0049432252287));
#30852=CARTESIAN_POINT('Ctrl Pts',(-20.4540905757563,24.4446324384933,-22.0051936954517));
#30853=CARTESIAN_POINT('Ctrl Pts',(-20.4520501340863,24.4375350878176,-22.0056465913305));
#30854=CARTESIAN_POINT('Ctrl Pts',(-20.4511441066211,24.4343653075644,-22.0058489313075));
#30855=CARTESIAN_POINT('Ctrl Pts',(-20.4492091566527,24.4275562712909,-22.0062837326579));
#30856=CARTESIAN_POINT('Ctrl Pts',(-20.4481817740777,24.4239165860908,-22.0065162439245));
#30857=CARTESIAN_POINT('Ctrl Pts',(-20.4454432491164,24.4141491451834,-22.0071404654883));
#30858=CARTESIAN_POINT('Ctrl Pts',(-20.4437438482596,24.4080181400019,-22.0075325577168));
#30859=CARTESIAN_POINT('Ctrl Pts',(-20.4364320871533,24.3813324296251,-22.0092403753001));
#30860=CARTESIAN_POINT('Ctrl Pts',(-20.4310055984136,24.3607277575227,-22.010562128267));
#30861=CARTESIAN_POINT('Ctrl Pts',(-20.4225719059793,24.3273646466107,-22.0127077012763));
#30862=CARTESIAN_POINT('Ctrl Pts',(-20.4194374659943,24.3146387899524,-22.0135273558651));
#30863=CARTESIAN_POINT('Ctrl Pts',(-20.4152862838243,24.2973309808365,-22.0146438920765));
#30864=CARTESIAN_POINT('Ctrl Pts',(-20.4142017659447,24.2927652781992,-22.0149385942929));
#30865=CARTESIAN_POINT('Ctrl Pts',(-20.4124757908339,24.2854278718688,-22.0154124711553));
#30866=CARTESIAN_POINT('Ctrl Pts',(-20.4118280219748,24.282657647047,-22.0155914441848));
#30867=CARTESIAN_POINT('Ctrl Pts',(-20.3361989812132,23.9572825500086,-22.0366198922923));
#30868=CARTESIAN_POINT('Ctrl Pts',(-20.3114089338969,23.6250972393798,-22.0592364297752));
#30869=CARTESIAN_POINT('Ctrl Pts',(-20.3480106217355,23.1642630480681,-22.0903078671484));
#30870=CARTESIAN_POINT('Ctrl Pts',(-20.3663846149854,23.0341763322658,-22.0990027326934));
#30871=CARTESIAN_POINT('Ctrl Pts',(-20.3957324201398,22.8904353686377,-22.1082785590399));
#30872=CARTESIAN_POINT('Ctrl Pts',(-20.3989289333594,22.8753337038302,-22.1092488839153));
#30873=CARTESIAN_POINT('Ctrl Pts',(-20.4030295934696,22.8566250010155,-22.1104452450256));
#30874=CARTESIAN_POINT('Ctrl Pts',(-20.4038315680157,22.8529961270202,-22.1106770318504));
#30875=CARTESIAN_POINT('Ctrl Pts',(-20.4051060258887,22.8472762769086,-22.1110419439171));
#30876=CARTESIAN_POINT('Ctrl Pts',(-20.405574318107,22.8451843854648,-22.1111753102482));
#30877=CARTESIAN_POINT('Ctrl Pts',(-20.4064544359313,22.8412711621274,-22.1114246211755));
#30878=CARTESIAN_POINT('Ctrl Pts',(-20.40686575448,22.8394497333201,-22.1115405939494));
#30879=CARTESIAN_POINT('Ctrl Pts',(-20.4077939194577,22.8353561317143,-22.1118010819986));
#30880=CARTESIAN_POINT('Ctrl Pts',(-20.4083116462021,22.8330841661825,-22.1119455453993));
#30881=CARTESIAN_POINT('Ctrl Pts',(-20.4096360125962,22.827301344428,-22.1123129755955));
#30882=CARTESIAN_POINT('Ctrl Pts',(-20.4104460778757,22.8237912649708,-22.1125357446594));
#30883=CARTESIAN_POINT('Ctrl Pts',(-20.4149794470467,22.8042970353988,-22.1137715756596));
#30884=CARTESIAN_POINT('Ctrl Pts',(-20.418819011948,22.7883397702469,-22.1147780218024));
#30885=CARTESIAN_POINT('Ctrl Pts',(-20.4993754225448,22.4644456521415,-22.1351142833348));
#30886=CARTESIAN_POINT('Ctrl Pts',(-20.621051568194,22.1694235763795,-22.1520694929666));
#30887=CARTESIAN_POINT('Ctrl Pts',(-20.8714887306837,21.750397995155,-22.1797157350128));
#30888=CARTESIAN_POINT('Ctrl Pts',(-20.9705435461472,21.6110926833709,-22.1896057440371));
#30889=CARTESIAN_POINT('Ctrl Pts',(-21.0871724161455,21.4719182519041,-22.2006152295505));
#30890=CARTESIAN_POINT('Ctrl Pts',(-21.0942354072341,21.4635764873746,-22.2012796590383));
#30891=CARTESIAN_POINT('Ctrl Pts',(-21.1068688271197,21.4488087530163,-22.2024641338348));
#30892=CARTESIAN_POINT('Ctrl Pts',(-21.1124225381399,21.4423685683158,-22.2029834888604));
#30893=CARTESIAN_POINT('Ctrl Pts',(-21.1207744198263,21.4327607302075,-22.2037625418691));
#30894=CARTESIAN_POINT('Ctrl Pts',(-21.1235534683156,21.4295764411664,-22.2040214439535));
#30895=CARTESIAN_POINT('Ctrl Pts',(-21.1285153287477,21.4239135675535,-22.2044831299231));
#30896=CARTESIAN_POINT('Ctrl Pts',(-21.1306957060931,21.421432849778,-22.2046858119029));
#30897=CARTESIAN_POINT('Ctrl Pts',(-21.1350221605338,21.4165256723932,-22.2050876031595));
#30898=CARTESIAN_POINT('Ctrl Pts',(-21.1371680906735,21.4140990877062,-22.2052867061481));
#30899=CARTESIAN_POINT('Ctrl Pts',(-21.1429960429109,21.4075289176097,-22.2058269319618));
#30900=CARTESIAN_POINT('Ctrl Pts',(-21.1466850904273,21.4033916037783,-22.2061683500741));
#30901=CARTESIAN_POINT('Ctrl Pts',(-21.1604887283589,21.3879908228006,-22.2074438725158));
#30902=CARTESIAN_POINT('Ctrl Pts',(-21.1706718442596,21.3767892877239,-22.2083808715917));
#30903=CARTESIAN_POINT('Ctrl Pts',(-21.3472310480382,21.1853004347746,-22.2245607577407));
#30904=CARTESIAN_POINT('Ctrl Pts',(-21.5335417821625,21.0245582558592,-22.2407268987342));
#30905=CARTESIAN_POINT('Ctrl Pts',(-21.8697469197049,20.795599693897,-22.2681856464191));
#30906=CARTESIAN_POINT('Ctrl Pts',(-22.0099122039671,20.7148397461718,-22.2791951621481));
#30907=CARTESIAN_POINT('Ctrl Pts',(-22.2174957794679,20.6151887535421,-22.2944537454993));
#30908=CARTESIAN_POINT('Ctrl Pts',(-22.2803870449141,20.5874357950079,-22.2989465243157));
#30909=CARTESIAN_POINT('Ctrl Pts',(-22.3710855609554,20.5508312101109,-22.3051968377004));
#30910=CARTESIAN_POINT('Ctrl Pts',(-22.3981962309251,20.5403140879318,-22.3070366580032));
#30911=CARTESIAN_POINT('Ctrl Pts',(-22.4296367207027,20.5286043459448,-22.3091345933972));
#30912=CARTESIAN_POINT('Ctrl Pts',(-22.4338300394943,20.5270525095698,-22.3094136733833));
#30913=CARTESIAN_POINT('Ctrl Pts',(-22.4401916452302,20.5247132885132,-22.3098359422587));
#30914=CARTESIAN_POINT('Ctrl Pts',(-22.4423575483699,20.5239195047966,-22.309979513793));
#30915=CARTESIAN_POINT('Ctrl Pts',(-22.4461086046771,20.5225493434977,-22.3102278187852));
#30916=CARTESIAN_POINT('Ctrl Pts',(-22.4476933551452,20.5219718859087,-22.3103326173423));
#30917=CARTESIAN_POINT('Ctrl Pts',(-22.45100106165,20.5207695515296,-22.3105511331885));
#30918=CARTESIAN_POINT('Ctrl Pts',(-22.4527240926247,20.5201449020917,-22.3106648365326));
#30919=CARTESIAN_POINT('Ctrl Pts',(-22.4574901314118,20.5184216713449,-22.3109790067883));
#30920=CARTESIAN_POINT('Ctrl Pts',(-22.4605342728149,20.5173261979826,-22.311179286718));
#30921=CARTESIAN_POINT('Ctrl Pts',(-22.4724754285981,20.5130493188071,-22.3119634273581));
#30922=CARTESIAN_POINT('Ctrl Pts',(-22.4813848822013,20.5099024213506,-22.3125452429396));
#30923=CARTESIAN_POINT('Ctrl Pts',(-22.6425551330899,20.453771695304,-22.3230138975153));
#30924=CARTESIAN_POINT('Ctrl Pts',(-22.7985906006926,20.4122391139406,-22.3322481636096));
#30925=CARTESIAN_POINT('Ctrl Pts',(-23.1883914644191,20.3392487310983,-22.3545822653536));
#30926=CARTESIAN_POINT('Ctrl Pts',(-23.4237180835813,20.3214020566671,-22.3674874568137));
#30927=CARTESIAN_POINT('Ctrl Pts',(-23.7499164386583,20.3324043209362,-22.3864177524965));
#30928=CARTESIAN_POINT('Ctrl Pts',(-23.8407644591052,20.3393315878012,-22.3917944468746));
#30929=CARTESIAN_POINT('Ctrl Pts',(-23.9464573630477,20.3519130184907,-22.398221937255));
#30930=CARTESIAN_POINT('Ctrl Pts',(-23.9617097791744,20.3538394121238,-22.3991536511769));
#30931=CARTESIAN_POINT('Ctrl Pts',(-23.984586234049,20.3568951782322,-22.4005575746691));
#30932=CARTESIAN_POINT('Ctrl Pts',(-23.9922211038699,20.3579429083177,-22.4010272113882));
#30933=CARTESIAN_POINT('Ctrl Pts',(-24.0045052592011,20.3596735710986,-22.4017846116739));
#30934=CARTESIAN_POINT('Ctrl Pts',(-24.0091569687946,20.3603393100713,-22.4020718311482));
#30935=CARTESIAN_POINT('Ctrl Pts',(-24.0180446190865,20.3616311272855,-22.4026213900905));
#30936=CARTESIAN_POINT('Ctrl Pts',(-24.0222808037251,20.3622554790288,-22.4028836743489));
#30937=CARTESIAN_POINT('Ctrl Pts',(-24.0297907524361,20.3633776325662,-22.403349269258));
#30938=CARTESIAN_POINT('Ctrl Pts',(-24.0330650235965,20.3638720419574,-22.4035524719394));
#30939=CARTESIAN_POINT('Ctrl Pts',(-24.0395184437997,20.3648566729222,-22.4039533852735));
#30940=CARTESIAN_POINT('Ctrl Pts',(-24.0426976331161,20.3653466097258,-22.4041510866695));
#30941=CARTESIAN_POINT('Ctrl Pts',(-24.0503412688073,20.3665362694543,-22.4046268907203));
#30942=CARTESIAN_POINT('Ctrl Pts',(-24.0548049787478,20.3672406229375,-22.4049051403399));
#30943=CARTESIAN_POINT('Ctrl Pts',(-24.0684727828529,20.3694268141911,-22.4057583418736));
#30944=CARTESIAN_POINT('Ctrl Pts',(-24.0776718795837,20.3709391935063,-22.4063342643318));
#30945=CARTESIAN_POINT('Ctrl Pts',(-24.1831985764392,20.3887589276751,-22.4129604248652));
#30946=CARTESIAN_POINT('Ctrl Pts',(-24.2787338466558,20.409396894292,-22.4191484314502));
#30947=CARTESIAN_POINT('Ctrl Pts',(-24.6562743756093,20.5091067539253,-22.4444034379211));
#30948=CARTESIAN_POINT('Ctrl Pts',(-24.9278407102093,20.622104443896,-22.4645516423158));
#30949=CARTESIAN_POINT('Ctrl Pts',(-25.2183526124583,20.7924453775195,-22.4870477004555));
#30950=CARTESIAN_POINT('Ctrl Pts',(-25.2558947877275,20.8155052021426,-22.4899708975063));
#30951=CARTESIAN_POINT('Ctrl Pts',(-25.3504179741635,20.876268856528,-22.4973518930931));
#30952=CARTESIAN_POINT('Ctrl Pts',(-25.406698315013,20.9150305344662,-22.5017668269316));
#30953=CARTESIAN_POINT('Ctrl Pts',(-25.4705533180176,20.9620710964141,-22.5067614536495));
#30954=CARTESIAN_POINT('Ctrl Pts',(-25.4793650304505,20.9686322599755,-22.5074503534089));
#30955=CARTESIAN_POINT('Ctrl Pts',(-25.4907789477068,20.9772220862221,-22.5083420659091));
#30956=CARTESIAN_POINT('Ctrl Pts',(-25.4934116919839,20.979209762197,-22.5085477054076));
#30957=CARTESIAN_POINT('Ctrl Pts',(-25.4976757873681,20.9824393707813,-22.5088806898453));
#30958=CARTESIAN_POINT('Ctrl Pts',(-25.499309004844,20.9836788174544,-22.5090082098281));
#30959=CARTESIAN_POINT('Ctrl Pts',(-25.5024427955972,20.9860617635761,-22.5092528558147));
#30960=CARTESIAN_POINT('Ctrl Pts',(-25.503943543149,20.9872050187607,-22.509369998168));
#30961=CARTESIAN_POINT('Ctrl Pts',(-25.5073929143402,20.9898375067354,-22.509639205631));
#30962=CARTESIAN_POINT('Ctrl Pts',(-25.5093408473018,20.9913276501934,-22.5097912059474));
#30963=CARTESIAN_POINT('Ctrl Pts',(-25.5153680517507,20.9959492994993,-22.5102614417154));
#30964=CARTESIAN_POINT('Ctrl Pts',(-25.5194415558037,20.9990883665801,-22.5105791430952));
#30965=CARTESIAN_POINT('Ctrl Pts',(-25.5527520741753,21.024884972679,-22.5131763694091));
#30966=CARTESIAN_POINT('Ctrl Pts',(-25.5816060543516,21.0480357387641,-22.5154214839654));
#30967=CARTESIAN_POINT('Ctrl Pts',(-25.84900541703,21.2702564431668,-22.5362520093319));
#30968=CARTESIAN_POINT('Ctrl Pts',(-26.0580176865049,21.5023700042413,-22.5528513493944));
#30969=CARTESIAN_POINT('Ctrl Pts',(-26.2867160089689,21.8449354740634,-22.576283474658));
#30970=CARTESIAN_POINT('Ctrl Pts',(-26.338858591901,21.9316073264418,-22.5821211116812));
#30971=CARTESIAN_POINT('Ctrl Pts',(-26.4175808921299,22.0775881193931,-22.5919299012059));
#30972=CARTESIAN_POINT('Ctrl Pts',(-26.4465953681807,22.135505322366,-22.595815165304));
#30973=CARTESIAN_POINT('Ctrl Pts',(-26.477391902091,22.2019039958053,-22.6002766210332));
#30974=CARTESIAN_POINT('Ctrl Pts',(-26.4809098412002,22.2095674828963,-22.6007916448927));
#30975=CARTESIAN_POINT('Ctrl Pts',(-26.4861461764844,22.2210934217465,-22.6015664247636));
#30976=CARTESIAN_POINT('Ctrl Pts',(-26.4878871345634,22.2249456340914,-22.6018254026813));
#30977=CARTESIAN_POINT('Ctrl Pts',(-26.4908671729878,22.231574277607,-22.602271091526));
#30978=CARTESIAN_POINT('Ctrl Pts',(-26.492109916119,22.2343490641126,-22.6024576761554));
#30979=CARTESIAN_POINT('Ctrl Pts',(-26.4946601511432,22.2400648763471,-22.6028420603));
#30980=CARTESIAN_POINT('Ctrl Pts',(-26.4959671672635,22.2430061098749,-22.6030398759272));
#30981=CARTESIAN_POINT('Ctrl Pts',(-26.499101432582,22.250087847935,-22.6035162155664));
#30982=CARTESIAN_POINT('Ctrl Pts',(-26.5009243666712,22.2542302451921,-22.6037948872714));
#30983=CARTESIAN_POINT('Ctrl Pts',(-26.5064867819824,22.2669427288128,-22.6046502295817));
#30984=CARTESIAN_POINT('Ctrl Pts',(-26.510197671278,22.2755252038144,-22.6052278774032));
#30985=CARTESIAN_POINT('Ctrl Pts',(-26.5527125970797,22.3750395778857,-22.6119281692793));
#30986=CARTESIAN_POINT('Ctrl Pts',(-26.5873460708224,22.4676855344679,-22.6181919371124));
#30987=CARTESIAN_POINT('Ctrl Pts',(-26.7071661627195,22.839505168941,-22.6434698477019));
#30988=CARTESIAN_POINT('Ctrl Pts',(-26.7585223642132,23.1280919144093,-22.663549565601));
#30989=CARTESIAN_POINT('Ctrl Pts',(-26.772136978605,23.4635554195908,-22.685975446283));
#30990=CARTESIAN_POINT('Ctrl Pts',(-26.7730207433517,23.50757800266,-22.6888966099604));
#30991=CARTESIAN_POINT('Ctrl Pts',(-26.7729868457769,23.5882685850411,-22.6941963218512));
#30992=CARTESIAN_POINT('Ctrl Pts',(-26.7723458367552,23.6249294294618,-22.6965835148852));
#30993=CARTESIAN_POINT('Ctrl Pts',(-26.7697304455335,23.7006004617766,-22.7014578437141));
#30994=CARTESIAN_POINT('Ctrl Pts',(-26.7676722180439,23.7396025834573,-22.7039410043959));
#30995=CARTESIAN_POINT('Ctrl Pts',(-26.7645354487264,23.7837694899968,-22.7067126891186));
#30996=CARTESIAN_POINT('Ctrl Pts',(-26.7641527835129,23.7889783426434,-22.7070389326534));
#30997=CARTESIAN_POINT('Ctrl Pts',(-26.7635705941746,23.7966479179911,-22.7075183363536));
#30998=CARTESIAN_POINT('Ctrl Pts',(-26.7633809050503,23.7991093449085,-22.707672047434));
#30999=CARTESIAN_POINT('Ctrl Pts',(-26.763041067835,23.8034539403822,-22.7079430981767));
#31000=CARTESIAN_POINT('Ctrl Pts',(-26.7628920921192,23.8053371964363,-22.7080605043695));
#31001=CARTESIAN_POINT('Ctrl Pts',(-26.7625785682289,23.8092567226198,-22.7083046749269));
#31002=CARTESIAN_POINT('Ctrl Pts',(-26.7624137401219,23.8112929635124,-22.7084314229993));
#31003=CARTESIAN_POINT('Ctrl Pts',(-26.7619803831732,23.8165839720135,-22.7087605071955));
#31004=CARTESIAN_POINT('Ctrl Pts',(-26.7617088420718,23.8198385009681,-22.7089626725282));
#31005=CARTESIAN_POINT('Ctrl Pts',(-26.7605272084,23.8337456877951,-22.7098254876719));
#31006=CARTESIAN_POINT('Ctrl Pts',(-26.7595690423382,23.8443943538945,-22.7104834483862));
#31007=CARTESIAN_POINT('Ctrl Pts',(-26.7433140402595,24.0155014967206,-22.7210153542654));
#31008=CARTESIAN_POINT('Ctrl Pts',(-26.716050787073,24.1746205193702,-22.7302416418802));
#31009=CARTESIAN_POINT('Ctrl Pts',(-26.6368572599461,24.491753814629,-22.7486447217964));
#31010=CARTESIAN_POINT('Ctrl Pts',(-26.5843980891989,24.649122148077,-22.7577918226948));
#31011=CARTESIAN_POINT('Ctrl Pts',(-26.4524351953961,24.962269297259,-22.7770511095293));
#31012=CARTESIAN_POINT('Ctrl Pts',(-26.3719053780031,25.1170062751248,-22.7871614493294));
#31013=CARTESIAN_POINT('Ctrl Pts',(-26.2731675812366,25.274196613392,-22.7984498549883));
#31014=CARTESIAN_POINT('Ctrl Pts',(-26.2670044420189,25.2838928104908,-22.7991504352792));
#31015=CARTESIAN_POINT('Ctrl Pts',(-26.2583870673388,25.2972913482219,-22.8001245255463));
#31016=CARTESIAN_POINT('Ctrl Pts',(-26.2559767762293,25.301021963064,-22.8003963952071));
#31017=CARTESIAN_POINT('Ctrl Pts',(-26.2518188720105,25.3074284152137,-22.8008643904304));
#31018=CARTESIAN_POINT('Ctrl Pts',(-26.2500749715508,25.3101066648225,-22.8010603768324));
#31019=CARTESIAN_POINT('Ctrl Pts',(-26.2464737765852,25.3156193617767,-22.8014644802799));
#31020=CARTESIAN_POINT('Ctrl Pts',(-26.2446159904745,25.3184534812498,-22.8016726155933));
#31021=CARTESIAN_POINT('Ctrl Pts',(-26.2402921494517,25.3250270193733,-22.8021562628185));
#31022=CARTESIAN_POINT('Ctrl Pts',(-26.2378227659446,25.3287642305224,-22.8024318997627));
#31023=CARTESIAN_POINT('Ctrl Pts',(-26.2299730619153,25.3405904389913,-22.8033062796746));
#31024=CARTESIAN_POINT('Ctrl Pts',(-26.2245639906524,25.3486602050435,-22.803906107217));
#31025=CARTESIAN_POINT('Ctrl Pts',(-26.1330121703658,25.483919506964,-22.8140140667162));
#31026=CARTESIAN_POINT('Ctrl Pts',(-26.0379341571727,25.6047945216122,-22.8238689787797));
#31027=CARTESIAN_POINT('Ctrl Pts',(-25.7002619683624,25.9761374762792,-22.8569896490296));
#31028=CARTESIAN_POINT('Ctrl Pts',(-25.4257097716327,26.1941305322913,-22.8814493374239));
#31029=CARTESIAN_POINT('Ctrl Pts',(-25.1106236739297,26.3700961466631,-22.9042155777417));
#31030=CARTESIAN_POINT('Ctrl Pts',(-25.0995940299229,26.3761713289563,-22.9050060958647));
#31031=CARTESIAN_POINT('Ctrl Pts',(-25.0853438738055,26.3839118744868,-22.9060189158784));
#31032=CARTESIAN_POINT('Ctrl Pts',(-25.0821559648528,26.3856365570787,-22.9062449479937));
#31033=CARTESIAN_POINT('Ctrl Pts',(-25.0772826362361,26.3882624462306,-22.9065896397084));
#31034=CARTESIAN_POINT('Ctrl Pts',(-25.0755993268697,26.3891675303647,-22.9067085475171));
#31035=CARTESIAN_POINT('Ctrl Pts',(-25.0724374616398,26.3908639824054,-22.9069316107981));
#31036=CARTESIAN_POINT('Ctrl Pts',(-25.0709590988323,26.3916556906217,-22.9070357878665));
#31037=CARTESIAN_POINT('Ctrl Pts',(-25.0675588621271,26.3934732069059,-22.9072751231185));
#31038=CARTESIAN_POINT('Ctrl Pts',(-25.0656365691545,26.3944982185858,-22.907410229711));
#31039=CARTESIAN_POINT('Ctrl Pts',(-25.0604631273468,26.3972500854708,-22.9077733081871));
#31040=CARTESIAN_POINT('Ctrl Pts',(-25.0572100441796,26.3989733271245,-22.9080010489538));
#31041=CARTESIAN_POINT('Ctrl Pts',(-25.0400204451453,26.4080414145497,-22.9092015126386));
#31042=CARTESIAN_POINT('Ctrl Pts',(-25.0260328507375,26.415289740652,-22.9101681701937));
#31043=CARTESIAN_POINT('Ctrl Pts',(-24.8859889699608,26.4865622623997,-22.9197507232165));
#31044=CARTESIAN_POINT('Ctrl Pts',(-24.755884463948,26.5423369241634,-22.9278866877654));
#31045=CARTESIAN_POINT('Ctrl Pts',(-24.3701408559078,26.6784349823802,-22.9509977928228));
#31046=CARTESIAN_POINT('Ctrl Pts',(-24.1076669459429,26.7356929347805,-22.9655919263457));
#31047=CARTESIAN_POINT('Ctrl Pts',(-23.8180432194035,26.761941063838,-22.9825954544098));
#31048=CARTESIAN_POINT('Ctrl Pts',(-23.7949319314773,26.763784394633,-22.9839575931272));
#31049=CARTESIAN_POINT('Ctrl Pts',(-23.7668247338159,26.7657212294362,-22.9856215356915));
#31050=CARTESIAN_POINT('Ctrl Pts',(-23.761845539337,26.7660527219462,-22.9859165832064));
#31051=CARTESIAN_POINT('Ctrl Pts',(-23.7528971413496,26.766627593538,-22.9864473455226));
#31052=CARTESIAN_POINT('Ctrl Pts',(-23.7489282126842,26.76687519372,-22.9866829393556));
#31053=CARTESIAN_POINT('Ctrl Pts',(-23.7323990068503,26.7678756531333,-22.9876648783597));
#31054=CARTESIAN_POINT('Ctrl Pts',(-23.7198349504412,26.7685622878976,-22.9884131207696));
#31055=CARTESIAN_POINT('Ctrl Pts',(-23.7058963963234,26.7692421921015,-22.9892453970211));
#31056=CARTESIAN_POINT('Ctrl Pts',(-23.7045254307468,26.7693081880965,-22.9893272812253));
#31057=CARTESIAN_POINT('Ctrl Pts',(-23.6580778014003,26.7715143589604,-22.9921022723057));
#31058=CARTESIAN_POINT('Ctrl Pts',(-23.6129630348448,26.7727082921353,-22.9948231097119));
#31059=CARTESIAN_POINT('Ctrl Pts',(-23.5603646302011,26.7729953366416,-22.9980295912592));
#31060=CARTESIAN_POINT('Ctrl Pts',(-23.5528894548801,26.7730101221017,-22.9984860944758));
#31061=CARTESIAN_POINT('Ctrl Pts',(-23.5409690229497,26.7729922264102,-22.9992153727805));
#31062=CARTESIAN_POINT('Ctrl Pts',(-23.5365237372036,26.7729763553131,-22.9994876200081));
#31063=CARTESIAN_POINT('Ctrl Pts',(-23.5286829597378,26.7729321382073,-22.9999683370897));
#31064=CARTESIAN_POINT('Ctrl Pts',(-23.5252874461512,26.7729076229246,-23.000176686377));
#31065=CARTESIAN_POINT('Ctrl Pts',(-23.5182719947586,26.7728458838134,-23.0006075110921));
#31066=CARTESIAN_POINT('Ctrl Pts',(-23.5146520696526,26.7728079268422,-23.0008300092449));
#31067=CARTESIAN_POINT('Ctrl Pts',(-23.505394846672,26.7726952597143,-23.0013995068685));
#31068=CARTESIAN_POINT('Ctrl Pts',(-23.4997576840611,26.7726118563182,-23.0017467788382));
#31069=CARTESIAN_POINT('Ctrl Pts',(-23.4771811972381,26.7722185743032,-23.0031395164502));
#31070=CARTESIAN_POINT('Ctrl Pts',(-23.4602444537164,26.771789917463,-23.0041887047578));
#31071=CARTESIAN_POINT('Ctrl Pts',(-23.2428367908804,26.7645717116391,-23.0177142215618));
#31072=CARTESIAN_POINT('Ctrl Pts',(-23.0434595817204,26.739215704591,-23.0307904312862));
#31073=CARTESIAN_POINT('Ctrl Pts',(-22.6068056477271,26.6416894557977,-23.0607760366606));
#31074=CARTESIAN_POINT('Ctrl Pts',(-22.3728339085912,26.5603625911807,-23.0777932701458));
#31075=CARTESIAN_POINT('Ctrl Pts',(-22.125143031498,26.4409218748691,-23.0956529254266));
#31076=CARTESIAN_POINT('Ctrl Pts',(-22.1000060320639,26.4283928048774,-23.0974625602433));
#31077=CARTESIAN_POINT('Ctrl Pts',(-22.0750360144199,26.4155367740794,-23.0992549867839));
#31078=CARTESIAN_POINT('',(-26.7730012443091,23.5473068706377,-22.9355715880467));
#31079=CARTESIAN_POINT('Ctrl Pts',(-22.0750361484425,26.4155368430821,-23.3437344129902));
#31080=CARTESIAN_POINT('Ctrl Pts',(-22.1543302484992,26.4563620955829,-23.3377326299496));
#31081=CARTESIAN_POINT('Ctrl Pts',(-22.2353057299858,26.4938889063458,-23.3316846705842));
#31082=CARTESIAN_POINT('Ctrl Pts',(-22.3515899437915,26.5420189682118,-23.3231716910793));
#31083=CARTESIAN_POINT('Ctrl Pts',(-22.3856604926154,26.5554453451948,-23.3206978419997));
#31084=CARTESIAN_POINT('Ctrl Pts',(-22.5584381225785,26.6201531651689,-23.3082736710153));
#31085=CARTESIAN_POINT('Ctrl Pts',(-22.7003488752546,26.6624320289286,-23.2984514763994));
#31086=CARTESIAN_POINT('Ctrl Pts',(-22.8538398457921,26.6968721597427,-23.2885584840002));
#31087=CARTESIAN_POINT('Ctrl Pts',(-22.863009975991,26.6988876943567,-23.2879701886605));
#31088=CARTESIAN_POINT('Ctrl Pts',(-22.8753429596897,26.7015419568132,-23.2871827974317));
#31089=CARTESIAN_POINT('Ctrl Pts',(-22.8784980352251,26.7022160257628,-23.2869816983835));
#31090=CARTESIAN_POINT('Ctrl Pts',(-22.8834453200635,26.7032652271434,-23.2866668972446));
#31091=CARTESIAN_POINT('Ctrl Pts',(-22.8852368348243,26.7036435696253,-23.2865530101173));
#31092=CARTESIAN_POINT('Ctrl Pts',(-22.8886797905262,26.7043676084447,-23.2863343509322));
#31093=CARTESIAN_POINT('Ctrl Pts',(-22.8903311697055,26.7047135324434,-23.2862295664448));
#31094=CARTESIAN_POINT('Ctrl Pts',(-22.8942448496883,26.705530145969,-23.2859814527794));
#31095=CARTESIAN_POINT('Ctrl Pts',(-22.8965073832397,26.7059996988398,-23.285838189936));
#31096=CARTESIAN_POINT('Ctrl Pts',(-22.9011945822367,26.7069671953348,-23.2855417545288));
#31097=CARTESIAN_POINT('Ctrl Pts',(-22.9036193214394,26.7074647800062,-23.2853886026682));
#31098=CARTESIAN_POINT('Ctrl Pts',(-22.9171067210718,26.7102163618196,-23.2845377942743));
#31099=CARTESIAN_POINT('Ctrl Pts',(-22.9281807773505,26.7124150459538,-23.2838432832541));
#31100=CARTESIAN_POINT('Ctrl Pts',(-23.0275484942144,26.7316016730653,-23.2776459162308));
#31101=CARTESIAN_POINT('Ctrl Pts',(-23.1165147249962,26.7449476238273,-23.2723407839918));
#31102=CARTESIAN_POINT('Ctrl Pts',(-23.3539589562832,26.7704623974839,-23.2585493413111));
#31103=CARTESIAN_POINT('Ctrl Pts',(-23.502919957518,26.7760931610045,-23.2502687653335));
#31104=CARTESIAN_POINT('Ctrl Pts',(-23.8247403312459,26.7659533045394,-23.2322743890422));
#31105=CARTESIAN_POINT('Ctrl Pts',(-23.9970063058847,26.7465752787333,-23.2225672313433));
#31106=CARTESIAN_POINT('Ctrl Pts',(-24.1946127648312,26.7080549793497,-23.2108064143308));
#31107=CARTESIAN_POINT('Ctrl Pts',(-24.2222815075146,26.7022825754645,-23.2091456565943));
#31108=CARTESIAN_POINT('Ctrl Pts',(-24.2606535970744,26.6937489802295,-23.2068210019945));
#31109=CARTESIAN_POINT('Ctrl Pts',(-24.2714245182402,26.6912954408591,-23.2061661179996));
#31110=CARTESIAN_POINT('Ctrl Pts',(-24.3341411064715,26.676669456014,-23.2023386694301));
#31111=CARTESIAN_POINT('Ctrl Pts',(-24.3857882501499,26.6632645189796,-23.1991296349649));
#31112=CARTESIAN_POINT('Ctrl Pts',(-24.4454922574151,26.6461756606216,-23.1953451808447));
#31113=CARTESIAN_POINT('Ctrl Pts',(-24.4538979290822,26.6437326399436,-23.1948106341046));
#31114=CARTESIAN_POINT('Ctrl Pts',(-24.466410427428,26.6400406631838,-23.1940122927583));
#31115=CARTESIAN_POINT('Ctrl Pts',(-24.4705249293541,26.6388176841933,-23.1937493487763));
#31116=CARTESIAN_POINT('Ctrl Pts',(-24.4778588634135,26.6366218172976,-23.1932798998479));
#31117=CARTESIAN_POINT('Ctrl Pts',(-24.481079245029,26.6356521011775,-23.193073499146));
#31118=CARTESIAN_POINT('Ctrl Pts',(-24.4878652416896,26.6335971215827,-23.1926380150344));
#31119=CARTESIAN_POINT('Ctrl Pts',(-24.4914305016391,26.6325107107966,-23.1924088942194));
#31120=CARTESIAN_POINT('Ctrl Pts',(-24.5008419682279,26.6296249842234,-23.1918032074181));
#31121=CARTESIAN_POINT('Ctrl Pts',(-24.5066849298983,26.6278152110047,-23.1914262981945));
#31122=CARTESIAN_POINT('Ctrl Pts',(-24.5326560747106,26.6196899184631,-23.1897470502037));
#31123=CARTESIAN_POINT('Ctrl Pts',(-24.5527267470269,26.6131936029746,-23.18843876967));
#31124=CARTESIAN_POINT('Ctrl Pts',(-24.6051755161301,26.5956466713365,-23.1849916190427));
#31125=CARTESIAN_POINT('Ctrl Pts',(-24.6374432663421,26.5842769432619,-23.1828422959884));
#31126=CARTESIAN_POINT('Ctrl Pts',(-24.7822700051024,26.5306394234577,-23.173063048558));
#31127=CARTESIAN_POINT('Ctrl Pts',(-24.8925793726503,26.4826109666879,-23.1652448269617));
#31128=CARTESIAN_POINT('Ctrl Pts',(-25.0594956457667,26.3985414361393,-23.1528508555248));
#31129=CARTESIAN_POINT('Ctrl Pts',(-25.118105459658,26.3667043831666,-23.1483854720304));
#31130=CARTESIAN_POINT('Ctrl Pts',(-25.2345253596786,26.2987041348952,-23.1393054382843));
#31131=CARTESIAN_POINT('Ctrl Pts',(-25.2922616240397,26.2624776812719,-23.1346918548936));
#31132=CARTESIAN_POINT('Ctrl Pts',(-25.5132768620722,26.1138320632949,-23.1166628307839));
#31133=CARTESIAN_POINT('Ctrl Pts',(-25.6672141940529,25.9882635002258,-23.1032677765712));
#31134=CARTESIAN_POINT('Ctrl Pts',(-25.816888091021,25.8412379422775,-23.0900453799172));
#31135=CARTESIAN_POINT('Ctrl Pts',(-25.8250826529763,25.8331013745339,-23.0893208530978));
#31136=CARTESIAN_POINT('Ctrl Pts',(-25.8357071810506,25.822438019662,-23.0883809011256));
#31137=CARTESIAN_POINT('Ctrl Pts',(-25.8381768742783,25.8199512008762,-23.0881623662984));
#31138=CARTESIAN_POINT('Ctrl Pts',(-25.8419701397486,25.8161191493069,-23.0878266569877));
#31139=CARTESIAN_POINT('Ctrl Pts',(-25.843296585398,25.814776784533,-23.087709254111));
#31140=CARTESIAN_POINT('Ctrl Pts',(-25.8459315579267,25.8121054997849,-23.0874760147539));
#31141=CARTESIAN_POINT('Ctrl Pts',(-25.8472401028373,25.8107766166778,-23.08736017714));
#31142=CARTESIAN_POINT('Ctrl Pts',(-25.8501557972171,25.807810459026,-23.0871020466033));
#31143=CARTESIAN_POINT('Ctrl Pts',(-25.8517623485075,25.8061726076749,-23.0869598013957));
#31144=CARTESIAN_POINT('Ctrl Pts',(-25.8550825182506,25.8027805136235,-23.0866657966029));
#31145=CARTESIAN_POINT('Ctrl Pts',(-25.8567958869196,25.801026026932,-23.0865140567519));
#31146=CARTESIAN_POINT('Ctrl Pts',(-25.8612325391934,25.7964725160589,-23.0861210815517));
#31147=CARTESIAN_POINT('Ctrl Pts',(-25.8639527508269,25.7936704841905,-23.0858800856075));
#31148=CARTESIAN_POINT('Ctrl Pts',(-25.8986375582182,25.757812219905,-23.0828063999308));
#31149=CARTESIAN_POINT('Ctrl Pts',(-25.9298982345772,25.7240783926522,-23.0800274411334));
#31150=CARTESIAN_POINT('Ctrl Pts',(-26.0296733339258,25.6116768480862,-23.0710829798858));
#31151=CARTESIAN_POINT('Ctrl Pts',(-26.0950967377604,25.5303458303321,-23.065096452255));
#31152=CARTESIAN_POINT('Ctrl Pts',(-26.1802537802978,25.4132733357397,-23.0569082472821));
#31153=CARTESIAN_POINT('Ctrl Pts',(-26.2034254583523,25.3801231825796,-23.054634621974));
#31154=CARTESIAN_POINT('Ctrl Pts',(-26.2498064384664,25.3110351796392,-23.0499700512583));
#31155=CARTESIAN_POINT('Ctrl Pts',(-26.2729363593846,25.2750538657302,-23.0475803555466));
#31156=CARTESIAN_POINT('Ctrl Pts',(-26.435163333622,25.0112919297063,-23.0302782132406));
#31157=CARTESIAN_POINT('Ctrl Pts',(-26.5461824979433,24.7675133211699,-23.0153178038806));
#31158=CARTESIAN_POINT('Ctrl Pts',(-26.6309612708977,24.4966351834302,-22.9981181769861));
#31159=CARTESIAN_POINT('Ctrl Pts',(-26.6359096136664,24.4803744669891,-22.9970840759802));
#31160=CARTESIAN_POINT('Ctrl Pts',(-26.6423775040256,24.4585005795346,-22.9956905973267));
#31161=CARTESIAN_POINT('Ctrl Pts',(-26.6440108870025,24.452921130451,-22.9953349486562));
#31162=CARTESIAN_POINT('Ctrl Pts',(-26.6465459070653,24.4441740845337,-22.9947770511933));
#31163=CARTESIAN_POINT('Ctrl Pts',(-26.6474578064806,24.441009454038,-22.9945751379643));
#31164=CARTESIAN_POINT('Ctrl Pts',(-26.6491965033219,24.4349405792356,-22.9941877902089));
#31165=CARTESIAN_POINT('Ctrl Pts',(-26.6500240734706,24.4320365582249,-22.9940023811295));
#31166=CARTESIAN_POINT('Ctrl Pts',(-26.6519547515945,24.4252253225707,-22.993567372968));
#31167=CARTESIAN_POINT('Ctrl Pts',(-26.6530545582607,24.4213171845209,-22.9933176665351));
#31168=CARTESIAN_POINT('Ctrl Pts',(-26.6553061656553,24.4132577764344,-22.9928024917822));
#31169=CARTESIAN_POINT('Ctrl Pts',(-26.6564570326851,24.409106256119,-22.9925369935806));
#31170=CARTESIAN_POINT('Ctrl Pts',(-26.6593963035188,24.3984202431167,-22.9918532762552));
#31171=CARTESIAN_POINT('Ctrl Pts',(-26.6611724261289,24.3918824205768,-22.9914346580724));
#31172=CARTESIAN_POINT('Ctrl Pts',(-26.67547282118,24.3385795774857,-22.9880190548841));
#31173=CARTESIAN_POINT('Ctrl Pts',(-26.6869619014288,24.2915455281374,-22.9849886551368));
#31174=CARTESIAN_POINT('Ctrl Pts',(-26.7478713260265,24.0153429171023,-22.9670848689232));
#31175=CARTESIAN_POINT('Ctrl Pts',(-26.7732153269194,23.7816376651046,-22.9514286117027));
#31176=CARTESIAN_POINT('Ctrl Pts',(-26.7730011860229,23.5473074472221,-22.935571525082));
#31177=CARTESIAN_POINT('Ctrl Pts',(-26.7730011855023,23.547306877561,-22.9355714865331));
#31178=CARTESIAN_POINT('Ctrl Pts',(-26.7728003775001,23.3276090822578,-22.9207045733762));
#31179=CARTESIAN_POINT('Ctrl Pts',(-26.7501347209482,23.1084750127466,-22.9057600612752));
#31180=CARTESIAN_POINT('Ctrl Pts',(-26.7037367314502,22.8856348350834,-22.8914137520856));
#31181=CARTESIAN_POINT('Ctrl Pts',(-26.7021072044601,22.8779494709175,-22.8909200922095));
#31182=CARTESIAN_POINT('Ctrl Pts',(-26.6996019988161,22.8663434492828,-22.8901763659116));
#31183=CARTESIAN_POINT('Ctrl Pts',(-26.6987470804627,22.862418412263,-22.8899251521466));
#31184=CARTESIAN_POINT('Ctrl Pts',(-26.6973483902526,22.8560540981733,-22.889518326956));
#31185=CARTESIAN_POINT('Ctrl Pts',(-26.6968091192338,22.8536138523415,-22.8893624610396));
#31186=CARTESIAN_POINT('Ctrl Pts',(-26.6957620427135,22.8489017652036,-22.8890617239284));
#31187=CARTESIAN_POINT('Ctrl Pts',(-26.6952546133762,22.8466298431258,-22.888916831252));
#31188=CARTESIAN_POINT('Ctrl Pts',(-26.6943357363154,22.8425365919231,-22.8886559780684));
#31189=CARTESIAN_POINT('Ctrl Pts',(-26.6939251683346,22.8407150748359,-22.8885399670474));
#31190=CARTESIAN_POINT('Ctrl Pts',(-26.6930394300623,22.8368012879112,-22.8882908516684));
#31191=CARTESIAN_POINT('Ctrl Pts',(-26.6925637547108,22.8347091412707,-22.8881577772999));
#31192=CARTESIAN_POINT('Ctrl Pts',(-26.6912776931448,22.8290787151152,-22.8877998895869));
#31193=CARTESIAN_POINT('Ctrl Pts',(-26.6904634146712,22.8255413138112,-22.8875753013522));
#31194=CARTESIAN_POINT('Ctrl Pts',(-26.6866976995619,22.8093077467031,-22.886545801855));
#31195=CARTESIAN_POINT('Ctrl Pts',(-26.6836751761912,22.7966279500662,-22.8857449440323));
#31196=CARTESIAN_POINT('Ctrl Pts',(-26.6292224870703,22.5741855080108,-22.8717473548527));
#31197=CARTESIAN_POINT('Ctrl Pts',(-26.5569019811303,22.3700604504854,-22.8596943652166));
#31198=CARTESIAN_POINT('Ctrl Pts',(-26.4445321286364,22.1319815248712,-22.8449824598423));
#31199=CARTESIAN_POINT('Ctrl Pts',(-26.423442388395,22.0897296614306,-22.8423459273967));
#31200=CARTESIAN_POINT('Ctrl Pts',(-26.3794800720187,22.0062943992213,-22.8370644887152));
#31201=CARTESIAN_POINT('Ctrl Pts',(-26.3566178877872,21.9651189217063,-22.8344202774518));
#31202=CARTESIAN_POINT('Ctrl Pts',(-26.2645595977279,21.8075574713107,-22.8241134919961));
#31203=CARTESIAN_POINT('Ctrl Pts',(-26.1889650717893,21.695086933009,-22.8163419401613));
#31204=CARTESIAN_POINT('Ctrl Pts',(-26.0727388540961,21.5436985151804,-22.8050152105764));
#31205=CARTESIAN_POINT('Ctrl Pts',(-26.037820496943,21.500569309277,-22.8016813687809));
#31206=CARTESIAN_POINT('Ctrl Pts',(-25.9975543344784,21.4533800059698,-22.7979029878526));
#31207=CARTESIAN_POINT('Ctrl Pts',(-25.9932856743992,21.4484082068935,-22.7975032399048));
#31208=CARTESIAN_POINT('Ctrl Pts',(-25.9852988997786,21.4391630419603,-22.7967567728127));
#31209=CARTESIAN_POINT('Ctrl Pts',(-25.9815846186726,21.4348863859484,-22.7964102131329));
#31210=CARTESIAN_POINT('Ctrl Pts',(-25.9754741377605,21.4278880782975,-22.795841027892));
#31211=CARTESIAN_POINT('Ctrl Pts',(-25.9730845743508,21.4251606267456,-22.7956186793406));
#31212=CARTESIAN_POINT('Ctrl Pts',(-25.9684499122763,21.4198885941401,-22.7951878793955));
#31213=CARTESIAN_POINT('Ctrl Pts',(-25.9662053868691,21.4173435136352,-22.7949794521609));
#31214=CARTESIAN_POINT('Ctrl Pts',(-25.9610206458468,21.4114831897512,-22.7944984654819));
#31215=CARTESIAN_POINT('Ctrl Pts',(-25.958077608958,21.4081704615493,-22.7942257877192));
#31216=CARTESIAN_POINT('Ctrl Pts',(-25.9488972246816,21.3978797022613,-22.7933762768347));
#31217=CARTESIAN_POINT('Ctrl Pts',(-25.9426363471087,21.3909228123472,-22.7927984518255));
#31218=CARTESIAN_POINT('Ctrl Pts',(-25.8892608807416,21.3321307638952,-22.7878850634165));
#31219=CARTESIAN_POINT('Ctrl Pts',(-25.840501389739,21.2818206595933,-22.7834794504178));
#31220=CARTESIAN_POINT('Ctrl Pts',(-25.7840972156411,21.2272961752618,-22.7784668403634));
#31221=CARTESIAN_POINT('Ctrl Pts',(-25.7780270773474,21.2214741228413,-22.7779284432822));
#31222=CARTESIAN_POINT('Ctrl Pts',(-25.7340156017128,21.1795909429222,-22.774032366782));
#31223=CARTESIAN_POINT('Ctrl Pts',(-25.6952251851088,21.1444367959534,-22.7706387021536));
#31224=CARTESIAN_POINT('Ctrl Pts',(-25.5514195601596,21.0203550600468,-22.7582038865294));
#31225=CARTESIAN_POINT('Ctrl Pts',(-25.441600349126,20.9372373757034,-22.7489728037558));
#31226=CARTESIAN_POINT('Ctrl Pts',(-25.2334901504785,20.7997361332994,-22.7321092390691));
#31227=CARTESIAN_POINT('Ctrl Pts',(-25.1370165606523,20.7429744920888,-22.7245139418115));
#31228=CARTESIAN_POINT('Ctrl Pts',(-24.9522924421158,20.6468597644665,-22.7105607750245));
#31229=CARTESIAN_POINT('Ctrl Pts',(-24.8648386668492,20.6062294232143,-22.7041847647031));
#31230=CARTESIAN_POINT('Ctrl Pts',(-24.7431982323136,20.5562197779224,-22.6957412806181));
#31231=CARTESIAN_POINT('Ctrl Pts',(-24.7104904515217,20.5433937393436,-22.6935116576367));
#31232=CARTESIAN_POINT('Ctrl Pts',(-24.6742869340785,20.5298756404884,-22.6910933781915));
#31233=CARTESIAN_POINT('Ctrl Pts',(-24.6709939802508,20.5286522092759,-22.6908738679139));
#31234=CARTESIAN_POINT('Ctrl Pts',(-24.6655533209831,20.5266409585791,-22.6905119383139));
#31235=CARTESIAN_POINT('Ctrl Pts',(-24.6634067758961,20.5258500412249,-22.6903693354379));
#31236=CARTESIAN_POINT('Ctrl Pts',(-24.6592164985863,20.5243111543888,-22.6900913369758));
#31237=CARTESIAN_POINT('Ctrl Pts',(-24.6571728479127,20.5235629684313,-22.6899559284568));
#31238=CARTESIAN_POINT('Ctrl Pts',(-24.6535530171437,20.5222418953493,-22.6897163965669));
#31239=CARTESIAN_POINT('Ctrl Pts',(-24.6519771563294,20.5216681715501,-22.6896122230664));
#31240=CARTESIAN_POINT('Ctrl Pts',(-24.6486026483565,20.5204425964479,-22.6893893721141));
#31241=CARTESIAN_POINT('Ctrl Pts',(-24.6468038735213,20.5197911184315,-22.6892707174961));
#31242=CARTESIAN_POINT('Ctrl Pts',(-24.6415868967398,20.5179068934318,-22.6889269743915));
#31243=CARTESIAN_POINT('Ctrl Pts',(-24.6381671745489,20.5166783202416,-22.6887021365802));
#31244=CARTESIAN_POINT('Ctrl Pts',(-24.6228108565534,20.5111906989171,-22.6876946447829));
#31245=CARTESIAN_POINT('Ctrl Pts',(-24.6108510645216,20.5069962249757,-22.6869158045601));
#31246=CARTESIAN_POINT('Ctrl Pts',(-24.4057015973698,20.4364035832047,-22.673650446958));
#31247=CARTESIAN_POINT('Ctrl Pts',(-24.2066202783038,20.3884401898799,-22.6621900667291));
#31248=CARTESIAN_POINT('Ctrl Pts',(-23.8381705600278,20.3360057895516,-22.6413801665487));
#31249=CARTESIAN_POINT('Ctrl Pts',(-23.6704426066887,20.3253758583211,-22.6320499743358));
#31250=CARTESIAN_POINT('Ctrl Pts',(-23.4013444491763,20.3293503723596,-22.6165610348933));
#31251=CARTESIAN_POINT('Ctrl Pts',(-23.3001660085322,20.3356237695569,-22.6106228766124));
#31252=CARTESIAN_POINT('Ctrl Pts',(-23.1675068071789,20.3501499757812,-22.6026025065283));
#31253=CARTESIAN_POINT('Ctrl Pts',(-23.1356110440366,20.3541262858049,-22.6006563674381));
#31254=CARTESIAN_POINT('Ctrl Pts',(-23.0987744492221,20.3592792226422,-22.5983865996417));
#31255=CARTESIAN_POINT('Ctrl Pts',(-23.0937696251778,20.3599913396232,-22.598077742359));
#31256=CARTESIAN_POINT('Ctrl Pts',(-23.084214182764,20.3613738921973,-22.5974871434444));
#31257=CARTESIAN_POINT('Ctrl Pts',(-23.0796632799685,20.362042300871,-22.5972054666355));
#31258=CARTESIAN_POINT('Ctrl Pts',(-23.0717426467467,20.3632229632732,-22.5967145252651));
#31259=CARTESIAN_POINT('Ctrl Pts',(-23.068372260814,20.3637308254487,-22.596505400408));
#31260=CARTESIAN_POINT('Ctrl Pts',(-23.0618754911809,20.3647203257555,-22.59610186453));
#31261=CARTESIAN_POINT('Ctrl Pts',(-23.0587489968988,20.3652012222272,-22.5959074772848));
#31262=CARTESIAN_POINT('Ctrl Pts',(-23.0513581515767,20.3663491742286,-22.5954475050245));
#31263=CARTESIAN_POINT('Ctrl Pts',(-23.0470944299762,20.3670201938672,-22.595181794229));
#31264=CARTESIAN_POINT('Ctrl Pts',(-23.0344255447255,20.3690400979818,-22.5943912155654));
#31265=CARTESIAN_POINT('Ctrl Pts',(-23.0260244132669,20.3704137140007,-22.5938655618335));
#31266=CARTESIAN_POINT('Ctrl Pts',(-22.9491108026677,20.3833024617702,-22.5890401656157));
#31267=CARTESIAN_POINT('Ctrl Pts',(-22.8809866417579,20.3969961071503,-22.5846713166027));
#31268=CARTESIAN_POINT('Ctrl Pts',(-22.8035803528494,20.4151769054354,-22.5795921230051));
#31269=CARTESIAN_POINT('Ctrl Pts',(-22.793809418934,20.4175201239353,-22.5789488741472));
#31270=CARTESIAN_POINT('Ctrl Pts',(-22.6197852984883,20.4601153770153,-22.567454718774));
#31271=CARTESIAN_POINT('Ctrl Pts',(-22.4589619049632,20.5131835509343,-22.5562123522961));
#31272=CARTESIAN_POINT('Ctrl Pts',(-22.1452239829338,20.6448586181898,-22.5332574517513));
#31273=CARTESIAN_POINT('Ctrl Pts',(-21.9929111308331,20.7235743234257,-22.5215786293772));
#31274=CARTESIAN_POINT('Ctrl Pts',(-21.7925713044868,20.8482402840512,-22.5059722793803));
#31275=CARTESIAN_POINT('Ctrl Pts',(-21.7386142739113,20.8841164647915,-22.5017446788919));
#31276=CARTESIAN_POINT('Ctrl Pts',(-21.6627523749587,20.9379246053243,-22.4958045927193));
#31277=CARTESIAN_POINT('Ctrl Pts',(-21.6399475185426,20.9545543737369,-22.494019492314));
#31278=CARTESIAN_POINT('Ctrl Pts',(-21.6138227119388,20.9741359403435,-22.4919779601419));
#31279=CARTESIAN_POINT('Ctrl Pts',(-21.6102877388902,20.9767969283644,-22.4917017924691));
#31280=CARTESIAN_POINT('Ctrl Pts',(-21.6049107665644,20.9808618756914,-22.4912818471056));
#31281=CARTESIAN_POINT('Ctrl Pts',(-21.6030648001827,20.982260540927,-22.4911376987684));
#31282=CARTESIAN_POINT('Ctrl Pts',(-21.5997339809453,20.9847899166991,-22.4908776447693));
#31283=CARTESIAN_POINT('Ctrl Pts',(-21.5982486065357,20.9859199241771,-22.4907616900062));
#31284=CARTESIAN_POINT('Ctrl Pts',(-21.5952732060118,20.9881875612122,-22.4905294496601));
#31285=CARTESIAN_POINT('Ctrl Pts',(-21.5937831969001,20.9893251959678,-22.4904131653077));
#31286=CARTESIAN_POINT('Ctrl Pts',(-21.589559629184,20.9925557636601,-22.4900835894483));
#31287=CARTESIAN_POINT('Ctrl Pts',(-21.5868284199234,20.9946517857352,-22.4898705171086));
#31288=CARTESIAN_POINT('Ctrl Pts',(-21.5753565679965,21.0034849172372,-22.4889757427796));
#31289=CARTESIAN_POINT('Ctrl Pts',(-21.5666470669536,21.0102626265829,-22.4882968888774));
#31290=CARTESIAN_POINT('Ctrl Pts',(-21.420835389869,21.1249402818868,-22.476936314317));
#31291=CARTESIAN_POINT('Ctrl Pts',(-21.2926606307792,21.243771533754,-22.4670111527853));
#31292=CARTESIAN_POINT('Ctrl Pts',(-21.0634568507896,21.4937810694765,-22.4479702786533));
#31293=CARTESIAN_POINT('Ctrl Pts',(-20.9616573277731,21.623493173148,-22.4388641258175));
#31294=CARTESIAN_POINT('Ctrl Pts',(-20.8057966314606,21.8568732588851,-22.4228995872353));
#31295=CARTESIAN_POINT('Ctrl Pts',(-20.7466379731331,21.9567303338069,-22.416187551869));
#31296=CARTESIAN_POINT('Ctrl Pts',(-20.6695108405527,22.1045616334265,-22.4062603688895));
#31297=CARTESIAN_POINT('Ctrl Pts',(-20.6470961287025,22.1501177809193,-22.403203094347));
#31298=CARTESIAN_POINT('Ctrl Pts',(-20.6224427318062,22.2033635380363,-22.3996252916015));
#31299=CARTESIAN_POINT('Ctrl Pts',(-20.6191442930036,22.2105567912829,-22.3991418581384));
#31300=CARTESIAN_POINT('Ctrl Pts',(-20.6141503931983,22.221554243623,-22.3984025956947));
#31301=CARTESIAN_POINT('Ctrl Pts',(-20.6124357412117,22.2253497376357,-22.3981474285246));
#31302=CARTESIAN_POINT('Ctrl Pts',(-20.60948558749,22.2319139807837,-22.3977060664247));
#31303=CARTESIAN_POINT('Ctrl Pts',(-20.6082466237093,22.2346811758869,-22.3975199908699));
#31304=CARTESIAN_POINT('Ctrl Pts',(-20.6056901292916,22.2404127154925,-22.3971345462204));
#31305=CARTESIAN_POINT('Ctrl Pts',(-20.6043731662223,22.243377308229,-22.3969351578765));
#31306=CARTESIAN_POINT('Ctrl Pts',(-20.601192031959,22.2505675457626,-22.3964515156698));
#31307=CARTESIAN_POINT('Ctrl Pts',(-20.5993324678859,22.2547952107367,-22.3961671041153));
#31308=CARTESIAN_POINT('Ctrl Pts',(-20.5924366759677,22.2705644842909,-22.3951060723345));
#31309=CARTESIAN_POINT('Ctrl Pts',(-20.5874590713919,22.2821314651509,-22.3943274492603));
#31310=CARTESIAN_POINT('Ctrl Pts',(-20.5034946782776,22.4804413446423,-22.3809716170596));
#31311=CARTESIAN_POINT('Ctrl Pts',(-20.4422520955118,22.6741620367655,-22.367778099392));
#31312=CARTESIAN_POINT('Ctrl Pts',(-20.3624362557347,23.0450987059174,-22.3423672900487));
#31313=CARTESIAN_POINT('Ctrl Pts',(-20.3395352696603,23.2206387530685,-22.3302943600274));
#31314=CARTESIAN_POINT('Ctrl Pts',(-20.327205866074,23.4799053754935,-22.3129198699933));
#31315=CARTESIAN_POINT('Ctrl Pts',(-20.3264622318478,23.5627702893158,-22.3074387303705));
#31316=CARTESIAN_POINT('Ctrl Pts',(-20.3302413170015,23.690477912021,-22.2991867794028));
#31317=CARTESIAN_POINT('Ctrl Pts',(-20.3325087053473,23.7353486209164,-22.2963248488783));
#31318=CARTESIAN_POINT('Ctrl Pts',(-20.3360638022641,23.7850555623404,-22.2932067464514));
#31319=CARTESIAN_POINT('Ctrl Pts',(-20.3364251240258,23.7899503541195,-22.2929002614062));
#31320=CARTESIAN_POINT('Ctrl Pts',(-20.3369809966539,23.7972534262692,-22.2924438439408));
#31321=CARTESIAN_POINT('Ctrl Pts',(-20.3371670737936,23.7996623152657,-22.2922934362927));
#31322=CARTESIAN_POINT('Ctrl Pts',(-20.3374888482222,23.803767764672,-22.2920373387685));
#31323=CARTESIAN_POINT('Ctrl Pts',(-20.3376231805611,23.8054644269529,-22.2919315713571));
#31324=CARTESIAN_POINT('Ctrl Pts',(-20.3379014221426,23.8089436791239,-22.291714824714));
#31325=CARTESIAN_POINT('Ctrl Pts',(-20.3380454708194,23.8107262518686,-22.2916038537135));
#31326=CARTESIAN_POINT('Ctrl Pts',(-20.3383951746939,23.8150093554041,-22.2913374013672));
#31327=CARTESIAN_POINT('Ctrl Pts',(-20.3386022666777,23.8175097724529,-22.2911820016016));
#31328=CARTESIAN_POINT('Ctrl Pts',(-20.3393652236529,23.82659271338,-22.290618043041));
#31329=CARTESIAN_POINT('Ctrl Pts',(-20.3399384123775,23.8331738248032,-22.2902104571092));
#31330=CARTESIAN_POINT('Ctrl Pts',(-20.3498053285582,23.9425692388969,-22.283451818093));
#31331=CARTESIAN_POINT('Ctrl Pts',(-20.3640148350406,24.044892895086,-22.2773721968987));
#31332=CARTESIAN_POINT('Ctrl Pts',(-20.4146708024058,24.314025629629,-22.2616126796113));
#31333=CARTESIAN_POINT('Ctrl Pts',(-20.4594914831987,24.4789208250043,-22.2521857994242));
#31334=CARTESIAN_POINT('Ctrl Pts',(-20.5626956300021,24.766300823851,-22.2350806753798));
#31335=CARTESIAN_POINT('Ctrl Pts',(-20.6161365021468,24.8901140105494,-22.2274708141901));
#31336=CARTESIAN_POINT('Ctrl Pts',(-20.70999532912,25.0748208890429,-22.2154135129741));
#31337=CARTESIAN_POINT('Ctrl Pts',(-20.7449939674206,25.1382994065509,-22.2111345608755));
#31338=CARTESIAN_POINT('Ctrl Pts',(-20.7986062795056,25.2282273324524,-22.2048427136954));
#31339=CARTESIAN_POINT('Ctrl Pts',(-20.8155259359901,25.2556635847532,-22.2028911116017));
#31340=CARTESIAN_POINT('Ctrl Pts',(-20.8366097723268,25.2887315642404,-22.2004979539775));
#31341=CARTESIAN_POINT('Ctrl Pts',(-20.8403848566796,25.2946101655433,-22.2000709192453));
#31342=CARTESIAN_POINT('Ctrl Pts',(-20.8463251608539,25.3037946476477,-22.1994012165683));
#31343=CARTESIAN_POINT('Ctrl Pts',(-20.8484774125457,25.3071089243828,-22.199159033901));
#31344=CARTESIAN_POINT('Ctrl Pts',(-20.8522801172308,25.3129412387021,-22.1987319374245));
#31345=CARTESIAN_POINT('Ctrl Pts',(-20.8539280162127,25.3154609426574,-22.1985471195906));
#31346=CARTESIAN_POINT('Ctrl Pts',(-20.857694356812,25.3212022497634,-22.1981253098602));
#31347=CARTESIAN_POINT('Ctrl Pts',(-20.859815050979,25.3244223632524,-22.1978882334461));
#31348=CARTESIAN_POINT('Ctrl Pts',(-20.8655384417292,25.3330790384958,-22.1972495537734));
#31349=CARTESIAN_POINT('Ctrl Pts',(-20.8691518570501,25.3385084612617,-22.1968475467653));
#31350=CARTESIAN_POINT('Ctrl Pts',(-20.8858252040093,25.363397260562,-22.1949981023802));
#31351=CARTESIAN_POINT('Ctrl Pts',(-20.8990804068363,25.3827243895842,-22.1935432809991));
#31352=CARTESIAN_POINT('Ctrl Pts',(-20.9194429969747,25.4117312169147,-22.1913309451614));
#31353=CARTESIAN_POINT('Ctrl Pts',(-20.9263958305049,25.4215188699868,-22.1905793952976));
#31354=CARTESIAN_POINT('Ctrl Pts',(-20.9404291323972,25.4410418624213,-22.1890700941812));
#31355=CARTESIAN_POINT('Ctrl Pts',(-20.947509779636,25.4507768354036,-22.1883123438282));
#31356=CARTESIAN_POINT('Ctrl Pts',(-20.9556125825063,25.4617869318254,-22.1874494390629));
#31357=CARTESIAN_POINT('Ctrl Pts',(-20.9565814384575,25.4631013205166,-22.1873463292215));
#31358=CARTESIAN_POINT('Ctrl Pts',(-20.9652495563864,25.4748421423247,-22.1864244380318));
#31359=CARTESIAN_POINT('Ctrl Pts',(-20.9730105628445,25.4852226549424,-22.1856032988037));
#31360=CARTESIAN_POINT('Ctrl Pts',(-20.983234353423,25.4987265628163,-22.1845271037257));
#31361=CARTESIAN_POINT('Ctrl Pts',(-20.9856406786778,25.5018927189918,-22.1842741989603));
#31362=CARTESIAN_POINT('Ctrl Pts',(-20.9910715836346,25.5090111196676,-22.1837042951428));
#31363=CARTESIAN_POINT('Ctrl Pts',(-20.9940994654849,25.512960821925,-22.183387171381));
#31364=CARTESIAN_POINT('Ctrl Pts',(-21.00651896264,25.5290838750406,-22.1820889198472));
#31365=CARTESIAN_POINT('Ctrl Pts',(-21.0159883702982,25.5411968059797,-22.1811048636631));
#31366=CARTESIAN_POINT('Ctrl Pts',(-21.1607908389761,25.7237160637803,-22.1661441783079));
#31367=CARTESIAN_POINT('Ctrl Pts',(-21.3129373096749,25.8800303519374,-22.1515082071629));
#31368=CARTESIAN_POINT('Ctrl Pts',(-21.5769504323395,26.1013939599233,-22.1281857935563));
#31369=CARTESIAN_POINT('Ctrl Pts',(-21.6790027218157,26.1771653807462,-22.1195921001276));
#31370=CARTESIAN_POINT('Ctrl Pts',(-21.8494620353522,26.2887404901414,-22.1061535769285));
#31371=CARTESIAN_POINT('Ctrl Pts',(-21.9151458343257,26.3284593085886,-22.1011767150081));
#31372=CARTESIAN_POINT('Ctrl Pts',(-21.9890024426792,26.3695922616609,-22.0958489200036));
#31373=CARTESIAN_POINT('Ctrl Pts',(-21.9958279678048,26.3733612138983,-22.0953590145356));
#31374=CARTESIAN_POINT('Ctrl Pts',(-22.0077159609082,26.3798693997689,-22.0945101181163));
#31375=CARTESIAN_POINT('Ctrl Pts',(-22.012772178387,26.3826198907633,-22.0941504317189));
#31376=CARTESIAN_POINT('Ctrl Pts',(-22.0201083020142,26.3865851765035,-22.0936305670834));
#31377=CARTESIAN_POINT('Ctrl Pts',(-22.0223823057429,26.3878107792722,-22.0934697016536));
#31378=CARTESIAN_POINT('Ctrl Pts',(-22.0263321811675,26.3899334893096,-22.0931907702478));
#31379=CARTESIAN_POINT('Ctrl Pts',(-22.0280073750754,26.3908318491959,-22.09307262362));
#31380=CARTESIAN_POINT('Ctrl Pts',(-22.0312457122428,26.3925647919606,-22.0928445274506));
#31381=CARTESIAN_POINT('Ctrl Pts',(-22.0328087453143,26.3933995658126,-22.0927345655403));
#31382=CARTESIAN_POINT('Ctrl Pts',(-22.0365322406288,26.3953842391471,-22.0924729243622));
#31383=CARTESIAN_POINT('Ctrl Pts',(-22.038693329655,26.3965329695922,-22.0923213202111));
#31384=CARTESIAN_POINT('Ctrl Pts',(-22.0463624827773,26.4005983227503,-22.0917841960065));
#31385=CARTESIAN_POINT('Ctrl Pts',(-22.0518777428109,26.4035014520304,-22.091399532474));
#31386=CARTESIAN_POINT('Ctrl Pts',(-22.0632703262331,26.4094561510319,-22.0906081938959));
#31387=CARTESIAN_POINT('Ctrl Pts',(-22.0691485448093,26.4125055591381,-22.0902016588721));
#31388=CARTESIAN_POINT('Ctrl Pts',(-22.0750360154714,26.4155367746208,-22.0897962101869));
#31389=CARTESIAN_POINT('Origin',(-23.5502525316942,23.5502525316942,-77.3107734492734));
#31390=CARTESIAN_POINT('',(-22.0750360153462,26.4155367745563,-20.5963779455771));
#31391=CARTESIAN_POINT('',(-22.0750362008292,26.4155368700539,-20.8439479435254));
#31392=CARTESIAN_POINT('',(-22.0750360153461,26.4155367745563,-77.3107734492734));
#31393=CARTESIAN_POINT('',(-26.7730017999178,23.5524243199183,-21.439226550727));
#31394=CARTESIAN_POINT('Ctrl Pts',(-26.7730017999178,23.5524243199183,-21.439226550727));
#31395=CARTESIAN_POINT('Ctrl Pts',(-26.7730695458364,23.4518951305702,-21.4330445306115));
#31396=CARTESIAN_POINT('Ctrl Pts',(-26.7684291602479,23.3513372290751,-21.426862510496));
#31397=CARTESIAN_POINT('Ctrl Pts',(-26.7590992073237,23.2512197997044,-21.4206804903805));
#31398=CARTESIAN_POINT('Ctrl Pts',(-26.74976893384,23.1510989304877,-21.4144982578625));
#31399=CARTESIAN_POINT('Ctrl Pts',(-26.7357488122823,23.0514189895722,-21.4083160253445));
#31400=CARTESIAN_POINT('Ctrl Pts',(-26.7171093049967,22.952644181779,-21.4021337928264));
#31401=CARTESIAN_POINT('Ctrl Pts',(-26.698464366672,22.8538405937272,-21.3959497589761));
#31402=CARTESIAN_POINT('Ctrl Pts',(-26.675197445963,22.7559430835201,-21.3897657251258));
#31403=CARTESIAN_POINT('Ctrl Pts',(-26.6474299655197,22.6594048983124,-21.3835816912755));
#31404=CARTESIAN_POINT('Ctrl Pts',(-26.6196275020893,22.562745089031,-21.3773898664419));
#31405=CARTESIAN_POINT('Ctrl Pts',(-26.5873132744722,22.4674484366389,-21.3711980416083));
#31406=CARTESIAN_POINT('Ctrl Pts',(-26.550658404634,22.3739523318608,-21.3650062167746));
#31407=CARTESIAN_POINT('Ctrl Pts',(-26.5139794964912,22.2803949122324,-21.3588103313354));
#31408=CARTESIAN_POINT('Ctrl Pts',(-26.4729544512409,22.1886407824143,-21.3526144458961));
#31409=CARTESIAN_POINT('Ctrl Pts',(-26.4278014156728,22.0991047160623,-21.3464185604568));
#31410=CARTESIAN_POINT('Ctrl Pts',(-26.3825657353556,22.0094047695711,-21.3402113345309));
#31411=CARTESIAN_POINT('Ctrl Pts',(-26.3331871808525,21.9219313698342,-21.3340041086049));
#31412=CARTESIAN_POINT('Ctrl Pts',(-26.279928637451,21.8370724710583,-21.327796882679));
#31413=CARTESIAN_POINT('Ctrl Pts',(-26.2371032800918,21.7688371714596,-21.3228056333599));
#31414=CARTESIAN_POINT('Ctrl Pts',(-26.1917700887546,21.7022918649348,-21.3178143840408));
#31415=CARTESIAN_POINT('Ctrl Pts',(-26.1440843613951,21.6376224049497,-21.3128231347217));
#31416=CARTESIAN_POINT('Ctrl Pts',(-26.0851170278193,21.5576532856711,-21.3066510434094));
#31417=CARTESIAN_POINT('Ctrl Pts',(-26.0223441438312,21.4802728672081,-21.3004789520971));
#31418=CARTESIAN_POINT('Ctrl Pts',(-25.9560210816719,21.4058656154783,-21.2943068607848));
#31419=CARTESIAN_POINT('Ctrl Pts',(-25.889787880705,21.3315591782185,-21.288143132046));
#31420=CARTESIAN_POINT('Ctrl Pts',(-25.8200143487319,21.2602182223442,-21.2819794033072));
#31421=CARTESIAN_POINT('Ctrl Pts',(-25.746998079538,21.1921968579391,-21.2758156745684));
#31422=CARTESIAN_POINT('Ctrl Pts',(-25.6740591642283,21.1242475557855,-21.2696584757217));
#31423=CARTESIAN_POINT('Ctrl Pts',(-25.5978846576295,21.0596111478621,-21.263501276875));
#31424=CARTESIAN_POINT('Ctrl Pts',(-25.5188105665381,20.9986066264104,-21.2573440780283));
#31425=CARTESIAN_POINT('Ctrl Pts',(-25.4397942738123,20.9376466955646,-21.2511913797206));
#31426=CARTESIAN_POINT('Ctrl Pts',(-25.3578829532623,20.880313637768,-21.2450386814129));
#31427=CARTESIAN_POINT('Ctrl Pts',(-25.2734467122386,20.8268870808893,-21.2388859831052));
#31428=CARTESIAN_POINT('Ctrl Pts',(-25.1890424895578,20.773480783437,-21.2327356179095));
#31429=CARTESIAN_POINT('Ctrl Pts',(-25.1021156155338,20.723978275489,-21.2265852527137));
#31430=CARTESIAN_POINT('Ctrl Pts',(-25.0130655448243,20.6786161251975,-21.220434887518));
#31431=CARTESIAN_POINT('Ctrl Pts',(-24.9240254185138,20.6332590405878,-21.2142852091458));
#31432=CARTESIAN_POINT('Ctrl Pts',(-24.8328629539827,20.5920415915724,-21.2081355307736));
#31433=CARTESIAN_POINT('Ctrl Pts',(-24.7400016940692,20.5551541204349,-21.2019858524014));
#31434=CARTESIAN_POINT('Ctrl Pts',(-24.6471259612319,20.5182609001879,-21.1958352155689));
#31435=CARTESIAN_POINT('Ctrl Pts',(-24.5525513108732,20.4856991586283,-21.1896845787365));
#31436=CARTESIAN_POINT('Ctrl Pts',(-24.4567197704975,20.4576105046441,-21.1835339419041));
#31437=CARTESIAN_POINT('Ctrl Pts',(-24.3607857105047,20.4294918017007,-21.1773767251822));
#31438=CARTESIAN_POINT('Ctrl Pts',(-24.2635924931236,20.4058558644567,-21.1712195084604));
#31439=CARTESIAN_POINT('Ctrl Pts',(-24.1655956505453,20.3867939167314,-21.1650622917386));
#31440=CARTESIAN_POINT('Ctrl Pts',(-24.0675441359299,20.3677213344235,-21.1589016399308));
#31441=CARTESIAN_POINT('Ctrl Pts',(-23.9686885330799,20.3532278865423,-21.152740988123));
#31442=CARTESIAN_POINT('Ctrl Pts',(-23.8694907840872,20.3433530164756,-21.1465803363152));
#31443=CARTESIAN_POINT('Ctrl Pts',(-23.7701270419852,20.3334616222398,-21.1404093755462));
#31444=CARTESIAN_POINT('Ctrl Pts',(-23.6704204441282,20.3282042662422,-21.1342384147771));
#31445=CARTESIAN_POINT('Ctrl Pts',(-23.5708343754725,20.3275682545416,-21.1280674540081));
#31446=CARTESIAN_POINT('Ctrl Pts',(-23.4948184594487,20.3270827748688,-21.1233570437877));
#31447=CARTESIAN_POINT('Ctrl Pts',(-23.4188728013988,20.3292888687728,-21.1186466335673));
#31448=CARTESIAN_POINT('Ctrl Pts',(-23.3432007797727,20.3341606277639,-21.1139362233469));
#31449=CARTESIAN_POINT('Ctrl Pts',(-23.2440470743816,20.340544135768,-21.1077641320346));
#31450=CARTESIAN_POINT('Ctrl Pts',(-23.1450142250939,20.3515286197181,-21.1015920407222));
#31451=CARTESIAN_POINT('Ctrl Pts',(-23.046563729059,20.3671070507901,-21.0954199494099));
#31452=CARTESIAN_POINT('Ctrl Pts',(-22.9482466237134,20.3826643746282,-21.0892562206711));
#31453=CARTESIAN_POINT('Ctrl Pts',(-22.8505107286187,20.4028032067469,-21.0830924919323));
#31454=CARTESIAN_POINT('Ctrl Pts',(-22.7538148245869,20.4274645880135,-21.0769287631936));
#31455=CARTESIAN_POINT('Ctrl Pts',(-22.65722136079,20.4520998428612,-21.0707715643469));
#31456=CARTESIAN_POINT('Ctrl Pts',(-22.5616661162353,20.481248014723,-21.0646143655002));
#31457=CARTESIAN_POINT('Ctrl Pts',(-22.4675990903657,20.5147988442729,-21.0584571666535));
#31458=CARTESIAN_POINT('Ctrl Pts',(-22.3736008217876,20.548325150201,-21.0523044683458));
#31459=CARTESIAN_POINT('Ctrl Pts',(-22.2810890170904,20.5862475702482,-21.0461517700381));
#31460=CARTESIAN_POINT('Ctrl Pts',(-22.1904989906047,20.628405877608,-21.0399990717304));
#31461=CARTESIAN_POINT('Ctrl Pts',(-22.0999433159859,20.6705481984778,-21.0338487065346));
#31462=CARTESIAN_POINT('Ctrl Pts',(-22.0113083649821,20.7169230319686,-21.0276983413389));
#31463=CARTESIAN_POINT('Ctrl Pts',(-21.9250090885254,20.7673221852901,-21.0215479761431));
#31464=CARTESIAN_POINT('Ctrl Pts',(-21.8387194492812,20.8177157104375,-21.0153982977709));
#31465=CARTESIAN_POINT('Ctrl Pts',(-21.7547653411378,20.8721324428693,-21.0092486193987));
#31466=CARTESIAN_POINT('Ctrl Pts',(-21.6735358451112,20.930318936963,-21.0030989410265));
#31467=CARTESIAN_POINT('Ctrl Pts',(-21.5922936890335,20.9885144997329,-20.9969483041941));
#31468=CARTESIAN_POINT('Ctrl Pts',(-21.5137773417076,21.0504807381733,-20.9907976673616));
#31469=CARTESIAN_POINT('Ctrl Pts',(-21.438344875672,21.1159223127356,-20.9846470305292));
#31470=CARTESIAN_POINT('Ctrl Pts',(-21.3628317127436,21.1814338960356,-20.9784898138074));
#31471=CARTESIAN_POINT('Ctrl Pts',(-21.2904093478632,21.2504279544712,-20.9723325970855));
#31472=CARTESIAN_POINT('Ctrl Pts',(-21.2214007636211,21.3225705515088,-20.9661753803637));
#31473=CARTESIAN_POINT('Ctrl Pts',(-21.1523536797726,21.3947533966057,-20.9600147285559));
#31474=CARTESIAN_POINT('Ctrl Pts',(-21.0867244547687,21.4700879509065,-20.9538540767481));
#31475=CARTESIAN_POINT('Ctrl Pts',(-21.0247959722769,21.5482068956019,-20.9476934249403));
#31476=CARTESIAN_POINT('Ctrl Pts',(-20.9627638614119,21.6264565610712,-20.9415224641713));
#31477=CARTESIAN_POINT('Ctrl Pts',(-20.9044451165975,21.7074995709584,-20.9353515034022));
#31478=CARTESIAN_POINT('Ctrl Pts',(-20.8500795374211,21.7909392101115,-20.9291805426332));
#31479=CARTESIAN_POINT('Ctrl Pts',(-20.8085812700727,21.854630253332,-20.9244701324128));
#31480=CARTESIAN_POINT('Ctrl Pts',(-20.7693854461475,21.9197170969625,-20.9197597221924));
#31481=CARTESIAN_POINT('Ctrl Pts',(-20.7325802030727,21.9860146306636,-20.915049311972));
#31482=CARTESIAN_POINT('Ctrl Pts',(-20.6843539742728,22.0728848633268,-20.9088772206597));
#31483=CARTESIAN_POINT('Ctrl Pts',(-20.6400639515799,22.1621404402705,-20.9027051293474));
#31484=CARTESIAN_POINT('Ctrl Pts',(-20.5999536803001,22.2533892968223,-20.896533038035));
#31485=CARTESIAN_POINT('Ctrl Pts',(-20.5598977544723,22.3445145201947,-20.8903693092962));
#31486=CARTESIAN_POINT('Ctrl Pts',(-20.5240104972107,22.4376272610807,-20.8842055805574));
#31487=CARTESIAN_POINT('Ctrl Pts',(-20.4924902956854,22.5323096695753,-20.8780418518187));
#31488=CARTESIAN_POINT('Ctrl Pts',(-20.4610034868554,22.6268917709445,-20.871884652972));
#31489=CARTESIAN_POINT('Ctrl Pts',(-20.4338746723418,22.7230398240079,-20.8657274541253));
#31490=CARTESIAN_POINT('Ctrl Pts',(-20.4112543328994,22.8203156368443,-20.8595702552786));
#31491=CARTESIAN_POINT('Ctrl Pts',(-20.3886505275535,22.9175203469602,-20.8534175569709));
#31492=CARTESIAN_POINT('Ctrl Pts',(-20.3705487435183,23.0158507561188,-20.8472648586632));
#31493=CARTESIAN_POINT('Ctrl Pts',(-20.3570494851434,23.1148540176884,-20.8411121603555));
#31494=CARTESIAN_POINT('Ctrl Pts',(-20.3435553457064,23.2138197370804,-20.8349617951597));
#31495=CARTESIAN_POINT('Ctrl Pts',(-20.3346603226908,23.3134573719695,-20.828811429964));
#31496=CARTESIAN_POINT('Ctrl Pts',(-20.3304135585788,23.4133052801449,-20.8226610647682));
#31497=CARTESIAN_POINT('Ctrl Pts',(-20.3261672687113,23.5131420381054,-20.816511386396));
#31498=CARTESIAN_POINT('Ctrl Pts',(-20.3265682242048,23.6131885886578,-20.8103617080238));
#31499=CARTESIAN_POINT('Ctrl Pts',(-20.3316135117881,23.7129805933118,-20.8042120296516));
#31500=CARTESIAN_POINT('Ctrl Pts',(-20.3366595857064,23.8127881510832,-20.7980613928192));
#31501=CARTESIAN_POINT('Ctrl Pts',(-20.3463514075174,23.9123406502677,-20.7919107559867));
#31502=CARTESIAN_POINT('Ctrl Pts',(-20.3606340564901,24.0111771948844,-20.7857601191542));
#31503=CARTESIAN_POINT('Ctrl Pts',(-20.3749319848969,24.1101194738413,-20.7796029024324));
#31504=CARTESIAN_POINT('Ctrl Pts',(-20.3938304854383,24.2083438379856,-20.7734456857106));
#31505=CARTESIAN_POINT('Ctrl Pts',(-20.417223197488,24.305398049792,-20.7672884689888));
#31506=CARTESIAN_POINT('Ctrl Pts',(-20.4406289602359,24.4025064077458,-20.761127817181));
#31507=CARTESIAN_POINT('Ctrl Pts',(-20.468533806416,24.4984428961431,-20.7549671653732));
#31508=CARTESIAN_POINT('Ctrl Pts',(-20.5007816151657,24.5927709688199,-20.7488065135654));
#31509=CARTESIAN_POINT('Ctrl Pts',(-20.5330833859669,24.6872568859056,-20.7426355527963));
#31510=CARTESIAN_POINT('Ctrl Pts',(-20.5697424760654,24.7801286069053,-20.7364645920273));
#31511=CARTESIAN_POINT('Ctrl Pts',(-20.6105547441904,24.8709699430451,-20.7302936312583));
#31512=CARTESIAN_POINT('Ctrl Pts',(-20.6417075147376,24.9403108405491,-20.7255832210379));
#31513=CARTESIAN_POINT('Ctrl Pts',(-20.6752791638666,25.0084691430639,-20.7208728108175));
#31514=CARTESIAN_POINT('Ctrl Pts',(-20.7111615971587,25.0752706391075,-20.7161624005971));
#31515=CARTESIAN_POINT('Ctrl Pts',(-20.758172755292,25.1627902247632,-20.7099910844564));
#31516=CARTESIAN_POINT('Ctrl Pts',(-20.8093173903843,25.2482881022242,-20.7038197683157));
#31517=CARTESIAN_POINT('Ctrl Pts',(-20.8643973761013,25.3313476009354,-20.697648452175));
#31518=CARTESIAN_POINT('Ctrl Pts',(-20.9194067984958,25.4143006915906,-20.6914850421469));
#31519=CARTESIAN_POINT('Ctrl Pts',(-20.9783413163236,25.4948212516903,-20.6853216321189));
#31520=CARTESIAN_POINT('Ctrl Pts',(-21.0409566669169,25.5725165662633,-20.6791582220908));
#31521=CARTESIAN_POINT('Ctrl Pts',(-21.1035085611367,25.650133141951,-20.6730010582571));
#31522=CARTESIAN_POINT('Ctrl Pts',(-21.169733602951,25.7249298265717,-20.6668438944234));
#31523=CARTESIAN_POINT('Ctrl Pts',(-21.2393444878606,25.7965431574693,-20.6606867305896));
#31524=CARTESIAN_POINT('Ctrl Pts',(-21.3089028324128,25.8681024366191,-20.6545342140117));
#31525=CARTESIAN_POINT('Ctrl Pts',(-21.3818416363882,25.9364828294316,-20.6483816974338));
#31526=CARTESIAN_POINT('Ctrl Pts',(-21.4578342756263,26.001355019183,-20.6422291808559));
#31527=CARTESIAN_POINT('Ctrl Pts',(-21.5337933864888,26.066198586963,-20.6360793788026));
#31528=CARTESIAN_POINT('Ctrl Pts',(-21.6128033228271,26.1275367486431,-20.6299295767492));
#31529=CARTESIAN_POINT('Ctrl Pts',(-21.6945023688294,26.185078692094,-20.6237797746958));
#31530=CARTESIAN_POINT('Ctrl Pts',(-21.7762010364686,26.2426203690577,-20.6176300011234));
#31531=CARTESIAN_POINT('Ctrl Pts',(-21.8605884378157,26.2963656070947,-20.6114802275509));
#31532=CARTESIAN_POINT('Ctrl Pts',(-21.947272332421,26.3460658379144,-20.6053304539784));
#31533=CARTESIAN_POINT('Ctrl Pts',(-21.9893355772739,26.370182808982,-20.6023462845113));
#31534=CARTESIAN_POINT('Ctrl Pts',(-22.0319391436515,26.3933479752826,-20.5993621150442));
#31535=CARTESIAN_POINT('Ctrl Pts',(-22.0750360153462,26.4155367745563,-20.5963779455771));
#31536=CARTESIAN_POINT('Ctrl Pts',(-26.7730017007064,23.5525668634057,-21.4370484864937));
#31537=CARTESIAN_POINT('Ctrl Pts',(-26.7728013093608,23.8316154713373,-21.4553107584596));
#31538=CARTESIAN_POINT('Ctrl Pts',(-26.7363625104451,24.1094214252021,-21.474563588989));
#31539=CARTESIAN_POINT('Ctrl Pts',(-26.6456384354794,24.4503328290884,-21.4979959163431));
#31540=CARTESIAN_POINT('Ctrl Pts',(-26.6242256844314,24.5209477490875,-21.5028293034063));
#31541=CARTESIAN_POINT('Ctrl Pts',(-26.5906331816968,24.6194201418758,-21.5094839514482));
#31542=CARTESIAN_POINT('Ctrl Pts',(-26.5804561887718,24.6479318275351,-21.5114003538769));
#31543=CARTESIAN_POINT('Ctrl Pts',(-26.568300543437,24.6805286737495,-21.5135759137909));
#31544=CARTESIAN_POINT('Ctrl Pts',(-26.5667136595805,24.6847569270265,-21.5138578130019));
#31545=CARTESIAN_POINT('Ctrl Pts',(-26.564299493191,24.6911486009801,-21.5142834781383));
#31546=CARTESIAN_POINT('Ctrl Pts',(-26.5634787663595,24.6933144660734,-21.51442763606));
#31547=CARTESIAN_POINT('Ctrl Pts',(-26.5619925133816,24.6972239036709,-21.5146876942772));
#31548=CARTESIAN_POINT('Ctrl Pts',(-26.5613278093555,24.6989677782819,-21.5148036437055));
#31549=CARTESIAN_POINT('Ctrl Pts',(-26.5598926804892,24.7027230851596,-21.5150532152692));
#31550=CARTESIAN_POINT('Ctrl Pts',(-26.5591217559987,24.704734317147,-21.5151868063604));
#31551=CARTESIAN_POINT('Ctrl Pts',(-26.5570332287601,24.710166684739,-21.5155474468762));
#31552=CARTESIAN_POINT('Ctrl Pts',(-26.5557117987193,24.7135863605034,-21.5157742652339));
#31553=CARTESIAN_POINT('Ctrl Pts',(-26.5495401457452,24.7294770312655,-21.5168273325627));
#31554=CARTESIAN_POINT('Ctrl Pts',(-26.5446180265116,24.7419202330133,-21.5176492994726));
#31555=CARTESIAN_POINT('Ctrl Pts',(-26.5390547833571,24.7557320790169,-21.518559116728));
#31556=CARTESIAN_POINT('Ctrl Pts',(-26.5384901352657,24.7571310936038,-21.5186512436514));
#31557=CARTESIAN_POINT('Ctrl Pts',(-26.4089853603229,25.0773537965999,-21.539731726087));
#31558=CARTESIAN_POINT('Ctrl Pts',(-26.2298219384581,25.3735459443323,-21.5579188324066));
#31559=CARTESIAN_POINT('Ctrl Pts',(-25.9701584838787,25.679440968662,-21.5808049714193));
#31560=CARTESIAN_POINT('Ctrl Pts',(-25.9319958562318,25.7220459161568,-21.5840960951235));
#31561=CARTESIAN_POINT('Ctrl Pts',(-25.8466543215041,25.8123655901543,-21.5913339516413));
#31562=CARTESIAN_POINT('Ctrl Pts',(-25.7990792618654,25.8596667612672,-21.5952939458109));
#31563=CARTESIAN_POINT('Ctrl Pts',(-25.7243926206778,25.9294260277076,-21.6014263927167));
#31564=CARTESIAN_POINT('Ctrl Pts',(-25.6983302822796,25.9529829531879,-21.6035515242263));
#31565=CARTESIAN_POINT('Ctrl Pts',(-25.6664910374549,25.9808293299509,-21.6061322825843));
#31566=CARTESIAN_POINT('Ctrl Pts',(-25.6610775274115,25.9855321504714,-21.6065705517221));
#31567=CARTESIAN_POINT('Ctrl Pts',(-25.6531699033447,25.9923554794144,-21.6072099925374));
#31568=CARTESIAN_POINT('Ctrl Pts',(-25.6506881560157,25.9944903407482,-21.6074105694397));
#31569=CARTESIAN_POINT('Ctrl Pts',(-25.6457478653105,25.9987270223518,-21.6078096383237));
#31570=CARTESIAN_POINT('Ctrl Pts',(-25.6432894017999,26.0008289301896,-21.6080081263542));
#31571=CARTESIAN_POINT('Ctrl Pts',(-25.6383808988938,26.0050127688151,-21.6084042197757));
#31572=CARTESIAN_POINT('Ctrl Pts',(-25.6359308998012,26.0070947415924,-21.608601823125));
#31573=CARTESIAN_POINT('Ctrl Pts',(-25.6300343620521,26.0120903550668,-21.6090771670718));
#31574=CARTESIAN_POINT('Ctrl Pts',(-25.6265848172344,26.0150004235031,-21.609355054009));
#31575=CARTESIAN_POINT('Ctrl Pts',(-25.6160091378937,26.0238842087383,-21.6102064178512));
#31576=CARTESIAN_POINT('Ctrl Pts',(-25.6088632993215,26.0298342976844,-21.6107808595919));
#31577=CARTESIAN_POINT('Ctrl Pts',(-25.5271073468363,26.0973126011693,-21.6173440994967));
#31578=CARTESIAN_POINT('Ctrl Pts',(-25.4497970941437,26.1554775065662,-21.6234678515026));
#31579=CARTESIAN_POINT('Ctrl Pts',(-25.2874626070312,26.2665402087721,-21.636183749382));
#31580=CARTESIAN_POINT('Ctrl Pts',(-25.2023530776515,26.3191292799408,-21.6427779895879));
#31581=CARTESIAN_POINT('Ctrl Pts',(-25.0547214746422,26.4011183524669,-21.6540624923588));
#31582=CARTESIAN_POINT('Ctrl Pts',(-24.9934449517728,26.4326227116797,-21.6587034825646));
#31583=CARTESIAN_POINT('Ctrl Pts',(-24.8087654158153,26.5202065554043,-21.6725204503512));
#31584=CARTESIAN_POINT('Ctrl Pts',(-24.6827797766678,26.5704951460938,-21.6817326098741));
#31585=CARTESIAN_POINT('Ctrl Pts',(-24.4994680262209,26.6305773012484,-21.6945737084611));
#31586=CARTESIAN_POINT('Ctrl Pts',(-24.4444653866184,26.6469919197969,-21.6983562317433));
#31587=CARTESIAN_POINT('Ctrl Pts',(-24.3389018079802,26.6754481349556,-21.7054476235642));
#31588=CARTESIAN_POINT('Ctrl Pts',(-24.2884295456229,26.6877532430825,-21.7087663453197));
#31589=CARTESIAN_POINT('Ctrl Pts',(-24.2327329042231,26.6999134225422,-21.7123339035894));
#31590=CARTESIAN_POINT('Ctrl Pts',(-24.2277848360209,26.7009815209364,-21.7126500286315));
#31591=CARTESIAN_POINT('Ctrl Pts',(-24.2204611672869,26.7025443702075,-21.7131167006382));
#31592=CARTESIAN_POINT('Ctrl Pts',(-24.218087522272,26.7030480968766,-21.7132677613898));
#31593=CARTESIAN_POINT('Ctrl Pts',(-24.2140464469816,26.7039009113762,-21.7135246120452));
#31594=CARTESIAN_POINT('Ctrl Pts',(-24.2123793085098,26.7042513579658,-21.7136304806841));
#31595=CARTESIAN_POINT('Ctrl Pts',(-24.2089650543874,26.7049662366334,-21.7138471021924));
#31596=CARTESIAN_POINT('Ctrl Pts',(-24.2072179174365,26.7053305385998,-21.7139578473314));
#31597=CARTESIAN_POINT('Ctrl Pts',(-24.2030270419204,26.7062007614792,-21.7142232452066));
#31598=CARTESIAN_POINT('Ctrl Pts',(-24.2005830120232,26.7067052965456,-21.7143778177782));
#31599=CARTESIAN_POINT('Ctrl Pts',(-24.1931303144796,26.7082347761101,-21.7148485549258));
#31600=CARTESIAN_POINT('Ctrl Pts',(-24.1881197608429,26.7092506479444,-21.7151642008028));
#31601=CARTESIAN_POINT('Ctrl Pts',(-24.1336801929353,26.7201532709657,-21.7185848069968));
#31602=CARTESIAN_POINT('Ctrl Pts',(-24.0840247638312,26.7288916167078,-21.7216253681602));
#31603=CARTESIAN_POINT('Ctrl Pts',(-24.0275432143783,26.7374701661473,-21.7250151308859));
#31604=CARTESIAN_POINT('Ctrl Pts',(-24.0209017975675,26.7384576560629,-21.7254126452682));
#31605=CARTESIAN_POINT('Ctrl Pts',(-24.0093088443239,26.7401443589875,-21.7261047322912));
#31606=CARTESIAN_POINT('Ctrl Pts',(-24.0043586997956,26.7408528132454,-21.7263996800349));
#31607=CARTESIAN_POINT('Ctrl Pts',(-23.6819820339473,26.7862252363658,-21.7455720801825));
#31608=CARTESIAN_POINT('Ctrl Pts',(-23.3596417195506,26.7832991759603,-21.7626424865299));
#31609=CARTESIAN_POINT('Ctrl Pts',(-22.972282390405,26.7215609136378,-21.7852247434321));
#31610=CARTESIAN_POINT('Ctrl Pts',(-22.9019588850543,26.7079353314881,-21.7894010835479));
#31611=CARTESIAN_POINT('Ctrl Pts',(-22.794198198009,26.683304568177,-21.7959566892817));
#31612=CARTESIAN_POINT('Ctrl Pts',(-22.7564071428748,26.6739430609185,-21.7982856517863));
#31613=CARTESIAN_POINT('Ctrl Pts',(-22.7039534540641,26.6599360281156,-21.8015641700752));
#31614=CARTESIAN_POINT('Ctrl Pts',(-22.68913952431,26.655866473029,-21.8024952331016));
#31615=CARTESIAN_POINT('Ctrl Pts',(-22.6635713130845,26.6486455914143,-21.8041113769522));
#31616=CARTESIAN_POINT('Ctrl Pts',(-22.6528032405026,26.6455437782032,-21.8047948434589));
#31617=CARTESIAN_POINT('Ctrl Pts',(-22.6375054845003,26.6410506229808,-21.8057699151429));
#31618=CARTESIAN_POINT('Ctrl Pts',(-22.6329622687593,26.6397053289395,-21.806060013364));
#31619=CARTESIAN_POINT('Ctrl Pts',(-22.6254059962958,26.637449699946,-21.8065433694009));
#31620=CARTESIAN_POINT('Ctrl Pts',(-22.6223912662697,26.6365449581686,-21.8067364437013));
#31621=CARTESIAN_POINT('Ctrl Pts',(-22.616097827797,26.634646198157,-21.807139980023));
#31622=CARTESIAN_POINT('Ctrl Pts',(-22.6128193708965,26.6336513656783,-21.8073504685501));
#31623=CARTESIAN_POINT('Ctrl Pts',(-22.6056010407122,26.6314484205112,-21.8078145160028));
#31624=CARTESIAN_POINT('Ctrl Pts',(-22.6016618898375,26.63023797624,-21.808068151283));
#31625=CARTESIAN_POINT('Ctrl Pts',(-22.5879334322225,26.6259905841027,-21.8089534982555));
#31626=CARTESIAN_POINT('Ctrl Pts',(-22.5781563786545,26.6229145179191,-21.8095864954968));
#31627=CARTESIAN_POINT('Ctrl Pts',(-22.5441376770551,26.6120329035142,-21.8117977177717));
#31628=CARTESIAN_POINT('Ctrl Pts',(-22.5199745053113,26.603986847947,-21.8133838544205));
#31629=CARTESIAN_POINT('Ctrl Pts',(-22.4902007945646,26.5936789520496,-21.8153580121245));
#31630=CARTESIAN_POINT('Ctrl Pts',(-22.4844974132162,26.5916864185549,-21.8157370776543));
#31631=CARTESIAN_POINT('Ctrl Pts',(-22.4723319156831,26.5873978589314,-21.8165475693896));
#31632=CARTESIAN_POINT('Ctrl Pts',(-22.4658714666897,26.5850972225918,-21.8169791460031));
#31633=CARTESIAN_POINT('Ctrl Pts',(-22.4578242095134,26.5822025302701,-21.8175181895506));
#31634=CARTESIAN_POINT('Ctrl Pts',(-22.4562304238111,26.5816278071118,-21.8176250206067));
#31635=CARTESIAN_POINT('Ctrl Pts',(-22.4481841114409,26.5787191143273,-21.818164725485));
#31636=CARTESIAN_POINT('Ctrl Pts',(-22.441738635235,26.5763658119985,-21.8185982326311));
#31637=CARTESIAN_POINT('Ctrl Pts',(-22.4302000172079,26.5721111455872,-21.8193764130208));
#31638=CARTESIAN_POINT('Ctrl Pts',(-22.4251040634224,26.570217438998,-21.8197208348809));
#31639=CARTESIAN_POINT('Ctrl Pts',(-22.3020719814884,26.524142872546,-21.828054271201));
#31640=CARTESIAN_POINT('Ctrl Pts',(-22.186885621001,26.4731235321204,-21.8362636789268));
#31641=CARTESIAN_POINT('Ctrl Pts',(-22.0750357083693,26.4155366165066,-21.8446295278275));
#31642=CARTESIAN_POINT('Ctrl Pts',(-22.0750360154714,26.4155367746208,-22.0897962101869));
#31643=CARTESIAN_POINT('Ctrl Pts',(-22.1397156334464,26.4488376385527,-22.0853419602089));
#31644=CARTESIAN_POINT('Ctrl Pts',(-22.2055118983304,26.4799427965672,-22.0810187234138));
#31645=CARTESIAN_POINT('Ctrl Pts',(-22.4906085190755,26.6030899893747,-22.062924202422));
#31646=CARTESIAN_POINT('Ctrl Pts',(-22.718686093474,26.672940286287,-22.0499736395622));
#31647=CARTESIAN_POINT('Ctrl Pts',(-23.0882378527218,26.7427080921484,-22.0287424396187));
#31648=CARTESIAN_POINT('Ctrl Pts',(-23.2255820122374,26.7595847278466,-22.0208104453863));
#31649=CARTESIAN_POINT('Ctrl Pts',(-23.4198999471845,26.7708594310218,-22.0092544120261));
#31650=CARTESIAN_POINT('Ctrl Pts',(-23.4762967925865,26.7726476875099,-22.0058624412068));
#31651=CARTESIAN_POINT('Ctrl Pts',(-23.5409413710247,26.7729995957803,-22.0019215788501));
#31652=CARTESIAN_POINT('Ctrl Pts',(-23.5491738437247,26.7730128658238,-22.0014187347695));
#31653=CARTESIAN_POINT('Ctrl Pts',(-23.5616271716978,26.7729852225343,-22.00065657237));
#31654=CARTESIAN_POINT('Ctrl Pts',(-23.5658480877119,26.7729675605805,-22.0003979842468));
#31655=CARTESIAN_POINT('Ctrl Pts',(-23.5731084794561,26.7729229162194,-21.9999527327249));
#31656=CARTESIAN_POINT('Ctrl Pts',(-23.5761479815624,26.7728999258742,-21.9997661949026));
#31657=CARTESIAN_POINT('Ctrl Pts',(-23.5824085913836,26.7728437138005,-21.9993816898606));
#31658=CARTESIAN_POINT('Ctrl Pts',(-23.5856296902047,26.7728099626321,-21.9991837062057));
#31659=CARTESIAN_POINT('Ctrl Pts',(-23.5933857847771,26.7727170628734,-21.9987066052624));
#31660=CARTESIAN_POINT('Ctrl Pts',(-23.5979207080045,26.7726531704836,-21.9984273392636));
#31661=CARTESIAN_POINT('Ctrl Pts',(-23.6118433162056,26.7724276189102,-21.997569010909));
#31662=CARTESIAN_POINT('Ctrl Pts',(-23.6212303787722,26.7722345086209,-21.9969889620322));
#31663=CARTESIAN_POINT('Ctrl Pts',(-23.6558430966231,26.7713711228168,-21.9948451464724));
#31664=CARTESIAN_POINT('Ctrl Pts',(-23.6810609475122,26.7704456074862,-21.9932733915553));
#31665=CARTESIAN_POINT('Ctrl Pts',(-23.7122961753202,26.7689317458183,-21.9913139675977));
#31666=CARTESIAN_POINT('Ctrl Pts',(-23.7183267197134,26.7686224750654,-21.990935081125));
#31667=CARTESIAN_POINT('Ctrl Pts',(-23.7312119980531,26.76792535096,-21.9901242719562));
#31668=CARTESIAN_POINT('Ctrl Pts',(-23.7380664238393,26.7675325383225,-21.9896921967949));
#31669=CARTESIAN_POINT('Ctrl Pts',(-23.7464124576076,26.7670274823321,-21.9891651666114));
#31670=CARTESIAN_POINT('Ctrl Pts',(-23.747905350477,26.7669360975429,-21.989070858084));
#31671=CARTESIAN_POINT('Ctrl Pts',(-23.7560517179306,26.7664317395026,-21.9885560404172));
#31672=CARTESIAN_POINT('Ctrl Pts',(-23.762703924072,26.7659991645309,-21.9881349266085));
#31673=CARTESIAN_POINT('Ctrl Pts',(-23.7783873950682,26.7649304339192,-21.9871403847978));
#31674=CARTESIAN_POINT('Ctrl Pts',(-23.7874173814534,26.7642768567907,-21.9865664254657));
#31675=CARTESIAN_POINT('Ctrl Pts',(-23.8004149113002,26.7632810413189,-21.9857383466372));
#31676=CARTESIAN_POINT('Ctrl Pts',(-23.8043848200852,26.7629694815052,-21.9854851615955));
#31677=CARTESIAN_POINT('Ctrl Pts',(-23.8135702653924,26.7622314726833,-21.9848987468561));
#31678=CARTESIAN_POINT('Ctrl Pts',(-23.8187853506972,26.7617996776732,-21.9845653563707));
#31679=CARTESIAN_POINT('Ctrl Pts',(-24.1060376848745,26.7373113889743,-21.9661769941089));
#31680=CARTESIAN_POINT('Ctrl Pts',(-24.3836388485926,26.6762163351353,-21.9469212255843));
#31681=CARTESIAN_POINT('Ctrl Pts',(-24.7244993575928,26.5525194527128,-21.9224662141823));
#31682=CARTESIAN_POINT('Ctrl Pts',(-24.7983459032414,26.5225793074199,-21.9171275469122));
#31683=CARTESIAN_POINT('Ctrl Pts',(-24.939133173161,26.459325512432,-21.9069566425914));
#31684=CARTESIAN_POINT('Ctrl Pts',(-25.0061779727307,26.4263572231912,-21.9021166597251));
#31685=CARTESIAN_POINT('Ctrl Pts',(-25.0822070053008,26.3856302047552,-21.8966819337281));
#31686=CARTESIAN_POINT('Ctrl Pts',(-25.0923625801301,26.3801196074191,-21.8959571350096));
#31687=CARTESIAN_POINT('Ctrl Pts',(-25.1054272074286,26.3729392899424,-21.8950264163969));
#31688=CARTESIAN_POINT('Ctrl Pts',(-25.1083634269068,26.3713195719645,-21.8948173525166));
#31689=CARTESIAN_POINT('Ctrl Pts',(-25.1131152074289,26.3686886473414,-21.8944792044879));
#31690=CARTESIAN_POINT('Ctrl Pts',(-25.1149323180847,26.3676802676458,-21.894349938922));
#31691=CARTESIAN_POINT('Ctrl Pts',(-25.1183903218322,26.3657569204857,-21.8941040299365));
#31692=CARTESIAN_POINT('Ctrl Pts',(-25.1200313780292,26.3648422825777,-21.8939873668676));
#31693=CARTESIAN_POINT('Ctrl Pts',(-25.1237647592908,26.3627572125379,-21.8937220435087));
#31694=CARTESIAN_POINT('Ctrl Pts',(-25.1258565759431,26.3615858819037,-21.8935734422864));
#31695=CARTESIAN_POINT('Ctrl Pts',(-25.1323467664628,26.3579421251654,-21.8931125628303));
#31696=CARTESIAN_POINT('Ctrl Pts',(-25.1367406696649,26.3554616878665,-21.8928008001684));
#31697=CARTESIAN_POINT('Ctrl Pts',(-25.1699964379025,26.3365850816795,-21.8904429896448));
#31698=CARTESIAN_POINT('Ctrl Pts',(-25.198610610142,26.3197534354784,-21.8884245651528));
#31699=CARTESIAN_POINT('Ctrl Pts',(-25.3279156407261,26.2409784477269,-21.8793268610795));
#31700=CARTESIAN_POINT('Ctrl Pts',(-25.4254208741628,26.1739601388371,-21.8725306456431));
#31701=CARTESIAN_POINT('Ctrl Pts',(-25.5788822722026,26.055545708991,-21.8615676810002));
#31702=CARTESIAN_POINT('Ctrl Pts',(-25.6370910142789,26.0072706706436,-21.8573403930705));
#31703=CARTESIAN_POINT('Ctrl Pts',(-25.8170267934989,25.8470307746364,-21.8438760508893));
#31704=CARTESIAN_POINT('Ctrl Pts',(-25.9318542899437,25.7277337505138,-21.834656128004));
#31705=CARTESIAN_POINT('Ctrl Pts',(-26.0871309389041,25.5393661561986,-21.8205538165869));
#31706=CARTESIAN_POINT('Ctrl Pts',(-26.1349962876144,25.4767580108924,-21.8159349588007));
#31707=CARTESIAN_POINT('Ctrl Pts',(-26.2056867492304,25.3769117854276,-21.8086252301833));
#31708=CARTESIAN_POINT('Ctrl Pts',(-26.2301319817349,25.3408559951559,-21.8059965936573));
#31709=CARTESIAN_POINT('Ctrl Pts',(-26.2580003163491,25.2979018036724,-21.8028736255794));
#31710=CARTESIAN_POINT('Ctrl Pts',(-26.2621396604287,25.291471714498,-21.8024063535968));
#31711=CARTESIAN_POINT('Ctrl Pts',(-26.2684434936972,25.2816022855385,-21.801689466429));
#31712=CARTESIAN_POINT('Ctrl Pts',(-26.2706244487298,25.2781734525745,-21.8014404647197));
#31713=CARTESIAN_POINT('Ctrl Pts',(-26.2745880321742,25.2719159200036,-21.8009861462325));
#31714=CARTESIAN_POINT('Ctrl Pts',(-26.2763727573436,25.2690885497574,-21.8007809076939));
#31715=CARTESIAN_POINT('Ctrl Pts',(-26.279950613076,25.2634009034132,-21.8003681165152));
#31716=CARTESIAN_POINT('Ctrl Pts',(-26.2817436556665,25.2605405771842,-21.8001605609571));
#31717=CARTESIAN_POINT('Ctrl Pts',(-26.2868292968561,25.2523993819194,-21.7995699104841));
#31718=CARTESIAN_POINT('Ctrl Pts',(-26.2901110846551,25.2471118070182,-21.799186416604));
#31719=CARTESIAN_POINT('Ctrl Pts',(-26.3039464257378,25.2246757011917,-21.7975596797204));
#31720=CARTESIAN_POINT('Ctrl Pts',(-26.3143542744461,25.2074382601876,-21.7963110904648));
#31721=CARTESIAN_POINT('Ctrl Pts',(-26.5000987177289,24.8931906863811,-21.7735668922653));
#31722=CARTESIAN_POINT('Ctrl Pts',(-26.6267595323852,24.5700826973941,-21.7501112866366));
#31723=CARTESIAN_POINT('Ctrl Pts',(-26.7318793432411,24.0852950624069,-21.7167137754285));
#31724=CARTESIAN_POINT('Ctrl Pts',(-26.7534963184788,23.9353002746372,-21.706670392128));
#31725=CARTESIAN_POINT('Ctrl Pts',(-26.7649357089465,23.7782155411509,-21.6968014624371));
#31726=CARTESIAN_POINT('Ctrl Pts',(-26.7653630820495,23.7721065698632,-21.6964186896849));
#31727=CARTESIAN_POINT('Ctrl Pts',(-26.7659486745192,23.7633786974122,-21.6958733251129));
#31728=CARTESIAN_POINT('Ctrl Pts',(-26.7661211094625,23.7607608121329,-21.6957099384551));
#31729=CARTESIAN_POINT('Ctrl Pts',(-26.76641342336,23.756238748776,-21.6954280454724));
#31730=CARTESIAN_POINT('Ctrl Pts',(-26.7665348082835,23.7543346722147,-21.6953094536784));
#31731=CARTESIAN_POINT('Ctrl Pts',(-26.7667650398001,23.7506719725173,-21.6950815289967));
#31732=CARTESIAN_POINT('Ctrl Pts',(-26.7668741348517,23.7489133713154,-21.6949721820557));
#31733=CARTESIAN_POINT('Ctrl Pts',(-26.7671289776176,23.7447500841011,-21.6947135229608));
#31734=CARTESIAN_POINT('Ctrl Pts',(-26.7672734715797,23.7423453182745,-21.6945642819705));
#31735=CARTESIAN_POINT('Ctrl Pts',(-26.7676958695233,23.7351813227336,-21.6941201623205));
#31736=CARTESIAN_POINT('Ctrl Pts',(-26.7679659114317,23.7304216090741,-21.6938257250096));
#31737=CARTESIAN_POINT('Ctrl Pts',(-26.7703569245595,23.6865571180879,-21.6911179428636));
#31738=CARTESIAN_POINT('Ctrl Pts',(-26.7717756183619,23.6474151871149,-21.6887433357252));
#31739=CARTESIAN_POINT('Ctrl Pts',(-26.772530702764,23.6054677646739,-21.6862338536634));
#31740=CARTESIAN_POINT('Ctrl Pts',(-26.7725772587729,23.6026804543206,-21.6860672713219));
#31741=CARTESIAN_POINT('Ctrl Pts',(-26.772639516561,23.5986390506592,-21.685825976303));
#31742=CARTESIAN_POINT('Ctrl Pts',(-26.7726581028293,23.5973850107663,-21.6857511360902));
#31743=CARTESIAN_POINT('Ctrl Pts',(-26.7728375379543,23.5847817897861,-21.6849993153472));
#31744=CARTESIAN_POINT('Ctrl Pts',(-26.7729391632966,23.5734316948266,-21.6843249412117));
#31745=CARTESIAN_POINT('Ctrl Pts',(-26.7729908973031,23.5593366714227,-21.6834905610337));
#31746=CARTESIAN_POINT('Ctrl Pts',(-26.7729974647922,23.5565921730349,-21.6833282408137));
#31747=CARTESIAN_POINT('Ctrl Pts',(-26.7730013448547,23.5531140046475,-21.6831227089113));
#31748=CARTESIAN_POINT('Ctrl Pts',(-26.7730019127583,23.5523803478423,-21.6830793658396));
#31749=CARTESIAN_POINT('Ctrl Pts',(-26.7730329026782,23.4807438793125,-21.6788482049968));
#31750=CARTESIAN_POINT('Ctrl Pts',(-26.7707236934208,23.4098549168674,-21.6747554572151));
#31751=CARTESIAN_POINT('Ctrl Pts',(-26.7493540991225,23.0844052198086,-21.6561719539325));
#31752=CARTESIAN_POINT('Ctrl Pts',(-26.7024350143171,22.8326051831719,-21.6423002486468));
#31753=CARTESIAN_POINT('Ctrl Pts',(-26.6094442920165,22.5350402964159,-21.6243442182658));
#31754=CARTESIAN_POINT('Ctrl Pts',(-26.5911760246669,22.4815645855389,-21.6210564753802));
#31755=CARTESIAN_POINT('Ctrl Pts',(-26.5690381891529,22.421934647947,-21.6173076367352));
#31756=CARTESIAN_POINT('Ctrl Pts',(-26.5665421212536,22.4152788741713,-21.6168880284294));
#31757=CARTESIAN_POINT('Ctrl Pts',(-26.5605982761544,22.3995876860481,-21.6158959739561));
#31758=CARTESIAN_POINT('Ctrl Pts',(-26.5571318212733,22.3905594588324,-21.6153229659559));
#31759=CARTESIAN_POINT('Ctrl Pts',(-26.5521264713762,22.3776965697511,-21.6145033464791));
#31760=CARTESIAN_POINT('Ctrl Pts',(-26.5506207356753,22.3738489980616,-21.6142577664051));
#31761=CARTESIAN_POINT('Ctrl Pts',(-26.5465918677512,22.3636121756935,-21.613603264815));
#31762=CARTESIAN_POINT('Ctrl Pts',(-26.5440557083515,22.3572281020725,-21.6131939362411));
#31763=CARTESIAN_POINT('Ctrl Pts',(-26.5247671088486,22.3091232633921,-21.6101007302464));
#31764=CARTESIAN_POINT('Ctrl Pts',(-26.5071643669126,22.2677507113663,-21.6073899435756));
#31765=CARTESIAN_POINT('Ctrl Pts',(-26.4856363195235,22.2199535691617,-21.604194264443));
#31766=CARTESIAN_POINT('Ctrl Pts',(-26.482546400603,22.21315643326,-21.6037382893228));
#31767=CARTESIAN_POINT('Ctrl Pts',(-26.4775802255011,22.2023319572768,-21.6030096885569));
#31768=CARTESIAN_POINT('Ctrl Pts',(-26.475719200706,22.1982976248817,-21.6027375891909));
#31769=CARTESIAN_POINT('Ctrl Pts',(-26.4724212354756,22.1911869859597,-21.6022570352598));
#31770=CARTESIAN_POINT('Ctrl Pts',(-26.4709877617437,22.1881090712726,-21.6020487009713));
#31771=CARTESIAN_POINT('Ctrl Pts',(-26.4680153285654,22.1817530109198,-21.60161781197));
#31772=CARTESIAN_POINT('Ctrl Pts',(-26.4664757029423,22.1784751836998,-21.601395234371));
#31773=CARTESIAN_POINT('Ctrl Pts',(-26.4625228614473,22.1700964056286,-21.6008253366974));
#31774=CARTESIAN_POINT('Ctrl Pts',(-26.4601017742897,22.1649992008574,-21.6004777434042));
#31775=CARTESIAN_POINT('Ctrl Pts',(-26.4501927696255,22.1442780094415,-21.5990610247447));
#31776=CARTESIAN_POINT('Ctrl Pts',(-26.4425924121971,22.1287083932358,-21.5979879860891));
#31777=CARTESIAN_POINT('Ctrl Pts',(-26.392136931319,22.0274283675497,-21.5909510556204));
#31778=CARTESIAN_POINT('Ctrl Pts',(-26.3456066827329,21.9436124319097,-21.5848580484688));
#31779=CARTESIAN_POINT('Ctrl Pts',(-26.2198491474801,21.7391258367661,-21.5692853668725));
#31780=CARTESIAN_POINT('Ctrl Pts',(-26.1361256380688,21.6214761123938,-21.5596621955199));
#31781=CARTESIAN_POINT('Ctrl Pts',(-25.8873866165867,21.3173736338316,-21.5331496075216));
#31782=CARTESIAN_POINT('Ctrl Pts',(-25.7082033520016,21.1437586293915,-21.5160852662097));
#31783=CARTESIAN_POINT('Ctrl Pts',(-25.4992460748774,20.9835903774546,-21.4994466633055));
#31784=CARTESIAN_POINT('Ctrl Pts',(-25.4876056828333,20.9747927217979,-21.4985296337012));
#31785=CARTESIAN_POINT('Ctrl Pts',(-25.4728687957438,20.9638112299131,-21.4973814411078));
#31786=CARTESIAN_POINT('Ctrl Pts',(-25.4698279029615,20.9615535726179,-21.4971451966096));
#31787=CARTESIAN_POINT('Ctrl Pts',(-25.4650286288935,20.9580035424827,-21.4967734248046));
#31788=CARTESIAN_POINT('Ctrl Pts',(-25.4632729150456,20.9567075952368,-21.4966376470368));
#31789=CARTESIAN_POINT('Ctrl Pts',(-25.4600291577348,20.9543183625289,-21.4963872129));
#31790=CARTESIAN_POINT('Ctrl Pts',(-25.4585414997633,20.953224579132,-21.4962725217658));
#31791=CARTESIAN_POINT('Ctrl Pts',(-25.4552208547745,20.9507875069722,-21.4960168801193));
#31792=CARTESIAN_POINT('Ctrl Pts',(-25.453387390922,20.9494448812977,-21.4958759765108));
#31793=CARTESIAN_POINT('Ctrl Pts',(-25.4480740563697,20.9455626111492,-21.4954683498485));
#31794=CARTESIAN_POINT('Ctrl Pts',(-25.4445904943156,20.9430279910007,-21.4952019778541));
#31795=CARTESIAN_POINT('Ctrl Pts',(-25.4206895748936,20.9257110069899,-21.4933803173217));
#31796=CARTESIAN_POINT('Ctrl Pts',(-25.4001037410081,20.9111611074345,-21.4918409271065));
#31797=CARTESIAN_POINT('Ctrl Pts',(-25.3361825670815,20.8670976354963,-21.4871442760681));
#31798=CARTESIAN_POINT('Ctrl Pts',(-25.2922942069247,20.8383974904788,-21.4840355794075));
#31799=CARTESIAN_POINT('Ctrl Pts',(-25.1839071833568,20.7712372361683,-21.4765859468629));
#31800=CARTESIAN_POINT('Ctrl Pts',(-25.1187260889777,20.7339348194565,-21.4722946342769));
#31801=CARTESIAN_POINT('Ctrl Pts',(-24.7466470279695,20.5379268271521,-21.4485100834268));
#31802=CARTESIAN_POINT('Ctrl Pts',(-24.4171318937395,20.4271159394865,-21.4297945584365));
#31803=CARTESIAN_POINT('Ctrl Pts',(-24.0558283625011,20.3673385663929,-21.4076524514498));
#31804=CARTESIAN_POINT('Ctrl Pts',(-24.0353222782952,20.3641490272819,-21.4063915839923));
#31805=CARTESIAN_POINT('Ctrl Pts',(-24.0085556127557,20.360250101471,-21.4047398898518));
#31806=CARTESIAN_POINT('Ctrl Pts',(-24.0023214282005,20.3593606609373,-21.4043547818353));
#31807=CARTESIAN_POINT('Ctrl Pts',(-23.9927265124743,20.3580204229073,-21.4037614190082));
#31808=CARTESIAN_POINT('Ctrl Pts',(-23.9893675854421,20.3575566442865,-21.4035535758202));
#31809=CARTESIAN_POINT('Ctrl Pts',(-23.9827278004184,20.356650542694,-21.4031424756143));
#31810=CARTESIAN_POINT('Ctrl Pts',(-23.9794469799743,20.3562079722619,-21.4029392267076));
#31811=CARTESIAN_POINT('Ctrl Pts',(-23.9722550809867,20.3552490928797,-21.4024934230672));
#31812=CARTESIAN_POINT('Ctrl Pts',(-23.9683437287578,20.3547349090917,-21.402250801366));
#31813=CARTESIAN_POINT('Ctrl Pts',(-23.9572867543433,20.3533020146955,-21.4015644528629));
#31814=CARTESIAN_POINT('Ctrl Pts',(-23.9501390148824,20.3524000857926,-21.4011201956895));
#31815=CARTESIAN_POINT('Ctrl Pts',(-23.9341432761456,20.3504361504537,-21.400124706239));
#31816=CARTESIAN_POINT('Ctrl Pts',(-23.9252938009096,20.3493868642302,-21.3995730746057));
#31817=CARTESIAN_POINT('Ctrl Pts',(-23.7470544409016,20.3290022513304,-21.3884443025886));
#31818=CARTESIAN_POINT('Ctrl Pts',(-23.5764277764343,20.3231048475553,-21.3774371080272));
#31819=CARTESIAN_POINT('Ctrl Pts',(-23.0841170963695,20.3451388637449,-21.3446999144034));
#31820=CARTESIAN_POINT('Ctrl Pts',(-22.7660831410456,20.4077843219346,-21.3221820358439));
#31821=CARTESIAN_POINT('Ctrl Pts',(-22.4476150512043,20.5219587854325,-21.3007758002489));
#31822=CARTESIAN_POINT('Ctrl Pts',(-22.4326270276535,20.527458181289,-21.2997716705232));
#31823=CARTESIAN_POINT('Ctrl Pts',(-22.4143411164558,20.5343222375458,-21.2985511974473));
#31824=CARTESIAN_POINT('Ctrl Pts',(-22.4110041710114,20.5355811639633,-21.2983286648767));
#31825=CARTESIAN_POINT('Ctrl Pts',(-22.4055008248396,20.537667848985,-21.2979619794036));
#31826=CARTESIAN_POINT('Ctrl Pts',(-22.4033332275068,20.5384924066853,-21.2978176351443));
#31827=CARTESIAN_POINT('Ctrl Pts',(-22.3994226280074,20.5399848393864,-21.2975573713165));
#31828=CARTESIAN_POINT('Ctrl Pts',(-22.3976793204664,20.5406518871917,-21.2974414022713));
#31829=CARTESIAN_POINT('Ctrl Pts',(-22.3939274272259,20.5420912251724,-21.2971919339717));
#31830=CARTESIAN_POINT('Ctrl Pts',(-22.3919190408195,20.5428640105248,-21.2970584655028));
#31831=CARTESIAN_POINT('Ctrl Pts',(-22.3864098358734,20.5449901755619,-21.2966925412369));
#31832=CARTESIAN_POINT('Ctrl Pts',(-22.3829105911449,20.5463476656946,-21.2964603337267));
#31833=CARTESIAN_POINT('Ctrl Pts',(-22.3645969279809,20.5534890656138,-21.2952461338671));
#31834=CARTESIAN_POINT('Ctrl Pts',(-22.3498227623998,20.5593765938139,-21.2942703166142));
#31835=CARTESIAN_POINT('Ctrl Pts',(-22.1660553897168,20.634189264258,-21.2821719162451));
#31836=CARTESIAN_POINT('Ctrl Pts',(-22.003142134991,20.7172512150757,-21.2718524170749));
#31837=CARTESIAN_POINT('Ctrl Pts',(-21.6671876415675,20.9262126422353,-21.2496886238375));
#31838=CARTESIAN_POINT('Ctrl Pts',(-21.4978748770997,21.0564083949596,-21.2379087859107));
#31839=CARTESIAN_POINT('Ctrl Pts',(-21.2689602879166,21.2716445074885,-21.219636835821));
#31840=CARTESIAN_POINT('Ctrl Pts',(-21.1985784868721,21.3443570705315,-21.2136355467367));
#31841=CARTESIAN_POINT('Ctrl Pts',(-21.1255210877273,21.4273103691255,-21.2069076620542));
#31842=CARTESIAN_POINT('Ctrl Pts',(-21.1193365973462,21.4343948526048,-21.2063340007468));
#31843=CARTESIAN_POINT('Ctrl Pts',(-21.1102131906344,21.4449387356408,-21.2054815345016));
#31844=CARTESIAN_POINT('Ctrl Pts',(-21.1072503937657,21.4483774831945,-21.20520372024));
#31845=CARTESIAN_POINT('Ctrl Pts',(-21.1021967574798,21.454268068025,-21.2047281702889));
#31846=CARTESIAN_POINT('Ctrl Pts',(-21.100102306204,21.4567168099964,-21.2045305840908));
#31847=CARTESIAN_POINT('Ctrl Pts',(-21.0959095523669,21.4616337064876,-21.2041340474302));
#31848=CARTESIAN_POINT('Ctrl Pts',(-21.0938112922177,21.4641018913856,-21.2039350956008));
#31849=CARTESIAN_POINT('Ctrl Pts',(-21.0889781384199,21.4698045354876,-21.203475657223));
#31850=CARTESIAN_POINT('Ctrl Pts',(-21.0862458973494,21.4730412257507,-21.203215062175));
#31851=CARTESIAN_POINT('Ctrl Pts',(-21.0780201496004,21.482824745494,-21.202427873656));
#31852=CARTESIAN_POINT('Ctrl Pts',(-21.0725463291268,21.4893880107398,-21.2019004760195));
#31853=CARTESIAN_POINT('Ctrl Pts',(-21.0600878649234,21.5044474421297,-21.2006918863166));
#31854=CARTESIAN_POINT('Ctrl Pts',(-21.0531205079773,21.5129577117385,-21.2000099986102));
#31855=CARTESIAN_POINT('Ctrl Pts',(-20.9902975642925,21.5904991592799,-21.193806614963));
#31856=CARTESIAN_POINT('Ctrl Pts',(-20.9372786560383,21.6617696125376,-21.1881722908001));
#31857=CARTESIAN_POINT('Ctrl Pts',(-20.7760781876752,21.8982682963463,-21.1696653488789));
#31858=CARTESIAN_POINT('Ctrl Pts',(-20.680122166148,22.0712569168643,-21.1563798293143));
#31859=CARTESIAN_POINT('Ctrl Pts',(-20.5175538124135,22.4405890482319,-21.1290643912704));
#31860=CARTESIAN_POINT('Ctrl Pts',(-20.4527884274916,22.6368243443284,-21.1150951347814));
#31861=CARTESIAN_POINT('Ctrl Pts',(-20.4044811009938,22.8499723424508,-21.1013110674143));
#31862=CARTESIAN_POINT('Ctrl Pts',(-20.4018192638445,22.8620387514423,-21.1005354432051));
#31863=CARTESIAN_POINT('Ctrl Pts',(-20.3984719099176,22.8776386582551,-21.0995390114092));
#31864=CARTESIAN_POINT('Ctrl Pts',(-20.3977228676956,22.8811581971943,-21.0993146184708));
#31865=CARTESIAN_POINT('Ctrl Pts',(-20.3965860826335,22.8865439183527,-21.0989718867595));
#31866=CARTESIAN_POINT('Ctrl Pts',(-20.3961941011873,22.8884091874301,-21.0988533041756));
#31867=CARTESIAN_POINT('Ctrl Pts',(-20.3954602837374,22.8919165627003,-21.0986305491103));
#31868=CARTESIAN_POINT('Ctrl Pts',(-20.3951180763147,22.893558581402,-21.0985263556083));
#31869=CARTESIAN_POINT('Ctrl Pts',(-20.3943329088923,22.8973408426373,-21.0982865654807));
#31870=CARTESIAN_POINT('Ctrl Pts',(-20.3938908448596,22.8994812652391,-21.0981510212401));
#31871=CARTESIAN_POINT('Ctrl Pts',(-20.3926648466504,22.9054480425408,-21.0977735989148));
#31872=CARTESIAN_POINT('Ctrl Pts',(-20.3918856872463,22.9092753915027,-21.0975319958077));
#31873=CARTESIAN_POINT('Ctrl Pts',(-20.3875530226601,22.9307578133918,-21.096178619143));
#31874=CARTESIAN_POINT('Ctrl Pts',(-20.3841405037507,22.9484414713543,-21.0950748291119));
#31875=CARTESIAN_POINT('Ctrl Pts',(-20.3746855123621,22.9997451241154,-21.0918997804587));
#31876=CARTESIAN_POINT('Ctrl Pts',(-20.3690288826947,23.0334347663059,-21.0898486062595));
#31877=CARTESIAN_POINT('Ctrl Pts',(-20.3492545644892,23.1638740135483,-21.0820149485816));
#31878=CARTESIAN_POINT('Ctrl Pts',(-20.3390055780899,23.2611635362846,-21.0763999868643));
#31879=CARTESIAN_POINT('Ctrl Pts',(-20.3155180158724,23.6557846864663,-21.0540189978929));
#31880=CARTESIAN_POINT('Ctrl Pts',(-20.3390530645731,23.9537905574934,-21.0378676350291));
#31881=CARTESIAN_POINT('Ctrl Pts',(-20.4042516068,24.2494110775156,-21.0199914156989));
#31882=CARTESIAN_POINT('Ctrl Pts',(-20.4053814778823,24.2544758954725,-21.0196846287967));
#31883=CARTESIAN_POINT('Ctrl Pts',(-20.4073988750514,24.2634175003758,-21.0191420896494));
#31884=CARTESIAN_POINT('Ctrl Pts',(-20.4082813555709,24.2672954229075,-21.0189064851552));
#31885=CARTESIAN_POINT('Ctrl Pts',(-20.4121824727497,24.2842927893224,-21.0178724363121));
#31886=CARTESIAN_POINT('Ctrl Pts',(-20.4152760885205,24.2973947454349,-21.0170717907858));
#31887=CARTESIAN_POINT('Ctrl Pts',(-20.4191657661327,24.3134185640695,-21.0160880485105));
#31888=CARTESIAN_POINT('Ctrl Pts',(-20.4198840045022,24.3163593194986,-21.0159073203032));
#31889=CARTESIAN_POINT('Ctrl Pts',(-20.4209229549919,24.3205873438322,-21.0156472088915));
#31890=CARTESIAN_POINT('Ctrl Pts',(-20.4212403216225,24.3218754393567,-21.0155679278589));
#31891=CARTESIAN_POINT('Ctrl Pts',(-20.4232047894374,24.3298274808054,-21.0150782620721));
#31892=CARTESIAN_POINT('Ctrl Pts',(-20.4248723740313,24.3364863090442,-21.0146672516103));
#31893=CARTESIAN_POINT('Ctrl Pts',(-20.4280450168518,24.3489853845465,-21.0138938901853));
#31894=CARTESIAN_POINT('Ctrl Pts',(-20.4295452216216,24.3548268415526,-21.0135316911908));
#31895=CARTESIAN_POINT('Ctrl Pts',(-20.4374047932153,24.3850775266208,-21.0116519667107));
#31896=CARTESIAN_POINT('Ctrl Pts',(-20.4440340388428,24.409415167225,-21.0101260336545));
#31897=CARTESIAN_POINT('Ctrl Pts',(-20.4535238946154,24.4427084710636,-21.0080189143858));
#31898=CARTESIAN_POINT('Ctrl Pts',(-20.456139128987,24.4517335928759,-21.0074457229372));
#31899=CARTESIAN_POINT('Ctrl Pts',(-20.4600756245269,24.4650994210565,-21.006593843931));
#31900=CARTESIAN_POINT('Ctrl Pts',(-20.4613666597229,24.4694490385191,-21.0063161451754));
#31901=CARTESIAN_POINT('Ctrl Pts',(-20.4635901331589,24.4768825440327,-21.0058407421613));
#31902=CARTESIAN_POINT('Ctrl Pts',(-20.4645180211027,24.4799677958101,-21.0056431871914));
#31903=CARTESIAN_POINT('Ctrl Pts',(-20.4663880891635,24.4861521817373,-21.0052467035905));
#31904=CARTESIAN_POINT('Ctrl Pts',(-20.4673303182028,24.4892512964952,-21.0050477735782));
#31905=CARTESIAN_POINT('Ctrl Pts',(-20.4695156644645,24.4964004405901,-21.0045883081232));
#31906=CARTESIAN_POINT('Ctrl Pts',(-20.4707620965587,24.5004494429982,-21.0043276640495));
#31907=CARTESIAN_POINT('Ctrl Pts',(-20.4745523240955,24.5126761082325,-21.0035393261919));
#31908=CARTESIAN_POINT('Ctrl Pts',(-20.4771207211096,24.5208460512488,-21.0030108238813));
#31909=CARTESIAN_POINT('Ctrl Pts',(-20.4830681708321,24.5395043102009,-21.0017998469576));
#31910=CARTESIAN_POINT('Ctrl Pts',(-20.4864684981775,24.5499856840432,-21.0011166745857));
#31911=CARTESIAN_POINT('Ctrl Pts',(-20.4977313881168,24.5841059280638,-20.9988831484188));
#31912=CARTESIAN_POINT('Ctrl Pts',(-20.5058141528056,24.6076706505411,-20.9973255403671));
#31913=CARTESIAN_POINT('Ctrl Pts',(-20.5390631198272,24.7010631214974,-20.9910910659739));
#31914=CARTESIAN_POINT('Ctrl Pts',(-20.5663635329161,24.7701015764511,-20.9863443010329));
#31915=CARTESIAN_POINT('Ctrl Pts',(-20.6555433113177,24.974668654292,-20.971854661949));
#31916=CARTESIAN_POINT('Ctrl Pts',(-20.7244534683802,25.1069008604537,-20.9619018762077));
#31917=CARTESIAN_POINT('Ctrl Pts',(-20.9290432972204,25.4408300253337,-20.9354521088407));
#31918=CARTESIAN_POINT('Ctrl Pts',(-21.078816841397,25.6328106460435,-20.9188262471932));
#31919=CARTESIAN_POINT('Ctrl Pts',(-21.2582956321969,25.8159174632993,-20.9026360720793));
#31920=CARTESIAN_POINT('Ctrl Pts',(-21.2679159074272,25.8256082315375,-20.9017783079509));
#31921=CARTESIAN_POINT('Ctrl Pts',(-21.2802170567106,25.837843000542,-20.9006945492155));
#31922=CARTESIAN_POINT('Ctrl Pts',(-21.2828409199592,25.8404437451397,-20.9004641273487));
#31923=CARTESIAN_POINT('Ctrl Pts',(-21.2870063867937,25.8445583348108,-20.9000995148651));
#31924=CARTESIAN_POINT('Ctrl Pts',(-21.2885450403901,25.8460751412323,-20.8999650894175));
#31925=CARTESIAN_POINT('Ctrl Pts',(-21.2912822052316,25.848768019178,-20.8997264122682));
#31926=CARTESIAN_POINT('Ctrl Pts',(-21.2924801034659,25.8499446946585,-20.8996221124508));
#31927=CARTESIAN_POINT('Ctrl Pts',(-21.2952666130387,25.8526775607714,-20.8993798541809));
#31928=CARTESIAN_POINT('Ctrl Pts',(-21.2968559132407,25.8542330411322,-20.8992419524046));
#31929=CARTESIAN_POINT('Ctrl Pts',(-21.3013664093794,25.8586384237436,-20.8988513462173));
#31930=CARTESIAN_POINT('Ctrl Pts',(-21.3042914238071,25.8614844369879,-20.8985989489147));
#31931=CARTESIAN_POINT('Ctrl Pts',(-21.3221638287181,25.8788081615754,-20.8970622152849));
#31932=CARTESIAN_POINT('Ctrl Pts',(-21.3372461958914,25.8931468104773,-20.8957886231893));
#31933=CARTESIAN_POINT('Ctrl Pts',(-21.3829141056527,25.9357283140973,-20.8919975213357));
#31934=CARTESIAN_POINT('Ctrl Pts',(-21.4139101656069,25.9635267010424,-20.8895105640596));
#31935=CARTESIAN_POINT('Ctrl Pts',(-21.4853444244239,26.0251362101969,-20.8839474901083));
#31936=CARTESIAN_POINT('Ctrl Pts',(-21.5260912709333,26.0585719751414,-20.8808913037503));
#31937=CARTESIAN_POINT('Ctrl Pts',(-21.6732027120815,26.1733670650776,-20.8701909697272));
#31938=CARTESIAN_POINT('Ctrl Pts',(-21.7837996861613,26.2490844284423,-20.8627387053836));
#31939=CARTESIAN_POINT('Ctrl Pts',(-21.9565296392942,26.3521600693959,-20.8514971429009));
#31940=CARTESIAN_POINT('Ctrl Pts',(-22.0153075857551,26.3847850779201,-20.8477367945974));
#31941=CARTESIAN_POINT('Ctrl Pts',(-22.0750362008293,26.4155368700539,-20.8439479435254));
#31942=CARTESIAN_POINT('Origin',(-23.5502525316942,23.5502525316942,-77.3107734492734));
#31943=CARTESIAN_POINT('',(-22.0750360113656,26.4155367725069,-19.3485684984428));
#31944=CARTESIAN_POINT('',(-22.075036015346,26.4155367745563,-19.592915740792));
#31945=CARTESIAN_POINT('',(-22.0750360153461,26.4155367745563,-77.3107734492734));
#31946=CARTESIAN_POINT('',(-26.7730016852365,23.5479167572311,-20.189226550727));
#31947=CARTESIAN_POINT('Ctrl Pts',(-22.0750360113656,26.4155367725069,-19.3485684984428));
#31948=CARTESIAN_POINT('Ctrl Pts',(-22.0324063855993,26.3935885387889,-19.3513199436375));
#31949=CARTESIAN_POINT('Ctrl Pts',(-21.9902669454401,26.370689129756,-19.3540423519884));
#31950=CARTESIAN_POINT('Ctrl Pts',(-21.6552252746965,26.1788121170182,-19.3758272973173));
#31951=CARTESIAN_POINT('Ctrl Pts',(-21.3901068379,25.9656645484058,-19.3942131632512));
#31952=CARTESIAN_POINT('Ctrl Pts',(-21.1496257678348,25.7004857929686,-19.4158687651846));
#31953=CARTESIAN_POINT('Ctrl Pts',(-21.1364216884345,25.6856523935268,-19.4170757169032));
#31954=CARTESIAN_POINT('Ctrl Pts',(-21.1192835353348,25.6660373995469,-19.418666396409));
#31955=CARTESIAN_POINT('Ctrl Pts',(-21.1152247582842,25.6613649422902,-19.4190449172998));
#31956=CARTESIAN_POINT('Ctrl Pts',(-21.108977545863,25.6541311772974,-19.4196303405881));
#31957=CARTESIAN_POINT('Ctrl Pts',(-21.1067796094569,25.6515780633588,-19.4198368489277));
#31958=CARTESIAN_POINT('Ctrl Pts',(-21.1024080175492,25.6464839069891,-19.4202486662474));
#31959=CARTESIAN_POINT('Ctrl Pts',(-21.1002343055045,25.643942918405,-19.4204539725238));
#31960=CARTESIAN_POINT('Ctrl Pts',(-21.0954741468798,25.6383609056819,-19.4209047482335));
#31961=CARTESIAN_POINT('Ctrl Pts',(-21.0928893911118,25.6353184527499,-19.4211502868506));
#31962=CARTESIAN_POINT('Ctrl Pts',(-21.085530519771,25.6266238149476,-19.4218515448076));
#31963=CARTESIAN_POINT('Ctrl Pts',(-21.080770229043,25.6209600092022,-19.4223078304448));
#31964=CARTESIAN_POINT('Ctrl Pts',(-21.0701212483635,25.6082008789787,-19.4233345811151));
#31965=CARTESIAN_POINT('Ctrl Pts',(-21.0642434393196,25.6010965951066,-19.4239054857318));
#31966=CARTESIAN_POINT('Ctrl Pts',(-20.9266463548883,25.4333275040937,-19.4373694648908));
#31967=CARTESIAN_POINT('Ctrl Pts',(-20.8107647769009,25.260357047993,-19.4509122901936));
#31968=CARTESIAN_POINT('Ctrl Pts',(-20.5774310115296,24.8267721832549,-19.4839319755977));
#31969=CARTESIAN_POINT('Ctrl Pts',(-20.4763280712769,24.5592973509226,-19.5036523149232));
#31970=CARTESIAN_POINT('Ctrl Pts',(-20.4081297605235,24.2667903292781,-19.5226509964112));
#31971=CARTESIAN_POINT('Ctrl Pts',(-20.4046910469264,24.2515405564094,-19.5236340444236));
#31972=CARTESIAN_POINT('Ctrl Pts',(-20.4006099815383,24.2328079466327,-19.5248319845485));
#31973=CARTESIAN_POINT('Ctrl Pts',(-20.3998623057592,24.2293486315534,-19.5250528043334));
#31974=CARTESIAN_POINT('Ctrl Pts',(-20.3986359326965,24.2236288855914,-19.5254172436215));
#31975=CARTESIAN_POINT('Ctrl Pts',(-20.3981539676953,24.2213691713123,-19.5255610504826));
#31976=CARTESIAN_POINT('Ctrl Pts',(-20.3973258924179,24.2174661332563,-19.5258091363349));
#31977=CARTESIAN_POINT('Ctrl Pts',(-20.3969786370743,24.2158230601311,-19.5259134815507));
#31978=CARTESIAN_POINT('Ctrl Pts',(-20.3962015183368,24.2121317861626,-19.5261476925619));
#31979=CARTESIAN_POINT('Ctrl Pts',(-20.3957723663953,24.2100834412098,-19.5262775166999));
#31980=CARTESIAN_POINT('Ctrl Pts',(-20.3946331497376,24.2046194391458,-19.5266234470054));
#31981=CARTESIAN_POINT('Ctrl Pts',(-20.3939266329333,24.2012030324489,-19.5268393484085));
#31982=CARTESIAN_POINT('Ctrl Pts',(-20.3906477388599,24.1852168854184,-19.5278477864977));
#31983=CARTESIAN_POINT('Ctrl Pts',(-20.3881448445428,24.1726327734237,-19.5286363745129));
#31984=CARTESIAN_POINT('Ctrl Pts',(-20.3299439530956,23.87059204003,-19.5474456161531));
#31985=CARTESIAN_POINT('Ctrl Pts',(-20.3141330183758,23.5748105509576,-19.5633537629813));
#31986=CARTESIAN_POINT('Ctrl Pts',(-20.3557014824733,23.0790802370371,-19.5913499418242));
#31987=CARTESIAN_POINT('Ctrl Pts',(-20.3916238208292,22.8792788516211,-19.6029962454273));
#31988=CARTESIAN_POINT('Ctrl Pts',(-20.449407649001,22.6721669400113,-19.6160633649876));
#31989=CARTESIAN_POINT('Ctrl Pts',(-20.4528309957934,22.6601665162353,-19.6168239817271));
#31990=CARTESIAN_POINT('Ctrl Pts',(-20.4576117131381,22.643769494096,-19.6178681402334));
#31991=CARTESIAN_POINT('Ctrl Pts',(-20.4589089607933,22.6393553605794,-19.618149716062));
#31992=CARTESIAN_POINT('Ctrl Pts',(-20.4611355687091,22.631838440731,-19.6186300496754));
#31993=CARTESIAN_POINT('Ctrl Pts',(-20.4620601652255,22.6287342404746,-19.6188286513023));
#31994=CARTESIAN_POINT('Ctrl Pts',(-20.463922233094,22.622516889919,-19.6192269149563));
#31995=CARTESIAN_POINT('Ctrl Pts',(-20.4648597387094,22.6194037545269,-19.6194265778784));
#31996=CARTESIAN_POINT('Ctrl Pts',(-20.4670191236614,22.6122722791442,-19.6198845247216));
#31997=CARTESIAN_POINT('Ctrl Pts',(-20.4682441486332,22.6082549048084,-19.6201429116296));
#31998=CARTESIAN_POINT('Ctrl Pts',(-20.4719391875614,22.5962216764022,-19.6209180984171));
#31999=CARTESIAN_POINT('Ctrl Pts',(-20.4744326316097,22.5882131054614,-19.6214356676769));
#32000=CARTESIAN_POINT('Ctrl Pts',(-20.4801903991027,22.5699712248482,-19.6226183964494));
#32001=CARTESIAN_POINT('Ctrl Pts',(-20.4834746633945,22.5597443588191,-19.6232842093964));
#32002=CARTESIAN_POINT('Ctrl Pts',(-20.4942846670143,22.5266523045667,-19.6254476557528));
#32003=CARTESIAN_POINT('Ctrl Pts',(-20.5020153379869,22.5038553914684,-19.6269520349394));
#32004=CARTESIAN_POINT('Ctrl Pts',(-20.5335662179376,22.4141330136436,-19.6329294339128));
#32005=CARTESIAN_POINT('Ctrl Pts',(-20.5593396127607,22.3479204143598,-19.6374663891675));
#32006=CARTESIAN_POINT('Ctrl Pts',(-20.6467638627611,22.1435746960247,-19.6518715983428));
#32007=CARTESIAN_POINT('Ctrl Pts',(-20.7159568202081,22.0089064204421,-19.6619678131959));
#32008=CARTESIAN_POINT('Ctrl Pts',(-20.9211493835702,21.6704189925308,-19.688694798623));
#32009=CARTESIAN_POINT('Ctrl Pts',(-21.0713743044207,21.4763331640326,-19.7054623361572));
#32010=CARTESIAN_POINT('Ctrl Pts',(-21.2518837759907,21.2910902703407,-19.7217992599717));
#32011=CARTESIAN_POINT('Ctrl Pts',(-21.2617070911371,21.2811397438866,-19.7226777524069));
#32012=CARTESIAN_POINT('Ctrl Pts',(-21.2742308544671,21.2686178589289,-19.7237840774876));
#32013=CARTESIAN_POINT('Ctrl Pts',(-21.2768712283336,21.2659870250077,-19.7240165612863));
#32014=CARTESIAN_POINT('Ctrl Pts',(-21.2810547326442,21.2618330744549,-19.7243837053143));
#32015=CARTESIAN_POINT('Ctrl Pts',(-21.2825948357581,21.2603069346083,-19.7245186058686));
#32016=CARTESIAN_POINT('Ctrl Pts',(-21.2854626190067,21.257470882156,-19.7247693174513));
#32017=CARTESIAN_POINT('Ctrl Pts',(-21.2867898877474,21.2561605761357,-19.7248851597342));
#32018=CARTESIAN_POINT('Ctrl Pts',(-21.2897547532663,21.2532386799526,-19.7251435014887));
#32019=CARTESIAN_POINT('Ctrl Pts',(-21.2913929325571,21.2516276921791,-19.7252859528485));
#32020=CARTESIAN_POINT('Ctrl Pts',(-21.2961928331783,21.2469175497213,-19.7257024944224));
#32021=CARTESIAN_POINT('Ctrl Pts',(-21.2993592359291,21.2438231407764,-19.7259762094056));
#32022=CARTESIAN_POINT('Ctrl Pts',(-21.3225747567711,21.2212288079685,-19.7279753217666));
#32023=CARTESIAN_POINT('Ctrl Pts',(-21.3428713845086,21.2019833022699,-19.7296810737574));
#32024=CARTESIAN_POINT('Ctrl Pts',(-21.4097834998578,21.1401707030678,-19.7351795656534));
#32025=CARTESIAN_POINT('Ctrl Pts',(-21.4574019337613,21.0987061652177,-19.7388997536697));
#32026=CARTESIAN_POINT('Ctrl Pts',(-21.6214472849169,20.9641271242077,-19.7512044792263));
#32027=CARTESIAN_POINT('Ctrl Pts',(-21.7431114300877,20.8776917068828,-19.7595091210275));
#32028=CARTESIAN_POINT('Ctrl Pts',(-22.0285067156216,20.7033660758271,-19.7781954220176));
#32029=CARTESIAN_POINT('Ctrl Pts',(-22.1947100928316,20.6205819871243,-19.7885685731215));
#32030=CARTESIAN_POINT('Ctrl Pts',(-22.3868943477496,20.5447295816147,-19.8006596444988));
#32031=CARTESIAN_POINT('Ctrl Pts',(-22.4067664327626,20.5371129762922,-19.8019106231367));
#32032=CARTESIAN_POINT('Ctrl Pts',(-22.4315551481153,20.5278924562185,-19.8034727619962));
#32033=CARTESIAN_POINT('Ctrl Pts',(-22.4364024158384,20.5261027039184,-19.8037783055445));
#32034=CARTESIAN_POINT('Ctrl Pts',(-22.4449908151605,20.5229550669031,-19.8043198195477));
#32035=CARTESIAN_POINT('Ctrl Pts',(-22.4487302047519,20.5215924376237,-19.8045556454322));
#32036=CARTESIAN_POINT('Ctrl Pts',(-22.4617722117909,20.5168672938779,-19.8053783326243));
#32037=CARTESIAN_POINT('Ctrl Pts',(-22.4710877150946,20.5135407074795,-19.8059662868663));
#32038=CARTESIAN_POINT('Ctrl Pts',(-22.4858110310312,20.5083592828704,-19.8068961662564));
#32039=CARTESIAN_POINT('Ctrl Pts',(-22.4912087645313,20.5064758407729,-19.8072371988405));
#32040=CARTESIAN_POINT('Ctrl Pts',(-22.4982881541329,20.5040267261077,-19.8076846600247));
#32041=CARTESIAN_POINT('Ctrl Pts',(-22.4999653286532,20.5034480579235,-19.8077906810664));
#32042=CARTESIAN_POINT('Ctrl Pts',(-22.508121272378,20.5006415829897,-19.808306317247));
#32043=CARTESIAN_POINT('Ctrl Pts',(-22.5146066216677,20.4984330665099,-19.8087165364357));
#32044=CARTESIAN_POINT('Ctrl Pts',(-22.5268819340266,20.4942964745398,-19.8094933993487));
#32045=CARTESIAN_POINT('Ctrl Pts',(-22.5326704344476,20.4923641298674,-19.8098599057579));
#32046=CARTESIAN_POINT('Ctrl Pts',(-22.56316358176,20.4822809340344,-19.8117915776066));
#32047=CARTESIAN_POINT('Ctrl Pts',(-22.5879602132796,20.4744131743574,-19.8133657065999));
#32048=CARTESIAN_POINT('Ctrl Pts',(-22.6222528684818,20.463987669889,-19.8155482097231));
#32049=CARTESIAN_POINT('Ctrl Pts',(-22.631669851872,20.4611717575642,-19.8161481107525));
#32050=CARTESIAN_POINT('Ctrl Pts',(-22.6453708182116,20.4571430171703,-19.817021797726));
#32051=CARTESIAN_POINT('Ctrl Pts',(-22.6496447290464,20.4558958990922,-19.8172944614795));
#32052=CARTESIAN_POINT('Ctrl Pts',(-22.6571839231105,20.4537129209718,-19.8177756646758));
#32053=CARTESIAN_POINT('Ctrl Pts',(-22.6604481343065,20.4527733574851,-19.8179840827766));
#32054=CARTESIAN_POINT('Ctrl Pts',(-22.6667253928913,20.4509772664725,-19.8183850263193));
#32055=CARTESIAN_POINT('Ctrl Pts',(-22.6697382170709,20.4501199673916,-19.8185775263032));
#32056=CARTESIAN_POINT('Ctrl Pts',(-22.677661233151,20.4478779547492,-19.8190839256426));
#32057=CARTESIAN_POINT('Ctrl Pts',(-22.6825734572458,20.4465005098256,-19.8193980616306));
#32058=CARTESIAN_POINT('Ctrl Pts',(-22.7004368810623,20.441537119292,-19.8205410614067));
#32059=CARTESIAN_POINT('Ctrl Pts',(-22.7134070683091,20.4380205646029,-19.8213721803461));
#32060=CARTESIAN_POINT('Ctrl Pts',(-22.7450293766645,20.4296589016538,-19.82340162249));
#32061=CARTESIAN_POINT('Ctrl Pts',(-22.7637035155375,20.4248998232173,-19.8246027085615));
#32062=CARTESIAN_POINT('Ctrl Pts',(-22.8337093076507,20.4077260963937,-19.8291157250854));
#32063=CARTESIAN_POINT('Ctrl Pts',(-22.8852986427714,20.3964068815349,-19.832462463383));
#32064=CARTESIAN_POINT('Ctrl Pts',(-23.0589403267471,20.3627578748562,-19.8438017704267));
#32065=CARTESIAN_POINT('Ctrl Pts',(-23.1819886790433,20.3462104280648,-19.8519648258069));
#32066=CARTESIAN_POINT('Ctrl Pts',(-23.5617583205988,20.3173057936627,-19.8774395521724));
#32067=CARTESIAN_POINT('Ctrl Pts',(-23.8192478414564,20.3284953991281,-19.8951718110219));
#32068=CARTESIAN_POINT('Ctrl Pts',(-24.0799383857797,20.3713211702789,-19.9123198902541));
#32069=CARTESIAN_POINT('Ctrl Pts',(-24.0871951543888,20.3725388368365,-19.9127965118293));
#32070=CARTESIAN_POINT('Ctrl Pts',(-24.1389999168944,20.3814140643021,-19.9161935552828));
#32071=CARTESIAN_POINT('Ctrl Pts',(-24.1833894759612,20.389983738241,-19.919075473664));
#32072=CARTESIAN_POINT('Ctrl Pts',(-24.2329062909015,20.4006285838789,-19.9222467589812));
#32073=CARTESIAN_POINT('Ctrl Pts',(-24.2382229606921,20.4017856258068,-19.9225866973914));
#32074=CARTESIAN_POINT('Ctrl Pts',(-24.2457692741795,20.4034479223214,-19.92306836645));
#32075=CARTESIAN_POINT('Ctrl Pts',(-24.2480013121186,20.4039420848147,-19.9232107307666));
#32076=CARTESIAN_POINT('Ctrl Pts',(-24.2520916969035,20.4048522431548,-19.9234714331651));
#32077=CARTESIAN_POINT('Ctrl Pts',(-24.2539502035897,20.4052675117625,-19.9235898133965));
#32078=CARTESIAN_POINT('Ctrl Pts',(-24.2577323758251,20.4061161286591,-19.9238305751887));
#32079=CARTESIAN_POINT('Ctrl Pts',(-24.2596560119239,20.4065495951828,-19.9239529496923));
#32080=CARTESIAN_POINT('Ctrl Pts',(-24.2644495779728,20.4076343871742,-19.9242577055948));
#32081=CARTESIAN_POINT('Ctrl Pts',(-24.2673190233495,20.4082878804147,-19.9244399612417));
#32082=CARTESIAN_POINT('Ctrl Pts',(-24.2781296480994,20.4107654947097,-19.9251259729906));
#32083=CARTESIAN_POINT('Ctrl Pts',(-24.2860648832492,20.4126158193451,-19.9256282271659));
#32084=CARTESIAN_POINT('Ctrl Pts',(-24.4298732951135,20.446724386004,-19.9347083925568));
#32085=CARTESIAN_POINT('Ctrl Pts',(-24.5635352286405,20.4877553701181,-19.9427924550898));
#32086=CARTESIAN_POINT('Ctrl Pts',(-24.7975954582408,20.5766181461353,-19.9569846703623));
#32087=CARTESIAN_POINT('Ctrl Pts',(-24.898971945649,20.6212043876961,-19.9631449823489));
#32088=CARTESIAN_POINT('Ctrl Pts',(-25.115644617033,20.730137939894,-19.9767032424342));
#32089=CARTESIAN_POINT('Ctrl Pts',(-25.2296834886624,20.7965264416605,-19.9841022682964));
#32090=CARTESIAN_POINT('Ctrl Pts',(-25.3734690391325,20.8924933821671,-19.9940669678421));
#32091=CARTESIAN_POINT('Ctrl Pts',(-25.4071678481933,20.9159276748197,-19.9964506597254));
#32092=CARTESIAN_POINT('Ctrl Pts',(-25.4565681177933,20.951699764486,-20.0000247535676));
#32093=CARTESIAN_POINT('Ctrl Pts',(-25.4726179534102,20.9635506240094,-20.0011987982374));
#32094=CARTESIAN_POINT('Ctrl Pts',(-25.4926880101929,20.9786598893812,-20.0026838023914));
#32095=CARTESIAN_POINT('Ctrl Pts',(-25.4968120287339,20.9817801393602,-20.0029898495689));
#32096=CARTESIAN_POINT('Ctrl Pts',(-25.5041956509593,20.987394616141,-20.0035394382383));
#32097=CARTESIAN_POINT('Ctrl Pts',(-25.5074580397276,20.9898851737274,-20.0037828473505));
#32098=CARTESIAN_POINT('Ctrl Pts',(-25.5133725791594,20.9944183336544,-20.0042251933871));
#32099=CARTESIAN_POINT('Ctrl Pts',(-25.5160263254498,20.9964588516383,-20.004424054252));
#32100=CARTESIAN_POINT('Ctrl Pts',(-25.5604492198402,21.0307267618891,-20.0077594719829));
#32101=CARTESIAN_POINT('Ctrl Pts',(-25.6014220046944,21.0639693364731,-20.0109332015926));
#32102=CARTESIAN_POINT('Ctrl Pts',(-25.6481957933262,21.103861776483,-20.0146795714722));
#32103=CARTESIAN_POINT('Ctrl Pts',(-25.6548098153013,21.1095492941272,-20.0152122728861));
#32104=CARTESIAN_POINT('Ctrl Pts',(-25.6646391023183,21.1180713369771,-20.0160083821883));
#32105=CARTESIAN_POINT('Ctrl Pts',(-25.667871973619,21.1208855703497,-20.0162709464227));
#32106=CARTESIAN_POINT('Ctrl Pts',(-25.6736308473351,21.1259189332804,-20.0167399609807));
#32107=CARTESIAN_POINT('Ctrl Pts',(-25.6761590139065,21.1281355864409,-20.016946307753));
#32108=CARTESIAN_POINT('Ctrl Pts',(-25.6810395243587,21.1324282622721,-20.0173455197156));
#32109=CARTESIAN_POINT('Ctrl Pts',(-25.6833923156485,21.1345037724241,-20.017538363306));
#32110=CARTESIAN_POINT('Ctrl Pts',(-25.688481870819,21.1390067461524,-20.0179563743439));
#32111=CARTESIAN_POINT('Ctrl Pts',(-25.6912175374457,21.1414354383975,-20.0181815932918));
#32112=CARTESIAN_POINT('Ctrl Pts',(-25.7019722084491,21.1510161009857,-20.0190691092503));
#32113=CARTESIAN_POINT('Ctrl Pts',(-25.709959488574,21.1582034365274,-20.0197328964554));
#32114=CARTESIAN_POINT('Ctrl Pts',(-25.7878670596029,21.229016676879,-20.0262535134748));
#32115=CARTESIAN_POINT('Ctrl Pts',(-25.8549851260073,21.2956440718766,-20.0322387819725));
#32116=CARTESIAN_POINT('Ctrl Pts',(-25.9633729879638,21.4131432674172,-20.0425673365422));
#32117=CARTESIAN_POINT('Ctrl Pts',(-26.0061998656384,21.4625005900652,-20.0468440646524));
#32118=CARTESIAN_POINT('Ctrl Pts',(-26.234049278312,21.7418128355501,-20.0706906139472));
#32119=CARTESIAN_POINT('Ctrl Pts',(-26.3882879258702,21.9950177552171,-20.091191647569));
#32120=CARTESIAN_POINT('Ctrl Pts',(-26.5274473670701,22.3152032224774,-20.1138764610917));
#32121=CARTESIAN_POINT('Ctrl Pts',(-26.5477329248028,22.3652850038846,-20.1173336060852));
#32122=CARTESIAN_POINT('Ctrl Pts',(-26.5685836657827,22.4207296979341,-20.1210438005859));
#32123=CARTESIAN_POINT('Ctrl Pts',(-26.5704044321117,22.4256071803502,-20.1213692038817));
#32124=CARTESIAN_POINT('Ctrl Pts',(-26.573088496102,22.4328507963107,-20.1218509840738));
#32125=CARTESIAN_POINT('Ctrl Pts',(-26.5739608408444,22.4352135336148,-20.1220078987762));
#32126=CARTESIAN_POINT('Ctrl Pts',(-26.5754487451984,22.4392580944012,-20.1222761050777));
#32127=CARTESIAN_POINT('Ctrl Pts',(-26.576065672528,22.4409394078694,-20.1223874789815));
#32128=CARTESIAN_POINT('Ctrl Pts',(-26.577265705739,22.4442183102791,-20.1226044479894));
#32129=CARTESIAN_POINT('Ctrl Pts',(-26.5778489469364,22.4458158421532,-20.1227100508703));
#32130=CARTESIAN_POINT('Ctrl Pts',(-26.5792550493484,22.4496767231417,-20.1229650106527));
#32131=CARTESIAN_POINT('Ctrl Pts',(-26.5800766404044,22.4519405392733,-20.1231142907623));
#32132=CARTESIAN_POINT('Ctrl Pts',(-26.5825858790168,22.4588787500655,-20.1235711572206));
#32133=CARTESIAN_POINT('Ctrl Pts',(-26.5842652626288,22.4635561574379,-20.1238782491583));
#32134=CARTESIAN_POINT('Ctrl Pts',(-26.6017084467488,22.5124944297801,-20.1270819847663));
#32135=CARTESIAN_POINT('Ctrl Pts',(-26.6165143756569,22.5570939559234,-20.1299224801813));
#32136=CARTESIAN_POINT('Ctrl Pts',(-26.6566799556547,22.6875592705903,-20.1380465941811));
#32137=CARTESIAN_POINT('Ctrl Pts',(-26.6794453249952,22.7741816695343,-20.1432114601558));
#32138=CARTESIAN_POINT('Ctrl Pts',(-26.7478922037191,23.0871221436809,-20.1614170461536));
#32139=CARTESIAN_POINT('Ctrl Pts',(-26.7728426734292,23.3172330135266,-20.174018082798));
#32140=CARTESIAN_POINT('Ctrl Pts',(-26.7730017660406,23.5480310413434,-20.1872301387646));
#32141=CARTESIAN_POINT('Ctrl Pts',(-22.0750360153462,26.4155367745563,-20.5963779455771));
#32142=CARTESIAN_POINT('Ctrl Pts',(-22.1638777420742,26.4612777103593,-20.5902262515474));
#32143=CARTESIAN_POINT('Ctrl Pts',(-22.2548169866545,26.5028664262311,-20.5840745575176));
#32144=CARTESIAN_POINT('Ctrl Pts',(-22.3474260531731,26.5401231016468,-20.5779228634878));
#32145=CARTESIAN_POINT('Ctrl Pts',(-22.4401405378047,26.5774221868239,-20.5717641669042));
#32146=CARTESIAN_POINT('Ctrl Pts',(-22.5345282342079,26.6103792283644,-20.5656054703206));
#32147=CARTESIAN_POINT('Ctrl Pts',(-22.6301437886602,26.6388634595212,-20.559446773737));
#32148=CARTESIAN_POINT('Ctrl Pts',(-22.7258238098815,26.6673668955695,-20.5532839247822));
#32149=CARTESIAN_POINT('Ctrl Pts',(-22.822732916224,26.6913914138537,-20.5471210758275));
#32150=CARTESIAN_POINT('Ctrl Pts',(-22.9204149840781,26.7108572564443,-20.5409582268727));
#32151=CARTESIAN_POINT('Ctrl Pts',(-23.0182467023896,26.7303529210106,-20.5347859363369));
#32152=CARTESIAN_POINT('Ctrl Pts',(-23.1168533171266,26.7452759086086,-20.528613645801));
#32153=CARTESIAN_POINT('Ctrl Pts',(-23.2157732093474,26.7555982455638,-20.5224413552651));
#32154=CARTESIAN_POINT('Ctrl Pts',(-23.2433700368798,26.7584779874063,-20.5207193999175));
#32155=CARTESIAN_POINT('Ctrl Pts',(-23.2709912485032,26.7609999694031,-20.5189974445698));
#32156=CARTESIAN_POINT('Ctrl Pts',(-23.2986268448676,26.7631643070514,-20.5172754892222));
#32157=CARTESIAN_POINT('Ctrl Pts',(-23.3976825053207,26.7709220515331,-20.5111033979099));
#32158=CARTESIAN_POINT('Ctrl Pts',(-23.4972717224806,26.7741082642045,-20.5049313065975));
#32159=CARTESIAN_POINT('Ctrl Pts',(-23.5969366756859,26.7726643851356,-20.4987592152852));
#32160=CARTESIAN_POINT('Ctrl Pts',(-23.6964665927324,26.7712224623802,-20.4925954865464));
#32161=CARTESIAN_POINT('Ctrl Pts',(-23.7960716113389,26.7651629230061,-20.4864317578076));
#32162=CARTESIAN_POINT('Ctrl Pts',(-23.8952892272566,26.7544789970389,-20.4802680290689));
#32163=CARTESIAN_POINT('Ctrl Pts',(-23.9944017314228,26.7438063896885,-20.4741108302222));
#32164=CARTESIAN_POINT('Ctrl Pts',(-24.0931272193255,26.7285191818588,-20.4679536313755));
#32165=CARTESIAN_POINT('Ctrl Pts',(-24.1910045961852,26.7086626308344,-20.4617964325288));
#32166=CARTESIAN_POINT('Ctrl Pts',(-24.2888104306174,26.6888205937446,-20.4556437342211));
#32167=CARTESIAN_POINT('Ctrl Pts',(-24.3857689620633,26.6644159398765,-20.4494910359134));
#32168=CARTESIAN_POINT('Ctrl Pts',(-24.4814265383603,26.6355454726982,-20.4433383376057));
#32169=CARTESIAN_POINT('Ctrl Pts',(-24.5770478411683,26.6066859532422,-20.4371879724099));
#32170=CARTESIAN_POINT('Ctrl Pts',(-24.6713687536461,26.5733641107049,-20.4310376072142));
#32171=CARTESIAN_POINT('Ctrl Pts',(-24.7639489711685,26.5357271196462,-20.4248872420184));
#32172=CARTESIAN_POINT('Ctrl Pts',(-24.8565188500734,26.4980943315854,-20.4187375636462));
#32173=CARTESIAN_POINT('Ctrl Pts',(-24.947348018071,26.4561475166455,-20.412587885274));
#32174=CARTESIAN_POINT('Ctrl Pts',(-25.0360153539962,26.4100823165529,-20.4064382069018));
#32175=CARTESIAN_POINT('Ctrl Pts',(-25.1246965091997,26.3640099369527,-20.4002875700694));
#32176=CARTESIAN_POINT('Ctrl Pts',(-25.2112147775757,26.3138180975655,-20.3941369332369));
#32177=CARTESIAN_POINT('Ctrl Pts',(-25.2951737847896,26.2597483119079,-20.3879862964045));
#32178=CARTESIAN_POINT('Ctrl Pts',(-25.3792226105042,26.205620682938,-20.3818290796827));
#32179=CARTESIAN_POINT('Ctrl Pts',(-25.4607063418638,26.1476070590383,-20.3756718629608));
#32180=CARTESIAN_POINT('Ctrl Pts',(-25.539257859553,26.0859921414036,-20.369514646239));
#32181=CARTESIAN_POINT('Ctrl Pts',(-25.6178532008122,26.0243428490588,-20.3633539944312));
#32182=CARTESIAN_POINT('Ctrl Pts',(-25.6935127416238,25.9590885455185,-20.3571933426234));
#32183=CARTESIAN_POINT('Ctrl Pts',(-25.7659043162503,25.890552668876,-20.3510326908156));
#32184=CARTESIAN_POINT('Ctrl Pts',(-25.838417027724,25.8219021073403,-20.3448617300466));
#32185=CARTESIAN_POINT('Ctrl Pts',(-25.9076505485135,25.7499593172403,-20.3386907692775));
#32186=CARTESIAN_POINT('Ctrl Pts',(-25.9733111872545,25.6750829518017,-20.3325198085085));
#32187=CARTESIAN_POINT('Ctrl Pts',(-26.0234311856438,25.6179284161905,-20.3278093982881));
#32188=CARTESIAN_POINT('Ctrl Pts',(-26.0714702194857,25.559065345811,-20.3230989880677));
#32189=CARTESIAN_POINT('Ctrl Pts',(-26.1173147644303,25.4986644634375,-20.3183885778473));
#32190=CARTESIAN_POINT('Ctrl Pts',(-26.1775491597017,25.419304735295,-20.3121996471588));
#32191=CARTESIAN_POINT('Ctrl Pts',(-26.2342080193949,25.3370069965089,-20.3060107164704));
#32192=CARTESIAN_POINT('Ctrl Pts',(-26.2869923957093,25.2521257582334,-20.2998217857819));
#32193=CARTESIAN_POINT('Ctrl Pts',(-26.3397054514696,25.1673592087609,-20.2936412173778));
#32194=CARTESIAN_POINT('Ctrl Pts',(-26.3885542013232,25.0800164585051,-20.2874606489738));
#32195=CARTESIAN_POINT('Ctrl Pts',(-26.4332805275755,24.9904841580185,-20.2812800805697));
#32196=CARTESIAN_POINT('Ctrl Pts',(-26.4779581565968,24.9010493387132,-20.2751062414589));
#32197=CARTESIAN_POINT('Ctrl Pts',(-26.518522092179,24.8094300906717,-20.2689324023481));
#32198=CARTESIAN_POINT('Ctrl Pts',(-26.5547585763202,24.7160402440611,-20.2627585632373));
#32199=CARTESIAN_POINT('Ctrl Pts',(-26.5909645161969,24.6227291171236,-20.2565899281461));
#32200=CARTESIAN_POINT('Ctrl Pts',(-26.6228501031439,24.5276507598022,-20.250421293055));
#32201=CARTESIAN_POINT('Ctrl Pts',(-26.6502488565259,24.4312408111453,-20.2442526579638));
#32202=CARTESIAN_POINT('Ctrl Pts',(-26.6776333669897,24.334880980061,-20.2380872295648));
#32203=CARTESIAN_POINT('Ctrl Pts',(-26.700535564415,24.2371913478903,-20.2319218011657));
#32204=CARTESIAN_POINT('Ctrl Pts',(-26.7188384674342,24.138623783822,-20.2257563727666));
#32205=CARTESIAN_POINT('Ctrl Pts',(-26.7371416973062,24.040054459537,-20.2195908342654));
#32206=CARTESIAN_POINT('Ctrl Pts',(-26.7508453764792,23.9406075932114,-20.2134252957643));
#32207=CARTESIAN_POINT('Ctrl Pts',(-26.7598835437495,23.8407457828255,-20.2072597572632));
#32208=CARTESIAN_POINT('Ctrl Pts',(-26.7686952713363,23.7433858819598,-20.2012486884178));
#32209=CARTESIAN_POINT('Ctrl Pts',(-26.7730725069817,23.6456319789118,-20.1952376195724));
#32210=CARTESIAN_POINT('Ctrl Pts',(-26.7730016852365,23.5479167572311,-20.189226550727));
#32211=CARTESIAN_POINT('',(-26.7730016643153,23.5526169957307,-20.4357734492732));
#32212=CARTESIAN_POINT('Ctrl Pts',(-22.0750362008293,26.4155368700539,-20.8439479435254));
#32213=CARTESIAN_POINT('Ctrl Pts',(-22.1728011864774,26.4658720153252,-20.8377462766994));
#32214=CARTESIAN_POINT('Ctrl Pts',(-22.2731130362056,26.5111884925568,-20.8314660366905));
#32215=CARTESIAN_POINT('Ctrl Pts',(-22.3953000544431,26.5590148235372,-20.823786419488));
#32216=CARTESIAN_POINT('Ctrl Pts',(-22.4150894173956,26.5665367406279,-20.8225418481915));
#32217=CARTESIAN_POINT('Ctrl Pts',(-22.4402142728685,26.5758043980314,-20.8209600092893));
#32218=CARTESIAN_POINT('Ctrl Pts',(-22.4454824364433,26.5777320226312,-20.8206282358822));
#32219=CARTESIAN_POINT('Ctrl Pts',(-22.4545154449924,26.5810104893776,-20.8200591849443));
#32220=CARTESIAN_POINT('Ctrl Pts',(-22.4582778319827,26.5823680994493,-20.8198221134987));
#32221=CARTESIAN_POINT('Ctrl Pts',(-22.467444802669,26.5856566106294,-20.8192443568174));
#32222=CARTESIAN_POINT('Ctrl Pts',(-22.4728520225352,26.5875800811548,-20.8189034456791));
#32223=CARTESIAN_POINT('Ctrl Pts',(-22.4847371184443,26.5917721479415,-20.8181538442351));
#32224=CARTESIAN_POINT('Ctrl Pts',(-22.4912171506158,26.594034510165,-20.8177449636832));
#32225=CARTESIAN_POINT('Ctrl Pts',(-22.5057864918327,26.5990689209045,-20.8168252176098));
#32226=CARTESIAN_POINT('Ctrl Pts',(-22.5138796845367,26.601829501582,-20.8163139983253));
#32227=CARTESIAN_POINT('Ctrl Pts',(-22.5278247006265,26.6065242599274,-20.8154325620961));
#32228=CARTESIAN_POINT('Ctrl Pts',(-22.5336712881877,26.6084739300081,-20.8150628371232));
#32229=CARTESIAN_POINT('Ctrl Pts',(-22.5521150338715,26.6145656591625,-20.8138959138742));
#32230=CARTESIAN_POINT('Ctrl Pts',(-22.5647320687554,26.6186467073016,-20.8130967871932));
#32231=CARTESIAN_POINT('Ctrl Pts',(-22.5973670987757,26.6289806338534,-20.8110273103342));
#32232=CARTESIAN_POINT('Ctrl Pts',(-22.6174213489648,26.6351161149852,-20.8097532256629));
#32233=CARTESIAN_POINT('Ctrl Pts',(-22.6435980254541,26.6428461280065,-20.8080866088396));
#32234=CARTESIAN_POINT('Ctrl Pts',(-22.6496675823347,26.6446190732861,-20.8076999245154));
#32235=CARTESIAN_POINT('Ctrl Pts',(-22.6593673566637,26.6474214656511,-20.8070815542785));
#32236=CARTESIAN_POINT('Ctrl Pts',(-22.6629942538854,26.6484624259435,-20.8068502448462));
#32237=CARTESIAN_POINT('Ctrl Pts',(-22.669526467058,26.6503248336288,-20.8064334785065));
#32238=CARTESIAN_POINT('Ctrl Pts',(-22.6724311293727,26.6511485737564,-20.8062480966874));
#32239=CARTESIAN_POINT('Ctrl Pts',(-22.6784146895188,26.6528363848247,-20.8058660888893));
#32240=CARTESIAN_POINT('Ctrl Pts',(-22.6814937236553,26.6536999570736,-20.805669446869));
#32241=CARTESIAN_POINT('Ctrl Pts',(-22.6907101316287,26.6562700790897,-20.8050806373804));
#32242=CARTESIAN_POINT('Ctrl Pts',(-22.6968512582895,26.6579630085337,-20.804688026764));
#32243=CARTESIAN_POINT('Ctrl Pts',(-22.7264740353126,26.6660347174153,-20.8027928565694));
#32244=CARTESIAN_POINT('Ctrl Pts',(-22.7500219001005,26.6721654907448,-20.8012822608865));
#32245=CARTESIAN_POINT('Ctrl Pts',(-22.8136341204583,26.6879601862086,-20.7971896458651));
#32246=CARTESIAN_POINT('Ctrl Pts',(-22.8538170594614,26.6971229434944,-20.7945917207726));
#32247=CARTESIAN_POINT('Ctrl Pts',(-22.9715958797011,26.72161329674,-20.7869374055628));
#32248=CARTESIAN_POINT('Ctrl Pts',(-23.0495893452092,26.7348572693042,-20.7818181383961));
#32249=CARTESIAN_POINT('Ctrl Pts',(-23.2168930447791,26.7569691619173,-20.7707356370175));
#32250=CARTESIAN_POINT('Ctrl Pts',(-23.3062465495207,26.7650028202297,-20.764755701666));
#32251=CARTESIAN_POINT('Ctrl Pts',(-23.6423057295988,26.7811257644728,-20.7421248145408));
#32252=CARTESIAN_POINT('Ctrl Pts',(-23.8893464196204,26.7646018520771,-20.7251397971366));
#32253=CARTESIAN_POINT('Ctrl Pts',(-24.1672613922096,26.713588823874,-20.7069900151416));
#32254=CARTESIAN_POINT('Ctrl Pts',(-24.202326985266,26.7065471320127,-20.7047193356227));
#32255=CARTESIAN_POINT('Ctrl Pts',(-24.2418072720009,26.6979328159498,-20.7021902556745));
#32256=CARTESIAN_POINT('Ctrl Pts',(-24.2463425686781,26.6969329717431,-20.7019001394121));
#32257=CARTESIAN_POINT('Ctrl Pts',(-24.2531964449155,26.6954064341752,-20.7014623463951));
#32258=CARTESIAN_POINT('Ctrl Pts',(-24.2555166044744,26.6948869783607,-20.701314256522));
#32259=CARTESIAN_POINT('Ctrl Pts',(-24.2595472996977,26.6939798689087,-20.7010571828101));
#32260=CARTESIAN_POINT('Ctrl Pts',(-24.2612580934725,26.6935933865525,-20.7009481312661));
#32261=CARTESIAN_POINT('Ctrl Pts',(-24.2648356490652,26.6927821172494,-20.70072021548));
#32262=CARTESIAN_POINT('Ctrl Pts',(-24.2667023466836,26.6923570637467,-20.7006013673076));
#32263=CARTESIAN_POINT('Ctrl Pts',(-24.271161130064,26.6913376033693,-20.7003176612241));
#32264=CARTESIAN_POINT('Ctrl Pts',(-24.2737528686925,26.6907416492027,-20.7001528930762));
#32265=CARTESIAN_POINT('Ctrl Pts',(-24.2825118407148,26.6887161598126,-20.6995965129649));
#32266=CARTESIAN_POINT('Ctrl Pts',(-24.2886756492856,26.6872716488953,-20.6992057620682));
#32267=CARTESIAN_POINT('Ctrl Pts',(-24.3033008666448,26.6837986820017,-20.6982803752122));
#32268=CARTESIAN_POINT('Ctrl Pts',(-24.3117584462962,26.6817540911566,-20.6977466446204));
#32269=CARTESIAN_POINT('Ctrl Pts',(-24.4105428425839,26.6574494290197,-20.691528060085));
#32270=CARTESIAN_POINT('Ctrl Pts',(-24.4998829263389,26.6313201566784,-20.6860541746404));
#32271=CARTESIAN_POINT('Ctrl Pts',(-24.7138612024888,26.5585431990297,-20.6730351439377));
#32272=CARTESIAN_POINT('Ctrl Pts',(-24.8369832640881,26.5079756012638,-20.6656185777861));
#32273=CARTESIAN_POINT('Ctrl Pts',(-25.0159081157461,26.4211950756656,-20.6545073286861));
#32274=CARTESIAN_POINT('Ctrl Pts',(-25.0742856695943,26.3906363450886,-20.6508266112345));
#32275=CARTESIAN_POINT('Ctrl Pts',(-25.2109697327046,26.3136590796689,-20.6420021301325));
#32276=CARTESIAN_POINT('Ctrl Pts',(-25.2883242426479,26.2656719677553,-20.6368389076801));
#32277=CARTESIAN_POINT('Ctrl Pts',(-25.4596775539725,26.1490478180627,-20.624859523605));
#32278=CARTESIAN_POINT('Ctrl Pts',(-25.5521914651937,26.0784686239829,-20.6179901499027));
#32279=CARTESIAN_POINT('Ctrl Pts',(-25.6487442819638,25.9961801944573,-20.6102706684643));
#32280=CARTESIAN_POINT('Ctrl Pts',(-25.6567718942425,25.9892699421326,-20.6096245169186));
#32281=CARTESIAN_POINT('Ctrl Pts',(-25.6680023711404,25.9795058285841,-20.6087143845018));
#32282=CARTESIAN_POINT('Ctrl Pts',(-25.6712338874162,25.9766849027516,-20.6084517739132));
#32283=CARTESIAN_POINT('Ctrl Pts',(-25.6768334831204,25.9717770479041,-20.6079954562565));
#32284=CARTESIAN_POINT('Ctrl Pts',(-25.6792041522966,25.9696930708689,-20.6078018726408));
#32285=CARTESIAN_POINT('Ctrl Pts',(-25.6839683569311,25.9654925918635,-20.6074120403205));
#32286=CARTESIAN_POINT('Ctrl Pts',(-25.6863618136091,25.9633760069261,-20.6072157882734));
#32287=CARTESIAN_POINT('Ctrl Pts',(-25.6912358597575,25.9590528500609,-20.6068153070132));
#32288=CARTESIAN_POINT('Ctrl Pts',(-25.6937161942924,25.9568459979444,-20.6066110661496));
#32289=CARTESIAN_POINT('Ctrl Pts',(-25.7018764469939,25.949562874211,-20.605937657493));
#32290=CARTESIAN_POINT('Ctrl Pts',(-25.7075417447434,25.9444703251003,-20.6054678033207));
#32291=CARTESIAN_POINT('Ctrl Pts',(-25.7453762986048,25.9102174462648,-20.6023141873179));
#32292=CARTESIAN_POINT('Ctrl Pts',(-25.7769701735555,25.8804308501906,-20.5996038495936));
#32293=CARTESIAN_POINT('Ctrl Pts',(-25.8646841965859,25.7943211959147,-20.5918526594682));
#32294=CARTESIAN_POINT('Ctrl Pts',(-25.9193322750013,25.736550206616,-20.5867491694219));
#32295=CARTESIAN_POINT('Ctrl Pts',(-26.0046111093449,25.6394428677489,-20.5783217624909));
#32296=CARTESIAN_POINT('Ctrl Pts',(-26.0365658478906,25.6013103125668,-20.5750479017174));
#32297=CARTESIAN_POINT('Ctrl Pts',(-26.2581846089199,25.324053512358,-20.5515095091151));
#32298=CARTESIAN_POINT('Ctrl Pts',(-26.4138994550013,25.0598148845557,-20.5302607346492));
#32299=CARTESIAN_POINT('Ctrl Pts',(-26.5441958444199,24.7434774216934,-20.5082673758524));
#32300=CARTESIAN_POINT('Ctrl Pts',(-26.5576772209766,24.7090791917104,-20.5059205628949));
#32301=CARTESIAN_POINT('Ctrl Pts',(-26.5723581623587,24.6696369824769,-20.5032863829817));
#32302=CARTESIAN_POINT('Ctrl Pts',(-26.5741399697726,24.6648146673562,-20.5029652795554));
#32303=CARTESIAN_POINT('Ctrl Pts',(-26.5767546689224,24.6576857754895,-20.5024920250336));
#32304=CARTESIAN_POINT('Ctrl Pts',(-26.5775964681088,24.6553825090545,-20.5023393428675));
#32305=CARTESIAN_POINT('Ctrl Pts',(-26.579081250292,24.6513055346493,-20.5020694766608));
#32306=CARTESIAN_POINT('Ctrl Pts',(-26.5797253051365,24.6495322217483,-20.5019522279953));
#32307=CARTESIAN_POINT('Ctrl Pts',(-26.5810661292679,24.6458303263405,-20.5017077405588));
#32308=CARTESIAN_POINT('Ctrl Pts',(-26.581762613718,24.6439016481864,-20.5015805191754));
#32309=CARTESIAN_POINT('Ctrl Pts',(-26.5835750936215,24.6388675631667,-20.5012488594026));
#32310=CARTESIAN_POINT('Ctrl Pts',(-26.5846881648032,24.635761094625,-20.5010445968256));
#32311=CARTESIAN_POINT('Ctrl Pts',(-26.589489014007,24.6222973255368,-20.5001610117546));
#32312=CARTESIAN_POINT('Ctrl Pts',(-26.5931286070458,24.6119227411936,-20.4994845421618));
#32313=CARTESIAN_POINT('Ctrl Pts',(-26.6190264814844,24.5368741069226,-20.4946212373618));
#32314=CARTESIAN_POINT('Ctrl Pts',(-26.6392758342009,24.4715192153636,-20.4905476198389));
#32315=CARTESIAN_POINT('Ctrl Pts',(-26.7339273442685,24.1276688725295,-20.4697100781083));
#32316=CARTESIAN_POINT('Ctrl Pts',(-26.7728002853682,23.840763589504,-20.45422022849));
#32317=CARTESIAN_POINT('Ctrl Pts',(-26.7730017446375,23.5525048579221,-20.4377341936612));
#32318=CARTESIAN_POINT('Ctrl Pts',(-26.7730016643153,23.5526169957307,-20.4357734492732));
#32319=CARTESIAN_POINT('Ctrl Pts',(-26.773075151987,23.4524537761962,-20.4296113721848));
#32320=CARTESIAN_POINT('Ctrl Pts',(-26.7684747048648,23.35224768617,-20.4234492950963));
#32321=CARTESIAN_POINT('Ctrl Pts',(-26.7592150105535,23.2524650709557,-20.4172872180079));
#32322=CARTESIAN_POINT('Ctrl Pts',(-26.7499560101931,23.152689933767,-20.411125602725));
#32323=CARTESIAN_POINT('Ctrl Pts',(-26.7360384965427,23.0533386380498,-20.4049639874422));
#32324=CARTESIAN_POINT('Ctrl Pts',(-26.7175290969173,22.9548730544796,-20.3988023721593));
#32325=CARTESIAN_POINT('Ctrl Pts',(-26.6990162147105,22.8563889444077,-20.3926395975559));
#32326=CARTESIAN_POINT('Ctrl Pts',(-26.6759098092089,22.7587913018524,-20.3864768229525));
#32327=CARTESIAN_POINT('Ctrl Pts',(-26.6483275643628,22.662531486289,-20.3803140483491));
#32328=CARTESIAN_POINT('Ctrl Pts',(-26.6206478325784,22.5659314491534,-20.3741294919788));
#32329=CARTESIAN_POINT('Ctrl Pts',(-26.5884606872596,22.4706791326,-20.3679449356084));
#32330=CARTESIAN_POINT('Ctrl Pts',(-26.5519348922841,22.3772135005348,-20.3617603792381));
#32331=CARTESIAN_POINT('Ctrl Pts',(-26.5154740447795,22.2839140621532,-20.3555868197891));
#32332=CARTESIAN_POINT('Ctrl Pts',(-26.474690179984,22.1923953376775,-20.3494132603401));
#32333=CARTESIAN_POINT('Ctrl Pts',(-26.4297981252393,22.1030708785507,-20.3432397008912));
#32334=CARTESIAN_POINT('Ctrl Pts',(-26.3847861216062,22.0135077498055,-20.3370496460602));
#32335=CARTESIAN_POINT('Ctrl Pts',(-26.3356441787839,21.9261509953061,-20.3308595912292));
#32336=CARTESIAN_POINT('Ctrl Pts',(-26.2826327711642,21.8413886431841,-20.3246695363982));
#32337=CARTESIAN_POINT('Ctrl Pts',(-26.2296213635445,21.7566262910621,-20.3184794815671));
#32338=CARTESIAN_POINT('Ctrl Pts',(-26.1727407892357,21.6744586579882,-20.3122894267362));
#32339=CARTESIAN_POINT('Ctrl Pts',(-26.1122913561492,21.5952398400511,-20.3060993719051));
#32340=CARTESIAN_POINT('Ctrl Pts',(-26.0520173471179,21.5162509148622,-20.2999272805928));
#32341=CARTESIAN_POINT('Ctrl Pts',(-25.9879808586206,21.4399129016145,-20.2937551892805));
#32342=CARTESIAN_POINT('Ctrl Pts',(-25.920443548776,21.366606016105,-20.2875830979682));
#32343=CARTESIAN_POINT('Ctrl Pts',(-25.8529977453093,21.2933984541781,-20.2814193692294));
#32344=CARTESIAN_POINT('Ctrl Pts',(-25.7820608399872,21.2232141737987,-20.2752556404906));
#32345=CARTESIAN_POINT('Ctrl Pts',(-25.7079362077355,21.1564023449355,-20.2690919117518));
#32346=CARTESIAN_POINT('Ctrl Pts',(-25.6338901035747,21.0896612969342,-20.2629347129051));
#32347=CARTESIAN_POINT('Ctrl Pts',(-25.5566633073516,21.0262858866402,-20.2567775140585));
#32348=CARTESIAN_POINT('Ctrl Pts',(-25.4765970244963,20.9665895394386,-20.2506203152118));
#32349=CARTESIAN_POINT('Ctrl Pts',(-25.3965892652386,20.9069368266469,-20.2444676169041));
#32350=CARTESIAN_POINT('Ctrl Pts',(-25.3137464929835,20.8509580892937,-20.2383149185964));
#32351=CARTESIAN_POINT('Ctrl Pts',(-25.2284433619803,20.7989268331184,-20.2321622202887));
#32352=CARTESIAN_POINT('Ctrl Pts',(-25.1431725780458,20.7469153072695,-20.2260118550929));
#32353=CARTESIAN_POINT('Ctrl Pts',(-25.0554436596131,20.6988485142483,-20.2198614898972));
#32354=CARTESIAN_POINT('Ctrl Pts',(-24.9656598963966,20.6549564234444,-20.2137111247014));
#32355=CARTESIAN_POINT('Ctrl Pts',(-24.8758861595119,20.6110692341579,-20.2075614463292));
#32356=CARTESIAN_POINT('Ctrl Pts',(-24.7840584243222,20.5713560110114,-20.201411767957));
#32357=CARTESIAN_POINT('Ctrl Pts',(-24.6906033055421,20.536000107778,-20.1952620895848));
#32358=CARTESIAN_POINT('Ctrl Pts',(-24.5971336212825,20.5006386941383,-20.1891114527524));
#32359=CARTESIAN_POINT('Ctrl Pts',(-24.5020364559823,20.469636103026,-20.1829608159199));
#32360=CARTESIAN_POINT('Ctrl Pts',(-24.4057561053769,20.4431266575275,-20.1768101790875));
#32361=CARTESIAN_POINT('Ctrl Pts',(-24.3093727550212,20.4165888524909,-20.1706529623657));
#32362=CARTESIAN_POINT('Ctrl Pts',(-24.211804111398,20.3945539071583,-20.1644957456439));
#32363=CARTESIAN_POINT('Ctrl Pts',(-24.1135071448038,20.377105544347,-20.1583385289221));
#32364=CARTESIAN_POINT('Ctrl Pts',(-24.0151553387346,20.3596474471655,-20.1521778771142));
#32365=CARTESIAN_POINT('Ctrl Pts',(-23.9160748312988,20.3467810843303,-20.1460172253064));
#32366=CARTESIAN_POINT('Ctrl Pts',(-23.816728150589,20.3385382998494,-20.1398565734986));
#32367=CARTESIAN_POINT('Ctrl Pts',(-23.7172152275543,20.3302817222589,-20.1336856127296));
#32368=CARTESIAN_POINT('Ctrl Pts',(-23.617435675889,20.3266641930229,-20.1275146519606));
#32369=CARTESIAN_POINT('Ctrl Pts',(-23.5178526092488,20.3276654021466,-20.1213436911915));
#32370=CARTESIAN_POINT('Ctrl Pts',(-23.4418389847191,20.3284296438694,-20.1166332809711));
#32371=CARTESIAN_POINT('Ctrl Pts',(-23.3659398565144,20.3318839404417,-20.1119228707507));
#32372=CARTESIAN_POINT('Ctrl Pts',(-23.2903581496809,20.3379990434561,-20.1072124605302));
#32373=CARTESIAN_POINT('Ctrl Pts',(-23.1913227845457,20.3460117159035,-20.1010403692179));
#32374=CARTESIAN_POINT('Ctrl Pts',(-23.09248389645,20.3586227557379,-20.0948682779056));
#32375=CARTESIAN_POINT('Ctrl Pts',(-22.994302804629,20.3758175483505,-20.0886961865933));
#32376=CARTESIAN_POINT('Ctrl Pts',(-22.8962547384809,20.3929890437191,-20.0825324578545));
#32377=CARTESIAN_POINT('Ctrl Pts',(-22.7988631212729,20.4147318734957,-20.0763687291157));
#32378=CARTESIAN_POINT('Ctrl Pts',(-22.7025857025666,20.4409795444355,-20.0702050003769));
#32379=CARTESIAN_POINT('Ctrl Pts',(-22.6064102807493,20.4671994084313,-20.0640478015302));
#32380=CARTESIAN_POINT('Ctrl Pts',(-22.5113471275059,20.4979145118858,-20.0578906026835));
#32381=CARTESIAN_POINT('Ctrl Pts',(-22.4178443688714,20.5330072126536,-20.0517334038368));
#32382=CARTESIAN_POINT('Ctrl Pts',(-22.3244099550834,20.5680742627852,-20.0455807055291));
#32383=CARTESIAN_POINT('Ctrl Pts',(-22.2325340737648,20.6075123963934,-20.0394280072214));
#32384=CARTESIAN_POINT('Ctrl Pts',(-22.1426493463878,20.6511542520191,-20.0332753089137));
#32385=CARTESIAN_POINT('Ctrl Pts',(-22.0527987034272,20.6947795585911,-20.027124943718));
#32386=CARTESIAN_POINT('Ctrl Pts',(-21.9649381044761,20.7426052302821,-20.0209745785222));
#32387=CARTESIAN_POINT('Ctrl Pts',(-21.8794790218281,20.794416280893,-20.0148242133265));
#32388=CARTESIAN_POINT('Ctrl Pts',(-21.7940294825662,20.8462215456607,-20.0086745349543));
#32389=CARTESIAN_POINT('Ctrl Pts',(-21.7109812978908,20.9020110793106,-20.0025248565821));
#32390=CARTESIAN_POINT('Ctrl Pts',(-21.630719329746,20.9615250742127,-19.9963751782098));
#32391=CARTESIAN_POINT('Ctrl Pts',(-21.5504448523447,21.0210483446889,-19.9902245413774));
#32392=CARTESIAN_POINT('Ctrl Pts',(-21.472957802973,21.0842969706306,-19.984073904545));
#32393=CARTESIAN_POINT('Ctrl Pts',(-21.398611350577,21.1509697659034,-19.9779232677125));
#32394=CARTESIAN_POINT('Ctrl Pts',(-21.3241853630945,21.2177138870616,-19.9717660509907));
#32395=CARTESIAN_POINT('Ctrl Pts',(-21.2529070057718,21.2878892018926,-19.9656088342689));
#32396=CARTESIAN_POINT('Ctrl Pts',(-21.1850937278375,21.361156509351,-19.9594516175471));
#32397=CARTESIAN_POINT('Ctrl Pts',(-21.1172426171531,21.43446469234,-19.9532909657393));
#32398=CARTESIAN_POINT('Ctrl Pts',(-21.052860715635,21.5108679710866,-19.9471303139315));
#32399=CARTESIAN_POINT('Ctrl Pts',(-20.9922248302234,21.5899944259826,-19.9409696621237));
#32400=CARTESIAN_POINT('Ctrl Pts',(-20.9314874794131,21.6692532875753,-19.9347987013546));
#32401=CARTESIAN_POINT('Ctrl Pts',(-20.8745089137407,21.7512440706073,-19.9286277405856));
#32402=CARTESIAN_POINT('Ctrl Pts',(-20.8215223786301,21.8355661713767,-19.9224567798166));
#32403=CARTESIAN_POINT('Ctrl Pts',(-20.7810767615102,21.8999308141175,-19.9177463695962));
#32404=CARTESIAN_POINT('Ctrl Pts',(-20.742956222787,21.9656532178648,-19.9130359593758));
#32405=CARTESIAN_POINT('Ctrl Pts',(-20.7072458448747,22.0325468483683,-19.9083255491555));
#32406=CARTESIAN_POINT('Ctrl Pts',(-20.6604542273806,22.1201981518354,-19.9021534578431));
#32407=CARTESIAN_POINT('Ctrl Pts',(-20.6176374976908,22.2101697683839,-19.8959813665308));
#32408=CARTESIAN_POINT('Ctrl Pts',(-20.5790327228931,22.3020656825856,-19.8898092752185));
#32409=CARTESIAN_POINT('Ctrl Pts',(-20.5404802537487,22.3938370869085,-19.8836455464798));
#32410=CARTESIAN_POINT('Ctrl Pts',(-20.5061285634217,22.4875272097641,-19.877481817741));
#32411=CARTESIAN_POINT('Ctrl Pts',(-20.4761691430729,22.5827149963485,-19.8713180890022));
#32412=CARTESIAN_POINT('Ctrl Pts',(-20.4462414619181,22.6778019404071,-19.8651608901555));
#32413=CARTESIAN_POINT('Ctrl Pts',(-20.4206969294587,22.7743829817467,-19.8590036913088));
#32414=CARTESIAN_POINT('Ctrl Pts',(-20.3996788025033,22.8720175138486,-19.8528464924621));
#32415=CARTESIAN_POINT('Ctrl Pts',(-20.3786760385242,22.969580681028,-19.8466937941544));
#32416=CARTESIAN_POINT('Ctrl Pts',(-20.3621931932836,23.0681953846139,-19.8405410958467));
#32417=CARTESIAN_POINT('Ctrl Pts',(-20.3503233130239,23.1674071869397,-19.834388397539));
#32418=CARTESIAN_POINT('Ctrl Pts',(-20.3384579338397,23.2665813680089,-19.8282380323433));
#32419=CARTESIAN_POINT('Ctrl Pts',(-20.331202095456,23.3663517670764,-19.8220876671475));
#32420=CARTESIAN_POINT('Ctrl Pts',(-20.3285973445946,23.4662559964432,-19.8159373019518));
#32421=CARTESIAN_POINT('Ctrl Pts',(-20.3259928846109,23.5661490693058,-19.8097876235796));
#32422=CARTESIAN_POINT('Ctrl Pts',(-20.3280384908415,23.6661755085001,-19.8036379452074));
#32423=CARTESIAN_POINT('Ctrl Pts',(-20.3347236169645,23.7658710861774,-19.7974882668351));
#32424=CARTESIAN_POINT('Ctrl Pts',(-20.3414097850002,23.8655822019431,-19.7913376300027));
#32425=CARTESIAN_POINT('Ctrl Pts',(-20.3527368801113,23.9649619202974,-19.7851869931702));
#32426=CARTESIAN_POINT('Ctrl Pts',(-20.368642412137,24.0635503104069,-19.7790363563378));
#32427=CARTESIAN_POINT('Ctrl Pts',(-20.3845649597408,24.1622441693835,-19.772879139616));
#32428=CARTESIAN_POINT('Ctrl Pts',(-20.4050756556899,24.260144579934,-19.7667219228942));
#32429=CARTESIAN_POINT('Ctrl Pts',(-20.4300607192191,24.356801114151,-19.7605647061723));
#32430=CARTESIAN_POINT('Ctrl Pts',(-20.4550597218129,24.4535115726526,-19.7544040543645));
#32431=CARTESIAN_POINT('Ctrl Pts',(-20.4845379350223,24.5489763577428,-19.7482434025567));
#32432=CARTESIAN_POINT('Ctrl Pts',(-20.5183320825269,24.6427615487833,-19.7420827507489));
#32433=CARTESIAN_POINT('Ctrl Pts',(-20.5521827796576,24.7367036757989,-19.7359117899799));
#32434=CARTESIAN_POINT('Ctrl Pts',(-20.5903636708451,24.8289601931645,-19.7297408292109));
#32435=CARTESIAN_POINT('Ctrl Pts',(-20.6326638005135,24.9191183243077,-19.7235698684418));
#32436=CARTESIAN_POINT('Ctrl Pts',(-20.6649522837129,24.9879377186105,-19.7188594582214));
#32437=CARTESIAN_POINT('Ctrl Pts',(-20.6996398774685,25.055534912831,-19.7141490480009));
#32438=CARTESIAN_POINT('Ctrl Pts',(-20.7366156380375,25.1217374960365,-19.7094386377805));
#32439=CARTESIAN_POINT('Ctrl Pts',(-20.7850601153911,25.2084740362317,-19.7032672066121));
#32440=CARTESIAN_POINT('Ctrl Pts',(-20.8376044284376,25.2931211116169,-19.6970957754438));
#32441=CARTESIAN_POINT('Ctrl Pts',(-20.894043615899,25.3752653421013,-19.6909243442754));
#32442=CARTESIAN_POINT('Ctrl Pts',(-20.9504102682931,25.4573040016598,-19.6847608445673));
#32443=CARTESIAN_POINT('Ctrl Pts',(-21.0106616052613,25.5368458529681,-19.6785973448593));
#32444=CARTESIAN_POINT('Ctrl Pts',(-21.0745469290363,25.6135022333707,-19.6724338451512));
#32445=CARTESIAN_POINT('Ctrl Pts',(-21.1383672489474,25.69008061525,-19.6662766168569));
#32446=CARTESIAN_POINT('Ctrl Pts',(-21.2058139297149,25.7637790299982,-19.6601193885625));
#32447=CARTESIAN_POINT('Ctrl Pts',(-21.2765937197516,25.8342387771378,-19.6539621602682));
#32448=CARTESIAN_POINT('Ctrl Pts',(-21.347318687336,25.9046439497143,-19.647809701052));
#32449=CARTESIAN_POINT('Ctrl Pts',(-21.421371322735,25.9718151382193,-19.6416572418359));
#32450=CARTESIAN_POINT('Ctrl Pts',(-21.4984196399852,26.0354284504173,-19.6355047826197));
#32451=CARTESIAN_POINT('Ctrl Pts',(-21.5754338373058,26.0990135922177,-19.6293550479469));
#32452=CARTESIAN_POINT('Ctrl Pts',(-21.6554407433668,26.1590437153627,-19.623205313274));
#32453=CARTESIAN_POINT('Ctrl Pts',(-21.7380739215636,26.2152340039535,-19.6170555786012));
#32454=CARTESIAN_POINT('Ctrl Pts',(-21.8207025318221,26.2714211863612,-19.6109061838839));
#32455=CARTESIAN_POINT('Ctrl Pts',(-21.9059567684882,26.3237687090981,-19.6047567891666));
#32456=CARTESIAN_POINT('Ctrl Pts',(-21.993440431219,26.3720345300623,-19.5986073944493));
#32457=CARTESIAN_POINT('Ctrl Pts',(-22.0204309851315,26.3869255531653,-19.5967101765635));
#32458=CARTESIAN_POINT('Ctrl Pts',(-22.0476335546389,26.4014283792986,-19.5948129586777));
#32459=CARTESIAN_POINT('Ctrl Pts',(-22.075036015346,26.4155367745563,-19.592915740792));
#32460=CARTESIAN_POINT('Origin',(-23.5502525316942,23.5502525316942,-77.3107734492734));
#32461=CARTESIAN_POINT('',(-22.0750358296283,26.4155366789378,-18.0972636326348));
#32462=CARTESIAN_POINT('',(-22.0750360259987,26.4155367800409,-18.341133076278));
#32463=CARTESIAN_POINT('',(-22.0750360153461,26.4155367745563,-77.3107734492734));
#32464=CARTESIAN_POINT('Ctrl Pts',(-22.0750358296283,26.4155366789378,-18.0972636326348));
#32465=CARTESIAN_POINT('Ctrl Pts',(-22.0020986630162,26.377984338277,-18.102806008076));
#32466=CARTESIAN_POINT('Ctrl Pts',(-21.9305937987179,26.3376462382369,-18.1083246445035));
#32467=CARTESIAN_POINT('Ctrl Pts',(-21.8038493267266,26.2596154407692,-18.1181781376872));
#32468=CARTESIAN_POINT('Ctrl Pts',(-21.7481143339664,26.2228674993881,-18.1225375247352));
#32469=CARTESIAN_POINT('Ctrl Pts',(-21.670171863103,26.1679295164869,-18.1286294835558));
#32470=CARTESIAN_POINT('Ctrl Pts',(-21.6470062787083,26.1511350659498,-18.1304394755775));
#32471=CARTESIAN_POINT('Ctrl Pts',(-21.6205071235855,26.1313801790844,-18.1325062873023));
#32472=CARTESIAN_POINT('Ctrl Pts',(-21.6169532444161,26.1287193510681,-18.1327833966795));
#32473=CARTESIAN_POINT('Ctrl Pts',(-21.6115512989377,26.1246574087145,-18.1332044751031));
#32474=CARTESIAN_POINT('Ctrl Pts',(-21.6096992461742,26.1232616429988,-18.1333488178742));
#32475=CARTESIAN_POINT('Ctrl Pts',(-21.606359336024,26.1207389234167,-18.1336090740878));
#32476=CARTESIAN_POINT('Ctrl Pts',(-21.6048709548795,26.119612679056,-18.1337250370098));
#32477=CARTESIAN_POINT('Ctrl Pts',(-21.601891129799,26.117353799138,-18.1339571683571));
#32478=CARTESIAN_POINT('Ctrl Pts',(-21.6003997007127,26.1162211611328,-18.1340733357544));
#32479=CARTESIAN_POINT('Ctrl Pts',(-21.5961765344237,26.1130081481537,-18.1344022342692));
#32480=CARTESIAN_POINT('Ctrl Pts',(-21.5934471230568,26.1109246984879,-18.134614747664));
#32481=CARTESIAN_POINT('Ctrl Pts',(-21.5820171355823,26.1021708653282,-18.1355044982852));
#32482=CARTESIAN_POINT('Ctrl Pts',(-21.5733471632337,26.0954603676825,-18.1361789268954));
#32483=CARTESIAN_POINT('Ctrl Pts',(-21.4281818613913,25.9819141815755,-18.1474664078731));
#32484=CARTESIAN_POINT('Ctrl Pts',(-21.3004679833139,25.8642642891345,-18.1573323739583));
#32485=CARTESIAN_POINT('Ctrl Pts',(-21.0682662590245,25.6128645685548,-18.1765489436329));
#32486=CARTESIAN_POINT('Ctrl Pts',(-20.9636349811097,25.4800279033554,-18.185882145641));
#32487=CARTESIAN_POINT('Ctrl Pts',(-20.8067748497906,25.2450595326062,-18.2019678016775));
#32488=CARTESIAN_POINT('Ctrl Pts',(-20.7487093743279,25.1472474376841,-18.208551885238));
#32489=CARTESIAN_POINT('Ctrl Pts',(-20.6726468593584,25.0021544072442,-18.2183081332504));
#32490=CARTESIAN_POINT('Ctrl Pts',(-20.650399470392,24.9571943414834,-18.2213292895717));
#32491=CARTESIAN_POINT('Ctrl Pts',(-20.6258784175525,24.9045847803885,-18.2248685794831));
#32492=CARTESIAN_POINT('Ctrl Pts',(-20.6225719084987,24.8974221446742,-18.2253505263329));
#32493=CARTESIAN_POINT('Ctrl Pts',(-20.6175622636763,24.8864645866742,-18.2260879719957));
#32494=CARTESIAN_POINT('Ctrl Pts',(-20.6158401039702,24.8826783524294,-18.226342813992));
#32495=CARTESIAN_POINT('Ctrl Pts',(-20.6128756735162,24.8761273157195,-18.2267837999672));
#32496=CARTESIAN_POINT('Ctrl Pts',(-20.611629961403,24.8733640686204,-18.2269698251464));
#32497=CARTESIAN_POINT('Ctrl Pts',(-20.609058301373,24.8676380478646,-18.2273553427459));
#32498=CARTESIAN_POINT('Ctrl Pts',(-20.6077329280414,24.8646750211089,-18.2275548546781));
#32499=CARTESIAN_POINT('Ctrl Pts',(-20.6045294415223,24.8574841258487,-18.2280390945077));
#32500=CARTESIAN_POINT('Ctrl Pts',(-20.6026559549719,24.8532542144542,-18.2283239809441));
#32501=CARTESIAN_POINT('Ctrl Pts',(-20.5956963639405,24.8374492011152,-18.2293886206598));
#32502=CARTESIAN_POINT('Ctrl Pts',(-20.5906693333279,24.8258483527939,-18.2301703944077));
#32503=CARTESIAN_POINT('Ctrl Pts',(-20.5048355749253,24.6245313883292,-18.243743658637));
#32504=CARTESIAN_POINT('Ctrl Pts',(-20.4423683425129,24.4275585491703,-18.2571737445082));
#32505=CARTESIAN_POINT('Ctrl Pts',(-20.3618196484221,24.051950741957,-18.2829206116642));
#32506=CARTESIAN_POINT('Ctrl Pts',(-20.3389799904374,23.8751095567697,-18.2950839985776));
#32507=CARTESIAN_POINT('Ctrl Pts',(-20.3266631055028,23.605430093448,-18.3131304331952));
#32508=CARTESIAN_POINT('Ctrl Pts',(-20.3264007874225,23.5134243435429,-18.3191945238189));
#32509=CARTESIAN_POINT('Ctrl Pts',(-20.3313362401963,23.3899608836843,-18.3271050704948));
#32510=CARTESIAN_POINT('Ctrl Pts',(-20.3330621556767,23.3584146455631,-18.3291062369557));
#32511=CARTESIAN_POINT('Ctrl Pts',(-20.3355669769764,23.322359935849,-18.3313665519523));
#32512=CARTESIAN_POINT('Ctrl Pts',(-20.3358918191513,23.317823055899,-18.3316504875094));
#32513=CARTESIAN_POINT('Ctrl Pts',(-20.3363984765793,23.3109511314928,-18.3320798055029));
#32514=CARTESIAN_POINT('Ctrl Pts',(-20.3365732322871,23.3086155966791,-18.3322255842483));
#32515=CARTESIAN_POINT('Ctrl Pts',(-20.3368785532151,23.3045940357584,-18.3324763712541));
#32516=CARTESIAN_POINT('Ctrl Pts',(-20.3370078993699,23.3029079237434,-18.332581448628));
#32517=CARTESIAN_POINT('Ctrl Pts',(-20.3372789520385,23.2994106707504,-18.3327992501669));
#32518=CARTESIAN_POINT('Ctrl Pts',(-20.3374208624473,23.2975995525102,-18.3329119623605));
#32519=CARTESIAN_POINT('Ctrl Pts',(-20.3378134090581,23.2926435274327,-18.3332201752954));
#32520=CARTESIAN_POINT('Ctrl Pts',(-20.3380671328196,23.2894988564007,-18.3334155009554));
#32521=CARTESIAN_POINT('Ctrl Pts',(-20.3390535923024,23.2774925657636,-18.334160351134));
#32522=CARTESIAN_POINT('Ctrl Pts',(-20.3398183928529,23.2686335125753,-18.3347080810222));
#32523=CARTESIAN_POINT('Ctrl Pts',(-20.3531492734833,23.1213325664763,-18.3437858295871));
#32524=CARTESIAN_POINT('Ctrl Pts',(-20.3746250627678,22.9838228441027,-18.3518296007611));
#32525=CARTESIAN_POINT('Ctrl Pts',(-20.4493581744545,22.6490452192847,-18.3712707417994));
#32526=CARTESIAN_POINT('Ctrl Pts',(-20.5125940193044,22.4546457854139,-18.3824594673435));
#32527=CARTESIAN_POINT('Ctrl Pts',(-20.6239302144503,22.1980347164166,-18.3983771671318));
#32528=CARTESIAN_POINT('Ctrl Pts',(-20.6565186569245,22.1296334601545,-18.4027361683782));
#32529=CARTESIAN_POINT('Ctrl Pts',(-20.7318549960012,21.9848772975832,-18.4122851134753));
#32530=CARTESIAN_POINT('Ctrl Pts',(-20.7753620094961,21.9089893790141,-18.4174956697838));
#32531=CARTESIAN_POINT('Ctrl Pts',(-20.8269260061065,21.8269709381329,-18.4233961208994));
#32532=CARTESIAN_POINT('Ctrl Pts',(-20.83198940777,21.8189950690965,-18.4239727974267));
#32533=CARTESIAN_POINT('Ctrl Pts',(-20.8395060741637,21.8072690877395,-18.4248249308773));
#32534=CARTESIAN_POINT('Ctrl Pts',(-20.8419322401638,21.803501593215,-18.4250993768899));
#32535=CARTESIAN_POINT('Ctrl Pts',(-20.8462070756401,21.7968936923288,-18.425581900644));
#32536=CARTESIAN_POINT('Ctrl Pts',(-20.848052386662,21.7940511127125,-18.4257898524937));
#32537=CARTESIAN_POINT('Ctrl Pts',(-20.8516463131601,21.7885339813305,-18.4261942059967));
#32538=CARTESIAN_POINT('Ctrl Pts',(-20.8533944301623,21.7858591080257,-18.4263905887921));
#32539=CARTESIAN_POINT('Ctrl Pts',(-20.8575807652294,21.7794741632461,-18.4268601714873));
#32540=CARTESIAN_POINT('Ctrl Pts',(-20.8600226724847,21.7757665282578,-18.4271335099537));
#32541=CARTESIAN_POINT('Ctrl Pts',(-20.8688049317978,21.7624919048084,-18.4281145331383));
#32542=CARTESIAN_POINT('Ctrl Pts',(-20.8751886617104,21.7529538430998,-18.4288238527858));
#32543=CARTESIAN_POINT('Ctrl Pts',(-20.9785398306536,21.600305177606,-18.4402480859513));
#32544=CARTESIAN_POINT('Ctrl Pts',(-21.0867994443325,21.4652148827186,-18.4514049328044));
#32545=CARTESIAN_POINT('Ctrl Pts',(-21.3646770035448,21.1704792752876,-18.4783165566837));
#32546=CARTESIAN_POINT('Ctrl Pts',(-21.5417916363208,21.0192179241965,-18.4942813455054));
#32547=CARTESIAN_POINT('Ctrl Pts',(-21.7948166535963,20.8465416646728,-18.5146317129483));
#32548=CARTESIAN_POINT('Ctrl Pts',(-21.8574449574504,20.806894767084,-18.5194875999644));
#32549=CARTESIAN_POINT('Ctrl Pts',(-21.9475497228463,20.7541158282959,-18.5261669380718));
#32550=CARTESIAN_POINT('Ctrl Pts',(-21.9739265294444,20.7391614166204,-18.5280864433305));
#32551=CARTESIAN_POINT('Ctrl Pts',(-22.00446069886,20.7224149376269,-18.5302642868526));
#32552=CARTESIAN_POINT('Ctrl Pts',(-22.0084143564803,20.7202573212886,-18.530545437944));
#32553=CARTESIAN_POINT('Ctrl Pts',(-22.0144225385172,20.7169948243676,-18.5309713966716));
#32554=CARTESIAN_POINT('Ctrl Pts',(-22.0164737399099,20.7158838855892,-18.5311165913318));
#32555=CARTESIAN_POINT('Ctrl Pts',(-22.0201692336278,20.7138875779177,-18.531377764323));
#32556=CARTESIAN_POINT('Ctrl Pts',(-22.0218130856495,20.713001413117,-18.5314937937483));
#32557=CARTESIAN_POINT('Ctrl Pts',(-22.025343970863,20.7111019490016,-18.5317427011315));
#32558=CARTESIAN_POINT('Ctrl Pts',(-22.027231238995,20.71008910468,-18.5318755495466));
#32559=CARTESIAN_POINT('Ctrl Pts',(-22.0323060928317,20.7073720846653,-18.5322322628288));
#32560=CARTESIAN_POINT('Ctrl Pts',(-22.035495550083,20.7056713825056,-18.5324559050817));
#32561=CARTESIAN_POINT('Ctrl Pts',(-22.0500737023155,20.6979294011274,-18.5334756543707));
#32562=CARTESIAN_POINT('Ctrl Pts',(-22.0614959299326,20.6919510158999,-18.5342678004516));
#32563=CARTESIAN_POINT('Ctrl Pts',(-22.2656934835936,20.5866303104901,-18.548313058811));
#32564=CARTESIAN_POINT('Ctrl Pts',(-22.4680098801037,20.5069104117566,-18.5604119558014));
#32565=CARTESIAN_POINT('Ctrl Pts',(-22.9408034806555,20.3737930195518,-18.5878595234725));
#32566=CARTESIAN_POINT('Ctrl Pts',(-23.2131382556604,20.3334760865714,-18.6031903870781));
#32567=CARTESIAN_POINT('Ctrl Pts',(-23.5043957681837,20.3277832947156,-18.6208446579915));
#32568=CARTESIAN_POINT('Ctrl Pts',(-23.5215195678297,20.3275851232959,-18.6218866651325));
#32569=CARTESIAN_POINT('Ctrl Pts',(-23.5443076332117,20.3275030379853,-18.6232790108695));
#32570=CARTESIAN_POINT('Ctrl Pts',(-23.5499714017471,20.3274975671743,-18.6236255309148));
#32571=CARTESIAN_POINT('Ctrl Pts',(-23.5592610076012,20.3275130825749,-18.6241946593744));
#32572=CARTESIAN_POINT('Ctrl Pts',(-23.5628868637297,20.3275252576247,-18.6244169908575));
#32573=CARTESIAN_POINT('Ctrl Pts',(-23.5699059049083,20.3275606721317,-18.6248477636452));
#32574=CARTESIAN_POINT('Ctrl Pts',(-23.5732990904062,20.3275831516987,-18.6250561808035));
#32575=CARTESIAN_POINT('Ctrl Pts',(-23.5811232230414,20.3276473436527,-18.625537152734));
#32576=CARTESIAN_POINT('Ctrl Pts',(-23.5855541248295,20.3276928356164,-18.6258098258307));
#32577=CARTESIAN_POINT('Ctrl Pts',(-23.5993438904945,20.3278628586427,-18.6266593531892));
#32578=CARTESIAN_POINT('Ctrl Pts',(-23.6087022524835,20.3280190215847,-18.627237199442));
#32579=CARTESIAN_POINT('Ctrl Pts',(-23.6881102002113,20.329690147829,-18.6321517456311));
#32580=CARTESIAN_POINT('Ctrl Pts',(-23.7580890866394,20.3334482903648,-18.6365585324857));
#32581=CARTESIAN_POINT('Ctrl Pts',(-23.836148137421,20.3401980083756,-18.641564836027));
#32582=CARTESIAN_POINT('Ctrl Pts',(-23.8444076800902,20.3409443372878,-18.6420956907095));
#32583=CARTESIAN_POINT('Ctrl Pts',(-23.8786744171778,20.3441740595482,-18.6443027704666));
#32584=CARTESIAN_POINT('Ctrl Pts',(-23.9046532727445,20.3469417196782,-18.6459872892983));
#32585=CARTESIAN_POINT('Ctrl Pts',(-24.2048989950582,20.3826254970169,-18.6655855722686));
#32586=CARTESIAN_POINT('Ctrl Pts',(-24.4738514568601,20.450358098373,-18.6845405247809));
#32587=CARTESIAN_POINT('Ctrl Pts',(-24.8105245870061,20.5829017473478,-18.708784564421));
#32588=CARTESIAN_POINT('Ctrl Pts',(-24.8889597853849,20.6174515754247,-18.7144600003672));
#32589=CARTESIAN_POINT('Ctrl Pts',(-24.9937431888341,20.6686885805699,-18.7219976110423));
#32590=CARTESIAN_POINT('Ctrl Pts',(-25.021359903857,20.6826892206582,-18.7239797914386));
#32591=CARTESIAN_POINT('Ctrl Pts',(-25.0635708684427,20.7048589552883,-18.7269977638478));
#32592=CARTESIAN_POINT('Ctrl Pts',(-25.0783097240559,20.7127468949328,-18.7280493186583));
#32593=CARTESIAN_POINT('Ctrl Pts',(-25.0963279723545,20.7225710122527,-18.7293314671674));
#32594=CARTESIAN_POINT('Ctrl Pts',(-25.0996658248035,20.724398591538,-18.7295688400058));
#32595=CARTESIAN_POINT('Ctrl Pts',(-25.1049112252408,20.7272827011938,-18.7299416340169));
#32596=CARTESIAN_POINT('Ctrl Pts',(-25.1068209377049,20.7283352552999,-18.7300773094332));
#32597=CARTESIAN_POINT('Ctrl Pts',(-25.1101975168179,20.7302007558514,-18.7303171094058));
#32598=CARTESIAN_POINT('Ctrl Pts',(-25.1116648093723,20.7310129047397,-18.7304212845952));
#32599=CARTESIAN_POINT('Ctrl Pts',(-25.114801510911,20.7327522742419,-18.7306439211502));
#32600=CARTESIAN_POINT('Ctrl Pts',(-25.1164707251204,20.7336798307436,-18.7307623600377));
#32601=CARTESIAN_POINT('Ctrl Pts',(-25.1212988698302,20.7363683752656,-18.7311048319742));
#32602=CARTESIAN_POINT('Ctrl Pts',(-25.1244556746874,20.7381332050536,-18.7313286172352));
#32603=CARTESIAN_POINT('Ctrl Pts',(-25.1385278664169,20.7460314655823,-18.7323256217192));
#32604=CARTESIAN_POINT('Ctrl Pts',(-25.149410618544,20.7522232695375,-18.7330951233033));
#32605=CARTESIAN_POINT('Ctrl Pts',(-25.1658708920401,20.7617158419241,-18.7342570966659));
#32606=CARTESIAN_POINT('Ctrl Pts',(-25.1714748417691,20.7649701798691,-18.7346523565235));
#32607=CARTESIAN_POINT('Ctrl Pts',(-25.1839891042055,20.7722880543678,-18.7355343485289));
#32608=CARTESIAN_POINT('Ctrl Pts',(-25.1908941732116,20.776360530794,-18.7360205523593));
#32609=CARTESIAN_POINT('Ctrl Pts',(-25.2044998312129,20.7844534620317,-18.7369778017514));
#32610=CARTESIAN_POINT('Ctrl Pts',(-25.211201129971,20.7884726023474,-18.7374489165066));
#32611=CARTESIAN_POINT('Ctrl Pts',(-25.3123063223608,20.8496120880592,-18.7445522958534));
#32612=CARTESIAN_POINT('Ctrl Pts',(-25.403740194443,20.9115254234033,-18.7509175933737));
#32613=CARTESIAN_POINT('Ctrl Pts',(-25.5461958201045,21.0190535360002,-18.761039318768));
#32614=CARTESIAN_POINT('Ctrl Pts',(-25.5992526125021,21.0618078255325,-18.7648589048497));
#32615=CARTESIAN_POINT('Ctrl Pts',(-25.7535175693735,21.1943992196435,-18.7762362958474));
#32616=CARTESIAN_POINT('Ctrl Pts',(-25.8504629604877,21.2889581587594,-18.7837603616064));
#32617=CARTESIAN_POINT('Ctrl Pts',(-26.0096059908036,21.4650395386185,-18.7972571773124));
#32618=CARTESIAN_POINT('Ctrl Pts',(-26.074395671517,21.5439545870268,-18.8031476437638));
#32619=CARTESIAN_POINT('Ctrl Pts',(-26.1611357459002,21.6604710416067,-18.8117369201242));
#32620=CARTESIAN_POINT('Ctrl Pts',(-26.1862414336318,21.6956508269345,-18.814316784412));
#32621=CARTESIAN_POINT('Ctrl Pts',(-26.2249120656496,21.7522107761879,-18.8184498485922));
#32622=CARTESIAN_POINT('Ctrl Pts',(-26.2389460385455,21.7732649271205,-18.8199852085452));
#32623=CARTESIAN_POINT('Ctrl Pts',(-26.2562553141048,21.7999073180454,-18.8219249601846));
#32624=CARTESIAN_POINT('Ctrl Pts',(-26.2597639182748,21.8053435167647,-18.822320591064));
#32625=CARTESIAN_POINT('Ctrl Pts',(-26.2653103972228,21.8139942458221,-18.8229499237613));
#32626=CARTESIAN_POINT('Ctrl Pts',(-26.2673590018506,21.8172019040248,-18.8231832252581));
#32627=CARTESIAN_POINT('Ctrl Pts',(-26.2712000184038,21.823239631013,-18.8236222695301));
#32628=CARTESIAN_POINT('Ctrl Pts',(-26.2729937107963,21.8260688825322,-18.8238279643233));
#32629=CARTESIAN_POINT('Ctrl Pts',(-26.2770068335159,21.8324207951588,-18.8242896812571));
#32630=CARTESIAN_POINT('Ctrl Pts',(-26.2792238521986,21.8359449661867,-18.8245457924001));
#32631=CARTESIAN_POINT('Ctrl Pts',(-26.2848275111551,21.8448909542795,-18.82519577833));
#32632=CARTESIAN_POINT('Ctrl Pts',(-26.2882048486781,21.8503185515071,-18.8255899963843));
#32633=CARTESIAN_POINT('Ctrl Pts',(-26.3065826923311,21.880049762623,-18.8277487520558));
#32634=CARTESIAN_POINT('Ctrl Pts',(-26.3212753830407,21.9045412821433,-18.8295245752832));
#32635=CARTESIAN_POINT('Ctrl Pts',(-26.5249390601308,22.2544934097971,-18.8548715028241));
#32636=CARTESIAN_POINT('Ctrl Pts',(-26.65576628624,22.610370572396,-18.8808216122646));
#32637=CARTESIAN_POINT('Ctrl Pts',(-26.7326788134364,23.0386288612668,-18.9098075378692));
#32638=CARTESIAN_POINT('Ctrl Pts',(-26.7415090870816,23.096955504035,-18.9136977982153));
#32639=CARTESIAN_POINT('Ctrl Pts',(-26.7551800657609,23.2077230855739,-18.9209397360323));
#32640=CARTESIAN_POINT('Ctrl Pts',(-26.7603463622836,23.2601054541113,-18.9243032076897));
#32641=CARTESIAN_POINT('Ctrl Pts',(-26.7646018312375,23.3176544112297,-18.927914464213));
#32642=CARTESIAN_POINT('Ctrl Pts',(-26.764964040301,23.3227152327999,-18.9282313250719));
#32643=CARTESIAN_POINT('Ctrl Pts',(-26.7654819660451,23.3301999333398,-18.9286988741158));
#32644=CARTESIAN_POINT('Ctrl Pts',(-26.7656468943645,23.332623135334,-18.9288500788735));
#32645=CARTESIAN_POINT('Ctrl Pts',(-26.765922868151,23.3367466695968,-18.9291070968865));
#32646=CARTESIAN_POINT('Ctrl Pts',(-26.7660353045173,23.3384469038467,-18.9292129891401));
#32647=CARTESIAN_POINT('Ctrl Pts',(-26.7662626964322,23.3419273885443,-18.9294295873037));
#32648=CARTESIAN_POINT('Ctrl Pts',(-26.7663775220232,23.343707641689,-18.9295402855908));
#32649=CARTESIAN_POINT('Ctrl Pts',(-26.7666492496946,23.3479756705539,-18.9298054611776));
#32650=CARTESIAN_POINT('Ctrl Pts',(-26.7668047440432,23.3504635393855,-18.9299598586127));
#32651=CARTESIAN_POINT('Ctrl Pts',(-26.7672696396885,23.3580429867806,-18.9304297119781));
#32652=CARTESIAN_POINT('Ctrl Pts',(-26.7675698411566,23.3631351531289,-18.9307446518818));
#32653=CARTESIAN_POINT('Ctrl Pts',(-26.7706837640678,23.4181792618025,-18.934141378813));
#32654=CARTESIAN_POINT('Ctrl Pts',(-26.7723461947943,23.4681929285441,-18.9371597307708));
#32655=CARTESIAN_POINT('Ctrl Pts',(-26.7729447253812,23.5284229979129,-18.9407345898242));
#32656=CARTESIAN_POINT('Ctrl Pts',(-26.7729976582524,23.5386181950847,-18.9413376384116));
#32657=CARTESIAN_POINT('Ctrl Pts',(-26.7730372952479,23.6273916831091,-18.9465718943153));
#32658=CARTESIAN_POINT('Ctrl Pts',(-26.7701984882302,23.7059499859438,-18.9510901250681));
#32659=CARTESIAN_POINT('Ctrl Pts',(-26.738507148839,24.1411189798893,-18.9758586346407));
#32660=CARTESIAN_POINT('Ctrl Pts',(-26.6533123248868,24.491058250259,-18.9951350607033));
#32661=CARTESIAN_POINT('Ctrl Pts',(-26.5043364157131,24.8386324304217,-19.018003598287));
#32662=CARTESIAN_POINT('Ctrl Pts',(-26.4961156515518,24.8573197857052,-19.0192441377773));
#32663=CARTESIAN_POINT('Ctrl Pts',(-26.4851442788581,24.8816304432354,-19.0208728439227));
#32664=CARTESIAN_POINT('Ctrl Pts',(-26.4825539338123,24.887325901848,-19.0212554876822));
#32665=CARTESIAN_POINT('Ctrl Pts',(-26.4785377007967,24.8960886927518,-19.0218458757334));
#32666=CARTESIAN_POINT('Ctrl Pts',(-26.4771235320184,24.8991614060509,-19.0220532150047));
#32667=CARTESIAN_POINT('Ctrl Pts',(-26.4743021609076,24.9052663704381,-19.0224657964235));
#32668=CARTESIAN_POINT('Ctrl Pts',(-26.4728950728785,24.9082986699445,-19.0226710344182));
#32669=CARTESIAN_POINT('Ctrl Pts',(-26.4697718026634,24.9150020365453,-19.0231254363995));
#32670=CARTESIAN_POINT('Ctrl Pts',(-26.4680534110744,24.9186720626133,-19.0233746767447));
#32671=CARTESIAN_POINT('Ctrl Pts',(-26.4630945008023,24.9292111644222,-19.0240917412002));
#32672=CARTESIAN_POINT('Ctrl Pts',(-26.4598366318303,24.9360720042177,-19.0245601675125));
#32673=CARTESIAN_POINT('Ctrl Pts',(-26.4381922633688,24.9812407314923,-19.0276548966073));
#32674=CARTESIAN_POINT('Ctrl Pts',(-26.419074652922,25.0191917678929,-19.0303066236142));
#32675=CARTESIAN_POINT('Ctrl Pts',(-26.3606375898138,25.1297028239749,-19.0381859472661));
#32676=CARTESIAN_POINT('Ctrl Pts',(-26.3192775248967,25.201138970678,-19.0434844162707));
#32677=CARTESIAN_POINT('Ctrl Pts',(-26.1157899912737,25.523399291582,-19.0683554509675));
#32678=CARTESIAN_POINT('Ctrl Pts',(-25.9220696746796,25.7524630989853,-19.0890227882896));
#32679=CARTESIAN_POINT('Ctrl Pts',(-25.6330270212063,26.0111781413648,-19.1146742047232));
#32680=CARTESIAN_POINT('Ctrl Pts',(-25.5639785225902,26.0679926942967,-19.1204752568961));
#32681=CARTESIAN_POINT('Ctrl Pts',(-25.4875407475089,26.125727814493,-19.1264803784946));
#32682=CARTESIAN_POINT('Ctrl Pts',(-25.4824197283844,26.12957191656,-19.1268807615697));
#32683=CARTESIAN_POINT('Ctrl Pts',(-25.4753025829964,26.1348813238737,-19.1274344923704));
#32684=CARTESIAN_POINT('Ctrl Pts',(-25.4733162179885,26.1363595967515,-19.1275887438654));
#32685=CARTESIAN_POINT('Ctrl Pts',(-25.469899363085,26.1388963410757,-19.1278535752755));
#32686=CARTESIAN_POINT('Ctrl Pts',(-25.4684697005586,26.1399559166839,-19.1279642330125));
#32687=CARTESIAN_POINT('Ctrl Pts',(-25.4655149393362,26.1421420099164,-19.1281926210819));
#32688=CARTESIAN_POINT('Ctrl Pts',(-25.4639897269814,26.1432683636616,-19.1283103394235));
#32689=CARTESIAN_POINT('Ctrl Pts',(-25.4604069392783,26.1459093328407,-19.1285864612054));
#32690=CARTESIAN_POINT('Ctrl Pts',(-25.458348549777,26.1474228526466,-19.1287447873349));
#32691=CARTESIAN_POINT('Ctrl Pts',(-25.4516596136515,26.1523289376635,-19.1292582796233));
#32692=CARTESIAN_POINT('Ctrl Pts',(-25.4470217685376,26.1557116039476,-19.1296127556672));
#32693=CARTESIAN_POINT('Ctrl Pts',(-25.3166527291841,26.2502651899831,-19.1395341189983));
#32694=CARTESIAN_POINT('Ctrl Pts',(-25.1844832161355,26.3322559317665,-19.1484790605671));
#32695=CARTESIAN_POINT('Ctrl Pts',(-24.7447150827609,26.5628591746677,-19.1765241230685));
#32696=CARTESIAN_POINT('Ctrl Pts',(-24.4193256523109,26.6723102604059,-19.1950478732565));
#32697=CARTESIAN_POINT('Ctrl Pts',(-24.0628041742597,26.7320476646317,-19.2169102087032));
#32698=CARTESIAN_POINT('Ctrl Pts',(-24.0427572216129,26.7352122732593,-19.2181434826066));
#32699=CARTESIAN_POINT('Ctrl Pts',(-24.0165071496756,26.7391023495238,-19.2197639699858));
#32700=CARTESIAN_POINT('Ctrl Pts',(-24.0103296223558,26.7399994807864,-19.2201457297175));
#32701=CARTESIAN_POINT('Ctrl Pts',(-24.000803646443,26.7413546418142,-19.2207350532318));
#32702=CARTESIAN_POINT('Ctrl Pts',(-23.9974569947268,26.741825365317,-19.2209422143555));
#32703=CARTESIAN_POINT('Ctrl Pts',(-23.9907984052143,26.7427512508724,-19.2213546306447));
#32704=CARTESIAN_POINT('Ctrl Pts',(-23.9874864871222,26.7432065255245,-19.2215598819665));
#32705=CARTESIAN_POINT('Ctrl Pts',(-23.9802345575883,26.7441919213293,-19.2220095737955));
#32706=CARTESIAN_POINT('Ctrl Pts',(-23.9762942657422,26.7447199063715,-19.2222540816298));
#32707=CARTESIAN_POINT('Ctrl Pts',(-23.9650721674279,26.7462024950677,-19.2229509398948));
#32708=CARTESIAN_POINT('Ctrl Pts',(-23.9577880958527,26.7471394957723,-19.2234038468337));
#32709=CARTESIAN_POINT('Ctrl Pts',(-23.9414485928975,26.7491846086234,-19.2244211434862));
#32710=CARTESIAN_POINT('Ctrl Pts',(-23.9323915583628,26.7502791804348,-19.2249859584167));
#32711=CARTESIAN_POINT('Ctrl Pts',(-23.7357485100187,26.7731973961969,-19.2372694933105));
#32712=CARTESIAN_POINT('Ctrl Pts',(-23.5466435914315,26.7785255136717,-19.2495201031416));
#32713=CARTESIAN_POINT('Ctrl Pts',(-23.0793767528534,26.7506285470333,-19.2807733954771));
#32714=CARTESIAN_POINT('Ctrl Pts',(-22.8039219727572,26.6978104959097,-19.3001285623604));
#32715=CARTESIAN_POINT('Ctrl Pts',(-22.5027167431305,26.598239557912,-19.3205357950218));
#32716=CARTESIAN_POINT('Ctrl Pts',(-22.4669157934068,26.5856994455135,-19.3229464002846));
#32717=CARTESIAN_POINT('Ctrl Pts',(-22.4264223849635,26.570707942943,-19.3256491606233));
#32718=CARTESIAN_POINT('Ctrl Pts',(-22.4215065015531,26.5688743182733,-19.3259768716167));
#32719=CARTESIAN_POINT('Ctrl Pts',(-22.4143148143236,26.5661717943083,-19.3264556822973));
#32720=CARTESIAN_POINT('Ctrl Pts',(-22.4120355151096,26.5653123187637,-19.3266073438389));
#32721=CARTESIAN_POINT('Ctrl Pts',(-22.4079950191913,26.5637834984208,-19.3268760297899));
#32722=CARTESIAN_POINT('Ctrl Pts',(-22.4062334341881,26.5631151931682,-19.3269931169525));
#32723=CARTESIAN_POINT('Ctrl Pts',(-22.4025487295212,26.561713602506,-19.3272379114874));
#32724=CARTESIAN_POINT('Ctrl Pts',(-22.4006257302273,26.5609800211797,-19.3273656003782));
#32725=CARTESIAN_POINT('Ctrl Pts',(-22.3955894630251,26.5590532689303,-19.3276998429006));
#32726=CARTESIAN_POINT('Ctrl Pts',(-22.3924773313694,26.557857104156,-19.3279062155926));
#32727=CARTESIAN_POINT('Ctrl Pts',(-22.3788173781799,26.5525824824962,-19.3288113130218));
#32728=CARTESIAN_POINT('Ctrl Pts',(-22.3682890413697,26.5484532869622,-19.3295070095386));
#32729=CARTESIAN_POINT('Ctrl Pts',(-22.2912232514053,26.5177591816892,-19.3345869440783));
#32730=CARTESIAN_POINT('Ctrl Pts',(-22.2255606086061,26.4890351958121,-19.3388470206358));
#32731=CARTESIAN_POINT('Ctrl Pts',(-22.1320704356073,26.4443669586381,-19.3448884612601));
#32732=CARTESIAN_POINT('Ctrl Pts',(-22.103444381051,26.4301630688019,-19.3467349361993));
#32733=CARTESIAN_POINT('Ctrl Pts',(-22.0750360113656,26.4155367725069,-19.3485684984428));
#32734=CARTESIAN_POINT('',(-26.7730018214075,23.5481128698841,-19.1857734492732));
#32735=CARTESIAN_POINT('Ctrl Pts',(-22.075036015346,26.4155367745563,-19.592915740792));
#32736=CARTESIAN_POINT('Ctrl Pts',(-22.1638817756157,26.4612797870632,-19.5867644769599));
#32737=CARTESIAN_POINT('Ctrl Pts',(-22.2548303270937,26.5028728174781,-19.5806132131277));
#32738=CARTESIAN_POINT('Ctrl Pts',(-22.3474545181231,26.5401345529535,-19.5744619492956));
#32739=CARTESIAN_POINT('Ctrl Pts',(-22.4401819008943,26.5774378013786,-19.5683038323982));
#32740=CARTESIAN_POINT('Ctrl Pts',(-22.5345882459535,26.6103999605182,-19.5621457155008));
#32741=CARTESIAN_POINT('Ctrl Pts',(-22.6302284943965,26.6388886924121,-19.5559875986034));
#32742=CARTESIAN_POINT('Ctrl Pts',(-22.7259291705768,26.6673954241507,-19.5498255908643));
#32743=CARTESIAN_POINT('Ctrl Pts',(-22.8228648810819,26.6914229971941,-19.5436635831252));
#32744=CARTESIAN_POINT('Ctrl Pts',(-22.9205795626509,26.7108900488031,-19.537501575386));
#32745=CARTESIAN_POINT('Ctrl Pts',(-23.0184488317674,26.7303878978696,-19.5313298191664));
#32746=CARTESIAN_POINT('Ctrl Pts',(-23.1170991033048,26.7453107579507,-19.5251580629468));
#32747=CARTESIAN_POINT('Ctrl Pts',(-23.2160684532901,26.7556290406618,-19.5189863067272));
#32748=CARTESIAN_POINT('Ctrl Pts',(-23.2611536717233,26.7603295063105,-19.5161747799533));
#32749=CARTESIAN_POINT('Ctrl Pts',(-23.3063050959804,26.7640751313075,-19.5133632531795));
#32750=CARTESIAN_POINT('Ctrl Pts',(-23.3514791794028,26.7668667014259,-19.5105517264056));
#32751=CARTESIAN_POINT('Ctrl Pts',(-23.4506489865071,26.7729949822716,-19.5043796350932));
#32752=CARTESIAN_POINT('Ctrl Pts',(-23.550277124991,26.7745435777351,-19.4982075437809));
#32753=CARTESIAN_POINT('Ctrl Pts',(-23.6499048733714,26.7714614620957,-19.4920354524686));
#32754=CARTESIAN_POINT('Ctrl Pts',(-23.749397636002,26.7683835224183,-19.4858717237298));
#32755=CARTESIAN_POINT('Ctrl Pts',(-23.8488895792128,26.7606873555042,-19.479707994991));
#32756=CARTESIAN_POINT('Ctrl Pts',(-23.9479181499618,26.7483737955846,-19.4735442662523));
#32757=CARTESIAN_POINT('Ctrl Pts',(-24.0468418092345,26.736073280726,-19.4673870674056));
#32758=CARTESIAN_POINT('Ctrl Pts',(-24.1453026432962,26.7191651513008,-19.4612298685589));
#32759=CARTESIAN_POINT('Ctrl Pts',(-24.2428403636803,26.6977022385974,-19.4550726697122));
#32760=CARTESIAN_POINT('Ctrl Pts',(-24.3403067899057,26.6762550139816,-19.4489199714045));
#32761=CARTESIAN_POINT('Ctrl Pts',(-24.4368510209793,26.650259718311,-19.4427672730968));
#32762=CARTESIAN_POINT('Ctrl Pts',(-24.5320210574339,26.6198205997401,-19.4366145747891));
#32763=CARTESIAN_POINT('Ctrl Pts',(-24.6271550052752,26.5893930237263,-19.4304642095933));
#32764=CARTESIAN_POINT('Ctrl Pts',(-24.7209153806172,26.554525105284,-19.4243138443976));
#32765=CARTESIAN_POINT('Ctrl Pts',(-24.8128643577964,26.5153712374271,-19.4181634792018));
#32766=CARTESIAN_POINT('Ctrl Pts',(-24.9048030668498,26.4762217419607,-19.4120138008296));
#32767=CARTESIAN_POINT('Ctrl Pts',(-24.99493038023,26.4327874188326,-19.4058641224574));
#32768=CARTESIAN_POINT('Ctrl Pts',(-25.0828284499124,26.3852708063086,-19.3997144440852));
#32769=CARTESIAN_POINT('Ctrl Pts',(-25.1707402189784,26.3377467880668,-19.3935638072528));
#32770=CARTESIAN_POINT('Ctrl Pts',(-25.2564216720679,26.2861394232798,-19.3874131704204));
#32771=CARTESIAN_POINT('Ctrl Pts',(-25.3394804587469,26.2306967089817,-19.3812625335879));
#32772=CARTESIAN_POINT('Ctrl Pts',(-25.4226281008802,26.1751946826258,-19.3751053168661));
#32773=CARTESIAN_POINT('Ctrl Pts',(-25.5031471118834,26.1158493550813,-19.3689481001443));
#32774=CARTESIAN_POINT('Ctrl Pts',(-25.5806751023678,26.0529514242898,-19.3627908834225));
#32775=CARTESIAN_POINT('Ctrl Pts',(-25.6582463454004,25.9900184030004,-19.3566302316147));
#32776=CARTESIAN_POINT('Ctrl Pts',(-25.7328229205091,25.9235291204702,-19.3504695798069));
#32777=CARTESIAN_POINT('Ctrl Pts',(-25.8040780239711,25.8538124316888,-19.3443089279991));
#32778=CARTESIAN_POINT('Ctrl Pts',(-25.8754523625599,25.7839790820953,-19.3381379672301));
#32779=CARTESIAN_POINT('Ctrl Pts',(-25.9434938313503,25.7109078567522,-19.331967006461));
#32780=CARTESIAN_POINT('Ctrl Pts',(-26.0079146747089,25.6349621885271,-19.325796045692));
#32781=CARTESIAN_POINT('Ctrl Pts',(-26.0570883140048,25.5769914340214,-19.3210856354715));
#32782=CARTESIAN_POINT('Ctrl Pts',(-26.1041531826861,25.5173465854334,-19.3163752252511));
#32783=CARTESIAN_POINT('Ctrl Pts',(-26.1489985783231,25.4562002087385,-19.3116648150306));
#32784=CARTESIAN_POINT('Ctrl Pts',(-26.2081317902181,25.37557249661,-19.3054536604244));
#32785=CARTESIAN_POINT('Ctrl Pts',(-26.2636129571008,25.292048867266,-19.2992425058183));
#32786=CARTESIAN_POINT('Ctrl Pts',(-26.3151478242801,25.2059915158147,-19.2930313512121));
#32787=CARTESIAN_POINT('Ctrl Pts',(-26.3666114707859,25.1200530947665,-19.2868287803597));
#32788=CARTESIAN_POINT('Ctrl Pts',(-26.414139439793,25.0315882738076,-19.2806262095074));
#32789=CARTESIAN_POINT('Ctrl Pts',(-26.4574788902681,24.9409906315941,-19.274423638655));
#32790=CARTESIAN_POINT('Ctrl Pts',(-26.5007695487846,24.8504949850534,-19.2682280507149));
#32791=CARTESIAN_POINT('Ctrl Pts',(-26.5398808802617,24.7578716736682,-19.2620324627749));
#32792=CARTESIAN_POINT('Ctrl Pts',(-26.5746048697898,24.6635406783821,-19.2558368748348));
#32793=CARTESIAN_POINT('Ctrl Pts',(-26.6092963985878,24.5692978657333,-19.2496470786631));
#32794=CARTESIAN_POINT('Ctrl Pts',(-26.6396085982497,24.4733509444553,-19.2434572824915));
#32795=CARTESIAN_POINT('Ctrl Pts',(-26.6653811061292,24.3761408578247,-19.2372674863199));
#32796=CARTESIAN_POINT('Ctrl Pts',(-26.691139177631,24.278985223075,-19.2310811573404));
#32797=CARTESIAN_POINT('Ctrl Pts',(-26.7123625051649,24.1805682420417,-19.2248948283609));
#32798=CARTESIAN_POINT('Ctrl Pts',(-26.7289404592313,24.0813463292759,-19.2187084993813));
#32799=CARTESIAN_POINT('Ctrl Pts',(-26.745516241683,23.9821374139982,-19.2125229807746));
#32800=CARTESIAN_POINT('Ctrl Pts',(-26.7574477822821,23.8821241963588,-19.2063374621679));
#32801=CARTESIAN_POINT('Ctrl Pts',(-26.7646756306367,23.7817729486884,-19.2001519435611));
#32802=CARTESIAN_POINT('Ctrl Pts',(-26.7702761082946,23.7040160709902,-19.1953591121318));
#32803=CARTESIAN_POINT('Ctrl Pts',(-26.773053570087,23.6260565053534,-19.1905662807025));
#32804=CARTESIAN_POINT('Ctrl Pts',(-26.7730018214075,23.5481128698841,-19.1857734492732));
#32805=CARTESIAN_POINT('Ctrl Pts',(-26.7730017222135,23.5479683454044,-19.1879840164276));
#32806=CARTESIAN_POINT('Ctrl Pts',(-26.7727851743233,23.2424418036611,-19.1680091024078));
#32807=CARTESIAN_POINT('Ctrl Pts',(-26.7291278268916,22.9385397708267,-19.1468119365999));
#32808=CARTESIAN_POINT('Ctrl Pts',(-26.6283095396878,22.5939304488475,-19.1231910839668));
#32809=CARTESIAN_POINT('Ctrl Pts',(-26.6119884302315,22.5428991258433,-19.1197103222852));
#32810=CARTESIAN_POINT('Ctrl Pts',(-26.5855073949,22.4667030152096,-19.1145627778049));
#32811=CARTESIAN_POINT('Ctrl Pts',(-26.576290339709,22.4412228014047,-19.1128499526712));
#32812=CARTESIAN_POINT('Ctrl Pts',(-26.5652069471654,22.4117505691125,-19.1108812278628));
#32813=CARTESIAN_POINT('Ctrl Pts',(-26.5636528152118,22.4076434217999,-19.1106071561069));
#32814=CARTESIAN_POINT('Ctrl Pts',(-26.5612754264844,22.4013992190108,-19.1101909225071));
#32815=CARTESIAN_POINT('Ctrl Pts',(-26.5604582865436,22.3992598642265,-19.1100483943854));
#32816=CARTESIAN_POINT('Ctrl Pts',(-26.5589716268404,22.3953800511084,-19.1097900602408));
#32817=CARTESIAN_POINT('Ctrl Pts',(-26.5583028790647,22.3936393086812,-19.1096742081957));
#32818=CARTESIAN_POINT('Ctrl Pts',(-26.5569534186101,22.3901357660666,-19.1094411446805));
#32819=CARTESIAN_POINT('Ctrl Pts',(-26.5562726691571,22.3883729912583,-19.1093239361097));
#32820=CARTESIAN_POINT('Ctrl Pts',(-26.5543204380999,22.383330963498,-19.1089888420098));
#32821=CARTESIAN_POINT('Ctrl Pts',(-26.5530451331687,22.3800531788366,-19.1087711876993));
#32822=CARTESIAN_POINT('Ctrl Pts',(-26.5475218182632,22.3659256561478,-19.1078338633722));
#32823=CARTESIAN_POINT('Ctrl Pts',(-26.5432202822737,22.3550967350997,-19.1071173882909));
#32824=CARTESIAN_POINT('Ctrl Pts',(-26.4684372615227,22.1697698191272,-19.0948859760059));
#32825=CARTESIAN_POINT('Ctrl Pts',(-26.382850748013,22.0017226862924,-19.0842479495856));
#32826=CARTESIAN_POINT('Ctrl Pts',(-26.1946319991938,21.7005999602954,-19.0643573407785));
#32827=CARTESIAN_POINT('Ctrl Pts',(-26.0953436979259,21.5661995676183,-19.0551114814917));
#32828=CARTESIAN_POINT('Ctrl Pts',(-25.9360271155736,21.38229382275,-19.0411969509695));
#32829=CARTESIAN_POINT('Ctrl Pts',(-25.8839178786734,21.3262987954141,-19.0367690107676));
#32830=CARTESIAN_POINT('Ctrl Pts',(-25.7786063710529,21.2209144114224,-19.027989646342));
#32831=CARTESIAN_POINT('Ctrl Pts',(-25.7256302583036,21.1713646818381,-19.023648701961));
#32832=CARTESIAN_POINT('Ctrl Pts',(-25.6645590027993,21.1179902947171,-19.0187056806998));
#32833=CARTESIAN_POINT('Ctrl Pts',(-25.6580644561203,21.1123599310708,-19.0181807777443));
#32834=CARTESIAN_POINT('Ctrl Pts',(-25.6489488222144,21.1045209049677,-19.0174450562022));
#32835=CARTESIAN_POINT('Ctrl Pts',(-25.6463465769597,21.1022903050509,-19.0172351452867));
#32836=CARTESIAN_POINT('Ctrl Pts',(-25.6413477613603,21.0980192209926,-19.0168321338162));
#32837=CARTESIAN_POINT('Ctrl Pts',(-25.6389517491361,21.095978087262,-19.0166390603576));
#32838=CARTESIAN_POINT('Ctrl Pts',(-25.6339417453161,21.0917227761092,-19.0162355473379));
#32839=CARTESIAN_POINT('Ctrl Pts',(-25.6313272070536,21.0895092509987,-19.0160250813059));
#32840=CARTESIAN_POINT('Ctrl Pts',(-25.6255612101237,21.0846433943147,-19.0155611731351));
#32841=CARTESIAN_POINT('Ctrl Pts',(-25.6224081890818,21.0819929301925,-19.0153076548332));
#32842=CARTESIAN_POINT('Ctrl Pts',(-25.6114011369336,21.0727762369637,-19.0144231858524));
#32843=CARTESIAN_POINT('Ctrl Pts',(-25.603520969599,21.0662414443892,-19.0137909530803));
#32844=CARTESIAN_POINT('Ctrl Pts',(-25.523549154059,21.0005637074516,-19.0073842716041));
#32845=CARTESIAN_POINT('Ctrl Pts',(-25.4489607177624,20.944543995985,-19.0014847619186));
#32846=CARTESIAN_POINT('Ctrl Pts',(-25.2887092551718,20.8347241236295,-18.9889437212693));
#32847=CARTESIAN_POINT('Ctrl Pts',(-25.2027307802655,20.7815635108702,-18.9822879953149));
#32848=CARTESIAN_POINT('Ctrl Pts',(-25.0542620623923,20.6991466872039,-18.9709478547943));
#32849=CARTESIAN_POINT('Ctrl Pts',(-24.9930684421427,20.667696213721,-18.9663156439852));
#32850=CARTESIAN_POINT('Ctrl Pts',(-24.8100347282932,20.5809152700826,-18.952625691578));
#32851=CARTESIAN_POINT('Ctrl Pts',(-24.6856986754023,20.5311833786956,-18.9435300632271));
#32852=CARTESIAN_POINT('Ctrl Pts',(-24.5083866875914,20.4727706395849,-18.9310850111468));
#32853=CARTESIAN_POINT('Ctrl Pts',(-24.457741506682,20.4574576538197,-18.9275889483037));
#32854=CARTESIAN_POINT('Ctrl Pts',(-24.3666222173832,20.4323381887796,-18.9214282686706));
#32855=CARTESIAN_POINT('Ctrl Pts',(-24.3262917772876,20.4220561227769,-18.9187459978098));
#32856=CARTESIAN_POINT('Ctrl Pts',(-24.2655166518835,20.4078095966196,-18.9147817170289));
#32857=CARTESIAN_POINT('Ctrl Pts',(-24.2452157306226,20.4032576844156,-18.9134704075289));
#32858=CARTESIAN_POINT('Ctrl Pts',(-24.2208811617263,20.3980483099226,-18.9119151055985));
#32859=CARTESIAN_POINT('Ctrl Pts',(-24.2168891572155,20.3972016559351,-18.9116604949295));
#32860=CARTESIAN_POINT('Ctrl Pts',(-24.2107192964807,20.3959053472258,-18.9112678124196));
#32861=CARTESIAN_POINT('Ctrl Pts',(-24.2085425832429,20.3954503642587,-18.9111294347809));
#32862=CARTESIAN_POINT('Ctrl Pts',(-24.204721417179,20.3946557798971,-18.9108867989433));
#32863=CARTESIAN_POINT('Ctrl Pts',(-24.2030771764796,20.3943152120986,-18.9107824851344));
#32864=CARTESIAN_POINT('Ctrl Pts',(-24.1995920177915,20.3935961794033,-18.9105615747626));
#32865=CARTESIAN_POINT('Ctrl Pts',(-24.1977510402101,20.393218040882,-18.9104449974503));
#32866=CARTESIAN_POINT('Ctrl Pts',(-24.1925136743651,20.3921470548996,-18.9101136728131));
#32867=CARTESIAN_POINT('Ctrl Pts',(-24.1891164843744,20.3914580736486,-18.9098991484444));
#32868=CARTESIAN_POINT('Ctrl Pts',(-24.1747105180798,20.3885606023934,-18.908991063629));
#32869=CARTESIAN_POINT('Ctrl Pts',(-24.1636911791029,20.3864041365891,-18.9083004574845));
#32870=CARTESIAN_POINT('Ctrl Pts',(-23.9701402187951,20.3495757717686,-18.8962367605639));
#32871=CARTESIAN_POINT('Ctrl Pts',(-23.7849272988383,20.3306893285851,-18.8857207502765));
#32872=CARTESIAN_POINT('Ctrl Pts',(-23.4313002381038,20.3253294054016,-18.8659029823924));
#32873=CARTESIAN_POINT('Ctrl Pts',(-23.2635699743342,20.3358956868316,-18.8566088604368));
#32874=CARTESIAN_POINT('Ctrl Pts',(-22.9940877148605,20.3741397411742,-18.8410536659842));
#32875=CARTESIAN_POINT('Ctrl Pts',(-22.8915298939915,20.3938157409492,-18.834987326594));
#32876=CARTESIAN_POINT('Ctrl Pts',(-22.7595035902304,20.4258604553327,-18.8268872276437));
#32877=CARTESIAN_POINT('Ctrl Pts',(-22.7290049573259,20.4337381242611,-18.8249957437281));
#32878=CARTESIAN_POINT('Ctrl Pts',(-22.6795406433711,20.4472910387426,-18.8218924719085));
#32879=CARTESIAN_POINT('Ctrl Pts',(-22.6605027274858,20.4526963210785,-18.8206894285754));
#32880=CARTESIAN_POINT('Ctrl Pts',(-22.6358385380682,20.4599451634573,-18.8191192012695));
#32881=CARTESIAN_POINT('Ctrl Pts',(-22.6301655858851,20.4616294414917,-18.8187572332951));
#32882=CARTESIAN_POINT('Ctrl Pts',(-22.6209990340417,20.4643784515717,-18.8181710408125));
#32883=CARTESIAN_POINT('Ctrl Pts',(-22.6175025309151,20.465433519638,-18.8179471333759));
#32884=CARTESIAN_POINT('Ctrl Pts',(-22.6107896615104,20.4674715810982,-18.8175166602941));
#32885=CARTESIAN_POINT('Ctrl Pts',(-22.6075730240163,20.4684536707237,-18.8173101245567));
#32886=CARTESIAN_POINT('Ctrl Pts',(-22.6002545045834,20.4707006590298,-18.8168396090541));
#32887=CARTESIAN_POINT('Ctrl Pts',(-22.5961536068795,20.471968719352,-18.816575525666));
#32888=CARTESIAN_POINT('Ctrl Pts',(-22.5836973058663,20.4758476807298,-18.8157720618658));
#32889=CARTESIAN_POINT('Ctrl Pts',(-22.5753500472922,20.4784844194027,-18.815231831985));
#32890=CARTESIAN_POINT('Ctrl Pts',(-22.5161985416387,20.497434634842,-18.8113905867852));
#32891=CARTESIAN_POINT('Ctrl Pts',(-22.4657981816182,20.5149728120127,-18.8080492954933));
#32892=CARTESIAN_POINT('Ctrl Pts',(-22.4054743031966,20.5376583909354,-18.8039635722731));
#32893=CARTESIAN_POINT('Ctrl Pts',(-22.3951102168828,20.5416171471634,-18.8032584970778));
#32894=CARTESIAN_POINT('Ctrl Pts',(-22.1933274174503,20.619888178015,-18.7894699363532));
#32895=CARTESIAN_POINT('Ctrl Pts',(-22.0094531657702,20.7122614412642,-18.7757827427425));
#32896=CARTESIAN_POINT('Ctrl Pts',(-21.7020842150694,20.9053950298511,-18.7512401506563));
#32897=CARTESIAN_POINT('Ctrl Pts',(-21.574864167231,20.999009284987,-18.7405085025313));
#32898=CARTESIAN_POINT('Ctrl Pts',(-21.4101263058538,21.1399690771474,-18.7262078865154));
#32899=CARTESIAN_POINT('Ctrl Pts',(-21.3663067844025,21.1796010350458,-18.72236179553));
#32900=CARTESIAN_POINT('Ctrl Pts',(-21.3037535050426,21.2393840287388,-18.7168388324749));
#32901=CARTESIAN_POINT('Ctrl Pts',(-21.2841506326168,21.2586039065244,-18.7151031527016));
#32902=CARTESIAN_POINT('Ctrl Pts',(-21.261688341662,21.281197458358,-18.7131111243461));
#32903=CARTESIAN_POINT('Ctrl Pts',(-21.2585881168428,21.284328616823,-18.7128361152916));
#32904=CARTESIAN_POINT('Ctrl Pts',(-21.2538841534632,21.2890990444458,-18.7124187506081));
#32905=CARTESIAN_POINT('Ctrl Pts',(-21.252275742674,21.2907336672813,-18.7122760256658));
#32906=CARTESIAN_POINT('Ctrl Pts',(-21.2493624761166,21.2937007390973,-18.7120174841272));
#32907=CARTESIAN_POINT('Ctrl Pts',(-21.2480570363215,21.295032599699,-18.7119016211253));
#32908=CARTESIAN_POINT('Ctrl Pts',(-21.2452338089533,21.2979179723267,-18.7116510267126));
#32909=CARTESIAN_POINT('Ctrl Pts',(-21.2437164396839,21.2994718813803,-18.7115163285433));
#32910=CARTESIAN_POINT('Ctrl Pts',(-21.2395884277564,21.303707858168,-18.7111498394251));
#32911=CARTESIAN_POINT('Ctrl Pts',(-21.2369808744193,21.3063929524509,-18.7109182923639));
#32912=CARTESIAN_POINT('Ctrl Pts',(-21.2245467215858,21.3192415711978,-18.7098139017879));
#32913=CARTESIAN_POINT('Ctrl Pts',(-21.2147821935364,21.329465342895,-18.708945861074));
#32914=CARTESIAN_POINT('Ctrl Pts',(-21.0367734704654,21.5183187274303,-18.6930997606971));
#32915=CARTESIAN_POINT('Ctrl Pts',(-20.8893759641594,21.7155562691804,-18.6795839602382));
#32916=CARTESIAN_POINT('Ctrl Pts',(-20.6901999939081,22.0573514762352,-18.6574639116931));
#32917=CARTESIAN_POINT('Ctrl Pts',(-20.6237753719986,22.1921727410893,-18.6490265385683));
#32918=CARTESIAN_POINT('Ctrl Pts',(-20.540084517025,22.3969678528042,-18.6361706441773));
#32919=CARTESIAN_POINT('Ctrl Pts',(-20.5153657563358,22.4636807664651,-18.6319789214494));
#32920=CARTESIAN_POINT('Ctrl Pts',(-20.485255674619,22.554013371,-18.6262700132007));
#32921=CARTESIAN_POINT('Ctrl Pts',(-20.4778926881231,22.5769575389117,-18.6248172296217));
#32922=CARTESIAN_POINT('Ctrl Pts',(-20.4676181586077,22.6102533619206,-18.622704168575));
#32923=CARTESIAN_POINT('Ctrl Pts',(-20.4644999259151,22.6205407651366,-18.6220506356219));
#32924=CARTESIAN_POINT('Ctrl Pts',(-20.4590382420843,22.6388896755676,-18.6208837158024));
#32925=CARTESIAN_POINT('Ctrl Pts',(-20.4566747018435,22.6469451375194,-18.6203709889245));
#32926=CARTESIAN_POINT('Ctrl Pts',(-20.4531757978372,22.6590449732178,-18.6196001628558));
#32927=CARTESIAN_POINT('Ctrl Pts',(-20.4520168098509,22.6630825258254,-18.6193428358228));
#32928=CARTESIAN_POINT('Ctrl Pts',(-20.4499747700928,22.6702491599057,-18.618885877511));
#32929=CARTESIAN_POINT('Ctrl Pts',(-20.4490885517624,22.6733773393849,-18.6186863498723));
#32930=CARTESIAN_POINT('Ctrl Pts',(-20.4473289251669,22.6796245137946,-18.6182877407046));
#32931=CARTESIAN_POINT('Ctrl Pts',(-20.4464554821057,22.6827434952383,-18.6180886605641));
#32932=CARTESIAN_POINT('Ctrl Pts',(-20.444352847166,22.6902956281589,-18.6176064481669));
#32933=CARTESIAN_POINT('Ctrl Pts',(-20.4431284452773,22.6947300962448,-18.6173231601931));
#32934=CARTESIAN_POINT('Ctrl Pts',(-20.4386189040151,22.7111998691456,-18.616270480797));
#32935=CARTESIAN_POINT('Ctrl Pts',(-20.435394196112,22.7232514762808,-18.6154991268424));
#32936=CARTESIAN_POINT('Ctrl Pts',(-20.3810804200021,22.9310617368419,-18.602179176972));
#32937=CARTESIAN_POINT('Ctrl Pts',(-20.3484763792263,23.1311455924071,-18.5890170612016));
#32938=CARTESIAN_POINT('Ctrl Pts',(-20.3149181792262,23.6276625113623,-18.5556932082558));
#32939=CARTESIAN_POINT('Ctrl Pts',(-20.3356134682672,23.923733169724,-18.5351866409336));
#32940=CARTESIAN_POINT('Ctrl Pts',(-20.3989383067089,24.2251558402493,-18.5157615024163));
#32941=CARTESIAN_POINT('Ctrl Pts',(-20.4015968617121,24.2374521422998,-18.514971911023));
#32942=CARTESIAN_POINT('Ctrl Pts',(-20.4050793761773,24.2531148139321,-18.5139700582298));
#32943=CARTESIAN_POINT('Ctrl Pts',(-20.405836806879,24.2564956313287,-18.5137540389695));
#32944=CARTESIAN_POINT('Ctrl Pts',(-20.4070593405504,24.2619114972591,-18.5134083692571));
#32945=CARTESIAN_POINT('Ctrl Pts',(-20.4075209687431,24.2639473147859,-18.5132785185702));
#32946=CARTESIAN_POINT('Ctrl Pts',(-20.4084013318278,24.2678123701854,-18.5130321589998));
#32947=CARTESIAN_POINT('Ctrl Pts',(-20.4088196832696,24.2696416772707,-18.5129156292191));
#32948=CARTESIAN_POINT('Ctrl Pts',(-20.4097812606891,24.2738294910194,-18.512649019332));
#32949=CARTESIAN_POINT('Ctrl Pts',(-20.4103255451283,24.27618774864,-18.5124990014317));
#32950=CARTESIAN_POINT('Ctrl Pts',(-20.4120091444995,24.2834450739504,-18.5120376872073));
#32951=CARTESIAN_POINT('Ctrl Pts',(-20.4131572792847,24.2883421193555,-18.511726899427));
#32952=CARTESIAN_POINT('Ctrl Pts',(-20.4218894466482,24.3251982511677,-18.5093914369112));
#32953=CARTESIAN_POINT('Ctrl Pts',(-20.4299505621905,24.3570438819683,-18.5073938027028));
#32954=CARTESIAN_POINT('Ctrl Pts',(-20.4406826865939,24.3968713803727,-18.504914693581));
#32955=CARTESIAN_POINT('Ctrl Pts',(-20.4428995474941,24.4049720945271,-18.5044114596321));
#32956=CARTESIAN_POINT('Ctrl Pts',(-20.446060058516,24.416346207733,-18.5037061690489));
#32957=CARTESIAN_POINT('Ctrl Pts',(-20.446977250674,24.4196268449872,-18.5035028935876));
#32958=CARTESIAN_POINT('Ctrl Pts',(-20.4497965758113,24.4296497709661,-18.5028822974948));
#32959=CARTESIAN_POINT('Ctrl Pts',(-20.4517155047012,24.4363873593577,-18.5024657396535));
#32960=CARTESIAN_POINT('Ctrl Pts',(-20.4552200562278,24.4485416789617,-18.5017153152276));
#32961=CARTESIAN_POINT('Ctrl Pts',(-20.4567979618975,24.4539605828386,-18.501381114507));
#32962=CARTESIAN_POINT('Ctrl Pts',(-20.5326802544959,24.712030895423,-18.4854815339245));
#32963=CARTESIAN_POINT('Ctrl Pts',(-20.6376665064033,24.9546554500305,-18.4712150431435));
#32964=CARTESIAN_POINT('Ctrl Pts',(-20.8659720275389,25.3435537016485,-18.4457478274155));
#32965=CARTESIAN_POINT('Ctrl Pts',(-20.9748410045294,25.4966672971269,-18.4349100854264));
#32966=CARTESIAN_POINT('Ctrl Pts',(-21.1017441367832,25.6457220179755,-18.4230091418124));
#32967=CARTESIAN_POINT('Ctrl Pts',(-21.1071204287556,25.6519878274655,-18.422506231955));
#32968=CARTESIAN_POINT('Ctrl Pts',(-21.1157439934182,25.6619603769088,-18.4217015628531));
#32969=CARTESIAN_POINT('Ctrl Pts',(-21.1189758181134,25.6656804761191,-18.4214004433954));
#32970=CARTESIAN_POINT('Ctrl Pts',(-21.1251430673902,25.6727466923139,-18.4208266553661));
#32971=CARTESIAN_POINT('Ctrl Pts',(-21.1280769193577,25.6760941717062,-18.4205540526225));
#32972=CARTESIAN_POINT('Ctrl Pts',(-21.1332225629593,25.6819407899663,-18.4200765559045));
#32973=CARTESIAN_POINT('Ctrl Pts',(-21.1354313240291,25.6844425970569,-18.4198717889806));
#32974=CARTESIAN_POINT('Ctrl Pts',(-21.139743820916,25.6893119859717,-18.4194723744698));
#32975=CARTESIAN_POINT('Ctrl Pts',(-21.1418471694528,25.6916799072263,-18.4192777432756));
#32976=CARTESIAN_POINT('Ctrl Pts',(-21.1468353042485,25.697278836788,-18.4188165863946));
#32977=CARTESIAN_POINT('Ctrl Pts',(-21.1497231154221,25.7005071317997,-18.4185499333667));
#32978=CARTESIAN_POINT('Ctrl Pts',(-21.1598572852436,25.7117902989115,-18.4176153053039));
#32979=CARTESIAN_POINT('Ctrl Pts',(-21.16713768669,25.7198143732358,-18.4169458906686));
#32980=CARTESIAN_POINT('Ctrl Pts',(-21.2612398816587,25.82248368211,-18.4083188457779));
#32981=CARTESIAN_POINT('Ctrl Pts',(-21.3535922850532,25.911881119943,-18.4001213143432));
#32982=CARTESIAN_POINT('Ctrl Pts',(-21.6083652100675,26.1306002489539,-18.378139209562));
#32983=CARTESIAN_POINT('Ctrl Pts',(-21.7783670839434,26.2501647503204,-18.3640416408662));
#32984=CARTESIAN_POINT('Ctrl Pts',(-21.9970129901276,26.3743472442521,-18.3470590293967));
#32985=CARTESIAN_POINT('Ctrl Pts',(-22.035816559176,26.3953442965779,-18.3440874952961));
#32986=CARTESIAN_POINT('Ctrl Pts',(-22.0750360259987,26.4155367800409,-18.341133076278));
#32987=CARTESIAN_POINT('Origin',(-23.5502525316942,23.5502525316942,-77.3107734492734));
#32988=CARTESIAN_POINT('',(-22.0750360036057,26.4155367685116,-16.8432706449041));
#32989=CARTESIAN_POINT('',(-22.0750360832114,26.4155368094973,-17.0912958973716));
#32990=CARTESIAN_POINT('',(-22.0750360153461,26.4155367745563,-77.3107734492734));
#32991=CARTESIAN_POINT('',(-26.7730012670434,23.5531887946472,-17.6894770438844));
#32992=CARTESIAN_POINT('Ctrl Pts',(-22.0750360036057,26.4155367685116,-16.8432706449041));
#32993=CARTESIAN_POINT('Ctrl Pts',(-21.96804694704,26.3604525215311,-16.8508191866373));
#32994=CARTESIAN_POINT('Ctrl Pts',(-21.8642302636496,26.2994208678429,-16.8585779079896));
#32995=CARTESIAN_POINT('Ctrl Pts',(-21.5633378707484,26.099065331876,-16.8823973090096));
#32996=CARTESIAN_POINT('Ctrl Pts',(-21.3782495467658,25.9432968497533,-16.8989554479486));
#32997=CARTESIAN_POINT('Ctrl Pts',(-21.1808597702974,25.7352424798406,-16.9181188309119));
#32998=CARTESIAN_POINT('Ctrl Pts',(-21.1501344007855,25.701446712473,-16.9211496604168));
#32999=CARTESIAN_POINT('Ctrl Pts',(-21.0959682993008,25.6392619682466,-16.9265650425278));
#33000=CARTESIAN_POINT('Ctrl Pts',(-21.0722758943645,25.6111027284705,-16.9289603448162));
#33001=CARTESIAN_POINT('Ctrl Pts',(-21.0247681712526,25.5526339692323,-16.9338085687613));
#33002=CARTESIAN_POINT('Ctrl Pts',(-21.0010033897433,25.5222900105741,-16.9362585083589));
#33003=CARTESIAN_POINT('Ctrl Pts',(-20.9749289354075,25.4877376168091,-16.9389680688449));
#33004=CARTESIAN_POINT('Ctrl Pts',(-20.9720788623098,25.4839434614478,-16.9392645347807));
#33005=CARTESIAN_POINT('Ctrl Pts',(-20.9677979087803,25.4782181588588,-16.939710272599));
#33006=CARTESIAN_POINT('Ctrl Pts',(-20.9663608071792,25.476291704456,-16.9398599788844));
#33007=CARTESIAN_POINT('Ctrl Pts',(-20.9638747984296,25.4729513855323,-16.9401190773998));
#33008=CARTESIAN_POINT('Ctrl Pts',(-20.9628248949125,25.4715382694568,-16.9402285399604));
#33009=CARTESIAN_POINT('Ctrl Pts',(-20.9606389506813,25.4685910595728,-16.940456525414));
#33010=CARTESIAN_POINT('Ctrl Pts',(-20.9595031162403,25.4670568182227,-16.9405750333541));
#33011=CARTESIAN_POINT('Ctrl Pts',(-20.9572447703715,25.4640006573558,-16.9408107503835));
#33012=CARTESIAN_POINT('Ctrl Pts',(-20.9561222326798,25.4624787553751,-16.9409279613844));
#33013=CARTESIAN_POINT('Ctrl Pts',(-20.9522620661767,25.4572356060327,-16.9413311835222));
#33014=CARTESIAN_POINT('Ctrl Pts',(-20.9495310829099,25.4535094379466,-16.9416167296418));
#33015=CARTESIAN_POINT('Ctrl Pts',(-20.9269107289283,25.4225065086866,-16.9439842800525));
#33016=CARTESIAN_POINT('Ctrl Pts',(-20.9074421058048,25.3949233540039,-16.9460375037073));
#33017=CARTESIAN_POINT('Ctrl Pts',(-20.8386717953634,25.2941653038298,-16.9533676938207));
#33018=CARTESIAN_POINT('Ctrl Pts',(-20.7919431031212,25.2192742892847,-16.9584986188464));
#33019=CARTESIAN_POINT('Ctrl Pts',(-20.6504257555518,24.9702518474096,-16.9748694763735));
#33020=CARTESIAN_POINT('Ctrl Pts',(-20.5686070458863,24.7892803981913,-16.9857434101372));
#33021=CARTESIAN_POINT('Ctrl Pts',(-20.4426548413835,24.4244441448356,-17.0075353906023));
#33022=CARTESIAN_POINT('Ctrl Pts',(-20.3970179391443,24.2419678355796,-17.018381759352));
#33023=CARTESIAN_POINT('Ctrl Pts',(-20.365573583826,24.044308993587,-17.0305452570156));
#33024=CARTESIAN_POINT('Ctrl Pts',(-20.3636934196434,24.0320334021841,-17.0313022108979));
#33025=CARTESIAN_POINT('Ctrl Pts',(-20.3612153948387,24.0152049841527,-17.0323421107643));
#33026=CARTESIAN_POINT('Ctrl Pts',(-20.3605562263855,24.0106611793497,-17.032623111525));
#33027=CARTESIAN_POINT('Ctrl Pts',(-20.3594489787931,24.0029121428463,-17.0331027120925));
#33028=CARTESIAN_POINT('Ctrl Pts',(-20.3589960123647,23.9997076067543,-17.0333011567648));
#33029=CARTESIAN_POINT('Ctrl Pts',(-20.3581277515499,23.9934975610663,-17.0336859376894));
#33030=CARTESIAN_POINT('Ctrl Pts',(-20.3577118727966,23.9904921360718,-17.0338722551661));
#33031=CARTESIAN_POINT('Ctrl Pts',(-20.3567328343199,23.9833425869162,-17.0343157179243));
#33032=CARTESIAN_POINT('Ctrl Pts',(-20.3561734971423,23.9791979527247,-17.0345729839876));
#33033=CARTESIAN_POINT('Ctrl Pts',(-20.3545528916947,23.9670104795249,-17.03533004539));
#33034=CARTESIAN_POINT('Ctrl Pts',(-20.3535139288785,23.9589647525921,-17.0358305459737));
#33035=CARTESIAN_POINT('Ctrl Pts',(-20.3456798904373,23.8964401570158,-17.0397256913232));
#33036=CARTESIAN_POINT('Ctrl Pts',(-20.340247903784,23.8418024812624,-17.0431631955353));
#33037=CARTESIAN_POINT('Ctrl Pts',(-20.3265403901067,23.6557553758703,-17.0549926988762));
#33038=CARTESIAN_POINT('Ctrl Pts',(-20.3249224193299,23.5240019232793,-17.0635868173886));
#33039=CARTESIAN_POINT('Ctrl Pts',(-20.340012973357,23.216021887351,-17.0841202573986));
#33040=CARTESIAN_POINT('Ctrl Pts',(-20.3631656999452,23.0405268389459,-17.0961726180614));
#33041=CARTESIAN_POINT('Ctrl Pts',(-20.4311993539924,22.7265239113891,-17.1177944931616));
#33042=CARTESIAN_POINT('Ctrl Pts',(-20.4712936712857,22.5874207338688,-17.1273862976394));
#33043=CARTESIAN_POINT('Ctrl Pts',(-20.5237631528781,22.4427483184868,-17.13706344723));
#33044=CARTESIAN_POINT('Ctrl Pts',(-20.5269622483884,22.4340449299208,-17.1376444115209));
#33045=CARTESIAN_POINT('Ctrl Pts',(-20.531319261265,22.4223474942285,-17.1384234897314));
#33046=CARTESIAN_POINT('Ctrl Pts',(-20.5324441114198,22.4193413045942,-17.138623554));
#33047=CARTESIAN_POINT('Ctrl Pts',(-20.5342165065292,22.4146260096051,-17.1389371108304));
#33048=CARTESIAN_POINT('Ctrl Pts',(-20.5348610134828,22.4129157765051,-17.1390507859801));
#33049=CARTESIAN_POINT('Ctrl Pts',(-20.5361035694441,22.4096270694643,-17.1392692779407));
#33050=CARTESIAN_POINT('Ctrl Pts',(-20.5367013997857,22.4080485275388,-17.1393741067806));
#33051=CARTESIAN_POINT('Ctrl Pts',(-20.5381229949944,22.4043037598441,-17.1396226862725));
#33052=CARTESIAN_POINT('Ctrl Pts',(-20.5389478557297,22.4021379545899,-17.1397663698265));
#33053=CARTESIAN_POINT('Ctrl Pts',(-20.541357039018,22.3958327113567,-17.1401844329048));
#33054=CARTESIAN_POINT('Ctrl Pts',(-20.5429475737639,22.3916956284733,-17.1404584385661));
#33055=CARTESIAN_POINT('Ctrl Pts',(-20.5548018470508,22.3610507989383,-17.1424859649064));
#33056=CARTESIAN_POINT('Ctrl Pts',(-20.5654077729336,22.3346755222715,-17.1442191818706));
#33057=CARTESIAN_POINT('Ctrl Pts',(-20.6017292012615,22.247692813452,-17.1499066817369));
#33058=CARTESIAN_POINT('Ctrl Pts',(-20.6289540819225,22.1877297734362,-17.153781279089));
#33059=CARTESIAN_POINT('Ctrl Pts',(-20.7372658994601,21.9673708566774,-17.1679965221193));
#33060=CARTESIAN_POINT('Ctrl Pts',(-20.8298874308516,21.8130044935711,-17.1779212820264));
#33061=CARTESIAN_POINT('Ctrl Pts',(-21.0697770029897,21.4798321146654,-17.2009104912029));
#33062=CARTESIAN_POINT('Ctrl Pts',(-21.2243639869269,21.3075713596742,-17.2140341460924));
#33063=CARTESIAN_POINT('Ctrl Pts',(-21.407173196034,21.1432722858051,-17.2289467389562));
#33064=CARTESIAN_POINT('Ctrl Pts',(-21.4184088251431,21.13331534965,-17.229860817));
#33065=CARTESIAN_POINT('Ctrl Pts',(-21.4338731860062,21.1198026675201,-17.2311157467339));
#33066=CARTESIAN_POINT('Ctrl Pts',(-21.4380422232875,21.1161786442416,-17.231453750464));
#33067=CARTESIAN_POINT('Ctrl Pts',(-21.4446679149906,21.1104489631132,-17.2319904410409));
#33068=CARTESIAN_POINT('Ctrl Pts',(-21.4471184716641,21.1083362438626,-17.2321888347765));
#33069=CARTESIAN_POINT('Ctrl Pts',(-21.4518733433731,21.1042493526764,-17.2325735818699));
#33070=CARTESIAN_POINT('Ctrl Pts',(-21.4541772740624,21.1022747368623,-17.2327599166013));
#33071=CARTESIAN_POINT('Ctrl Pts',(-21.4596648744836,21.0975849394553,-17.2332035223859));
#33072=CARTESIAN_POINT('Ctrl Pts',(-21.4628510441962,21.0948727035968,-17.2334609144467));
#33073=CARTESIAN_POINT('Ctrl Pts',(-21.4694597672096,21.0892691698485,-17.2339944456541));
#33074=CARTESIAN_POINT('Ctrl Pts',(-21.4728830841221,21.0863787902088,-17.2342706217937));
#33075=CARTESIAN_POINT('Ctrl Pts',(-21.492359883828,21.0700035586344,-17.235840834072));
#33076=CARTESIAN_POINT('Ctrl Pts',(-21.5085383256254,21.0566687280514,-17.2371409867368));
#33077=CARTESIAN_POINT('Ctrl Pts',(-21.5512427408478,21.0221644912691,-17.2405626831116));
#33078=CARTESIAN_POINT('Ctrl Pts',(-21.5779744559629,21.0012550161763,-17.2426944903578));
#33079=CARTESIAN_POINT('Ctrl Pts',(-21.6996767922388,20.9091204109294,-17.2523581312154));
#33080=CARTESIAN_POINT('Ctrl Pts',(-21.7981990149075,20.842760632787,-17.2600734043017));
#33081=CARTESIAN_POINT('Ctrl Pts',(-22.033301404395,20.7026207861129,-17.2782136140443));
#33082=CARTESIAN_POINT('Ctrl Pts',(-22.1720017570271,20.6329649998257,-17.2887274587443));
#33083=CARTESIAN_POINT('Ctrl Pts',(-22.4308285575074,20.5255725859626,-17.3076802213987));
#33084=CARTESIAN_POINT('Ctrl Pts',(-22.549199646221,20.4843601060258,-17.3161103330227));
#33085=CARTESIAN_POINT('Ctrl Pts',(-22.6748546029482,20.4486682578361,-17.3246370894903));
#33086=CARTESIAN_POINT('Ctrl Pts',(-22.680036676437,20.4472103296837,-17.3249879944401));
#33087=CARTESIAN_POINT('Ctrl Pts',(-22.6905340072655,20.4442853675455,-17.3256972884426));
#33088=CARTESIAN_POINT('Ctrl Pts',(-22.6958494286436,20.4428189758001,-17.3260556513625));
#33089=CARTESIAN_POINT('Ctrl Pts',(-22.7107655350814,20.4387451613446,-17.3270590124645));
#33090=CARTESIAN_POINT('Ctrl Pts',(-22.7203746521251,20.4361685182054,-17.3277027496838));
#33091=CARTESIAN_POINT('Ctrl Pts',(-22.7316890351813,20.433190705099,-17.3284575075749));
#33092=CARTESIAN_POINT('Ctrl Pts',(-22.7333827737537,20.432746408649,-17.3285704084954));
#33093=CARTESIAN_POINT('Ctrl Pts',(-22.7743444358782,20.4220371413395,-17.3312987626036));
#33094=CARTESIAN_POINT('Ctrl Pts',(-22.8138047610682,20.4125129049238,-17.3338813594173));
#33095=CARTESIAN_POINT('Ctrl Pts',(-22.8585920405919,20.4025944802969,-17.3367530450246));
#33096=CARTESIAN_POINT('Ctrl Pts',(-22.8637502232173,20.4014654596809,-17.3370828908535));
#33097=CARTESIAN_POINT('Ctrl Pts',(-22.8713353541448,20.3998247543918,-17.3375666021878));
#33098=CARTESIAN_POINT('Ctrl Pts',(-22.8737601217602,20.3993031932612,-17.3377210327133));
#33099=CARTESIAN_POINT('Ctrl Pts',(-22.8780346559443,20.3983889137949,-17.337992918496));
#33100=CARTESIAN_POINT('Ctrl Pts',(-22.8798841677855,20.3979950239611,-17.3381104416108));
#33101=CARTESIAN_POINT('Ctrl Pts',(-22.8837275527096,20.397180035273,-17.3383544170978));
#33102=CARTESIAN_POINT('Ctrl Pts',(-22.8857214749929,20.3967592004767,-17.3384808539184));
#33103=CARTESIAN_POINT('Ctrl Pts',(-22.8897616608319,20.3959104858391,-17.3387367735365));
#33104=CARTESIAN_POINT('Ctrl Pts',(-22.8918079445305,20.395482705156,-17.3388662505562));
#33105=CARTESIAN_POINT('Ctrl Pts',(-22.8998270433523,20.393814434748,-17.3393731024957));
#33106=CARTESIAN_POINT('Ctrl Pts',(-22.9058030101936,20.3925889030892,-17.3397496212549));
#33107=CARTESIAN_POINT('Ctrl Pts',(-23.0043178110267,20.3726771288172,-17.3459374434307));
#33108=CARTESIAN_POINT('Ctrl Pts',(-23.0976409194408,20.3580468877669,-17.351521241554));
#33109=CARTESIAN_POINT('Ctrl Pts',(-23.3390432656529,20.3310048111058,-17.3655639843818));
#33110=CARTESIAN_POINT('Ctrl Pts',(-23.4875802407342,20.3246916601377,-17.3738269725923));
#33111=CARTESIAN_POINT('Ctrl Pts',(-23.7963756034704,20.3329136186268,-17.391089225246));
#33112=CARTESIAN_POINT('Ctrl Pts',(-23.9561698241481,20.3491476900238,-17.4000750001182));
#33113=CARTESIAN_POINT('Ctrl Pts',(-24.1481326698673,20.3832582173666,-17.4113942252007));
#33114=CARTESIAN_POINT('Ctrl Pts',(-24.1820832267468,20.3898564329187,-17.4134157812549));
#33115=CARTESIAN_POINT('Ctrl Pts',(-24.2863502877249,20.4118677378608,-17.4196931617098));
#33116=CARTESIAN_POINT('Ctrl Pts',(-24.3562578225558,20.4290903657804,-17.423999651768));
#33117=CARTESIAN_POINT('Ctrl Pts',(-24.434719751617,20.4512322753629,-17.4289649146538));
#33118=CARTESIAN_POINT('Ctrl Pts',(-24.4439015124666,20.4538674929203,-17.4295480154675));
#33119=CARTESIAN_POINT('Ctrl Pts',(-24.4572956640277,20.4577762289306,-17.4304016828261));
#33120=CARTESIAN_POINT('Ctrl Pts',(-24.4615174374266,20.4590176330908,-17.4306711988149));
#33121=CARTESIAN_POINT('Ctrl Pts',(-24.4689853690408,20.4612301917346,-17.43114873944));
#33122=CARTESIAN_POINT('Ctrl Pts',(-24.4722325697174,20.4621978280765,-17.4313566485794));
#33123=CARTESIAN_POINT('Ctrl Pts',(-24.4789637907268,20.4642152343999,-17.4317881827261));
#33124=CARTESIAN_POINT('Ctrl Pts',(-24.4824475697235,20.4652657871772,-17.4320118331544));
#33125=CARTESIAN_POINT('Ctrl Pts',(-24.4914048405004,20.4679834596311,-17.4325876645351));
#33126=CARTESIAN_POINT('Ctrl Pts',(-24.4968756680402,20.4696592547382,-17.4329401299383));
#33127=CARTESIAN_POINT('Ctrl Pts',(-24.5086808465571,20.4733097712065,-17.4337023600789));
#33128=CARTESIAN_POINT('Ctrl Pts',(-24.5150136104179,20.4752895000512,-17.4341122884583));
#33129=CARTESIAN_POINT('Ctrl Pts',(-24.5640902599528,20.4907982178886,-17.4372972083485));
#33130=CARTESIAN_POINT('Ctrl Pts',(-24.6065519239492,20.5051977039566,-17.4401007952553));
#33131=CARTESIAN_POINT('Ctrl Pts',(-24.74547229614,20.5555633003076,-17.4494380162596));
#33132=CARTESIAN_POINT('Ctrl Pts',(-24.8405007964626,20.5952619060911,-17.4560931892079));
#33133=CARTESIAN_POINT('Ctrl Pts',(-25.0062329707142,20.6740170766408,-17.4681777336673));
#33134=CARTESIAN_POINT('Ctrl Pts',(-25.0776802754617,20.7113138777421,-17.4735545408708));
#33135=CARTESIAN_POINT('Ctrl Pts',(-25.2142658345626,20.7892635755675,-17.4841314241855));
#33136=CARTESIAN_POINT('Ctrl Pts',(-25.2795005427411,20.8296457565682,-17.4893242238635));
#33137=CARTESIAN_POINT('Ctrl Pts',(-25.4638365354826,20.953065598104,-17.5043400411272));
#33138=CARTESIAN_POINT('Ctrl Pts',(-25.5788577619415,21.0418764631769,-17.5141492582854));
#33139=CARTESIAN_POINT('Ctrl Pts',(-25.6935130119421,21.1434670236394,-17.524136936191));
#33140=CARTESIAN_POINT('Ctrl Pts',(-25.6994998051523,21.1488116875558,-17.5246590669108));
#33141=CARTESIAN_POINT('Ctrl Pts',(-25.7443728087281,21.1891739371715,-17.5285768787183));
#33142=CARTESIAN_POINT('Ctrl Pts',(-25.7824237520687,21.2251141803083,-17.5319233599273));
#33143=CARTESIAN_POINT('Ctrl Pts',(-25.8236561060968,21.2660050355662,-17.535560355957));
#33144=CARTESIAN_POINT('Ctrl Pts',(-25.827716392031,21.2700532417767,-17.5359186207287));
#33145=CARTESIAN_POINT('Ctrl Pts',(-25.8333894611651,21.27573970293,-17.536419328156));
#33146=CARTESIAN_POINT('Ctrl Pts',(-25.8350112968492,21.2773688496605,-17.5365624877546));
#33147=CARTESIAN_POINT('Ctrl Pts',(-25.8379758026856,21.2803530984839,-17.5368241913237));
#33148=CARTESIAN_POINT('Ctrl Pts',(-25.8393190146191,21.2817076592414,-17.5369427786302));
#33149=CARTESIAN_POINT('Ctrl Pts',(-25.8420450773319,21.2844616408839,-17.5371834714584));
#33150=CARTESIAN_POINT('Ctrl Pts',(-25.8434278497673,21.2858611358111,-17.5373055707346));
#33151=CARTESIAN_POINT('Ctrl Pts',(-25.8462036552274,21.2886756606445,-17.5375506973321));
#33152=CARTESIAN_POINT('Ctrl Pts',(-25.8475966637942,21.2900907135765,-17.5376737226982));
#33153=CARTESIAN_POINT('Ctrl Pts',(-25.8509391731548,21.2934924009907,-17.5379689503513));
#33154=CARTESIAN_POINT('Ctrl Pts',(-25.8528874140144,21.2954802796499,-17.5381410532511));
#33155=CARTESIAN_POINT('Ctrl Pts',(-25.8667138213189,21.3096246005948,-17.5393626392026));
#33156=CARTESIAN_POINT('Ctrl Pts',(-25.8784985318812,21.3218726214436,-17.5404048595836));
#33157=CARTESIAN_POINT('Ctrl Pts',(-25.9787338810159,21.4277119440664,-17.5492844128103));
#33158=CARTESIAN_POINT('Ctrl Pts',(-26.0616097220952,21.5264458220591,-17.5567285263041));
#33159=CARTESIAN_POINT('Ctrl Pts',(-26.1639331037628,21.6643487877935,-17.5664634220971));
#33160=CARTESIAN_POINT('Ctrl Pts',(-26.1888134171712,21.6993188101822,-17.568879186385));
#33161=CARTESIAN_POINT('Ctrl Pts',(-26.2381809917884,21.771725581756,-17.5737955040987));
#33162=CARTESIAN_POINT('Ctrl Pts',(-26.2626019947166,21.8091959672489,-17.5762948004595));
#33163=CARTESIAN_POINT('Ctrl Pts',(-26.4286473133635,22.0759447483404,-17.5938515949625));
#33164=CARTESIAN_POINT('Ctrl Pts',(-26.5417804183748,22.3216457388228,-17.6089401347476));
#33165=CARTESIAN_POINT('Ctrl Pts',(-26.6282426640411,22.5950591688404,-17.6263134833063));
#33166=CARTESIAN_POINT('Ctrl Pts',(-26.6333322020503,22.6116166367759,-17.6273672319988));
#33167=CARTESIAN_POINT('Ctrl Pts',(-26.6399642398489,22.6338282566221,-17.6287832823414));
#33168=CARTESIAN_POINT('Ctrl Pts',(-26.6416252212874,22.6394469625577,-17.6291416995508));
#33169=CARTESIAN_POINT('Ctrl Pts',(-26.6441984180381,22.6482396045388,-17.6297029203342));
#33170=CARTESIAN_POINT('Ctrl Pts',(-26.6451210983771,22.6514104859446,-17.6299053814626));
#33171=CARTESIAN_POINT('Ctrl Pts',(-26.646877599503,22.657481643505,-17.6302931591227));
#33172=CARTESIAN_POINT('Ctrl Pts',(-26.6477122240757,22.6603816852491,-17.6304784491741));
#33173=CARTESIAN_POINT('Ctrl Pts',(-26.6496553301233,22.6671691852948,-17.6309122557648));
#33174=CARTESIAN_POINT('Ctrl Pts',(-26.6507605712623,22.6710575590427,-17.6311608777462));
#33175=CARTESIAN_POINT('Ctrl Pts',(-26.653021987363,22.6790707947807,-17.6316734651046));
#33176=CARTESIAN_POINT('Ctrl Pts',(-26.6541772590579,22.6831959012837,-17.631937459399));
#33177=CARTESIAN_POINT('Ctrl Pts',(-26.6571229753068,22.6937954497064,-17.6326161152338));
#33178=CARTESIAN_POINT('Ctrl Pts',(-26.6589014013733,22.7002731845175,-17.6330311675787));
#33179=CARTESIAN_POINT('Ctrl Pts',(-26.6733009722911,22.7533718584892,-17.6364359452005));
#33180=CARTESIAN_POINT('Ctrl Pts',(-26.6848922723432,22.80026342731,-17.6394589367402));
#33181=CARTESIAN_POINT('Ctrl Pts',(-26.7472119689281,23.079134187124,-17.6575448897184));
#33182=CARTESIAN_POINT('Ctrl Pts',(-26.773217394735,23.3158359840599,-17.673413816263));
#33183=CARTESIAN_POINT('Ctrl Pts',(-26.7730011947243,23.5531880789698,-17.6894771219796));
#33184=CARTESIAN_POINT('Ctrl Pts',(-26.7730011940801,23.5531887860566,-17.6894771698332));
#33185=CARTESIAN_POINT('Ctrl Pts',(-26.7728035334531,23.7701354272215,-17.7041594933754));
#33186=CARTESIAN_POINT('Ctrl Pts',(-26.750700095684,23.9865403688873,-17.7189048342478));
#33187=CARTESIAN_POINT('Ctrl Pts',(-26.7054279707792,24.2067942912656,-17.7330769488637));
#33188=CARTESIAN_POINT('Ctrl Pts',(-26.703820059033,24.2144746232993,-17.7335700142139));
#33189=CARTESIAN_POINT('Ctrl Pts',(-26.7013473410846,24.2260743815403,-17.7343129250898));
#33190=CARTESIAN_POINT('Ctrl Pts',(-26.700503252243,24.2299981227726,-17.7345639150239));
#33191=CARTESIAN_POINT('Ctrl Pts',(-26.699121999286,24.236361033653,-17.7349704207056));
#33192=CARTESIAN_POINT('Ctrl Pts',(-26.698589328965,24.2388011584762,-17.735126190413));
#33193=CARTESIAN_POINT('Ctrl Pts',(-26.6975549418408,24.243513316233,-17.7354267604997));
#33194=CARTESIAN_POINT('Ctrl Pts',(-26.697053600321,24.245785428735,-17.7355715822987));
#33195=CARTESIAN_POINT('Ctrl Pts',(-26.6961492433367,24.249863040753,-17.7358312892841));
#33196=CARTESIAN_POINT('Ctrl Pts',(-26.6957471348637,24.2516687321048,-17.735946226568));
#33197=CARTESIAN_POINT('Ctrl Pts',(-26.6948765312281,24.2555624233151,-17.7361939218202));
#33198=CARTESIAN_POINT('Ctrl Pts',(-26.694407512394,24.2576502975004,-17.7363266487428));
#33199=CARTESIAN_POINT('Ctrl Pts',(-26.6931425309738,24.2632553500378,-17.7366827202205));
#33200=CARTESIAN_POINT('Ctrl Pts',(-26.6923427410553,24.2667716752463,-17.7369058435285));
#33201=CARTESIAN_POINT('Ctrl Pts',(-26.6886742590934,24.2827761185761,-17.7379202384871));
#33202=CARTESIAN_POINT('Ctrl Pts',(-26.6857369557167,24.2952486283448,-17.7387075995406));
#33203=CARTESIAN_POINT('Ctrl Pts',(-26.6325100435688,24.5153709223802,-17.7525526223934));
#33204=CARTESIAN_POINT('Ctrl Pts',(-26.5617591528579,24.7175671545417,-17.7644892674023));
#33205=CARTESIAN_POINT('Ctrl Pts',(-26.4514109483188,24.9544105521194,-17.7790919781919));
#33206=CARTESIAN_POINT('Ctrl Pts',(-26.4303715395265,24.9970746987324,-17.7817475530847));
#33207=CARTESIAN_POINT('Ctrl Pts',(-26.3864584058268,25.0813659080866,-17.7870688223549));
#33208=CARTESIAN_POINT('Ctrl Pts',(-26.3635935689955,25.1229839214066,-17.7897338211128));
#33209=CARTESIAN_POINT('Ctrl Pts',(-26.2717749514428,25.2816959764744,-17.8000854151909));
#33210=CARTESIAN_POINT('Ctrl Pts',(-26.1963685145398,25.3948785722305,-17.8078795774982));
#33211=CARTESIAN_POINT('Ctrl Pts',(-26.0803588544134,25.5471930432055,-17.8192351448813));
#33212=CARTESIAN_POINT('Ctrl Pts',(-26.0455299702784,25.5905464661932,-17.8225740260591));
#33213=CARTESIAN_POINT('Ctrl Pts',(-26.005028931909,25.6383713948799,-17.8263889033132));
#33214=CARTESIAN_POINT('Ctrl Pts',(-26.00044152117,25.6437523469423,-17.8268200545638));
#33215=CARTESIAN_POINT('Ctrl Pts',(-25.9929495705041,25.6524819169802,-17.8275226780766));
#33216=CARTESIAN_POINT('Ctrl Pts',(-25.9900557482718,25.6558397362144,-17.8277937075588));
#33217=CARTESIAN_POINT('Ctrl Pts',(-25.9844393862448,25.6623295049565,-17.8283190270339));
#33218=CARTESIAN_POINT('Ctrl Pts',(-25.9817177052509,25.6654621887675,-17.8285732811022));
#33219=CARTESIAN_POINT('Ctrl Pts',(-25.9769984613108,25.6708729445602,-17.8290136038822));
#33220=CARTESIAN_POINT('Ctrl Pts',(-25.9750037178381,25.673153477939,-17.8291995548565));
#33221=CARTESIAN_POINT('Ctrl Pts',(-25.9708625323528,25.6778745259783,-17.8295852567235));
#33222=CARTESIAN_POINT('Ctrl Pts',(-25.9687156092587,25.6803146125233,-17.8297850276312));
#33223=CARTESIAN_POINT('Ctrl Pts',(-25.9628610868698,25.6869483113336,-17.8303292786548));
#33224=CARTESIAN_POINT('Ctrl Pts',(-25.9591462598095,25.6911355040328,-17.8306740618876));
#33225=CARTESIAN_POINT('Ctrl Pts',(-25.9451054690054,25.7068788651299,-17.8319751549206));
#33226=CARTESIAN_POINT('Ctrl Pts',(-25.9347072325416,25.7183700330137,-17.8329345109604));
#33227=CARTESIAN_POINT('Ctrl Pts',(-25.7647938320869,25.903441791644,-17.8485450138293));
#33228=CARTESIAN_POINT('Ctrl Pts',(-25.5868230700623,26.0590431341482,-17.8640432729725));
#33229=CARTESIAN_POINT('Ctrl Pts',(-25.3716960621877,26.209043404578,-17.8817262533506));
#33230=CARTESIAN_POINT('Ctrl Pts',(-25.3496841183654,26.2239898760536,-17.8835234858929));
#33231=CARTESIAN_POINT('Ctrl Pts',(-25.2363760842775,26.2988948571337,-17.8927083679957));
#33232=CARTESIAN_POINT('Ctrl Pts',(-25.1422580262028,26.3544576793462,-17.9001229345794));
#33233=CARTESIAN_POINT('Ctrl Pts',(-24.9600283072215,26.449900627059,-17.913907583769));
#33234=CARTESIAN_POINT('Ctrl Pts',(-24.8725820426677,26.4908094153954,-17.9202911940178));
#33235=CARTESIAN_POINT('Ctrl Pts',(-24.7509725740385,26.5411759226895,-17.9287417151288));
#33236=CARTESIAN_POINT('Ctrl Pts',(-24.7183012032523,26.5540857334741,-17.9309711779779));
#33237=CARTESIAN_POINT('Ctrl Pts',(-24.6821253946209,26.5677007589501,-17.9333900180984));
#33238=CARTESIAN_POINT('Ctrl Pts',(-24.6788250694092,26.5689366836709,-17.9336102368542));
#33239=CARTESIAN_POINT('Ctrl Pts',(-24.6733746801333,26.5709675888983,-17.9339731674107));
#33240=CARTESIAN_POINT('Ctrl Pts',(-24.6712257939587,26.5717656894515,-17.9341160642425));
#33241=CARTESIAN_POINT('Ctrl Pts',(-24.6670320090291,26.5733181797033,-17.934394563579));
#33242=CARTESIAN_POINT('Ctrl Pts',(-24.6649871935428,26.5740727887383,-17.9345301791998));
#33243=CARTESIAN_POINT('Ctrl Pts',(-24.6613676932683,26.5754043415516,-17.9347699177233));
#33244=CARTESIAN_POINT('Ctrl Pts',(-24.6597933320916,26.5759821275511,-17.9348740911488));
#33245=CARTESIAN_POINT('Ctrl Pts',(-24.6564246109142,26.5772154556602,-17.9350967711779));
#33246=CARTESIAN_POINT('Ctrl Pts',(-24.6546301239791,26.5778706294102,-17.935215255227));
#33247=CARTESIAN_POINT('Ctrl Pts',(-24.6494332596186,26.5797627885037,-17.935557997589));
#33248=CARTESIAN_POINT('Ctrl Pts',(-24.6460293650796,26.5809956419686,-17.9357820074977));
#33249=CARTESIAN_POINT('Ctrl Pts',(-24.6308131773084,26.5864777934003,-17.9367812573661));
#33250=CARTESIAN_POINT('Ctrl Pts',(-24.6189779848573,26.5906638635103,-17.9375527591955));
#33251=CARTESIAN_POINT('Ctrl Pts',(-24.4161254700783,26.6610813091487,-17.9506834035905));
#33252=CARTESIAN_POINT('Ctrl Pts',(-24.2192839323799,26.7092738162329,-17.9620366300861));
#33253=CARTESIAN_POINT('Ctrl Pts',(-23.8489258161291,26.763744577359,-17.9829719347536));
#33254=CARTESIAN_POINT('Ctrl Pts',(-23.6769269959545,26.77510703349,-17.9925349779485));
#33255=CARTESIAN_POINT('Ctrl Pts',(-23.392971874663,26.7711064833021,-18.008891086484));
#33256=CARTESIAN_POINT('Ctrl Pts',(-23.2812599049993,26.7637049200551,-18.0154671849132));
#33257=CARTESIAN_POINT('Ctrl Pts',(-23.1490820364862,26.74800653137,-18.0235144916919));
#33258=CARTESIAN_POINT('Ctrl Pts',(-23.1280227536391,26.7452940634512,-18.0248046057233));
#33259=CARTESIAN_POINT('Ctrl Pts',(-23.1025383600989,26.7417552815286,-18.0263759263683));
#33260=CARTESIAN_POINT('Ctrl Pts',(-23.0980858416614,26.7411275003744,-18.0266508352648));
#33261=CARTESIAN_POINT('Ctrl Pts',(-23.0894810167038,26.7398958941639,-18.027182848125));
#33262=CARTESIAN_POINT('Ctrl Pts',(-23.0853285447567,26.7392932738109,-18.0274399134497));
#33263=CARTESIAN_POINT('Ctrl Pts',(-23.0781736617958,26.7382406621713,-18.0278834196943));
#33264=CARTESIAN_POINT('Ctrl Pts',(-23.0751706806876,26.7377945336463,-18.0280697377896));
#33265=CARTESIAN_POINT('Ctrl Pts',(-23.0689732858832,26.7368648846715,-18.0284546118971));
#33266=CARTESIAN_POINT('Ctrl Pts',(-23.0657789607793,26.7363808027408,-18.0286531855597));
#33267=CARTESIAN_POINT('Ctrl Pts',(-23.057148814067,26.7350596742105,-18.0291902120993));
#33268=CARTESIAN_POINT('Ctrl Pts',(-23.0517144165878,26.7342135174079,-18.0295289540927));
#33269=CARTESIAN_POINT('Ctrl Pts',(-23.0316095850853,26.7310303830804,-18.0307843009646));
#33270=CARTESIAN_POINT('Ctrl Pts',(-23.0169533713841,26.7286059166507,-18.0317036838377));
#33271=CARTESIAN_POINT('Ctrl Pts',(-22.7629733867044,26.684785763111,-18.0477110970093));
#33272=CARTESIAN_POINT('Ctrl Pts',(-22.5291197751893,26.6165773670986,-18.0637028269546));
#33273=CARTESIAN_POINT('Ctrl Pts',(-22.227063604625,26.4900591572379,-18.0858020752168));
#33274=CARTESIAN_POINT('Ctrl Pts',(-22.1502873850307,26.4542806029891,-18.0915453905923));
#33275=CARTESIAN_POINT('Ctrl Pts',(-22.0750358296283,26.4155366789378,-18.0972636326348));
#33276=CARTESIAN_POINT('Ctrl Pts',(-22.0750360259987,26.4155367800409,-18.341133076278));
#33277=CARTESIAN_POINT('Ctrl Pts',(-22.1107494798326,26.4339241622357,-18.3384427667008));
#33278=CARTESIAN_POINT('Ctrl Pts',(-22.1468077974856,26.4516443954618,-18.3357666641265));
#33279=CARTESIAN_POINT('Ctrl Pts',(-22.2398433215542,26.495224313223,-18.3289790137113));
#33280=CARTESIAN_POINT('Ctrl Pts',(-22.2972591835044,26.520107725815,-18.3248999815242));
#33281=CARTESIAN_POINT('Ctrl Pts',(-22.3812604016217,26.5536426650787,-18.3191249420596));
#33282=CARTESIAN_POINT('Ctrl Pts',(-22.4072880474223,26.5636438455556,-18.3173617455498));
#33283=CARTESIAN_POINT('Ctrl Pts',(-22.437593091106,26.5748394626856,-18.3153416885302));
#33284=CARTESIAN_POINT('Ctrl Pts',(-22.4417460973369,26.5763640001303,-18.3150655712501));
#33285=CARTESIAN_POINT('Ctrl Pts',(-22.4480601401913,26.5786670955536,-18.3146468696084));
#33286=CARTESIAN_POINT('Ctrl Pts',(-22.4502188702196,26.5794518949228,-18.3145039123284));
#33287=CARTESIAN_POINT('Ctrl Pts',(-22.4541320335498,26.5808697782033,-18.3142451254041));
#33288=CARTESIAN_POINT('Ctrl Pts',(-22.4558861719905,26.5815036450292,-18.3141292489129));
#33289=CARTESIAN_POINT('Ctrl Pts',(-22.459681324592,26.5828713189604,-18.3138788241553));
#33290=CARTESIAN_POINT('Ctrl Pts',(-22.4617225238618,26.5836045865594,-18.313744308768));
#33291=CARTESIAN_POINT('Ctrl Pts',(-22.4672761975808,26.5855933257188,-18.3133787898246));
#33292=CARTESIAN_POINT('Ctrl Pts',(-22.4707901277886,26.5868447655985,-18.3131480280056));
#33293=CARTESIAN_POINT('Ctrl Pts',(-22.4875113190866,26.592767104514,-18.3120523259615));
#33294=CARTESIAN_POINT('Ctrl Pts',(-22.5007470330634,26.5973580493987,-18.3111920981217));
#33295=CARTESIAN_POINT('Ctrl Pts',(-22.5160201263872,26.6025443574281,-18.3102071309731));
#33296=CARTESIAN_POINT('Ctrl Pts',(-22.5180283853333,26.6032240954885,-18.3100777700008));
#33297=CARTESIAN_POINT('Ctrl Pts',(-22.8280940049207,26.7078314963447,-18.2901283470691));
#33298=CARTESIAN_POINT('Ctrl Pts',(-23.1501613477646,26.7645688927759,-18.2728100441047));
#33299=CARTESIAN_POINT('Ctrl Pts',(-23.6306063543078,26.7757428592564,-18.2455409653934));
#33300=CARTESIAN_POINT('Ctrl Pts',(-23.7859310549281,26.7681230463719,-18.2365330128787));
#33301=CARTESIAN_POINT('Ctrl Pts',(-23.955229316461,26.7474925931426,-18.2262329649932));
#33302=CARTESIAN_POINT('Ctrl Pts',(-23.9703564997288,26.7455401322749,-18.2253085078733));
#33303=CARTESIAN_POINT('Ctrl Pts',(-23.9930608112159,26.7424456799021,-18.2239145797278));
#33304=CARTESIAN_POINT('Ctrl Pts',(-24.0006488010966,26.7413839089327,-18.2234476377551));
#33305=CARTESIAN_POINT('Ctrl Pts',(-24.0128659925645,26.7396299406051,-18.2226940643438));
#33306=CARTESIAN_POINT('Ctrl Pts',(-24.0174976296833,26.7389546953795,-18.222407969566));
#33307=CARTESIAN_POINT('Ctrl Pts',(-24.0263505382048,26.7376443295785,-18.2218603392672));
#33308=CARTESIAN_POINT('Ctrl Pts',(-24.0305720539617,26.7370109067949,-18.221598858062));
#33309=CARTESIAN_POINT('Ctrl Pts',(-24.0380618322143,26.7358718727354,-18.2211343262571));
#33310=CARTESIAN_POINT('Ctrl Pts',(-24.0413306046607,26.7353696136566,-18.2209313823916));
#33311=CARTESIAN_POINT('Ctrl Pts',(-24.0477816676953,26.7343682170087,-18.2205304515273));
#33312=CARTESIAN_POINT('Ctrl Pts',(-24.0509639951835,26.7338693379131,-18.2203324729523));
#33313=CARTESIAN_POINT('Ctrl Pts',(-24.0586248664506,26.7326566070337,-18.2198553957831));
#33314=CARTESIAN_POINT('Ctrl Pts',(-24.0631026530686,26.7319380727499,-18.219576148512));
#33315=CARTESIAN_POINT('Ctrl Pts',(-24.0768449981306,26.7297031239346,-18.2187179153245));
#33316=CARTESIAN_POINT('Ctrl Pts',(-24.0861043971485,26.7281556877863,-18.2181379431855));
#33317=CARTESIAN_POINT('Ctrl Pts',(-24.1202295320153,26.7222992926321,-18.2159940970215));
#33318=CARTESIAN_POINT('Ctrl Pts',(-24.1450506508554,26.7177388494945,-18.2144222331254));
#33319=CARTESIAN_POINT('Ctrl Pts',(-24.1757416351714,26.7117264625948,-18.212462655042));
#33320=CARTESIAN_POINT('Ctrl Pts',(-24.1816648674538,26.7105487987841,-18.2120837246081));
#33321=CARTESIAN_POINT('Ctrl Pts',(-24.1943149096219,26.7079967193742,-18.2112728658593));
#33322=CARTESIAN_POINT('Ctrl Pts',(-24.2010406985633,26.7066174444027,-18.2108407851845));
#33323=CARTESIAN_POINT('Ctrl Pts',(-24.2092195258783,26.7049129381032,-18.2103141802302));
#33324=CARTESIAN_POINT('Ctrl Pts',(-24.2106768521019,26.7046081705198,-18.2102203027552));
#33325=CARTESIAN_POINT('Ctrl Pts',(-24.2149499291643,26.7037114597849,-18.2099449076427));
#33326=CARTESIAN_POINT('Ctrl Pts',(-24.2177650936578,26.7031167566321,-18.2097633030979));
#33327=CARTESIAN_POINT('Ctrl Pts',(-24.2273194597711,26.7010850279332,-18.2091463774524));
#33328=CARTESIAN_POINT('Ctrl Pts',(-24.2340548124942,26.6996301660918,-18.2087104965281));
#33329=CARTESIAN_POINT('Ctrl Pts',(-24.2459811299407,26.6970139739804,-18.2079369378518));
#33330=CARTESIAN_POINT('Ctrl Pts',(-24.2511739992196,26.6958613682946,-18.2075995342262));
#33331=CARTESIAN_POINT('Ctrl Pts',(-24.2602719986079,26.6938183353587,-18.2070073661085));
#33332=CARTESIAN_POINT('Ctrl Pts',(-24.264178377251,26.6929334719395,-18.2067527751499));
#33333=CARTESIAN_POINT('Ctrl Pts',(-24.2723344098157,26.6910699955193,-18.2062205226688));
#33334=CARTESIAN_POINT('Ctrl Pts',(-24.2765837448691,26.6900900351729,-18.2059428199444));
#33335=CARTESIAN_POINT('Ctrl Pts',(-24.300816488232,26.6844497758177,-18.2043568947711));
#33336=CARTESIAN_POINT('Ctrl Pts',(-24.3207566627785,26.6796074127548,-18.203043097133));
#33337=CARTESIAN_POINT('Ctrl Pts',(-24.5746786807103,26.6153697946659,-18.1862000724388));
#33338=CARTESIAN_POINT('Ctrl Pts',(-24.8012843420482,26.5300641932563,-18.1698556441782));
#33339=CARTESIAN_POINT('Ctrl Pts',(-25.1804817650056,26.3363786438452,-18.1410641612364));
#33340=CARTESIAN_POINT('Ctrl Pts',(-25.3372774926578,26.238506057559,-18.1286851923449));
#33341=CARTESIAN_POINT('Ctrl Pts',(-25.4894785670449,26.124267566502,-18.1167655817952));
#33342=CARTESIAN_POINT('Ctrl Pts',(-25.4940950675145,26.1207830630774,-18.1164041559895));
#33343=CARTESIAN_POINT('Ctrl Pts',(-25.5007436745224,26.1157365860001,-18.1158838332921));
#33344=CARTESIAN_POINT('Ctrl Pts',(-25.5027833036801,26.1141846126407,-18.1157242379033));
#33345=CARTESIAN_POINT('Ctrl Pts',(-25.5063297218303,26.1114794230485,-18.1154467903434));
#33346=CARTESIAN_POINT('Ctrl Pts',(-25.5078373455214,26.1103273078513,-18.1153288599357));
#33347=CARTESIAN_POINT('Ctrl Pts',(-25.5107552607203,26.1080933733398,-18.115100644484));
#33348=CARTESIAN_POINT('Ctrl Pts',(-25.5121656711627,26.1070117215532,-18.1149903479462));
#33349=CARTESIAN_POINT('Ctrl Pts',(-25.5155323339002,26.1044253826419,-18.1147271011635));
#33350=CARTESIAN_POINT('Ctrl Pts',(-25.5174877575603,26.1029196113746,-18.1145742281793));
#33351=CARTESIAN_POINT('Ctrl Pts',(-25.524471524388,26.097528980691,-18.1140283295035));
#33352=CARTESIAN_POINT('Ctrl Pts',(-25.5294901482737,26.0936314648209,-18.1136361974022));
#33353=CARTESIAN_POINT('Ctrl Pts',(-25.6025391879921,26.0365536617826,-18.1079302485563));
#33354=CARTESIAN_POINT('Ctrl Pts',(-25.6684241479758,25.9806693583862,-18.1028061023772));
#33355=CARTESIAN_POINT('Ctrl Pts',(-25.8454757772924,25.8178157032674,-18.0888440465991));
#33356=CARTESIAN_POINT('Ctrl Pts',(-25.9513310879628,25.7054139877674,-18.0802618742853));
#33357=CARTESIAN_POINT('Ctrl Pts',(-26.144654827345,25.4681300964519,-18.0631590269419));
#33358=CARTESIAN_POINT('Ctrl Pts',(-26.2321269517698,25.3437750580544,-18.0546585686911));
#33359=CARTESIAN_POINT('Ctrl Pts',(-26.3499531767997,25.1482623858747,-18.0414607052276));
#33360=CARTESIAN_POINT('Ctrl Pts',(-26.3870603130505,25.0814218582283,-18.0369777477752));
#33361=CARTESIAN_POINT('Ctrl Pts',(-26.4416124099945,24.9743553693789,-18.0297985849056));
#33362=CARTESIAN_POINT('Ctrl Pts',(-26.4606738134305,24.9349830161767,-18.0271590784457));
#33363=CARTESIAN_POINT('Ctrl Pts',(-26.4821224871873,24.8882789666404,-18.0240244761523));
#33364=CARTESIAN_POINT('Ctrl Pts',(-26.4852928131585,24.8813102769195,-18.0235566739027));
#33365=CARTESIAN_POINT('Ctrl Pts',(-26.4901085988584,24.8706238414046,-18.0228391415516));
#33366=CARTESIAN_POINT('Ctrl Pts',(-26.491771920128,24.8669141352873,-18.0225900266542));
#33367=CARTESIAN_POINT('Ctrl Pts',(-26.4947904090256,24.8601477303123,-18.0221355898311));
#33368=CARTESIAN_POINT('Ctrl Pts',(-26.4961478496797,24.8570920466073,-18.0219303463571));
#33369=CARTESIAN_POINT('Ctrl Pts',(-26.4988657972233,24.8509480232269,-18.0215176204885));
#33370=CARTESIAN_POINT('Ctrl Pts',(-26.5002262133418,24.847859648196,-18.0213101352958));
#33371=CARTESIAN_POINT('Ctrl Pts',(-26.5040792661313,24.8390751898206,-18.0207199033599));
#33372=CARTESIAN_POINT('Ctrl Pts',(-26.506560263094,24.8333740448697,-18.0203367585644));
#33373=CARTESIAN_POINT('Ctrl Pts',(-26.5169876633755,24.8092218749029,-18.0187132379315));
#33374=CARTESIAN_POINT('Ctrl Pts',(-26.5247778118972,24.7907042545325,-18.0174675419625));
#33375=CARTESIAN_POINT('Ctrl Pts',(-26.6616749743222,24.4565859505783,-17.9949707901166));
#33376=CARTESIAN_POINT('Ctrl Pts',(-26.740031370464,24.1225972304051,-17.9718102504194));
#33377=CARTESIAN_POINT('Ctrl Pts',(-26.7702366830597,23.7048670766068,-17.9435926650705));
#33378=CARTESIAN_POINT('Ctrl Pts',(-26.77303610225,23.6268743742366,-17.9383726663722));
#33379=CARTESIAN_POINT('Ctrl Pts',(-26.7729984130383,23.540066620556,-17.93266390827));
#33380=CARTESIAN_POINT('Ctrl Pts',(-26.7729586632714,23.5312798995657,-17.932087226881));
#33381=CARTESIAN_POINT('Ctrl Pts',(-26.7728346119646,23.5168784717514,-17.9311440606414));
#33382=CARTESIAN_POINT('Ctrl Pts',(-26.7727715714455,23.5112636722634,-17.9307768427314));
#33383=CARTESIAN_POINT('Ctrl Pts',(-26.7726105908347,23.4996334059842,-17.9300172787948));
#33384=CARTESIAN_POINT('Ctrl Pts',(-26.7725104801115,23.4936179836301,-17.9296250125336));
#33385=CARTESIAN_POINT('Ctrl Pts',(-26.7723805932278,23.486937761939,-17.9291900815134));
#33386=CARTESIAN_POINT('Ctrl Pts',(-26.7723674558826,23.4862726886051,-17.9291467879639));
#33387=CARTESIAN_POINT('Ctrl Pts',(-26.7722800001526,23.4819136256339,-17.9288630805769));
#33388=CARTESIAN_POINT('Ctrl Pts',(-26.7721995349435,23.4782197470498,-17.9286229005753));
#33389=CARTESIAN_POINT('Ctrl Pts',(-26.7708675209552,23.4215478951566,-17.924941707468));
#33390=CARTESIAN_POINT('Ctrl Pts',(-26.7683157127863,23.3686045912169,-17.9215518572488));
#33391=CARTESIAN_POINT('Ctrl Pts',(-26.7640404577051,23.310007193485,-17.917872014338));
#33392=CARTESIAN_POINT('Ctrl Pts',(-26.7636064901182,23.3042708352119,-17.9175125458878));
#33393=CARTESIAN_POINT('Ctrl Pts',(-26.762977359392,23.2962406357882,-17.9170104382764));
#33394=CARTESIAN_POINT('Ctrl Pts',(-26.7627950981227,23.2939458389715,-17.9168670768707));
#33395=CARTESIAN_POINT('Ctrl Pts',(-26.7624572316607,23.2897488454673,-17.9166051142168));
#33396=CARTESIAN_POINT('Ctrl Pts',(-26.7623023953219,23.2878465892089,-17.9164864693392));
#33397=CARTESIAN_POINT('Ctrl Pts',(-26.761984594664,23.2839846495293,-17.916245777536));
#33398=CARTESIAN_POINT('Ctrl Pts',(-26.7618215264956,23.2820249770673,-17.9161237366613));
#33399=CARTESIAN_POINT('Ctrl Pts',(-26.7614120981776,23.2771585719892,-17.915820906119));
#33400=CARTESIAN_POINT('Ctrl Pts',(-26.7611635842041,23.2742520148904,-17.9156402388072));
#33401=CARTESIAN_POINT('Ctrl Pts',(-26.7602215564562,23.2634077828197,-17.9149669261762));
#33402=CARTESIAN_POINT('Ctrl Pts',(-26.7595025449506,23.2554722652478,-17.9144757115415));
#33403=CARTESIAN_POINT('Ctrl Pts',(-26.7468016128444,23.1208531956469,-17.9061668717925));
#33404=CARTESIAN_POINT('Ctrl Pts',(-26.7273546650133,22.9949683280943,-17.8987592711115));
#33405=CARTESIAN_POINT('Ctrl Pts',(-26.624848631325,22.5198786645754,-17.8710877456227));
#33406=CARTESIAN_POINT('Ctrl Pts',(-26.4911833219502,22.1843281864495,-17.8518211454671));
#33407=CARTESIAN_POINT('Ctrl Pts',(-26.3004775288236,21.8702359567385,-17.8296770502588));
#33408=CARTESIAN_POINT('Ctrl Pts',(-26.2959330104918,21.8628189972855,-17.829151775918));
#33409=CARTESIAN_POINT('Ctrl Pts',(-26.281189611876,21.8389740262555,-17.8274553279706));
#33410=CARTESIAN_POINT('Ctrl Pts',(-26.2708730349854,21.8226196103841,-17.8262799098585));
#33411=CARTESIAN_POINT('Ctrl Pts',(-26.2570960450433,21.8012090030495,-17.8247249961102));
#33412=CARTESIAN_POINT('Ctrl Pts',(-26.2537673524116,21.7960681958284,-17.8243504191986));
#33413=CARTESIAN_POINT('Ctrl Pts',(-26.2485920153734,21.7881251652126,-17.8237697378153));
#33414=CARTESIAN_POINT('Ctrl Pts',(-26.2467556011114,21.7853162661671,-17.8235640170239));
#33415=CARTESIAN_POINT('Ctrl Pts',(-26.2432633238885,21.7799928048318,-17.8231734196512));
#33416=CARTESIAN_POINT('Ctrl Pts',(-26.2416083169426,21.7774776828937,-17.8229885753775));
#33417=CARTESIAN_POINT('Ctrl Pts',(-26.2377722925888,21.7716658110838,-17.8225607398063));
#33418=CARTESIAN_POINT('Ctrl Pts',(-26.2355887327341,21.768370752481,-17.822317652915));
#33419=CARTESIAN_POINT('Ctrl Pts',(-26.2294474433035,21.7591402848179,-17.8216352148396));
#33420=CARTESIAN_POINT('Ctrl Pts',(-26.2254760779039,21.753214014634,-17.8211953489767));
#33421=CARTESIAN_POINT('Ctrl Pts',(-26.2023311417576,21.7189227391416,-17.8186401020144));
#33422=CARTESIAN_POINT('Ctrl Pts',(-26.182726811209,21.6908524174493,-17.8165083994494));
#33423=CARTESIAN_POINT('Ctrl Pts',(-26.124822155427,21.6106936942847,-17.8103016261583));
#33424=CARTESIAN_POINT('Ctrl Pts',(-26.0853987012908,21.5594410967762,-17.8061836435481));
#33425=CARTESIAN_POINT('Ctrl Pts',(-25.9941686199034,21.4479444134286,-17.7968809963556));
#33426=CARTESIAN_POINT('Ctrl Pts',(-25.9416227292213,21.3883616194807,-17.791670534089));
#33427=CARTESIAN_POINT('Ctrl Pts',(-25.6939991327186,21.1276608468566,-17.7677933779304));
#33428=CARTESIAN_POINT('Ctrl Pts',(-25.4754210128618,20.9505766118356,-17.7483776422649));
#33429=CARTESIAN_POINT('Ctrl Pts',(-25.2309597035605,20.8004549906187,-17.7297135635187));
#33430=CARTESIAN_POINT('Ctrl Pts',(-25.2251972307697,20.7969411851593,-17.7292752696607));
#33431=CARTESIAN_POINT('Ctrl Pts',(-25.1768645579165,20.7676770751543,-17.7256132031939));
#33432=CARTESIAN_POINT('Ctrl Pts',(-25.1337113701679,20.7428958306231,-17.7224349727554));
#33433=CARTESIAN_POINT('Ctrl Pts',(-25.0850936303776,20.7164544546487,-17.7189691218883));
#33434=CARTESIAN_POINT('Ctrl Pts',(-25.0801815192066,20.7137994589362,-17.7186202327174));
#33435=CARTESIAN_POINT('Ctrl Pts',(-25.0732261236062,20.7100633929081,-17.7181280570423));
#33436=CARTESIAN_POINT('Ctrl Pts',(-25.0711885741907,20.7089717535138,-17.7179840993204));
#33437=CARTESIAN_POINT('Ctrl Pts',(-25.0674643593718,20.7069816187229,-17.717721383831));
#33438=CARTESIAN_POINT('Ctrl Pts',(-25.0657780672334,20.7060824302802,-17.7176025815439));
#33439=CARTESIAN_POINT('Ctrl Pts',(-25.0623578205465,20.7042625436278,-17.7173619306523));
#33440=CARTESIAN_POINT('Ctrl Pts',(-25.0606238236938,20.703341929462,-17.7172400875017));
#33441=CARTESIAN_POINT('Ctrl Pts',(-25.0563768262911,20.7010920845256,-17.7169420566286));
#33442=CARTESIAN_POINT('Ctrl Pts',(-25.0538629000821,20.6997645901814,-17.7167659803341));
#33443=CARTESIAN_POINT('Ctrl Pts',(-25.044699539618,20.6949413160418,-17.7161253906069));
#33444=CARTESIAN_POINT('Ctrl Pts',(-25.0380395770449,20.6914654273294,-17.7156621359239));
#33445=CARTESIAN_POINT('Ctrl Pts',(-24.8896497576756,20.6146785764687,-17.7053907428935));
#33446=CARTESIAN_POINT('Ctrl Pts',(-24.7426582163145,20.5519590711582,-17.6962308940142));
#33447=CARTESIAN_POINT('Ctrl Pts',(-24.3366523796988,20.4133318871669,-17.6720439822094));
#33448=CARTESIAN_POINT('Ctrl Pts',(-24.0718103769255,20.3585963144676,-17.6573243651315));
#33449=CARTESIAN_POINT('Ctrl Pts',(-23.7931436461296,20.3366526583845,-17.6409112173878));
#33450=CARTESIAN_POINT('Ctrl Pts',(-23.7830383483094,20.3359048529803,-17.6403149457771));
#33451=CARTESIAN_POINT('Ctrl Pts',(-23.7037038974258,20.3304100742564,-17.6356247778303));
#33452=CARTESIAN_POINT('Ctrl Pts',(-23.6343456308052,20.3278528016023,-17.631470210821));
#33453=CARTESIAN_POINT('Ctrl Pts',(-23.5564528463312,20.3274972608486,-17.6267258576395));
#33454=CARTESIAN_POINT('Ctrl Pts',(-23.5479430519864,20.3274921242511,-17.6262064931044));
#33455=CARTESIAN_POINT('Ctrl Pts',(-23.5351179497119,20.3275351797913,-17.6254221537604));
#33456=CARTESIAN_POINT('Ctrl Pts',(-23.5308025488109,20.3275583352649,-17.6251579646609));
#33457=CARTESIAN_POINT('Ctrl Pts',(-23.5233242313344,20.3276134836149,-17.624699662203));
#33458=CARTESIAN_POINT('Ctrl Pts',(-23.5201612832678,20.3276414654583,-17.6245056749394));
#33459=CARTESIAN_POINT('Ctrl Pts',(-23.5135899992366,20.3277092752619,-17.6241023395748));
#33460=CARTESIAN_POINT('Ctrl Pts',(-23.5101816768893,20.3277498540663,-17.6238929681766));
#33461=CARTESIAN_POINT('Ctrl Pts',(-23.5021733516143,20.3278579066417,-17.6234006098322));
#33462=CARTESIAN_POINT('Ctrl Pts',(-23.4975734250476,20.3279298230729,-17.6231174837589));
#33463=CARTESIAN_POINT('Ctrl Pts',(-23.4828573222579,20.3281914178381,-17.6222106762619));
#33464=CARTESIAN_POINT('Ctrl Pts',(-23.4727419542397,20.3284188857227,-17.6215858096862));
#33465=CARTESIAN_POINT('Ctrl Pts',(-23.2491595853086,20.3345002027843,-17.6077391870997));
#33466=CARTESIAN_POINT('Ctrl Pts',(-23.0368413899666,20.3615072999008,-17.5938286696543));
#33467=CARTESIAN_POINT('Ctrl Pts',(-22.5856794462837,20.465137172929,-17.5627797848461));
#33468=CARTESIAN_POINT('Ctrl Pts',(-22.3498759310134,20.5490129724615,-17.5455846795741));
#33469=CARTESIAN_POINT('Ctrl Pts',(-22.1251251987002,20.6597282129364,-17.5293710257841));
#33470=CARTESIAN_POINT('Ctrl Pts',(-22.1241468316802,20.6602107871911,-17.5293004507838));
#33471=CARTESIAN_POINT('Ctrl Pts',(-22.1204316023287,20.6620456499874,-17.5290324702955));
#33472=CARTESIAN_POINT('Ctrl Pts',(-22.1176964077432,20.6634013347216,-17.5288352201083));
#33473=CARTESIAN_POINT('Ctrl Pts',(-22.1136045082945,20.6654367105488,-17.5285401948741));
#33474=CARTESIAN_POINT('Ctrl Pts',(-22.1122463582643,20.6661134729342,-17.5284422831528));
#33475=CARTESIAN_POINT('Ctrl Pts',(-22.1085530970545,20.6679570720138,-17.52817605864));
#33476=CARTESIAN_POINT('Ctrl Pts',(-22.1062189195616,20.6691257896266,-17.5280078347616));
#33477=CARTESIAN_POINT('Ctrl Pts',(-22.0686854646964,20.6879757798333,-17.5253033586762));
#33478=CARTESIAN_POINT('Ctrl Pts',(-22.0338098159976,20.7062991179851,-17.5227982288467));
#33479=CARTESIAN_POINT('Ctrl Pts',(-21.9950911342815,20.7275564103991,-17.5200332547236));
#33480=CARTESIAN_POINT('Ctrl Pts',(-21.9909103631002,20.7298638409071,-17.5197349127339));
#33481=CARTESIAN_POINT('Ctrl Pts',(-21.9846263647103,20.7333503180641,-17.5192868249005));
#33482=CARTESIAN_POINT('Ctrl Pts',(-21.9825193302346,20.7345224336497,-17.5191366382788));
#33483=CARTESIAN_POINT('Ctrl Pts',(-21.9788743474002,20.7365554494167,-17.5188769317378));
#33484=CARTESIAN_POINT('Ctrl Pts',(-21.9773357901874,20.7374152464581,-17.5187673407121));
#33485=CARTESIAN_POINT('Ctrl Pts',(-21.9741335248613,20.7392082279637,-17.5185393117267));
#33486=CARTESIAN_POINT('Ctrl Pts',(-21.9724699417812,20.7401416263702,-17.5184208884038));
#33487=CARTESIAN_POINT('Ctrl Pts',(-21.9685682311875,20.7423353438793,-17.518143229893));
#33488=CARTESIAN_POINT('Ctrl Pts',(-21.9663307735301,20.7435968662767,-17.5179840726572));
#33489=CARTESIAN_POINT('Ctrl Pts',(-21.9589987694759,20.7477423536151,-17.517462738449));
#33490=CARTESIAN_POINT('Ctrl Pts',(-21.9539105347606,20.7506375467164,-17.517101283876));
#33491=CARTESIAN_POINT('Ctrl Pts',(-21.941921902915,20.7575023597134,-17.516250376214));
#33492=CARTESIAN_POINT('Ctrl Pts',(-21.9350282322035,20.7614837352554,-17.515761664554));
#33493=CARTESIAN_POINT('Ctrl Pts',(-21.6937703901942,20.9020146471463,-17.4986758783388));
#33494=CARTESIAN_POINT('Ctrl Pts',(-21.4775192327476,21.0676083704097,-17.4838872958859));
#33495=CARTESIAN_POINT('Ctrl Pts',(-21.1775862598352,21.3641154601481,-17.4602493636112));
#33496=CARTESIAN_POINT('Ctrl Pts',(-21.078163242266,21.4772091025496,-17.4517329920023));
#33497=CARTESIAN_POINT('Ctrl Pts',(-20.9784172347789,21.6080935329503,-17.4420773547995));
#33498=CARTESIAN_POINT('Ctrl Pts',(-20.9699023745134,21.6194207346154,-17.4412433658083));
#33499=CARTESIAN_POINT('Ctrl Pts',(-20.9569341314748,21.6369112011389,-17.4399578454422));
#33500=CARTESIAN_POINT('Ctrl Pts',(-20.9524273320497,21.6430347667681,-17.4395081935723));
#33501=CARTESIAN_POINT('Ctrl Pts',(-20.9455429478767,21.6524585254603,-17.4388168143472));
#33502=CARTESIAN_POINT('Ctrl Pts',(-20.9431498521397,21.6557473920403,-17.4385756373674));
#33503=CARTESIAN_POINT('Ctrl Pts',(-20.9372203180953,21.6639289491493,-17.4379759428479));
#33504=CARTESIAN_POINT('Ctrl Pts',(-20.9336913988822,21.6688270495339,-17.43761715932));
#33505=CARTESIAN_POINT('Ctrl Pts',(-20.9261380232371,21.6793734046566,-17.4368451313633));
#33506=CARTESIAN_POINT('Ctrl Pts',(-20.922118000637,21.6850247849946,-17.4364317305295));
#33507=CARTESIAN_POINT('Ctrl Pts',(-20.9143089420797,21.6960781889489,-17.4356237178964));
#33508=CARTESIAN_POINT('Ctrl Pts',(-20.9105181908848,21.7014789625608,-17.4352291708948));
#33509=CARTESIAN_POINT('Ctrl Pts',(-20.9039556380263,21.7108901207165,-17.4345420660109));
#33510=CARTESIAN_POINT('Ctrl Pts',(-20.9011762914153,21.7148952364636,-17.4342497844195));
#33511=CARTESIAN_POINT('Ctrl Pts',(-20.8916725354774,21.7286569740134,-17.43324592072));
#33512=CARTESIAN_POINT('Ctrl Pts',(-20.8849929121193,21.7384442839333,-17.4325327102821));
#33513=CARTESIAN_POINT('Ctrl Pts',(-20.8756716281177,21.7522653797618,-17.4315264790985));
#33514=CARTESIAN_POINT('Ctrl Pts',(-20.8729847576868,21.7562686760909,-17.4312351315986));
#33515=CARTESIAN_POINT('Ctrl Pts',(-20.8593407233764,21.7766964916836,-17.4297489865336));
#33516=CARTESIAN_POINT('Ctrl Pts',(-20.848525862262,21.7932151490841,-17.4285489684857));
#33517=CARTESIAN_POINT('Ctrl Pts',(-20.8345287765827,21.8150291507777,-17.4269661365636));
#33518=CARTESIAN_POINT('Ctrl Pts',(-20.8312088649958,21.8202359902979,-17.4265884654841));
#33519=CARTESIAN_POINT('Ctrl Pts',(-20.8261023883533,21.8282958277458,-17.4260040581387));
#33520=CARTESIAN_POINT('Ctrl Pts',(-20.8243052812225,21.8311421567484,-17.4257977136756));
#33521=CARTESIAN_POINT('Ctrl Pts',(-20.8207316250555,21.8368219473462,-17.4253860323648));
#33522=CARTESIAN_POINT('Ctrl Pts',(-20.818955020483,21.8396553692171,-17.4251806979121));
#33523=CARTESIAN_POINT('Ctrl Pts',(-20.8150209574246,21.845951372347,-17.4247245140569));
#33524=CARTESIAN_POINT('Ctrl Pts',(-20.8128656596926,21.8494152909852,-17.4244735851987));
#33525=CARTESIAN_POINT('Ctrl Pts',(-20.8066495575367,21.8594480125048,-17.42374695506));
#33526=CARTESIAN_POINT('Ctrl Pts',(-20.8026058003689,21.8660272973236,-17.4232706262943));
#33527=CARTESIAN_POINT('Ctrl Pts',(-20.7786683636123,21.9052897029333,-17.4204291035387));
#33528=CARTESIAN_POINT('Ctrl Pts',(-20.7593350587508,21.9383093055352,-17.4180434764323));
#33529=CARTESIAN_POINT('Ctrl Pts',(-20.70332229656,22.0380038755256,-17.4108491971482));
#33530=CARTESIAN_POINT('Ctrl Pts',(-20.6684137181855,22.1056379574815,-17.4059790169273));
#33531=CARTESIAN_POINT('Ctrl Pts',(-20.5290299739496,22.4008879412209,-17.3847574894445));
#33532=CARTESIAN_POINT('Ctrl Pts',(-20.4488944814781,22.6390052990426,-17.3676497595669));
#33533=CARTESIAN_POINT('Ctrl Pts',(-20.367363341557,23.024830474815,-17.3411145481398));
#33534=CARTESIAN_POINT('Ctrl Pts',(-20.3470638832927,23.1675705633021,-17.3315638048573));
#33535=CARTESIAN_POINT('Ctrl Pts',(-20.3356944587533,23.3204276908054,-17.3219255173698));
#33536=CARTESIAN_POINT('Ctrl Pts',(-20.3350482762301,23.3296518462194,-17.3213461888227));
#33537=CARTESIAN_POINT('Ctrl Pts',(-20.3342315252711,23.3420777817474,-17.3205689744489));
#33538=CARTESIAN_POINT('Ctrl Pts',(-20.3340260293567,23.3452771035423,-17.3203691499387));
#33539=CARTESIAN_POINT('Ctrl Pts',(-20.3337109223972,23.3503000976843,-17.3200558762167));
#33540=CARTESIAN_POINT('Ctrl Pts',(-20.3335980882279,23.3521235545747,-17.3199422449907));
#33541=CARTESIAN_POINT('Ctrl Pts',(-20.3333839677419,23.3556322475165,-17.3197237781004));
#33542=CARTESIAN_POINT('Ctrl Pts',(-20.3332824557748,23.3573174560571,-17.3196189305044));
#33543=CARTESIAN_POINT('Ctrl Pts',(-20.3330446243956,23.3613180895402,-17.3193702169233));
#33544=CARTESIAN_POINT('Ctrl Pts',(-20.3329094804741,23.3636335801801,-17.3192264182362));
#33545=CARTESIAN_POINT('Ctrl Pts',(-20.3325228812875,23.3703826369332,-17.3188077200045));
#33546=CARTESIAN_POINT('Ctrl Pts',(-20.3322780884589,23.3748166020971,-17.3185331960443));
#33547=CARTESIAN_POINT('Ctrl Pts',(-20.3305228783936,23.4078492752377,-17.3164920219037));
#33548=CARTESIAN_POINT('Ctrl Pts',(-20.329384502001,23.4364676448994,-17.3147459860348));
#33549=CARTESIAN_POINT('Ctrl Pts',(-20.3268609144045,23.5319423870339,-17.3089842438403));
#33550=CARTESIAN_POINT('Ctrl Pts',(-20.3271747612635,23.5988299816057,-17.3050509569519));
#33551=CARTESIAN_POINT('Ctrl Pts',(-20.3362243331168,23.85136817129,-17.2904304812832));
#33552=CARTESIAN_POINT('Ctrl Pts',(-20.3589282845446,24.0361607395012,-17.2801853618862));
#33553=CARTESIAN_POINT('Ctrl Pts',(-20.4286585349257,24.3654087878855,-17.2613224123456));
#33554=CARTESIAN_POINT('Ctrl Pts',(-20.4701832453469,24.5104587224931,-17.2527888340894));
#33555=CARTESIAN_POINT('Ctrl Pts',(-20.5261481902739,24.6642901584963,-17.2431821416407));
#33556=CARTESIAN_POINT('Ctrl Pts',(-20.530671131705,24.676491877446,-17.2424163273379));
#33557=CARTESIAN_POINT('Ctrl Pts',(-20.5411591738803,24.7042685111507,-17.2406639440555));
#33558=CARTESIAN_POINT('Ctrl Pts',(-20.5471714934166,24.7198250945627,-17.2396759778056));
#33559=CARTESIAN_POINT('Ctrl Pts',(-20.555848407541,24.7417681098752,-17.2382727989229));
#33560=CARTESIAN_POINT('Ctrl Pts',(-20.558413299277,24.748193865019,-17.2378607204718));
#33561=CARTESIAN_POINT('Ctrl Pts',(-20.5618042222262,24.7566102351161,-17.2373194215051));
#33562=CARTESIAN_POINT('Ctrl Pts',(-20.5626115989688,24.7586083832702,-17.2371907947248));
#33563=CARTESIAN_POINT('Ctrl Pts',(-20.5648144138758,24.7640443478743,-17.2368405486044));
#33564=CARTESIAN_POINT('Ctrl Pts',(-20.5662137826276,24.7674805597356,-17.2366188039469));
#33565=CARTESIAN_POINT('Ctrl Pts',(-20.5687829468273,24.7737581995025,-17.2362130610085));
#33566=CARTESIAN_POINT('Ctrl Pts',(-20.5699508795061,24.7766003887535,-17.2360291228707));
#33567=CARTESIAN_POINT('Ctrl Pts',(-20.5734397759833,24.7850562733642,-17.2354811673729));
#33568=CARTESIAN_POINT('Ctrl Pts',(-20.5757725397995,24.7906650598765,-17.2351167687178));
#33569=CARTESIAN_POINT('Ctrl Pts',(-20.583218490467,24.808425961502,-17.233959839686));
#33570=CARTESIAN_POINT('Ctrl Pts',(-20.5883903498938,24.82055320062,-17.2331653943517));
#33571=CARTESIAN_POINT('Ctrl Pts',(-20.6020491859439,24.8520442098543,-17.2310904677951));
#33572=CARTESIAN_POINT('Ctrl Pts',(-20.610652450546,24.8713565665989,-17.2298061221463));
#33573=CARTESIAN_POINT('Ctrl Pts',(-20.6220830521878,24.8963510784387,-17.2281279285943));
#33574=CARTESIAN_POINT('Ctrl Pts',(-20.6247381621318,24.9021117961281,-17.2277400297952));
#33575=CARTESIAN_POINT('Ctrl Pts',(-20.6290016776327,24.9112908419168,-17.2271201701073));
#33576=CARTESIAN_POINT('Ctrl Pts',(-20.6305991259422,24.9147142659822,-17.2268885888975));
#33577=CARTESIAN_POINT('Ctrl Pts',(-20.6334838144629,24.9208680593313,-17.2264715894135));
#33578=CARTESIAN_POINT('Ctrl Pts',(-20.6347688802546,24.9235994479928,-17.226286246774));
#33579=CARTESIAN_POINT('Ctrl Pts',(-20.6377868515448,24.9299907759293,-17.2258519524374));
#33580=CARTESIAN_POINT('Ctrl Pts',(-20.6395228187341,24.9336492566099,-17.2256028945295));
#33581=CARTESIAN_POINT('Ctrl Pts',(-20.6445283297067,24.944147036498,-17.2248869044704));
#33582=CARTESIAN_POINT('Ctrl Pts',(-20.6478150992536,24.9509780500352,-17.2244193729758));
#33583=CARTESIAN_POINT('Ctrl Pts',(-20.6691922366224,24.9950086391638,-17.2213951919681));
#33584=CARTESIAN_POINT('Ctrl Pts',(-20.687972588244,25.0318671583642,-17.2188144875263));
#33585=CARTESIAN_POINT('Ctrl Pts',(-20.7362097283019,25.1221960822656,-17.2123635671191));
#33586=CARTESIAN_POINT('Ctrl Pts',(-20.7664852211094,25.1752085873638,-17.2084650994785));
#33587=CARTESIAN_POINT('Ctrl Pts',(-20.8659280990381,25.338390056095,-17.1961040905956));
#33588=CARTESIAN_POINT('Ctrl Pts',(-20.9402645650632,25.4452433490221,-17.1874717513421));
#33589=CARTESIAN_POINT('Ctrl Pts',(-21.1034615225553,25.651943766477,-17.1697564257296));
#33590=CARTESIAN_POINT('Ctrl Pts',(-21.1924896728254,25.7513536056379,-17.1606844528849));
#33591=CARTESIAN_POINT('Ctrl Pts',(-21.3892756791728,25.9454060623534,-17.1420912907719));
#33592=CARTESIAN_POINT('Ctrl Pts',(-21.4977228114358,26.0389698830556,-17.1326063673031));
#33593=CARTESIAN_POINT('Ctrl Pts',(-21.6193935505197,26.1305598413619,-17.1230306726729));
#33594=CARTESIAN_POINT('Ctrl Pts',(-21.6267681916344,26.1360619245084,-17.1224542279697));
#33595=CARTESIAN_POINT('Ctrl Pts',(-21.6367395298454,26.1434350928297,-17.1216802348175));
#33596=CARTESIAN_POINT('Ctrl Pts',(-21.6393155042683,26.1453339333167,-17.1214807683727));
#33597=CARTESIAN_POINT('Ctrl Pts',(-21.6433655873451,26.1483100902344,-17.1211679237028));
#33598=CARTESIAN_POINT('Ctrl Pts',(-21.6448377815073,26.1493899897421,-17.121054364309));
#33599=CARTESIAN_POINT('Ctrl Pts',(-21.6476732924421,26.1514662199852,-17.1208359506526));
#33600=CARTESIAN_POINT('Ctrl Pts',(-21.6490364655166,26.1524627237249,-17.120731084598));
#33601=CARTESIAN_POINT('Ctrl Pts',(-21.6522759710349,26.1548269554595,-17.1204821990784));
#33602=CARTESIAN_POINT('Ctrl Pts',(-21.6541529970658,26.1561937260822,-17.120338247187));
#33603=CARTESIAN_POINT('Ctrl Pts',(-21.6596336762357,26.1601754673729,-17.1199186689952));
#33604=CARTESIAN_POINT('Ctrl Pts',(-21.6632412919604,26.1627850134982,-17.1196434207054));
#33605=CARTESIAN_POINT('Ctrl Pts',(-21.6903411039546,26.1823020731279,-17.1175827151332));
#33606=CARTESIAN_POINT('Ctrl Pts',(-21.7140556801442,26.1989005965808,-17.1158183212167));
#33607=CARTESIAN_POINT('Ctrl Pts',(-21.7944481134526,26.2535708153226,-17.1099547007653));
#33608=CARTESIAN_POINT('Ctrl Pts',(-21.8521146139147,26.2901627286824,-17.1059416532585));
#33609=CARTESIAN_POINT('Ctrl Pts',(-21.9647388341749,26.3567046957881,-17.0983797782872));
#33610=CARTESIAN_POINT('Ctrl Pts',(-22.0194731270377,26.3869297398572,-17.0948230931305));
#33611=CARTESIAN_POINT('Ctrl Pts',(-22.0750360832114,26.4155368094973,-17.0912958973716));
#33612=CARTESIAN_POINT('Origin',(-23.5502525316942,23.5502525316942,-77.3107734492734));
#33613=CARTESIAN_POINT('',(-22.0750358970872,26.4155367136697,-15.5960174792939));
#33614=CARTESIAN_POINT('',(-22.0750360164986,26.4155367751497,-15.845717117064));
#33615=CARTESIAN_POINT('',(-22.0750360153461,26.4155367745563,-77.3107734492734));
#33616=CARTESIAN_POINT('Ctrl Pts',(-22.0750358970872,26.4155367136697,-15.5960174792939));
#33617=CARTESIAN_POINT('Ctrl Pts',(-22.010768538295,26.382448101605,-15.6000629323526));
#33618=CARTESIAN_POINT('Ctrl Pts',(-21.9476108572898,26.3471954248686,-15.6041236814064));
#33619=CARTESIAN_POINT('Ctrl Pts',(-21.7815274076261,26.2470138169797,-15.6151340211213));
#33620=CARTESIAN_POINT('Ctrl Pts',(-21.681032103164,26.1783546106423,-15.6221567777815));
#33621=CARTESIAN_POINT('Ctrl Pts',(-21.5573531351805,26.0831672900697,-15.6314417263071));
#33622=CARTESIAN_POINT('Ctrl Pts',(-21.5303829102972,26.0617126157181,-15.6335079648564));
#33623=CARTESIAN_POINT('Ctrl Pts',(-21.4873738060228,26.0263581465605,-15.6368739757199));
#33624=CARTESIAN_POINT('Ctrl Pts',(-21.4711186838194,26.0127248791463,-15.6381630142914));
#33625=CARTESIAN_POINT('Ctrl Pts',(-21.450343128026,25.9949479355673,-15.6398329156864));
#33626=CARTESIAN_POINT('Ctrl Pts',(-21.4456980090794,25.9909502560865,-15.6402077434834));
#33627=CARTESIAN_POINT('Ctrl Pts',(-21.438244431871,25.9844984639567,-15.6408115631217));
#33628=CARTESIAN_POINT('Ctrl Pts',(-21.4354287659736,25.9820526699072,-15.6410402091086));
#33629=CARTESIAN_POINT('Ctrl Pts',(-21.430082699872,25.9773925673824,-15.6414753807729));
#33630=CARTESIAN_POINT('Ctrl Pts',(-21.4275515054041,25.9751791741847,-15.6416818681135));
#33631=CARTESIAN_POINT('Ctrl Pts',(-21.4218007934832,25.9701345828742,-15.64215201569));
#33632=CARTESIAN_POINT('Ctrl Pts',(-21.4185834572788,25.9673009177249,-15.6424157789755));
#33633=CARTESIAN_POINT('Ctrl Pts',(-21.4088329865162,25.9586785913056,-15.6432173713615));
#33634=CARTESIAN_POINT('Ctrl Pts',(-21.4023177464113,25.9528698355637,-15.6437560441706));
#33635=CARTESIAN_POINT('Ctrl Pts',(-21.3565091238014,25.9116932525387,-15.6475651877568));
#33636=CARTESIAN_POINT('Ctrl Pts',(-21.318069610961,25.8753915145602,-15.6508751805944));
#33637=CARTESIAN_POINT('Ctrl Pts',(-21.2781649337681,25.8358042641474,-15.6544377548644));
#33638=CARTESIAN_POINT('Ctrl Pts',(-21.2757914964577,25.833442355915,-15.6546501362696));
#33639=CARTESIAN_POINT('Ctrl Pts',(-21.270526431938,25.8281865098886,-15.6551223542594));
#33640=CARTESIAN_POINT('Ctrl Pts',(-21.2676366290336,25.825290759856,-15.6553822685019));
#33641=CARTESIAN_POINT('Ctrl Pts',(-21.2611691643497,25.8187852579012,-15.6559656075945));
#33642=CARTESIAN_POINT('Ctrl Pts',(-21.2575945177382,25.8151725353809,-15.6562891594675));
#33643=CARTESIAN_POINT('Ctrl Pts',(-21.2401038824574,25.797411761369,-15.6578778644677));
#33644=CARTESIAN_POINT('Ctrl Pts',(-21.2263104660075,25.7831440724978,-15.6591481228983));
#33645=CARTESIAN_POINT('Ctrl Pts',(-21.1736817696435,25.7276898874861,-15.6640624482381));
#33646=CARTESIAN_POINT('Ctrl Pts',(-21.1358041340041,25.6856120726269,-15.6677439030843));
#33647=CARTESIAN_POINT('Ctrl Pts',(-21.0300368851294,25.5617028156594,-15.6784466643746));
#33648=CARTESIAN_POINT('Ctrl Pts',(-20.9650655598877,25.4774849240265,-15.685557778967));
#33649=CARTESIAN_POINT('Ctrl Pts',(-20.801508943067,25.2422899061871,-15.7048807677061));
#33650=CARTESIAN_POINT('Ctrl Pts',(-20.7112242492433,25.0859946485086,-15.7171836028927));
#33651=CARTESIAN_POINT('Ctrl Pts',(-20.6096552457239,24.8702526005743,-15.7329056498722));
#33652=CARTESIAN_POINT('Ctrl Pts',(-20.5862692555078,24.8168687464365,-15.7366984038022));
#33653=CARTESIAN_POINT('Ctrl Pts',(-20.55405410004,24.7375436213785,-15.7421629942875));
#33654=CARTESIAN_POINT('Ctrl Pts',(-20.5440883340895,24.7120795896661,-15.7438917807212));
#33655=CARTESIAN_POINT('Ctrl Pts',(-20.5329002022171,24.6823840354266,-15.7458759685245));
#33656=CARTESIAN_POINT('Ctrl Pts',(-20.531361316529,24.6782740977499,-15.7461498806865));
#33657=CARTESIAN_POINT('Ctrl Pts',(-20.5290258306396,24.6719976504383,-15.7465670946342));
#33658=CARTESIAN_POINT('Ctrl Pts',(-20.5282231626511,24.6698334279733,-15.7467107597736));
#33659=CARTESIAN_POINT('Ctrl Pts',(-20.5268379395623,24.6660861268393,-15.7469591692864));
#33660=CARTESIAN_POINT('Ctrl Pts',(-20.526254303247,24.6645034560227,-15.7470639789287));
#33661=CARTESIAN_POINT('Ctrl Pts',(-20.5250393873556,24.6612009329171,-15.7472824613604));
#33662=CARTESIAN_POINT('Ctrl Pts',(-20.5244083334255,24.6594810053201,-15.7473961202913));
#33663=CARTESIAN_POINT('Ctrl Pts',(-20.5226681805134,24.6547257104091,-15.7477100242254));
#33664=CARTESIAN_POINT('Ctrl Pts',(-20.5215621760857,24.651689200812,-15.7479100827855));
#33665=CARTESIAN_POINT('Ctrl Pts',(-20.5172485929353,24.6397907331625,-15.7486925146855));
#33666=CARTESIAN_POINT('Ctrl Pts',(-20.5140752852222,24.6309162713563,-15.7492728540497));
#33667=CARTESIAN_POINT('Ctrl Pts',(-20.4603225976594,24.4784858506931,-15.7591875811564));
#33668=CARTESIAN_POINT('Ctrl Pts',(-20.4199290283872,24.3315159038752,-15.76794053412));
#33669=CARTESIAN_POINT('Ctrl Pts',(-20.3446555373164,23.9551087271497,-15.7896078409666));
#33670=CARTESIAN_POINT('Ctrl Pts',(-20.3238532820834,23.7237700299913,-15.8022919399002));
#33671=CARTESIAN_POINT('Ctrl Pts',(-20.3295120627878,23.409686579751,-15.820422406692));
#33672=CARTESIAN_POINT('Ctrl Pts',(-20.3341672967765,23.3272680200889,-15.8252585636098));
#33673=CARTESIAN_POINT('Ctrl Pts',(-20.3459832019111,23.2030299629039,-15.8327199049889));
#33674=CARTESIAN_POINT('Ctrl Pts',(-20.3508144577647,23.1610209783441,-15.8352724468413));
#33675=CARTESIAN_POINT('Ctrl Pts',(-20.3574476667287,23.1118828273943,-15.8382967383826));
#33676=CARTESIAN_POINT('Ctrl Pts',(-20.3584493043332,23.104648380211,-15.838742976273));
#33677=CARTESIAN_POINT('Ctrl Pts',(-20.36006009167,23.0932984133447,-15.8394446316886));
#33678=CARTESIAN_POINT('Ctrl Pts',(-20.360652638206,23.0891805309549,-15.8396995224998));
#33679=CARTESIAN_POINT('Ctrl Pts',(-20.3616906898426,23.0820643951604,-15.8401405636022));
#33680=CARTESIAN_POINT('Ctrl Pts',(-20.3621324554379,23.0790655945103,-15.8403265950058));
#33681=CARTESIAN_POINT('Ctrl Pts',(-20.3630559980111,23.0728571482461,-15.8407120975768));
#33682=CARTESIAN_POINT('Ctrl Pts',(-20.3635383940179,23.0696475992777,-15.8409115882148));
#33683=CARTESIAN_POINT('Ctrl Pts',(-20.3647199623084,23.0618662066141,-15.8413957294315));
#33684=CARTESIAN_POINT('Ctrl Pts',(-20.3654241280295,23.0572951379912,-15.8416805384123));
#33685=CARTESIAN_POINT('Ctrl Pts',(-20.3680887344814,23.0402419664457,-15.8427445988345));
#33686=CARTESIAN_POINT('Ctrl Pts',(-20.3701127162663,23.0277700382262,-15.8435258679203));
#33687=CARTESIAN_POINT('Ctrl Pts',(-20.4038988980121,22.8270493759569,-15.8561497100863));
#33688=CARTESIAN_POINT('Ctrl Pts',(-20.4522468015887,22.6420120112111,-15.8685353144056));
#33689=CARTESIAN_POINT('Ctrl Pts',(-20.5813613610631,22.2819745304187,-15.8940801446763));
#33690=CARTESIAN_POINT('Ctrl Pts',(-20.6620103943619,22.1077210857707,-15.9071889968983));
#33691=CARTESIAN_POINT('Ctrl Pts',(-20.7919096143708,21.8822086118749,-15.9245945802106));
#33692=CARTESIAN_POINT('Ctrl Pts',(-20.8280523094128,21.8238536039231,-15.9291386908129));
#33693=CARTESIAN_POINT('Ctrl Pts',(-20.8871055226921,21.7349797084791,-15.9360748576416));
#33694=CARTESIAN_POINT('Ctrl Pts',(-20.9087398146202,21.7036398844754,-15.9385238354284));
#33695=CARTESIAN_POINT('Ctrl Pts',(-20.9422578632624,21.6568799505077,-15.9421737231464));
#33696=CARTESIAN_POINT('Ctrl Pts',(-20.9537334553779,21.6411730013783,-15.9433990280942));
#33697=CARTESIAN_POINT('Ctrl Pts',(-20.9677355741138,21.6223677658836,-15.9448642031369));
#33698=CARTESIAN_POINT('Ctrl Pts',(-20.9701262198227,21.6191694880023,-15.9451133266291));
#33699=CARTESIAN_POINT('Ctrl Pts',(-20.9736181469851,21.6145159430809,-15.9454757011331));
#33700=CARTESIAN_POINT('Ctrl Pts',(-20.974714718062,21.6130571715016,-15.9455892816566));
#33701=CARTESIAN_POINT('Ctrl Pts',(-20.9768360361437,21.6102401611601,-15.9458085849882));
#33702=CARTESIAN_POINT('Ctrl Pts',(-20.9778606208028,21.6088818009391,-15.9459143192462));
#33703=CARTESIAN_POINT('Ctrl Pts',(-20.9799648509826,21.6060966731937,-15.9461310837908));
#33704=CARTESIAN_POINT('Ctrl Pts',(-20.9810446066318,21.604669996412,-15.9462421057181));
#33705=CARTESIAN_POINT('Ctrl Pts',(-20.9836433314752,21.6012422476326,-15.9465088132865));
#33706=CARTESIAN_POINT('Ctrl Pts',(-20.9851634564067,21.5992420473637,-15.9466644169903));
#33707=CARTESIAN_POINT('Ctrl Pts',(-20.990701834886,21.5919722381826,-15.9472298690332));
#33708=CARTESIAN_POINT('Ctrl Pts',(-20.9947340366302,21.5867132016198,-15.9476387377724));
#33709=CARTESIAN_POINT('Ctrl Pts',(-21.0628267932135,21.4984676360012,-15.9544970809675));
#33710=CARTESIAN_POINT('Ctrl Pts',(-21.1308908243764,21.4186329001386,-15.9606666054038));
#33711=CARTESIAN_POINT('Ctrl Pts',(-21.3653305526648,21.1693797206497,-15.9803431369683));
#33712=CARTESIAN_POINT('Ctrl Pts',(-21.5465295370092,21.0149919761516,-15.9932609415746));
#33713=CARTESIAN_POINT('Ctrl Pts',(-21.8409155786779,20.8156124909234,-16.0134698080465));
#33714=CARTESIAN_POINT('Ctrl Pts',(-21.9423463705577,20.754769997483,-16.0203038930105));
#33715=CARTESIAN_POINT('Ctrl Pts',(-22.0923006039046,20.6756864330998,-16.0303942376606));
#33716=CARTESIAN_POINT('Ctrl Pts',(-22.1382823152275,20.6528237184469,-16.0334859214619));
#33717=CARTESIAN_POINT('Ctrl Pts',(-22.1919981881076,20.6276978186748,-16.0371017974909));
#33718=CARTESIAN_POINT('Ctrl Pts',(-22.1992201488088,20.6243522580917,-16.0375880242147));
#33719=CARTESIAN_POINT('Ctrl Pts',(-22.2102385444714,20.6192974978878,-16.0383300009811));
#33720=CARTESIAN_POINT('Ctrl Pts',(-22.2140260571149,20.6175688282371,-16.0385850784093));
#33721=CARTESIAN_POINT('Ctrl Pts',(-22.220577225028,20.6145941163198,-16.0390263303496));
#33722=CARTESIAN_POINT('Ctrl Pts',(-22.2233393148803,20.6133446223686,-16.039212385636));
#33723=CARTESIAN_POINT('Ctrl Pts',(-22.2290609536418,20.6107660285708,-16.0395978311382));
#33724=CARTESIAN_POINT('Ctrl Pts',(-22.2320207537833,20.6094374971269,-16.0397972406654));
#33725=CARTESIAN_POINT('Ctrl Pts',(-22.2392004843591,20.6062278310157,-16.0402810061358));
#33726=CARTESIAN_POINT('Ctrl Pts',(-22.2434224551925,20.6043513011993,-16.0405655199615));
#33727=CARTESIAN_POINT('Ctrl Pts',(-22.2591772031941,20.5973893575433,-16.0416273753202));
#33728=CARTESIAN_POINT('Ctrl Pts',(-22.2707356304771,20.5923625876015,-16.0424067237675));
#33729=CARTESIAN_POINT('Ctrl Pts',(-22.4681267831465,20.5078904893647,-16.0557225632843));
#33730=CARTESIAN_POINT('Ctrl Pts',(-22.6609609018353,20.4460464391205,-16.0688711497315));
#33731=CARTESIAN_POINT('Ctrl Pts',(-23.1468802572785,20.3392211500691,-16.1021862759221));
#33732=CARTESIAN_POINT('Ctrl Pts',(-23.442832925527,20.3157658377569,-16.1226991669451));
#33733=CARTESIAN_POINT('Ctrl Pts',(-23.7461048117153,20.3334485322113,-16.141857659537));
#33734=CARTESIAN_POINT('Ctrl Pts',(-23.754366928766,20.333962214715,-16.1423780630931));
#33735=CARTESIAN_POINT('Ctrl Pts',(-23.7686545929358,20.3349058020991,-16.1432752312063));
#33736=CARTESIAN_POINT('Ctrl Pts',(-23.7746810332003,20.335320821534,-16.143652799318));
#33737=CARTESIAN_POINT('Ctrl Pts',(-23.7833016107457,20.3359388476615,-16.1441916423399));
#33738=CARTESIAN_POINT('Ctrl Pts',(-23.785896677357,20.3361280522541,-16.1443536886514));
#33739=CARTESIAN_POINT('Ctrl Pts',(-23.7903999578517,20.3364618667089,-16.1446346060725));
#33740=CARTESIAN_POINT('Ctrl Pts',(-23.7923082747745,20.336605033609,-16.1447535590887));
#33741=CARTESIAN_POINT('Ctrl Pts',(-23.7959660444374,20.3368827255875,-16.1449813905479));
#33742=CARTESIAN_POINT('Ctrl Pts',(-23.7977155120714,20.3370169794008,-16.1450902843391));
#33743=CARTESIAN_POINT('Ctrl Pts',(-23.8018383681433,20.3373367536569,-16.1453467316237));
#33744=CARTESIAN_POINT('Ctrl Pts',(-23.8042116663202,20.3375234755974,-16.1454942168495));
#33745=CARTESIAN_POINT('Ctrl Pts',(-23.8112262394054,20.3380831764403,-16.1459297277339));
#33746=CARTESIAN_POINT('Ctrl Pts',(-23.8158669407877,20.3384635863751,-16.1462173356499));
#33747=CARTESIAN_POINT('Ctrl Pts',(-23.8564646428799,20.3418800741789,-16.1487289815435));
#33748=CARTESIAN_POINT('Ctrl Pts',(-23.8923709435871,20.3455099612613,-16.1509201766677));
#33749=CARTESIAN_POINT('Ctrl Pts',(-23.9335312281696,20.3503707044785,-16.153405012533));
#33750=CARTESIAN_POINT('Ctrl Pts',(-23.938850403698,20.351012315336,-16.153725610894));
#33751=CARTESIAN_POINT('Ctrl Pts',(-24.2412437156542,20.3882529662706,-16.1719232534179));
#33752=CARTESIAN_POINT('Ctrl Pts',(-24.5318136528108,20.4660505545078,-16.1879719027631));
#33753=CARTESIAN_POINT('Ctrl Pts',(-24.960353549938,20.6476173661421,-16.2143954608027));
#33754=CARTESIAN_POINT('Ctrl Pts',(-25.1079528844729,20.7240831302503,-16.2240469985579));
#33755=CARTESIAN_POINT('Ctrl Pts',(-25.2600807065299,20.8184444551972,-16.2349232932918));
#33756=CARTESIAN_POINT('Ctrl Pts',(-25.271124970129,20.8253881686354,-16.2357183467143));
#33757=CARTESIAN_POINT('Ctrl Pts',(-25.2864246415602,20.8351374436919,-16.2368274579456));
#33758=CARTESIAN_POINT('Ctrl Pts',(-25.2907161168922,20.837886397799,-16.2371394080807));
#33759=CARTESIAN_POINT('Ctrl Pts',(-25.2979466570163,20.8425422294161,-16.2376664454253));
#33760=CARTESIAN_POINT('Ctrl Pts',(-25.3008891757644,20.8444437474241,-16.2378813321513));
#33761=CARTESIAN_POINT('Ctrl Pts',(-25.3067032611842,20.8482143867174,-16.2383067291597));
#33762=CARTESIAN_POINT('Ctrl Pts',(-25.309574959735,20.8500832969837,-16.2385172313467));
#33763=CARTESIAN_POINT('Ctrl Pts',(-25.3158946897643,20.8542105584941,-16.2389813443974));
#33764=CARTESIAN_POINT('Ctrl Pts',(-25.3193413764872,20.8564709498664,-16.2392350316947));
#33765=CARTESIAN_POINT('Ctrl Pts',(-25.3313480136562,20.8643780735084,-16.2401207462866));
#33766=CARTESIAN_POINT('Ctrl Pts',(-25.3398852728665,20.8700589997226,-16.2407540605579));
#33767=CARTESIAN_POINT('Ctrl Pts',(-25.4263129262855,20.9281673853676,-16.2472017497701));
#33768=CARTESIAN_POINT('Ctrl Pts',(-25.5018967105281,20.9839292577078,-16.253142943193));
#33769=CARTESIAN_POINT('Ctrl Pts',(-25.8171293609277,21.2384794146637,-16.2793060483272));
#33770=CARTESIAN_POINT('Ctrl Pts',(-26.0296937018015,21.4681058460494,-16.3008083782085));
#33771=CARTESIAN_POINT('Ctrl Pts',(-26.259861311251,21.8029171853361,-16.3278215541238));
#33772=CARTESIAN_POINT('Ctrl Pts',(-26.3102439052869,21.8836355934166,-16.3340369780062));
#33773=CARTESIAN_POINT('Ctrl Pts',(-26.361313971744,21.9741406483432,-16.3405955626054));
#33774=CARTESIAN_POINT('Ctrl Pts',(-26.3656096393641,21.9818267447743,-16.3411494013173));
#33775=CARTESIAN_POINT('Ctrl Pts',(-26.3729687008238,21.9951217231519,-16.3421018557458));
#33776=CARTESIAN_POINT('Ctrl Pts',(-26.3760469847028,22.00072224346,-16.3425013893594));
#33777=CARTESIAN_POINT('Ctrl Pts',(-26.3803874956574,22.0086751659799,-16.3430663096522));
#33778=CARTESIAN_POINT('Ctrl Pts',(-26.381663464712,22.0110199900551,-16.3432325709968));
#33779=CARTESIAN_POINT('Ctrl Pts',(-26.3838503724448,22.0150507496727,-16.3435178584734));
#33780=CARTESIAN_POINT('Ctrl Pts',(-26.3847627220969,22.0167359145028,-16.3436369756159));
#33781=CARTESIAN_POINT('Ctrl Pts',(-26.386506143618,22.0199629906327,-16.3438647864181));
#33782=CARTESIAN_POINT('Ctrl Pts',(-26.3873374602829,22.0215047635375,-16.3439734959809));
#33783=CARTESIAN_POINT('Ctrl Pts',(-26.3892900573071,22.0251331586952,-16.3442290290336));
#33784=CARTESIAN_POINT('Ctrl Pts',(-26.3904102967319,22.0272203444061,-16.3443757854542));
#33785=CARTESIAN_POINT('Ctrl Pts',(-26.3937040272258,22.0333733637871,-16.3448077351599));
#33786=CARTESIAN_POINT('Ctrl Pts',(-26.3958711079054,22.0374426504409,-16.3450925202806));
#33787=CARTESIAN_POINT('Ctrl Pts',(-26.414361651163,22.0723440149388,-16.347527615613));
#33788=CARTESIAN_POINT('Ctrl Pts',(-26.4301930135577,22.1034361316098,-16.3496472474607));
#33789=CARTESIAN_POINT('Ctrl Pts',(-26.4478211484017,22.1394934480009,-16.3520557123517));
#33790=CARTESIAN_POINT('Ctrl Pts',(-26.45011366721,22.1442118223947,-16.3523699102967));
#33791=CARTESIAN_POINT('Ctrl Pts',(-26.455551299867,22.1554732185961,-16.3531175543574));
#33792=CARTESIAN_POINT('Ctrl Pts',(-26.4586858589235,22.1620213378661,-16.3535504740378));
#33793=CARTESIAN_POINT('Ctrl Pts',(-26.5894491268685,22.4375737887252,-16.3716946149772));
#33794=CARTESIAN_POINT('Ctrl Pts',(-26.6792235739005,22.7229917398335,-16.3876603733281));
#33795=CARTESIAN_POINT('Ctrl Pts',(-26.7393058296764,23.0808990059564,-16.4082902284006));
#33796=CARTESIAN_POINT('Ctrl Pts',(-26.7481336586921,23.1453953544504,-16.4120249039404));
#33797=CARTESIAN_POINT('Ctrl Pts',(-26.7641721297485,23.2965074438916,-16.4208646940189));
#33798=CARTESIAN_POINT('Ctrl Pts',(-26.7698437548746,23.3832313337948,-16.4260067265475));
#33799=CARTESIAN_POINT('Ctrl Pts',(-26.7725208419207,23.4908014556169,-16.4325142843219));
#33800=CARTESIAN_POINT('Ctrl Pts',(-26.7728366394631,23.5115339232404,-16.4337743854439));
#33801=CARTESIAN_POINT('Ctrl Pts',(-26.7729860115577,23.5382997794761,-16.4354092076705));
#33802=CARTESIAN_POINT('Ctrl Pts',(-26.7730027387142,23.5443319836837,-16.4357781717786));
#33803=CARTESIAN_POINT('Ctrl Pts',(-26.773002414159,23.5537014185231,-16.4363520874291));
#33804=CARTESIAN_POINT('Ctrl Pts',(-26.7729971148261,23.5570386577689,-16.4365566698283));
#33805=CARTESIAN_POINT('Ctrl Pts',(-26.7729761171642,23.5637231980577,-16.4369667804481));
#33806=CARTESIAN_POINT('Ctrl Pts',(-26.7729603873923,23.5670704948622,-16.4371723094054));
#33807=CARTESIAN_POINT('Ctrl Pts',(-26.7729135993226,23.5745478893007,-16.4376318042383));
#33808=CARTESIAN_POINT('Ctrl Pts',(-26.7728798163901,23.5786779584991,-16.4378858553278));
#33809=CARTESIAN_POINT('Ctrl Pts',(-26.772757656836,23.5907702554031,-16.4386304315405));
#33810=CARTESIAN_POINT('Ctrl Pts',(-26.7726477104821,23.598732191346,-16.4391216330619));
#33811=CARTESIAN_POINT('Ctrl Pts',(-26.7716183296428,23.6575002038599,-16.4427543688305));
#33812=CARTESIAN_POINT('Ctrl Pts',(-26.7695269415026,23.7082761538649,-16.4459325224983));
#33813=CARTESIAN_POINT('Ctrl Pts',(-26.7587256799193,23.8746980126637,-16.4564868790752));
#33814=CARTESIAN_POINT('Ctrl Pts',(-26.7449758354435,23.9899144930387,-16.464016600083));
#33815=CARTESIAN_POINT('Ctrl Pts',(-26.6808123863661,24.3576965711887,-16.4887339943904));
#33816=CARTESIAN_POINT('Ctrl Pts',(-26.6063627843755,24.6050253632018,-16.5064887308816));
#33817=CARTESIAN_POINT('Ctrl Pts',(-26.4680266309504,24.921554203162,-16.5293187768705));
#33818=CARTESIAN_POINT('Ctrl Pts',(-26.4294602260831,25.0007835899275,-16.535032637019));
#33819=CARTESIAN_POINT('Ctrl Pts',(-26.3846658489233,25.0839602755355,-16.5409548553504));
#33820=CARTESIAN_POINT('Ctrl Pts',(-26.3816229165237,25.0895705761438,-16.5413539259994));
#33821=CARTESIAN_POINT('Ctrl Pts',(-26.3773779963793,25.0973418255469,-16.5419061338582));
#33822=CARTESIAN_POINT('Ctrl Pts',(-26.3761901840895,25.099510438274,-16.5420601684062));
#33823=CARTESIAN_POINT('Ctrl Pts',(-26.3741436695224,25.103236616458,-16.5423247253604));
#33824=CARTESIAN_POINT('Ctrl Pts',(-26.3732861738627,25.1047948376656,-16.5424353252259));
#33825=CARTESIAN_POINT('Ctrl Pts',(-26.3715116258743,25.1080131946393,-16.5426636889085));
#33826=CARTESIAN_POINT('Ctrl Pts',(-26.3705943997094,25.1096732276734,-16.5427814405981));
#33827=CARTESIAN_POINT('Ctrl Pts',(-26.3684365167118,25.1135705203405,-16.5430577998073));
#33828=CARTESIAN_POINT('Ctrl Pts',(-26.3671946571006,25.1158071200922,-16.5432163296278));
#33829=CARTESIAN_POINT('Ctrl Pts',(-26.3631487881025,25.1230733647321,-16.5437311441233));
#33830=CARTESIAN_POINT('Ctrl Pts',(-26.3603339406385,25.128097010239,-16.5440867337083));
#33831=CARTESIAN_POINT('Ctrl Pts',(-26.2763178414771,25.2771022062031,-16.5546246028893));
#33832=CARTESIAN_POINT('Ctrl Pts',(-26.1841583954558,25.4146556912969,-16.5641021811261));
#33833=CARTESIAN_POINT('Ctrl Pts',(-25.8767988034859,25.8048219349782,-16.592081973591));
#33834=CARTESIAN_POINT('Ctrl Pts',(-25.6328827139552,26.0318930769095,-16.6101488225876));
#33835=CARTESIAN_POINT('Ctrl Pts',(-25.3419746128606,26.2291058475531,-16.6314061013047));
#33836=CARTESIAN_POINT('Ctrl Pts',(-25.3252005728499,26.2402492838476,-16.632629899594));
#33837=CARTESIAN_POINT('Ctrl Pts',(-25.3031077381031,26.2546295241833,-16.6342396624682));
#33838=CARTESIAN_POINT('Ctrl Pts',(-25.297882193997,26.2580093255589,-16.6346202628348));
#33839=CARTESIAN_POINT('Ctrl Pts',(-25.2898070768455,26.2631990742448,-16.6352081902425));
#33840=CARTESIAN_POINT('Ctrl Pts',(-25.2869643745615,26.2650197285271,-16.6354151177125));
#33841=CARTESIAN_POINT('Ctrl Pts',(-25.2813005818393,26.2686346587308,-16.6358273184942));
#33842=CARTESIAN_POINT('Ctrl Pts',(-25.2784795492928,26.2704290178825,-16.6360325883688));
#33843=CARTESIAN_POINT('Ctrl Pts',(-25.2722238197497,26.2743944068842,-16.636487695241));
#33844=CARTESIAN_POINT('Ctrl Pts',(-25.268787802895,26.2765633346748,-16.6367376098422));
#33845=CARTESIAN_POINT('Ctrl Pts',(-25.2590035420358,26.2827136382462,-16.6374491002396));
#33846=CARTESIAN_POINT('Ctrl Pts',(-25.2526455321466,26.2866793596312,-16.6379112545568));
#33847=CARTESIAN_POINT('Ctrl Pts',(-25.2114799432765,26.3121568338247,-16.6409023958203));
#33848=CARTESIAN_POINT('Ctrl Pts',(-25.1762805051653,26.3330253696343,-16.6434549231763));
#33849=CARTESIAN_POINT('Ctrl Pts',(-25.0703427078755,26.3931359796786,-16.6511263575044));
#33850=CARTESIAN_POINT('Ctrl Pts',(-24.9985184259472,26.4303887257047,-16.6563143504873));
#33851=CARTESIAN_POINT('Ctrl Pts',(-24.6870847592688,26.5773222196769,-16.6787580811849));
#33852=CARTESIAN_POINT('Ctrl Pts',(-24.4359223040316,26.6600908345066,-16.6968390638425));
#33853=CARTESIAN_POINT('Ctrl Pts',(-24.0892232617592,26.7288899825186,-16.720513163993));
#33854=CARTESIAN_POINT('Ctrl Pts',(-24.0001980434589,26.742708826642,-16.7264712575149));
#33855=CARTESIAN_POINT('Ctrl Pts',(-23.8715756730833,26.7571855592581,-16.7348055624111));
#33856=CARTESIAN_POINT('Ctrl Pts',(-23.8323673976582,26.7608723406366,-16.7373097274845));
#33857=CARTESIAN_POINT('Ctrl Pts',(-23.7883383201914,26.7641995623351,-16.7400737216579));
#33858=CARTESIAN_POINT('Ctrl Pts',(-23.7835765542512,26.7645487625424,-16.7403720194128));
#33859=CARTESIAN_POINT('Ctrl Pts',(-23.7764092124176,26.765058362607,-16.740820047701));
#33860=CARTESIAN_POINT('Ctrl Pts',(-23.7740042304935,26.7652266454445,-16.7409702188702));
#33861=CARTESIAN_POINT('Ctrl Pts',(-23.7698408474697,26.7655132738445,-16.7412299019444));
#33862=CARTESIAN_POINT('Ctrl Pts',(-23.7680825384887,26.765632875699,-16.7413394849364));
#33863=CARTESIAN_POINT('Ctrl Pts',(-23.7644209602992,26.7658789224754,-16.7415675004118));
#33864=CARTESIAN_POINT('Ctrl Pts',(-23.7625176790386,26.766005119836,-16.7416859182553));
#33865=CARTESIAN_POINT('Ctrl Pts',(-23.7580512997036,26.7662972813061,-16.741963564001));
#33866=CARTESIAN_POINT('Ctrl Pts',(-23.7554881059359,26.7664618716888,-16.7421227139573));
#33867=CARTESIAN_POINT('Ctrl Pts',(-23.7470844208006,26.7669914104831,-16.7426438974629));
#33868=CARTESIAN_POINT('Ctrl Pts',(-23.7412430883274,26.7673435181961,-16.7430052093063));
#33869=CARTESIAN_POINT('Ctrl Pts',(-23.727455781793,26.7681369147324,-16.743855820633));
#33870=CARTESIAN_POINT('Ctrl Pts',(-23.719509025633,26.7685646882122,-16.7443443790117));
#33871=CARTESIAN_POINT('Ctrl Pts',(-23.4406632197143,26.7825392590476,-16.7614297924199));
#33872=CARTESIAN_POINT('Ctrl Pts',(-23.1690829620679,26.761864679703,-16.7762181705965));
#33873=CARTESIAN_POINT('Ctrl Pts',(-22.7559390570677,26.6772000553047,-16.799854726454));
#33874=CARTESIAN_POINT('Ctrl Pts',(-22.6109154525277,26.6367350842044,-16.8083699612486));
#33875=CARTESIAN_POINT('Ctrl Pts',(-22.4558341201495,26.5815177652751,-16.8180288959535));
#33876=CARTESIAN_POINT('Ctrl Pts',(-22.4424432886137,26.5766496054537,-16.8188674544971));
#33877=CARTESIAN_POINT('Ctrl Pts',(-22.4223921379274,26.5692092160247,-16.8201301803131));
#33878=CARTESIAN_POINT('Ctrl Pts',(-22.4157072628945,26.5667033537038,-16.8205523497294));
#33879=CARTESIAN_POINT('Ctrl Pts',(-22.4052623349331,26.5627483822028,-16.82121387029));
#33880=CARTESIAN_POINT('Ctrl Pts',(-22.4014965551695,26.5613143886148,-16.8214527586597));
#33881=CARTESIAN_POINT('Ctrl Pts',(-22.3938797749693,26.5583975812164,-16.8219367304857));
#33882=CARTESIAN_POINT('Ctrl Pts',(-22.3900289140356,26.5569144262648,-16.8221818240965));
#33883=CARTESIAN_POINT('Ctrl Pts',(-22.3369601884303,26.5363579290019,-16.8255651577632));
#33884=CARTESIAN_POINT('Ctrl Pts',(-22.2882176655084,26.5160865212968,-16.8287405286875));
#33885=CARTESIAN_POINT('Ctrl Pts',(-22.2320260170298,26.4910810776542,-16.8324886683763));
#33886=CARTESIAN_POINT('Ctrl Pts',(-22.2240695523943,26.4875016501306,-16.8330214551079));
#33887=CARTESIAN_POINT('Ctrl Pts',(-22.2122258440204,26.4821155093004,-16.8338176672126));
#33888=CARTESIAN_POINT('Ctrl Pts',(-22.2083274655846,26.4803332563587,-16.8340802486095));
#33889=CARTESIAN_POINT('Ctrl Pts',(-22.2013775261303,26.4771391176962,-16.8345492823342));
#33890=CARTESIAN_POINT('Ctrl Pts',(-22.1983245914669,26.4757302212776,-16.8347556310788));
#33891=CARTESIAN_POINT('Ctrl Pts',(-22.1918895131608,26.4727482777622,-16.8351912451679));
#33892=CARTESIAN_POINT('Ctrl Pts',(-22.1885078865786,26.4711741323568,-16.8354205483232));
#33893=CARTESIAN_POINT('Ctrl Pts',(-22.1795755904479,26.4669972701619,-16.8360272661396));
#33894=CARTESIAN_POINT('Ctrl Pts',(-22.1740296213429,26.4643845889002,-16.8364050261754));
#33895=CARTESIAN_POINT('Ctrl Pts',(-22.1493006580692,26.4526485477194,-16.8380941713147));
#33896=CARTESIAN_POINT('Ctrl Pts',(-22.1302010410033,26.443351651158,-16.8394115859042));
#33897=CARTESIAN_POINT('Ctrl Pts',(-22.0991025237082,26.4278320466885,-16.8415780498589));
#33898=CARTESIAN_POINT('Ctrl Pts',(-22.0870492666874,26.4217219015699,-16.8424230571167));
#33899=CARTESIAN_POINT('Ctrl Pts',(-22.0750360036057,26.4155367685116,-16.8432706449041));
#33900=CARTESIAN_POINT('',(-26.7730012036304,23.553178285231,-16.6852117869365));
#33901=CARTESIAN_POINT('Ctrl Pts',(-22.0750360832114,26.4155368094973,-17.0912958973716));
#33902=CARTESIAN_POINT('Ctrl Pts',(-22.1535668768981,26.4559690693804,-17.0863106787744));
#33903=CARTESIAN_POINT('Ctrl Pts',(-22.233752977376,26.4931692513465,-17.0813837806402));
#33904=CARTESIAN_POINT('Ctrl Pts',(-22.4752708579841,26.5933580093501,-17.0667708531272));
#33905=CARTESIAN_POINT('Ctrl Pts',(-22.6402209590496,26.6466879184113,-17.0570632839845));
#33906=CARTESIAN_POINT('Ctrl Pts',(-22.8359745711018,26.692976406064,-17.0453123444403));
#33907=CARTESIAN_POINT('Ctrl Pts',(-22.863389019571,26.6990816482408,-17.0436620881841));
#33908=CARTESIAN_POINT('Ctrl Pts',(-22.9017596647664,26.7071019295469,-17.0413440422702));
#33909=CARTESIAN_POINT('Ctrl Pts',(-22.9126517240969,26.7093198505397,-17.0406851087459));
#33910=CARTESIAN_POINT('Ctrl Pts',(-22.9759360276291,26.7218656428443,-17.0368508300875));
#33911=CARTESIAN_POINT('Ctrl Pts',(-23.0285645596691,26.7309459025835,-17.0336389714329));
#33912=CARTESIAN_POINT('Ctrl Pts',(-23.0900548790222,26.7399879986226,-17.0298514728927));
#33913=CARTESIAN_POINT('Ctrl Pts',(-23.0987227205324,26.7412265296696,-17.0293167811369));
#33914=CARTESIAN_POINT('Ctrl Pts',(-23.1116476123205,26.7430196256445,-17.0285182651049));
#33915=CARTESIAN_POINT('Ctrl Pts',(-23.1159009478169,26.7436010395792,-17.0282552920034));
#33916=CARTESIAN_POINT('Ctrl Pts',(-23.1234886089753,26.7446228027192,-17.0277858105125));
#33917=CARTESIAN_POINT('Ctrl Pts',(-23.1268224923757,26.7450664348518,-17.0275794064221));
#33918=CARTESIAN_POINT('Ctrl Pts',(-23.1338521141308,26.7459906536671,-17.0271439351751));
#33919=CARTESIAN_POINT('Ctrl Pts',(-23.1375480016303,26.746470049739,-17.0269148306475));
#33920=CARTESIAN_POINT('Ctrl Pts',(-23.1473109141334,26.7477191877687,-17.0263092326643));
#33921=CARTESIAN_POINT('Ctrl Pts',(-23.1533792914866,26.7484780700596,-17.0259323961525));
#33922=CARTESIAN_POINT('Ctrl Pts',(-23.1803935549792,26.751778275601,-17.0242529900768));
#33923=CARTESIAN_POINT('Ctrl Pts',(-23.2013615593792,26.7541310885205,-17.0229444762228));
#33924=CARTESIAN_POINT('Ctrl Pts',(-23.340202739262,26.7683313099536,-17.0142455579066));
#33925=CARTESIAN_POINT('Ctrl Pts',(-23.4586156390194,26.7738760817245,-17.0066572019617));
#33926=CARTESIAN_POINT('Ctrl Pts',(-23.6030754443777,26.7726746764825,-16.9971890913247));
#33927=CARTESIAN_POINT('Ctrl Pts',(-23.6290930820044,26.772143103359,-16.9954757663598));
#33928=CARTESIAN_POINT('Ctrl Pts',(-23.8122754572498,26.7661803218788,-16.9833583251791));
#33929=CARTESIAN_POINT('Ctrl Pts',(-23.9688553027553,26.7495669811217,-16.9727033783324));
#33930=CARTESIAN_POINT('Ctrl Pts',(-24.3067094341909,26.6884878975699,-16.9494739427274));
#33931=CARTESIAN_POINT('Ctrl Pts',(-24.486647441895,26.6395778219922,-16.9369462902151));
#33932=CARTESIAN_POINT('Ctrl Pts',(-24.6719702688918,26.5715095994221,-16.9245070861992));
#33933=CARTESIAN_POINT('Ctrl Pts',(-24.6825445666759,26.5675625435694,-16.9237990433152));
#33934=CARTESIAN_POINT('Ctrl Pts',(-24.6963458025573,26.5623282016901,-16.9228773910607));
#33935=CARTESIAN_POINT('Ctrl Pts',(-24.6995915345834,26.5610911995753,-16.9226608184342));
#33936=CARTESIAN_POINT('Ctrl Pts',(-24.7045917194712,26.5591762827424,-16.9223274620397));
#33937=CARTESIAN_POINT('Ctrl Pts',(-24.7063475764904,26.5585020804352,-16.9222104549456));
#33938=CARTESIAN_POINT('Ctrl Pts',(-24.7096697492131,26.5572231163988,-16.921989174708));
#33939=CARTESIAN_POINT('Ctrl Pts',(-24.7112361746242,26.556618670812,-16.9218848833334));
#33940=CARTESIAN_POINT('Ctrl Pts',(-24.7148741016107,26.5552116157129,-16.9216427740848));
#33941=CARTESIAN_POINT('Ctrl Pts',(-24.7169452427108,26.5544080895629,-16.921505012633));
#33942=CARTESIAN_POINT('Ctrl Pts',(-24.7212064772963,26.5527498167611,-16.9212217307855));
#33943=CARTESIAN_POINT('Ctrl Pts',(-24.7233964704818,26.5518948136001,-16.9210762259824));
#33944=CARTESIAN_POINT('Ctrl Pts',(-24.7344492553768,26.547565711922,-16.9203422822242));
#33945=CARTESIAN_POINT('Ctrl Pts',(-24.7432976825977,26.5440547051928,-16.9197560527474));
#33946=CARTESIAN_POINT('Ctrl Pts',(-24.7657919765879,26.5350135280801,-16.9182688468553));
#33947=CARTESIAN_POINT('Ctrl Pts',(-24.7794159032692,26.5294288897283,-16.9173710157967));
#33948=CARTESIAN_POINT('Ctrl Pts',(-24.8353207454088,26.506063927783,-16.9136969541139));
#33949=CARTESIAN_POINT('Ctrl Pts',(-24.8772601048056,26.4874744665159,-16.9109646321013));
#33950=CARTESIAN_POINT('Ctrl Pts',(-24.9970029090544,26.4313102961489,-16.9031933193554));
#33951=CARTESIAN_POINT('Ctrl Pts',(-25.0737138454802,26.3914931168652,-16.8982513873834));
#33952=CARTESIAN_POINT('Ctrl Pts',(-25.2138467423114,26.3114469215322,-16.8891286217551));
#33953=CARTESIAN_POINT('Ctrl Pts',(-25.277640420067,26.2719930911369,-16.8849363828752));
#33954=CARTESIAN_POINT('Ctrl Pts',(-25.5665349624495,26.0790715053874,-16.8655242993437));
#33955=CARTESIAN_POINT('Ctrl Pts',(-25.772939675415,25.8997111854494,-16.8502916386441));
#33956=CARTESIAN_POINT('Ctrl Pts',(-25.9660425585434,25.6834158686752,-16.8327277529319));
#33957=CARTESIAN_POINT('Ctrl Pts',(-25.9776550352329,25.6701922343086,-16.8316572857906));
#33958=CARTESIAN_POINT('Ctrl Pts',(-25.993013206432,25.6524115704127,-16.8302220678694));
#33959=CARTESIAN_POINT('Ctrl Pts',(-25.9968556895914,25.6479382386457,-16.8298613363571));
#33960=CARTESIAN_POINT('Ctrl Pts',(-26.0028358299159,25.640937511541,-16.8292973232686));
#33961=CARTESIAN_POINT('Ctrl Pts',(-26.0049819212287,25.6384173105604,-16.8290943899135));
#33962=CARTESIAN_POINT('Ctrl Pts',(-26.0090763740541,25.6335940723103,-16.8287062107611));
#33963=CARTESIAN_POINT('Ctrl Pts',(-26.0110253933173,25.6312915957232,-16.8285209922938));
#33964=CARTESIAN_POINT('Ctrl Pts',(-26.0155698452952,25.6259076902571,-16.8280880953873));
#33965=CARTESIAN_POINT('Ctrl Pts',(-26.018162734055,25.6228241292174,-16.8278403130069));
#33966=CARTESIAN_POINT('Ctrl Pts',(-26.0255559181731,25.6139983308701,-16.8271315405065));
#33967=CARTESIAN_POINT('Ctrl Pts',(-26.0303419778832,25.6082442508509,-16.8266699697743));
#33968=CARTESIAN_POINT('Ctrl Pts',(-26.0409898359572,25.5953516887241,-16.8256369118406));
#33969=CARTESIAN_POINT('Ctrl Pts',(-26.0468410583227,25.5882045936378,-16.8250649994524));
#33970=CARTESIAN_POINT('Ctrl Pts',(-26.0907402773733,25.5341102073467,-16.8207419968735));
#33971=CARTESIAN_POINT('Ctrl Pts',(-26.1274895919554,25.4861289739368,-16.8169391030921));
#33972=CARTESIAN_POINT('Ctrl Pts',(-26.2438107248451,25.3250693831589,-16.8042645727324));
#33973=CARTESIAN_POINT('Ctrl Pts',(-26.3174495983621,25.207914382771,-16.7951787702345));
#33974=CARTESIAN_POINT('Ctrl Pts',(-26.4071199249425,25.0425381886739,-16.7825878435136));
#33975=CARTESIAN_POINT('Ctrl Pts',(-26.4298836294418,24.9981241856403,-16.7792291414005));
#33976=CARTESIAN_POINT('Ctrl Pts',(-26.4623134575627,24.9310579691324,-16.7741995481262));
#33977=CARTESIAN_POINT('Ctrl Pts',(-26.4727665624012,24.9087937421993,-16.7725366615279));
#33978=CARTESIAN_POINT('Ctrl Pts',(-26.494781266265,24.8604740896805,-16.7689441812351));
#33979=CARTESIAN_POINT('Ctrl Pts',(-26.5062541530103,24.8343804113196,-16.767014340597));
#33980=CARTESIAN_POINT('Ctrl Pts',(-26.5817546356709,24.6562882782503,-16.7539218144734));
#33981=CARTESIAN_POINT('Ctrl Pts',(-26.6343841769804,24.4997061500629,-16.7427837206607));
#33982=CARTESIAN_POINT('Ctrl Pts',(-26.6842960497413,24.3021781936186,-16.7296703432913));
#33983=CARTESIAN_POINT('Ctrl Pts',(-26.6931163120391,24.2644153756936,-16.7272051004348));
#33984=CARTESIAN_POINT('Ctrl Pts',(-26.702250877742,24.2218525523555,-16.7244801587211));
#33985=CARTESIAN_POINT('Ctrl Pts',(-26.703238119652,24.2172023379461,-16.7241831601281));
#33986=CARTESIAN_POINT('Ctrl Pts',(-26.7047094542041,24.2101956153712,-16.7237367519101));
#33987=CARTESIAN_POINT('Ctrl Pts',(-26.7052011981482,24.207840747675,-16.7235869060832));
#33988=CARTESIAN_POINT('Ctrl Pts',(-26.706048362062,24.2037610174578,-16.7233276281163));
#33989=CARTESIAN_POINT('Ctrl Pts',(-26.7064050048825,24.2020364145528,-16.7232181254253));
#33990=CARTESIAN_POINT('Ctrl Pts',(-26.7071452216315,24.1984421255273,-16.7229901187458));
#33991=CARTESIAN_POINT('Ctrl Pts',(-26.7075285478719,24.1965723929244,-16.7228716296236));
#33992=CARTESIAN_POINT('Ctrl Pts',(-26.7082882494431,24.1928500276516,-16.7226359698331));
#33993=CARTESIAN_POINT('Ctrl Pts',(-26.7086646565208,24.1909973999378,-16.722518797222));
#33994=CARTESIAN_POINT('Ctrl Pts',(-26.7095425181369,24.1866571073863,-16.722244556627));
#33995=CARTESIAN_POINT('Ctrl Pts',(-26.7100426658605,24.1841691748965,-16.7220875636834));
#33996=CARTESIAN_POINT('Ctrl Pts',(-26.711345021966,24.1776509039523,-16.7216767841636));
#33997=CARTESIAN_POINT('Ctrl Pts',(-26.7121424643921,24.1736196013311,-16.7214232680318));
#33998=CARTESIAN_POINT('Ctrl Pts',(-26.7526918072996,23.9665511448661,-16.7084283403808));
#33999=CARTESIAN_POINT('Ctrl Pts',(-26.772813325684,23.7601278435454,-16.6967895284045));
#34000=CARTESIAN_POINT('Ctrl Pts',(-26.7730012036304,23.553178285231,-16.6852117869365));
#34001=CARTESIAN_POINT('Ctrl Pts',(-26.7730012021961,23.5531798646698,-16.6852118752978));
#34002=CARTESIAN_POINT('Ctrl Pts',(-26.7731886828151,23.3467793900092,-16.6736648516152));
#34003=CARTESIAN_POINT('Ctrl Pts',(-26.7535484417044,23.1408458469785,-16.6622156702365));
#34004=CARTESIAN_POINT('Ctrl Pts',(-26.7017859055637,22.8732506738851,-16.6463314591706));
#34005=CARTESIAN_POINT('Ctrl Pts',(-26.6872256775366,22.8087050174693,-16.6424241534016));
#34006=CARTESIAN_POINT('Ctrl Pts',(-26.66499058144,22.7225784674869,-16.6370856317034));
#34007=CARTESIAN_POINT('Ctrl Pts',(-26.6590567980103,22.7005623127291,-16.6357099061423));
#34008=CARTESIAN_POINT('Ctrl Pts',(-26.6500995820468,22.6686787853832,-16.633700744437));
#34009=CARTESIAN_POINT('Ctrl Pts',(-26.6472615032878,22.6587597208574,-16.633073306443));
#34010=CARTESIAN_POINT('Ctrl Pts',(-26.6420859260347,22.6409941227649,-16.6319451783293));
#34011=CARTESIAN_POINT('Ctrl Pts',(-26.639766054212,22.6331425138677,-16.6314450655755));
#34012=CARTESIAN_POINT('Ctrl Pts',(-26.6362174456555,22.6212985174817,-16.6306883133069));
#34013=CARTESIAN_POINT('Ctrl Pts',(-26.6350108118583,22.6172994978173,-16.6304323985157));
#34014=CARTESIAN_POINT('Ctrl Pts',(-26.6329144750519,22.6104003583475,-16.6299901901601));
#34015=CARTESIAN_POINT('Ctrl Pts',(-26.6320284436364,22.6074991210713,-16.6298040173237));
#34016=CARTESIAN_POINT('Ctrl Pts',(-26.6301879575527,22.6015029204434,-16.6294187943395));
#34017=CARTESIAN_POINT('Ctrl Pts',(-26.6292329312423,22.5984081371756,-16.6292197255728));
#34018=CARTESIAN_POINT('Ctrl Pts',(-26.6269102882543,22.5909216351242,-16.6287375659948));
#34019=CARTESIAN_POINT('Ctrl Pts',(-26.6255379341191,22.586531403252,-16.6284543195392));
#34020=CARTESIAN_POINT('Ctrl Pts',(-26.6204098318996,22.5702488337087,-16.6274019476845));
#34021=CARTESIAN_POINT('Ctrl Pts',(-26.6165944989754,22.5583755087048,-16.6266308612285));
#34022=CARTESIAN_POINT('Ctrl Pts',(-26.5540100184194,22.3674249943145,-16.614169571502));
#34023=CARTESIAN_POINT('Ctrl Pts',(-26.4797231918104,22.1938532985899,-16.6019506643725));
#34024=CARTESIAN_POINT('Ctrl Pts',(-26.3423136630922,21.9374880641703,-16.5825376998385));
#34025=CARTESIAN_POINT('Ctrl Pts',(-26.2896358508681,21.8495491082791,-16.5756123557096));
#34026=CARTESIAN_POINT('Ctrl Pts',(-26.2106961338803,21.7309787382728,-16.565970089807));
#34027=CARTESIAN_POINT('Ctrl Pts',(-26.1879128567065,21.6981009901301,-16.563262352275));
#34028=CARTESIAN_POINT('Ctrl Pts',(-26.1430823207508,21.6359130648195,-16.5580832208535));
#34029=CARTESIAN_POINT('Ctrl Pts',(-26.1211348805077,21.6065380639062,-16.5556112898802));
#34030=CARTESIAN_POINT('Ctrl Pts',(-26.0410196708019,21.5030414693933,-16.5468239092346));
#34031=CARTESIAN_POINT('Ctrl Pts',(-25.9801044745044,21.4310978757263,-16.5405681664569));
#34032=CARTESIAN_POINT('Ctrl Pts',(-25.8852863209428,21.3285872402985,-16.5315460945985));
#34033=CARTESIAN_POINT('Ctrl Pts',(-25.8537498930171,21.2959056416921,-16.528652325866));
#34034=CARTESIAN_POINT('Ctrl Pts',(-25.8190518514082,21.2614363695734,-16.5255918707849));
#34035=CARTESIAN_POINT('Ctrl Pts',(-25.8165683749491,21.258977280659,-16.5253734864821));
#34036=CARTESIAN_POINT('Ctrl Pts',(-25.8124580806187,21.2549205697077,-16.5250131522398));
#34037=CARTESIAN_POINT('Ctrl Pts',(-25.8108335667756,21.2533206334423,-16.5248710210871));
#34038=CARTESIAN_POINT('Ctrl Pts',(-25.8079219512546,21.2504591491101,-16.5246167896617));
#34039=CARTESIAN_POINT('Ctrl Pts',(-25.8066354889158,21.2491969563128,-16.524504638403));
#34040=CARTESIAN_POINT('Ctrl Pts',(-25.8040137942302,21.2466290334321,-16.5242764473557));
#34041=CARTESIAN_POINT('Ctrl Pts',(-25.8026784875798,21.2453233866735,-16.524160414393));
#34042=CARTESIAN_POINT('Ctrl Pts',(-25.800006808813,21.2427155901679,-16.5239286387234));
#34043=CARTESIAN_POINT('Ctrl Pts',(-25.7986704461279,21.2414134454824,-16.5238128962442));
#34044=CARTESIAN_POINT('Ctrl Pts',(-25.7948963291772,21.2377423502139,-16.5234865548486));
#34045=CARTESIAN_POINT('Ctrl Pts',(-25.7924559474699,21.235376085841,-16.5232761681639));
#34046=CARTESIAN_POINT('Ctrl Pts',(-25.7823279709486,21.2255867499938,-16.5224056083224));
#34047=CARTESIAN_POINT('Ctrl Pts',(-25.7746071077891,21.2181979674697,-16.5217480953287));
#34048=CARTESIAN_POINT('Ctrl Pts',(-25.6334098933532,21.0844129545713,-16.5098317112634));
#34049=CARTESIAN_POINT('Ctrl Pts',(-25.4893743647855,20.9696058041119,-16.4994148506551));
#34050=CARTESIAN_POINT('Ctrl Pts',(-25.2578284535008,20.8154413175926,-16.4838214781806));
#34051=CARTESIAN_POINT('Ctrl Pts',(-25.1770890224939,20.7666557597724,-16.4785742993486));
#34052=CARTESIAN_POINT('Ctrl Pts',(-24.9983566505112,20.6690953877579,-16.4671524469688));
#34053=CARTESIAN_POINT('Ctrl Pts',(-24.8997875434432,20.6216308283257,-16.4609699269727));
#34054=CARTESIAN_POINT('Ctrl Pts',(-24.7257810379265,20.5484932580268,-16.4500536522867));
#34055=CARTESIAN_POINT('Ctrl Pts',(-24.6514523432598,20.520436776313,-16.4453907653291));
#34056=CARTESIAN_POINT('Ctrl Pts',(-24.5380680548735,20.4823618413013,-16.4382322928957));
#34057=CARTESIAN_POINT('Ctrl Pts',(-24.4997342475392,20.4702822324298,-16.4358046542446));
#34058=CARTESIAN_POINT('Ctrl Pts',(-24.4539743928971,20.4567980095001,-16.4328946945276));
#34059=CARTESIAN_POINT('Ctrl Pts',(-24.4467555739866,20.4546982393341,-16.4324352849339));
#34060=CARTESIAN_POINT('Ctrl Pts',(-24.4356501635879,20.4515100632595,-16.4317279695858));
#34061=CARTESIAN_POINT('Ctrl Pts',(-24.4317687307528,20.4504036575062,-16.4314806519444));
#34062=CARTESIAN_POINT('Ctrl Pts',(-24.4249819734829,20.4484828641797,-16.43104802516));
#34063=CARTESIAN_POINT('Ctrl Pts',(-24.4220775585106,20.4476652582781,-16.4308628212446));
#34064=CARTESIAN_POINT('Ctrl Pts',(-24.4159882688092,20.4459603214166,-16.4304744022758));
#34065=CARTESIAN_POINT('Ctrl Pts',(-24.4128031698434,20.4450738106206,-16.4302711607403));
#34066=CARTESIAN_POINT('Ctrl Pts',(-24.4039522627154,20.4426250002837,-16.4297061779155));
#34067=CARTESIAN_POINT('Ctrl Pts',(-24.3982835575465,20.4410733018675,-16.4293440920044));
#34068=CARTESIAN_POINT('Ctrl Pts',(-24.3757642254869,20.434975237549,-16.4279047298507));
#34069=CARTESIAN_POINT('Ctrl Pts',(-24.35888127498,20.4305503484322,-16.4268235150889));
#34070=CARTESIAN_POINT('Ctrl Pts',(-24.0794142380463,20.359725173855,-16.4088888859524));
#34071=CARTESIAN_POINT('Ctrl Pts',(-23.8095830196128,20.3265650428403,-16.3908925750674));
#34072=CARTESIAN_POINT('Ctrl Pts',(-23.3999439815969,20.3280140542681,-16.3631738479551));
#34073=CARTESIAN_POINT('Ctrl Pts',(-23.2612066785752,20.3374859424437,-16.3537457575569));
#34074=CARTESIAN_POINT('Ctrl Pts',(-23.0393590391651,20.3671231030872,-16.3389486175802));
#34075=CARTESIAN_POINT('Ctrl Pts',(-22.955677393428,20.3816868521624,-16.3334342857079));
#34076=CARTESIAN_POINT('Ctrl Pts',(-22.863391933768,20.4015337497925,-16.3274981078645));
#34077=CARTESIAN_POINT('Ctrl Pts',(-22.8541317380503,20.403568039325,-16.326904102412));
#34078=CARTESIAN_POINT('Ctrl Pts',(-22.8425901882034,20.4061569416004,-16.3261659312334));
#34079=CARTESIAN_POINT('Ctrl Pts',(-22.8403004126517,20.4066731926616,-16.3260195893414));
#34080=CARTESIAN_POINT('Ctrl Pts',(-22.8362328753497,20.4075949274258,-16.3257598214364));
#34081=CARTESIAN_POINT('Ctrl Pts',(-22.8344548932591,20.4079994183753,-16.3256463383676));
#34082=CARTESIAN_POINT('Ctrl Pts',(-22.8310193026044,20.408784082569,-16.3254271830307));
#34083=CARTESIAN_POINT('Ctrl Pts',(-22.8293616499371,20.4091640593123,-16.3253214993992));
#34084=CARTESIAN_POINT('Ctrl Pts',(-22.8259585942386,20.4099469632174,-16.3251046565664));
#34085=CARTESIAN_POINT('Ctrl Pts',(-22.8242132301794,20.4103500325812,-16.3249935059994));
#34086=CARTESIAN_POINT('Ctrl Pts',(-22.8200135118094,20.4113235924505,-16.3247262063095));
#34087=CARTESIAN_POINT('Ctrl Pts',(-22.8175594840771,20.411895507731,-16.3245701399173));
#34088=CARTESIAN_POINT('Ctrl Pts',(-22.8086109370771,20.4139920497274,-16.3240014964818));
#34089=CARTESIAN_POINT('Ctrl Pts',(-22.8021204264702,20.4155339764382,-16.3235899132966));
#34090=CARTESIAN_POINT('Ctrl Pts',(-22.6902346679673,20.4424815583643,-16.3165090402039));
#34091=CARTESIAN_POINT('Ctrl Pts',(-22.5861694055381,20.4731726451618,-16.3101392002413));
#34092=CARTESIAN_POINT('Ctrl Pts',(-22.456434731379,20.5186649194803,-16.3022466897869));
#34093=CARTESIAN_POINT('Ctrl Pts',(-22.4291621753271,20.5286441345075,-16.3005903899509));
#34094=CARTESIAN_POINT('Ctrl Pts',(-22.3719660104479,20.5504536150014,-16.2971158519121));
#34095=CARTESIAN_POINT('Ctrl Pts',(-22.3420771812277,20.5623661469095,-16.2952996205389));
#34096=CARTESIAN_POINT('Ctrl Pts',(-22.1644578634802,20.6362594535201,-16.2844771103072));
#34097=CARTESIAN_POINT('Ctrl Pts',(-22.0213401700413,20.7087371590719,-16.2756227027085));
#34098=CARTESIAN_POINT('Ctrl Pts',(-21.7749291177407,20.8575511228047,-16.2593166869138));
#34099=CARTESIAN_POINT('Ctrl Pts',(-21.669681139088,20.9299738534172,-16.2519626370568));
#34100=CARTESIAN_POINT('Ctrl Pts',(-21.5265341488565,21.0415512642001,-16.2411732739541));
#34101=CARTESIAN_POINT('Ctrl Pts',(-21.4848953716723,21.0757187541497,-16.2379327470344));
#34102=CARTESIAN_POINT('Ctrl Pts',(-21.4379904089147,21.1162163431359,-16.2341545335701));
#34103=CARTESIAN_POINT('Ctrl Pts',(-21.431866917209,21.121543856496,-16.2336587105104));
#34104=CARTESIAN_POINT('Ctrl Pts',(-21.4226336692887,21.1296383813033,-16.2329071545356));
#34105=CARTESIAN_POINT('Ctrl Pts',(-21.4195090090389,21.1323884062438,-16.2326521313249));
#34106=CARTESIAN_POINT('Ctrl Pts',(-21.4141178385373,21.1371517617791,-16.2322109319245));
#34107=CARTESIAN_POINT('Ctrl Pts',(-21.411848819817,21.1391622559058,-16.2320248748496));
#34108=CARTESIAN_POINT('Ctrl Pts',(-21.4071569665038,21.1433313674799,-16.2316393864508));
#34109=CARTESIAN_POINT('Ctrl Pts',(-21.4047345493572,21.1454904479051,-16.2314399357565));
#34110=CARTESIAN_POINT('Ctrl Pts',(-21.3981622312779,21.1513661366627,-16.2308976505708));
#34111=CARTESIAN_POINT('Ctrl Pts',(-21.3940187138381,21.1550898400334,-16.2305545168224));
#34112=CARTESIAN_POINT('Ctrl Pts',(-21.3785165886383,21.1690941444336,-16.2292660340754));
#34113=CARTESIAN_POINT('Ctrl Pts',(-21.3672218213473,21.1794448262429,-16.2283177141028));
#34114=CARTESIAN_POINT('Ctrl Pts',(-21.1844520724328,21.3493510390126,-16.2128142848181));
#34115=CARTESIAN_POINT('Ctrl Pts',(-21.0308359506586,21.527018231633,-16.1974236057871));
#34116=CARTESIAN_POINT('Ctrl Pts',(-20.8135628732052,21.8418423436627,-16.1716383790066));
#34117=CARTESIAN_POINT('Ctrl Pts',(-20.7378146135334,21.9696421185441,-16.1615288190238));
#34118=CARTESIAN_POINT('Ctrl Pts',(-20.6316891724106,22.1806485595747,-16.1457489330931));
#34119=CARTESIAN_POINT('Ctrl Pts',(-20.5954557133736,22.2606768149133,-16.1399601878728));
#34120=CARTESIAN_POINT('Ctrl Pts',(-20.5499157020365,22.37329487001,-16.1321719124068));
#34121=CARTESIAN_POINT('Ctrl Pts',(-20.5377867580971,22.4046956298663,-16.1300378091248));
#34122=CARTESIAN_POINT('Ctrl Pts',(-20.5245556003294,22.4406143220484,-16.127643657651));
#34123=CARTESIAN_POINT('Ctrl Pts',(-20.5229690851477,22.4449499434066,-16.1273554411144));
#34124=CARTESIAN_POINT('Ctrl Pts',(-20.5207459217611,22.4510660879061,-16.1269499660584));
#34125=CARTESIAN_POINT('Ctrl Pts',(-20.5201015252244,22.452843758324,-16.1268322451754));
#34126=CARTESIAN_POINT('Ctrl Pts',(-20.5188097508751,22.4564171360536,-16.1265958742382));
#34127=CARTESIAN_POINT('Ctrl Pts',(-20.5181624023122,22.4582128558976,-16.1264772258986));
#34128=CARTESIAN_POINT('Ctrl Pts',(-20.5169209723379,22.4616661483733,-16.1262493168309));
#34129=CARTESIAN_POINT('Ctrl Pts',(-20.5163266550762,22.4633236296203,-16.1261400418453));
#34130=CARTESIAN_POINT('Ctrl Pts',(-20.5149239515028,22.4672457197641,-16.1258817346467));
#34131=CARTESIAN_POINT('Ctrl Pts',(-20.5141167393244,22.4695107518074,-16.1257327731335));
#34132=CARTESIAN_POINT('Ctrl Pts',(-20.5117226560127,22.4762523849963,-16.1252900307727));
#34133=CARTESIAN_POINT('Ctrl Pts',(-20.51014313618,22.4807316181515,-16.124996687449));
#34134=CARTESIAN_POINT('Ctrl Pts',(-20.4958001610431,22.5216942124813,-16.1223214154674));
#34135=CARTESIAN_POINT('Ctrl Pts',(-20.483683416088,22.5584029031709,-16.1199772126381));
#34136=CARTESIAN_POINT('Ctrl Pts',(-20.4696392058571,22.6036715724507,-16.1171410835519));
#34137=CARTESIAN_POINT('Ctrl Pts',(-20.467082982401,22.6120310709995,-16.1166196212295));
#34138=CARTESIAN_POINT('Ctrl Pts',(-20.4622153522642,22.6281841932491,-16.1156161847289));
#34139=CARTESIAN_POINT('Ctrl Pts',(-20.4598993627259,22.6359763502786,-16.1151340084135));
#34140=CARTESIAN_POINT('Ctrl Pts',(-20.4543113080989,22.6550412271751,-16.113958668943));
#34141=CARTESIAN_POINT('Ctrl Pts',(-20.4510712783074,22.6663232894665,-16.1132668761383));
#34142=CARTESIAN_POINT('Ctrl Pts',(-20.443329185366,22.693847862018,-16.1115876639134));
#34143=CARTESIAN_POINT('Ctrl Pts',(-20.4388927268382,22.7101086025939,-16.1106028476062));
#34144=CARTESIAN_POINT('Ctrl Pts',(-20.4191558309595,22.784750479676,-16.1061121250309));
#34145=CARTESIAN_POINT('Ctrl Pts',(-20.4053690385359,22.8435217605578,-16.1026595942019));
#34146=CARTESIAN_POINT('Ctrl Pts',(-20.3510374635455,23.1083831230778,-16.0873367906854));
#34147=CARTESIAN_POINT('Ctrl Pts',(-20.3290460777488,23.3177497492138,-16.0758257934289));
#34148=CARTESIAN_POINT('Ctrl Pts',(-20.3268123077351,23.6379526737028,-16.057568707257));
#34149=CARTESIAN_POINT('Ctrl Pts',(-20.331694738321,23.7480919561354,-16.0511785528916));
#34150=CARTESIAN_POINT('Ctrl Pts',(-20.346907018349,23.9067938168242,-16.0416797053643));
#34151=CARTESIAN_POINT('Ctrl Pts',(-20.3527307720229,23.9557132030965,-16.0387118939301));
#34152=CARTESIAN_POINT('Ctrl Pts',(-20.3607918052294,24.0123356758224,-16.0352243408427));
#34153=CARTESIAN_POINT('Ctrl Pts',(-20.3619394828733,24.0201891856069,-16.0347394469777));
#34154=CARTESIAN_POINT('Ctrl Pts',(-20.3637276934001,24.0321176919695,-16.0340011450163));
#34155=CARTESIAN_POINT('Ctrl Pts',(-20.3643470639763,24.0361958702281,-16.0337484090218));
#34156=CARTESIAN_POINT('Ctrl Pts',(-20.3654344996915,24.0432645270689,-16.0333097830818));
#34157=CARTESIAN_POINT('Ctrl Pts',(-20.3658989524952,24.04625556303,-16.0331240081208));
#34158=CARTESIAN_POINT('Ctrl Pts',(-20.3668726234891,24.0524681830509,-16.0327377742826));
#34159=CARTESIAN_POINT('Ctrl Pts',(-20.3673825196473,24.0556896560851,-16.0325372940408));
#34160=CARTESIAN_POINT('Ctrl Pts',(-20.3686363724465,24.0635342324366,-16.032048607708));
#34161=CARTESIAN_POINT('Ctrl Pts',(-20.369385514774,24.0681564894043,-16.0317602369052));
#34162=CARTESIAN_POINT('Ctrl Pts',(-20.3722543180792,24.0856161548773,-16.0306693651491));
#34163=CARTESIAN_POINT('Ctrl Pts',(-20.3744416191771,24.098442183845,-16.029864713691));
#34164=CARTESIAN_POINT('Ctrl Pts',(-20.413516903677,24.3194881486243,-16.0159394306964));
#34165=CARTESIAN_POINT('Ctrl Pts',(-20.4707245656831,24.5235508593853,-16.0021455179283));
#34166=CARTESIAN_POINT('Ctrl Pts',(-20.6245276397996,24.9181951085208,-15.9737230216388));
#34167=CARTESIAN_POINT('Ctrl Pts',(-20.7209028401736,25.1077871698904,-15.9591664840777));
#34168=CARTESIAN_POINT('Ctrl Pts',(-20.8752433936825,25.3491313138205,-15.9402919596216));
#34169=CARTESIAN_POINT('Ctrl Pts',(-20.9174324149907,25.4103329088577,-15.9354772446921));
#34170=CARTESIAN_POINT('Ctrl Pts',(-20.9662614904042,25.4761721586606,-15.93031239053));
#34171=CARTESIAN_POINT('Ctrl Pts',(-20.9708414918576,25.4823019102951,-15.9298316821384));
#34172=CARTESIAN_POINT('Ctrl Pts',(-20.9788571997769,25.4929506123127,-15.9289969324869));
#34173=CARTESIAN_POINT('Ctrl Pts',(-20.9822830717815,25.497476874078,-15.9286422288976));
#34174=CARTESIAN_POINT('Ctrl Pts',(-20.9872547942927,25.5040095727518,-15.9281304766472));
#34175=CARTESIAN_POINT('Ctrl Pts',(-20.9887910542632,25.5060232434982,-15.9279727574624));
#34176=CARTESIAN_POINT('Ctrl Pts',(-20.9914846067776,25.5095452314235,-15.9276969488652));
#34177=CARTESIAN_POINT('Ctrl Pts',(-20.9926408616912,25.5110543376741,-15.9275787856276));
#34178=CARTESIAN_POINT('Ctrl Pts',(-20.9948771583557,25.5139677356675,-15.9273506975588));
#34179=CARTESIAN_POINT('Ctrl Pts',(-20.9959570201304,25.5153721567105,-15.9272407602935));
#34180=CARTESIAN_POINT('Ctrl Pts',(-20.9985305265296,25.5187134414523,-15.9269792378122));
#34181=CARTESIAN_POINT('Ctrl Pts',(-21.0000252217931,25.5206495000266,-15.9268277275541));
#34182=CARTESIAN_POINT('Ctrl Pts',(-21.0053310469445,25.5275059128826,-15.9262912464631));
#34183=CARTESIAN_POINT('Ctrl Pts',(-21.0091542560121,25.5324169678143,-15.9259071294703));
#34184=CARTESIAN_POINT('Ctrl Pts',(-21.0616195490663,25.5994093262723,-15.9206689085217));
#34185=CARTESIAN_POINT('Ctrl Pts',(-21.1125151687427,25.6597019085795,-15.9159729156732));
#34186=CARTESIAN_POINT('Ctrl Pts',(-21.1893537875207,25.7442270375602,-15.9093153633111));
#34187=CARTESIAN_POINT('Ctrl Pts',(-21.2135601287548,25.7699903025009,-15.9072755395345));
#34188=CARTESIAN_POINT('Ctrl Pts',(-21.4289105364382,25.9917643112244,-15.8895688304469));
#34189=CARTESIAN_POINT('Ctrl Pts',(-21.6438846905835,26.163076038386,-15.8747612741233));
#34190=CARTESIAN_POINT('Ctrl Pts',(-21.9423331558195,26.3442438517148,-15.8546127577004));
#34191=CARTESIAN_POINT('Ctrl Pts',(-22.0080725960456,26.3810600756767,-15.850204687245));
#34192=CARTESIAN_POINT('Ctrl Pts',(-22.0750360164986,26.4155367751497,-15.845717117064));
#34193=CARTESIAN_POINT('Origin',(-23.5502525316942,23.5502525316942,-77.3107734492734));
#34194=CARTESIAN_POINT('',(-22.0750360145738,26.4155367741587,-14.3492876249023));
#34195=CARTESIAN_POINT('',(-22.0750361948364,26.4155368669684,-14.5938261690085));
#34196=CARTESIAN_POINT('',(-22.0750360153461,26.4155367745563,-77.3107734492734));
#34197=CARTESIAN_POINT('',(-26.7730011825842,23.5473036867677,-15.1896424574236));
#34198=CARTESIAN_POINT('Ctrl Pts',(-22.0750360145738,26.4155367741587,-14.3492876249023));
#34199=CARTESIAN_POINT('Ctrl Pts',(-22.0575688255074,26.4065436399221,-14.3505366306308));
#34200=CARTESIAN_POINT('Ctrl Pts',(-22.0401831532783,26.3973904119975,-14.3517769408737));
#34201=CARTESIAN_POINT('Ctrl Pts',(-22.0178226531192,26.3853555688787,-14.3533673775319));
#34202=CARTESIAN_POINT('Ctrl Pts',(-22.0127713311615,26.3826194082525,-14.3537263452519));
#34203=CARTESIAN_POINT('Ctrl Pts',(-22.0057073247074,26.378768566466,-14.3542278676196));
#34204=CARTESIAN_POINT('Ctrl Pts',(-22.0036885151667,26.3776652356076,-14.3543711423095));
#34205=CARTESIAN_POINT('Ctrl Pts',(-21.9999975015453,26.3756428666488,-14.3546329909806));
#34206=CARTESIAN_POINT('Ctrl Pts',(-21.9983249299616,26.3747245040096,-14.3547516084697));
#34207=CARTESIAN_POINT('Ctrl Pts',(-21.9949300319399,26.3728565337436,-14.3549922924005));
#34208=CARTESIAN_POINT('Ctrl Pts',(-21.9932077586214,26.3719068346384,-14.3551143527132));
#34209=CARTESIAN_POINT('Ctrl Pts',(-21.9889829197636,26.3695721202513,-14.3554136744765));
#34210=CARTESIAN_POINT('Ctrl Pts',(-21.9864813205783,26.3681853454775,-14.3555908222648));
#34211=CARTESIAN_POINT('Ctrl Pts',(-21.977318120931,26.3630897175642,-14.3562394012561));
#34212=CARTESIAN_POINT('Ctrl Pts',(-21.9706677733736,26.3593605198019,-14.3567095323155));
#34213=CARTESIAN_POINT('Ctrl Pts',(-21.8159756742526,26.2718935226117,-14.3676329349495));
#34214=CARTESIAN_POINT('Ctrl Pts',(-21.674755321772,26.1765759007306,-14.3773499617286));
#34215=CARTESIAN_POINT('Ctrl Pts',(-21.3844110429276,25.9451852310465,-14.3982293484068));
#34216=CARTESIAN_POINT('Ctrl Pts',(-21.2392047384932,25.8053863497996,-14.4093053138431));
#34217=CARTESIAN_POINT('Ctrl Pts',(-21.0831217699524,25.6240978686232,-14.4230365260751));
#34218=CARTESIAN_POINT('Ctrl Pts',(-21.0587817396057,25.5947920468528,-14.4252375569533));
#34219=CARTESIAN_POINT('Ctrl Pts',(-20.9740065710603,25.488958874302,-14.4331351199572));
#34220=CARTESIAN_POINT('Ctrl Pts',(-20.916536378735,25.4101347438325,-14.4389264458014));
#34221=CARTESIAN_POINT('Ctrl Pts',(-20.8575886998007,25.3210619166707,-14.445427986792));
#34222=CARTESIAN_POINT('Ctrl Pts',(-20.8524799694093,25.3132691478456,-14.4459964242809));
#34223=CARTESIAN_POINT('Ctrl Pts',(-20.8449446023952,25.3016653845281,-14.4468423518024));
#34224=CARTESIAN_POINT('Ctrl Pts',(-20.8424920363326,25.2978712180274,-14.4471188718738));
#34225=CARTESIAN_POINT('Ctrl Pts',(-20.8383070689721,25.2913670354288,-14.447592769086));
#34226=CARTESIAN_POINT('Ctrl Pts',(-20.8365707266426,25.2886595521338,-14.4477899989938));
#34227=CARTESIAN_POINT('Ctrl Pts',(-20.8332005258119,25.2833870356314,-14.4481740094175));
#34228=CARTESIAN_POINT('Ctrl Pts',(-20.8315662389448,25.2808222797617,-14.4483607736759));
#34229=CARTESIAN_POINT('Ctrl Pts',(-20.8276658760257,25.2746821137794,-14.4488078201755));
#34230=CARTESIAN_POINT('Ctrl Pts',(-20.825403213664,25.2711045517557,-14.4490682288033));
#34231=CARTESIAN_POINT('Ctrl Pts',(-20.8189185811264,25.2608066527492,-14.4498176336531));
#34232=CARTESIAN_POINT('Ctrl Pts',(-20.8147144007027,25.254075199306,-14.4503072876308));
#34233=CARTESIAN_POINT('Ctrl Pts',(-20.7840685504616,25.2046012934978,-14.4539046363932));
#34234=CARTESIAN_POINT('Ctrl Pts',(-20.7586063758491,25.1612630602446,-14.4570481432129));
#34235=CARTESIAN_POINT('Ctrl Pts',(-20.6782440204722,25.016851344877,-14.4675059279114));
#34236=CARTESIAN_POINT('Ctrl Pts',(-20.6277447226589,24.9134429099686,-14.4749714358207));
#34237=CARTESIAN_POINT('Ctrl Pts',(-20.500943585716,24.6141813334663,-14.4964816459474));
#34238=CARTESIAN_POINT('Ctrl Pts',(-20.4381078469019,24.4132552915898,-14.5108462901237));
#34239=CARTESIAN_POINT('Ctrl Pts',(-20.3781682190555,24.1256013568599,-14.5305701779059));
#34240=CARTESIAN_POINT('Ctrl Pts',(-20.3642748138311,24.0428914228154,-14.5361414546074));
#34241=CARTESIAN_POINT('Ctrl Pts',(-20.3532218357711,23.9566048540769,-14.5417930348087));
#34242=CARTESIAN_POINT('Ctrl Pts',(-20.3528262698671,23.9534804832394,-14.5419974558662));
#34243=CARTESIAN_POINT('Ctrl Pts',(-20.3518319846269,23.9455336732009,-14.5425168357428));
#34244=CARTESIAN_POINT('Ctrl Pts',(-20.3512395895143,23.9407104334669,-14.5428315410619));
#34245=CARTESIAN_POINT('Ctrl Pts',(-20.3504590504145,23.9342343110051,-14.5432533697134));
#34246=CARTESIAN_POINT('Ctrl Pts',(-20.3502612766049,23.9325826208282,-14.5433608910492));
#34247=CARTESIAN_POINT('Ctrl Pts',(-20.3492955422134,23.9244641338245,-14.5438890737585));
#34248=CARTESIAN_POINT('Ctrl Pts',(-20.3485458992505,23.9179951221678,-14.5443089680674));
#34249=CARTESIAN_POINT('Ctrl Pts',(-20.3435190506629,23.87343535685,-14.5471943710217));
#34250=CARTESIAN_POINT('Ctrl Pts',(-20.3399018515944,23.835271113821,-14.5496309223314));
#34251=CARTESIAN_POINT('Ctrl Pts',(-20.3365632585357,23.7918027492416,-14.5523598351374));
#34252=CARTESIAN_POINT('Ctrl Pts',(-20.3361731376469,23.786555095597,-14.5526885131588));
#34253=CARTESIAN_POINT('Ctrl Pts',(-20.3356210138338,23.7788738670702,-14.5531684700172));
#34254=CARTESIAN_POINT('Ctrl Pts',(-20.3354489202794,23.7764410608908,-14.5533203145268));
#34255=CARTESIAN_POINT('Ctrl Pts',(-20.3351487453475,23.772128075526,-14.5535892106962));
#34256=CARTESIAN_POINT('Ctrl Pts',(-20.3350195514235,23.7702479784305,-14.5537063254471));
#34257=CARTESIAN_POINT('Ctrl Pts',(-20.3347528056066,23.7663157266867,-14.5539510599603));
#34258=CARTESIAN_POINT('Ctrl Pts',(-20.3346155693772,23.7642635579001,-14.5540786614417));
#34259=CARTESIAN_POINT('Ctrl Pts',(-20.3342658271957,23.7589573775578,-14.5544082842872));
#34260=CARTESIAN_POINT('Ctrl Pts',(-20.3340562946956,23.7557031621097,-14.5546101372365));
#34261=CARTESIAN_POINT('Ctrl Pts',(-20.3331829432767,23.7418104686691,-14.5554706130383));
#34262=CARTESIAN_POINT('Ctrl Pts',(-20.3325669569016,23.7311688914989,-14.5561265645515));
#34263=CARTESIAN_POINT('Ctrl Pts',(-20.3311027193244,23.7034938316689,-14.5578247101151));
#34264=CARTESIAN_POINT('Ctrl Pts',(-20.3303368446282,23.6864560824771,-14.5588625136608));
#34265=CARTESIAN_POINT('Ctrl Pts',(-20.3277896372984,23.6176125813417,-14.5630279636414));
#34266=CARTESIAN_POINT('Ctrl Pts',(-20.3271229468472,23.5657706382902,-14.5661008593813));
#34267=CARTESIAN_POINT('Ctrl Pts',(-20.3289532862687,23.4033727761203,-14.575589149138));
#34268=CARTESIAN_POINT('Ctrl Pts',(-20.3358882773262,23.2929427909179,-14.5818426856793));
#34269=CARTESIAN_POINT('Ctrl Pts',(-20.3649018457246,23.0399419932142,-14.5961281455535));
#34270=CARTESIAN_POINT('Ctrl Pts',(-20.3908966906889,22.8980669791499,-14.604113157778));
#34271=CARTESIAN_POINT('Ctrl Pts',(-20.4698707194228,22.5865015144479,-14.6223140775673));
#34272=CARTESIAN_POINT('Ctrl Pts',(-20.5275526817546,22.4185106500106,-14.6325978444968));
#34273=CARTESIAN_POINT('Ctrl Pts',(-20.6033762912805,22.2455798925902,-14.6440802920628));
#34274=CARTESIAN_POINT('Ctrl Pts',(-20.6080587087546,22.23505453351,-14.6447827381274));
#34275=CARTESIAN_POINT('Ctrl Pts',(-20.6146265479053,22.2205016459751,-14.6457590134565));
#34276=CARTESIAN_POINT('Ctrl Pts',(-20.6164640636208,22.2164524870682,-14.6460311927266));
#34277=CARTESIAN_POINT('Ctrl Pts',(-20.6196372377056,22.209498346903,-14.6464995802726));
#34278=CARTESIAN_POINT('Ctrl Pts',(-20.6209688535655,22.2065915185166,-14.6466956488549));
#34279=CARTESIAN_POINT('Ctrl Pts',(-20.623720428987,22.2006085440789,-14.6470997915825));
#34280=CARTESIAN_POINT('Ctrl Pts',(-20.6251409173961,22.197532647445,-14.6473078838005));
#34281=CARTESIAN_POINT('Ctrl Pts',(-20.6284488043302,22.1903993904504,-14.647791210669));
#34282=CARTESIAN_POINT('Ctrl Pts',(-20.6303398049179,22.1863437170456,-14.6480665698329));
#34283=CARTESIAN_POINT('Ctrl Pts',(-20.6362476362963,22.1737416497778,-14.6489239353258));
#34284=CARTESIAN_POINT('Ctrl Pts',(-20.6402935611782,22.1652090214372,-14.6495069508751));
#34285=CARTESIAN_POINT('Ctrl Pts',(-20.6958608318373,22.0493390258184,-14.6574586241757));
#34286=CARTESIAN_POINT('Ctrl Pts',(-20.7532480299174,21.9449322694041,-14.6650332158471));
#34287=CARTESIAN_POINT('Ctrl Pts',(-20.9283046359657,21.664442208574,-14.6865859010637));
#34288=CARTESIAN_POINT('Ctrl Pts',(-21.0577327806941,21.4964226521994,-14.7009457752117));
#34289=CARTESIAN_POINT('Ctrl Pts',(-21.3063803895804,21.2320482366041,-14.7254769411422));
#34290=CARTESIAN_POINT('Ctrl Pts',(-21.4177441317677,21.1292091593249,-14.7356337009553));
#34291=CARTESIAN_POINT('Ctrl Pts',(-21.5376361749517,21.0332110728419,-14.7454597151126));
#34292=CARTESIAN_POINT('Ctrl Pts',(-21.5393374965901,21.0318516448897,-14.7455989358607));
#34293=CARTESIAN_POINT('Ctrl Pts',(-21.5629531434609,21.0130209326772,-14.7475284347227));
#34294=CARTESIAN_POINT('Ctrl Pts',(-21.5850940099488,20.9958337796463,-14.7493017469318));
#34295=CARTESIAN_POINT('Ctrl Pts',(-21.6112322966511,20.976084612155,-14.7513511528556));
#34296=CARTESIAN_POINT('Ctrl Pts',(-21.6150137202537,20.9732405617439,-14.7516465763119));
#34297=CARTESIAN_POINT('Ctrl Pts',(-21.6207170836991,20.9689706323066,-14.7520905343305));
#34298=CARTESIAN_POINT('Ctrl Pts',(-21.6226343494491,20.9675385651963,-14.7522395028464));
#34299=CARTESIAN_POINT('Ctrl Pts',(-21.6260552883029,20.9649892878113,-14.7525048132422));
#34300=CARTESIAN_POINT('Ctrl Pts',(-21.6275583389808,20.9638712541134,-14.752621213326));
#34301=CARTESIAN_POINT('Ctrl Pts',(-21.6307506753295,20.961500977828,-14.7528680773018));
#34302=CARTESIAN_POINT('Ctrl Pts',(-21.6324402075769,20.9602490811644,-14.7529985166548));
#34303=CARTESIAN_POINT('Ctrl Pts',(-21.6358869016775,20.9577003979183,-14.7532641865188));
#34304=CARTESIAN_POINT('Ctrl Pts',(-21.637644159214,20.9564037417062,-14.7533994078373));
#34305=CARTESIAN_POINT('Ctrl Pts',(-21.6454429721302,20.950661338984,-14.7539985268956));
#34306=CARTESIAN_POINT('Ctrl Pts',(-21.6514987850783,20.9462348589824,-14.7544610842294));
#34307=CARTESIAN_POINT('Ctrl Pts',(-21.6663654646946,20.9354475351625,-14.7555902850245));
#34308=CARTESIAN_POINT('Ctrl Pts',(-21.675193226777,20.9291099827602,-14.7562553692522));
#34309=CARTESIAN_POINT('Ctrl Pts',(-21.7088209878239,20.9052250527912,-14.758769053955));
#34310=CARTESIAN_POINT('Ctrl Pts',(-21.733837475804,20.8879833888735,-14.7605983562596));
#34311=CARTESIAN_POINT('Ctrl Pts',(-21.8281348066066,20.8249406155197,-14.7673583511184));
#34312=CARTESIAN_POINT('Ctrl Pts',(-21.8989383414206,20.7814661488401,-14.7721660975756));
#34313=CARTESIAN_POINT('Ctrl Pts',(-22.0862793777882,20.6761819879954,-14.7844173473697));
#34314=CARTESIAN_POINT('Ctrl Pts',(-22.2050705579157,20.6187022788282,-14.7917421975329));
#34315=CARTESIAN_POINT('Ctrl Pts',(-22.552871131831,20.4760169153364,-14.8127664670626));
#34316=CARTESIAN_POINT('Ctrl Pts',(-22.7884438548675,20.409342345846,-14.8265787742771));
#34317=CARTESIAN_POINT('Ctrl Pts',(-23.0441168838522,20.3674596182057,-14.8422973047826));
#34318=CARTESIAN_POINT('Ctrl Pts',(-23.0589842438616,20.3651309513571,-14.843213559513));
#34319=CARTESIAN_POINT('Ctrl Pts',(-23.0793359235312,20.3620891597868,-14.8444710154158));
#34320=CARTESIAN_POINT('Ctrl Pts',(-23.0848067409135,20.3612858725619,-14.8448093537062));
#34321=CARTESIAN_POINT('Ctrl Pts',(-23.0934830818958,20.3600347165424,-14.8453464456185));
#34322=CARTESIAN_POINT('Ctrl Pts',(-23.0966872768557,20.3595775877582,-14.845544905345));
#34323=CARTESIAN_POINT('Ctrl Pts',(-23.1028963632434,20.3587013060153,-14.8459296962322));
#34324=CARTESIAN_POINT('Ctrl Pts',(-23.1059011699012,20.3582815677351,-14.8461160086317));
#34325=CARTESIAN_POINT('Ctrl Pts',(-23.1130487765332,20.3572934143711,-14.8465594292215));
#34326=CARTESIAN_POINT('Ctrl Pts',(-23.1171920912025,20.3567288190781,-14.8468166581291));
#34327=CARTESIAN_POINT('Ctrl Pts',(-23.1257733488591,20.3555764876093,-14.847349799984));
#34328=CARTESIAN_POINT('Ctrl Pts',(-23.1302114388364,20.3549899316414,-14.8476257497697));
#34329=CARTESIAN_POINT('Ctrl Pts',(-23.1553950791224,20.3517149344969,-14.8491928551748));
#34330=CARTESIAN_POINT('Ctrl Pts',(-23.1761648081041,20.3492193374951,-14.8504900993998));
#34331=CARTESIAN_POINT('Ctrl Pts',(-23.311918586412,20.3342470239319,-14.8590018759428));
#34332=CARTESIAN_POINT('Ctrl Pts',(-23.4274660116811,20.3277670725905,-14.866404800644));
#34333=CARTESIAN_POINT('Ctrl Pts',(-23.5684729234957,20.3274541636857,-14.8756362961598));
#34334=CARTESIAN_POINT('Ctrl Pts',(-23.5938442036817,20.3276974861467,-14.8773048826949));
#34335=CARTESIAN_POINT('Ctrl Pts',(-23.7726234968472,20.3315236908059,-14.8891137194571));
#34336=CARTESIAN_POINT('Ctrl Pts',(-23.9255973301185,20.3457597105112,-14.899496897803));
#34337=CARTESIAN_POINT('Ctrl Pts',(-24.2679048778954,20.4024672787699,-14.9229802326792));
#34338=CARTESIAN_POINT('Ctrl Pts',(-24.4556342924474,20.4512398190323,-14.9360400281714));
#34339=CARTESIAN_POINT('Ctrl Pts',(-24.6485254144695,20.5203940579723,-14.9489512266214));
#34340=CARTESIAN_POINT('Ctrl Pts',(-24.6591609075802,20.5242703905047,-14.9496613496025));
#34341=CARTESIAN_POINT('Ctrl Pts',(-24.6730366985582,20.5294107005456,-14.9505853057575));
#34342=CARTESIAN_POINT('Ctrl Pts',(-24.6762955155689,20.5306239364997,-14.9508021205004));
#34343=CARTESIAN_POINT('Ctrl Pts',(-24.6813146332027,20.532501775705,-14.9511357630521));
#34344=CARTESIAN_POINT('Ctrl Pts',(-24.683076313157,20.5331626452412,-14.951252814816));
#34345=CARTESIAN_POINT('Ctrl Pts',(-24.6865834323999,20.5344817966302,-14.9514857287252));
#34346=CARTESIAN_POINT('Ctrl Pts',(-24.6883288685655,20.53514004725,-14.9516015913762));
#34347=CARTESIAN_POINT('Ctrl Pts',(-24.69222834417,20.5366145122505,-14.9518603180991));
#34348=CARTESIAN_POINT('Ctrl Pts',(-24.6943820756408,20.5374315188784,-14.952003133377));
#34349=CARTESIAN_POINT('Ctrl Pts',(-24.698838934613,20.5391276729787,-14.9522985024685));
#34350=CARTESIAN_POINT('Ctrl Pts',(-24.7011419341183,20.5400071557773,-14.9524510359999));
#34351=CARTESIAN_POINT('Ctrl Pts',(-24.7138351372967,20.544871205589,-14.9532912381569));
#34352=CARTESIAN_POINT('Ctrl Pts',(-24.7242058289423,20.5489069901411,-14.9539758537043));
#34353=CARTESIAN_POINT('Ctrl Pts',(-24.7513187280967,20.5596200853037,-14.9557613544173));
#34354=CARTESIAN_POINT('Ctrl Pts',(-24.7680264403715,20.5663843746866,-14.9568572716985));
#34355=CARTESIAN_POINT('Ctrl Pts',(-24.8370256988262,20.5949955278656,-14.961368550071));
#34356=CARTESIAN_POINT('Ctrl Pts',(-24.8887962148524,20.6180808486393,-14.9647184312394));
#34357=CARTESIAN_POINT('Ctrl Pts',(-25.0121590636445,20.6770392084254,-14.9726779890572));
#34358=CARTESIAN_POINT('Ctrl Pts',(-25.083076828445,20.7142383302666,-14.9772349529812));
#34359=CARTESIAN_POINT('Ctrl Pts',(-25.216444826549,20.7906609473234,-14.9859011986569));
#34360=CARTESIAN_POINT('Ctrl Pts',(-25.2790773712428,20.8294608307051,-14.9900145213348));
#34361=CARTESIAN_POINT('Ctrl Pts',(-25.5607806434269,21.0176296074321,-15.0089432124281));
#34362=CARTESIAN_POINT('Ctrl Pts',(-25.7621869099377,21.1914981656296,-15.0238165702641));
#34363=CARTESIAN_POINT('Ctrl Pts',(-25.9512201375177,21.4004267992605,-15.0408932231552));
#34364=CARTESIAN_POINT('Ctrl Pts',(-25.9623213938666,21.4128896912224,-15.0419087764182));
#34365=CARTESIAN_POINT('Ctrl Pts',(-25.9771297591106,21.4297766926449,-15.0432809342589));
#34366=CARTESIAN_POINT('Ctrl Pts',(-25.9809226566522,21.4341255024506,-15.043633953751));
#34367=CARTESIAN_POINT('Ctrl Pts',(-25.9868561499726,21.4409656477735,-15.0441886815578));
#34368=CARTESIAN_POINT('Ctrl Pts',(-25.9890046645673,21.4434501238814,-15.0443900607696));
#34369=CARTESIAN_POINT('Ctrl Pts',(-25.9931220935282,21.4482261298337,-15.0447769733547));
#34370=CARTESIAN_POINT('Ctrl Pts',(-25.9950915921741,21.4505171534841,-15.0449624822638));
#34371=CARTESIAN_POINT('Ctrl Pts',(-25.9997109128501,21.4559058987425,-15.0453986087899));
#34372=CARTESIAN_POINT('Ctrl Pts',(-26.0023580803015,21.4590058800009,-15.0456493355794));
#34373=CARTESIAN_POINT('Ctrl Pts',(-26.0078056071717,21.4654098033826,-15.0461669530468));
#34374=CARTESIAN_POINT('Ctrl Pts',(-26.0106052009037,21.4687143832562,-15.0464338745385));
#34375=CARTESIAN_POINT('Ctrl Pts',(-26.0178021896918,21.4772443576292,-15.0471224065906));
#34376=CARTESIAN_POINT('Ctrl Pts',(-26.0221896347545,21.4824780851489,-15.0475444241729));
#34377=CARTESIAN_POINT('Ctrl Pts',(-26.0620951948564,21.5303894381937,-15.0514037529148));
#34378=CARTESIAN_POINT('Ctrl Pts',(-26.0965195771706,21.5739620689928,-15.0548852025836));
#34379=CARTESIAN_POINT('Ctrl Pts',(-26.2147742025962,21.7318640729124,-15.06741337013));
#34380=CARTESIAN_POINT('Ctrl Pts',(-26.2921592082476,21.8507964276416,-15.0767000472682));
#34381=CARTESIAN_POINT('Ctrl Pts',(-26.3856244079427,22.0175338694134,-15.0894727940733));
#34382=CARTESIAN_POINT('Ctrl Pts',(-26.4087952500272,22.0611946108251,-15.0927948322467));
#34383=CARTESIAN_POINT('Ctrl Pts',(-26.4418197668885,22.1270364473578,-15.0977634676192));
#34384=CARTESIAN_POINT('Ctrl Pts',(-26.4524422547958,22.1488247255272,-15.0994010956555));
#34385=CARTESIAN_POINT('Ctrl Pts',(-26.4750002078681,22.1964510172113,-15.1029647924168));
#34386=CARTESIAN_POINT('Ctrl Pts',(-26.4868412768271,22.2223315836779,-15.1048912881772));
#34387=CARTESIAN_POINT('Ctrl Pts',(-26.5799095072105,22.433081896117,-15.1204865646759));
#34388=CARTESIAN_POINT('Ctrl Pts',(-26.6439502866254,22.6250792042164,-15.1341522072137));
#34389=CARTESIAN_POINT('Ctrl Pts',(-26.6923899224194,22.8338431984258,-15.1476683709772));
#34390=CARTESIAN_POINT('Ctrl Pts',(-26.6951090005671,22.8458751350598,-15.1484426567889));
#34391=CARTESIAN_POINT('Ctrl Pts',(-26.6985314585964,22.8614344926445,-15.1494376059124));
#34392=CARTESIAN_POINT('Ctrl Pts',(-26.6992980621516,22.8649476798918,-15.1496618417252));
#34393=CARTESIAN_POINT('Ctrl Pts',(-26.7004618933235,22.8703244685306,-15.150004380943));
#34394=CARTESIAN_POINT('Ctrl Pts',(-26.7008633475779,22.8721871365773,-15.1501229277464));
#34395=CARTESIAN_POINT('Ctrl Pts',(-26.7016150688771,22.8756900551035,-15.1503456422033));
#34396=CARTESIAN_POINT('Ctrl Pts',(-26.7019657060022,22.8773302163331,-15.1504498308238));
#34397=CARTESIAN_POINT('Ctrl Pts',(-26.7027704139927,22.8811087928533,-15.150689646411));
#34398=CARTESIAN_POINT('Ctrl Pts',(-26.7032235887357,22.8832473930572,-15.1508252209289));
#34399=CARTESIAN_POINT('Ctrl Pts',(-26.7041493730521,22.8876383355476,-15.151103262638));
#34400=CARTESIAN_POINT('Ctrl Pts',(-26.7046217469071,22.8898907270308,-15.1512457161832));
#34401=CARTESIAN_POINT('Ctrl Pts',(-26.7058157791786,22.8956146730001,-15.1516072983909));
#34402=CARTESIAN_POINT('Ctrl Pts',(-26.7065341241278,22.8990869272138,-15.1518262380448));
#34403=CARTESIAN_POINT('Ctrl Pts',(-26.7085761166034,22.9090400483051,-15.1524526865943));
#34404=CARTESIAN_POINT('Ctrl Pts',(-26.7098855534321,22.9155238608583,-15.1528593980918));
#34405=CARTESIAN_POINT('Ctrl Pts',(-26.7520963747704,23.1279028300848,-15.1661375867121));
#34406=CARTESIAN_POINT('Ctrl Pts',(-26.7728090541682,23.3373294056183,-15.1779030483283));
#34407=CARTESIAN_POINT('Ctrl Pts',(-26.7730011825842,23.5473036867677,-15.1896424574236));
#34408=CARTESIAN_POINT('Ctrl Pts',(-26.7730011815105,23.5473025134888,-15.189642391827));
#34409=CARTESIAN_POINT('Ctrl Pts',(-26.7731220480874,23.6793432570931,-15.1970246309133));
#34410=CARTESIAN_POINT('Ctrl Pts',(-26.7651279187396,23.8112675563302,-15.2043751941072));
#34411=CARTESIAN_POINT('Ctrl Pts',(-26.7350653072654,24.0565379137957,-15.2184371318526));
#34412=CARTESIAN_POINT('Ctrl Pts',(-26.7149616201925,24.1699055028723,-15.2250978832352));
#34413=CARTESIAN_POINT('Ctrl Pts',(-26.6812839765029,24.3143648265673,-15.2339301582693));
#34414=CARTESIAN_POINT('Ctrl Pts',(-26.6732251997283,24.346661408296,-15.2359270959144));
#34415=CARTESIAN_POINT('Ctrl Pts',(-26.6611527625449,24.3920388695957,-15.2387668684762));
#34416=CARTESIAN_POINT('Ctrl Pts',(-26.6575536823376,24.4052285753785,-15.239596377073));
#34417=CARTESIAN_POINT('Ctrl Pts',(-26.6519660228538,24.425204519791,-15.2408590325723));
#34418=CARTESIAN_POINT('Ctrl Pts',(-26.650038824424,24.4320078837442,-15.241290187561));
#34419=CARTESIAN_POINT('Ctrl Pts',(-26.646867091773,24.4430657698963,-15.2419928163983));
#34420=CARTESIAN_POINT('Ctrl Pts',(-26.6456361352801,24.4473241890011,-15.2422638474578));
#34421=CARTESIAN_POINT('Ctrl Pts',(-26.6432357776294,24.455564314657,-15.2427891696531));
#34422=CARTESIAN_POINT('Ctrl Pts',(-26.6420674632112,24.4595463307494,-15.243043424863));
#34423=CARTESIAN_POINT('Ctrl Pts',(-26.6399511510272,24.4667082122633,-15.243501432421));
#34424=CARTESIAN_POINT('Ctrl Pts',(-26.639005925742,24.4698888964497,-15.2437050937192));
#34425=CARTESIAN_POINT('Ctrl Pts',(-26.6371054303765,24.4762480823514,-15.2441127876199));
#34426=CARTESIAN_POINT('Ctrl Pts',(-26.6361501590587,24.4794265795647,-15.2443168200571));
#34427=CARTESIAN_POINT('Ctrl Pts',(-26.6334711232074,24.4882908994902,-15.2448865508614));
#34428=CARTESIAN_POINT('Ctrl Pts',(-26.6317365492648,24.4939734179788,-15.2452526036811));
#34429=CARTESIAN_POINT('Ctrl Pts',(-26.6247045969124,24.5167842186546,-15.2467253527325));
#34430=CARTESIAN_POINT('Ctrl Pts',(-26.6192801210261,24.5338727013903,-15.2478362215902));
#34431=CARTESIAN_POINT('Ctrl Pts',(-26.5278060646413,24.8139144447451,-15.2661680402064));
#34432=CARTESIAN_POINT('Ctrl Pts',(-26.4084081479474,25.0646981230958,-15.2845861006355));
#34433=CARTESIAN_POINT('Ctrl Pts',(-26.2363188052158,25.3314996010499,-15.3060742672728));
#34434=CARTESIAN_POINT('Ctrl Pts',(-26.2134777109189,25.3654728514333,-15.3088462201104));
#34435=CARTESIAN_POINT('Ctrl Pts',(-26.1681622694999,25.4301766609059,-15.3141862757685));
#34436=CARTESIAN_POINT('Ctrl Pts',(-26.1457780977653,25.4609626710608,-15.3167546240849));
#34437=CARTESIAN_POINT('Ctrl Pts',(-26.0640199570113,25.5693197165789,-15.3258783293613));
#34438=CARTESIAN_POINT('Ctrl Pts',(-26.0016666703096,25.6445855410796,-15.3323740859227));
#34439=CARTESIAN_POINT('Ctrl Pts',(-25.9050914751152,25.7509257930706,-15.341663617091));
#34440=CARTESIAN_POINT('Ctrl Pts',(-25.8734710729006,25.7842814948884,-15.3445947125887));
#34441=CARTESIAN_POINT('Ctrl Pts',(-25.838409605783,25.8197172051514,-15.3477164718293));
#34442=CARTESIAN_POINT('Ctrl Pts',(-25.8356681104533,25.8224779458012,-15.3479597360686));
#34443=CARTESIAN_POINT('Ctrl Pts',(-25.8311948278581,25.8269663450178,-15.3483553097152));
#34444=CARTESIAN_POINT('Ctrl Pts',(-25.8294660713694,25.8286969981809,-15.3485078548546));
#34445=CARTESIAN_POINT('Ctrl Pts',(-25.8261152566336,25.8320438593307,-15.3488028901907));
#34446=CARTESIAN_POINT('Ctrl Pts',(-25.8244934437939,25.833660309437,-15.3489453996436));
#34447=CARTESIAN_POINT('Ctrl Pts',(-25.8215478010534,25.8365899606117,-15.3492037079574));
#34448=CARTESIAN_POINT('Ctrl Pts',(-25.8202245586377,25.8379037368452,-15.3493195528149));
#34449=CARTESIAN_POINT('Ctrl Pts',(-25.8175580449862,25.8405465832599,-15.3495526086458));
#34450=CARTESIAN_POINT('Ctrl Pts',(-25.8162147504733,25.84187561509,-15.3496698167091));
#34451=CARTESIAN_POINT('Ctrl Pts',(-25.8123676828936,25.8456751458137,-15.3500049285637));
#34452=CARTESIAN_POINT('Ctrl Pts',(-25.8098610231963,25.8481427379724,-15.3502226010809));
#34453=CARTESIAN_POINT('Ctrl Pts',(-25.7990309814348,25.8587691312998,-15.3511601614588));
#34454=CARTESIAN_POINT('Ctrl Pts',(-25.7906672773983,25.8668869835887,-15.3518768523136));
#34455=CARTESIAN_POINT('Ctrl Pts',(-25.6464820729941,26.0053226680869,-15.3641105584333));
#34456=CARTESIAN_POINT('Ctrl Pts',(-25.4995212726199,26.1235620252855,-15.3747503598337));
#34457=CARTESIAN_POINT('Ctrl Pts',(-25.2785814003165,26.2714685859045,-15.3896428622088));
#34458=CARTESIAN_POINT('Ctrl Pts',(-25.212569152684,26.3122881902462,-15.3939661692397));
#34459=CARTESIAN_POINT('Ctrl Pts',(-25.0756198261285,26.3902832227929,-15.4027931730439));
#34460=CARTESIAN_POINT('Ctrl Pts',(-25.0046429880872,26.4272765876484,-15.4072952460173));
#34461=CARTESIAN_POINT('Ctrl Pts',(-24.8329019432875,26.5088080197654,-15.4181349733544));
#34462=CARTESIAN_POINT('Ctrl Pts',(-24.7310929245895,26.5508945591447,-15.4245205646822));
#34463=CARTESIAN_POINT('Ctrl Pts',(-24.5967800033113,26.5985223569168,-15.4330112964077));
#34464=CARTESIAN_POINT('Ctrl Pts',(-24.5660625013207,26.6088958040356,-15.434957216392));
#34465=CARTESIAN_POINT('Ctrl Pts',(-24.5159258259378,26.624988648344,-15.4381424830605));
#34466=CARTESIAN_POINT('Ctrl Pts',(-24.4965996383479,26.6309917648829,-15.4393724888845));
#34467=CARTESIAN_POINT('Ctrl Pts',(-24.4729722702765,26.6380876152972,-15.4408792779505));
#34468=CARTESIAN_POINT('Ctrl Pts',(-24.468723398956,26.6393540977132,-15.4411503604168));
#34469=CARTESIAN_POINT('Ctrl Pts',(-24.4604919554392,26.6417892014652,-15.4416757712926));
#34470=CARTESIAN_POINT('Ctrl Pts',(-24.45650971057,26.6429589054967,-15.4419300637408));
#34471=CARTESIAN_POINT('Ctrl Pts',(-24.4493397089256,26.645049911304,-15.4423881116874));
#34472=CARTESIAN_POINT('Ctrl Pts',(-24.446152762575,26.645973990301,-15.4425917760666));
#34473=CARTESIAN_POINT('Ctrl Pts',(-24.4393088061563,26.6479469932796,-15.443029296651));
#34474=CARTESIAN_POINT('Ctrl Pts',(-24.4356513574372,26.6489943659993,-15.4432632031684));
#34475=CARTESIAN_POINT('Ctrl Pts',(-24.4257755539346,26.6518035585283,-15.4438950506039));
#34476=CARTESIAN_POINT('Ctrl Pts',(-24.4195537639769,26.653553145735,-15.4442933898549));
#34477=CARTESIAN_POINT('Ctrl Pts',(-24.3985860303906,26.6593813350175,-15.4456367579802));
#34478=CARTESIAN_POINT('Ctrl Pts',(-24.3838164902552,26.6633735949777,-15.4465845915601));
#34479=CARTESIAN_POINT('Ctrl Pts',(-24.1126700816536,26.7345975598202,-15.4640158352573));
#34480=CARTESIAN_POINT('Ctrl Pts',(-23.8490505375573,26.7700392607985,-15.4815905805253));
#34481=CARTESIAN_POINT('Ctrl Pts',(-23.440999015051,26.7743292555715,-15.509192847489));
#34482=CARTESIAN_POINT('Ctrl Pts',(-23.2979191699941,26.7662963723533,-15.5189181716028));
#34483=CARTESIAN_POINT('Ctrl Pts',(-23.0680289325428,26.7379486492674,-15.5342477704093));
#34484=CARTESIAN_POINT('Ctrl Pts',(-22.9806882689219,26.7235073268375,-15.5399989779649));
#34485=CARTESIAN_POINT('Ctrl Pts',(-22.885537460668,26.7037183922766,-15.5461058474224));
#34486=CARTESIAN_POINT('Ctrl Pts',(-22.8770376595901,26.7019147597314,-15.5466499620324));
#34487=CARTESIAN_POINT('Ctrl Pts',(-22.866311974197,26.6995934305078,-15.5473346929052));
#34488=CARTESIAN_POINT('Ctrl Pts',(-22.864079313774,26.6991077360846,-15.5474771239213));
#34489=CARTESIAN_POINT('Ctrl Pts',(-22.8597230375646,26.6981552156827,-15.5477548265462));
#34490=CARTESIAN_POINT('Ctrl Pts',(-22.8575993746171,26.697688614315,-15.5478901109868));
#34491=CARTESIAN_POINT('Ctrl Pts',(-22.8538386914514,26.6968583439427,-15.5481295101978));
#34492=CARTESIAN_POINT('Ctrl Pts',(-22.8522014918766,26.6964955484355,-15.5482336748758));
#34493=CARTESIAN_POINT('Ctrl Pts',(-22.8486957753428,26.6957158274978,-15.5484565999094));
#34494=CARTESIAN_POINT('Ctrl Pts',(-22.8468273518182,26.6952985160948,-15.5485753372829));
#34495=CARTESIAN_POINT('Ctrl Pts',(-22.8414068340739,26.6940827742929,-15.5489195971299));
#34496=CARTESIAN_POINT('Ctrl Pts',(-22.837855704882,26.6932799860401,-15.5491448677272));
#34497=CARTESIAN_POINT('Ctrl Pts',(-22.8218855626145,26.6896412293243,-15.5501568005669));
#34498=CARTESIAN_POINT('Ctrl Pts',(-22.8094818467412,26.6867376092168,-15.5509396078038));
#34499=CARTESIAN_POINT('Ctrl Pts',(-22.7892319830312,26.6818704351163,-15.5522129332371));
#34500=CARTESIAN_POINT('Ctrl Pts',(-22.781375584718,26.67995079383,-15.5527057991604));
#34501=CARTESIAN_POINT('Ctrl Pts',(-22.7649385393865,26.6758689182068,-15.5537347156383));
#34502=CARTESIAN_POINT('Ctrl Pts',(-22.7563593898575,26.6737008737209,-15.5542704604599));
#34503=CARTESIAN_POINT('Ctrl Pts',(-22.7452714847707,26.6708502043111,-15.5549613314683));
#34504=CARTESIAN_POINT('Ctrl Pts',(-22.7427545702257,26.6701998649943,-15.5551180539424));
#34505=CARTESIAN_POINT('Ctrl Pts',(-22.5945172986406,26.6317058078638,-15.5643425403541));
#34506=CARTESIAN_POINT('Ctrl Pts',(-22.4516080363896,26.5836953813842,-15.5729035730602));
#34507=CARTESIAN_POINT('Ctrl Pts',(-22.2318984448752,26.492308443191,-15.5862678891349));
#34508=CARTESIAN_POINT('Ctrl Pts',(-22.1526577784157,26.4555010185249,-15.5911313958584));
#34509=CARTESIAN_POINT('Ctrl Pts',(-22.0750358970872,26.4155367136697,-15.5960174792939));
#34510=CARTESIAN_POINT('Ctrl Pts',(-22.0750360164986,26.4155367751497,-15.845717117064));
#34511=CARTESIAN_POINT('Ctrl Pts',(-22.0813799877625,26.4188030239352,-15.845291974261));
#34512=CARTESIAN_POINT('Ctrl Pts',(-22.087734945045,26.4220482748863,-15.8448661251044));
#34513=CARTESIAN_POINT('Ctrl Pts',(-22.1320715052549,26.4445040355075,-15.841895188303));
#34514=CARTESIAN_POINT('Ctrl Pts',(-22.1704180126622,26.4629807419879,-15.8393259637509));
#34515=CARTESIAN_POINT('Ctrl Pts',(-22.2160638236638,26.48387084459,-15.836264188936));
#34516=CARTESIAN_POINT('Ctrl Pts',(-22.2230210375805,26.4870249903368,-15.8357974293847));
#34517=CARTESIAN_POINT('Ctrl Pts',(-22.2336947479676,26.4918183840204,-15.8350811657446));
#34518=CARTESIAN_POINT('Ctrl Pts',(-22.237403272247,26.4934754052109,-15.8348322734637));
#34519=CARTESIAN_POINT('Ctrl Pts',(-22.2441700864917,26.4964835795927,-15.834378069296));
#34520=CARTESIAN_POINT('Ctrl Pts',(-22.2472273696368,26.4978369949756,-15.8341728354432));
#34521=CARTESIAN_POINT('Ctrl Pts',(-22.2533768005446,26.5005478227503,-15.8337599807963));
#34522=CARTESIAN_POINT('Ctrl Pts',(-22.2564689865682,26.5019051373875,-15.8335523569673));
#34523=CARTESIAN_POINT('Ctrl Pts',(-22.2652706698497,26.5057521466903,-15.8329613003999));
#34524=CARTESIAN_POINT('Ctrl Pts',(-22.2709852364139,26.5082301424725,-15.8325774678101));
#34525=CARTESIAN_POINT('Ctrl Pts',(-22.2952451664967,26.5186664755345,-15.830947605066));
#34526=CARTESIAN_POINT('Ctrl Pts',(-22.3138575638419,26.5264669531227,-15.8296962032077));
#34527=CARTESIAN_POINT('Ctrl Pts',(-22.3369201692063,26.5358788487194,-15.8281441600935));
#34528=CARTESIAN_POINT('Ctrl Pts',(-22.3413025869535,26.5376560795097,-15.8278491734788));
#34529=CARTESIAN_POINT('Ctrl Pts',(-22.3564762710108,26.5437707071188,-15.8268275855064));
#34530=CARTESIAN_POINT('Ctrl Pts',(-22.3672869966791,26.5480592907115,-15.8260993437155));
#34531=CARTESIAN_POINT('Ctrl Pts',(-22.3817804029303,26.5537181770755,-15.8251224591094));
#34532=CARTESIAN_POINT('Ctrl Pts',(-22.3854428166297,26.5551404374495,-15.8248755568932));
#34533=CARTESIAN_POINT('Ctrl Pts',(-22.3960086662549,26.5592213563241,-15.8241631167938));
#34534=CARTESIAN_POINT('Ctrl Pts',(-22.4029186337065,26.5618629337149,-15.8236970134867));
#34535=CARTESIAN_POINT('Ctrl Pts',(-22.4241541826484,26.5698972748957,-15.8222640447014));
#34536=CARTESIAN_POINT('Ctrl Pts',(-22.4385089835142,26.5752117276235,-15.8212946179217));
#34537=CARTESIAN_POINT('Ctrl Pts',(-22.4596539947069,26.5828692200828,-15.819865444471));
#34538=CARTESIAN_POINT('Ctrl Pts',(-22.46641519784,26.5852921986497,-15.819408284113));
#34539=CARTESIAN_POINT('Ctrl Pts',(-22.4927574582739,26.5946330939844,-15.8176264506867));
#34540=CARTESIAN_POINT('Ctrl Pts',(-22.5123967784389,26.6013841647801,-15.8162965187948));
#34541=CARTESIAN_POINT('Ctrl Pts',(-22.5698463968849,26.6205137861791,-15.8124017477719));
#34542=CARTESIAN_POINT('Ctrl Pts',(-22.6078213665928,26.6323822581137,-15.8098216721482));
#34543=CARTESIAN_POINT('Ctrl Pts',(-22.8699560189756,26.7090108476705,-15.7919769809153));
#34544=CARTESIAN_POINT('Ctrl Pts',(-23.1003375778773,26.7499573158297,-15.7760483519954));
#34545=CARTESIAN_POINT('Ctrl Pts',(-23.4062189828573,26.770616713691,-15.7554066500887));
#34546=CARTESIAN_POINT('Ctrl Pts',(-23.4795079893906,26.7730599104725,-15.7505051089618));
#34547=CARTESIAN_POINT('Ctrl Pts',(-23.6243141498091,26.7729445556268,-15.7409778722624));
#34548=CARTESIAN_POINT('Ctrl Pts',(-23.6957933851422,26.770508527861,-15.7363509174702));
#34549=CARTESIAN_POINT('Ctrl Pts',(-23.7746016641019,26.7651928086171,-15.7313752416781));
#34550=CARTESIAN_POINT('Ctrl Pts',(-23.7820633175761,26.7646634076626,-15.7309053902673));
#34551=CARTESIAN_POINT('Ctrl Pts',(-23.7950761139163,26.7636946087277,-15.7300882522249));
#34552=CARTESIAN_POINT('Ctrl Pts',(-23.8006280502888,26.763266797093,-15.7297403373715));
#34553=CARTESIAN_POINT('Ctrl Pts',(-23.8086867627112,26.7626248077594,-15.7292364053266));
#34554=CARTESIAN_POINT('Ctrl Pts',(-23.811194401649,26.7624220839442,-15.729079746842));
#34555=CARTESIAN_POINT('Ctrl Pts',(-23.815593671767,26.7620612503294,-15.7288051808095));
#34556=CARTESIAN_POINT('Ctrl Pts',(-23.8174854030659,26.7619044054579,-15.7286872014067));
#34557=CARTESIAN_POINT('Ctrl Pts',(-23.8211469482804,26.7615975664508,-15.7284590153289));
#34558=CARTESIAN_POINT('Ctrl Pts',(-23.822916772335,26.7614477809913,-15.7283487969583));
#34559=CARTESIAN_POINT('Ctrl Pts',(-23.8271407295687,26.7610867777635,-15.7280859242587));
#34560=CARTESIAN_POINT('Ctrl Pts',(-23.8295947506074,26.7608742089836,-15.7279333466906));
#34561=CARTESIAN_POINT('Ctrl Pts',(-23.837011391256,26.7602232073652,-15.7274726535677));
#34562=CARTESIAN_POINT('Ctrl Pts',(-23.8419732699312,26.7597760779349,-15.7271650267466));
#34563=CARTESIAN_POINT('Ctrl Pts',(-23.8925684617701,26.7550984965022,-15.7240340190975));
#34564=CARTESIAN_POINT('Ctrl Pts',(-23.9381105100857,26.7499063525603,-15.7212638077876));
#34565=CARTESIAN_POINT('Ctrl Pts',(-24.2931767198342,26.7017327882941,-15.6999346360151));
#34566=CARTESIAN_POINT('Ctrl Pts',(-24.5951056189811,26.6149064423424,-15.6832574142852));
#34567=CARTESIAN_POINT('Ctrl Pts',(-24.9646544621277,26.4475363753833,-15.660098436646));
#34568=CARTESIAN_POINT('Ctrl Pts',(-25.0477579937007,26.4054691248088,-15.6547045569244));
#34569=CARTESIAN_POINT('Ctrl Pts',(-25.1806446106736,26.3308027271028,-15.6456772364674));
#34570=CARTESIAN_POINT('Ctrl Pts',(-25.2315544303152,26.3003181579484,-15.6421170677056));
#34571=CARTESIAN_POINT('Ctrl Pts',(-25.28971676101,26.2632719863008,-15.63791835879));
#34572=CARTESIAN_POINT('Ctrl Pts',(-25.2978186897424,26.258060295591,-15.6373304609273));
#34573=CARTESIAN_POINT('Ctrl Pts',(-25.3097801721264,26.250289843826,-15.636457966413));
#34574=CARTESIAN_POINT('Ctrl Pts',(-25.3136578258867,26.2477589306501,-15.6361744125689));
#34575=CARTESIAN_POINT('Ctrl Pts',(-25.3203846692324,26.2433476714415,-15.6356812705419));
#34576=CARTESIAN_POINT('Ctrl Pts',(-25.3232363578746,26.2414711344899,-15.6354718256897));
#34577=CARTESIAN_POINT('Ctrl Pts',(-25.3287184833864,26.2378511587163,-15.6350684346364));
#34578=CARTESIAN_POINT('Ctrl Pts',(-25.331349352985,26.2361083793467,-15.6348745134316));
#34579=CARTESIAN_POINT('Ctrl Pts',(-25.3375480649989,26.2319890244876,-15.6344168160085));
#34580=CARTESIAN_POINT('Ctrl Pts',(-25.3411137275117,26.2296091927585,-15.6341529169986));
#34581=CARTESIAN_POINT('Ctrl Pts',(-25.3534603374699,26.2213330328376,-15.6332369708439));
#34582=CARTESIAN_POINT('Ctrl Pts',(-25.3622169262856,26.2154006444354,-15.6325835590232));
#34583=CARTESIAN_POINT('Ctrl Pts',(-25.4663079619787,26.1441312372011,-15.6247705420027));
#34584=CARTESIAN_POINT('Ctrl Pts',(-25.558079226563,26.0737623146314,-15.6174174533563));
#34585=CARTESIAN_POINT('Ctrl Pts',(-25.8049739071177,25.8624399870858,-15.5962460504461));
#34586=CARTESIAN_POINT('Ctrl Pts',(-25.950413022526,25.7110833228611,-15.5820450288187));
#34587=CARTESIAN_POINT('Ctrl Pts',(-26.1889229446774,25.4088487210681,-15.5560128576535));
#34588=CARTESIAN_POINT('Ctrl Pts',(-26.2862836464221,25.2623013555872,-15.5442260783802));
#34589=CARTESIAN_POINT('Ctrl Pts',(-26.3770930086197,25.0979081113098,-15.5323862394424));
#34590=CARTESIAN_POINT('Ctrl Pts',(-26.3829017135751,25.0872507420613,-15.5316246324498));
#34591=CARTESIAN_POINT('Ctrl Pts',(-26.3902702045418,25.0735479334843,-15.5306532454589));
#34592=CARTESIAN_POINT('Ctrl Pts',(-26.3918854403425,25.0705326624424,-15.5304399793035));
#34593=CARTESIAN_POINT('Ctrl Pts',(-26.3944740264626,25.0656818331679,-15.5300976729679));
#34594=CARTESIAN_POINT('Ctrl Pts',(-26.3954504022205,25.0638479058544,-15.5299684393665));
#34595=CARTESIAN_POINT('Ctrl Pts',(-26.3973063649514,25.0603537081635,-15.5297225545905));
#34596=CARTESIAN_POINT('Ctrl Pts',(-26.3981862669506,25.0586936250894,-15.5296058838352));
#34597=CARTESIAN_POINT('Ctrl Pts',(-26.4001860697034,25.0549126739249,-15.5293404944994));
#34598=CARTESIAN_POINT('Ctrl Pts',(-26.4013050535352,25.0527913273603,-15.5291918350929));
#34599=CARTESIAN_POINT('Ctrl Pts',(-26.4047730343861,25.0461989778468,-15.5287305973293));
#34600=CARTESIAN_POINT('Ctrl Pts',(-26.4071139048033,25.0417236731195,-15.5284185357031));
#34601=CARTESIAN_POINT('Ctrl Pts',(-26.4248095737164,25.0076983605815,-15.5260538278495));
#34602=CARTESIAN_POINT('Ctrl Pts',(-26.4397167653928,24.9779160726506,-15.5240289861796));
#34603=CARTESIAN_POINT('Ctrl Pts',(-26.55590492653,24.7365117790282,-15.5079326470844));
#34604=CARTESIAN_POINT('Ctrl Pts',(-26.634277302723,24.5146075395105,-15.4950370647945));
#34605=CARTESIAN_POINT('Ctrl Pts',(-26.7197849948165,24.1500243582729,-15.4740794987766));
#34606=CARTESIAN_POINT('Ctrl Pts',(-26.7428152101527,24.011990136972,-15.4662014206117));
#34607=CARTESIAN_POINT('Ctrl Pts',(-26.7639174145687,23.8022740406461,-15.4539523746853));
#34608=CARTESIAN_POINT('Ctrl Pts',(-26.7686884655051,23.7314316681439,-15.4497687637593));
#34609=CARTESIAN_POINT('Ctrl Pts',(-26.7723734941796,23.6237673373602,-15.4433096994203));
#34610=CARTESIAN_POINT('Ctrl Pts',(-26.7730022290152,23.5870239997028,-15.4410876969372));
#34611=CARTESIAN_POINT('Ctrl Pts',(-26.7730025855875,23.5437208426695,-15.438445755659));
#34612=CARTESIAN_POINT('Ctrl Pts',(-26.7729826208195,23.5371626701843,-15.4380450124112));
#34613=CARTESIAN_POINT('Ctrl Pts',(-26.7729169399545,23.5263895499875,-15.4373856651596));
#34614=CARTESIAN_POINT('Ctrl Pts',(-26.772882972128,23.5221745281013,-15.4371274302223));
#34615=CARTESIAN_POINT('Ctrl Pts',(-26.7728071189599,23.5146049604687,-15.4366632010558));
#34616=CARTESIAN_POINT('Ctrl Pts',(-26.7727682647272,23.511250384815,-15.4364573022921));
#34617=CARTESIAN_POINT('Ctrl Pts',(-26.7726745900509,23.5041236640146,-15.4360195152071));
#34618=CARTESIAN_POINT('Ctrl Pts',(-26.7726183839737,23.5003515448623,-15.435787583679));
#34619=CARTESIAN_POINT('Ctrl Pts',(-26.772450303937,23.4902607179419,-15.4351665644317));
#34620=CARTESIAN_POINT('Ctrl Pts',(-26.7723264673371,23.483942249658,-15.4347771016143));
#34621=CARTESIAN_POINT('Ctrl Pts',(-26.7716514949522,23.4539991762576,-15.4329285412039));
#34622=CARTESIAN_POINT('Ctrl Pts',(-26.7708591222728,23.4303812269149,-15.4314618879537));
#34623=CARTESIAN_POINT('Ctrl Pts',(-26.7626441680427,23.2460427896882,-15.4199451220563));
#34624=CARTESIAN_POINT('Ctrl Pts',(-26.7434563323293,23.0860985169247,-15.4095220443941));
#34625=CARTESIAN_POINT('Ctrl Pts',(-26.65512144139,22.6370000216139,-15.3790871422077));
#34626=CARTESIAN_POINT('Ctrl Pts',(-26.5578662747802,22.3550567911624,-15.3584496253352));
#34627=CARTESIAN_POINT('Ctrl Pts',(-26.407116894781,22.0583623979864,-15.3370700950834));
#34628=CARTESIAN_POINT('Ctrl Pts',(-26.3902949867508,22.0265828551034,-15.3347870657845));
#34629=CARTESIAN_POINT('Ctrl Pts',(-26.3706993405364,21.9910158605267,-15.3322455219549));
#34630=CARTESIAN_POINT('Ctrl Pts',(-26.3684459273239,21.9869466807182,-15.3319549500272));
#34631=CARTESIAN_POINT('Ctrl Pts',(-26.3650264581359,21.9808032756401,-15.3315165860771));
#34632=CARTESIAN_POINT('Ctrl Pts',(-26.3638669140515,21.9787254616802,-15.3313683794264));
#34633=CARTESIAN_POINT('Ctrl Pts',(-26.3618484396901,21.9751179055519,-15.3311111593395));
#34634=CARTESIAN_POINT('Ctrl Pts',(-26.3609905616411,21.9735875808008,-15.3310020780096));
#34635=CARTESIAN_POINT('Ctrl Pts',(-26.3591941036806,21.9703890973018,-15.3307741574737));
#34636=CARTESIAN_POINT('Ctrl Pts',(-26.3582552878642,21.968721075312,-15.330655334256));
#34637=CARTESIAN_POINT('Ctrl Pts',(-26.3560096327567,21.9647394561019,-15.3303717887548));
#34638=CARTESIAN_POINT('Ctrl Pts',(-26.354701413187,21.9624266299491,-15.3302071559685));
#34639=CARTESIAN_POINT('Ctrl Pts',(-26.3502730028289,21.9546201053908,-15.3296517018959));
#34640=CARTESIAN_POINT('Ctrl Pts',(-26.3471394925309,21.9491339200525,-15.329261737773));
#34641=CARTESIAN_POINT('Ctrl Pts',(-26.3396632433027,21.9361333389742,-15.3283384876984));
#34642=CARTESIAN_POINT('Ctrl Pts',(-26.3353062175247,21.9286271565333,-15.3278061015328));
#34643=CARTESIAN_POINT('Ctrl Pts',(-26.2841109587621,21.8412441154336,-15.3216151174824));
#34644=CARTESIAN_POINT('Ctrl Pts',(-26.2338764552796,21.7633955489523,-15.3161655547298));
#34645=CARTESIAN_POINT('Ctrl Pts',(-25.9932168947353,21.4235410879099,-15.2921725922398));
#34646=CARTESIAN_POINT('Ctrl Pts',(-25.7673233880428,21.1889816048928,-15.2748489382622));
#34647=CARTESIAN_POINT('Ctrl Pts',(-25.4938751088604,20.9794795163518,-15.2546722553982));
#34648=CARTESIAN_POINT('Ctrl Pts',(-25.477389636887,20.9670984189246,-15.2534594308608));
#34649=CARTESIAN_POINT('Ctrl Pts',(-25.4571364479147,20.9521894381931,-15.2519731038887));
#34650=CARTESIAN_POINT('Ctrl Pts',(-25.4534804887665,20.9495100510011,-15.25170494813));
#34651=CARTESIAN_POINT('Ctrl Pts',(-25.4465816105758,20.9444763236278,-15.2511991954427));
#34652=CARTESIAN_POINT('Ctrl Pts',(-25.4433399265044,20.9421203001262,-15.2509616585829));
#34653=CARTESIAN_POINT('Ctrl Pts',(-25.4358985204637,20.9367331433962,-15.2504166255318));
#34654=CARTESIAN_POINT('Ctrl Pts',(-25.4316958761873,20.9337060809331,-15.250108985859));
#34655=CARTESIAN_POINT('Ctrl Pts',(-25.4218731858701,20.9266669373007,-15.2493903427809));
#34656=CARTESIAN_POINT('Ctrl Pts',(-25.4162475203116,20.922662771927,-15.2489790586655));
#34657=CARTESIAN_POINT('Ctrl Pts',(-25.4086482448746,20.9172905680487,-15.2484238648719));
#34658=CARTESIAN_POINT('Ctrl Pts',(-25.4066858843158,20.9159065908581,-15.2482805310533));
#34659=CARTESIAN_POINT('Ctrl Pts',(-25.4026925172639,20.9130969010916,-15.2479889167728));
#34660=CARTESIAN_POINT('Ctrl Pts',(-25.4006614075377,20.9116713386464,-15.2478406310191));
#34661=CARTESIAN_POINT('Ctrl Pts',(-25.3932662750824,20.906493700969,-15.2473008584088));
#34662=CARTESIAN_POINT('Ctrl Pts',(-25.3878924956088,20.9027556430378,-15.2469088651587));
#34663=CARTESIAN_POINT('Ctrl Pts',(-25.3769126324925,20.8951674690088,-15.2461083944734));
#34664=CARTESIAN_POINT('Ctrl Pts',(-25.3713056786125,20.8913186759953,-15.2456998715153));
#34665=CARTESIAN_POINT('Ctrl Pts',(-25.3426373520131,20.8717730307061,-15.2436122625739));
#34666=CARTESIAN_POINT('Ctrl Pts',(-25.3193855985676,20.8563587146079,-15.2419229100669));
#34667=CARTESIAN_POINT('Ctrl Pts',(-25.2897780160384,20.8372795608588,-15.239775449887));
#34668=CARTESIAN_POINT('Ctrl Pts',(-25.2836053382168,20.8333316094204,-15.2393279410292));
#34669=CARTESIAN_POINT('Ctrl Pts',(-25.2737030048101,20.8270457078997,-15.238610335863));
#34670=CARTESIAN_POINT('Ctrl Pts',(-25.2699819047533,20.8246942729924,-15.2383407410542));
#34671=CARTESIAN_POINT('Ctrl Pts',(-25.2633876635326,20.8205461251951,-15.2378630996283));
#34672=CARTESIAN_POINT('Ctrl Pts',(-25.2605164782831,20.8187463028015,-15.2376551686393));
#34673=CARTESIAN_POINT('Ctrl Pts',(-25.2545565558345,20.8150233649697,-15.2372236275006));
#34674=CARTESIAN_POINT('Ctrl Pts',(-25.2514673911508,20.8131009460139,-15.2369999919904));
#34675=CARTESIAN_POINT('Ctrl Pts',(-25.243513407324,20.8081697669455,-15.2364242796221));
#34676=CARTESIAN_POINT('Ctrl Pts',(-25.2386438366384,20.8051687292605,-15.2360719185691));
#34677=CARTESIAN_POINT('Ctrl Pts',(-25.2187764479559,20.7929976417427,-15.2346347042834));
#34678=CARTESIAN_POINT('Ctrl Pts',(-25.2037119289596,20.7839375479681,-15.2335458216456));
#34679=CARTESIAN_POINT('Ctrl Pts',(-25.1035346607323,20.724799623857,-15.2263098194471));
#34680=CARTESIAN_POINT('Ctrl Pts',(-25.0162410419218,20.6785381014474,-15.2200254040262));
#34681=CARTESIAN_POINT('Ctrl Pts',(-24.7937174754043,20.573403193626,-15.204039513471));
#34682=CARTESIAN_POINT('Ctrl Pts',(-24.6563179839261,20.5196670850238,-15.1941919238845));
#34683=CARTESIAN_POINT('Ctrl Pts',(-24.3265512654169,20.4161181249453,-15.1708489076429));
#34684=CARTESIAN_POINT('Ctrl Pts',(-24.132276834729,20.374296874546,-15.1573064641323));
#34685=CARTESIAN_POINT('Ctrl Pts',(-23.9275096798446,20.3496498564076,-15.1438961827688));
#34686=CARTESIAN_POINT('Ctrl Pts',(-23.9196333702916,20.3487312933848,-15.1433817176381));
#34687=CARTESIAN_POINT('Ctrl Pts',(-23.9078961836278,20.3474063520275,-15.142617164907));
#34688=CARTESIAN_POINT('Ctrl Pts',(-23.904037888688,20.3469778706898,-15.1423661753869));
#34689=CARTESIAN_POINT('Ctrl Pts',(-23.8971419425714,20.3462246554553,-15.1419181942622));
#34690=CARTESIAN_POINT('Ctrl Pts',(-23.8941045927834,20.3458972681001,-15.1417210915612));
#34691=CARTESIAN_POINT('Ctrl Pts',(-23.8849707468724,20.3449258929987,-15.1411290169273));
#34692=CARTESIAN_POINT('Ctrl Pts',(-23.8788728371517,20.3442949773366,-15.1407346055066));
#34693=CARTESIAN_POINT('Ctrl Pts',(-23.8377371149947,20.3401574993735,-15.138079968241));
#34694=CARTESIAN_POINT('Ctrl Pts',(-23.8026438847066,20.3372078135023,-15.1358446622168));
#34695=CARTESIAN_POINT('Ctrl Pts',(-23.7628949828957,20.3345221132771,-15.1333513059536));
#34696=CARTESIAN_POINT('Ctrl Pts',(-23.7582816535313,20.3342203768352,-15.1330625085419));
#34697=CARTESIAN_POINT('Ctrl Pts',(-23.7513002071158,20.333778838044,-15.1326263684331));
#34698=CARTESIAN_POINT('Ctrl Pts',(-23.7489325834987,20.3336317230131,-15.1324786169728));
#34699=CARTESIAN_POINT('Ctrl Pts',(-23.7448155167525,20.3333804672967,-15.1322219672592));
#34700=CARTESIAN_POINT('Ctrl Pts',(-23.7430661513904,20.3332751394905,-15.1321130018458));
#34701=CARTESIAN_POINT('Ctrl Pts',(-23.7394043951533,20.3330576658455,-15.1318850987389));
#34702=CARTESIAN_POINT('Ctrl Pts',(-23.7374919912631,20.3329457982453,-15.1317661773513));
#34703=CARTESIAN_POINT('Ctrl Pts',(-23.7329181215214,20.332682338031,-15.131482001677));
#34704=CARTESIAN_POINT('Ctrl Pts',(-23.7302565572012,20.3325323419044,-15.1313168379325));
#34705=CARTESIAN_POINT('Ctrl Pts',(-23.7213643561069,20.3320422771646,-15.1307656898636));
#34706=CARTESIAN_POINT('Ctrl Pts',(-23.7151328681393,20.3317169990321,-15.1303805358634));
#34707=CARTESIAN_POINT('Ctrl Pts',(-23.7003007211742,20.3309859634074,-15.1294662820104));
#34708=CARTESIAN_POINT('Ctrl Pts',(-23.6916992523223,20.3305965677801,-15.1289380767818));
#34709=CARTESIAN_POINT('Ctrl Pts',(-23.5919088450246,20.3264796484286,-15.1228320820669));
#34710=CARTESIAN_POINT('Ctrl Pts',(-23.5005931377506,20.3265924635539,-15.1174574329503));
#34711=CARTESIAN_POINT('Ctrl Pts',(-23.1484524519573,20.3419981112915,-15.0971352997133));
#34712=CARTESIAN_POINT('Ctrl Pts',(-22.8898551646639,20.385093417396,-15.0829931804492));
#34713=CARTESIAN_POINT('Ctrl Pts',(-22.5818456323604,20.4758597367537,-15.0646383215396));
#34714=CARTESIAN_POINT('Ctrl Pts',(-22.5248944891357,20.4943822253599,-15.0611822486005));
#34715=CARTESIAN_POINT('Ctrl Pts',(-22.446950456237,20.5221565676844,-15.0563437844396));
#34716=CARTESIAN_POINT('Ctrl Pts',(-22.4254892626766,20.5300624399978,-15.0550000343342));
#34717=CARTESIAN_POINT('Ctrl Pts',(-22.3994647183322,20.5399652163467,-15.0533555906488));
#34718=CARTESIAN_POINT('Ctrl Pts',(-22.3948191645827,20.5417452529742,-15.0530614627599));
#34719=CARTESIAN_POINT('Ctrl Pts',(-22.386467372297,20.544967606481,-15.0525316147014));
#34720=CARTESIAN_POINT('Ctrl Pts',(-22.3827596405654,20.5464060429548,-15.0522960134086));
#34721=CARTESIAN_POINT('Ctrl Pts',(-22.3666176395726,20.5527028291119,-15.0512686343233));
#34722=CARTESIAN_POINT('Ctrl Pts',(-22.3542110877954,20.5576315008724,-15.0504746953763));
#34723=CARTESIAN_POINT('Ctrl Pts',(-22.339565186803,20.5635554071477,-15.0495321943651));
#34724=CARTESIAN_POINT('Ctrl Pts',(-22.3372957775286,20.5644763389212,-15.0493860022005));
#34725=CARTESIAN_POINT('Ctrl Pts',(-22.3328734094752,20.5662768206442,-15.0491008256321));
#34726=CARTESIAN_POINT('Ctrl Pts',(-22.3307203482195,20.567156116092,-15.0489618494371));
#34727=CARTESIAN_POINT('Ctrl Pts',(-22.3223960111388,20.5705662365963,-15.0484240000634));
#34728=CARTESIAN_POINT('Ctrl Pts',(-22.3162316767447,20.5731138750599,-15.0480245876063));
#34729=CARTESIAN_POINT('Ctrl Pts',(-22.3032396558225,20.5785305900096,-15.047180375264));
#34730=CARTESIAN_POINT('Ctrl Pts',(-22.2964138693841,20.58140409858,-15.0467354329798));
#34731=CARTESIAN_POINT('Ctrl Pts',(-22.262945031639,20.595629766057,-15.0445467372489));
#34732=CARTESIAN_POINT('Ctrl Pts',(-22.2364465879361,20.6073168978924,-15.0427919823008));
#34733=CARTESIAN_POINT('Ctrl Pts',(-22.204266186974,20.6220312950076,-15.0406328708845));
#34734=CARTESIAN_POINT('Ctrl Pts',(-22.1984305137233,20.624720771152,-15.040240194337));
#34735=CARTESIAN_POINT('Ctrl Pts',(-22.1888174506451,20.6291860304856,-15.0395914461875));
#34736=CARTESIAN_POINT('Ctrl Pts',(-22.1850353791303,20.6309517403266,-15.0393357235571));
#34737=CARTESIAN_POINT('Ctrl Pts',(-22.1782231421844,20.6341482561339,-15.0388742378581));
#34738=CARTESIAN_POINT('Ctrl Pts',(-22.175191752963,20.6355764525595,-15.0386685655761));
#34739=CARTESIAN_POINT('Ctrl Pts',(-22.1687281500936,20.6386340160737,-15.0382293509754));
#34740=CARTESIAN_POINT('Ctrl Pts',(-22.165296581795,20.6402647286093,-15.0379957621126));
#34741=CARTESIAN_POINT('Ctrl Pts',(-22.1561727198709,20.644620265264,-15.0373736070515));
#34742=CARTESIAN_POINT('Ctrl Pts',(-22.150485553824,20.6473557377639,-15.036984670349));
#34743=CARTESIAN_POINT('Ctrl Pts',(-22.1234742380787,20.6604457561386,-15.0351319927094));
#34744=CARTESIAN_POINT('Ctrl Pts',(-22.1022571708309,20.6710184519921,-15.0336606433234));
#34745=CARTESIAN_POINT('Ctrl Pts',(-21.9362074498903,20.7560624232953,-15.0220156417662));
#34746=CARTESIAN_POINT('Ctrl Pts',(-21.797114655308,20.8411691360699,-15.0114594648272));
#34747=CARTESIAN_POINT('Ctrl Pts',(-21.4887398583535,21.0635788785438,-14.9861623451807));
#34748=CARTESIAN_POINT('Ctrl Pts',(-21.3257478223474,21.2082552288599,-14.9712490047915));
#34749=CARTESIAN_POINT('Ctrl Pts',(-21.14955622988,21.3997617663604,-14.9539046234572));
#34750=CARTESIAN_POINT('Ctrl Pts',(-21.1211777137389,21.4318689331248,-14.9510689535246));
#34751=CARTESIAN_POINT('Ctrl Pts',(-21.0896486173265,21.469007619922,-14.9478780898256));
#34752=CARTESIAN_POINT('Ctrl Pts',(-21.0858625682158,21.4734920459962,-14.9474942465429));
#34753=CARTESIAN_POINT('Ctrl Pts',(-21.0734704505337,21.4882516280451,-14.9462357125665));
#34754=CARTESIAN_POINT('Ctrl Pts',(-21.0649161178238,21.4985702645475,-14.9453634726955));
#34755=CARTESIAN_POINT('Ctrl Pts',(-21.0548315954411,21.5108903147397,-14.9443313470368));
#34756=CARTESIAN_POINT('Ctrl Pts',(-21.0532392006373,21.5128403678239,-14.9441682538802));
#34757=CARTESIAN_POINT('Ctrl Pts',(-21.0499396005216,21.5168907501636,-14.9438300720318));
#34758=CARTESIAN_POINT('Ctrl Pts',(-21.0482327519047,21.5189913692589,-14.9436550020984));
#34759=CARTESIAN_POINT('Ctrl Pts',(-21.0181159438763,21.5561516890539,-14.9405636478855));
#34760=CARTESIAN_POINT('Ctrl Pts',(-20.9904409478681,21.5918044103815,-14.9376866544317));
#34761=CARTESIAN_POINT('Ctrl Pts',(-20.9602782471072,21.632394260582,-14.9345202668162));
#34762=CARTESIAN_POINT('Ctrl Pts',(-20.9570452863316,21.6367679285355,-14.9341804709735));
#34763=CARTESIAN_POINT('Ctrl Pts',(-20.9524693488718,21.6429913219565,-14.9336989647292));
#34764=CARTESIAN_POINT('Ctrl Pts',(-20.9511172671283,21.6448342931716,-14.9335566212587));
#34765=CARTESIAN_POINT('Ctrl Pts',(-20.948642323886,21.6482153302827,-14.9332959404141));
#34766=CARTESIAN_POINT('Ctrl Pts',(-20.9475188632435,21.6497529552411,-14.9331775609276));
#34767=CARTESIAN_POINT('Ctrl Pts',(-20.9452347033954,21.6528849958458,-14.9329367825747));
#34768=CARTESIAN_POINT('Ctrl Pts',(-20.9440741047289,21.6544794812693,-14.932814390796));
#34769=CARTESIAN_POINT('Ctrl Pts',(-20.9412195049727,21.6584088412133,-14.9325132296502));
#34770=CARTESIAN_POINT('Ctrl Pts',(-20.9395271695759,21.6607449324811,-14.932334577064));
#34771=CARTESIAN_POINT('Ctrl Pts',(-20.9332660503652,21.6694122203887,-14.9316731937273));
#34772=CARTESIAN_POINT('Ctrl Pts',(-20.9287170934505,21.67575780801,-14.9311918327046));
#34773=CARTESIAN_POINT('Ctrl Pts',(-20.8143787534156,21.8364848874251,-14.9190697481409));
#34774=CARTESIAN_POINT('Ctrl Pts',(-20.7183716003689,22.0002592467038,-14.9083413770415));
#34775=CARTESIAN_POINT('Ctrl Pts',(-20.5611010005301,22.3325426378547,-14.8877389942324));
#34776=CARTESIAN_POINT('Ctrl Pts',(-20.4983817541327,22.4995734847129,-14.8778813714213));
#34777=CARTESIAN_POINT('Ctrl Pts',(-20.4342405348895,22.7257332738947,-14.8644040002754));
#34778=CARTESIAN_POINT('Ctrl Pts',(-20.4201537071223,22.7809387849163,-14.8611062794753));
#34779=CARTESIAN_POINT('Ctrl Pts',(-20.4033270067,22.8550268340747,-14.8566526366753));
#34780=CARTESIAN_POINT('Ctrl Pts',(-20.3992804203139,22.8736036101323,-14.8555336380128));
#34781=CARTESIAN_POINT('Ctrl Pts',(-20.3944464214141,22.8967794268848,-14.8541342452425));
#34782=CARTESIAN_POINT('Ctrl Pts',(-20.3935042537894,22.9013460561374,-14.8538583428607));
#34783=CARTESIAN_POINT('Ctrl Pts',(-20.3917645199682,22.9098718997552,-14.853342923482));
#34784=CARTESIAN_POINT('Ctrl Pts',(-20.3909644784546,22.9138306037025,-14.8531034791949));
#34785=CARTESIAN_POINT('Ctrl Pts',(-20.3894113630448,22.9215907093599,-14.8526338518122));
#34786=CARTESIAN_POINT('Ctrl Pts',(-20.3886576999869,22.9253919870724,-14.8524036864686));
#34787=CARTESIAN_POINT('Ctrl Pts',(-20.3777153550909,22.9811089037282,-14.8490282684573));
#34788=CARTESIAN_POINT('Ctrl Pts',(-20.3688002150822,23.0332638826459,-14.8458456954992));
#34789=CARTESIAN_POINT('Ctrl Pts',(-20.3599143725103,23.0942522860705,-14.8420897697068));
#34790=CARTESIAN_POINT('Ctrl Pts',(-20.3586906968907,23.1028971402921,-14.8415565885755));
#34791=CARTESIAN_POINT('Ctrl Pts',(-20.3569184700033,23.1157948016147,-14.8407598924292));
#34792=CARTESIAN_POINT('Ctrl Pts',(-20.3563432455858,23.1200439536645,-14.840497222864));
#34793=CARTESIAN_POINT('Ctrl Pts',(-20.3553320506602,23.127627414055,-14.8400280806362));
#34794=CARTESIAN_POINT('Ctrl Pts',(-20.3548928145463,23.1309612867553,-14.8398217117056));
#34795=CARTESIAN_POINT('Ctrl Pts',(-20.3539774215546,23.1379942475896,-14.8393861055743));
#34796=CARTESIAN_POINT('Ctrl Pts',(-20.3535024667847,23.1416934847683,-14.8391568306451));
#34797=CARTESIAN_POINT('Ctrl Pts',(-20.3522794967798,23.1513514209479,-14.8385578400213));
#34798=CARTESIAN_POINT('Ctrl Pts',(-20.3515417164861,23.1573113807776,-14.8381878010729));
#34799=CARTESIAN_POINT('Ctrl Pts',(-20.3483534574062,23.1836709835844,-14.8365494085477));
#34800=CARTESIAN_POINT('Ctrl Pts',(-20.3460814798355,23.2040913665023,-14.8352754265874));
#34801=CARTESIAN_POINT('Ctrl Pts',(-20.3352535773325,23.3106763104763,-14.8285999921787));
#34802=CARTESIAN_POINT('Ctrl Pts',(-20.3299782301424,23.3971311765341,-14.8230959654542));
#34803=CARTESIAN_POINT('Ctrl Pts',(-20.3255123560234,23.6133000402341,-14.8090989465709));
#34804=CARTESIAN_POINT('Ctrl Pts',(-20.3306580888177,23.7429435771971,-14.8004897463206));
#34805=CARTESIAN_POINT('Ctrl Pts',(-20.3584274325684,24.0197776728857,-14.781769525876));
#34806=CARTESIAN_POINT('Ctrl Pts',(-20.3834690051902,24.1664368443192,-14.7716432392594));
#34807=CARTESIAN_POINT('Ctrl Pts',(-20.4424297874457,24.4092060427564,-14.7548999727367));
#34808=CARTESIAN_POINT('Ctrl Pts',(-20.4709419921012,24.5063978188601,-14.7482055187393));
#34809=CARTESIAN_POINT('Ctrl Pts',(-20.5054214269573,24.6062546521523,-14.7414417449694));
#34810=CARTESIAN_POINT('Ctrl Pts',(-20.506866485453,24.6104120993058,-14.7411603546057));
#34811=CARTESIAN_POINT('Ctrl Pts',(-20.510025620634,24.619441272345,-14.7405497121778));
#34812=CARTESIAN_POINT('Ctrl Pts',(-20.5117429039002,24.6243118766444,-14.7402206197781));
#34813=CARTESIAN_POINT('Ctrl Pts',(-20.516186167569,24.6368180347194,-14.7393764409498));
#34814=CARTESIAN_POINT('Ctrl Pts',(-20.5189292861293,24.6444475226649,-14.7388622347415));
#34815=CARTESIAN_POINT('Ctrl Pts',(-20.5231807694212,24.6561335547935,-14.7380759333394));
#34816=CARTESIAN_POINT('Ctrl Pts',(-20.5246685395587,24.6601974844839,-14.7378027321635));
#34817=CARTESIAN_POINT('Ctrl Pts',(-20.5301667886824,24.6751230691417,-14.7368002716573));
#34818=CARTESIAN_POINT('Ctrl Pts',(-20.5342276703386,24.6859662573128,-14.7360738030184));
#34819=CARTESIAN_POINT('Ctrl Pts',(-20.5395951458232,24.7000664194689,-14.7351316979496));
#34820=CARTESIAN_POINT('Ctrl Pts',(-20.5408486777127,24.7033432980869,-14.7349129343708));
#34821=CARTESIAN_POINT('Ctrl Pts',(-20.5427849683427,24.7083803234547,-14.7345769507794));
#34822=CARTESIAN_POINT('Ctrl Pts',(-20.5434639216875,24.7101419149702,-14.7344595017787));
#34823=CARTESIAN_POINT('Ctrl Pts',(-20.5448166476947,24.71364248681,-14.7342262202607));
#34824=CARTESIAN_POINT('Ctrl Pts',(-20.5454903780316,24.715381468956,-14.7341103865274));
#34825=CARTESIAN_POINT('Ctrl Pts',(-20.5469958550077,24.7192573025565,-14.7338523361302));
#34826=CARTESIAN_POINT('Ctrl Pts',(-20.5478283709625,24.7213938466064,-14.7337101670389));
#34827=CARTESIAN_POINT('Ctrl Pts',(-20.5502347503358,24.7275500764412,-14.7333007489261));
#34828=CARTESIAN_POINT('Ctrl Pts',(-20.5518144185634,24.7315675106792,-14.7330338503929));
#34829=CARTESIAN_POINT('Ctrl Pts',(-20.5616528587383,24.7564418929862,-14.7313829814962));
#34830=CARTESIAN_POINT('Ctrl Pts',(-20.5701214042584,24.7772159830804,-14.730011492275));
#34831=CARTESIAN_POINT('Ctrl Pts',(-20.5969375456606,24.8410823228437,-14.7258125475855));
#34832=CARTESIAN_POINT('Ctrl Pts',(-20.6160088080624,24.883866128188,-14.7230244266254));
#34833=CARTESIAN_POINT('Ctrl Pts',(-20.6627493829402,24.9828607495343,-14.7165972218532));
#34834=CARTESIAN_POINT('Ctrl Pts',(-20.6911387562169,25.0387114531932,-14.7129896101063));
#34835=CARTESIAN_POINT('Ctrl Pts',(-20.7962740363095,25.2314224174036,-14.7004883415939));
#34836=CARTESIAN_POINT('Ctrl Pts',(-20.8813669134498,25.3634769151451,-14.6918159071477));
#34837=CARTESIAN_POINT('Ctrl Pts',(-21.0048959758671,25.5275301072561,-14.6802936892157));
#34838=CARTESIAN_POINT('Ctrl Pts',(-21.0349191858624,25.5655849142249,-14.6775643528621));
#34839=CARTESIAN_POINT('Ctrl Pts',(-21.1756124023363,25.7358718842449,-14.6650392326436));
#34840=CARTESIAN_POINT('Ctrl Pts',(-21.2959098931277,25.8597489709747,-14.6550251769472));
#34841=CARTESIAN_POINT('Ctrl Pts',(-21.4341513639941,25.9809653977659,-14.6438442572034));
#34842=CARTESIAN_POINT('Ctrl Pts',(-21.442817924519,25.9884831525354,-14.6431446666558));
#34843=CARTESIAN_POINT('Ctrl Pts',(-21.4548930284213,25.9988451517449,-14.6421717268801));
#34844=CARTESIAN_POINT('Ctrl Pts',(-21.4582676561704,26.0017289332085,-14.6419000128294));
#34845=CARTESIAN_POINT('Ctrl Pts',(-21.4640817501095,26.0066766081129,-14.6414322077035));
#34846=CARTESIAN_POINT('Ctrl Pts',(-21.4665183543875,26.0087438681363,-14.6412362555106));
#34847=CARTESIAN_POINT('Ctrl Pts',(-21.4715457622532,26.0129963707386,-14.6408321505107));
#34848=CARTESIAN_POINT('Ctrl Pts',(-21.4741369453984,26.0151811558684,-14.6406239793256));
#34849=CARTESIAN_POINT('Ctrl Pts',(-21.4801627530997,26.0202456410813,-14.6401401265828));
#34850=CARTESIAN_POINT('Ctrl Pts',(-21.4835999420538,26.0231222664901,-14.6398643196902));
#34851=CARTESIAN_POINT('Ctrl Pts',(-21.4944357788327,26.032152539488,-14.63899541322));
#34852=CARTESIAN_POINT('Ctrl Pts',(-21.5018559431566,26.0382801808326,-14.6384012552909));
#34853=CARTESIAN_POINT('Ctrl Pts',(-21.5730700978168,26.0965549861105,-14.6327067719172));
#34854=CARTESIAN_POINT('Ctrl Pts',(-21.6388091902006,26.1462665728181,-14.6275090496299));
#34855=CARTESIAN_POINT('Ctrl Pts',(-21.7647508544295,26.2341242270233,-14.6176442001909));
#34856=CARTESIAN_POINT('Ctrl Pts',(-21.8244550853129,26.2728993196253,-14.6130040539844));
#34857=CARTESIAN_POINT('Ctrl Pts',(-21.9474214609267,26.3470897849638,-14.6035273748634));
#34858=CARTESIAN_POINT('Ctrl Pts',(-22.0106735371924,26.3823991979172,-14.5986930264539));
#34859=CARTESIAN_POINT('Ctrl Pts',(-22.0750361948364,26.4155368669684,-14.5938261690085));
#34860=CARTESIAN_POINT('Origin',(-23.5502525316942,23.5502525316942,-77.3107734492734));
#34861=CARTESIAN_POINT('',(-22.0750356748951,26.4155365992721,-13.0947094732148));
#34862=CARTESIAN_POINT('',(-22.0750360153462,26.4155367745563,-13.3428506325468));
#34863=CARTESIAN_POINT('',(-22.0750360153461,26.4155367745563,-77.3107734492734));
#34864=CARTESIAN_POINT('Ctrl Pts',(-22.0750356748951,26.4155365992721,-13.0947094732148));
#34865=CARTESIAN_POINT('Ctrl Pts',(-22.0083520106634,26.3812039246655,-13.0997046728913));
#34866=CARTESIAN_POINT('Ctrl Pts',(-21.9428598907341,26.3445397821812,-13.1047516267623));
#34867=CARTESIAN_POINT('Ctrl Pts',(-21.7610611649787,26.2342491824425,-13.119116417468));
#34868=CARTESIAN_POINT('Ctrl Pts',(-21.6481287722094,26.1554339924971,-13.1284745675161));
#34869=CARTESIAN_POINT('Ctrl Pts',(-21.4983837045451,26.0359848078024,-13.141245825012));
#34870=CARTESIAN_POINT('Ctrl Pts',(-21.4570403577237,26.0012715034878,-13.1448129245727));
#34871=CARTESIAN_POINT('Ctrl Pts',(-21.3857261608882,25.9382723684787,-13.1510131155592));
#34872=CARTESIAN_POINT('Ctrl Pts',(-21.3553894285417,25.9104197860558,-13.1536665338162));
#34873=CARTESIAN_POINT('Ctrl Pts',(-21.3106573097603,25.867741896068,-13.1575923808026));
#34874=CARTESIAN_POINT('Ctrl Pts',(-21.2958580943671,25.8533481629355,-13.1588934761794));
#34875=CARTESIAN_POINT('Ctrl Pts',(-21.2783066200613,25.8359462803271,-13.1604381368472));
#34876=CARTESIAN_POINT('Ctrl Pts',(-21.275420902497,25.8330742937169,-13.1606921538052));
#34877=CARTESIAN_POINT('Ctrl Pts',(-21.2709689260576,25.8286266763774,-13.1610841111566));
#34878=CARTESIAN_POINT('Ctrl Pts',(-21.2693988542205,25.827054894683,-13.1612223555892));
#34879=CARTESIAN_POINT('Ctrl Pts',(-21.2666451025541,25.8242924369837,-13.1614648442129));
#34880=CARTESIAN_POINT('Ctrl Pts',(-21.2654607326394,25.8231024643297,-13.161569143783));
#34881=CARTESIAN_POINT('Ctrl Pts',(-21.2627531404233,25.8203778085975,-13.1618075991007));
#34882=CARTESIAN_POINT('Ctrl Pts',(-21.2612305352458,25.8188425205952,-13.1619417052926));
#34883=CARTESIAN_POINT('Ctrl Pts',(-21.257105350445,25.8146745930104,-13.1623050739833));
#34884=CARTESIAN_POINT('Ctrl Pts',(-21.2545057497669,25.812038989396,-13.1625340994643));
#34885=CARTESIAN_POINT('Ctrl Pts',(-21.2422859047403,25.7996071338631,-13.1636108870893));
#34886=CARTESIAN_POINT('Ctrl Pts',(-21.2327235988285,25.7897537571136,-13.1644541304079));
#34887=CARTESIAN_POINT('Ctrl Pts',(-21.0548731149077,25.6041305370049,-13.18015662214));
#34888=CARTESIAN_POINT('Ctrl Pts',(-20.9069334782329,25.4098867635605,-13.1935737466354));
#34889=CARTESIAN_POINT('Ctrl Pts',(-20.7064538541379,25.073681034789,-13.2154580544452));
#34890=CARTESIAN_POINT('Ctrl Pts',(-20.6394999607987,24.9414895186487,-13.2237700450278));
#34891=CARTESIAN_POINT('Ctrl Pts',(-20.5529211488902,24.7366964856991,-13.2366664155525));
#34892=CARTESIAN_POINT('Ctrl Pts',(-20.5263517520093,24.6672429172322,-13.2410412451782));
#34893=CARTESIAN_POINT('Ctrl Pts',(-20.4941073951359,24.5733442626343,-13.2469897713353));
#34894=CARTESIAN_POINT('Ctrl Pts',(-20.4862803193698,24.5496593631594,-13.248492969221));
#34895=CARTESIAN_POINT('Ctrl Pts',(-20.4753900969882,24.5153744012985,-13.2506738442773));
#34896=CARTESIAN_POINT('Ctrl Pts',(-20.4721050758065,24.5048453509938,-13.251344263924));
#34897=CARTESIAN_POINT('Ctrl Pts',(-20.4663631611793,24.4861036916264,-13.2525388771142));
#34898=CARTESIAN_POINT('Ctrl Pts',(-20.4638848518499,24.477897714777,-13.2530623654408));
#34899=CARTESIAN_POINT('Ctrl Pts',(-20.4602304707623,24.4656208617771,-13.2538462252109));
#34900=CARTESIAN_POINT('Ctrl Pts',(-20.4590296269875,24.4615573489257,-13.2541057851366));
#34901=CARTESIAN_POINT('Ctrl Pts',(-20.456925077583,24.4543837795141,-13.2545642012833));
#34902=CARTESIAN_POINT('Ctrl Pts',(-20.4560180378703,24.4512747005381,-13.2547629481559));
#34903=CARTESIAN_POINT('Ctrl Pts',(-20.4542182256958,24.4450706776469,-13.2551596717967));
#34904=CARTESIAN_POINT('Ctrl Pts',(-20.4533254035659,24.4419757517469,-13.255357646691));
#34905=CARTESIAN_POINT('Ctrl Pts',(-20.451186687573,24.4345200393279,-13.2558347322538));
#34906=CARTESIAN_POINT('Ctrl Pts',(-20.4499453584229,24.4301579597323,-13.2561139916314));
#34907=CARTESIAN_POINT('Ctrl Pts',(-20.4461624441928,24.4167572619743,-13.2569723182806));
#34908=CARTESIAN_POINT('Ctrl Pts',(-20.4436511648223,24.4077102060295,-13.2575523721091));
#34909=CARTESIAN_POINT('Ctrl Pts',(-20.4345369445851,24.374309944865,-13.2596960631648));
#34910=CARTESIAN_POINT('Ctrl Pts',(-20.4281806817739,24.3498909158756,-13.2612676870682));
#34911=CARTESIAN_POINT('Ctrl Pts',(-20.4206598747981,24.3195403917495,-13.2632268943196));
#34912=CARTESIAN_POINT('Ctrl Pts',(-20.4192242730923,24.3136764327889,-13.2636056964035));
#34913=CARTESIAN_POINT('Ctrl Pts',(-20.4161913656122,24.3011355468805,-13.264416397071));
#34914=CARTESIAN_POINT('Ctrl Pts',(-20.4145989036689,24.2944574894287,-13.2648484482815));
#34915=CARTESIAN_POINT('Ctrl Pts',(-20.4127144885043,24.2864416815978,-13.2653674743066));
#34916=CARTESIAN_POINT('Ctrl Pts',(-20.4124020244989,24.2851087294528,-13.2654537974869));
#34917=CARTESIAN_POINT('Ctrl Pts',(-20.3410933139109,23.9800354329428,-13.2852138569727));
#34918=CARTESIAN_POINT('Ctrl Pts',(-20.3145843724405,23.6676468020343,-13.3064256333339));
#34919=CARTESIAN_POINT('Ctrl Pts',(-20.3383290956884,23.2735658166588,-13.3330358993233));
#34920=CARTESIAN_POINT('Ctrl Pts',(-20.3465210644565,23.1909283189385,-13.3385918738686));
#34921=CARTESIAN_POINT('Ctrl Pts',(-20.3672685944779,23.0409284463298,-13.3485389577744));
#34922=CARTESIAN_POINT('Ctrl Pts',(-20.3787981885229,22.9734711781954,-13.3529604427561));
#34923=CARTESIAN_POINT('Ctrl Pts',(-20.3946642084834,22.8956528080165,-13.3579619205416));
#34924=CARTESIAN_POINT('Ctrl Pts',(-20.3969160023898,22.8848900702315,-13.3586514288398));
#34925=CARTESIAN_POINT('Ctrl Pts',(-20.399915166782,22.8709124557051,-13.3595438114012));
#34926=CARTESIAN_POINT('Ctrl Pts',(-20.4006124173684,22.8676870754414,-13.3597495176622));
#34927=CARTESIAN_POINT('Ctrl Pts',(-20.4017509648359,22.8624592120358,-13.3600825836484));
#34928=CARTESIAN_POINT('Ctrl Pts',(-20.4021892188173,22.8604560796514,-13.3602101185746));
#34929=CARTESIAN_POINT('Ctrl Pts',(-20.403034349671,22.8566108113337,-13.3604547746606));
#34930=CARTESIAN_POINT('Ctrl Pts',(-20.4034409310714,22.8547686198157,-13.3605719122031));
#34931=CARTESIAN_POINT('Ctrl Pts',(-20.4043796894102,22.8505328484733,-13.3608410832068));
#34932=CARTESIAN_POINT('Ctrl Pts',(-20.4049129819553,22.8481395124083,-13.3609930519314));
#34933=CARTESIAN_POINT('Ctrl Pts',(-20.4066145324135,22.8405440572291,-13.3614749605857));
#34934=CARTESIAN_POINT('Ctrl Pts',(-20.4077929763079,22.8353441928305,-13.3618043146132));
#34935=CARTESIAN_POINT('Ctrl Pts',(-20.4179527689577,22.791024794483,-13.3646068531805));
#34936=CARTESIAN_POINT('Ctrl Pts',(-20.4276518009596,22.7520710986331,-13.3670394681314));
#34937=CARTESIAN_POINT('Ctrl Pts',(-20.4386106719254,22.7113206343329,-13.3695617289842));
#34938=CARTESIAN_POINT('Ctrl Pts',(-20.4391466573235,22.7093351574092,-13.3696845639905));
#34939=CARTESIAN_POINT('Ctrl Pts',(-20.4898449335098,22.5222429794677,-13.3812541286794));
#34940=CARTESIAN_POINT('Ctrl Pts',(-20.5564350762511,22.3419589003215,-13.3919361168441));
#34941=CARTESIAN_POINT('Ctrl Pts',(-20.7177913302788,22.0019177450866,-13.4129665172933));
#34942=CARTESIAN_POINT('Ctrl Pts',(-20.8110778125817,21.8423030256289,-13.4232797042964));
#34943=CARTESIAN_POINT('Ctrl Pts',(-20.9659330079151,21.6229589155487,-13.4389556559534));
#34944=CARTESIAN_POINT('Ctrl Pts',(-21.0170192477865,21.5562878019546,-13.4439427946609));
#34945=CARTESIAN_POINT('Ctrl Pts',(-21.0774445447636,21.4835035223549,-13.4496799656041));
#34946=CARTESIAN_POINT('Ctrl Pts',(-21.0842824636588,21.4753495394669,-13.4503269860015));
#34947=CARTESIAN_POINT('Ctrl Pts',(-21.0965382042667,21.4608811467546,-13.4514828102283));
#34948=CARTESIAN_POINT('Ctrl Pts',(-21.1019403533559,21.4545535408602,-13.4519909694969));
#34949=CARTESIAN_POINT('Ctrl Pts',(-21.1100988159052,21.4450720288827,-13.4527564729705));
#34950=CARTESIAN_POINT('Ctrl Pts',(-21.112836903668,21.441902427445,-13.4530130618698));
#34951=CARTESIAN_POINT('Ctrl Pts',(-21.1177141067322,21.4362787921011,-13.4534695388629));
#34952=CARTESIAN_POINT('Ctrl Pts',(-21.1198507800445,21.4338226400944,-13.453669325197));
#34953=CARTESIAN_POINT('Ctrl Pts',(-21.1241246371097,21.42892475616,-13.4540685621153));
#34954=CARTESIAN_POINT('Ctrl Pts',(-21.1262617945411,21.4264830060158,-13.4542680114774));
#34955=CARTESIAN_POINT('Ctrl Pts',(-21.1314523712772,21.4205706975561,-13.4547519615063));
#34956=CARTESIAN_POINT('Ctrl Pts',(-21.1345095706871,21.4171034800128,-13.455036620311));
#34957=CARTESIAN_POINT('Ctrl Pts',(-21.1459405804623,21.4041954837803,-13.4560995583081));
#34958=CARTESIAN_POINT('Ctrl Pts',(-21.1543622744674,21.3947974336269,-13.456879849679));
#34959=CARTESIAN_POINT('Ctrl Pts',(-21.2998411396458,21.2343587338518,-13.4703117092561));
#34960=CARTESIAN_POINT('Ctrl Pts',(-21.4508490374558,21.096644600442,-13.4835872555689));
#34961=CARTESIAN_POINT('Ctrl Pts',(-21.7248143152441,20.8907090207424,-13.5065469677191));
#34962=CARTESIAN_POINT('Ctrl Pts',(-21.841076787437,20.8145418925604,-13.515990394558));
#34963=CARTESIAN_POINT('Ctrl Pts',(-22.0329889654937,20.7058357148056,-13.5308679535547));
#34964=CARTESIAN_POINT('Ctrl Pts',(-22.1056043664481,20.668275990454,-13.5363460294598));
#34965=CARTESIAN_POINT('Ctrl Pts',(-22.2421358820788,20.604114891618,-13.5462830875753));
#34966=CARTESIAN_POINT('Ctrl Pts',(-22.3056346031707,20.5767320627814,-13.5507663360385));
#34967=CARTESIAN_POINT('Ctrl Pts',(-22.3844495372438,20.5457121219633,-13.5561222276795));
#34968=CARTESIAN_POINT('Ctrl Pts',(-22.3989704858477,20.5401180878865,-13.5571004707037));
#34969=CARTESIAN_POINT('Ctrl Pts',(-22.4170185731768,20.5333149712937,-13.5583052750365));
#34970=CARTESIAN_POINT('Ctrl Pts',(-22.4205077163715,20.5320066668451,-13.5585376836117));
#34971=CARTESIAN_POINT('Ctrl Pts',(-22.4260097043341,20.5299544946848,-13.558903353777));
#34972=CARTESIAN_POINT('Ctrl Pts',(-22.4280210223918,20.5292065858624,-13.5590368581304));
#34973=CARTESIAN_POINT('Ctrl Pts',(-22.4317837347968,20.527811697071,-13.5592862927012));
#34974=CARTESIAN_POINT('Ctrl Pts',(-22.4335349325325,20.5271642345749,-13.5594022513761));
#34975=CARTESIAN_POINT('Ctrl Pts',(-22.4374701215967,20.5257131806889,-13.5596625352809));
#34976=CARTESIAN_POINT('Ctrl Pts',(-22.4396544165787,20.5249104345428,-13.5598068089902));
#34977=CARTESIAN_POINT('Ctrl Pts',(-22.4452128548071,20.5228744944253,-13.5601734389851));
#34978=CARTESIAN_POINT('Ctrl Pts',(-22.4485882041209,20.5216445713151,-13.5603955990214));
#34979=CARTESIAN_POINT('Ctrl Pts',(-22.4672783898046,20.5148695472773,-13.5616231655449));
#34980=CARTESIAN_POINT('Ctrl Pts',(-22.4826333974586,20.5094348349903,-13.5626220588064));
#34981=CARTESIAN_POINT('Ctrl Pts',(-22.7998260673583,20.3998673372801,-13.5830716347356));
#34982=CARTESIAN_POINT('Ctrl Pts',(-23.1154959395728,20.341026147284,-13.6001179677027));
#34983=CARTESIAN_POINT('Ctrl Pts',(-23.5149229875253,20.3266968010335,-13.622764315868));
#34984=CARTESIAN_POINT('Ctrl Pts',(-23.5952100892993,20.3268168806852,-13.6273604802626));
#34985=CARTESIAN_POINT('Ctrl Pts',(-23.7552040523833,20.333034810549,-13.6366885826787));
#34986=CARTESIAN_POINT('Ctrl Pts',(-23.8348541797061,20.3391008204674,-13.641416423137));
#34987=CARTESIAN_POINT('Ctrl Pts',(-23.9295620612457,20.3498648795173,-13.6471718492241));
#34988=CARTESIAN_POINT('Ctrl Pts',(-23.9449188299237,20.3517223468152,-13.6481092699471));
#34989=CARTESIAN_POINT('Ctrl Pts',(-23.9679400159539,20.3546751724777,-13.6495210564125));
#34990=CARTESIAN_POINT('Ctrl Pts',(-23.9756149774831,20.3556877285768,-13.6499928146082));
#34991=CARTESIAN_POINT('Ctrl Pts',(-23.9879571684302,20.3573612975733,-13.6507532312779));
#34992=CARTESIAN_POINT('Ctrl Pts',(-23.9926267578691,20.358004918242,-13.6510413397832));
#34993=CARTESIAN_POINT('Ctrl Pts',(-24.0015456120499,20.3592541704951,-13.6515924131169));
#34994=CARTESIAN_POINT('Ctrl Pts',(-24.0057951149735,20.359858051369,-13.6518553220055));
#34995=CARTESIAN_POINT('Ctrl Pts',(-24.0133224758315,20.360943082111,-13.6523216382853));
#34996=CARTESIAN_POINT('Ctrl Pts',(-24.0166008284844,20.3614208013716,-13.6525249365764));
#34997=CARTESIAN_POINT('Ctrl Pts',(-24.0230571530632,20.362371781726,-13.6529257164081));
#34998=CARTESIAN_POINT('Ctrl Pts',(-24.0262351661336,20.3628447420317,-13.6531231881889));
#34999=CARTESIAN_POINT('Ctrl Pts',(-24.0347616572915,20.364126713324,-13.6536535235515));
#35000=CARTESIAN_POINT('Ctrl Pts',(-24.0401087972791,20.364944436428,-13.6539866634931));
#35001=CARTESIAN_POINT('Ctrl Pts',(-24.0595594134578,20.3679690996865,-13.6552005241912));
#35002=CARTESIAN_POINT('Ctrl Pts',(-24.0736500836644,20.3702562528457,-13.6560837909211));
#35003=CARTESIAN_POINT('Ctrl Pts',(-24.3035629800566,20.4091444781796,-13.6705608880725));
#35004=CARTESIAN_POINT('Ctrl Pts',(-24.5150750082941,20.4675395840331,-13.6848785102126));
#35005=CARTESIAN_POINT('Ctrl Pts',(-24.9777300523539,20.6475808745823,-13.7182518411133));
#35006=CARTESIAN_POINT('Ctrl Pts',(-25.2223737474087,20.7812773116877,-13.737437422956));
#35007=CARTESIAN_POINT('Ctrl Pts',(-25.4561448262258,20.9514404967424,-13.7556547960255));
#35008=CARTESIAN_POINT('Ctrl Pts',(-25.4653930666789,20.9582482546693,-13.7563751053299));
#35009=CARTESIAN_POINT('Ctrl Pts',(-25.477294322151,20.9671074058177,-13.7573013287294));
#35010=CARTESIAN_POINT('Ctrl Pts',(-25.4799806472412,20.9691135962979,-13.7575103462015));
#35011=CARTESIAN_POINT('Ctrl Pts',(-25.484314325226,20.9723606032793,-13.757847457154));
#35012=CARTESIAN_POINT('Ctrl Pts',(-25.4859636173757,20.9735988086236,-13.7579757337333));
#35013=CARTESIAN_POINT('Ctrl Pts',(-25.4891163774683,20.9759704773782,-13.758220905742));
#35014=CARTESIAN_POINT('Ctrl Pts',(-25.4906200296642,20.9771036668868,-13.7583378186949));
#35015=CARTESIAN_POINT('Ctrl Pts',(-25.4940600010956,20.9797008444251,-13.7586052472907));
#35016=CARTESIAN_POINT('Ctrl Pts',(-25.495995657934,20.9811657013581,-13.7587557004781));
#35017=CARTESIAN_POINT('Ctrl Pts',(-25.5011212451101,20.9850537337724,-13.7591540299774));
#35018=CARTESIAN_POINT('Ctrl Pts',(-25.5043083284375,20.9874806820225,-13.7594016407547));
#35019=CARTESIAN_POINT('Ctrl Pts',(-25.5194574151618,20.9990613259702,-13.760578313633));
#35020=CARTESIAN_POINT('Ctrl Pts',(-25.5313599263875,21.0082930605982,-13.7615019546781));
#35021=CARTESIAN_POINT('Ctrl Pts',(-25.7797305223774,21.203736581209,-13.7807678109145));
#35022=CARTESIAN_POINT('Ctrl Pts',(-25.9890676528571,21.4221173260409,-13.7969566667996));
#35023=CARTESIAN_POINT('Ctrl Pts',(-26.238155563539,21.7678591778564,-13.8209895642372));
#35024=CARTESIAN_POINT('Ctrl Pts',(-26.3052669430688,21.8734579261095,-13.8281396498061));
#35025=CARTESIAN_POINT('Ctrl Pts',(-26.3808984994877,22.0093144668135,-13.8372993719535));
#35026=CARTESIAN_POINT('Ctrl Pts',(-26.3953462068264,22.0361559017175,-13.8391069392147));
#35027=CARTESIAN_POINT('Ctrl Pts',(-26.4298910926285,22.1025752984813,-13.8435783690554));
#35028=CARTESIAN_POINT('Ctrl Pts',(-26.4495550181563,22.1423702900796,-13.8462562565726));
#35029=CARTESIAN_POINT('Ctrl Pts',(-26.4716520271938,22.1895168386629,-13.8494319068066));
#35030=CARTESIAN_POINT('Ctrl Pts',(-26.4748889816027,22.196488049649,-13.8499015412386));
#35031=CARTESIAN_POINT('Ctrl Pts',(-26.4798025498354,22.2071699454801,-13.8506212939715));
#35032=CARTESIAN_POINT('Ctrl Pts',(-26.4814971362459,22.2108723727299,-13.8508707910636));
#35033=CARTESIAN_POINT('Ctrl Pts',(-26.4845705231875,22.2176210492361,-13.8513256171017));
#35034=CARTESIAN_POINT('Ctrl Pts',(-26.4859516101013,22.2206662561389,-13.8515308668632));
#35035=CARTESIAN_POINT('Ctrl Pts',(-26.4887153455509,22.2267854127254,-13.8519433431819));
#35036=CARTESIAN_POINT('Ctrl Pts',(-26.4900979158132,22.2298593929863,-13.8521505721173));
#35037=CARTESIAN_POINT('Ctrl Pts',(-26.494008985946,22.2385917860858,-13.8527393166197));
#35038=CARTESIAN_POINT('Ctrl Pts',(-26.4965259790903,22.2442553089449,-13.8531212270297));
#35039=CARTESIAN_POINT('Ctrl Pts',(-26.507067240029,22.2681599181462,-13.8547335253351));
#35040=CARTESIAN_POINT('Ctrl Pts',(-26.514938426467,22.2864676584871,-13.8559691429043));
#35041=CARTESIAN_POINT('Ctrl Pts',(-26.6713083941078,22.6596729741159,-13.8811777876664));
#35042=CARTESIAN_POINT('Ctrl Pts',(-26.7552107178971,23.0382077950116,-13.9076760916674));
#35043=CARTESIAN_POINT('Ctrl Pts',(-26.7721731756054,23.4654090356613,-13.9361761971723));
#35044=CARTESIAN_POINT('Ctrl Pts',(-26.7730191425728,23.5084589201117,-13.9390260147838));
#35045=CARTESIAN_POINT('Ctrl Pts',(-26.7729992036865,23.5593832492775,-13.942361868955));
#35046=CARTESIAN_POINT('Ctrl Pts',(-26.7729673028915,23.5672521628765,-13.9428763340315));
#35047=CARTESIAN_POINT('Ctrl Pts',(-26.7728058495649,23.5881746144899,-13.9442414518283));
#35048=CARTESIAN_POINT('Ctrl Pts',(-26.7726258043491,23.601227751241,-13.9450902466936));
#35049=CARTESIAN_POINT('Ctrl Pts',(-26.7722610364385,23.6195844129097,-13.9462795432568));
#35050=CARTESIAN_POINT('Ctrl Pts',(-26.7721425234256,23.6248889585419,-13.9466227027519));
#35051=CARTESIAN_POINT('Ctrl Pts',(-26.7719494943123,23.6326683905398,-13.9471251916365));
#35052=CARTESIAN_POINT('Ctrl Pts',(-26.7718852260108,23.635143495402,-13.9472849484876));
#35053=CARTESIAN_POINT('Ctrl Pts',(-26.771701091182,23.6419333498852,-13.947722882963));
#35054=CARTESIAN_POINT('Ctrl Pts',(-26.7715754079923,23.6462479529597,-13.9480008132674));
#35055=CARTESIAN_POINT('Ctrl Pts',(-26.7702801209892,23.6878427358036,-13.9506766917176));
#35056=CARTESIAN_POINT('Ctrl Pts',(-26.7684720113068,23.725102241726,-13.9530465914813));
#35057=CARTESIAN_POINT('Ctrl Pts',(-26.7656737502952,23.7675339437805,-13.955708235502));
#35058=CARTESIAN_POINT('Ctrl Pts',(-26.7653174976526,23.7727431846396,-13.9560343583586));
#35059=CARTESIAN_POINT('Ctrl Pts',(-26.7647768149559,23.7803766400378,-13.9565112859884));
#35060=CARTESIAN_POINT('Ctrl Pts',(-26.7646023016556,23.782801514412,-13.9566626463715));
#35061=CARTESIAN_POINT('Ctrl Pts',(-26.7642877251222,23.7871045636001,-13.9569309867099));
#35062=CARTESIAN_POINT('Ctrl Pts',(-26.7641487593398,23.7889828138333,-13.9570480288642));
#35063=CARTESIAN_POINT('Ctrl Pts',(-26.7638543088035,23.7929157271228,-13.9572929241231));
#35064=CARTESIAN_POINT('Ctrl Pts',(-26.7636985003589,23.79497035856,-13.957420758414));
#35065=CARTESIAN_POINT('Ctrl Pts',(-26.7632846177588,23.8003596343954,-13.9577557973066));
#35066=CARTESIAN_POINT('Ctrl Pts',(-26.7630233219941,23.8036940400134,-13.9579628193829));
#35067=CARTESIAN_POINT('Ctrl Pts',(-26.7618479749756,23.8183987414874,-13.9588746166696));
#35068=CARTESIAN_POINT('Ctrl Pts',(-26.7608787358078,23.8297647278527,-13.9595763079363));
#35069=CARTESIAN_POINT('Ctrl Pts',(-26.7532901846323,23.9134995139728,-13.9647246156897));
#35070=CARTESIAN_POINT('Ctrl Pts',(-26.7442845309411,23.985637449347,-13.9690435087567));
#35071=CARTESIAN_POINT('Ctrl Pts',(-26.7201156608629,24.1373041681785,-13.9779927262528));
#35072=CARTESIAN_POINT('Ctrl Pts',(-26.7043806848107,24.216690003693,-13.9826000255598));
#35073=CARTESIAN_POINT('Ctrl Pts',(-26.6079485345692,24.6224540222739,-14.0061193975498));
#35074=CARTESIAN_POINT('Ctrl Pts',(-26.4795488709317,24.9352916931509,-14.0244148164406));
#35075=CARTESIAN_POINT('Ctrl Pts',(-26.2948779216795,25.2394944004927,-14.045944301923));
#35076=CARTESIAN_POINT('Ctrl Pts',(-26.2844878392806,25.2562607023923,-14.0471431511272));
#35077=CARTESIAN_POINT('Ctrl Pts',(-26.2706451959008,25.2781470354461,-14.0487246447038));
#35078=CARTESIAN_POINT('Ctrl Pts',(-26.2673307496776,25.2833542656059,-14.0491021570046));
#35079=CARTESIAN_POINT('Ctrl Pts',(-26.2621860619854,25.2913859029982,-14.0496863657435));
#35080=CARTESIAN_POINT('Ctrl Pts',(-26.2603663091161,25.2942170389813,-14.0498926707855));
#35081=CARTESIAN_POINT('Ctrl Pts',(-26.256729510789,25.2998556603448,-14.050304303584));
#35082=CARTESIAN_POINT('Ctrl Pts',(-26.2549125234928,25.3026631784275,-14.0505096289949));
#35083=CARTESIAN_POINT('Ctrl Pts',(-26.2508689344897,25.3088898609722,-14.0509658366997));
#35084=CARTESIAN_POINT('Ctrl Pts',(-26.2486402054202,25.3123076310078,-14.0512167985272));
#35085=CARTESIAN_POINT('Ctrl Pts',(-26.2421726854089,25.3221845667361,-14.0519436569247));
#35086=CARTESIAN_POINT('Ctrl Pts',(-26.2379171726087,25.3286327011448,-14.0524201816295));
#35087=CARTESIAN_POINT('Ctrl Pts',(-26.2085817857222,25.3727371375646,-14.0556933646411));
#35088=CARTESIAN_POINT('Ctrl Pts',(-26.1827356043435,25.4098753690209,-14.0585189247731));
#35089=CARTESIAN_POINT('Ctrl Pts',(-26.108577587697,25.5117873136047,-14.0664737870782));
#35090=CARTESIAN_POINT('Ctrl Pts',(-26.0586015664174,25.5753029224919,-14.0716661951356));
#35091=CARTESIAN_POINT('Ctrl Pts',(-25.8099939073765,25.8679253920806,-14.0967343797163));
#35092=CARTESIAN_POINT('Ctrl Pts',(-25.5821108278621,26.0700832854051,-14.1177443458217));
#35093=CARTESIAN_POINT('Ctrl Pts',(-25.3069463817119,26.2522643045322,-14.1395136487628));
#35094=CARTESIAN_POINT('Ctrl Pts',(-25.284335421391,26.2668308050833,-14.1412775274237));
#35095=CARTESIAN_POINT('Ctrl Pts',(-25.2547628703622,26.2853624219483,-14.1435498508367));
#35096=CARTESIAN_POINT('Ctrl Pts',(-25.2479657202709,26.2895866730746,-14.1440697920628));
#35097=CARTESIAN_POINT('Ctrl Pts',(-25.2354693414437,26.2972884686461,-14.1450213034697));
#35098=CARTESIAN_POINT('Ctrl Pts',(-25.2297749225072,26.3007736959443,-14.1454532329046));
#35099=CARTESIAN_POINT('Ctrl Pts',(-25.2223330331715,26.3052967217282,-14.1460155083316));
#35100=CARTESIAN_POINT('Ctrl Pts',(-25.2205953959572,26.3063505720964,-14.146146640203));
#35101=CARTESIAN_POINT('Ctrl Pts',(-25.2160321361956,26.3091122186658,-14.1464905976192));
#35102=CARTESIAN_POINT('Ctrl Pts',(-25.2132048765253,26.3108173221266,-14.1467032894843));
#35103=CARTESIAN_POINT('Ctrl Pts',(-25.1773609186585,26.3323595519688,-14.1493945086868));
#35104=CARTESIAN_POINT('Ctrl Pts',(-25.1439919209377,26.3516086789016,-14.151843188912));
#35105=CARTESIAN_POINT('Ctrl Pts',(-25.1061323342117,26.3725526777194,-14.154551484359));
#35106=CARTESIAN_POINT('Ctrl Pts',(-25.1019755301281,26.3748402557614,-14.154847907316));
#35107=CARTESIAN_POINT('Ctrl Pts',(-25.0957056261584,26.3782726997463,-14.1552935913781));
#35108=CARTESIAN_POINT('Ctrl Pts',(-25.0935962958551,26.3794243829286,-14.1554432867409));
#35109=CARTESIAN_POINT('Ctrl Pts',(-25.0899396295782,26.3814155969606,-14.1557023715276));
#35110=CARTESIAN_POINT('Ctrl Pts',(-25.0883928942793,26.3822562192871,-14.1558118312638));
#35111=CARTESIAN_POINT('Ctrl Pts',(-25.0851674600941,26.3840057618148,-14.1560398160448));
#35112=CARTESIAN_POINT('Ctrl Pts',(-25.0834886440861,26.3849144569191,-14.1561583261292));
#35113=CARTESIAN_POINT('Ctrl Pts',(-25.0795419492055,26.3870461581294,-14.1564365686477));
#35114=CARTESIAN_POINT('Ctrl Pts',(-25.0772734027019,26.3882679405871,-14.1565962221835));
#35115=CARTESIAN_POINT('Ctrl Pts',(-25.069807685094,26.3922772464007,-14.1571207272365));
#35116=CARTESIAN_POINT('Ctrl Pts',(-25.0646042883601,26.3950532455602,-14.1574848442081));
#35117=CARTESIAN_POINT('Ctrl Pts',(-25.0522934320256,26.4015777081451,-14.1583429712535));
#35118=CARTESIAN_POINT('Ctrl Pts',(-25.0451794771443,26.4053139249172,-14.1588362226774));
#35119=CARTESIAN_POINT('Ctrl Pts',(-24.8823042252298,26.490079594058,-14.1700711172647));
#35120=CARTESIAN_POINT('Ctrl Pts',(-24.7201677361425,26.5582855019013,-14.1800491480166));
#35121=CARTESIAN_POINT('Ctrl Pts',(-24.2675718147414,26.7065068428227,-14.2067748534045));
#35122=CARTESIAN_POINT('Ctrl Pts',(-23.9702382988431,26.7596267929562,-14.2232975655068));
#35123=CARTESIAN_POINT('Ctrl Pts',(-23.6445422763731,26.7717224917826,-14.2428990824624));
#35124=CARTESIAN_POINT('Ctrl Pts',(-23.6192183555388,26.7723640937979,-14.2444315816337));
#35125=CARTESIAN_POINT('Ctrl Pts',(-23.5845712542195,26.7728332744458,-14.2465407078534));
#35126=CARTESIAN_POINT('Ctrl Pts',(-23.5752520387482,26.772919042528,-14.2471092390029));
#35127=CARTESIAN_POINT('Ctrl Pts',(-23.5614144903551,26.7729863692157,-14.2479552836639));
#35128=CARTESIAN_POINT('Ctrl Pts',(-23.556896299223,26.7729988507274,-14.2482318268449));
#35129=CARTESIAN_POINT('Ctrl Pts',(-23.5491615873628,26.7730039522033,-14.2487057534324));
#35130=CARTESIAN_POINT('Ctrl Pts',(-23.5459450672254,26.7730012581993,-14.248902989566));
#35131=CARTESIAN_POINT('Ctrl Pts',(-23.5396874115666,26.7729866487757,-14.2492870037418));
#35132=CARTESIAN_POINT('Ctrl Pts',(-23.5366462778263,26.7729752440795,-14.2494737655132));
#35133=CARTESIAN_POINT('Ctrl Pts',(-23.5293724543417,26.7729376700925,-14.24992079268));
#35134=CARTESIAN_POINT('Ctrl Pts',(-23.5251397993997,26.7729074665709,-14.2501811844316));
#35135=CARTESIAN_POINT('Ctrl Pts',(-23.5126176743434,26.7727934395002,-14.2509523346288));
#35136=CARTESIAN_POINT('Ctrl Pts',(-23.5043285012374,26.7726859703146,-14.2514638345715));
#35137=CARTESIAN_POINT('Ctrl Pts',(-23.4390418115037,26.7715875716286,-14.2555007015803));
#35138=CARTESIAN_POINT('Ctrl Pts',(-23.3820823961684,26.7691165233904,-14.2590723078735));
#35139=CARTESIAN_POINT('Ctrl Pts',(-23.1845567442088,26.7552903796023,-14.271642038286));
#35140=CARTESIAN_POINT('Ctrl Pts',(-23.0447079933374,26.7362244083592,-14.2808749312802));
#35141=CARTESIAN_POINT('Ctrl Pts',(-22.6672263459862,26.6592794960374,-14.3066071317356));
#35142=CARTESIAN_POINT('Ctrl Pts',(-22.4342138532829,26.5834420348808,-14.323442301079));
#35143=CARTESIAN_POINT('Ctrl Pts',(-22.1959241754897,26.474671252359,-14.3406083269416));
#35144=CARTESIAN_POINT('Ctrl Pts',(-22.1799007748588,26.4671972067472,-14.3417619806383));
#35145=CARTESIAN_POINT('Ctrl Pts',(-22.1340809458916,26.4453638517106,-14.3450574533542));
#35146=CARTESIAN_POINT('Ctrl Pts',(-22.1044429561877,26.4306771938573,-14.3471848573424));
#35147=CARTESIAN_POINT('Ctrl Pts',(-22.0750360145738,26.4155367741587,-14.3492876249023));
#35148=CARTESIAN_POINT('',(-26.7730011641602,23.5472836196309,-14.1857734492732));
#35149=CARTESIAN_POINT('Ctrl Pts',(-22.0750361948364,26.4155368669684,-14.5938261690085));
#35150=CARTESIAN_POINT('Ctrl Pts',(-22.1529748938833,26.4556642779524,-14.5879327433542));
#35151=CARTESIAN_POINT('Ctrl Pts',(-22.2325420634903,26.4926071512902,-14.581991238956));
#35152=CARTESIAN_POINT('Ctrl Pts',(-22.4878132603249,26.5986874494668,-14.5632850366916));
#35153=CARTESIAN_POINT('Ctrl Pts',(-22.6681322416348,26.6556695193257,-14.5505680012588));
#35154=CARTESIAN_POINT('Ctrl Pts',(-22.8638382575462,26.699076082963,-14.5379327783548));
#35155=CARTESIAN_POINT('Ctrl Pts',(-22.8752687559018,26.701546111353,-14.5371990027969));
#35156=CARTESIAN_POINT('Ctrl Pts',(-22.8901593024758,26.7046790875856,-14.5362488006713));
#35157=CARTESIAN_POINT('Ctrl Pts',(-22.8936071581102,26.7053986172831,-14.5360291807727));
#35158=CARTESIAN_POINT('Ctrl Pts',(-22.8989076197223,26.7064957008315,-14.5356921704626));
#35159=CARTESIAN_POINT('Ctrl Pts',(-22.9007593759063,26.7068772762126,-14.5355745488345));
#35160=CARTESIAN_POINT('Ctrl Pts',(-22.9044381328837,26.7076319517035,-14.5353411087892));
#35161=CARTESIAN_POINT('Ctrl Pts',(-22.9062651114416,26.7080050935962,-14.5352252888435));
#35162=CARTESIAN_POINT('Ctrl Pts',(-22.9103349664637,26.70883264135,-14.5349675349158));
#35163=CARTESIAN_POINT('Ctrl Pts',(-22.9125779982417,26.7092862429528,-14.5348256479764));
#35164=CARTESIAN_POINT('Ctrl Pts',(-22.917217760309,26.7102193851504,-14.5345324991033));
#35165=CARTESIAN_POINT('Ctrl Pts',(-22.9196145579069,26.7106985892683,-14.5343812565649));
#35166=CARTESIAN_POINT('Ctrl Pts',(-22.9326310479226,26.7132856465956,-14.533560919835));
#35167=CARTESIAN_POINT('Ctrl Pts',(-22.9432609350784,26.715342734628,-14.5328947107282));
#35168=CARTESIAN_POINT('Ctrl Pts',(-23.04445356753,26.7343969117425,-14.5265862225262));
#35169=CARTESIAN_POINT('Ctrl Pts',(-23.1357054217989,26.7475580080232,-14.5211526117193));
#35170=CARTESIAN_POINT('Ctrl Pts',(-23.3786046763016,26.7720141111179,-14.5070656259211));
#35171=CARTESIAN_POINT('Ctrl Pts',(-23.5307008236378,26.7765249800005,-14.4986228120105));
#35172=CARTESIAN_POINT('Ctrl Pts',(-23.7875013464481,26.7659737404454,-14.484256001229));
#35173=CARTESIAN_POINT('Ctrl Pts',(-23.8921709884389,26.7565339244768,-14.4783700186535));
#35174=CARTESIAN_POINT('Ctrl Pts',(-24.1466701526975,26.7209764347829,-14.4637083241453));
#35175=CARTESIAN_POINT('Ctrl Pts',(-24.2954556135771,26.689339464077,-14.45482767804));
#35176=CARTESIAN_POINT('Ctrl Pts',(-24.4522229871592,26.6442293742173,-14.4449056876568));
#35177=CARTESIAN_POINT('Ctrl Pts',(-24.4629871015457,26.6410710324498,-14.4442215634225));
#35178=CARTESIAN_POINT('Ctrl Pts',(-24.4779465715137,26.6365967543204,-14.4432667543107));
#35179=CARTESIAN_POINT('Ctrl Pts',(-24.4821561426524,26.6353283089849,-14.4429976255283));
#35180=CARTESIAN_POINT('Ctrl Pts',(-24.4894099896754,26.6331263485544,-14.4425330921687));
#35181=CARTESIAN_POINT('Ctrl Pts',(-24.4924555100992,26.6321969258939,-14.4423378220439));
#35182=CARTESIAN_POINT('Ctrl Pts',(-24.4987457200043,26.6302671035853,-14.4419340210756));
#35183=CARTESIAN_POINT('Ctrl Pts',(-24.5019902142863,26.6292660871577,-14.4417254702038));
#35184=CARTESIAN_POINT('Ctrl Pts',(-24.5095508916181,26.626920316326,-14.4412388492059));
#35185=CARTESIAN_POINT('Ctrl Pts',(-24.5138658310568,26.6255716060835,-14.4409606492585));
#35186=CARTESIAN_POINT('Ctrl Pts',(-24.5228954220955,26.6227283789244,-14.4403774638809));
#35187=CARTESIAN_POINT('Ctrl Pts',(-24.5276094963504,26.6212320801872,-14.4400724202754));
#35188=CARTESIAN_POINT('Ctrl Pts',(-24.560537114989,26.6106969974119,-14.4379376196246));
#35189=CARTESIAN_POINT('Ctrl Pts',(-24.5886275212507,26.6012806458792,-14.4360954345587));
#35190=CARTESIAN_POINT('Ctrl Pts',(-24.6670256066189,26.5737922925714,-14.4308932247388));
#35191=CARTESIAN_POINT('Ctrl Pts',(-24.7170174009859,26.5548546647446,-14.4275048550132));
#35192=CARTESIAN_POINT('Ctrl Pts',(-24.8792879911885,26.488723706357,-14.4162663795987));
#35193=CARTESIAN_POINT('Ctrl Pts',(-24.9893557575942,26.4364133924099,-14.4082547827664));
#35194=CARTESIAN_POINT('Ctrl Pts',(-25.1783747031892,26.3330764031351,-14.3938506268614));
#35195=CARTESIAN_POINT('Ctrl Pts',(-25.2585584521191,26.2845861469276,-14.3875191880015));
#35196=CARTESIAN_POINT('Ctrl Pts',(-25.4645677693668,26.1474017314385,-14.3707653515543));
#35197=CARTESIAN_POINT('Ctrl Pts',(-25.5863596408755,26.0530631311435,-14.3603428258114));
#35198=CARTESIAN_POINT('Ctrl Pts',(-25.7049823542067,25.9467679678763,-14.3499454415899));
#35199=CARTESIAN_POINT('Ctrl Pts',(-25.7090032614252,25.9431466228489,-14.3495927060471));
#35200=CARTESIAN_POINT('Ctrl Pts',(-25.7184808567197,25.9345674956429,-14.348760609184));
#35201=CARTESIAN_POINT('Ctrl Pts',(-25.7239297142545,25.9296010611565,-14.348281691453));
#35202=CARTESIAN_POINT('Ctrl Pts',(-25.7321197451101,25.9220845327543,-14.347561105084));
#35203=CARTESIAN_POINT('Ctrl Pts',(-25.7348735618021,25.9195483201717,-14.3473186884582));
#35204=CARTESIAN_POINT('Ctrl Pts',(-25.7411772231156,25.9137224346399,-14.3467635030599));
#35205=CARTESIAN_POINT('Ctrl Pts',(-25.7447240984481,25.9104295438876,-14.3464509141872));
#35206=CARTESIAN_POINT('Ctrl Pts',(-25.7503301009169,25.9052014136746,-14.3459565489124));
#35207=CARTESIAN_POINT('Ctrl Pts',(-25.7523941097658,25.9032714473814,-14.345774468762));
#35208=CARTESIAN_POINT('Ctrl Pts',(-25.7829900701246,25.8745869574742,-14.3430744534272));
#35209=CARTESIAN_POINT('Ctrl Pts',(-25.8110368073388,25.847316362196,-14.3405872370274));
#35210=CARTESIAN_POINT('Ctrl Pts',(-25.8419373361861,25.8161565523279,-14.3378402368675));
#35211=CARTESIAN_POINT('Ctrl Pts',(-25.8452855631034,25.8127652187962,-14.3375424956511));
#35212=CARTESIAN_POINT('Ctrl Pts',(-25.8503147292063,25.8076486537209,-14.3370951588641));
#35213=CARTESIAN_POINT('Ctrl Pts',(-25.8520012583047,25.8059289632343,-14.3369451245644));
#35214=CARTESIAN_POINT('Ctrl Pts',(-25.8549180935857,25.8029480980112,-14.3366856096098));
#35215=CARTESIAN_POINT('Ctrl Pts',(-25.8561492932698,25.8016878053947,-14.336576058096));
#35216=CARTESIAN_POINT('Ctrl Pts',(-25.8587116745477,25.7990605690405,-14.3363480392613));
#35217=CARTESIAN_POINT('Ctrl Pts',(-25.8600426742777,25.7976934542324,-14.3362295866796));
#35218=CARTESIAN_POINT('Ctrl Pts',(-25.8632012504843,25.7944434041925,-14.3359484607114));
#35219=CARTESIAN_POINT('Ctrl Pts',(-25.8650277482358,25.7925594118868,-14.335785872824));
#35220=CARTESIAN_POINT('Ctrl Pts',(-25.8688758974944,25.7885804178831,-14.3354432727126));
#35221=CARTESIAN_POINT('Ctrl Pts',(-25.8708970169311,25.7864849015126,-14.335263302104));
#35222=CARTESIAN_POINT('Ctrl Pts',(-25.8868846540543,25.7698637463973,-14.3338394112749));
#35223=CARTESIAN_POINT('Ctrl Pts',(-25.9007179102175,25.7552097134203,-14.3326057499154));
#35224=CARTESIAN_POINT('Ctrl Pts',(-26.0029332399891,25.6448744280127,-14.323468906908));
#35225=CARTESIAN_POINT('Ctrl Pts',(-26.0855903906801,25.5440313185129,-14.315958498784));
#35226=CARTESIAN_POINT('Ctrl Pts',(-26.187870094986,25.4025625020677,-14.3060774700461));
#35227=CARTESIAN_POINT('Ctrl Pts',(-26.2130739087754,25.3661437935234,-14.3035879545081));
#35228=CARTESIAN_POINT('Ctrl Pts',(-26.2628664158555,25.290928247686,-14.2985325526093));
#35229=CARTESIAN_POINT('Ctrl Pts',(-26.287392209136,25.2521022491927,-14.2959678251093));
#35230=CARTESIAN_POINT('Ctrl Pts',(-26.4468880762129,24.9872377639166,-14.2786921335534));
#35231=CARTESIAN_POINT('Ctrl Pts',(-26.5545299934082,24.745959264001,-14.2639088453605));
#35232=CARTESIAN_POINT('Ctrl Pts',(-26.6363833815997,24.4787873842402,-14.2469685661757));
#35233=CARTESIAN_POINT('Ctrl Pts',(-26.6410170174616,24.4632451240166,-14.2459815744053));
#35234=CARTESIAN_POINT('Ctrl Pts',(-26.647128904575,24.4421645991918,-14.2446406132537));
#35235=CARTESIAN_POINT('Ctrl Pts',(-26.6487100387485,24.4366562102536,-14.2442900083879));
#35236=CARTESIAN_POINT('Ctrl Pts',(-26.6511721334537,24.4279916292927,-14.2437381764648));
#35237=CARTESIAN_POINT('Ctrl Pts',(-26.6520629924532,24.4248382424324,-14.2435372725999));
#35238=CARTESIAN_POINT('Ctrl Pts',(-26.6537664972082,24.4187729792357,-14.2431507145183));
#35239=CARTESIAN_POINT('Ctrl Pts',(-26.6545798584962,24.4158613058583,-14.2429650838459));
#35240=CARTESIAN_POINT('Ctrl Pts',(-26.6564847171522,24.4090050708421,-14.2425278269855));
#35241=CARTESIAN_POINT('Ctrl Pts',(-26.6575727977719,24.4050595726373,-14.2422760898469));
#35242=CARTESIAN_POINT('Ctrl Pts',(-26.6598027881911,24.3969128644017,-14.2417560634275));
#35243=CARTESIAN_POINT('Ctrl Pts',(-26.6609437060333,24.3927113937467,-14.2414877424238));
#35244=CARTESIAN_POINT('Ctrl Pts',(-26.663866378184,24.3818616655537,-14.2407944988928));
#35245=CARTESIAN_POINT('Ctrl Pts',(-26.6656353472703,24.3752100141166,-14.2403691615185));
#35246=CARTESIAN_POINT('Ctrl Pts',(-26.6797216155946,24.3215515487727,-14.2369352616329));
#35247=CARTESIAN_POINT('Ctrl Pts',(-26.6909950379124,24.2742794743362,-14.2338930518393));
#35248=CARTESIAN_POINT('Ctrl Pts',(-26.7491504470632,24.0034163399461,-14.2163531150854));
#35249=CARTESIAN_POINT('Ctrl Pts',(-26.773211034177,23.7756419122829,-14.2011169766266));
#35250=CARTESIAN_POINT('Ctrl Pts',(-26.7730011706773,23.5472907023771,-14.185668766916));
#35251=CARTESIAN_POINT('Ctrl Pts',(-26.7730011641601,23.5472836196309,-14.1857734492732));
#35252=CARTESIAN_POINT('Ctrl Pts',(-26.7728767773161,23.4122619271285,-14.1774340875472));
#35253=CARTESIAN_POINT('Ctrl Pts',(-26.7642634230747,23.2776162714252,-14.1690947258212));
#35254=CARTESIAN_POINT('Ctrl Pts',(-26.7473235194452,23.1442295498557,-14.1607553640952));
#35255=CARTESIAN_POINT('Ctrl Pts',(-26.7336796613005,23.0367962640898,-14.1540386158246));
#35256=CARTESIAN_POINT('Ctrl Pts',(-26.7146351950569,22.9301788636574,-14.1473218675541));
#35257=CARTESIAN_POINT('Ctrl Pts',(-26.6902963387095,22.8248268273487,-14.1406051192835));
#35258=CARTESIAN_POINT('Ctrl Pts',(-26.6679311051526,22.72801772243,-14.1344330279712));
#35259=CARTESIAN_POINT('Ctrl Pts',(-26.6410452778483,22.632073382233,-14.1282609366589));
#35260=CARTESIAN_POINT('Ctrl Pts',(-26.6097205700781,22.5374480665544,-14.1220888453465));
#35261=CARTESIAN_POINT('Ctrl Pts',(-26.5784383041901,22.4429509588235,-14.1159251166077));
#35262=CARTESIAN_POINT('Ctrl Pts',(-26.5427292471014,22.3497697322221,-14.1097613878689));
#35263=CARTESIAN_POINT('Ctrl Pts',(-26.502725916035,22.2583475517289,-14.1035976591301));
#35264=CARTESIAN_POINT('Ctrl Pts',(-26.4627649647434,22.1670222244556,-14.0974404602834));
#35265=CARTESIAN_POINT('Ctrl Pts',(-26.4185189572323,22.0774526341689,-14.0912832614368));
#35266=CARTESIAN_POINT('Ctrl Pts',(-26.3701696101475,21.9900649682432,-14.0851260625901));
#35267=CARTESIAN_POINT('Ctrl Pts',(-26.3218556035036,21.902741177402,-14.0789733642824));
#35268=CARTESIAN_POINT('Ctrl Pts',(-26.2694444300505,21.8175965190385,-14.0728206659747));
#35269=CARTESIAN_POINT('Ctrl Pts',(-26.2131647341598,21.735034593137,-14.066667967667));
#35270=CARTESIAN_POINT('Ctrl Pts',(-26.1569063796098,21.6525039748352,-14.0605176024712));
#35271=CARTESIAN_POINT('Ctrl Pts',(-26.0967826618406,21.5725545015265,-14.0543672372754));
#35272=CARTESIAN_POINT('Ctrl Pts',(-26.033066257837,21.4955619068611,-14.0482168720797));
#35273=CARTESIAN_POINT('Ctrl Pts',(-25.9693569691713,21.4185779101122,-14.0420671937075));
#35274=CARTESIAN_POINT('Ctrl Pts',(-25.9020560688728,21.3445504701877,-14.0359175153353));
#35275=CARTESIAN_POINT('Ctrl Pts',(-25.8314766970087,21.2738224602698,-14.029767836963));
#35276=CARTESIAN_POINT('Ctrl Pts',(-25.7608863249723,21.2030834270136,-14.0236172001306));
#35277=CARTESIAN_POINT('Ctrl Pts',(-25.6870167733329,21.1356451526846,-14.0174665632981));
#35278=CARTESIAN_POINT('Ctrl Pts',(-25.6102174981083,21.0718131235895,-14.0113159264657));
#35279=CARTESIAN_POINT('Ctrl Pts',(-25.5333360637923,21.0079128076322,-14.0051587097439));
#35280=CARTESIAN_POINT('Ctrl Pts',(-25.4535189819524,20.9476267190143,-13.9990014930221));
#35281=CARTESIAN_POINT('Ctrl Pts',(-25.3711481098542,20.8912194638409,-13.9928442763002));
#35282=CARTESIAN_POINT('Ctrl Pts',(-25.2887312833839,20.8347807392909,-13.9866836244924));
#35283=CARTESIAN_POINT('Ctrl Pts',(-25.2037581987513,20.7822253862395,-13.9805229726846));
#35284=CARTESIAN_POINT('Ctrl Pts',(-25.1166371570558,20.7337730327575,-13.9743623208768));
#35285=CARTESIAN_POINT('Ctrl Pts',(-25.0293703308769,20.6852396012582,-13.9681913601078));
#35286=CARTESIAN_POINT('Ctrl Pts',(-24.9399487573529,20.6408230768919,-13.9620203993388));
#35287=CARTESIAN_POINT('Ctrl Pts',(-24.8488027644645,20.6006958098337,-13.9558494385697));
#35288=CARTESIAN_POINT('Ctrl Pts',(-24.7792293167448,20.5700659134627,-13.9511390283494));
#35289=CARTESIAN_POINT('Ctrl Pts',(-24.7086515831127,20.5419341992923,-13.946428618129));
#35290=CARTESIAN_POINT('Ctrl Pts',(-24.6372665088554,20.5163576462448,-13.9417182079087));
#35291=CARTESIAN_POINT('Ctrl Pts',(-24.5437300277332,20.4828444672477,-13.9355461165964));
#35292=CARTESIAN_POINT('Ctrl Pts',(-24.4484775151185,20.45360198161,-13.929374025284));
#35293=CARTESIAN_POINT('Ctrl Pts',(-24.3519353168928,20.4288069892546,-13.9232019339717));
#35294=CARTESIAN_POINT('Ctrl Pts',(-24.2555239238012,20.4040455916624,-13.9170382052329));
#35295=CARTESIAN_POINT('Ctrl Pts',(-24.1578267352732,20.3837198173159,-13.9108744764941));
#35296=CARTESIAN_POINT('Ctrl Pts',(-24.0592882246176,20.3679577267099,-13.9047107477554));
#35297=CARTESIAN_POINT('Ctrl Pts',(-23.9608541062657,20.3522123345595,-13.8985535489087));
#35298=CARTESIAN_POINT('Ctrl Pts',(-23.8615808643558,20.3410210823747,-13.892396350062));
#35299=CARTESIAN_POINT('Ctrl Pts',(-23.7619252830272,20.3344614612353,-13.8862391512153));
#35300=CARTESIAN_POINT('Ctrl Pts',(-23.6623425438852,20.3279066347812,-13.8800864529076));
#35301=CARTESIAN_POINT('Ctrl Pts',(-23.5623784531072,20.3259767369911,-13.8739337545999));
#35302=CARTESIAN_POINT('Ctrl Pts',(-23.4624961581072,20.3286975684203,-13.8677810562922));
#35303=CARTESIAN_POINT('Ctrl Pts',(-23.3626517386156,20.3314173681063,-13.8616306910965));
#35304=CARTESIAN_POINT('Ctrl Pts',(-23.2628894870293,20.338784381014,-13.8554803259007));
#35305=CARTESIAN_POINT('Ctrl Pts',(-23.1636729078426,20.3507722993873,-13.849329960705));
#35306=CARTESIAN_POINT('Ctrl Pts',(-23.064467408369,20.3627588790458,-13.8431802823328));
#35307=CARTESIAN_POINT('Ctrl Pts',(-22.9658078914109,20.3793652861328,-13.8370306039605));
#35308=CARTESIAN_POINT('Ctrl Pts',(-22.8681520874105,20.4005134081464,-13.8308809255883));
#35309=CARTESIAN_POINT('Ctrl Pts',(-22.7704810632311,20.4216648262077,-13.8247302887559));
#35310=CARTESIAN_POINT('Ctrl Pts',(-22.6738144873285,20.4473592732172,-13.8185796519234));
#35311=CARTESIAN_POINT('Ctrl Pts',(-22.57859826625,20.4774678742631,-13.812429015091));
#35312=CARTESIAN_POINT('Ctrl Pts',(-22.4832801838168,20.5076086851872,-13.8062717983692));
#35313=CARTESIAN_POINT('Ctrl Pts',(-22.3894159695468,20.542172948723,-13.8001145816474));
#35314=CARTESIAN_POINT('Ctrl Pts',(-22.2974346510364,20.5809824327635,-13.7939573649256));
#35315=CARTESIAN_POINT('Ctrl Pts',(-22.2054020165251,20.6198135684562,-13.7877967131178));
#35316=CARTESIAN_POINT('Ctrl Pts',(-22.1152547617075,20.662894453953,-13.7816360613099));
#35317=CARTESIAN_POINT('Ctrl Pts',(-22.0273983674179,20.7100002969717,-13.7754754095021));
#35318=CARTESIAN_POINT('Ctrl Pts',(-21.9393949581386,20.7571849648167,-13.7693044487331));
#35319=CARTESIAN_POINT('Ctrl Pts',(-21.8536904396184,20.8084078205895,-13.7631334879641));
#35320=CARTESIAN_POINT('Ctrl Pts',(-21.7706624234681,20.8633999847159,-13.756962527195));
#35321=CARTESIAN_POINT('Ctrl Pts',(-21.7072855798137,20.9053765361217,-13.7522521169746));
#35322=CARTESIAN_POINT('Ctrl Pts',(-21.6454676396496,20.9495483835006,-13.7475417067542));
#35323=CARTESIAN_POINT('Ctrl Pts',(-21.5853629975758,20.9957806330013,-13.7428312965338));
#35324=CARTESIAN_POINT('Ctrl Pts',(-21.5066073644536,21.0563591499753,-13.7366592052214));
#35325=CARTESIAN_POINT('Ctrl Pts',(-21.4305171495401,21.1206898838442,-13.7304871139091));
#35326=CARTESIAN_POINT('Ctrl Pts',(-21.3574715555996,21.188509710518,-13.7243150225968));
#35327=CARTESIAN_POINT('Ctrl Pts',(-21.2845249312174,21.2562376480314,-13.718151293858));
#35328=CARTESIAN_POINT('Ctrl Pts',(-21.2146150441517,21.3274449892226,-13.7119875651192));
#35329=CARTESIAN_POINT('Ctrl Pts',(-21.1480898905112,21.4018270133658,-13.7058238363804));
#35330=CARTESIAN_POINT('Ctrl Pts',(-21.0816352140273,21.4761302367355,-13.6996666375337));
#35331=CARTESIAN_POINT('Ctrl Pts',(-21.0185584300508,21.5536011345486,-13.693509438687));
#35332=CARTESIAN_POINT('Ctrl Pts',(-20.9591716443192,21.6338972938586,-13.6873522398404));
#35333=CARTESIAN_POINT('Ctrl Pts',(-20.8998282667267,21.7141347615454,-13.6811995415327));
#35334=CARTESIAN_POINT('Ctrl Pts',(-20.8441697824914,21.7971930367696,-13.6750468432249));
#35335=CARTESIAN_POINT('Ctrl Pts',(-20.792468248865,21.8826964121347,-13.6688941449172));
#35336=CARTESIAN_POINT('Ctrl Pts',(-20.7407863205338,21.9681673644981,-13.6627437797215));
#35337=CARTESIAN_POINT('Ctrl Pts',(-20.6930585858942,22.0560812033799,-13.6565934145257));
#35338=CARTESIAN_POINT('Ctrl Pts',(-20.6495134556182,22.1460337542148,-13.65044304933));
#35339=CARTESIAN_POINT('Ctrl Pts',(-20.6059731881137,22.235976259869,-13.6442933709578));
#35340=CARTESIAN_POINT('Ctrl Pts',(-20.5666147856328,22.3279566338457,-13.6381436925856));
#35341=CARTESIAN_POINT('Ctrl Pts',(-20.5316199535256,22.4215475567254,-13.6319940142133));
#35342=CARTESIAN_POINT('Ctrl Pts',(-20.4966196672868,22.5151530662506,-13.6258433773809));
#35343=CARTESIAN_POINT('Ctrl Pts',(-20.4659844544014,22.6103692163269,-13.6196927405484));
#35344=CARTESIAN_POINT('Ctrl Pts',(-20.4398469216358,22.7067511959412,-13.613542103716));
#35345=CARTESIAN_POINT('Ctrl Pts',(-20.4136814272008,22.8032362840269,-13.6073848869941));
#35346=CARTESIAN_POINT('Ctrl Pts',(-20.3920233350419,22.9008892720935,-13.6012276702723));
#35347=CARTESIAN_POINT('Ctrl Pts',(-20.3749546031006,22.9992528700164,-13.5950704535505));
#35348=CARTESIAN_POINT('Ctrl Pts',(-20.3578763485836,23.0976713445877,-13.5889098017427));
#35349=CARTESIAN_POINT('Ctrl Pts',(-20.3453926075317,23.1968007875181,-13.5827491499349));
#35350=CARTESIAN_POINT('Ctrl Pts',(-20.3375334380064,23.2961785512203,-13.5765884981271));
#35351=CARTESIAN_POINT('Ctrl Pts',(-20.3296611172957,23.3957226092603,-13.570417537358));
#35352=CARTESIAN_POINT('Ctrl Pts',(-20.3264288397547,23.4955153836992,-13.564246576589));
#35353=CARTESIAN_POINT('Ctrl Pts',(-20.3278145075697,23.5950938427448,-13.55807561582));
#35354=CARTESIAN_POINT('Ctrl Pts',(-20.3288722138301,23.6711039502095,-13.5533652055996));
#35355=CARTESIAN_POINT('Ctrl Pts',(-20.332619512849,23.746989176551,-13.5486547953793));
#35356=CARTESIAN_POINT('Ctrl Pts',(-20.3390263729923,23.8225467111563,-13.5439443851589));
#35357=CARTESIAN_POINT('Ctrl Pts',(-20.3474213373331,23.9215504032133,-13.5377722938466));
#35358=CARTESIAN_POINT('Ctrl Pts',(-20.36041387624,24.0203398665099,-13.5316002025343));
#35359=CARTESIAN_POINT('Ctrl Pts',(-20.377987594171,24.1184538416727,-13.5254281112219));
#35360=CARTESIAN_POINT('Ctrl Pts',(-20.3955375014517,24.2164348820989,-13.5192643824831));
#35361=CARTESIAN_POINT('Ctrl Pts',(-20.4176561746807,24.3137418296599,-13.5131006537444));
#35362=CARTESIAN_POINT('Ctrl Pts',(-20.4442753538481,24.4099171949202,-13.5069369250056));
#35363=CARTESIAN_POINT('Ctrl Pts',(-20.4708663324936,24.5059906714076,-13.5007797261589));
#35364=CARTESIAN_POINT('Ctrl Pts',(-20.5019482228957,24.6009345325774,-13.4946225273122));
#35365=CARTESIAN_POINT('Ctrl Pts',(-20.5374016536794,24.6943011099223,-13.4884653284655));
#35366=CARTESIAN_POINT('Ctrl Pts',(-20.5728291701553,24.7875994419611,-13.4823126301578));
#35367=CARTESIAN_POINT('Ctrl Pts',(-20.6126217204138,24.8793223774489,-13.4761599318501));
#35368=CARTESIAN_POINT('Ctrl Pts',(-20.6566102739965,24.96903794428,-13.4700072335424));
#35369=CARTESIAN_POINT('Ctrl Pts',(-20.700582147057,25.0587194908404,-13.4638568683467));
#35370=CARTESIAN_POINT('Ctrl Pts',(-20.7487466708534,25.1463947916281,-13.4577065031509));
#35371=CARTESIAN_POINT('Ctrl Pts',(-20.8008872721935,25.2316532074257,-13.4515561379552));
#35372=CARTESIAN_POINT('Ctrl Pts',(-20.8530220508887,25.3169021022462,-13.445406459583));
#35373=CARTESIAN_POINT('Ctrl Pts',(-20.9091317977227,25.3997342780776,-13.4392567812108));
#35374=CARTESIAN_POINT('Ctrl Pts',(-20.9689552211427,25.4797658788986,-13.4331071028386));
#35375=CARTESIAN_POINT('Ctrl Pts',(-21.0287879683631,25.5598099530723,-13.4269564660061));
#35376=CARTESIAN_POINT('Ctrl Pts',(-21.0923352816988,25.6370522372933,-13.4208058291737));
#35377=CARTESIAN_POINT('Ctrl Pts',(-21.1592946137603,25.7111407280545,-13.4146551923412));
#35378=CARTESIAN_POINT('Ctrl Pts',(-21.2263255782413,25.7853084779374,-13.4084979756194));
#35379=CARTESIAN_POINT('Ctrl Pts',(-21.296775558584,25.8563153741095,-13.4023407588976));
#35380=CARTESIAN_POINT('Ctrl Pts',(-21.370304130676,25.9238452792813,-13.3961835421757));
#35381=CARTESIAN_POINT('Ctrl Pts',(-21.4438737240572,25.9914128591106,-13.3900228903679));
#35382=CARTESIAN_POINT('Ctrl Pts',(-21.5205249963508,26.0554993062122,-13.3838622385601));
#35383=CARTESIAN_POINT('Ctrl Pts',(-21.5998849620357,26.1158292516003,-13.3777015867523));
#35384=CARTESIAN_POINT('Ctrl Pts',(-21.679377725164,26.1762601504407,-13.3715306259833));
#35385=CARTESIAN_POINT('Ctrl Pts',(-21.7615878776102,26.2329217448682,-13.3653596652142));
#35386=CARTESIAN_POINT('Ctrl Pts',(-21.8461139181537,26.285582337831,-13.3591887044452));
#35387=CARTESIAN_POINT('Ctrl Pts',(-21.910634231954,26.3257791571901,-13.3544782942248));
#35388=CARTESIAN_POINT('Ctrl Pts',(-21.9765033200759,26.3636456734935,-13.3497678840044));
#35389=CARTESIAN_POINT('Ctrl Pts',(-22.0435343211767,26.3990975251249,-13.345057473784));
#35390=CARTESIAN_POINT('Ctrl Pts',(-22.0540023958228,26.4046339578668,-13.3443218600383));
#35391=CARTESIAN_POINT('Ctrl Pts',(-22.0645031770524,26.41011385114,-13.3435862462925));
#35392=CARTESIAN_POINT('Ctrl Pts',(-22.0750360153462,26.4155367745563,-13.3428506325468));
#35393=CARTESIAN_POINT('Origin',(-23.5502525316942,23.5502525316942,-77.3107734492734));
#35394=CARTESIAN_POINT('',(-22.075036015346,26.4155367745563,-11.8463751360594));
#35395=CARTESIAN_POINT('',(-22.0750360352296,26.4155367847935,-12.0938589134715));
#35396=CARTESIAN_POINT('',(-22.0750360153461,26.4155367745563,-77.3107734492734));
#35397=CARTESIAN_POINT('',(-26.7730017570585,23.5524870146403,-12.689226550727));
#35398=CARTESIAN_POINT('Ctrl Pts',(-26.7730017570585,23.5524870146403,-12.689226550727));
#35399=CARTESIAN_POINT('Ctrl Pts',(-26.7730713768293,23.4520758376819,-12.683051009313));
#35400=CARTESIAN_POINT('Ctrl Pts',(-26.7684439056258,23.3516314719299,-12.6768754678991));
#35401=CARTESIAN_POINT('Ctrl Pts',(-26.7591366801023,23.2516221839477,-12.6706999264851));
#35402=CARTESIAN_POINT('Ctrl Pts',(-26.7498294620169,23.1516129758906,-12.6645243900065));
#35403=CARTESIAN_POINT('Ctrl Pts',(-26.7358425367357,23.0520392722014,-12.6583488535278));
#35404=CARTESIAN_POINT('Ctrl Pts',(-26.7172451528587,22.9533645187556,-12.6521733170492));
#35405=CARTESIAN_POINT('Ctrl Pts',(-26.6986429662274,22.8546642826618,-12.645996185745));
#35406=CARTESIAN_POINT('Ctrl Pts',(-26.6754280335397,22.7568638799424,-12.6398190544408));
#35407=CARTESIAN_POINT('Ctrl Pts',(-26.6477205945032,22.6604159386175,-12.6336419231366));
#35408=CARTESIAN_POINT('Ctrl Pts',(-26.6199790275691,22.5638492001183,-12.627457183316));
#35409=CARTESIAN_POINT('Ctrl Pts',(-26.5877340220277,22.4686386631177,-12.6212724434954));
#35410=CARTESIAN_POINT('Ctrl Pts',(-26.5511555595458,22.3752212215023,-12.6150877036747));
#35411=CARTESIAN_POINT('Ctrl Pts',(-26.5145540442593,22.2817449055144,-12.6088990660523));
#35412=CARTESIAN_POINT('Ctrl Pts',(-26.4736138075433,22.1900643273661,-12.6027104284298));
#35413=CARTESIAN_POINT('Ctrl Pts',(-26.4285519111379,22.1005938667685,-12.5965217908074));
#35414=CARTESIAN_POINT('Ctrl Pts',(-26.383407128174,22.010958834789,-12.5903217698452));
#35415=CARTESIAN_POINT('Ctrl Pts',(-26.3341257493065,21.9235424166777,-12.584121748883));
#35416=CARTESIAN_POINT('Ctrl Pts',(-26.2809696583642,21.8387322903266,-12.5779217279209));
#35417=CARTESIAN_POINT('Ctrl Pts',(-26.2348935038113,21.7652181469775,-12.5725474966894));
#35418=CARTESIAN_POINT('Ctrl Pts',(-26.185906855583,21.6936619245205,-12.567173265458));
#35419=CARTESIAN_POINT('Ctrl Pts',(-26.13420441032,21.6242955613944,-12.5617990342266));
#35420=CARTESIAN_POINT('Ctrl Pts',(-26.0748262035605,21.5446310458982,-12.5556269429142));
#35421=CARTESIAN_POINT('Ctrl Pts',(-26.0116558225816,21.4675747866283,-12.5494548516019));
#35422=CARTESIAN_POINT('Ctrl Pts',(-25.9449506153437,21.393509929837,-12.5432827602896));
#35423=CARTESIAN_POINT('Ctrl Pts',(-25.8783357870669,21.3195454236045,-12.5371190315508));
#35424=CARTESIAN_POINT('Ctrl Pts',(-25.8081959400041,21.2485645839149,-12.530955302812));
#35425=CARTESIAN_POINT('Ctrl Pts',(-25.7348304868387,21.1809199842461,-12.5247915740732));
#35426=CARTESIAN_POINT('Ctrl Pts',(-25.6615427574853,21.113347047682,-12.5186343752265));
#35427=CARTESIAN_POINT('Ctrl Pts',(-25.5850365333912,21.0491036172036,-12.5124771763799));
#35428=CARTESIAN_POINT('Ctrl Pts',(-25.5056494589671,20.9885069511746,-12.5063199775332));
#35429=CARTESIAN_POINT('Ctrl Pts',(-25.4263204116803,20.9279545776338,-12.5001672792255));
#35430=CARTESIAN_POINT('Ctrl Pts',(-25.3441150448641,20.87104393173,-12.4940145809178));
#35431=CARTESIAN_POINT('Ctrl Pts',(-25.2594049003968,20.8180527324375,-12.4878618826101));
#35432=CARTESIAN_POINT('Ctrl Pts',(-25.1747268781368,20.7650816274832,-12.4817115174143));
#35433=CARTESIAN_POINT('Ctrl Pts',(-25.0875463333687,20.7160272460816,-12.4755611522186));
#35434=CARTESIAN_POINT('Ctrl Pts',(-24.9982639332319,20.6711240969909,-12.4694107870228));
#35435=CARTESIAN_POINT('Ctrl Pts',(-24.9089915034387,20.6262259623244,-12.4632611086506));
#35436=CARTESIAN_POINT('Ctrl Pts',(-24.8176180730134,20.5854783334969,-12.4571114302784));
#35437=CARTESIAN_POINT('Ctrl Pts',(-24.7245681590013,20.5490693700124,-12.4509617519062));
#35438=CARTESIAN_POINT('Ctrl Pts',(-24.6315037426627,20.5126547319963,-12.4448111150737));
#35439=CARTESIAN_POINT('Ctrl Pts',(-24.5367627283256,20.4805802607415,-12.4386604782413));
#35440=CARTESIAN_POINT('Ctrl Pts',(-24.4407878665935,20.4529852878491,-12.4325098414088));
#35441=CARTESIAN_POINT('Ctrl Pts',(-24.3447103319206,20.4253607941325,-12.426352624687));
#35442=CARTESIAN_POINT('Ctrl Pts',(-24.2473967323311,20.4022254884456,-12.4201954079652));
#35443=CARTESIAN_POINT('Ctrl Pts',(-24.1493030635705,20.3836682484706,-12.4140381912434));
#35444=CARTESIAN_POINT('Ctrl Pts',(-24.0511546687539,20.3651006554875,-12.4078775394356));
#35445=CARTESIAN_POINT('Ctrl Pts',(-23.9522257682191,20.3511162754397,-12.4017168876277));
#35446=CARTESIAN_POINT('Ctrl Pts',(-23.8529785009793,20.3417521732681,-12.3955562358199));
#35447=CARTESIAN_POINT('Ctrl Pts',(-23.7535651577685,20.3323724016236,-12.3893852750509));
#35448=CARTESIAN_POINT('Ctrl Pts',(-23.6538328178349,20.327628371727,-12.3832143142819));
#35449=CARTESIAN_POINT('Ctrl Pts',(-23.5542447946509,20.3275050044534,-12.3770433535128));
#35450=CARTESIAN_POINT('Ctrl Pts',(-23.4782273866993,20.3274108358972,-12.3723329432924));
#35451=CARTESIAN_POINT('Ctrl Pts',(-23.4022940911173,20.3300078435913,-12.3676225330721));
#35452=CARTESIAN_POINT('Ctrl Pts',(-23.326648150292,20.3352690724649,-12.3629121228517));
#35453=CARTESIAN_POINT('Ctrl Pts',(-23.2275286187997,20.3421629062296,-12.3567400315394));
#35454=CARTESIAN_POINT('Ctrl Pts',(-23.1285536261054,20.3536570328534,-12.350567940227));
#35455=CARTESIAN_POINT('Ctrl Pts',(-23.0301846270619,20.3697420479713,-12.3443958489147));
#35456=CARTESIAN_POINT('Ctrl Pts',(-22.9319489082871,20.3858052694839,-12.3382321201759));
#35457=CARTESIAN_POINT('Ctrl Pts',(-22.8343179761455,20.4064469466979,-12.3320683914372));
#35458=CARTESIAN_POINT('Ctrl Pts',(-22.7377503018681,20.4316057596106,-12.3259046626984));
#35459=CARTESIAN_POINT('Ctrl Pts',(-22.6412849319784,20.4567379191222,-12.3197474638517));
#35460=CARTESIAN_POINT('Ctrl Pts',(-22.5458809985728,20.486377591447,-12.313590265005));
#35461=CARTESIAN_POINT('Ctrl Pts',(-22.4519879275536,20.5204122022722,-12.3074330661583));
#35462=CARTESIAN_POINT('Ctrl Pts',(-22.3581634866755,20.5544219358608,-12.3012803678506));
#35463=CARTESIAN_POINT('Ctrl Pts',(-22.2658481197188,20.5928200735007,-12.2951276695429));
#35464=CARTESIAN_POINT('Ctrl Pts',(-22.1754763104521,20.6354441496548,-12.2889749712352));
#35465=CARTESIAN_POINT('Ctrl Pts',(-22.085138770304,20.6780520626985,-12.2828246060394));
#35466=CARTESIAN_POINT('Ctrl Pts',(-21.9967437158916,20.7248825450383,-12.2766742408437));
#35467=CARTESIAN_POINT('Ctrl Pts',(-21.9107050209418,20.7757252706125,-12.270523875648));
#35468=CARTESIAN_POINT('Ctrl Pts',(-21.8246759341047,20.8265623184781,-12.2643741972757));
#35469=CARTESIAN_POINT('Ctrl Pts',(-21.7410030575587,20.8814104977851,-12.2582245189035));
#35470=CARTESIAN_POINT('Ctrl Pts',(-21.6600741625112,20.940014363409,-12.2520748405313));
#35471=CARTESIAN_POINT('Ctrl Pts',(-21.5791326542628,20.9986273627587,-12.2459242036988));
#35472=CARTESIAN_POINT('Ctrl Pts',(-21.5009363288369,21.0609969562621,-12.2397735668664));
#35473=CARTESIAN_POINT('Ctrl Pts',(-21.4258417337178,21.1268259650449,-12.2336229300339));
#35474=CARTESIAN_POINT('Ctrl Pts',(-21.3506668031569,21.1927253970387,-12.2274657133121));
#35475=CARTESIAN_POINT('Ctrl Pts',(-21.2786005563182,21.2620913476259,-12.2213084965903));
#35476=CARTESIAN_POINT('Ctrl Pts',(-21.2099642525184,21.3345882220903,-12.2151512798685));
#35477=CARTESIAN_POINT('Ctrl Pts',(-21.1412896568058,21.4071255422641,-12.2089906280607));
#35478=CARTESIAN_POINT('Ctrl Pts',(-21.0760490986054,21.4827969358819,-12.2028299762528));
#35479=CARTESIAN_POINT('Ctrl Pts',(-21.0145235670017,21.5612336328097,-12.196669324445));
#35480=CARTESIAN_POINT('Ctrl Pts',(-20.9528950813049,21.639801582224,-12.190498363676));
#35481=CARTESIAN_POINT('Ctrl Pts',(-20.8949942916683,21.7211437238712,-12.184327402907));
#35482=CARTESIAN_POINT('Ctrl Pts',(-20.8410589523442,21.8048621134471,-12.1781564421379));
#35483=CARTESIAN_POINT('Ctrl Pts',(-20.7998890951534,21.8687659320989,-12.1734460319175));
#35484=CARTESIAN_POINT('Ctrl Pts',(-20.7610288359968,21.9340536804532,-12.1687356216972));
#35485=CARTESIAN_POINT('Ctrl Pts',(-20.7245653582472,22.0005397969213,-12.1640252114768));
#35486=CARTESIAN_POINT('Ctrl Pts',(-20.6767869475132,22.0876571312179,-12.1578531201645));
#35487=CARTESIAN_POINT('Ctrl Pts',(-20.6329569696939,22.1771395159093,-12.1516810288521));
#35488=CARTESIAN_POINT('Ctrl Pts',(-20.5933169486501,22.2685936378275,-12.1455089375398));
#35489=CARTESIAN_POINT('Ctrl Pts',(-20.553730635916,22.3599238484516,-12.139345208801));
#35490=CARTESIAN_POINT('Ctrl Pts',(-20.5183231675958,22.4532200913351,-12.1331814800623));
#35491=CARTESIAN_POINT('Ctrl Pts',(-20.4872907772788,22.5480635008778,-12.1270177513235));
#35492=CARTESIAN_POINT('Ctrl Pts',(-20.4562912628667,22.6428064327301,-12.1208605524768));
#35493=CARTESIAN_POINT('Ctrl Pts',(-20.4296577460297,22.7390928620219,-12.1147033536301));
#35494=CARTESIAN_POINT('Ctrl Pts',(-20.4075384498623,22.8364838280126,-12.1085461547834));
#35495=CARTESIAN_POINT('Ctrl Pts',(-20.3854353215592,22.9338036071125,-12.1023934564757));
#35496=CARTESIAN_POINT('Ctrl Pts',(-20.3678399496428,23.0322258954301,-12.0962407581679));
#35497=CARTESIAN_POINT('Ctrl Pts',(-20.3548505060269,23.1312973349708,-12.0900880598602));
#35498=CARTESIAN_POINT('Ctrl Pts',(-20.3418659880266,23.2303312064806,-12.0839376946645));
#35499=CARTESIAN_POINT('Ctrl Pts',(-20.3334839843102,23.3300133098615,-12.0777873294687));
#35500=CARTESIAN_POINT('Ctrl Pts',(-20.3297512603281,23.42988175605,-12.071636964273));
#35501=CARTESIAN_POINT('Ctrl Pts',(-20.3260189531867,23.5297390497301,-12.0654872859008));
#35502=CARTESIAN_POINT('Ctrl Pts',(-20.3269349097758,23.6297822107471,-12.0593376075286));
#35503=CARTESIAN_POINT('Ctrl Pts',(-20.3324938266029,23.7295469217595,-12.0531879291564));
#35504=CARTESIAN_POINT('Ctrl Pts',(-20.3380536098168,23.8293271816354,-12.0470372923239));
#35505=CARTESIAN_POINT('Ctrl Pts',(-20.3482577664134,23.9288284715368,-12.0408866554914));
#35506=CARTESIAN_POINT('Ctrl Pts',(-20.3630490038501,24.0275901843031,-12.034736018659));
#35507=CARTESIAN_POINT('Ctrl Pts',(-20.3778560648037,24.1264575513552,-12.0285788019372));
#35508=CARTESIAN_POINT('Ctrl Pts',(-20.3972599413504,24.2245833308896,-12.0224215852153));
#35509=CARTESIAN_POINT('Ctrl Pts',(-20.4211519463045,24.3215158388819,-12.0162643684935));
#35510=CARTESIAN_POINT('Ctrl Pts',(-20.4450572805103,24.4185024251232,-12.0101037166857));
#35511=CARTESIAN_POINT('Ctrl Pts',(-20.4734556061434,24.5142939975477,-12.003943064878));
#35512=CARTESIAN_POINT('Ctrl Pts',(-20.5061885572147,24.6084548194333,-11.9977824130702));
#35513=CARTESIAN_POINT('Ctrl Pts',(-20.5389762821533,24.7027732058582,-11.9916114523011));
#35514=CARTESIAN_POINT('Ctrl Pts',(-20.5761129593124,24.7954549875517,-11.9854404915321));
#35515=CARTESIAN_POINT('Ctrl Pts',(-20.6173923077243,24.8860850321056,-11.979269530763));
#35516=CARTESIAN_POINT('Ctrl Pts',(-20.6489016094245,24.9552646467752,-11.9745591205426));
#35517=CARTESIAN_POINT('Ctrl Pts',(-20.6828236700518,25.0232492305408,-11.9698487103222));
#35518=CARTESIAN_POINT('Ctrl Pts',(-20.719049499837,25.0898651306627,-11.9651383001018));
#35519=CARTESIAN_POINT('Ctrl Pts',(-20.7665108309347,25.1771420629181,-11.9589669483232));
#35520=CARTESIAN_POINT('Ctrl Pts',(-20.8180952248085,25.2623760123839,-11.9527955965446));
#35521=CARTESIAN_POINT('Ctrl Pts',(-20.8736024092598,25.345151326772,-11.946624244766));
#35522=CARTESIAN_POINT('Ctrl Pts',(-20.9290384121267,25.4278204913332,-11.9404608070367));
#35523=CARTESIAN_POINT('Ctrl Pts',(-20.9883869704736,25.5080369280774,-11.9342973693074));
#35524=CARTESIAN_POINT('Ctrl Pts',(-21.051401799618,25.5854091795477,-11.9281339315781));
#35525=CARTESIAN_POINT('Ctrl Pts',(-21.114352687096,25.6627029207568,-11.9219767479399));
#35526=CARTESIAN_POINT('Ctrl Pts',(-21.1809621784385,25.7371578779558,-11.9158195643017));
#35527=CARTESIAN_POINT('Ctrl Pts',(-21.2509410986799,25.8084120691295,-11.9096623806635));
#35528=CARTESIAN_POINT('Ctrl Pts',(-21.3208667543957,25.8796120251038,-11.9035098835718));
#35529=CARTESIAN_POINT('Ctrl Pts',(-21.3941564353851,25.9476157509724,-11.8973573864801));
#35530=CARTESIAN_POINT('Ctrl Pts',(-21.4704818292711,26.0120956192696,-11.8912048893884));
#35531=CARTESIAN_POINT('Ctrl Pts',(-21.5467735089542,26.0765470057305,-11.8850551099576));
#35532=CARTESIAN_POINT('Ctrl Pts',(-21.626097903105,26.1374773506302,-11.8789053305267));
#35533=CARTESIAN_POINT('Ctrl Pts',(-21.7080918074273,26.1945977112176,-11.8727555510959));
#35534=CARTESIAN_POINT('Ctrl Pts',(-21.7900839706634,26.2517168588919,-11.8666059022515));
#35535=CARTESIAN_POINT('Ctrl Pts',(-21.8747451782836,26.305025930145,-11.8604562534072));
#35536=CARTESIAN_POINT('Ctrl Pts',(-21.961681939521,26.354278393947,-11.8543066045629));
#35537=CARTESIAN_POINT('Ctrl Pts',(-21.9990573084783,26.375452739304,-11.8516627817284));
#35538=CARTESIAN_POINT('Ctrl Pts',(-22.0368529107137,26.3958778709974,-11.8490189588939));
#35539=CARTESIAN_POINT('Ctrl Pts',(-22.075036015346,26.4155367745563,-11.8463751360594));
#35540=CARTESIAN_POINT('Ctrl Pts',(-26.7730016580803,23.5526254787844,-12.6871150197353));
#35541=CARTESIAN_POINT('Ctrl Pts',(-26.7728024292441,23.823202332439,-12.704858087551));
#35542=CARTESIAN_POINT('Ctrl Pts',(-26.7385252597147,24.09268227854,-12.7235107134275));
#35543=CARTESIAN_POINT('Ctrl Pts',(-26.6524087047625,24.4267739169828,-12.746450801584));
#35544=CARTESIAN_POINT('Ctrl Pts',(-26.6313266338863,24.4982223453642,-12.7513366336673));
#35545=CARTESIAN_POINT('Ctrl Pts',(-26.5975699392434,24.5995470299869,-12.7581774061602));
#35546=CARTESIAN_POINT('Ctrl Pts',(-26.5868922639258,24.6300588393201,-12.7602255931275));
#35547=CARTESIAN_POINT('Ctrl Pts',(-26.5741762559277,24.6647138032508,-12.7625342434736));
#35548=CARTESIAN_POINT('Ctrl Pts',(-26.5725864670231,24.6690180119281,-12.762820668572));
#35549=CARTESIAN_POINT('Ctrl Pts',(-26.5701751351274,24.6755038217674,-12.7632517801217));
#35550=CARTESIAN_POINT('Ctrl Pts',(-26.5693604172905,24.6776879275158,-12.7633968737986));
#35551=CARTESIAN_POINT('Ctrl Pts',(-26.5678947764696,24.6816040546985,-12.7636568756696));
#35552=CARTESIAN_POINT('Ctrl Pts',(-26.5672447330568,24.6833363957719,-12.763771836472));
#35553=CARTESIAN_POINT('Ctrl Pts',(-26.5658407572021,24.687068164387,-12.7640193659137));
#35554=CARTESIAN_POINT('Ctrl Pts',(-26.5650863300132,24.689067396865,-12.7641519038925));
#35555=CARTESIAN_POINT('Ctrl Pts',(-26.563058028894,24.6944262546565,-12.7645069775629));
#35556=CARTESIAN_POINT('Ctrl Pts',(-26.5617805192994,24.6977845148843,-12.7647292941284));
#35557=CARTESIAN_POINT('Ctrl Pts',(-26.5559648426152,24.7129959073165,-12.7657354144316));
#35558=CARTESIAN_POINT('Ctrl Pts',(-26.5513622130052,24.7248245162577,-12.7665153847189));
#35559=CARTESIAN_POINT('Ctrl Pts',(-26.5457923528426,24.7388923782542,-12.7674404885065));
#35560=CARTESIAN_POINT('Ctrl Pts',(-26.5448923985021,24.7411578902946,-12.7675893905717));
#35561=CARTESIAN_POINT('Ctrl Pts',(-26.4172435973322,25.0614366671033,-12.7886291254906));
#35562=CARTESIAN_POINT('Ctrl Pts',(-26.240613571568,25.3572862510724,-12.8067442158744));
#35563=CARTESIAN_POINT('Ctrl Pts',(-25.9815636904075,25.6665118819232,-12.8297424468919));
#35564=CARTESIAN_POINT('Ctrl Pts',(-25.9411346004929,25.7120827699075,-12.8332477659115));
#35565=CARTESIAN_POINT('Ctrl Pts',(-25.8545985970419,25.8042262006905,-12.8406175107926));
#35566=CARTESIAN_POINT('Ctrl Pts',(-25.8083144823472,25.8505923875056,-12.8444873627208));
#35567=CARTESIAN_POINT('Ctrl Pts',(-25.735542368011,25.9191798118072,-12.8504898584851));
#35568=CARTESIAN_POINT('Ctrl Pts',(-25.7100550290956,25.9424400572493,-12.8525775674002));
#35569=CARTESIAN_POINT('Ctrl Pts',(-25.6788544142718,25.9700092284564,-12.8551179743324));
#35570=CARTESIAN_POINT('Ctrl Pts',(-25.673493320229,25.974714739824,-12.8555539484492));
#35571=CARTESIAN_POINT('Ctrl Pts',(-25.6656520438504,25.9815511884352,-12.8561908556173));
#35572=CARTESIAN_POINT('Ctrl Pts',(-25.6631841442848,25.9836962344931,-12.8563912014066));
#35573=CARTESIAN_POINT('Ctrl Pts',(-25.658265413252,25.9879583675865,-12.8567902926236));
#35574=CARTESIAN_POINT('Ctrl Pts',(-25.6558146464417,25.9900755236288,-12.8569890348515));
#35575=CARTESIAN_POINT('Ctrl Pts',(-25.6509200641132,25.9942909634285,-12.8573857471995));
#35576=CARTESIAN_POINT('Ctrl Pts',(-25.6484762856836,25.9963892849485,-12.857583715443));
#35577=CARTESIAN_POINT('Ctrl Pts',(-25.6425843515558,26.0014329989903,-12.8580607698772));
#35578=CARTESIAN_POINT('Ctrl Pts',(-25.6391331234176,26.0043747782121,-12.8583400047343));
#35579=CARTESIAN_POINT('Ctrl Pts',(-25.6285185519188,26.0133838797383,-12.8591982067779));
#35580=CARTESIAN_POINT('Ctrl Pts',(-25.6213349462069,26.0194271544861,-12.859778160131));
#35581=CARTESIAN_POINT('Ctrl Pts',(-25.536977335455,26.0897666491354,-12.8665789456912));
#35582=CARTESIAN_POINT('Ctrl Pts',(-25.456872187522,26.1504458433308,-12.8729455178736));
#35583=CARTESIAN_POINT('Ctrl Pts',(-25.2979634669048,26.2595228534622,-12.885425623497));
#35584=CARTESIAN_POINT('Ctrl Pts',(-25.2196515452597,26.308466414566,-12.8915118621672));
#35585=CARTESIAN_POINT('Ctrl Pts',(-25.0845001851517,26.3850676908425,-12.9018831248896));
#35586=CARTESIAN_POINT('Ctrl Pts',(-25.0287491052723,26.4145395819322,-12.9061250645356));
#35587=CARTESIAN_POINT('Ctrl Pts',(-24.8662734538015,26.4944216102783,-12.9183524596235));
#35588=CARTESIAN_POINT('Ctrl Pts',(-24.7575956753323,26.5406313776276,-12.9263720331903));
#35589=CARTESIAN_POINT('Ctrl Pts',(-24.5623748321191,26.6112578653706,-12.9403004435979));
#35590=CARTESIAN_POINT('Ctrl Pts',(-24.4768805779146,26.6382143416627,-12.9462456511234));
#35591=CARTESIAN_POINT('Ctrl Pts',(-24.3449861284423,26.6738283268949,-12.9550807304739));
#35592=CARTESIAN_POINT('Ctrl Pts',(-24.2993384833941,26.6850887412567,-12.9580781883776));
#35593=CARTESIAN_POINT('Ctrl Pts',(-24.2486074931249,26.6964315814224,-12.9613309029506));
#35594=CARTESIAN_POINT('Ctrl Pts',(-24.2437545419645,26.6975048615279,-12.96164126881));
#35595=CARTESIAN_POINT('Ctrl Pts',(-24.2365463402488,26.6990815475519,-12.9621010696985));
#35596=CARTESIAN_POINT('Ctrl Pts',(-24.2341930063927,26.6995935405289,-12.9622509969513));
#35597=CARTESIAN_POINT('Ctrl Pts',(-24.2301768826751,26.7004625773501,-12.9625065337299));
#35598=CARTESIAN_POINT('Ctrl Pts',(-24.2285143841615,26.7008209430052,-12.9626122199212));
#35599=CARTESIAN_POINT('Ctrl Pts',(-24.2251006174136,26.7015539820446,-12.9628290401184));
#35600=CARTESIAN_POINT('Ctrl Pts',(-24.2233493243553,26.7019285108406,-12.9629401655331));
#35601=CARTESIAN_POINT('Ctrl Pts',(-24.2191344626538,26.7028262212049,-12.9632073612932));
#35602=CARTESIAN_POINT('Ctrl Pts',(-24.2166705864744,26.7033479761302,-12.9633633490377));
#35603=CARTESIAN_POINT('Ctrl Pts',(-24.2076852516814,26.7052397245907,-12.9639314652179));
#35604=CARTESIAN_POINT('Ctrl Pts',(-24.2011601008287,26.706592390931,-12.9643426021408));
#35605=CARTESIAN_POINT('Ctrl Pts',(-24.0889762482193,26.7294854660483,-12.9713872796732));
#35606=CARTESIAN_POINT('Ctrl Pts',(-23.9822928871635,26.7457324794956,-12.9777245859901));
#35607=CARTESIAN_POINT('Ctrl Pts',(-23.6925062602712,26.7750813566795,-12.9944503465642));
#35608=CARTESIAN_POINT('Ctrl Pts',(-23.5087760349682,26.7779519890575,-13.0045503956241));
#35609=CARTESIAN_POINT('Ctrl Pts',(-23.2297184306843,26.7584686244722,-13.0202613815187));
#35610=CARTESIAN_POINT('Ctrl Pts',(-23.1339985601556,26.7474581379977,-13.0257141649896));
#35611=CARTESIAN_POINT('Ctrl Pts',(-22.9584398214559,26.7192459849636,-13.0359773131177));
#35612=CARTESIAN_POINT('Ctrl Pts',(-22.8784852439815,26.7032652081371,-13.0407535763453));
#35613=CARTESIAN_POINT('Ctrl Pts',(-22.7717218795319,26.6776807952038,-13.0473148002795));
#35614=CARTESIAN_POINT('Ctrl Pts',(-22.7443057286715,26.6707280072929,-13.0490161108776));
#35615=CARTESIAN_POINT('Ctrl Pts',(-22.7052863497455,26.6602841045353,-13.0514624536307));
#35616=CARTESIAN_POINT('Ctrl Pts',(-22.6936052887585,26.657086889631,-13.0521980221621));
#35617=CARTESIAN_POINT('Ctrl Pts',(-22.6730451426903,26.6513346205017,-13.053498517771));
#35618=CARTESIAN_POINT('Ctrl Pts',(-22.6641584564048,26.6488070675682,-13.0540625477542));
#35619=CARTESIAN_POINT('Ctrl Pts',(-22.6510779734098,26.6450258407694,-13.0548956258773));
#35620=CARTESIAN_POINT('Ctrl Pts',(-22.6468756100976,26.6438017648659,-13.055163706508));
#35621=CARTESIAN_POINT('Ctrl Pts',(-22.6396045970329,26.6416677652353,-13.0556283082512));
#35622=CARTESIAN_POINT('Ctrl Pts',(-22.6365347775454,26.6407618218769,-13.0558246988591));
#35623=CARTESIAN_POINT('Ctrl Pts',(-22.6304319193563,26.6389509018736,-13.0562155984939));
#35624=CARTESIAN_POINT('Ctrl Pts',(-22.6273988537835,26.6380460270364,-13.0564101040078));
#35625=CARTESIAN_POINT('Ctrl Pts',(-22.620225375751,26.6358944015734,-13.0568706786738));
#35626=CARTESIAN_POINT('Ctrl Pts',(-22.6160861369505,26.6346437855061,-13.0571368744195));
#35627=CARTESIAN_POINT('Ctrl Pts',(-22.6037756554997,26.630897283059,-13.0579298679471));
#35628=CARTESIAN_POINT('Ctrl Pts',(-22.5956118563361,26.6283772432643,-13.0584574583748));
#35629=CARTESIAN_POINT('Ctrl Pts',(-22.5203084058696,26.6048038311013,-13.0633399615579));
#35630=CARTESIAN_POINT('Ctrl Pts',(-22.4538697177707,26.5815908513199,-13.0677657831591));
#35631=CARTESIAN_POINT('Ctrl Pts',(-22.2813592805787,26.5149042724407,-13.0795851129866));
#35632=CARTESIAN_POINT('Ctrl Pts',(-22.176809626988,26.4679358190944,-13.0870856988103));
#35633=CARTESIAN_POINT('Ctrl Pts',(-22.0750356748951,26.4155365992721,-13.0947094732148));
#35634=CARTESIAN_POINT('',(-26.7730023334763,23.5513828472991,-12.9357734492733));
#35635=CARTESIAN_POINT('Ctrl Pts',(-22.0750360153462,26.4155367745563,-13.3428506325468));
#35636=CARTESIAN_POINT('Ctrl Pts',(-22.1633950675454,26.4610292011796,-13.3366796336625));
#35637=CARTESIAN_POINT('Ctrl Pts',(-22.254012492317,26.5025088954541,-13.3305086347781));
#35638=CARTESIAN_POINT('Ctrl Pts',(-22.3464881231975,26.5397456009848,-13.3243376358938));
#35639=CARTESIAN_POINT('Ctrl Pts',(-22.4388417141158,26.5769331652867,-13.3181747808682));
#35640=CARTESIAN_POINT('Ctrl Pts',(-22.5330482372733,26.6098887097839,-13.3120119258426));
#35641=CARTESIAN_POINT('Ctrl Pts',(-22.6286833006791,26.6384279986886,-13.305849070817));
#35642=CARTESIAN_POINT('Ctrl Pts',(-22.7242204126601,26.6669380570589,-13.2996925279159));
#35643=CARTESIAN_POINT('Ctrl Pts',(-22.8211827418363,26.6910407291222,-13.2935359850148));
#35644=CARTESIAN_POINT('Ctrl Pts',(-22.9191272056496,26.7106003583305,-13.2873794421138));
#35645=CARTESIAN_POINT('Ctrl Pts',(-23.01700470997,26.7301466156463,-13.2812271081182));
#35646=CARTESIAN_POINT('Ctrl Pts',(-23.1158625892922,26.7451559197203,-13.2750747741226));
#35647=CARTESIAN_POINT('Ctrl Pts',(-23.2152448092349,26.755543062737,-13.268922440127));
#35648=CARTESIAN_POINT('Ctrl Pts',(-23.3145925100241,26.7659265979113,-13.2627722430666));
#35649=CARTESIAN_POINT('Ctrl Pts',(-23.4144637578971,26.7716911170298,-13.2566220460062));
#35650=CARTESIAN_POINT('Ctrl Pts',(-23.5143954910274,26.7728030487745,-13.2504718489458));
#35651=CARTESIAN_POINT('Ctrl Pts',(-23.6143192487935,26.773914891778,-13.244322142721));
#35652=CARTESIAN_POINT('Ctrl Pts',(-23.7143030478139,26.7703748809936,-13.2381724364963));
#35653=CARTESIAN_POINT('Ctrl Pts',(-23.8138829186434,26.7622015632912,-13.2320227302716));
#35654=CARTESIAN_POINT('Ctrl Pts',(-23.9134814825028,26.7540267113021,-13.2258718696304));
#35655=CARTESIAN_POINT('Ctrl Pts',(-24.0126755345869,26.7412168602083,-13.2197210089892));
#35656=CARTESIAN_POINT('Ctrl Pts',(-24.1110063311914,26.7238424136496,-13.213570148348));
#35657=CARTESIAN_POINT('Ctrl Pts',(-24.2094440354683,26.706449077163,-13.2074126003391));
#35658=CARTESIAN_POINT('Ctrl Pts',(-24.307016181848,26.6844813124313,-13.2012550523302));
#35659=CARTESIAN_POINT('Ctrl Pts',(-24.4032744644503,26.6580606249871,-13.1950975043213));
#35660=CARTESIAN_POINT('Ctrl Pts',(-24.4995891995657,26.6316244426249,-13.1889363451005));
#35661=CARTESIAN_POINT('Ctrl Pts',(-24.5945881236382,26.6007302717376,-13.1827751858796));
#35662=CARTESIAN_POINT('Ctrl Pts',(-24.6878403224892,26.5655487991834,-13.1766140266588));
#35663=CARTESIAN_POINT('Ctrl Pts',(-24.781245215733,26.5303097192627,-13.1704427789416));
#35664=CARTESIAN_POINT('Ctrl Pts',(-24.8728972732914,26.4907694902959,-13.1642715312244));
#35665=CARTESIAN_POINT('Ctrl Pts',(-24.9623876519566,26.4471460341588,-13.1581002835073));
#35666=CARTESIAN_POINT('Ctrl Pts',(-25.0200526659792,26.4190363396041,-13.1541237098079));
#35667=CARTESIAN_POINT('Ctrl Pts',(-25.0768206287237,26.3892321664748,-13.1501471361085));
#35668=CARTESIAN_POINT('Ctrl Pts',(-25.1325885561893,26.3578013323538,-13.1461705624091));
#35669=CARTESIAN_POINT('Ctrl Pts',(-25.2191466754743,26.3090171294487,-13.1399984710968));
#35670=CARTESIAN_POINT('Ctrl Pts',(-25.3035990662544,26.2561403120594,-13.1338263797844));
#35671=CARTESIAN_POINT('Ctrl Pts',(-25.3855330115357,26.1993775047396,-13.1276542884721));
#35672=CARTESIAN_POINT('Ctrl Pts',(-25.4673559444213,26.142691605412,-13.1214905597333));
#35673=CARTESIAN_POINT('Ctrl Pts',(-25.5466668600733,26.0821304263655,-13.1153268309945));
#35674=CARTESIAN_POINT('Ctrl Pts',(-25.6230780267043,26.0179461977995,-13.1091631022557));
#35675=CARTESIAN_POINT('Ctrl Pts',(-25.6994082428757,25.9538299663998,-13.1030059034091));
#35676=CARTESIAN_POINT('Ctrl Pts',(-25.7728444866747,25.8860985941896,-13.0968487045624));
#35677=CARTESIAN_POINT('Ctrl Pts',(-25.8430292020959,25.8150467170809,-13.0906915057157));
#35678=CARTESIAN_POINT('Ctrl Pts',(-25.9131626167464,25.7440467745856,-13.084538807408));
#35679=CARTESIAN_POINT('Ctrl Pts',(-25.9800489238839,25.6697314607662,-13.0783861091003));
#35680=CARTESIAN_POINT('Ctrl Pts',(-26.0433654836239,25.5924340543361,-13.0722334107926));
#35681=CARTESIAN_POINT('Ctrl Pts',(-26.1066580336345,25.5151659591926,-13.0660830455968));
#35682=CARTESIAN_POINT('Ctrl Pts',(-26.1663832509785,25.4349183540323,-13.0599326804011));
#35683=CARTESIAN_POINT('Ctrl Pts',(-26.2222576588591,25.3520588927954,-13.0537823152054));
#35684=CARTESIAN_POINT('Ctrl Pts',(-26.278125827133,25.2692086846398,-13.0476326368331));
#35685=CARTESIAN_POINT('Ctrl Pts',(-26.3301437980267,25.1837475604556,-13.0414829584609));
#35686=CARTESIAN_POINT('Ctrl Pts',(-26.3780710411866,25.0960727152447,-13.0353332800887));
#35687=CARTESIAN_POINT('Ctrl Pts',(-26.4260057540636,25.0083842054406,-13.0291826432562));
#35688=CARTESIAN_POINT('Ctrl Pts',(-26.4698482644615,24.9184816705158,-13.0230320064238));
#35689=CARTESIAN_POINT('Ctrl Pts',(-26.5094041600705,24.8267865902989,-13.0168813695913));
#35690=CARTESIAN_POINT('Ctrl Pts',(-26.5490023721785,24.7349934156082,-13.0107241528695));
#35691=CARTESIAN_POINT('Ctrl Pts',(-26.5843046397494,24.6414042659238,-13.0045669361477));
#35692=CARTESIAN_POINT('Ctrl Pts',(-26.615164914666,24.5464601642719,-12.9984097194259));
#35693=CARTESIAN_POINT('Ctrl Pts',(-26.6460424064036,24.4514630936946,-12.9922490676181));
#35694=CARTESIAN_POINT('Ctrl Pts',(-26.6724728553308,24.3551099846848,-12.9860884158103));
#35695=CARTESIAN_POINT('Ctrl Pts',(-26.6943608269484,24.2578545315599,-12.9799277640025));
#35696=CARTESIAN_POINT('Ctrl Pts',(-26.7162854249259,24.1604363354774,-12.9737568032334));
#35697=CARTESIAN_POINT('Ctrl Pts',(-26.7336522868242,24.0621132071905,-12.9675858424644));
#35698=CARTESIAN_POINT('Ctrl Pts',(-26.7464175512049,23.963346625765,-12.9614148816953));
#35699=CARTESIAN_POINT('Ctrl Pts',(-26.7561615171861,23.8879562397308,-12.9567044714749));
#35700=CARTESIAN_POINT('Ctrl Pts',(-26.7632254033539,23.8123076353871,-12.9519940612545));
#35701=CARTESIAN_POINT('Ctrl Pts',(-26.7676101446616,23.7366058326589,-12.9472836510341));
#35702=CARTESIAN_POINT('Ctrl Pts',(-26.7711816140072,23.6749450301463,-12.9434469171139));
#35703=CARTESIAN_POINT('Ctrl Pts',(-26.7729806591481,23.6131805757407,-12.9396101831936));
#35704=CARTESIAN_POINT('Ctrl Pts',(-26.7730023334763,23.5513828472991,-12.9357734492733));
#35705=CARTESIAN_POINT('Ctrl Pts',(-26.773002271887,23.551546590173,-12.9329876023809));
#35706=CARTESIAN_POINT('Ctrl Pts',(-26.7731524659094,23.1775003206321,-12.91081626142));
#35707=CARTESIAN_POINT('Ctrl Pts',(-26.7081903843668,22.8062196535971,-12.891201579423));
#35708=CARTESIAN_POINT('Ctrl Pts',(-26.5659400232813,22.4128476063482,-12.8667037715344));
#35709=CARTESIAN_POINT('Ctrl Pts',(-26.5500998401361,22.3717039023126,-12.8640980270859));
#35710=CARTESIAN_POINT('Ctrl Pts',(-26.5166506260304,22.2898698166229,-12.8588177209579));
#35711=CARTESIAN_POINT('Ctrl Pts',(-26.4990360226658,22.2491922455496,-12.8561434403133));
#35712=CARTESIAN_POINT('Ctrl Pts',(-26.4773907378184,22.2019059434223,-12.8529716293445));
#35713=CARTESIAN_POINT('Ctrl Pts',(-26.4741677571019,22.1949310374084,-12.8525021482509));
#35714=CARTESIAN_POINT('Ctrl Pts',(-26.4691988615638,22.184277984974,-12.851782573542));
#35715=CARTESIAN_POINT('Ctrl Pts',(-26.467470852937,22.1805914769398,-12.8515331006168));
#35716=CARTESIAN_POINT('Ctrl Pts',(-26.4643108894116,22.1738831655274,-12.8510782888982));
#35717=CARTESIAN_POINT('Ctrl Pts',(-26.4628812063443,22.1708602931425,-12.8508730292272));
#35718=CARTESIAN_POINT('Ctrl Pts',(-26.4600007483429,22.1647943970046,-12.8504605076865));
#35719=CARTESIAN_POINT('Ctrl Pts',(-26.4585498982928,22.1617514137377,-12.8502532433975));
#35720=CARTESIAN_POINT('Ctrl Pts',(-26.4544172432108,22.1531185618607,-12.8496643253296));
#35721=CARTESIAN_POINT('Ctrl Pts',(-26.4517240892132,22.1475341703223,-12.8492822763588));
#35722=CARTESIAN_POINT('Ctrl Pts',(-26.4402993689607,22.1240181097122,-12.8476688167637));
#35723=CARTESIAN_POINT('Ctrl Pts',(-26.4314177029296,22.1061602301769,-12.8464321672748));
#35724=CARTESIAN_POINT('Ctrl Pts',(-26.2679660733681,21.7850279528911,-12.8239833824949));
#35725=CARTESIAN_POINT('Ctrl Pts',(-26.0665012933793,21.5081078148008,-12.8008691448452));
#35726=CARTESIAN_POINT('Ctrl Pts',(-25.7627511569584,21.2052932954409,-12.7719682453309));
#35727=CARTESIAN_POINT('Ctrl Pts',(-25.697376919529,21.1452904159161,-12.7660378382998));
#35728=CARTESIAN_POINT('Ctrl Pts',(-25.5934001439874,21.0574807248441,-12.7571301395297));
#35729=CARTESIAN_POINT('Ctrl Pts',(-25.5565211568815,21.0277041815248,-12.7540650881623));
#35730=CARTESIAN_POINT('Ctrl Pts',(-25.5070417292952,20.989525757529,-12.7500895456775));
#35731=CARTESIAN_POINT('Ctrl Pts',(-25.4950217798436,20.9803851873211,-12.7491341250556));
#35732=CARTESIAN_POINT('Ctrl Pts',(-25.4777393646855,20.9674334765861,-12.7477756668102));
#35733=CARTESIAN_POINT('Ctrl Pts',(-25.4725291467834,20.9635534035425,-12.7473680891556));
#35734=CARTESIAN_POINT('Ctrl Pts',(-25.4633153777544,20.9567350804184,-12.74665083707));
#35735=CARTESIAN_POINT('Ctrl Pts',(-25.4593167215666,20.9537902957313,-12.7463407187368));
#35736=CARTESIAN_POINT('Ctrl Pts',(-25.4533748080266,20.9494355585704,-12.7458816272946));
#35737=CARTESIAN_POINT('Ctrl Pts',(-25.4514367802767,20.9480185338774,-12.7457321622825));
#35738=CARTESIAN_POINT('Ctrl Pts',(-25.4480420440691,20.9455422266401,-12.7454708332372));
#35739=CARTESIAN_POINT('Ctrl Pts',(-25.446586030523,20.9444819992374,-12.7453589028189));
#35740=CARTESIAN_POINT('Ctrl Pts',(-25.4436761484083,20.9423668369706,-12.7451355160898));
#35741=CARTESIAN_POINT('Ctrl Pts',(-25.4422222906469,20.941311899882,-12.7450240595706));
#35742=CARTESIAN_POINT('Ctrl Pts',(-25.4382960369615,20.9384679697673,-12.7447234750262));
#35743=CARTESIAN_POINT('Ctrl Pts',(-25.4358219727111,20.9366812663585,-12.7445345072585));
#35744=CARTESIAN_POINT('Ctrl Pts',(-25.4266980409565,20.9301119042582,-12.7438392326342));
#35745=CARTESIAN_POINT('Ctrl Pts',(-25.4200324113546,20.9253510360491,-12.7433344275144));
#35746=CARTESIAN_POINT('Ctrl Pts',(-25.298674564842,20.8393690802654,-12.734199084352));
#35747=CARTESIAN_POINT('Ctrl Pts',(-25.1787916177853,20.7656986447333,-12.7260680688597));
#35748=CARTESIAN_POINT('Ctrl Pts',(-24.9846302895578,20.6632275365289,-12.7136275151696));
#35749=CARTESIAN_POINT('Ctrl Pts',(-24.913462658014,20.6289494657348,-12.7092098757905));
#35750=CARTESIAN_POINT('Ctrl Pts',(-24.6831034968294,20.5282495849825,-12.6951594426078));
#35751=CARTESIAN_POINT('Ctrl Pts',(-24.5198177797213,20.4719751898048,-12.6855507018088));
#35752=CARTESIAN_POINT('Ctrl Pts',(-24.280927648137,20.4105483487553,-12.671278267432));
#35753=CARTESIAN_POINT('Ctrl Pts',(-24.2084179640144,20.3945520471503,-12.666921882954));
#35754=CARTESIAN_POINT('Ctrl Pts',(-24.09229813527,20.3731111426938,-12.6598674146807));
#35755=CARTESIAN_POINT('Ctrl Pts',(-24.0490156063595,20.3660295575784,-12.6572211036155));
#35756=CARTESIAN_POINT('Ctrl Pts',(-23.9980190585062,20.3587510986307,-12.6540792190819));
#35757=CARTESIAN_POINT('Ctrl Pts',(-23.9904307200801,20.3576956534772,-12.6536110862217));
#35758=CARTESIAN_POINT('Ctrl Pts',(-23.9788088422864,20.3561214152225,-12.6528931516362));
#35759=CARTESIAN_POINT('Ctrl Pts',(-23.9747779281215,20.3555831766421,-12.6526439661935));
#35760=CARTESIAN_POINT('Ctrl Pts',(-23.967430913548,20.354616297627,-12.6521894555724));
#35761=CARTESIAN_POINT('Ctrl Pts',(-23.9641151395371,20.354185185022,-12.6519842089776));
#35762=CARTESIAN_POINT('Ctrl Pts',(-23.9574521696298,20.3533294169721,-12.6515715236388));
#35763=CARTESIAN_POINT('Ctrl Pts',(-23.9541049660027,20.3529048562381,-12.6513640821726));
#35764=CARTESIAN_POINT('Ctrl Pts',(-23.9445911794907,20.3517133012875,-12.6507741103193));
#35765=CARTESIAN_POINT('Ctrl Pts',(-23.9384230612519,20.3509588882919,-12.6503911824465));
#35766=CARTESIAN_POINT('Ctrl Pts',(-23.9123335540016,20.3478444802989,-12.64876965767));
#35767=CARTESIAN_POINT('Ctrl Pts',(-23.8923928795088,20.3456527208835,-12.6475257568095));
#35768=CARTESIAN_POINT('Ctrl Pts',(-23.4875771918388,20.3049792172327,-12.6221772488443));
#35769=CARTESIAN_POINT('Ctrl Pts',(-23.0989539909326,20.3359284799628,-12.5955154780121));
#35770=CARTESIAN_POINT('Ctrl Pts',(-22.6585667973289,20.4525476658325,-12.5651690911467));
#35771=CARTESIAN_POINT('Ctrl Pts',(-22.5924433775991,20.4723503556785,-12.5606257468027));
#35772=CARTESIAN_POINT('Ctrl Pts',(-22.4997655078763,20.5033820702191,-12.5543222641361));
#35773=CARTESIAN_POINT('Ctrl Pts',(-22.4726504326853,20.5128660822901,-12.5524860455227));
#35774=CARTESIAN_POINT('Ctrl Pts',(-22.4358667874512,20.5262864680318,-12.5500094730623));
#35775=CARTESIAN_POINT('Ctrl Pts',(-22.4260860915399,20.529908815673,-12.5493523573817));
#35776=CARTESIAN_POINT('Ctrl Pts',(-22.4116949087097,20.535318279142,-12.5483877347386));
#35777=CARTESIAN_POINT('Ctrl Pts',(-22.407070791694,20.5370685814245,-12.5480781294716));
#35778=CARTESIAN_POINT('Ctrl Pts',(-22.3997572995012,20.5398561140447,-12.5475890234976));
#35779=CARTESIAN_POINT('Ctrl Pts',(-22.3970652799823,20.5408863138105,-12.5474091101355));
#35780=CARTESIAN_POINT('Ctrl Pts',(-22.3919741662415,20.5428424493237,-12.5470690950192));
#35781=CARTESIAN_POINT('Ctrl Pts',(-22.3895747934566,20.5437676467346,-12.5469089493266));
#35782=CARTESIAN_POINT('Ctrl Pts',(-22.3854284464584,20.5453721802796,-12.5466323763116));
#35783=CARTESIAN_POINT('Ctrl Pts',(-22.3836809552352,20.546050169514,-12.5465158672869));
#35784=CARTESIAN_POINT('Ctrl Pts',(-22.3802975146165,20.5473662694471,-12.5462903910306));
#35785=CARTESIAN_POINT('Ctrl Pts',(-22.3786614977482,20.5480041916677,-12.5461814125325));
#35786=CARTESIAN_POINT('Ctrl Pts',(-22.3748039385112,20.5495119799014,-12.5459245626718));
#35787=CARTESIAN_POINT('Ctrl Pts',(-22.3725828353681,20.550382977725,-12.5457767600933));
#35788=CARTESIAN_POINT('Ctrl Pts',(-22.3660113332181,20.5529683924391,-12.5453397113533));
#35789=CARTESIAN_POINT('Ctrl Pts',(-22.3616636720064,20.5546898214716,-12.5450508870859));
#35790=CARTESIAN_POINT('Ctrl Pts',(-22.3233114661414,20.5699717767936,-12.5425058044055));
#35791=CARTESIAN_POINT('Ctrl Pts',(-22.2895347842532,20.5841020304023,-12.5402833577977));
#35792=CARTESIAN_POINT('Ctrl Pts',(-22.1056225849042,20.6647499298748,-12.5282484804328));
#35793=CARTESIAN_POINT('Ctrl Pts',(-21.9604813831869,20.7420998110335,-12.5189882438998));
#35794=CARTESIAN_POINT('Ctrl Pts',(-21.6962944421301,20.9099707236333,-12.501463874872));
#35795=CARTESIAN_POINT('Ctrl Pts',(-21.5764101303173,20.9983525922383,-12.4932074765565));
#35796=CARTESIAN_POINT('Ctrl Pts',(-21.3872608185746,21.159126904729,-12.4790753960702));
#35797=CARTESIAN_POINT('Ctrl Pts',(-21.3144880751643,21.2270285346655,-12.4733271236601));
#35798=CARTESIAN_POINT('Ctrl Pts',(-21.2001398894239,21.3440782892917,-12.4636468780076));
#35799=CARTESIAN_POINT('Ctrl Pts',(-21.156687035876,21.3912996475806,-12.459797341398));
#35800=CARTESIAN_POINT('Ctrl Pts',(-21.1091636886812,21.4461437797272,-12.455373824558));
#35801=CARTESIAN_POINT('Ctrl Pts',(-21.1036777773866,21.4525251068235,-12.4548598414543));
#35802=CARTESIAN_POINT('Ctrl Pts',(-21.0954758963984,21.462141644899,-12.4540863104182));
#35803=CARTESIAN_POINT('Ctrl Pts',(-21.0927411611016,21.4653608635524,-12.4538275367802));
#35804=CARTESIAN_POINT('Ctrl Pts',(-21.0880491283552,21.4709061909218,-12.4533820731343));
#35805=CARTESIAN_POINT('Ctrl Pts',(-21.0860887739371,21.4732297154619,-12.4531955090403));
#35806=CARTESIAN_POINT('Ctrl Pts',(-21.082058712602,21.4780201115581,-12.4528110496928));
#35807=CARTESIAN_POINT('Ctrl Pts',(-21.0799894099033,21.4804873177966,-12.4526131381517));
#35808=CARTESIAN_POINT('Ctrl Pts',(-21.0750172621702,21.4864336312706,-12.4521363748397));
#35809=CARTESIAN_POINT('Ctrl Pts',(-21.0721180555479,21.4899157604236,-12.4518573748193));
#35810=CARTESIAN_POINT('Ctrl Pts',(-21.0632450375034,21.5006186346117,-12.4510003976597));
#35811=CARTESIAN_POINT('Ctrl Pts',(-21.0572954109348,21.5078592837357,-12.4504214382343));
#35812=CARTESIAN_POINT('Ctrl Pts',(-20.9883888397283,21.5924677264314,-12.4436651755835));
#35813=CARTESIAN_POINT('Ctrl Pts',(-20.9290311542365,21.6726844620707,-12.4373441884769));
#35814=CARTESIAN_POINT('Ctrl Pts',(-20.7114289983159,21.9972274410809,-12.4120510206018));
#35815=CARTESIAN_POINT('Ctrl Pts',(-20.5828654837701,22.2597602822964,-12.3920253210485));
#35816=CARTESIAN_POINT('Ctrl Pts',(-20.4774455073804,22.5776728234169,-12.3696540344095));
#35817=CARTESIAN_POINT('Ctrl Pts',(-20.4644505572474,22.619725393383,-12.3667341243952));
#35818=CARTESIAN_POINT('Ctrl Pts',(-20.4379367785655,22.7122000830338,-12.3604160639647));
#35819=CARTESIAN_POINT('Ctrl Pts',(-20.4247728127029,22.7627130311901,-12.3570306995681));
#35820=CARTESIAN_POINT('Ctrl Pts',(-20.4090704948337,22.8295827095398,-12.3526543522629));
#35821=CARTESIAN_POINT('Ctrl Pts',(-20.4054233885426,22.8456680668642,-12.3516095775238));
#35822=CARTESIAN_POINT('Ctrl Pts',(-20.4004186496425,22.8685545403423,-12.3501350102391));
#35823=CARTESIAN_POINT('Ctrl Pts',(-20.398959302462,22.8753328169068,-12.349699772953));
#35824=CARTESIAN_POINT('Ctrl Pts',(-20.3967612723538,22.8857046419039,-12.3490361158524));
#35825=CARTESIAN_POINT('Ctrl Pts',(-20.3960068424366,22.8892947776155,-12.3488068207167));
#35826=CARTESIAN_POINT('Ctrl Pts',(-20.394778583634,22.8951897391341,-12.3484310272796));
#35827=CARTESIAN_POINT('Ctrl Pts',(-20.3943011483796,22.8974937973047,-12.3482843246371));
#35828=CARTESIAN_POINT('Ctrl Pts',(-20.3933997912314,22.9018677680449,-12.3480061663405));
#35829=CARTESIAN_POINT('Ctrl Pts',(-20.3929753810188,22.9039375770589,-12.3478746827219));
#35830=CARTESIAN_POINT('Ctrl Pts',(-20.3921875875827,22.9077988659029,-12.3476296663321));
#35831=CARTESIAN_POINT('Ctrl Pts',(-20.3918236942632,22.909590231534,-12.3475161045552));
#35832=CARTESIAN_POINT('Ctrl Pts',(-20.391086467587,22.9132353282144,-12.3472852482819));
#35833=CARTESIAN_POINT('Ctrl Pts',(-20.3907132430304,22.9150890711815,-12.347167960409));
#35834=CARTESIAN_POINT('Ctrl Pts',(-20.3896492384126,22.9203979452554,-12.3468323925823));
#35835=CARTESIAN_POINT('Ctrl Pts',(-20.3889624901199,22.9238538959309,-12.3466143448951));
#35836=CARTESIAN_POINT('Ctrl Pts',(-20.3860187284844,22.9387960511729,-12.34567329019));
#35837=CARTESIAN_POINT('Ctrl Pts',(-20.3838186005794,22.9502935674653,-12.344953509534));
#35838=CARTESIAN_POINT('Ctrl Pts',(-20.3809245233384,22.965877046188,-12.3439834803662));
#35839=CARTESIAN_POINT('Ctrl Pts',(-20.3801757718782,22.9699525489977,-12.3437303040536));
#35840=CARTESIAN_POINT('Ctrl Pts',(-20.3191771648423,23.3056133137435,-12.32291990611));
#35841=CARTESIAN_POINT('Ctrl Pts',(-20.3112901341222,23.6446596198105,-12.3050503199702));
#35842=CARTESIAN_POINT('Ctrl Pts',(-20.371301421233,24.091926941817,-12.2793604265429));
#35843=CARTESIAN_POINT('Ctrl Pts',(-20.3924732825126,24.2041391710111,-12.2727518455337));
#35844=CARTESIAN_POINT('Ctrl Pts',(-20.4314928611286,24.363879587465,-12.2629595046616));
#35845=CARTESIAN_POINT('Ctrl Pts',(-20.4445794635597,24.4124852321162,-12.2599279774414));
#35846=CARTESIAN_POINT('Ctrl Pts',(-20.4610426728404,24.4683827596517,-12.2563747013305));
#35847=CARTESIAN_POINT('Ctrl Pts',(-20.4633151716134,24.4759946127755,-12.2558893870087));
#35848=CARTESIAN_POINT('Ctrl Pts',(-20.4668108286694,24.4875474979495,-12.2551505747585));
#35849=CARTESIAN_POINT('Ctrl Pts',(-20.4680134629966,24.4914947496503,-12.2548977503613));
#35850=CARTESIAN_POINT('Ctrl Pts',(-20.4701963319781,24.4986102531169,-12.254441278492));
#35851=CARTESIAN_POINT('Ctrl Pts',(-20.4711738840452,24.5017793272449,-12.2542377193995));
#35852=CARTESIAN_POINT('Ctrl Pts',(-20.4731432483963,24.508128891344,-12.2538293492048));
#35853=CARTESIAN_POINT('Ctrl Pts',(-20.4741351042261,24.5113093635359,-12.2536245368763));
#35854=CARTESIAN_POINT('Ctrl Pts',(-20.4769280706857,24.5202166342024,-12.2530502012729));
#35855=CARTESIAN_POINT('Ctrl Pts',(-20.4787402472114,24.5259399243963,-12.2526803139572));
#35856=CARTESIAN_POINT('Ctrl Pts',(-20.4861701234834,24.5491794233054,-12.2511748863607));
#35857=CARTESIAN_POINT('Ctrl Pts',(-20.4919216671991,24.5666521773952,-12.2500349375313));
#35858=CARTESIAN_POINT('Ctrl Pts',(-20.6253699068414,24.9606672616657,-12.2241419078027));
#35859=CARTESIAN_POINT('Ctrl Pts',(-20.8215061009952,25.3103538651415,-12.196656796137));
#35860=CARTESIAN_POINT('Ctrl Pts',(-21.1404242787078,25.6924266010298,-12.1636044055868));
#35861=CARTESIAN_POINT('Ctrl Pts',(-21.2082799011705,25.7664093044123,-12.1570648596029));
#35862=CARTESIAN_POINT('Ctrl Pts',(-21.2827313059631,25.840336807273,-12.1504861054253));
#35863=CARTESIAN_POINT('Ctrl Pts',(-21.2859850160769,25.8435538892838,-12.1501997305347));
#35864=CARTESIAN_POINT('Ctrl Pts',(-21.2911918080841,25.8486801831239,-12.1497432774549));
#35865=CARTESIAN_POINT('Ctrl Pts',(-21.2931404695809,25.8505938457188,-12.1495728538394));
#35866=CARTESIAN_POINT('Ctrl Pts',(-21.2968512376721,25.8542287117108,-12.1492490969219));
#35867=CARTESIAN_POINT('Ctrl Pts',(-21.298612888035,25.8559503751212,-12.1490957274979));
#35868=CARTESIAN_POINT('Ctrl Pts',(-21.3017047683997,25.8589651513782,-12.1488271306));
#35869=CARTESIAN_POINT('Ctrl Pts',(-21.3030341423073,25.8602591365716,-12.1487118339197));
#35870=CARTESIAN_POINT('Ctrl Pts',(-21.3056447210455,25.8627958339153,-12.1484857884603));
#35871=CARTESIAN_POINT('Ctrl Pts',(-21.3069258375463,25.8640386263096,-12.1483750331223));
#35872=CARTESIAN_POINT('Ctrl Pts',(-21.3100009149295,25.8670167591795,-12.1481096016754));
#35873=CARTESIAN_POINT('Ctrl Pts',(-21.3117958639214,25.8687510843731,-12.1479550057664));
#35874=CARTESIAN_POINT('Ctrl Pts',(-21.3182900577626,25.8750113674683,-12.1473968864787));
#35875=CARTESIAN_POINT('Ctrl Pts',(-21.3230010704576,25.8795251777659,-12.1469943098849));
#35876=CARTESIAN_POINT('Ctrl Pts',(-21.3982043455782,25.9511436892873,-12.1406036309618));
#35877=CARTESIAN_POINT('Ctrl Pts',(-21.4716954094851,26.015043465493,-12.1348566866873));
#35878=CARTESIAN_POINT('Ctrl Pts',(-21.686833803462,26.1856258142931,-12.1190115702637));
#35879=CARTESIAN_POINT('Ctrl Pts',(-21.8345459780461,26.2840924171514,-12.1092270156187));
#35880=CARTESIAN_POINT('Ctrl Pts',(-22.0178611211012,26.3855543776125,-12.0974891941272));
#35881=CARTESIAN_POINT('Ctrl Pts',(-22.046338854748,26.4007617920497,-12.0956770989418));
#35882=CARTESIAN_POINT('Ctrl Pts',(-22.0750360352296,26.4155367847935,-12.0938589134715));
#35883=CARTESIAN_POINT('Origin',(-23.5502525316942,23.5502525316942,-77.3107734492734));
#35884=CARTESIAN_POINT('',(-22.075035905646,26.4155367180762,-10.5984952470527));
#35885=CARTESIAN_POINT('',(-22.0750360250409,26.4155367795477,-10.8457129588805));
#35886=CARTESIAN_POINT('',(-22.0750360153461,26.4155367745563,-77.3107734492734));
#35887=CARTESIAN_POINT('',(-26.7730017274927,23.5479758059353,-11.439226550727));
#35888=CARTESIAN_POINT('Ctrl Pts',(-22.075035905646,26.4155367180762,-10.5984952470527));
#35889=CARTESIAN_POINT('Ctrl Pts',(-22.0082494477041,26.3811511260226,-10.6027955967541));
#35890=CARTESIAN_POINT('Ctrl Pts',(-21.9426497206584,26.3444224858523,-10.6070294630284));
#35891=CARTESIAN_POINT('Ctrl Pts',(-21.6913677781022,26.191938982473,-10.6235035177627));
#35892=CARTESIAN_POINT('Ctrl Pts',(-21.5164249175405,26.0597343351953,-10.6355824193442));
#35893=CARTESIAN_POINT('Ctrl Pts',(-21.2836165715118,25.8433518425092,-10.6540810912497));
#35894=CARTESIAN_POINT('Ctrl Pts',(-21.2141697239007,25.7725614858273,-10.6599655885503));
#35895=CARTESIAN_POINT('Ctrl Pts',(-21.1418621279038,25.6917148288458,-10.6665675258275));
#35896=CARTESIAN_POINT('Ctrl Pts',(-21.1356550781298,25.6847136443714,-10.6671382957971));
#35897=CARTESIAN_POINT('Ctrl Pts',(-21.1264900636983,25.6742849131555,-10.6679871400436));
#35898=CARTESIAN_POINT('Ctrl Pts',(-21.1235086531116,25.6708779597656,-10.6682642351291));
#35899=CARTESIAN_POINT('Ctrl Pts',(-21.1184197109837,25.6650378769279,-10.6687388633998));
#35900=CARTESIAN_POINT('Ctrl Pts',(-21.1163086216336,25.6626078443408,-10.6689362483453));
#35901=CARTESIAN_POINT('Ctrl Pts',(-21.1120818100213,25.6577276973459,-10.6693324397305));
#35902=CARTESIAN_POINT('Ctrl Pts',(-21.1099661320312,25.6552775503964,-10.6695312476259));
#35903=CARTESIAN_POINT('Ctrl Pts',(-21.1050864217937,25.6496091604009,-10.6699909464535));
#35904=CARTESIAN_POINT('Ctrl Pts',(-21.1023250499135,25.6463886444428,-10.6702519469213));
#35905=CARTESIAN_POINT('Ctrl Pts',(-21.093997466427,25.6366375030656,-10.671041675918));
#35906=CARTESIAN_POINT('Ctrl Pts',(-21.0884510043524,25.6300901292264,-10.6715712164442));
#35907=CARTESIAN_POINT('Ctrl Pts',(-21.0758206225907,25.6150591672939,-10.6727852929513));
#35908=CARTESIAN_POINT('Ctrl Pts',(-21.0687540928762,25.6065611681707,-10.6734705331395));
#35909=CARTESIAN_POINT('Ctrl Pts',(-21.0048399583152,25.5288906698619,-10.6797233476217));
#35910=CARTESIAN_POINT('Ctrl Pts',(-20.9508593489849,25.4574196888613,-10.6854056464397));
#35911=CARTESIAN_POINT('Ctrl Pts',(-20.7880815475201,25.2221303907948,-10.7039121548336));
#35912=CARTESIAN_POINT('Ctrl Pts',(-20.6912760989912,25.0505856021648,-10.7171419390181));
#35913=CARTESIAN_POINT('Ctrl Pts',(-20.5261971030751,24.6832631794334,-10.7444021448771));
#35914=CARTESIAN_POINT('Ctrl Pts',(-20.4599138771022,24.4875100927262,-10.7583729946229));
#35915=CARTESIAN_POINT('Ctrl Pts',(-20.4099679292265,24.2747401200836,-10.77215675483));
#35916=CARTESIAN_POINT('Ctrl Pts',(-20.4072184980087,24.2627177764797,-10.7729308746654));
#35917=CARTESIAN_POINT('Ctrl Pts',(-20.4037566469526,24.2471701291711,-10.7739256408794));
#35918=CARTESIAN_POINT('Ctrl Pts',(-20.4029810687037,24.2436592153334,-10.7741498581627));
#35919=CARTESIAN_POINT('Ctrl Pts',(-20.4018034797623,24.2382857869489,-10.7744923751738));
#35920=CARTESIAN_POINT('Ctrl Pts',(-20.4013972457082,24.2364242164129,-10.7746109182515));
#35921=CARTESIAN_POINT('Ctrl Pts',(-20.4006365236844,24.23292329984,-10.7748336291285));
#35922=CARTESIAN_POINT('Ctrl Pts',(-20.4002816659728,24.2312840439842,-10.7749378178886));
#35923=CARTESIAN_POINT('Ctrl Pts',(-20.3994672185931,24.2275074707945,-10.7751776385289));
#35924=CARTESIAN_POINT('Ctrl Pts',(-20.3990085247228,24.2253699662078,-10.7753132179515));
#35925=CARTESIAN_POINT('Ctrl Pts',(-20.3977357692289,24.2194093917535,-10.7756908574139));
#35926=CARTESIAN_POINT('Ctrl Pts',(-20.3969264838941,24.2155852887705,-10.7759326419409));
#35927=CARTESIAN_POINT('Ctrl Pts',(-20.3924181847837,24.1940892946679,-10.7772890190434));
#35928=CARTESIAN_POINT('Ctrl Pts',(-20.3888606733955,24.1763875760883,-10.7783955862215));
#35929=CARTESIAN_POINT('Ctrl Pts',(-20.3789811070337,24.1249959633797,-10.7815805502338));
#35930=CARTESIAN_POINT('Ctrl Pts',(-20.3730473285589,24.0912329082794,-10.7836387121224));
#35931=CARTESIAN_POINT('Ctrl Pts',(-20.3521057749331,23.9598092258375,-10.7915398835067));
#35932=CARTESIAN_POINT('Ctrl Pts',(-20.3410523111349,23.8615666652851,-10.7972116468456));
#35933=CARTESIAN_POINT('Ctrl Pts',(-20.3140457034024,23.4532874682306,-10.8203683713949));
#35934=CARTESIAN_POINT('Ctrl Pts',(-20.3383976973719,23.1423005812777,-10.8372038792582));
#35935=CARTESIAN_POINT('Ctrl Pts',(-20.4186737860706,22.7872228011523,-10.8588362377704));
#35936=CARTESIAN_POINT('Ctrl Pts',(-20.4318185359028,22.7351643759521,-10.8620650350633));
#35937=CARTESIAN_POINT('Ctrl Pts',(-20.4486157215334,22.6750133737784,-10.8658708168336));
#35938=CARTESIAN_POINT('Ctrl Pts',(-20.4510091165323,22.6665757033945,-10.866406400639));
#35939=CARTESIAN_POINT('Ctrl Pts',(-20.4546260174877,22.6540201399369,-10.8672059823003));
#35940=CARTESIAN_POINT('Ctrl Pts',(-20.4558233762952,22.6498947042575,-10.8674691255744));
#35941=CARTESIAN_POINT('Ctrl Pts',(-20.4579729436409,22.6425434237791,-10.8679387874319));
#35942=CARTESIAN_POINT('Ctrl Pts',(-20.4589219624818,22.6393166464641,-10.8681452013827));
#35943=CARTESIAN_POINT('Ctrl Pts',(-20.4609113324972,22.6325914620952,-10.8685759504609));
#35944=CARTESIAN_POINT('Ctrl Pts',(-20.4619525782567,22.6290933265964,-10.8688003146477));
#35945=CARTESIAN_POINT('Ctrl Pts',(-20.4646906064705,22.6199515600604,-10.8693874611124));
#35946=CARTESIAN_POINT('Ctrl Pts',(-20.466396924869,22.6143108199795,-10.8697505557558));
#35947=CARTESIAN_POINT('Ctrl Pts',(-20.4701575613993,22.6020008587639,-10.8705447275384));
#35948=CARTESIAN_POINT('Ctrl Pts',(-20.4722180853762,22.5953335784315,-10.8709760074188));
#35949=CARTESIAN_POINT('Ctrl Pts',(-20.4783066341009,22.575857199754,-10.8722392301557));
#35950=CARTESIAN_POINT('Ctrl Pts',(-20.4823930396295,22.5630666379553,-10.8730730919133));
#35951=CARTESIAN_POINT('Ctrl Pts',(-20.4966398415405,22.5194166406222,-10.8759336372528));
#35952=CARTESIAN_POINT('Ctrl Pts',(-20.5071866270585,22.4886862967091,-10.8779730079546));
#35953=CARTESIAN_POINT('Ctrl Pts',(-20.5556435566923,22.354156505536,-10.8870161497905));
#35954=CARTESIAN_POINT('Ctrl Pts',(-20.5984096548996,22.2521971694377,-10.8941782101637));
#35955=CARTESIAN_POINT('Ctrl Pts',(-20.7947489100216,21.8442464939157,-10.9240873062915));
#35956=CARTESIAN_POINT('Ctrl Pts',(-20.991331870595,21.56149464271,-10.9480900724662));
#35957=CARTESIAN_POINT('Ctrl Pts',(-21.230423468183,21.3131747745721,-10.9698780231028));
#35958=CARTESIAN_POINT('Ctrl Pts',(-21.2321543765422,21.3113812271125,-10.9700354201093));
#35959=CARTESIAN_POINT('Ctrl Pts',(-21.2426843049032,21.3004955379876,-10.9709908828255));
#35960=CARTESIAN_POINT('Ctrl Pts',(-21.2515348936091,21.2914530972571,-10.9717852526862));
#35961=CARTESIAN_POINT('Ctrl Pts',(-21.2629939245468,21.2798827793163,-10.9728023082248));
#35962=CARTESIAN_POINT('Ctrl Pts',(-21.2655535425654,21.2773070246778,-10.97302876204));
#35963=CARTESIAN_POINT('Ctrl Pts',(-21.2694679372964,21.2733812454079,-10.9733739590075));
#35964=CARTESIAN_POINT('Ctrl Pts',(-21.2708195603943,21.2720281025055,-10.9734929515035));
#35965=CARTESIAN_POINT('Ctrl Pts',(-21.2733585774839,21.2694907519356,-10.9737160971687));
#35966=CARTESIAN_POINT('Ctrl Pts',(-21.2745456867866,21.2683062722913,-10.973820272082));
#35967=CARTESIAN_POINT('Ctrl Pts',(-21.2772758249208,21.2655864311053,-10.9740594972554));
#35968=CARTESIAN_POINT('Ctrl Pts',(-21.2788194822835,21.2640517087508,-10.9741944961222));
#35969=CARTESIAN_POINT('Ctrl Pts',(-21.2831090223769,21.2597956304971,-10.9745689098273));
#35970=CARTESIAN_POINT('Ctrl Pts',(-21.2858582602591,21.2570776382453,-10.9748080567713));
#35971=CARTESIAN_POINT('Ctrl Pts',(-21.3010320960005,21.2421301509825,-10.9761235078629));
#35972=CARTESIAN_POINT('Ctrl Pts',(-21.3135511909019,21.2299963740798,-10.977192345543));
#35973=CARTESIAN_POINT('Ctrl Pts',(-21.5305602912756,21.0230551775137,-10.9954519356519));
#35974=CARTESIAN_POINT('Ctrl Pts',(-21.7597239494885,20.855823252836,-11.0107537959102));
#35975=CARTESIAN_POINT('Ctrl Pts',(-22.1614378749016,20.6368469007539,-11.0364672597661));
#35976=CARTESIAN_POINT('Ctrl Pts',(-22.3216283847113,20.5657575972518,-11.0464636290546));
#35977=CARTESIAN_POINT('Ctrl Pts',(-22.4930629474543,20.505829437058,-11.0573218973698));
#35978=CARTESIAN_POINT('Ctrl Pts',(-22.4993479860483,20.503654194018,-11.0577201606163));
#35979=CARTESIAN_POINT('Ctrl Pts',(-22.5126030217927,20.4991125418319,-11.0585605066676));
#35980=CARTESIAN_POINT('Ctrl Pts',(-22.5195744753416,20.4967505281018,-11.0590027261689));
#35981=CARTESIAN_POINT('Ctrl Pts',(-22.5540512732195,20.4852008890178,-11.0611909716551));
#35982=CARTESIAN_POINT('Ctrl Pts',(-22.5816709864127,20.47636115022,-11.0629480392461));
#35983=CARTESIAN_POINT('Ctrl Pts',(-22.6155540793369,20.4660188031581,-11.0651096750472));
#35984=CARTESIAN_POINT('Ctrl Pts',(-22.6217081720238,20.4641604623841,-11.0655025310838));
#35985=CARTESIAN_POINT('Ctrl Pts',(-22.6318678553787,20.4611257008009,-11.066151507628));
#35986=CARTESIAN_POINT('Ctrl Pts',(-22.6358702649024,20.4599386219186,-11.0664072787073));
#35987=CARTESIAN_POINT('Ctrl Pts',(-22.6430893657167,20.4578127535847,-11.0668688065347));
#35988=CARTESIAN_POINT('Ctrl Pts',(-22.6463052412599,20.4568711961777,-11.0670744723894));
#35989=CARTESIAN_POINT('Ctrl Pts',(-22.6525430464783,20.4550554234331,-11.0674735389025));
#35990=CARTESIAN_POINT('Ctrl Pts',(-22.655564800337,20.4541806135888,-11.0676669198558));
#35991=CARTESIAN_POINT('Ctrl Pts',(-22.6640051054853,20.4517504997816,-11.0682072458707));
#35992=CARTESIAN_POINT('Ctrl Pts',(-22.6694264446796,20.4502049923786,-11.0685545103682));
#35993=CARTESIAN_POINT('Ctrl Pts',(-22.6915668349342,20.4439560090704,-11.0699735717799));
#35994=CARTESIAN_POINT('Ctrl Pts',(-22.7083194801779,20.4393735674711,-11.0710493044085));
#35995=CARTESIAN_POINT('Ctrl Pts',(-22.7508666453998,20.4281042619805,-11.0737867515267));
#35996=CARTESIAN_POINT('Ctrl Pts',(-22.7767081808666,20.421601595307,-11.0754543662919));
#35997=CARTESIAN_POINT('Ctrl Pts',(-22.8807084565449,20.3967985822548,-11.0821871359502));
#35998=CARTESIAN_POINT('Ctrl Pts',(-22.9594525628269,20.38110206654,-11.0873340918957));
#35999=CARTESIAN_POINT('Ctrl Pts',(-23.1356781981863,20.3527700081307,-11.0989630364996));
#36000=CARTESIAN_POINT('Ctrl Pts',(-23.2333162799396,20.3416211684696,-11.1054806736465));
#36001=CARTESIAN_POINT('Ctrl Pts',(-23.6133184023116,20.3157447197496,-11.1310357498993));
#36002=CARTESIAN_POINT('Ctrl Pts',(-23.896637817994,20.333725045191,-11.1506051927682));
#36003=CARTESIAN_POINT('Ctrl Pts',(-24.1753540336778,20.3887073991743,-11.168570128039));
#36004=CARTESIAN_POINT('Ctrl Pts',(-24.1767239667431,20.3889785711165,-11.1686583936659));
#36005=CARTESIAN_POINT('Ctrl Pts',(-24.1919492603721,20.3920026333742,-11.1696389786119));
#36006=CARTESIAN_POINT('Ctrl Pts',(-24.2057868564855,20.3948457626159,-11.1705265982599));
#36007=CARTESIAN_POINT('Ctrl Pts',(-24.2232656457137,20.3985569704711,-11.1716428484581));
#36008=CARTESIAN_POINT('Ctrl Pts',(-24.2269243468718,20.399340470535,-11.1718762304354));
#36009=CARTESIAN_POINT('Ctrl Pts',(-24.2327042705662,20.4005887556591,-11.172244478921));
#36010=CARTESIAN_POINT('Ctrl Pts',(-24.2348263875254,20.4010493127931,-11.1723795881609));
#36011=CARTESIAN_POINT('Ctrl Pts',(-24.2387700793088,20.4019093758691,-11.1726304944831));
#36012=CARTESIAN_POINT('Ctrl Pts',(-24.2405917615,20.4023083155387,-11.1727463232345));
#36013=CARTESIAN_POINT('Ctrl Pts',(-24.2446529863457,20.4032013991681,-11.173004392791));
#36014=CARTESIAN_POINT('Ctrl Pts',(-24.2468923430636,20.4036963514476,-11.1731465859687));
#36015=CARTESIAN_POINT('Ctrl Pts',(-24.253433684206,20.4051494722824,-11.1735616383687));
#36016=CARTESIAN_POINT('Ctrl Pts',(-24.2577342556955,20.4061140808109,-11.1738341264483));
#36017=CARTESIAN_POINT('Ctrl Pts',(-24.2888364748846,20.4131572833891,-11.1758020859789));
#36018=CARTESIAN_POINT('Ctrl Pts',(-24.3155624307594,20.4195699035218,-11.1774785997989));
#36019=CARTESIAN_POINT('Ctrl Pts',(-24.3997830938571,20.4409208042443,-11.1827250822084));
#36020=CARTESIAN_POINT('Ctrl Pts',(-24.4569513897218,20.4571078386367,-11.186232066871));
#36021=CARTESIAN_POINT('Ctrl Pts',(-24.6541301853821,20.518875772836,-11.1982414241774));
#36022=CARTESIAN_POINT('Ctrl Pts',(-24.7914468020693,20.5724624331988,-11.2064564775664));
#36023=CARTESIAN_POINT('Ctrl Pts',(-24.9883225854023,20.6652861117598,-11.2186184015814));
#36024=CARTESIAN_POINT('Ctrl Pts',(-25.0510170334093,20.6973973936696,-11.2225514401361));
#36025=CARTESIAN_POINT('Ctrl Pts',(-25.1983638424373,20.7790686716482,-11.2320302319616));
#36026=CARTESIAN_POINT('Ctrl Pts',(-25.2819010856265,20.8304873975059,-11.2375993406465));
#36027=CARTESIAN_POINT('Ctrl Pts',(-25.38622187057,20.9014555161335,-11.2449142389547));
#36028=CARTESIAN_POINT('Ctrl Pts',(-25.4092742200644,20.9175832887211,-11.2465542440943));
#36029=CARTESIAN_POINT('Ctrl Pts',(-25.4455196241831,20.9436545606976,-11.2491729601276));
#36030=CARTESIAN_POINT('Ctrl Pts',(-25.4588527197663,20.9534014302927,-11.2501450625548));
#36031=CARTESIAN_POINT('Ctrl Pts',(-25.4843148395328,20.9723169792927,-11.2520189746015));
#36032=CARTESIAN_POINT('Ctrl Pts',(-25.4964550711007,20.9814698652471,-11.2529202116714));
#36033=CARTESIAN_POINT('Ctrl Pts',(-25.5139768055794,20.9948755392144,-11.2542325524569));
#36034=CARTESIAN_POINT('Ctrl Pts',(-25.5194103259272,20.9990602265348,-11.2546411475155));
#36035=CARTESIAN_POINT('Ctrl Pts',(-25.5348013812039,21.0109922849481,-11.2558032425856));
#36036=CARTESIAN_POINT('Ctrl Pts',(-25.5447267602058,21.0187807696688,-11.2565582743586));
#36037=CARTESIAN_POINT('Ctrl Pts',(-25.563879979986,21.0339929423079,-11.2580264099037));
#36038=CARTESIAN_POINT('Ctrl Pts',(-25.5731131451546,21.0414096201995,-11.2587392362961));
#36039=CARTESIAN_POINT('Ctrl Pts',(-25.5860466530475,21.0519164663021,-11.2597450291674));
#36040=CARTESIAN_POINT('Ctrl Pts',(-25.5897813378104,21.0549643622012,-11.2600363244526));
#36041=CARTESIAN_POINT('Ctrl Pts',(-25.6087842899706,21.0705439347006,-11.2615229300539));
#36042=CARTESIAN_POINT('Ctrl Pts',(-25.6239436950967,21.0832072022289,-11.262723465729));
#36043=CARTESIAN_POINT('Ctrl Pts',(-25.6436887753596,21.1000116455906,-11.2643068716919));
#36044=CARTESIAN_POINT('Ctrl Pts',(-25.6483805324044,21.1040279716789,-11.264684594379));
#36045=CARTESIAN_POINT('Ctrl Pts',(-25.6556116213914,21.1102541715505,-11.2652690564658));
#36046=CARTESIAN_POINT('Ctrl Pts',(-25.6581591023426,21.1124545943428,-11.2654754039147));
#36047=CARTESIAN_POINT('Ctrl Pts',(-25.6632304535699,21.1168489384932,-11.2658870751226));
#36048=CARTESIAN_POINT('Ctrl Pts',(-25.6657543659634,21.1190428050749,-11.2660923964613));
#36049=CARTESIAN_POINT('Ctrl Pts',(-25.6706893373576,21.1233459455328,-11.2664947246509));
#36050=CARTESIAN_POINT('Ctrl Pts',(-25.6731006756701,21.1254548943098,-11.2666917177957));
#36051=CARTESIAN_POINT('Ctrl Pts',(-25.6785040067931,21.1301948680034,-11.2671340559293));
#36052=CARTESIAN_POINT('Ctrl Pts',(-25.6814942691802,21.1328278497199,-11.2673794827075));
#36053=CARTESIAN_POINT('Ctrl Pts',(-25.6951326345143,21.1448816577241,-11.2685017565974));
#36054=CARTESIAN_POINT('Ctrl Pts',(-25.7057230773603,21.1543672228431,-11.2693813219542));
#36055=CARTESIAN_POINT('Ctrl Pts',(-25.7804233902968,21.2221703776673,-11.2756437333455));
#36056=CARTESIAN_POINT('Ctrl Pts',(-25.8422152319003,21.282978128385,-11.281132823447));
#36057=CARTESIAN_POINT('Ctrl Pts',(-25.9458151347108,21.3934956288553,-11.2909080674684));
#36058=CARTESIAN_POINT('Ctrl Pts',(-25.9887131343269,21.4421183906944,-11.2951464215273));
#36059=CARTESIAN_POINT('Ctrl Pts',(-26.2480944317104,21.7546307550851,-11.321984194109));
#36060=CARTESIAN_POINT('Ctrl Pts',(-26.4229508008435,22.0501891559384,-11.3459160403214));
#36061=CARTESIAN_POINT('Ctrl Pts',(-26.549192806043,22.370217626214,-11.3676612623035));
#36062=CARTESIAN_POINT('Ctrl Pts',(-26.5502001289748,22.3727808501055,-11.3678351596448));
#36063=CARTESIAN_POINT('Ctrl Pts',(-26.5557492502397,22.3869544334551,-11.3687952480426));
#36064=CARTESIAN_POINT('Ctrl Pts',(-26.5602270181877,22.3985899972243,-11.3695778836949));
#36065=CARTESIAN_POINT('Ctrl Pts',(-26.5659144525721,22.4136286808745,-11.3705820298454));
#36066=CARTESIAN_POINT('Ctrl Pts',(-26.5671859982344,22.4170080487784,-11.370807193563));
#36067=CARTESIAN_POINT('Ctrl Pts',(-26.5691209391378,22.4221768502446,-11.3711508447404));
#36068=CARTESIAN_POINT('Ctrl Pts',(-26.5697884232705,22.4239647336315,-11.371269578078));
#36069=CARTESIAN_POINT('Ctrl Pts',(-26.571039506128,22.427324915916,-11.3714924722904));
#36070=CARTESIAN_POINT('Ctrl Pts',(-26.571623463354,22.4288970713062,-11.3715966544587));
#36071=CARTESIAN_POINT('Ctrl Pts',(-26.5729644043445,22.4325158636334,-11.3718362195848));
#36072=CARTESIAN_POINT('Ctrl Pts',(-26.5737205354696,22.4345628103097,-11.3719715505402));
#36073=CARTESIAN_POINT('Ctrl Pts',(-26.5758189525608,22.4402613016097,-11.3723478084771));
#36074=CARTESIAN_POINT('Ctrl Pts',(-26.5771567120487,22.4439145267105,-11.372588463221));
#36075=CARTESIAN_POINT('Ctrl Pts',(-26.5845733955768,22.4642825531138,-11.3739271330178));
#36076=CARTESIAN_POINT('Ctrl Pts',(-26.5905206402388,22.4810454602382,-11.3750173671274));
#36077=CARTESIAN_POINT('Ctrl Pts',(-26.6844521437447,22.7529228893475,-11.3925276521857));
#36078=CARTESIAN_POINT('Ctrl Pts',(-26.7402056058759,23.0180934710657,-11.4072228653874));
#36079=CARTESIAN_POINT('Ctrl Pts',(-26.7693552008018,23.3739537078708,-11.427249448118));
#36080=CARTESIAN_POINT('Ctrl Pts',(-26.772943488292,23.4610070063838,-11.4321654148819));
#36081=CARTESIAN_POINT('Ctrl Pts',(-26.7730018090362,23.5480943167315,-11.4371602447912));
#36082=CARTESIAN_POINT('Ctrl Pts',(-22.075036015346,26.4155367745563,-11.8463751360594));
#36083=CARTESIAN_POINT('Ctrl Pts',(-22.1638791174928,26.4612784185055,-11.8402235822661));
#36084=CARTESIAN_POINT('Ctrl Pts',(-22.254821394332,26.5028685328931,-11.8340720284728));
#36085=CARTESIAN_POINT('Ctrl Pts',(-22.3474353189619,26.5401268292617,-11.8279204746795));
#36086=CARTESIAN_POINT('Ctrl Pts',(-22.440153973422,26.5774272581181,-11.8217619645761));
#36087=CARTESIAN_POINT('Ctrl Pts',(-22.5345476448762,26.6103859303396,-11.8156034544726));
#36088=CARTESIAN_POINT('Ctrl Pts',(-22.6301710703149,26.638871586697,-11.8094449443692));
#36089=CARTESIAN_POINT('Ctrl Pts',(-22.7258576981229,26.6673760706687,-11.8032823637942));
#36090=CARTESIAN_POINT('Ctrl Pts',(-22.8227752769979,26.6914015490826,-11.7971197832192));
#36091=CARTESIAN_POINT('Ctrl Pts',(-22.9204677005841,26.7108677612031,-11.7909572026442));
#36092=CARTESIAN_POINT('Ctrl Pts',(-23.0183113022632,26.730364097101,-11.7847850855346));
#36093=CARTESIAN_POINT('Ctrl Pts',(-23.1169317133489,26.7452870211307,-11.7786129684251));
#36094=CARTESIAN_POINT('Ctrl Pts',(-23.2158672180003,26.7556080540171,-11.7724408513155));
#36095=CARTESIAN_POINT('Ctrl Pts',(-23.2489383989166,26.7590580666999,-11.7703776971193));
#36096=CARTESIAN_POINT('Ctrl Pts',(-23.2820447872775,26.7619943119972,-11.7683145429232));
#36097=CARTESIAN_POINT('Ctrl Pts',(-23.3151691812701,26.7644170235728,-11.7662513887271));
#36098=CARTESIAN_POINT('Ctrl Pts',(-23.4142634635937,26.7716647596347,-11.7600792974147));
#36099=CARTESIAN_POINT('Ctrl Pts',(-23.5138677628276,26.7743382778831,-11.7539072061024));
#36100=CARTESIAN_POINT('Ctrl Pts',(-23.6135239629293,26.7723813758731,-11.7477351147901));
#36101=CARTESIAN_POINT('Ctrl Pts',(-23.7130451387318,26.7704271252718,-11.7415713860513));
#36102=CARTESIAN_POINT('Ctrl Pts',(-23.8126176451428,26.7638549326342,-11.7354076573125));
#36103=CARTESIAN_POINT('Ctrl Pts',(-23.9117789491918,26.752660408894,-11.7292439285737));
#36104=CARTESIAN_POINT('Ctrl Pts',(-24.010835201146,26.741477744701,-11.7230867297271));
#36105=CARTESIAN_POINT('Ctrl Pts',(-24.109480687534,26.7256825334003,-11.7169295308804));
#36106=CARTESIAN_POINT('Ctrl Pts',(-24.207254552655,26.7053224052395,-11.7107723320338));
#36107=CARTESIAN_POINT('Ctrl Pts',(-24.3049569510098,26.6849771590978,-11.7046196337261));
#36108=CARTESIAN_POINT('Ctrl Pts',(-24.4017885707688,26.6600737182635,-11.6984669354183));
#36109=CARTESIAN_POINT('Ctrl Pts',(-24.4972962640925,26.6307112201731,-11.6923142371106));
#36110=CARTESIAN_POINT('Ctrl Pts',(-24.5927677407629,26.6013598563838,-11.6861638719149));
#36111=CARTESIAN_POINT('Ctrl Pts',(-24.6869158737756,26.5675529226133,-11.6800135067191));
#36112=CARTESIAN_POINT('Ctrl Pts',(-24.7793011219447,26.5294398580138,-11.6738631415234));
#36113=CARTESIAN_POINT('Ctrl Pts',(-24.8716760532692,26.491331049576,-11.6677134631512));
#36114=CARTESIAN_POINT('Ctrl Pts',(-24.9622880895723,26.4489172320187,-11.6615637847789));
#36115=CARTESIAN_POINT('Ctrl Pts',(-25.0507171223673,26.4023962122679,-11.6554141064067));
#36116=CARTESIAN_POINT('Ctrl Pts',(-25.1391599372994,26.3558679419675,-11.6492634695743));
#36117=CARTESIAN_POINT('Ctrl Pts',(-25.2254186884504,26.3052314002832,-11.6431128327418));
#36118=CARTESIAN_POINT('Ctrl Pts',(-25.3090982499685,26.250730137935,-11.6369621959094));
#36119=CARTESIAN_POINT('Ctrl Pts',(-25.3928673310391,26.196170570685,-11.6308049791875));
#36120=CARTESIAN_POINT('Ctrl Pts',(-25.4740513479296,26.1377382642457,-11.6246477624657));
#36121=CARTESIAN_POINT('Ctrl Pts',(-25.5522846517356,26.0757198058481,-11.6184905457439));
#36122=CARTESIAN_POINT('Ctrl Pts',(-25.6305616015813,26.0136667476067,-11.6123298939361));
#36123=CARTESIAN_POINT('Ctrl Pts',(-25.7058842324766,25.9480238384593,-11.6061692421283));
#36124=CARTESIAN_POINT('Ctrl Pts',(-25.777922048037,25.8791162220928,-11.6000085903205));
#36125=CARTESIAN_POINT('Ctrl Pts',(-25.8500804084799,25.8100932987802,-11.5938376295515));
#36126=CARTESIAN_POINT('Ctrl Pts',(-25.9189426743867,25.7377950707075,-11.5876666687825));
#36127=CARTESIAN_POINT('Ctrl Pts',(-25.9842170045119,25.662581698174,-11.5814957080134));
#36128=CARTESIAN_POINT('Ctrl Pts',(-26.0340421262817,25.6051699187194,-11.576785297793));
#36129=CARTESIAN_POINT('Ctrl Pts',(-26.0817775161061,25.5460603392475,-11.5720748875726));
#36130=CARTESIAN_POINT('Ctrl Pts',(-26.1273105299634,25.4854242646566,-11.5673644773521));
#36131=CARTESIAN_POINT('Ctrl Pts',(-26.1872004936594,25.4056691156278,-11.5611688343846));
#36132=CARTESIAN_POINT('Ctrl Pts',(-26.2434912396094,25.3229891618407,-11.5549731914171));
#36133=CARTESIAN_POINT('Ctrl Pts',(-26.2958852886696,25.2377412950119,-11.5487775484496));
#36134=CARTESIAN_POINT('Ctrl Pts',(-26.348208064848,25.1526093929014,-11.5425903335638));
#36135=CARTESIAN_POINT('Ctrl Pts',(-26.3966444552897,25.0649168819929,-11.5364031186781));
#36136=CARTESIAN_POINT('Ctrl Pts',(-26.4409379947223,24.9750525584833,-11.5302159037923));
#36137=CARTESIAN_POINT('Ctrl Pts',(-26.4851828220737,24.8852870637933,-11.5240354933326));
#36138=CARTESIAN_POINT('Ctrl Pts',(-26.5252936662427,24.7933548872637,-11.5178550828729));
#36139=CARTESIAN_POINT('Ctrl Pts',(-26.5610585690881,24.6996717623026,-11.5116746724132));
#36140=CARTESIAN_POINT('Ctrl Pts',(-26.5967923198493,24.6060702375799,-11.5054996452385));
#36141=CARTESIAN_POINT('Ctrl Pts',(-26.6281875054638,24.5107211977596,-11.4993246180639));
#36142=CARTESIAN_POINT('Ctrl Pts',(-26.6550795643388,24.4140619203092,-11.4931495908892));
#36143=CARTESIAN_POINT('Ctrl Pts',(-26.6819573249434,24.3174540357435,-11.486977846922));
#36144=CARTESIAN_POINT('Ctrl Pts',(-26.7043366050413,24.2195377121399,-11.4808061029548));
#36145=CARTESIAN_POINT('Ctrl Pts',(-26.7221024170935,24.12076621864,-11.4746343589876));
#36146=CARTESIAN_POINT('Ctrl Pts',(-26.7398677128267,24.0219975956868,-11.4684627943867));
#36147=CARTESIAN_POINT('Ctrl Pts',(-26.7530197187827,23.922374272976,-11.4622912297859));
#36148=CARTESIAN_POINT('Ctrl Pts',(-26.7614945193228,23.8223599725909,-11.456119665185));
#36149=CARTESIAN_POINT('Ctrl Pts',(-26.7692270682408,23.7311052620432,-11.4504886270323));
#36150=CARTESIAN_POINT('Ctrl Pts',(-26.773066403134,23.6395254228175,-11.4448575888797));
#36151=CARTESIAN_POINT('Ctrl Pts',(-26.7730017274927,23.5479758059353,-11.439226550727));
#36152=CARTESIAN_POINT('Ctrl Pts',(-22.0750360352296,26.4155367847935,-12.0938589134715));
#36153=CARTESIAN_POINT('Ctrl Pts',(-22.141904313061,26.4499644987072,-12.0896222975693));
#36154=CARTESIAN_POINT('Ctrl Pts',(-22.2099640499397,26.4820443585534,-12.085352014354));
#36155=CARTESIAN_POINT('Ctrl Pts',(-22.3840259436386,26.5567576726363,-12.0744419892762));
#36156=CARTESIAN_POINT('Ctrl Pts',(-22.4912699591345,26.5961857486819,-12.0677275327897));
#36157=CARTESIAN_POINT('Ctrl Pts',(-22.6188477338851,26.6355363916311,-12.0596467714977));
#36158=CARTESIAN_POINT('Ctrl Pts',(-22.6373741276867,26.6410686679099,-12.0584711847134));
#36159=CARTESIAN_POINT('Ctrl Pts',(-22.6615979135229,26.6480654870124,-12.0569309472581));
#36160=CARTESIAN_POINT('Ctrl Pts',(-22.6672513804879,26.6496816892615,-12.0565712583184));
#36161=CARTESIAN_POINT('Ctrl Pts',(-22.6764445637053,26.6522826245131,-12.0559859934471));
#36162=CARTESIAN_POINT('Ctrl Pts',(-22.6799816141837,26.6532767970896,-12.0557607257635));
#36163=CARTESIAN_POINT('Ctrl Pts',(-22.6867726961014,26.6551730682862,-12.0553280420279));
#36164=CARTESIAN_POINT('Ctrl Pts',(-22.6900264621821,26.6560761059205,-12.0551206569004));
#36165=CARTESIAN_POINT('Ctrl Pts',(-22.697449662049,26.6581237520593,-12.0546473482485));
#36166=CARTESIAN_POINT('Ctrl Pts',(-22.7016199855978,26.6592650852654,-12.0543813185049));
#36167=CARTESIAN_POINT('Ctrl Pts',(-22.7146216392645,26.6627952660597,-12.05355152536));
#36168=CARTESIAN_POINT('Ctrl Pts',(-22.7234607952735,26.6651548870583,-12.0529868132175));
#36169=CARTESIAN_POINT('Ctrl Pts',(-22.7921855753088,26.6831878961381,-12.0485915007129));
#36170=CARTESIAN_POINT('Ctrl Pts',(-22.8524979207607,26.6971696184901,-12.0447064209677));
#36171=CARTESIAN_POINT('Ctrl Pts',(-22.9181075849285,26.7104005783717,-12.0404460099879));
#36172=CARTESIAN_POINT('Ctrl Pts',(-22.9230452281013,26.7113842765766,-12.0401251757339));
#36173=CARTESIAN_POINT('Ctrl Pts',(-22.9500891241205,26.7167062190314,-12.0383668140076));
#36174=CARTESIAN_POINT('Ctrl Pts',(-22.9722376679158,26.7208240649012,-12.0369226233702));
#36175=CARTESIAN_POINT('Ctrl Pts',(-23.2463070505,26.7688117159694,-12.0190010101658));
#36176=CARTESIAN_POINT('Ctrl Pts',(-23.5025106856627,26.782772831883,-12.0016087899334));
#36177=CARTESIAN_POINT('Ctrl Pts',(-23.8552716957069,26.76002778508,-11.9777539070983));
#36178=CARTESIAN_POINT('Ctrl Pts',(-23.9525965168783,26.7492860741959,-11.9711959680989));
#36179=CARTESIAN_POINT('Ctrl Pts',(-24.11077941454,26.7244928168055,-11.9607133646114));
#36180=CARTESIAN_POINT('Ctrl Pts',(-24.171984805859,26.7130743727495,-11.956701635958));
#36181=CARTESIAN_POINT('Ctrl Pts',(-24.2395641474985,26.6984289242487,-11.9523495509254));
#36182=CARTESIAN_POINT('Ctrl Pts',(-24.2462980068534,26.6969469561461,-11.951916755115));
#36183=CARTESIAN_POINT('Ctrl Pts',(-24.2565929360581,26.6946466140983,-11.9512564584681));
#36184=CARTESIAN_POINT('Ctrl Pts',(-24.2601574051069,26.6938437874575,-11.9510280928944));
#36185=CARTESIAN_POINT('Ctrl Pts',(-24.266009074252,26.6925153535603,-11.950653616417));
#36186=CARTESIAN_POINT('Ctrl Pts',(-24.2682970671439,26.6919933095259,-11.9505073031892));
#36187=CARTESIAN_POINT('Ctrl Pts',(-24.2727153673917,26.6909801214287,-11.9502249688609));
#36188=CARTESIAN_POINT('Ctrl Pts',(-24.274845748211,26.6904893082016,-11.9500889287986));
#36189=CARTESIAN_POINT('Ctrl Pts',(-24.2786848318684,26.6896007163373,-11.9498439467526));
#36190=CARTESIAN_POINT('Ctrl Pts',(-24.2803937023712,26.6892037118308,-11.9497349604602));
#36191=CARTESIAN_POINT('Ctrl Pts',(-24.2842271615044,26.6883098233958,-11.9494906120856));
#36192=CARTESIAN_POINT('Ctrl Pts',(-24.2863515654272,26.6878121782685,-11.9493552949786));
#36193=CARTESIAN_POINT('Ctrl Pts',(-24.2921608759784,26.6864451127616,-11.9489855164906));
#36194=CARTESIAN_POINT('Ctrl Pts',(-24.2958447733596,26.6855713522255,-11.948751306354));
#36195=CARTESIAN_POINT('Ctrl Pts',(-24.3137055949855,26.6813017964703,-11.9476170945413));
#36196=CARTESIAN_POINT('Ctrl Pts',(-24.3278612013306,26.677816256732,-11.9467222128187));
#36197=CARTESIAN_POINT('Ctrl Pts',(-24.3505279965161,26.6720715957018,-11.9452950480826));
#36198=CARTESIAN_POINT('Ctrl Pts',(-24.3590542171703,26.6698734903214,-11.9447595284686));
#36199=CARTESIAN_POINT('Ctrl Pts',(-24.3726481313066,26.6663094285981,-11.9439076586451));
#36200=CARTESIAN_POINT('Ctrl Pts',(-24.3777216102767,26.6649660067612,-11.943590159657));
#36201=CARTESIAN_POINT('Ctrl Pts',(-24.3871837336574,26.6624357515392,-11.9429987890098));
#36202=CARTESIAN_POINT('Ctrl Pts',(-24.3915731837441,26.6612520160465,-11.9427247638796));
#36203=CARTESIAN_POINT('Ctrl Pts',(-24.6979098770364,26.5779441716384,-11.9236214492977));
#36204=CARTESIAN_POINT('Ctrl Pts',(-24.9863370758769,26.4522797329199,-11.9069080461384));
#36205=CARTESIAN_POINT('Ctrl Pts',(-25.3512756988829,26.2253335264758,-11.8824879028166));
#36206=CARTESIAN_POINT('Ctrl Pts',(-25.4469681261721,26.158356969656,-11.8757428998191));
#36207=CARTESIAN_POINT('Ctrl Pts',(-25.580993095657,26.0532674322934,-11.865616769211));
#36208=CARTESIAN_POINT('Ctrl Pts',(-25.622341173741,26.0191468124521,-11.8623912096068));
#36209=CARTESIAN_POINT('Ctrl Pts',(-25.6689114167839,25.9787226694689,-11.8586312177299));
#36210=CARTESIAN_POINT('Ctrl Pts',(-25.6749855153543,25.973410064277,-11.8581382544008));
#36211=CARTESIAN_POINT('Ctrl Pts',(-25.6841550548324,25.965329099659,-11.8573901643942));
#36212=CARTESIAN_POINT('Ctrl Pts',(-25.6872652347003,25.9625774505892,-11.8571357374902));
#36213=CARTESIAN_POINT('Ctrl Pts',(-25.6926357791813,25.9578074669582,-11.8566952111291));
#36214=CARTESIAN_POINT('Ctrl Pts',(-25.6948986368102,25.955791936721,-11.8565092297092));
#36215=CARTESIAN_POINT('Ctrl Pts',(-25.699581876376,25.9516087084781,-11.8561235560615));
#36216=CARTESIAN_POINT('Ctrl Pts',(-25.702001828769,25.9494405364357,-11.855923843951));
#36217=CARTESIAN_POINT('Ctrl Pts',(-25.7078678522686,25.9441688206148,-11.8554387027153));
#36218=CARTESIAN_POINT('Ctrl Pts',(-25.711310504101,25.9410614971876,-11.8551531138208));
#36219=CARTESIAN_POINT('Ctrl Pts',(-25.7241675971189,25.9294062781512,-11.8540832699426));
#36220=CARTESIAN_POINT('Ctrl Pts',(-25.7335380307643,25.9208102051252,-11.8532969690902));
#36221=CARTESIAN_POINT('Ctrl Pts',(-25.8839848030249,25.7811474768813,-11.840564796284));
#36222=CARTESIAN_POINT('Ctrl Pts',(-26.0130596873307,25.6377762435552,-11.8280660194604));
#36223=CARTESIAN_POINT('Ctrl Pts',(-26.2475252882178,25.3251217559499,-11.8019545718791));
#36224=CARTESIAN_POINT('Ctrl Pts',(-26.3515961455029,25.155839979797,-11.7883764777622));
#36225=CARTESIAN_POINT('Ctrl Pts',(-26.4766613551673,24.902770219912,-11.7695444466733));
#36226=CARTESIAN_POINT('Ctrl Pts',(-26.5109199089142,24.8260361159522,-11.7640157667073));
#36227=CARTESIAN_POINT('Ctrl Pts',(-26.5543253674755,24.7176163428053,-11.7565330141741));
#36228=CARTESIAN_POINT('Ctrl Pts',(-26.5660430672305,24.6870020744771,-11.7544556537255));
#36229=CARTESIAN_POINT('Ctrl Pts',(-26.5788720835645,24.6518887543233,-11.7521176072309));
#36230=CARTESIAN_POINT('Ctrl Pts',(-26.5804427086096,24.6475611707439,-11.7518302191037));
#36231=CARTESIAN_POINT('Ctrl Pts',(-26.582795748347,24.6410342013344,-11.7513979446661));
#36232=CARTESIAN_POINT('Ctrl Pts',(-26.5835850469411,24.6388373302832,-11.7512526478649));
#36233=CARTESIAN_POINT('Ctrl Pts',(-26.5850015682601,24.6348811943899,-11.7509913585452));
#36234=CARTESIAN_POINT('Ctrl Pts',(-26.5856296471964,24.6331222457525,-11.7508753147503));
#36235=CARTESIAN_POINT('Ctrl Pts',(-26.5868817555751,24.6296060402704,-11.7506435964224));
#36236=CARTESIAN_POINT('Ctrl Pts',(-26.5875057864466,24.6278487948381,-11.7505279219896));
#36237=CARTESIAN_POINT('Ctrl Pts',(-26.5892612073748,24.6228919627205,-11.7502019868022));
#36238=CARTESIAN_POINT('Ctrl Pts',(-26.5903890734256,24.6196911169978,-11.7499919374142));
#36239=CARTESIAN_POINT('Ctrl Pts',(-26.5950339544138,24.6064423723755,-11.7491242327899));
#36240=CARTESIAN_POINT('Ctrl Pts',(-26.5985062804809,24.5963787106053,-11.7484692162088));
#36241=CARTESIAN_POINT('Ctrl Pts',(-26.6602930171192,24.4143855986378,-11.7366942865875));
#36242=CARTESIAN_POINT('Ctrl Pts',(-26.7040359707909,24.2378198014382,-11.7263958643788));
#36243=CARTESIAN_POINT('Ctrl Pts',(-26.7593992612187,23.8911489492485,-11.7067094764478));
#36244=CARTESIAN_POINT('Ctrl Pts',(-26.7728825408738,23.7219710894425,-11.6973325312428));
#36245=CARTESIAN_POINT('Ctrl Pts',(-26.7730373760849,23.5018494115182,-11.6847662010004));
#36246=CARTESIAN_POINT('Ctrl Pts',(-26.771878018203,23.4511872622335,-11.6818502444379));
#36247=CARTESIAN_POINT('Ctrl Pts',(-26.7648382225419,23.2997749819227,-11.6730349342752));
#36248=CARTESIAN_POINT('Ctrl Pts',(-26.7554204206028,23.1992599943009,-11.6670475195143));
#36249=CARTESIAN_POINT('Ctrl Pts',(-26.7399895831919,23.0900531848866,-11.6603345982499));
#36250=CARTESIAN_POINT('Ctrl Pts',(-26.7386339354106,23.0807528852675,-11.6597612741537));
#36251=CARTESIAN_POINT('Ctrl Pts',(-26.7365634806811,23.0669713611633,-11.6589092293575));
#36252=CARTESIAN_POINT('Ctrl Pts',(-26.7358798515899,23.0624854440236,-11.658631497989));
#36253=CARTESIAN_POINT('Ctrl Pts',(-26.7346946293359,23.0548168951078,-11.6581560534883));
#36254=CARTESIAN_POINT('Ctrl Pts',(-26.7341977321053,23.0516335349656,-11.6579584897021));
#36255=CARTESIAN_POINT('Ctrl Pts',(-26.7332228166025,23.0454486434365,-11.6575742601792));
#36256=CARTESIAN_POINT('Ctrl Pts',(-26.7327453242576,23.0424470321234,-11.6573876113801));
#36257=CARTESIAN_POINT('Ctrl Pts',(-26.7315948250151,23.0352801267279,-11.6569415276695));
#36258=CARTESIAN_POINT('Ctrl Pts',(-26.7309178841769,23.0311154781202,-11.6566819679007));
#36259=CARTESIAN_POINT('Ctrl Pts',(-26.7288700457156,23.0186712175734,-11.6559053527913));
#36260=CARTESIAN_POINT('Ctrl Pts',(-26.7274749911721,23.0103956665729,-11.6553875293497));
#36261=CARTESIAN_POINT('Ctrl Pts',(-26.7152683425993,22.9396714945797,-11.6509502869785));
#36262=CARTESIAN_POINT('Ctrl Pts',(-26.7026497718723,22.8775527446523,-11.6469735072737));
#36263=CARTESIAN_POINT('Ctrl Pts',(-26.666013125833,22.7210116797256,-11.6367384716623));
#36264=CARTESIAN_POINT('Ctrl Pts',(-26.6395313934538,22.6272370678872,-11.6304057951029));
#36265=CARTESIAN_POINT('Ctrl Pts',(-26.5015604862611,22.2116566717861,-11.6014625951904));
#36266=CARTESIAN_POINT('Ctrl Pts',(-26.3437557371046,21.9075793658389,-11.5775911630559));
#36267=CARTESIAN_POINT('Ctrl Pts',(-26.1395697085601,21.6315126944463,-11.5558869418025));
#36268=CARTESIAN_POINT('Ctrl Pts',(-26.1378386876699,21.6291789019263,-11.5557034768337));
#36269=CARTESIAN_POINT('Ctrl Pts',(-26.1287259213196,21.6169275748415,-11.5547404722456));
#36270=CARTESIAN_POINT('Ctrl Pts',(-26.1212901732604,21.6070500545347,-11.5539644077823));
#36271=CARTESIAN_POINT('Ctrl Pts',(-26.1116165001503,21.5943524480285,-11.5529674909093));
#36272=CARTESIAN_POINT('Ctrl Pts',(-26.1094305677089,21.5914931548255,-11.5527430489065));
#36273=CARTESIAN_POINT('Ctrl Pts',(-26.106079599208,21.5871251295831,-11.552400258397));
#36274=CARTESIAN_POINT('Ctrl Pts',(-26.1049180161304,21.5856137713544,-11.5522816659478));
#36275=CARTESIAN_POINT('Ctrl Pts',(-26.1027317979032,21.5827744577653,-11.5520589013934));
#36276=CARTESIAN_POINT('Ctrl Pts',(-26.1017074710651,21.5814462770792,-11.5519547082502));
#36277=CARTESIAN_POINT('Ctrl Pts',(-26.0993461335054,21.5783894158617,-11.5517149314509));
#36278=CARTESIAN_POINT('Ctrl Pts',(-26.0980084034458,21.5766612983333,-11.5515794001561));
#36279=CARTESIAN_POINT('Ctrl Pts',(-26.0942755028341,21.5718491519918,-11.5512020498367));
#36280=CARTESIAN_POINT('Ctrl Pts',(-26.0918764731326,21.5687681004671,-11.5509605056179));
#36281=CARTESIAN_POINT('Ctrl Pts',(-26.0783905485038,21.5515130411277,-11.5496080561479));
#36282=CARTESIAN_POINT('Ctrl Pts',(-26.0671904022372,21.5374273593754,-11.5485051215592));
#36283=CARTESIAN_POINT('Ctrl Pts',(-26.0344135348248,21.4969074761311,-11.5453331139805));
#36284=CARTESIAN_POINT('Ctrl Pts',(-26.0125336022343,21.4707203864211,-11.5432840795104));
#36285=CARTESIAN_POINT('Ctrl Pts',(-25.9265563190034,21.3710781478826,-11.5354692455696));
#36286=CARTESIAN_POINT('Ctrl Pts',(-25.8595502832995,21.3001930534863,-11.529869955924));
#36287=CARTESIAN_POINT('Ctrl Pts',(-25.5382899223414,20.9898307854437,-11.5045779426702));
#36288=CARTESIAN_POINT('Ctrl Pts',(-25.2494218773259,20.7896594059914,-11.4856929433556));
#36289=CARTESIAN_POINT('Ctrl Pts',(-24.9152396361417,20.6307727623383,-11.4633212951716));
#36290=CARTESIAN_POINT('Ctrl Pts',(-24.8963314965093,20.6220067585805,-11.4620550803262));
#36291=CARTESIAN_POINT('Ctrl Pts',(-24.8715917977068,20.6108274356281,-11.4603973473469));
#36292=CARTESIAN_POINT('Ctrl Pts',(-24.8658360122322,20.6082468457493,-11.4600115999601));
#36293=CARTESIAN_POINT('Ctrl Pts',(-24.8569726721231,20.6043042040786,-11.4594174672457));
#36294=CARTESIAN_POINT('Ctrl Pts',(-24.8538704581745,20.6029301238122,-11.4592094952645));
#36295=CARTESIAN_POINT('Ctrl Pts',(-24.8477931353258,20.600249734718,-11.4588020258503));
#36296=CARTESIAN_POINT('Ctrl Pts',(-24.8448182086018,20.5989430209369,-11.4586025426014));
#36297=CARTESIAN_POINT('Ctrl Pts',(-24.8385197517321,20.596187827553,-11.458180152177));
#36298=CARTESIAN_POINT('Ctrl Pts',(-24.8351957452489,20.5947404535176,-11.4579572074583));
#36299=CARTESIAN_POINT('Ctrl Pts',(-24.8257148785467,20.5906312118609,-11.4573212302767));
#36300=CARTESIAN_POINT('Ctrl Pts',(-24.8195521676355,20.5879829645953,-11.4569077329533));
#36301=CARTESIAN_POINT('Ctrl Pts',(-24.8058691274709,20.5821536112319,-11.4559894008776));
#36302=CARTESIAN_POINT('Ctrl Pts',(-24.7983449040709,20.5789818161112,-11.4554842513851));
#36303=CARTESIAN_POINT('Ctrl Pts',(-24.625706606652,20.5069785489612,-11.4438898489663));
#36304=CARTESIAN_POINT('Ctrl Pts',(-24.455187682488,20.451996450664,-11.4323251316667));
#36305=CARTESIAN_POINT('Ctrl Pts',(-23.9740679553818,20.3399845257404,-11.3994472392227));
#36306=CARTESIAN_POINT('Ctrl Pts',(-23.6583168313934,20.3139337483487,-11.3774658963678));
#36307=CARTESIAN_POINT('Ctrl Pts',(-23.327523705548,20.3351668566534,-11.3564861016113));
#36308=CARTESIAN_POINT('Ctrl Pts',(-23.3112412308057,20.3363362831438,-11.3554591774012));
#36309=CARTESIAN_POINT('Ctrl Pts',(-23.2913838105475,20.3379142128347,-11.354214386083));
#36310=CARTESIAN_POINT('Ctrl Pts',(-23.2878001381906,20.3382050178712,-11.3539900407692));
#36311=CARTESIAN_POINT('Ctrl Pts',(-23.2818967585076,20.3386940063553,-11.3536209836586));
#36312=CARTESIAN_POINT('Ctrl Pts',(-23.279576779002,20.3388887062058,-11.3534760762236));
#36313=CARTESIAN_POINT('Ctrl Pts',(-23.2753964832033,20.339244091708,-11.3532152071376));
#36314=CARTESIAN_POINT('Ctrl Pts',(-23.2735360999324,20.3394038797788,-11.3530991949451));
#36315=CARTESIAN_POINT('Ctrl Pts',(-23.2695385087444,20.3397507325356,-11.3528500888909));
#36316=CARTESIAN_POINT('Ctrl Pts',(-23.2674013543699,20.3399383139529,-11.3527170249973));
#36317=CARTESIAN_POINT('Ctrl Pts',(-23.2615552280395,20.3404573208414,-11.352353331752));
#36318=CARTESIAN_POINT('Ctrl Pts',(-23.2578466259508,20.3407930420963,-11.3521229456498));
#36319=CARTESIAN_POINT('Ctrl Pts',(-23.2386781969474,20.3425617649046,-11.3509338288754));
#36320=CARTESIAN_POINT('Ctrl Pts',(-23.2232279461484,20.3441000766881,-11.3499809734857));
#36321=CARTESIAN_POINT('Ctrl Pts',(-23.1352367201633,20.3535036522515,-11.3445832232496));
#36322=CARTESIAN_POINT('Ctrl Pts',(-23.062962282041,20.3637196884551,-11.3402615051862));
#36323=CARTESIAN_POINT('Ctrl Pts',(-22.9091135509578,20.3908242158234,-11.3311840095511));
#36324=CARTESIAN_POINT('Ctrl Pts',(-22.8277217661702,20.4084382096876,-11.3264559130388));
#36325=CARTESIAN_POINT('Ctrl Pts',(-22.5558477524613,20.4784003092772,-11.3106533724097));
#36326=CARTESIAN_POINT('Ctrl Pts',(-22.3695297953643,20.5450886411294,-11.2997819464066));
#36327=CARTESIAN_POINT('Ctrl Pts',(-22.1321173251209,20.6555754981075,-11.2847921199108));
#36328=CARTESIAN_POINT('Ctrl Pts',(-22.0745765457262,20.6844817292307,-11.2810671729841));
#36329=CARTESIAN_POINT('Ctrl Pts',(-22.0071428917295,20.7209273655582,-11.2765681752944));
#36330=CARTESIAN_POINT('Ctrl Pts',(-21.9963770340512,20.7268256796352,-11.2758457740146));
#36331=CARTESIAN_POINT('Ctrl Pts',(-21.9259808504998,20.7659183729809,-11.2710942010826));
#36332=CARTESIAN_POINT('Ctrl Pts',(-21.8673877093177,20.8009362274774,-11.2670068380896));
#36333=CARTESIAN_POINT('Ctrl Pts',(-21.8020335167647,20.8428670065289,-11.2622772292564));
#36334=CARTESIAN_POINT('Ctrl Pts',(-21.794136039208,20.8479829359844,-11.261702799807));
#36335=CARTESIAN_POINT('Ctrl Pts',(-21.7826008177714,20.8555272934198,-11.2608594761728));
#36336=CARTESIAN_POINT('Ctrl Pts',(-21.7789453816287,20.85792868948,-11.2605915964451));
#36337=CARTESIAN_POINT('Ctrl Pts',(-21.7724701390622,20.8622014198005,-11.260115939557));
#36338=CARTESIAN_POINT('Ctrl Pts',(-21.7696483650283,20.8640697722345,-11.2599082748532));
#36339=CARTESIAN_POINT('Ctrl Pts',(-21.7638504152943,20.867921859708,-11.2594807903488));
#36340=CARTESIAN_POINT('Ctrl Pts',(-21.7608745896182,20.869906110874,-11.2592609512581));
#36341=CARTESIAN_POINT('Ctrl Pts',(-21.7532603366251,20.8750015513314,-11.2586973405516));
#36342=CARTESIAN_POINT('Ctrl Pts',(-21.7486266967359,20.8781198427631,-11.2583533004721));
#36343=CARTESIAN_POINT('Ctrl Pts',(-21.7385950569707,20.8849087698546,-11.2576061629992));
#36344=CARTESIAN_POINT('Ctrl Pts',(-21.7332000651039,20.8885837868745,-11.2572028999372));
#36345=CARTESIAN_POINT('Ctrl Pts',(-21.7177118992512,20.8992032130097,-11.256040981323));
#36346=CARTESIAN_POINT('Ctrl Pts',(-21.7076471934574,20.906188761572,-11.2552807580479));
#36347=CARTESIAN_POINT('Ctrl Pts',(-21.6105691107426,20.9743906261362,-11.2478973922628));
#36348=CARTESIAN_POINT('Ctrl Pts',(-21.5266067147818,21.0398163794405,-11.2411116985377));
#36349=CARTESIAN_POINT('Ctrl Pts',(-21.2949796700702,21.2394868389777,-11.2211817427192));
#36350=CARTESIAN_POINT('Ctrl Pts',(-21.1563483875284,21.3834346232592,-11.2076828726417));
#36351=CARTESIAN_POINT('Ctrl Pts',(-20.9161574363896,21.6842195359519,-11.1816406360991));
#36352=CARTESIAN_POINT('Ctrl Pts',(-20.8131096941293,21.838936352253,-11.1691544153083));
#36353=CARTESIAN_POINT('Ctrl Pts',(-20.7185870257793,22.0114503488514,-11.1567620396726));
#36354=CARTESIAN_POINT('Ctrl Pts',(-20.713284006594,22.0212491662408,-11.1560631645944));
#36355=CARTESIAN_POINT('Ctrl Pts',(-20.706402801591,22.0341231779158,-11.1551517070603));
#36356=CARTESIAN_POINT('Ctrl Pts',(-20.704778678292,22.0371735335358,-11.1549362412944));
#36357=CARTESIAN_POINT('Ctrl Pts',(-20.7022798554167,22.0418849631516,-11.1546042122703));
#36358=CARTESIAN_POINT('Ctrl Pts',(-20.701401701886,22.0435441869247,-11.1544874285238));
#36359=CARTESIAN_POINT('Ctrl Pts',(-20.6996535433311,22.0468542304672,-11.1542547467543));
#36360=CARTESIAN_POINT('Ctrl Pts',(-20.6987835275693,22.0485050285722,-11.1541388487279));
#36361=CARTESIAN_POINT('Ctrl Pts',(-20.6968390951136,22.0522022439667,-11.1538796031437));
#36362=CARTESIAN_POINT('Ctrl Pts',(-20.6957654482599,22.0542490573644,-11.1537363052734));
#36363=CARTESIAN_POINT('Ctrl Pts',(-20.692611402426,22.0602777258823,-11.1533148874902));
#36364=CARTESIAN_POINT('Ctrl Pts',(-20.690537115639,22.0642627990928,-11.1530371563274));
#36365=CARTESIAN_POINT('Ctrl Pts',(-20.6748453152691,22.0945640762878,-11.150931606834));
#36366=CARTESIAN_POINT('Ctrl Pts',(-20.6615824102286,22.1210637336271,-11.1491258799801));
#36367=CARTESIAN_POINT('Ctrl Pts',(-20.6177423398682,22.2117618184915,-11.1430532289471));
#36368=CARTESIAN_POINT('Ctrl Pts',(-20.5889231110985,22.2767914951118,-11.1388801528287));
#36369=CARTESIAN_POINT('Ctrl Pts',(-20.4317098374001,22.6658094082142,-11.1146673850531));
#36370=CARTESIAN_POINT('Ctrl Pts',(-20.3544012393794,23.0079261207296,-11.0961163829572));
#36371=CARTESIAN_POINT('Ctrl Pts',(-20.3329972408215,23.3620375716651,-11.0751444405818));
#36372=CARTESIAN_POINT('Ctrl Pts',(-20.332638946003,23.3682654710559,-11.074775149737));
#36373=CARTESIAN_POINT('Ctrl Pts',(-20.3291047356388,23.432973269957,-11.0709334189033));
#36374=CARTESIAN_POINT('Ctrl Pts',(-20.3275055692309,23.491525264142,-11.0674161107802));
#36375=CARTESIAN_POINT('Ctrl Pts',(-20.3275020697863,23.5590868323728,-11.0632996861545));
#36376=CARTESIAN_POINT('Ctrl Pts',(-20.3275393145615,23.5680879494281,-11.0627500831965));
#36377=CARTESIAN_POINT('Ctrl Pts',(-20.3276504210972,23.5814302376652,-11.0619336259482));
#36378=CARTESIAN_POINT('Ctrl Pts',(-20.3276953477459,23.5857716598433,-11.0616676803245));
#36379=CARTESIAN_POINT('Ctrl Pts',(-20.3277907204021,23.5934820312754,-11.0611948582121));
#36380=CARTESIAN_POINT('Ctrl Pts',(-20.3278376770741,23.5968510236899,-11.0609880915805));
#36381=CARTESIAN_POINT('Ctrl Pts',(-20.3279461408953,23.6038457802976,-11.0605584431339));
#36382=CARTESIAN_POINT('Ctrl Pts',(-20.3280084845895,23.6074715251033,-11.060335535339));
#36383=CARTESIAN_POINT('Ctrl Pts',(-20.3281862935942,23.616887836597,-11.0597561083046));
#36384=CARTESIAN_POINT('Ctrl Pts',(-20.3283112489331,23.6226781922177,-11.0593992915113));
#36385=CARTESIAN_POINT('Ctrl Pts',(-20.3286175957744,23.6352970080275,-11.0586205616068));
#36386=CARTESIAN_POINT('Ctrl Pts',(-20.328805089886,23.6421252795975,-11.0581984581353));
#36387=CARTESIAN_POINT('Ctrl Pts',(-20.3294136468704,23.6619864799954,-11.0569685821752));
#36388=CARTESIAN_POINT('Ctrl Pts',(-20.3298920988453,23.6750173972613,-11.0561590105538));
#36389=CARTESIAN_POINT('Ctrl Pts',(-20.3317850816313,23.7192508449693,-11.0534017355312));
#36390=CARTESIAN_POINT('Ctrl Pts',(-20.3335741042706,23.7504348006801,-11.0514423501007));
#36391=CARTESIAN_POINT('Ctrl Pts',(-20.3431774021607,23.883874472474,-11.0429890662033));
#36392=CARTESIAN_POINT('Ctrl Pts',(-20.3554161543005,23.9857423150514,-11.036359679306));
#36393=CARTESIAN_POINT('Ctrl Pts',(-20.4002591410788,24.2513076632075,-11.0186251511043));
#36394=CARTESIAN_POINT('Ctrl Pts',(-20.4407536000566,24.4133543127671,-11.0073331271241));
#36395=CARTESIAN_POINT('Ctrl Pts',(-20.5533437646642,24.7503348948696,-10.9832909540427));
#36396=CARTESIAN_POINT('Ctrl Pts',(-20.628669929482,24.9235817454716,-10.9705877683187));
#36397=CARTESIAN_POINT('Ctrl Pts',(-20.7243003760567,25.099526030514,-10.9579658431494));
#36398=CARTESIAN_POINT('Ctrl Pts',(-20.7299334492485,25.1097570181433,-10.9572330209411));
#36399=CARTESIAN_POINT('Ctrl Pts',(-20.7373367663845,25.1230318717555,-10.9562838748192));
#36400=CARTESIAN_POINT('Ctrl Pts',(-20.7390564617027,25.1261036070177,-10.9560643662478));
#36401=CARTESIAN_POINT('Ctrl Pts',(-20.741707308586,25.1308204250409,-10.9557274894138));
#36402=CARTESIAN_POINT('Ctrl Pts',(-20.7426348731287,25.1324675041543,-10.9556098902253));
#36403=CARTESIAN_POINT('Ctrl Pts',(-20.7444803346888,25.135737762856,-10.9553764708517));
#36404=CARTESIAN_POINT('Ctrl Pts',(-20.7453981861716,25.1373609527406,-10.9552606491788));
#36405=CARTESIAN_POINT('Ctrl Pts',(-20.7474458796603,25.1409749064102,-10.9550028570207));
#36406=CARTESIAN_POINT('Ctrl Pts',(-20.7485764313825,25.1429652588136,-10.9548609336465));
#36407=CARTESIAN_POINT('Ctrl Pts',(-20.7518795295061,25.1487660105674,-10.9544474578528));
#36408=CARTESIAN_POINT('Ctrl Pts',(-20.7540577465721,25.152573200509,-10.9541762722495));
#36409=CARTESIAN_POINT('Ctrl Pts',(-20.7696866439071,25.1797611960014,-10.9522409462619));
#36410=CARTESIAN_POINT('Ctrl Pts',(-20.7834231412716,25.2029776700911,-10.9505950564734));
#36411=CARTESIAN_POINT('Ctrl Pts',(-20.823404865293,25.2686561135142,-10.9459501724487));
#36412=CARTESIAN_POINT('Ctrl Pts',(-20.8503482493828,25.3106861463705,-10.9429913556266));
#36413=CARTESIAN_POINT('Ctrl Pts',(-20.9050930514259,25.3918693509267,-10.9372685578144));
#36414=CARTESIAN_POINT('Ctrl Pts',(-20.9328140951954,25.4310602237635,-10.9345022019202));
#36415=CARTESIAN_POINT('Ctrl Pts',(-20.9823801223373,25.4979151446925,-10.9297501169584));
#36416=CARTESIAN_POINT('Ctrl Pts',(-21.0038219327036,25.5258662750326,-10.9277529211528));
#36417=CARTESIAN_POINT('Ctrl Pts',(-21.1980512743488,25.770642959815,-10.9101179198671));
#36418=CARTESIAN_POINT('Ctrl Pts',(-21.3976749256344,25.96466572331,-10.8949955102029));
#36419=CARTESIAN_POINT('Ctrl Pts',(-21.6251372096428,26.1348405511653,-10.8782883019415));
#36420=CARTESIAN_POINT('Ctrl Pts',(-21.6306203456497,26.1389156041942,-10.877885920855));
#36421=CARTESIAN_POINT('Ctrl Pts',(-21.6916017370523,26.1839365311524,-10.8734145388434));
#36422=CARTESIAN_POINT('Ctrl Pts',(-21.7483842412458,26.2231056451519,-10.8692848236058));
#36423=CARTESIAN_POINT('Ctrl Pts',(-21.8143135424199,26.2655282946416,-10.8645096481306));
#36424=CARTESIAN_POINT('Ctrl Pts',(-21.8222729718332,26.2706005390368,-10.8639334865715));
#36425=CARTESIAN_POINT('Ctrl Pts',(-21.8339577650372,26.2779748439592,-10.8630880938868));
#36426=CARTESIAN_POINT('Ctrl Pts',(-21.8376657736613,26.2803044240202,-10.8628198843771));
#36427=CARTESIAN_POINT('Ctrl Pts',(-21.8442485226174,26.2844213893906,-10.8623438465494));
#36428=CARTESIAN_POINT('Ctrl Pts',(-21.8471213583685,26.2862118200774,-10.8621361312973));
#36429=CARTESIAN_POINT('Ctrl Pts',(-21.8530340518322,26.2898838527492,-10.8617086972607));
#36430=CARTESIAN_POINT('Ctrl Pts',(-21.8560742292637,26.2917649287298,-10.8614889594392));
#36431=CARTESIAN_POINT('Ctrl Pts',(-21.8638571161662,26.2965626134129,-10.8609265252893));
#36432=CARTESIAN_POINT('Ctrl Pts',(-21.8686042510996,26.2994719885973,-10.8605835631688));
#36433=CARTESIAN_POINT('Ctrl Pts',(-21.878916981061,26.3057556438926,-10.8598386963904));
#36434=CARTESIAN_POINT('Ctrl Pts',(-21.8844852977342,26.3091253894773,-10.8594366268668));
#36435=CARTESIAN_POINT('Ctrl Pts',(-21.9005219436543,26.3187639428006,-10.8582789918572));
#36436=CARTESIAN_POINT('Ctrl Pts',(-21.9110156314546,26.3249901453856,-10.8575218726729));
#36437=CARTESIAN_POINT('Ctrl Pts',(-21.9461964382207,26.3455946930952,-10.8549847189624));
#36438=CARTESIAN_POINT('Ctrl Pts',(-21.971038796963,26.3597040165143,-10.8531949987811));
#36439=CARTESIAN_POINT('Ctrl Pts',(-22.0221954802462,26.38786578011,-10.8495124069177));
#36440=CARTESIAN_POINT('Ctrl Pts',(-22.0485217771435,26.4018856884949,-10.8476187983523));
#36441=CARTESIAN_POINT('Ctrl Pts',(-22.0750360250409,26.4155367795477,-10.8457129588805));
#36442=CARTESIAN_POINT('Origin',(-23.5502525316942,23.5502525316942,-77.3107734492734));
#36443=CARTESIAN_POINT('',(-22.075036015341,26.4155367745536,-9.34735996012824));
#36444=CARTESIAN_POINT('',(-22.0750360153461,26.4155367745563,-9.5929697214734));
#36445=CARTESIAN_POINT('',(-22.0750360153461,26.4155367745563,-77.3107734492734));
#36446=CARTESIAN_POINT('Ctrl Pts',(-22.075036015341,26.4155367745536,-9.34735996012824));
#36447=CARTESIAN_POINT('Ctrl Pts',(-22.0747390535194,26.4153838811766,-9.34738251109341));
#36448=CARTESIAN_POINT('Ctrl Pts',(-22.074442114912,26.4152309413477,-9.34740506162473));
#36449=CARTESIAN_POINT('Ctrl Pts',(-21.9846698447257,26.3689755900912,-9.35422307522353));
#36450=CARTESIAN_POINT('Ctrl Pts',(-21.897397509723,26.3187036640452,-9.36097361240509));
#36451=CARTESIAN_POINT('Ctrl Pts',(-21.7782939954875,26.2424526342591,-9.37023478749855));
#36452=CARTESIAN_POINT('Ctrl Pts',(-21.7443895201671,26.2198288196812,-9.3728766708831));
#36453=CARTESIAN_POINT('Ctrl Pts',(-21.6862415807607,26.179412874206,-9.37740532370636));
#36454=CARTESIAN_POINT('Ctrl Pts',(-21.6618015139228,26.1619136594497,-9.37930800960738));
#36455=CARTESIAN_POINT('Ctrl Pts',(-21.6339917551444,26.1414071768864,-9.38146880448542));
#36456=CARTESIAN_POINT('Ctrl Pts',(-21.630380282287,26.1387324534987,-9.38174932972123));
#36457=CARTESIAN_POINT('Ctrl Pts',(-21.624904404594,26.1346591529001,-9.38217453312394));
#36458=CARTESIAN_POINT('Ctrl Pts',(-21.6230359214072,26.1332661072253,-9.38231959624138));
#36459=CARTESIAN_POINT('Ctrl Pts',(-21.6196731006669,26.1307532795934,-9.3825806272189));
#36460=CARTESIAN_POINT('Ctrl Pts',(-21.6181782286314,26.1296342283258,-9.38269664592237));
#36461=CARTESIAN_POINT('Ctrl Pts',(-21.6151910482777,26.1273939911176,-9.38292844961065));
#36462=CARTESIAN_POINT('Ctrl Pts',(-21.6136987473629,26.1262728124598,-9.38304423427671));
#36463=CARTESIAN_POINT('Ctrl Pts',(-21.6094885644167,26.1231039393174,-9.38337084826195));
#36464=CARTESIAN_POINT('Ctrl Pts',(-21.6067729400595,26.1210532278869,-9.38358146475285));
#36465=CARTESIAN_POINT('Ctrl Pts',(-21.5955224347469,26.1125293621777,-9.38445382326191));
#36466=CARTESIAN_POINT('Ctrl Pts',(-21.5870164786845,26.1060178800281,-9.38511289173423));
#36467=CARTESIAN_POINT('Ctrl Pts',(-21.4442423141574,25.9955879750525,-9.39617036879566));
#36468=CARTESIAN_POINT('Ctrl Pts',(-21.3183385674023,25.8812442180018,-9.40585086607581));
#36469=CARTESIAN_POINT('Ctrl Pts',(-21.0837018777555,25.6316195088344,-9.42510198676223));
#36470=CARTESIAN_POINT('Ctrl Pts',(-20.975700453274,25.4964389287546,-9.43464376881431));
#36471=CARTESIAN_POINT('Ctrl Pts',(-20.8154770566981,25.2590634167451,-9.45095020197856));
#36472=CARTESIAN_POINT('Ctrl Pts',(-20.7569321223013,25.1615839265824,-9.45753208671471));
#36473=CARTESIAN_POINT('Ctrl Pts',(-20.6801694375884,25.0169668922129,-9.46728276647328));
#36474=CARTESIAN_POINT('Ctrl Pts',(-20.6577147213345,24.9721711549148,-9.47030061012103));
#36475=CARTESIAN_POINT('Ctrl Pts',(-20.6329331207617,24.9197150798299,-9.4738381028785));
#36476=CARTESIAN_POINT('Ctrl Pts',(-20.6295784043342,24.9125457659714,-9.47432165391052));
#36477=CARTESIAN_POINT('Ctrl Pts',(-20.6244987995178,24.9015852106788,-9.47506105062484));
#36478=CARTESIAN_POINT('Ctrl Pts',(-20.6227547759665,24.897802827819,-9.47531623408223));
#36479=CARTESIAN_POINT('Ctrl Pts',(-20.6197539517938,24.8912614158912,-9.47575760587462));
#36480=CARTESIAN_POINT('Ctrl Pts',(-20.6184937000125,24.8885039681021,-9.47594367479258));
#36481=CARTESIAN_POINT('Ctrl Pts',(-20.6158932303915,24.882792802761,-9.47632908813932));
#36482=CARTESIAN_POINT('Ctrl Pts',(-20.6145535773565,24.879838832965,-9.47652845178942));
#36483=CARTESIAN_POINT('Ctrl Pts',(-20.6113176049361,24.8726746958927,-9.47701200465124));
#36484=CARTESIAN_POINT('Ctrl Pts',(-20.6094258739274,24.8684624742697,-9.47729635145109));
#36485=CARTESIAN_POINT('Ctrl Pts',(-20.6024112757544,24.8527531724368,-9.47835696069549));
#36486=CARTESIAN_POINT('Ctrl Pts',(-20.5973467762154,24.8412302934675,-9.47913522400431));
#36487=CARTESIAN_POINT('Ctrl Pts',(-20.511514307439,24.642794314304,-9.49254377675888));
#36488=CARTESIAN_POINT('Ctrl Pts',(-20.4485872706461,24.448707695008,-9.50579587912776));
#36489=CARTESIAN_POINT('Ctrl Pts',(-20.3686898450663,24.0895205169718,-9.530443807561));
#36490=CARTESIAN_POINT('Ctrl Pts',(-20.3453248601385,23.9265335490469,-9.54165917316333));
#36491=CARTESIAN_POINT('Ctrl Pts',(-20.3285343974546,23.6721162340426,-9.55877587430546));
#36492=CARTESIAN_POINT('Ctrl Pts',(-20.3263818166247,23.5815353264292,-9.56479027668491));
#36493=CARTESIAN_POINT('Ctrl Pts',(-20.3289403104488,23.4424542564692,-9.57379463976762));
#36494=CARTESIAN_POINT('Ctrl Pts',(-20.3309289690499,23.3939536662682,-9.57689133459828));
#36495=CARTESIAN_POINT('Ctrl Pts',(-20.3343289991591,23.3405427262172,-9.58024032595217));
#36496=CARTESIAN_POINT('Ctrl Pts',(-20.3346569432289,23.335572812433,-9.58055136525348));
#36497=CARTESIAN_POINT('Ctrl Pts',(-20.3351620663596,23.3281787380981,-9.58101322711576));
#36498=CARTESIAN_POINT('Ctrl Pts',(-20.3353304663261,23.3257540154612,-9.58116454166228));
#36499=CARTESIAN_POINT('Ctrl Pts',(-20.3356216094619,23.3216294779106,-9.58142168733151));
#36500=CARTESIAN_POINT('Ctrl Pts',(-20.3357429578991,23.3199295694686,-9.58152759765232));
#36501=CARTESIAN_POINT('Ctrl Pts',(-20.3359940496529,23.3164510057501,-9.58174417829698));
#36502=CARTESIAN_POINT('Ctrl Pts',(-20.3361239206669,23.3146723654604,-9.58185484107985));
#36503=CARTESIAN_POINT('Ctrl Pts',(-20.3364387004545,23.3104100343879,-9.58211984809862));
#36504=CARTESIAN_POINT('Ctrl Pts',(-20.3366250124269,23.3079264437729,-9.58227411269627));
#36505=CARTESIAN_POINT('Ctrl Pts',(-20.3373073214612,23.2989702624481,-9.58282987742307));
#36506=CARTESIAN_POINT('Ctrl Pts',(-20.3378200000249,23.2924989012617,-9.58323044113451));
#36507=CARTESIAN_POINT('Ctrl Pts',(-20.3461491522941,23.1912497306722,-9.58948238160495));
#36508=CARTESIAN_POINT('Ctrl Pts',(-20.3581384015592,23.096851044737,-9.59510353979885));
#36509=CARTESIAN_POINT('Ctrl Pts',(-20.4035777894445,22.8330912459621,-9.61056684772774));
#36510=CARTESIAN_POINT('Ctrl Pts',(-20.4464751059084,22.6656873590403,-9.62010688841638));
#36511=CARTESIAN_POINT('Ctrl Pts',(-20.5470761590138,22.3730571221707,-9.63742849064915));
#36512=CARTESIAN_POINT('Ctrl Pts',(-20.5997818017243,22.2465747241142,-9.64514636155865));
#36513=CARTESIAN_POINT('Ctrl Pts',(-20.6881973355374,22.0674472030933,-9.65675171250586));
#36514=CARTESIAN_POINT('Ctrl Pts',(-20.7176719379784,22.0118904072639,-9.66045042146399));
#36515=CARTESIAN_POINT('Ctrl Pts',(-20.7708824173946,21.9183138468992,-9.66687813589731));
#36516=CARTESIAN_POINT('Ctrl Pts',(-20.7938211840708,21.879860954121,-9.66957889943404));
#36517=CARTESIAN_POINT('Ctrl Pts',(-20.8216432702251,21.8353564389058,-9.67277976901697));
#36518=CARTESIAN_POINT('Ctrl Pts',(-20.8257573184495,21.8288278478321,-9.67325124469969));
#36519=CARTESIAN_POINT('Ctrl Pts',(-20.8320992698812,21.818843477422,-9.67397526689835));
#36520=CARTESIAN_POINT('Ctrl Pts',(-20.8343104245528,21.8153770496123,-9.67422719008157));
#36521=CARTESIAN_POINT('Ctrl Pts',(-20.8383330506354,21.8090973154977,-9.67468457956155));
#36522=CARTESIAN_POINT('Ctrl Pts',(-20.8401422840608,21.8062825766283,-9.67488996213777));
#36523=CARTESIAN_POINT('Ctrl Pts',(-20.8440390567054,21.8002408283811,-9.67533160513456));
#36524=CARTESIAN_POINT('Ctrl Pts',(-20.8461279898384,21.7970147281226,-9.67556791749557));
#36525=CARTESIAN_POINT('Ctrl Pts',(-20.8517487772766,21.7883680557496,-9.67620260630327));
#36526=CARTESIAN_POINT('Ctrl Pts',(-20.8552911780625,21.7829543902832,-9.6766013779747));
#36527=CARTESIAN_POINT('Ctrl Pts',(-20.8714722502908,21.7583874838224,-9.67841736847568));
#36528=CARTESIAN_POINT('Ctrl Pts',(-20.8842987166384,21.7393592830675,-9.67984165159534));
#36529=CARTESIAN_POINT('Ctrl Pts',(-20.9042960531253,21.7103659765101,-9.6820396668591));
#36530=CARTESIAN_POINT('Ctrl Pts',(-20.9113226617626,21.70030189525,-9.6828078612671));
#36531=CARTESIAN_POINT('Ctrl Pts',(-20.9214112362097,21.6860266573506,-9.68390501421969));
#36532=CARTESIAN_POINT('Ctrl Pts',(-20.9244262424308,21.6817823110277,-9.68423217595527));
#36533=CARTESIAN_POINT('Ctrl Pts',(-20.9285214914673,21.6760467517025,-9.6846755792827));
#36534=CARTESIAN_POINT('Ctrl Pts',(-20.9295927593767,21.6745491140992,-9.68479147830318));
#36535=CARTESIAN_POINT('Ctrl Pts',(-20.9333950427281,21.6692431199714,-9.68520252397582));
#36536=CARTESIAN_POINT('Ctrl Pts',(-20.9361330710183,21.6654398169953,-9.68549793770175));
#36537=CARTESIAN_POINT('Ctrl Pts',(-20.9400733968353,21.6599915449934,-9.6859222421535));
#36538=CARTESIAN_POINT('Ctrl Pts',(-20.9412689831607,21.6583417099727,-9.68605087713408));
#36539=CARTESIAN_POINT('Ctrl Pts',(-20.946536609641,21.6510872009053,-9.68661715139819));
#36540=CARTESIAN_POINT('Ctrl Pts',(-20.9506251277027,21.6454945639614,-9.68705541680821));
#36541=CARTESIAN_POINT('Ctrl Pts',(-20.9576949891945,21.6358889446205,-9.68781112252777));
#36542=CARTESIAN_POINT('Ctrl Pts',(-20.9606677080853,21.6318696200805,-9.68812823470617));
#36543=CARTESIAN_POINT('Ctrl Pts',(-20.9689327041858,21.6207489821766,-9.68900811656925));
#36544=CARTESIAN_POINT('Ctrl Pts',(-20.9742448912833,21.6136625819231,-9.68957163732889));
#36545=CARTESIAN_POINT('Ctrl Pts',(-20.9902763494368,21.5924594647369,-9.69126628620316));
#36546=CARTESIAN_POINT('Ctrl Pts',(-21.0010828125483,21.5784093659837,-9.69240067716879));
#36547=CARTESIAN_POINT('Ctrl Pts',(-21.0262806186788,21.5462016008251,-9.69502770223168));
#36548=CARTESIAN_POINT('Ctrl Pts',(-21.0407528471351,21.5281087083611,-9.6965232796239));
#36549=CARTESIAN_POINT('Ctrl Pts',(-21.0955479468654,21.4610992005697,-9.70213690134174));
#36550=CARTESIAN_POINT('Ctrl Pts',(-21.1371144419831,21.4132218745046,-9.70629882116239));
#36551=CARTESIAN_POINT('Ctrl Pts',(-21.3265191106306,21.2076371705,-9.72483299511883));
#36552=CARTESIAN_POINT('Ctrl Pts',(-21.4885934981391,21.0638115873531,-9.73964224288625));
#36553=CARTESIAN_POINT('Ctrl Pts',(-21.7325980098313,20.8876513193275,-9.75978129155776));
#36554=CARTESIAN_POINT('Ctrl Pts',(-21.803313444654,20.8407287259957,-9.76539032347615));
#36555=CARTESIAN_POINT('Ctrl Pts',(-21.911519628833,20.7749292336555,-9.77355446550235));
#36556=CARTESIAN_POINT('Ctrl Pts',(-21.9476574030216,20.753905949627,-9.77621448616853));
#36557=CARTESIAN_POINT('Ctrl Pts',(-21.9885050780738,20.7311947527816,-9.77913888715837));
#36558=CARTESIAN_POINT('Ctrl Pts',(-21.992819598548,20.7288088357721,-9.77944676284489));
#36559=CARTESIAN_POINT('Ctrl Pts',(-21.9992604264859,20.7252663528676,-9.77990483953177));
#36560=CARTESIAN_POINT('Ctrl Pts',(-22.0013825635011,20.7241022804333,-9.78005552085674));
#36561=CARTESIAN_POINT('Ctrl Pts',(-22.004999696645,20.7221234439255,-9.78031193102136));
#36562=CARTESIAN_POINT('Ctrl Pts',(-22.0064940271831,20.7213074737059,-9.78041773790236));
#36563=CARTESIAN_POINT('Ctrl Pts',(-22.0095578730891,20.7196376296129,-9.78063442293591));
#36564=CARTESIAN_POINT('Ctrl Pts',(-22.0111274486605,20.7187838785471,-9.78074529307251));
#36565=CARTESIAN_POINT('Ctrl Pts',(-22.0148976076577,20.7167372087553,-9.78101128314075));
#36566=CARTESIAN_POINT('Ctrl Pts',(-22.0170988765896,20.7155455454201,-9.78116632210662));
#36567=CARTESIAN_POINT('Ctrl Pts',(-22.025083306796,20.7112351719233,-9.78172773152173));
#36568=CARTESIAN_POINT('Ctrl Pts',(-22.0308746651521,20.7081315571201,-9.78213314045711));
#36569=CARTESIAN_POINT('Ctrl Pts',(-22.1254957442279,20.6577955730134,-9.78872821189812));
#36570=CARTESIAN_POINT('Ctrl Pts',(-22.2164904522242,20.61472488069,-9.79466012494776));
#36571=CARTESIAN_POINT('Ctrl Pts',(-22.5520284211504,20.4747357422122,-9.81560844117375));
#36572=CARTESIAN_POINT('Ctrl Pts',(-22.8061803318503,20.4035672265499,-9.82984096156313));
#36573=CARTESIAN_POINT('Ctrl Pts',(-23.166379967222,20.3488413569926,-9.85068814070944));
#36574=CARTESIAN_POINT('Ctrl Pts',(-23.2672455667249,20.3383534202546,-9.8565856651163));
#36575=CARTESIAN_POINT('Ctrl Pts',(-23.4155357047346,20.3299738430851,-9.86544377773439));
#36576=CARTESIAN_POINT('Ctrl Pts',(-23.4626906719376,20.328346881503,-9.86828780846819));
#36577=CARTESIAN_POINT('Ctrl Pts',(-23.5176815465956,20.3276576394121,-9.87164146282653));
#36578=CARTESIAN_POINT('Ctrl Pts',(-23.5255008203747,20.3275880968017,-9.87211919510026));
#36579=CARTESIAN_POINT('Ctrl Pts',(-23.537453797147,20.327525295042,-9.87285083661871));
#36580=CARTESIAN_POINT('Ctrl Pts',(-23.5415874010033,20.3275115298879,-9.87310410183783));
#36581=CARTESIAN_POINT('Ctrl Pts',(-23.5490378281936,20.3275010537897,-9.8735610383569));
#36582=CARTESIAN_POINT('Ctrl Pts',(-23.5523546470086,20.3275015104671,-9.87376462044286));
#36583=CARTESIAN_POINT('Ctrl Pts',(-23.5594877326846,20.3275135044656,-9.8742027883526));
#36584=CARTESIAN_POINT('Ctrl Pts',(-23.5633039884165,20.327526700067,-9.87443742593883));
#36585=CARTESIAN_POINT('Ctrl Pts',(-23.5736362062145,20.3275807789736,-9.87507327412818));
#36586=CARTESIAN_POINT('Ctrl Pts',(-23.5801520566657,20.3276346456541,-9.87547489178656));
#36587=CARTESIAN_POINT('Ctrl Pts',(-23.6093342788254,20.327964408197,-9.87727645487755));
#36588=CARTESIAN_POINT('Ctrl Pts',(-23.6319970813382,20.3284596783319,-9.87868327024003));
#36589=CARTESIAN_POINT('Ctrl Pts',(-23.6670701360143,20.3295964534935,-9.88087286852073));
#36590=CARTESIAN_POINT('Ctrl Pts',(-23.6794853811566,20.3300707370793,-9.88165035446542));
#36591=CARTESIAN_POINT('Ctrl Pts',(-23.6972252015651,20.3308511841064,-9.88276477548147));
#36592=CARTESIAN_POINT('Ctrl Pts',(-23.7025523524905,20.3310987971587,-9.88309987888756));
#36593=CARTESIAN_POINT('Ctrl Pts',(-23.7097512048707,20.3314513185223,-9.88355333299904));
#36594=CARTESIAN_POINT('Ctrl Pts',(-23.7116234875956,20.3315446401281,-9.8836713236013));
#36595=CARTESIAN_POINT('Ctrl Pts',(-23.7198280824767,20.3319607647021,-9.88418861983742));
#36596=CARTESIAN_POINT('Ctrl Pts',(-23.7261594820091,20.3323006195582,-9.88458845294889));
#36597=CARTESIAN_POINT('Ctrl Pts',(-23.7393456647753,20.3330474553642,-9.88542251391946));
#36598=CARTESIAN_POINT('Ctrl Pts',(-23.7462002268581,20.3334576647911,-9.88585683928375));
#36599=CARTESIAN_POINT('Ctrl Pts',(-23.7568096402509,20.3341266185862,-9.88653025964454));
#36600=CARTESIAN_POINT('Ctrl Pts',(-23.7605654665859,20.3343700404819,-9.88676888475878));
#36601=CARTESIAN_POINT('Ctrl Pts',(-23.7737523594959,20.3352479069463,-9.88760751308457));
#36602=CARTESIAN_POINT('Ctrl Pts',(-23.7831809850994,20.3359172593937,-9.88820857613902));
#36603=CARTESIAN_POINT('Ctrl Pts',(-24.0719187312115,20.3576922755111,-9.9066596858067));
#36604=CARTESIAN_POINT('Ctrl Pts',(-24.3472515408912,20.4150792757007,-9.92568629299455));
#36605=CARTESIAN_POINT('Ctrl Pts',(-24.7633295307349,20.5602068282034,-9.95542712266374));
#36606=CARTESIAN_POINT('Ctrl Pts',(-24.9108788538933,20.6243955747775,-9.96615011634887));
#36607=CARTESIAN_POINT('Ctrl Pts',(-25.0624403420376,20.704287229215,-9.97693631001475));
#36608=CARTESIAN_POINT('Ctrl Pts',(-25.0718160400266,20.7092887912853,-9.97760253609404));
#36609=CARTESIAN_POINT('Ctrl Pts',(-25.0840281774851,20.7158812781397,-9.97846881598465));
#36610=CARTESIAN_POINT('Ctrl Pts',(-25.0868870473853,20.7174301758083,-9.97867150486809));
#36611=CARTESIAN_POINT('Ctrl Pts',(-25.0915487623728,20.7199649643391,-9.97900183002843));
#36612=CARTESIAN_POINT('Ctrl Pts',(-25.0933530083647,20.7209482526204,-9.97912963271979));
#36613=CARTESIAN_POINT('Ctrl Pts',(-25.0968107425152,20.7228369596891,-9.97937447178313));
#36614=CARTESIAN_POINT('Ctrl Pts',(-25.0984643716151,20.7237421009656,-9.97949152512684));
#36615=CARTESIAN_POINT('Ctrl Pts',(-25.1022591203435,20.7258235488114,-9.97976005206337));
#36616=CARTESIAN_POINT('Ctrl Pts',(-25.1043997023312,20.727000842125,-9.97991146194047));
#36617=CARTESIAN_POINT('Ctrl Pts',(-25.1111657035001,20.7307320849471,-9.98038984703385));
#36618=CARTESIAN_POINT('Ctrl Pts',(-25.1157862121243,20.733294992802,-9.98071624845048));
#36619=CARTESIAN_POINT('Ctrl Pts',(-25.1543543425834,20.7548122005366,-9.98343853891612));
#36620=CARTESIAN_POINT('Ctrl Pts',(-25.1879645355018,20.7743690707541,-9.98579638434052));
#36621=CARTESIAN_POINT('Ctrl Pts',(-25.2237875798539,20.796090760667,-9.98830280071763));
#36622=CARTESIAN_POINT('Ctrl Pts',(-25.2263586099929,20.7976546618934,-9.9884826494509));
#36623=CARTESIAN_POINT('Ctrl Pts',(-25.2305181845883,20.8001928285594,-9.98877356563378));
#36624=CARTESIAN_POINT('Ctrl Pts',(-25.2321080751696,20.8011648710305,-9.98888474797332));
#36625=CARTESIAN_POINT('Ctrl Pts',(-25.328339293603,20.8601143579881,-9.99561354959413));
#36626=CARTESIAN_POINT('Ctrl Pts',(-25.4199324553258,20.9229464103117,-10.0019768269906));
#36627=CARTESIAN_POINT('Ctrl Pts',(-25.5671900831203,21.0355730070908,-10.0124509496099));
#36628=CARTESIAN_POINT('Ctrl Pts',(-25.6246912956887,21.0827934296245,-10.0166087227454));
#36629=CARTESIAN_POINT('Ctrl Pts',(-25.8034326485388,21.240245449707,-10.0299189994371));
#36630=CARTESIAN_POINT('Ctrl Pts',(-25.9179173118541,21.3577397371085,-10.0390594299042));
#36631=CARTESIAN_POINT('Ctrl Pts',(-26.0747348527825,21.5453530286679,-10.0531902584915));
#36632=CARTESIAN_POINT('Ctrl Pts',(-26.1241530730788,21.6092044963813,-10.0579260128179));
#36633=CARTESIAN_POINT('Ctrl Pts',(-26.1949155845257,21.7080942925147,-10.06520144191));
#36634=CARTESIAN_POINT('Ctrl Pts',(-26.2180753396393,21.7417971487987,-10.0676710064229));
#36635=CARTESIAN_POINT('Ctrl Pts',(-26.2447238609835,21.7822032444536,-10.0706235045224));
#36636=CARTESIAN_POINT('Ctrl Pts',(-26.2488389391339,21.7884905084494,-10.0710826841287));
#36637=CARTESIAN_POINT('Ctrl Pts',(-26.2551299220064,21.7981760071205,-10.0717897108842));
#36638=CARTESIAN_POINT('Ctrl Pts',(-26.2573215149605,21.8015640619583,-10.0720369706387));
#36639=CARTESIAN_POINT('Ctrl Pts',(-26.2612996729755,21.8077394266714,-10.0724875370242));
#36640=CARTESIAN_POINT('Ctrl Pts',(-26.2630883194998,21.8105253945555,-10.0726907656131));
#36641=CARTESIAN_POINT('Ctrl Pts',(-26.2666968242171,21.8161650415384,-10.0731020817524));
#36642=CARTESIAN_POINT('Ctrl Pts',(-26.2685164860016,21.8190188408053,-10.0733101762752));
#36643=CARTESIAN_POINT('Ctrl Pts',(-26.2736927005022,21.8271650453788,-10.0739040697769));
#36644=CARTESIAN_POINT('Ctrl Pts',(-26.2770383020341,21.8324643607146,-10.0742902748534));
#36645=CARTESIAN_POINT('Ctrl Pts',(-26.2912617880296,21.8551401198139,-10.0759422882866));
#36646=CARTESIAN_POINT('Ctrl Pts',(-26.3019890038667,21.8726100821049,-10.0772136507182));
#36647=CARTESIAN_POINT('Ctrl Pts',(-26.4995866551252,22.2014050583506,-10.1011196089587));
#36648=CARTESIAN_POINT('Ctrl Pts',(-26.6326452279545,22.5419521747354,-10.1259601704792));
#36649=CARTESIAN_POINT('Ctrl Pts',(-26.732547040215,23.0248274841494,-10.159025998282));
#36650=CARTESIAN_POINT('Ctrl Pts',(-26.7511783079503,23.153827383647,-10.1676132462524));
#36651=CARTESIAN_POINT('Ctrl Pts',(-26.7626162805975,23.2916004492935,-10.1762937282554));
#36652=CARTESIAN_POINT('Ctrl Pts',(-26.7632493920115,23.2995875483942,-10.1767952067479));
#36653=CARTESIAN_POINT('Ctrl Pts',(-26.7640728546898,23.310492150462,-10.177477393871));
#36654=CARTESIAN_POINT('Ctrl Pts',(-26.7642890251168,23.3134075865963,-10.1776595414301));
#36655=CARTESIAN_POINT('Ctrl Pts',(-26.764644058261,23.3182858352149,-10.1779639120214));
#36656=CARTESIAN_POINT('Ctrl Pts',(-26.7647850903777,23.3202484805264,-10.1780862578335));
#36657=CARTESIAN_POINT('Ctrl Pts',(-26.765059292106,23.3241138710123,-10.1783269965325));
#36658=CARTESIAN_POINT('Ctrl Pts',(-26.7651925700087,23.3260166052245,-10.1784453953639));
#36659=CARTESIAN_POINT('Ctrl Pts',(-26.7654826872429,23.3302118771472,-10.178706220523));
#36660=CARTESIAN_POINT('Ctrl Pts',(-26.7656387642892,23.3325044705812,-10.1788486035922));
#36661=CARTESIAN_POINT('Ctrl Pts',(-26.7661753359414,23.3405124777155,-10.1793454276422));
#36662=CARTESIAN_POINT('Ctrl Pts',(-26.766543047716,23.3462287809585,-10.17969914965));
#36663=CARTESIAN_POINT('Ctrl Pts',(-26.7701038148466,23.4039864428252,-10.1832641191217));
#36664=CARTESIAN_POINT('Ctrl Pts',(-26.7720489639991,23.4561006919476,-10.1864065994673));
#36665=CARTESIAN_POINT('Ctrl Pts',(-26.7727859288459,23.5126316309057,-10.1897571632614));
#36666=CARTESIAN_POINT('Ctrl Pts',(-26.7728341783268,23.5170206328173,-10.1900169169239));
#36667=CARTESIAN_POINT('Ctrl Pts',(-26.7729151238169,23.5260647172103,-10.1905514123317));
#36668=CARTESIAN_POINT('Ctrl Pts',(-26.7729467005438,23.5307198017021,-10.1908261082017));
#36669=CARTESIAN_POINT('Ctrl Pts',(-26.772988734737,23.5398250691909,-10.1913626260476));
#36670=CARTESIAN_POINT('Ctrl Pts',(-26.7730000611601,23.5442752352923,-10.1916244815034));
#36671=CARTESIAN_POINT('Ctrl Pts',(-26.7730410078804,23.630688050694,-10.1967023026275));
#36672=CARTESIAN_POINT('Ctrl Pts',(-26.7699530515089,23.7126276716292,-10.2013978952144));
#36673=CARTESIAN_POINT('Ctrl Pts',(-26.7373615528694,24.1416612933297,-10.2257532562892));
#36674=CARTESIAN_POINT('Ctrl Pts',(-26.6548659564374,24.4823478884039,-10.2445976408222));
#36675=CARTESIAN_POINT('Ctrl Pts',(-26.5113575270721,24.8224192390291,-10.2669140183395));
#36676=CARTESIAN_POINT('Ctrl Pts',(-26.5030783615903,24.8415195496261,-10.2681787942277));
#36677=CARTESIAN_POINT('Ctrl Pts',(-26.4920515154291,24.8662981434579,-10.269834889117));
#36678=CARTESIAN_POINT('Ctrl Pts',(-26.4894712680562,24.8720507507399,-10.2702204513702));
#36679=CARTESIAN_POINT('Ctrl Pts',(-26.485476833354,24.8808867294941,-10.2708143537528));
#36680=CARTESIAN_POINT('Ctrl Pts',(-26.4840746205018,24.8839755241083,-10.2710222810232));
#36681=CARTESIAN_POINT('Ctrl Pts',(-26.4812944263676,24.8900741362478,-10.271433447829));
#36682=CARTESIAN_POINT('Ctrl Pts',(-26.4799166791037,24.8930840563509,-10.2716366790894));
#36683=CARTESIAN_POINT('Ctrl Pts',(-26.4768541329118,24.8997475548306,-10.2720872765549));
#36684=CARTESIAN_POINT('Ctrl Pts',(-26.4751671266824,24.9034001073525,-10.2723347188659));
#36685=CARTESIAN_POINT('Ctrl Pts',(-26.4703328160856,24.9138156357279,-10.2730416111586));
#36686=CARTESIAN_POINT('Ctrl Pts',(-26.4671688801472,24.9205708234068,-10.2735016369658));
#36687=CARTESIAN_POINT('Ctrl Pts',(-26.4469553181897,24.9633407388018,-10.2764242207016));
#36688=CARTESIAN_POINT('Ctrl Pts',(-26.4292630706707,24.9990463061302,-10.27890906874));
#36689=CARTESIAN_POINT('Ctrl Pts',(-26.3747472386604,25.1041234174917,-10.2863604748528));
#36690=CARTESIAN_POINT('Ctrl Pts',(-26.3360472482928,25.1724828424994,-10.2913920875343));
#36691=CARTESIAN_POINT('Ctrl Pts',(-26.215888854951,25.3677292585338,-10.3063138446229));
#36692=CARTESIAN_POINT('Ctrl Pts',(-26.1279844275276,25.4903887584476,-10.3164081400788));
#36693=CARTESIAN_POINT('Ctrl Pts',(-25.9631484643416,25.6893268042344,-10.3338711529497));
#36694=CARTESIAN_POINT('Ctrl Pts',(-25.8903565521599,25.768724801521,-10.3411804086497));
#36695=CARTESIAN_POINT('Ctrl Pts',(-25.749961845605,25.9072465457364,-10.3544182485395));
#36696=CARTESIAN_POINT('Ctrl Pts',(-25.6835959627367,25.9674802999819,-10.3603663577646));
#36697=CARTESIAN_POINT('Ctrl Pts',(-25.6134363757629,26.0260136571732,-10.3662814487804));
#36698=CARTESIAN_POINT('Ctrl Pts',(-25.6120699421875,26.0271517405184,-10.3663965121296));
#36699=CARTESIAN_POINT('Ctrl Pts',(-25.6090070836841,26.0296984615862,-10.3666541130383));
#36700=CARTESIAN_POINT('Ctrl Pts',(-25.6073101519687,26.0311064918299,-10.366796618075));
#36701=CARTESIAN_POINT('Ctrl Pts',(-25.6028073070069,26.0348349340807,-10.367174185893));
#36702=CARTESIAN_POINT('Ctrl Pts',(-25.5999988958438,26.0371523412579,-10.3674090856819));
#36703=CARTESIAN_POINT('Ctrl Pts',(-25.5658462902489,26.0652367781078,-10.3702584681927));
#36704=CARTESIAN_POINT('Ctrl Pts',(-25.5340202497699,26.0904159087824,-10.3728403131384));
#36705=CARTESIAN_POINT('Ctrl Pts',(-25.4975235686233,26.1181857371555,-10.3757112434972));
#36706=CARTESIAN_POINT('Ctrl Pts',(-25.4933138863965,26.121372523406,-10.3760410625589));
#36707=CARTESIAN_POINT('Ctrl Pts',(-25.4871152557348,26.1260410520835,-10.3765247419013));
#36708=CARTESIAN_POINT('Ctrl Pts',(-25.4851324256313,26.1275308460571,-10.3766791670963));
#36709=CARTESIAN_POINT('Ctrl Pts',(-25.4816347628029,26.1301524940222,-10.3769510466832));
#36710=CARTESIAN_POINT('Ctrl Pts',(-25.4801206522641,26.1312853047417,-10.3770685689229));
#36711=CARTESIAN_POINT('Ctrl Pts',(-25.4769727259063,26.13363616729,-10.3773125458114));
#36712=CARTESIAN_POINT('Ctrl Pts',(-25.4753387546854,26.1348539999197,-10.3774389849033));
#36713=CARTESIAN_POINT('Ctrl Pts',(-25.4711012710935,26.1380060366129,-10.3777663722579));
#36714=CARTESIAN_POINT('Ctrl Pts',(-25.4684959838848,26.1399378678344,-10.3779671530195));
#36715=CARTESIAN_POINT('Ctrl Pts',(-25.4574481158722,26.1481040883759,-10.3788164663138));
#36716=CARTESIAN_POINT('Ctrl Pts',(-25.4489779002112,26.1543012426461,-10.3794624134995));
#36717=CARTESIAN_POINT('Ctrl Pts',(-25.2999487995973,26.2622232533784,-10.3907394740924));
#36718=CARTESIAN_POINT('Ctrl Pts',(-25.1514079213656,26.3524913545503,-10.4006187100444));
#36719=CARTESIAN_POINT('Ctrl Pts',(-24.780799301934,26.5385663304335,-10.4239075562659));
#36720=CARTESIAN_POINT('Ctrl Pts',(-24.5538531419888,26.6222297956865,-10.4371691245691));
#36721=CARTESIAN_POINT('Ctrl Pts',(-24.2962005002622,26.6855778593387,-10.4526788413348));
#36722=CARTESIAN_POINT('Ctrl Pts',(-24.2726348731474,26.6910911127933,-10.4541006896964));
#36723=CARTESIAN_POINT('Ctrl Pts',(-24.242551413933,26.6977727601466,-10.4559210691844));
#36724=CARTESIAN_POINT('Ctrl Pts',(-24.2360886580852,26.6991872940708,-10.4563124449478));
#36725=CARTESIAN_POINT('Ctrl Pts',(-24.2256234156549,26.7014441254717,-10.4569467304876));
#36726=CARTESIAN_POINT('Ctrl Pts',(-24.2216235811078,26.7022987251038,-10.457189279381));
#36727=CARTESIAN_POINT('Ctrl Pts',(-24.2143451124789,26.703839350972,-10.4576308756856));
#36728=CARTESIAN_POINT('Ctrl Pts',(-24.2110670109104,26.7045278853237,-10.4578298488174));
#36729=CARTESIAN_POINT('Ctrl Pts',(-24.1560273364177,26.7159988846331,-10.4611720969003));
#36730=CARTESIAN_POINT('Ctrl Pts',(-24.1040116901775,26.7255105338787,-10.4643526991278));
#36731=CARTESIAN_POINT('Ctrl Pts',(-24.0431651257261,26.7350964734748,-10.4681064801058));
#36732=CARTESIAN_POINT('Ctrl Pts',(-24.0345370083894,26.7364198691269,-10.4686395390466));
#36733=CARTESIAN_POINT('Ctrl Pts',(-24.0216632658515,26.73834096582,-10.4694360791374));
#36734=CARTESIAN_POINT('Ctrl Pts',(-24.0174216022654,26.738965281897,-10.469698715282));
#36735=CARTESIAN_POINT('Ctrl Pts',(-24.0098511282861,26.7400641246684,-10.4701678101567));
#36736=CARTESIAN_POINT('Ctrl Pts',(-24.006522791117,26.7405419102447,-10.4703741652009));
#36737=CARTESIAN_POINT('Ctrl Pts',(-23.9995755093569,26.7415281041753,-10.4708051432333));
#36738=CARTESIAN_POINT('Ctrl Pts',(-23.9959564373302,26.7420355672553,-10.4710297958756));
#36739=CARTESIAN_POINT('Ctrl Pts',(-23.986470531573,26.7433492243799,-10.4716190054387));
#36740=CARTESIAN_POINT('Ctrl Pts',(-23.9806023449593,26.7441454024292,-10.4719838791925));
#36741=CARTESIAN_POINT('Ctrl Pts',(-23.9677795161654,26.7458491849888,-10.4727820148168));
#36742=CARTESIAN_POINT('Ctrl Pts',(-23.9608240514467,26.7467502681596,-10.4732154816285));
#36743=CARTESIAN_POINT('Ctrl Pts',(-23.9404519885845,26.7493218873508,-10.4744866697063));
#36744=CARTESIAN_POINT('Ctrl Pts',(-23.9270278780822,26.7509306923079,-10.4753263390749));
#36745=CARTESIAN_POINT('Ctrl Pts',(-23.7889539270268,26.7665974159093,-10.4839841655148));
#36746=CARTESIAN_POINT('Ctrl Pts',(-23.6636100162066,26.773449074996,-10.4920293276984));
#36747=CARTESIAN_POINT('Ctrl Pts',(-23.2541100671017,26.771917391328,-10.5189258715085));
#36748=CARTESIAN_POINT('Ctrl Pts',(-22.9714529131186,26.7332992108208,-10.5385757582083));
#36749=CARTESIAN_POINT('Ctrl Pts',(-22.6146964474554,26.6354156880464,-10.5630026097525));
#36750=CARTESIAN_POINT('Ctrl Pts',(-22.5327877612221,26.6093807480631,-10.5685711418652));
#36751=CARTESIAN_POINT('Ctrl Pts',(-22.4460429320873,26.5779379513891,-10.574354953665));
#36752=CARTESIAN_POINT('Ctrl Pts',(-22.4400826561104,26.575757562176,-10.5747517737126));
#36753=CARTESIAN_POINT('Ctrl Pts',(-22.4318148335707,26.572705304213,-10.5753013677805));
#36754=CARTESIAN_POINT('Ctrl Pts',(-22.4295018392485,26.5718483902055,-10.5754550281635));
#36755=CARTESIAN_POINT('Ctrl Pts',(-22.4255242221584,26.5703695741141,-10.5757191119432));
#36756=CARTESIAN_POINT('Ctrl Pts',(-22.4238591303581,26.5697489509085,-10.5758296121771));
#36757=CARTESIAN_POINT('Ctrl Pts',(-22.4204170534887,26.5684627555401,-10.5760579349384));
#36758=CARTESIAN_POINT('Ctrl Pts',(-22.4186401461027,26.5677969923327,-10.5761757451013));
#36759=CARTESIAN_POINT('Ctrl Pts',(-22.4144636335321,26.566227948588,-10.576452518254));
#36760=CARTESIAN_POINT('Ctrl Pts',(-22.4120645099564,26.5653233706262,-10.5766114028691));
#36761=CARTESIAN_POINT('Ctrl Pts',(-22.4042511253066,26.5623667168061,-10.5771285256818));
#36762=CARTESIAN_POINT('Ctrl Pts',(-22.3988412746458,26.5603028977132,-10.5774860600588));
#36763=CARTESIAN_POINT('Ctrl Pts',(-22.2847648255116,26.5164310086626,-10.5850150796031));
#36764=CARTESIAN_POINT('Ctrl Pts',(-22.1784769288177,26.4687942336566,-10.5918347265396));
#36765=CARTESIAN_POINT('Ctrl Pts',(-22.075035905646,26.4155367180763,-10.5984952470527));
#36766=CARTESIAN_POINT('',(-26.7730018644027,23.5481786398916,-10.4357734492733));
#36767=CARTESIAN_POINT('Ctrl Pts',(-22.0750360250409,26.4155367795477,-10.8457129588805));
#36768=CARTESIAN_POINT('Ctrl Pts',(-22.1186364234956,26.4379848237672,-10.8425789699142));
#36769=CARTESIAN_POINT('Ctrl Pts',(-22.1627450527255,26.459435550147,-10.8394118105694));
#36770=CARTESIAN_POINT('Ctrl Pts',(-22.3068659884537,26.5254999520909,-10.8290756717199));
#36771=CARTESIAN_POINT('Ctrl Pts',(-22.4086571099247,26.5660217169583,-10.8217910895913));
#36772=CARTESIAN_POINT('Ctrl Pts',(-22.7472610985681,26.6812133045392,-10.7977341548963));
#36773=CARTESIAN_POINT('Ctrl Pts',(-22.9906690033895,26.7337392538618,-10.780649362133));
#36774=CARTESIAN_POINT('Ctrl Pts',(-23.2722114397519,26.7611734344379,-10.7624927365297));
#36775=CARTESIAN_POINT('Ctrl Pts',(-23.306776414413,26.7639792649023,-10.7602921210766));
#36776=CARTESIAN_POINT('Ctrl Pts',(-23.3459741781228,26.7665250787828,-10.7578338329385));
#36777=CARTESIAN_POINT('Ctrl Pts',(-23.3505673859086,26.7668135191576,-10.7575463490808));
#36778=CARTESIAN_POINT('Ctrl Pts',(-23.3575236717974,26.7672353962311,-10.757111855883));
#36779=CARTESIAN_POINT('Ctrl Pts',(-23.3598862804473,26.7673760690542,-10.7569644420961));
#36780=CARTESIAN_POINT('Ctrl Pts',(-23.3639972328375,26.7676162961331,-10.7567082151541));
#36781=CARTESIAN_POINT('Ctrl Pts',(-23.3657455025255,26.7677170280482,-10.7565993353797));
#36782=CARTESIAN_POINT('Ctrl Pts',(-23.3694076571209,26.7679250396233,-10.7563714432651));
#36783=CARTESIAN_POINT('Ctrl Pts',(-23.3713215547332,26.7680320366399,-10.7562524474683));
#36784=CARTESIAN_POINT('Ctrl Pts',(-23.3759037720577,26.7682841060366,-10.7559677968425));
#36785=CARTESIAN_POINT('Ctrl Pts',(-23.3785721869316,26.7684275677663,-10.7558022333426));
#36786=CARTESIAN_POINT('Ctrl Pts',(-23.3876383268769,26.768903681518,-10.7552403901871));
#36787=CARTESIAN_POINT('Ctrl Pts',(-23.3940369175444,26.7692205786672,-10.7548449948147));
#36788=CARTESIAN_POINT('Ctrl Pts',(-23.4092588850723,26.7699289684798,-10.7539069769913));
#36789=CARTESIAN_POINT('Ctrl Pts',(-23.4180830636382,26.7703032769285,-10.7533652933066));
#36790=CARTESIAN_POINT('Ctrl Pts',(-23.522475620302,26.7743016043603,-10.7469805105668));
#36791=CARTESIAN_POINT('Ctrl Pts',(-23.6181685134833,26.7737064700194,-10.7413602200678));
#36792=CARTESIAN_POINT('Ctrl Pts',(-23.7934804061028,26.764803614745,-10.7312622507125));
#36793=CARTESIAN_POINT('Ctrl Pts',(-23.873083375536,26.7577873743404,-10.7267525480799));
#36794=CARTESIAN_POINT('Ctrl Pts',(-23.9754114797162,26.7449196264872,-10.7209664070455));
#36795=CARTESIAN_POINT('Ctrl Pts',(-23.9984447124259,26.7417696876728,-10.7196647600313));
#36796=CARTESIAN_POINT('Ctrl Pts',(-24.0413981973451,26.7354213574736,-10.7172359457595));
#36797=CARTESIAN_POINT('Ctrl Pts',(-24.0613263473817,26.7322845980414,-10.7161085233793));
#36798=CARTESIAN_POINT('Ctrl Pts',(-24.098747839914,26.7260337145355,-10.7139885111132));
#36799=CARTESIAN_POINT('Ctrl Pts',(-24.1162474076649,26.7229616303184,-10.7129959172454));
#36800=CARTESIAN_POINT('Ctrl Pts',(-24.2950407083182,26.6900477820063,-10.7028357101551));
#36801=CARTESIAN_POINT('Ctrl Pts',(-24.453849231696,26.648079322576,-10.6936379361411));
#36802=CARTESIAN_POINT('Ctrl Pts',(-24.7021016010934,26.5617516392709,-10.6783386398349));
#36803=CARTESIAN_POINT('Ctrl Pts',(-24.7938894798,26.5250209711235,-10.6724715911893));
#36804=CARTESIAN_POINT('Ctrl Pts',(-24.8923505303703,26.4802658324181,-10.6658884371132));
#36805=CARTESIAN_POINT('Ctrl Pts',(-24.9008452840558,26.4763598767592,-10.6653180783301));
#36806=CARTESIAN_POINT('Ctrl Pts',(-24.9134264794258,26.4705084850461,-10.6644697404444));
#36807=CARTESIAN_POINT('Ctrl Pts',(-24.9175260666033,26.4685912929176,-10.6641927388863));
#36808=CARTESIAN_POINT('Ctrl Pts',(-24.9245343095529,26.4652958448211,-10.663718222566));
#36809=CARTESIAN_POINT('Ctrl Pts',(-24.9274449723851,26.463921851221,-10.6635208558686));
#36810=CARTESIAN_POINT('Ctrl Pts',(-24.9332787603214,26.4611572865424,-10.6631246919534));
#36811=CARTESIAN_POINT('Ctrl Pts',(-24.9362018578121,26.4597666674534,-10.6629258932666));
#36812=CARTESIAN_POINT('Ctrl Pts',(-24.9420750918104,26.4569617065763,-10.6625258603448));
#36813=CARTESIAN_POINT('Ctrl Pts',(-24.9450251792501,26.4555472719393,-10.6623246230632));
#36814=CARTESIAN_POINT('Ctrl Pts',(-24.9544155445809,26.4510274138008,-10.6616830983064));
#36815=CARTESIAN_POINT('Ctrl Pts',(-24.9608476107363,26.4479050652257,-10.6612422206946));
#36816=CARTESIAN_POINT('Ctrl Pts',(-24.9985386008922,26.4294533125468,-10.658650119938));
#36817=CARTESIAN_POINT('Ctrl Pts',(-25.0295568576001,26.413640076657,-10.6564819985231));
#36818=CARTESIAN_POINT('Ctrl Pts',(-25.1188597197917,26.3662747614309,-10.6501349854303));
#36819=CARTESIAN_POINT('Ctrl Pts',(-25.1764319868637,26.3334250120501,-10.6459107400589));
#36820=CARTESIAN_POINT('Ctrl Pts',(-25.2934901246181,26.2617612341691,-10.6370394978176));
#36821=CARTESIAN_POINT('Ctrl Pts',(-25.3527879726953,26.2227086367218,-10.632386173533));
#36822=CARTESIAN_POINT('Ctrl Pts',(-25.6656754720295,26.0014928519467,-10.6069852620368));
#36823=CARTESIAN_POINT('Ctrl Pts',(-25.8930407898517,25.7851847057837,-10.5852195151103));
#36824=CARTESIAN_POINT('Ctrl Pts',(-26.0890263970071,25.5353905786491,-10.5648825610526));
#36825=CARTESIAN_POINT('Ctrl Pts',(-26.0922964742507,25.5312013951432,-10.5645427587257));
#36826=CARTESIAN_POINT('Ctrl Pts',(-26.0985817249438,25.5231083844709,-10.5638887549967));
#36827=CARTESIAN_POINT('Ctrl Pts',(-26.1015983258644,25.5192056881396,-10.5635744689783));
#36828=CARTESIAN_POINT('Ctrl Pts',(-26.1099636351831,25.5083316507855,-10.5627018519501));
#36829=CARTESIAN_POINT('Ctrl Pts',(-26.1152928585734,25.5013452756132,-10.5621447123836));
#36830=CARTESIAN_POINT('Ctrl Pts',(-26.1293971596473,25.4826974947723,-10.5606670972836));
#36831=CARTESIAN_POINT('Ctrl Pts',(-26.1381218446569,25.4709979561346,-10.5597498465658));
#36832=CARTESIAN_POINT('Ctrl Pts',(-26.1490105679224,25.4561876245415,-10.5586014133792));
#36833=CARTESIAN_POINT('Ctrl Pts',(-26.1512488204985,25.4531319853079,-10.5583651468825));
#36834=CARTESIAN_POINT('Ctrl Pts',(-26.1547681522083,25.4483096191727,-10.5579933480443));
#36835=CARTESIAN_POINT('Ctrl Pts',(-26.1560528237101,25.4465455372783,-10.557857565181));
#36836=CARTESIAN_POINT('Ctrl Pts',(-26.15842118067,25.443286411606,-10.5576071262134));
#36837=CARTESIAN_POINT('Ctrl Pts',(-26.159505366674,25.4417917502084,-10.557492435334));
#36838=CARTESIAN_POINT('Ctrl Pts',(-26.1619209631023,25.4384555744418,-10.5572367998868));
#36839=CARTESIAN_POINT('Ctrl Pts',(-26.163251707542,25.4366135876298,-10.5570959022119));
#36840=CARTESIAN_POINT('Ctrl Pts',(-26.1670993885261,25.4312758291826,-10.5566883094799));
#36841=CARTESIAN_POINT('Ctrl Pts',(-26.1696112784083,25.4277763995399,-10.5564219653913));
#36842=CARTESIAN_POINT('Ctrl Pts',(-26.1867681528064,25.4037729205623,-10.5546009379943));
#36843=CARTESIAN_POINT('Ctrl Pts',(-26.2011797800713,25.3831020265392,-10.553062140381));
#36844=CARTESIAN_POINT('Ctrl Pts',(-26.2448215143331,25.3189140094615,-10.548366544238));
#36845=CARTESIAN_POINT('Ctrl Pts',(-26.2732348019774,25.2748491961707,-10.5452583038612));
#36846=CARTESIAN_POINT('Ctrl Pts',(-26.4619042194894,24.9659540271525,-10.5241108139773));
#36847=CARTESIAN_POINT('Ctrl Pts',(-26.5843616713091,24.6799193791891,-10.507565278112));
#36848=CARTESIAN_POINT('Ctrl Pts',(-26.669002553184,24.3625769289211,-10.4886402584093));
#36849=CARTESIAN_POINT('Ctrl Pts',(-26.6736987403518,24.3443283387611,-10.4875507373793));
#36850=CARTESIAN_POINT('Ctrl Pts',(-26.6842475491618,24.3017954376839,-10.4850073101816));
#36851=CARTESIAN_POINT('Ctrl Pts',(-26.6899783460662,24.2774823962192,-10.4835503734112));
#36852=CARTESIAN_POINT('Ctrl Pts',(-26.6991928383443,24.2362487785721,-10.4810726185537));
#36853=CARTESIAN_POINT('Ctrl Pts',(-26.7028242113375,24.2193621600604,-10.4800559565639));
#36854=CARTESIAN_POINT('Ctrl Pts',(-26.7073655540932,24.1973859325922,-10.4787299657776));
#36855=CARTESIAN_POINT('Ctrl Pts',(-26.708399310886,24.1923219947657,-10.4784242205001));
#36856=CARTESIAN_POINT('Ctrl Pts',(-26.7102151843335,24.1833163084684,-10.4778801154029));
#36857=CARTESIAN_POINT('Ctrl Pts',(-26.7110021197231,24.1793755348572,-10.4776418965239));
#36858=CARTESIAN_POINT('Ctrl Pts',(-26.7126666403108,24.170958081026,-10.4771327880346));
#36859=CARTESIAN_POINT('Ctrl Pts',(-26.71354209437,24.1664809923417,-10.4768618365091));
#36860=CARTESIAN_POINT('Ctrl Pts',(-26.7157368383524,24.1551291060743,-10.4761743914436));
#36861=CARTESIAN_POINT('Ctrl Pts',(-26.7170432357442,24.1482518641046,-10.4757575181272));
#36862=CARTESIAN_POINT('Ctrl Pts',(-26.7186244927516,24.1397771756368,-10.4752432958245));
#36863=CARTESIAN_POINT('Ctrl Pts',(-26.7189205745393,24.138183670237,-10.4751465835001));
#36864=CARTESIAN_POINT('Ctrl Pts',(-26.7214629390903,24.1244430171188,-10.4743124459254));
#36865=CARTESIAN_POINT('Ctrl Pts',(-26.7236405419754,24.112283395142,-10.4735729655562));
#36866=CARTESIAN_POINT('Ctrl Pts',(-26.7278395703761,24.0880335551028,-10.4720954160416));
#36867=CARTESIAN_POINT('Ctrl Pts',(-26.7298620325906,24.0759437272445,-10.4713573922601));
#36868=CARTESIAN_POINT('Ctrl Pts',(-26.7354777387432,24.0411558345171,-10.469229545288));
#36869=CARTESIAN_POINT('Ctrl Pts',(-26.738897181758,24.0184308369839,-10.4678343817444));
#36870=CARTESIAN_POINT('Ctrl Pts',(-26.74296793344,23.9892603127437,-10.4660362987347));
#36871=CARTESIAN_POINT('Ctrl Pts',(-26.7438433132651,23.9828463218323,-10.4656404926972));
#36872=CARTESIAN_POINT('Ctrl Pts',(-26.7452077396333,23.9726191509497,-10.465008652282));
#36873=CARTESIAN_POINT('Ctrl Pts',(-26.7457093014396,23.9688076347377,-10.4647730145555));
#36874=CARTESIAN_POINT('Ctrl Pts',(-26.7466327308141,23.9616918122765,-10.4643327939177));
#36875=CARTESIAN_POINT('Ctrl Pts',(-26.7470562979422,23.9583877285369,-10.4641282651092));
#36876=CARTESIAN_POINT('Ctrl Pts',(-26.7478779461743,23.9518986123362,-10.4637263360939));
#36877=CARTESIAN_POINT('Ctrl Pts',(-26.748276393221,23.9487136294325,-10.4635289477265));
#36878=CARTESIAN_POINT('Ctrl Pts',(-26.7491615030231,23.9415516614389,-10.4630848286318));
#36879=CARTESIAN_POINT('Ctrl Pts',(-26.7496455081749,23.937574358605,-10.4628380140951));
#36880=CARTESIAN_POINT('Ctrl Pts',(-26.7508429064305,23.9275793625489,-10.4622173127949));
#36881=CARTESIAN_POINT('Ctrl Pts',(-26.7515467437073,23.9215605594346,-10.4618431243511));
#36882=CARTESIAN_POINT('Ctrl Pts',(-26.752860338551,23.9100460454496,-10.4611264656767));
#36883=CARTESIAN_POINT('Ctrl Pts',(-26.7534729365567,23.9045506749863,-10.4607840868392));
#36884=CARTESIAN_POINT('Ctrl Pts',(-26.7667647450157,23.7824623899342,-10.4531697521634));
#36885=CARTESIAN_POINT('Ctrl Pts',(-26.7730826164252,23.665281353586,-10.4456974470109));
#36886=CARTESIAN_POINT('Ctrl Pts',(-26.773001765511,23.5480302730957,-10.4380474642037));
#36887=CARTESIAN_POINT('Ctrl Pts',(-26.7730018644027,23.5481786398916,-10.4357734492733));
#36888=CARTESIAN_POINT('Ctrl Pts',(-26.7729292341586,23.4353139908667,-10.4288341238586));
#36889=CARTESIAN_POINT('Ctrl Pts',(-26.7669235627087,23.3226754865815,-10.421894798444));
#36890=CARTESIAN_POINT('Ctrl Pts',(-26.755080179162,23.2108452357707,-10.4149554730293));
#36891=CARTESIAN_POINT('Ctrl Pts',(-26.7431850598284,23.0985264737172,-10.4079858343635));
#36892=CARTESIAN_POINT('Ctrl Pts',(-26.7254012379132,22.9870232448594,-10.4010161956977));
#36893=CARTESIAN_POINT('Ctrl Pts',(-26.7018749653354,22.8769074505733,-10.3940465570318));
#36894=CARTESIAN_POINT('Ctrl Pts',(-26.6782170628028,22.7661755562667,-10.3870379231015));
#36895=CARTESIAN_POINT('Ctrl Pts',(-26.6487523832634,22.6568468639344,-10.3800292891711));
#36896=CARTESIAN_POINT('Ctrl Pts',(-26.6136780058931,22.5494818653927,-10.3730206552408));
#36897=CARTESIAN_POINT('Ctrl Pts',(-26.5948831962548,22.4919497048615,-10.3692650378807));
#36898=CARTESIAN_POINT('Ctrl Pts',(-26.5744784225793,22.4349810255353,-10.3655094205207));
#36899=CARTESIAN_POINT('Ctrl Pts',(-26.5524995027409,22.3786593056378,-10.3617538031606));
#36900=CARTESIAN_POINT('Ctrl Pts',(-26.5163787036329,22.2860985453826,-10.3555817118483));
#36901=CARTESIAN_POINT('Ctrl Pts',(-26.4759097362695,22.1950467644762,-10.349409620536));
#36902=CARTESIAN_POINT('Ctrl Pts',(-26.4312391033891,22.1059416454188,-10.3432375292236));
#36903=CARTESIAN_POINT('Ctrl Pts',(-26.3866289948,22.0169572549884,-10.3370738004848));
#36904=CARTESIAN_POINT('Ctrl Pts',(-26.3378287287879,21.9299146689386,-10.330910071746));
#36905=CARTESIAN_POINT('Ctrl Pts',(-26.2850334753614,21.8452332494998,-10.3247463430072));
#36906=CARTESIAN_POINT('Ctrl Pts',(-26.2322941535509,21.7606415420773,-10.3185891441606));
#36907=CARTESIAN_POINT('Ctrl Pts',(-26.1755684871054,21.6784063947794,-10.3124319453139));
#36908=CARTESIAN_POINT('Ctrl Pts',(-26.1150978754791,21.5989232604114,-10.3062747464672));
#36909=CARTESIAN_POINT('Ctrl Pts',(-26.0546714642027,21.5194982233945,-10.3001220481595));
#36910=CARTESIAN_POINT('Ctrl Pts',(-25.990505812244,21.4428215446761,-10.2939693498518));
#36911=CARTESIAN_POINT('Ctrl Pts',(-25.9228854899555,21.3692595450314,-10.2878166515441));
#36912=CARTESIAN_POINT('Ctrl Pts',(-25.8552908093894,21.2957254402017,-10.2816662863483));
#36913=CARTESIAN_POINT('Ctrl Pts',(-25.7842443551357,21.2253039870875,-10.2755159211526));
#36914=CARTESIAN_POINT('Ctrl Pts',(-25.7100702408391,21.1583275692917,-10.2693655559568));
#36915=CARTESIAN_POINT('Ctrl Pts',(-25.6359044097136,21.091358630886,-10.2632158775846));
#36916=CARTESIAN_POINT('Ctrl Pts',(-25.5586119353587,21.0278342540622,-10.2570661992124));
#36917=CARTESIAN_POINT('Ctrl Pts',(-25.4785522209244,20.9680484593918,-10.2509165208402));
#36918=CARTESIAN_POINT('Ctrl Pts',(-25.3984800287558,20.908253346786,-10.2447658840077));
#36919=CARTESIAN_POINT('Ctrl Pts',(-25.3156400879515,20.8521982336258,-10.2386152471753));
#36920=CARTESIAN_POINT('Ctrl Pts',(-25.2304223334371,20.8001348978808,-10.2324646103428));
#36921=CARTESIAN_POINT('Ctrl Pts',(-25.1451134138266,20.7480158653033,-10.226307393621));
#36922=CARTESIAN_POINT('Ctrl Pts',(-25.0574219722847,20.6998973645516,-10.2201501768992));
#36923=CARTESIAN_POINT('Ctrl Pts',(-24.9677640970661,20.6559860400703,-10.2139929601774));
#36924=CARTESIAN_POINT('Ctrl Pts',(-24.8780562020862,20.612050217641,-10.2078323083696));
#36925=CARTESIAN_POINT('Ctrl Pts',(-24.7863800872479,20.5723264185468,-10.2016716565618));
#36926=CARTESIAN_POINT('Ctrl Pts',(-24.6931715070611,20.5369729598247,-10.195511004754));
#36927=CARTESIAN_POINT('Ctrl Pts',(-24.5998069557743,20.5015603421942,-10.1893400439849));
#36928=CARTESIAN_POINT('Ctrl Pts',(-24.5049052299846,20.4705328078024,-10.1831690832159));
#36929=CARTESIAN_POINT('Ctrl Pts',(-24.4089170475075,20.4439987088743,-10.1769981224469));
#36930=CARTESIAN_POINT('Ctrl Pts',(-24.3356474655575,20.4237447329607,-10.1722877122265));
#36931=CARTESIAN_POINT('Ctrl Pts',(-24.2617451641514,20.4061078490576,-10.1675773020061));
#36932=CARTESIAN_POINT('Ctrl Pts',(-24.187413255466,20.3911159764655,-10.1628668917857));
#36933=CARTESIAN_POINT('Ctrl Pts',(-24.0900155116688,20.3714719959516,-10.1566948004734));
#36934=CARTESIAN_POINT('Ctrl Pts',(-23.9915369282417,20.3563018696539,-10.1505227091611));
#36935=CARTESIAN_POINT('Ctrl Pts',(-23.8924249257566,20.3457189283064,-10.1443506178487));
#36936=CARTESIAN_POINT('Ctrl Pts',(-23.7934472102364,20.3351503257982,-10.1381868891099));
#36937=CARTESIAN_POINT('Ctrl Pts',(-23.6938382096012,20.32915660062,-10.1320231603712));
#36938=CARTESIAN_POINT('Ctrl Pts',(-23.594056237995,20.3278002360327,-10.1258594316324));
#36939=CARTESIAN_POINT('Ctrl Pts',(-23.4943799760226,20.3264453083863,-10.1197022327857));
#36940=CARTESIAN_POINT('Ctrl Pts',(-23.3945315393536,20.3297179800143,-10.113545033939));
#36941=CARTESIAN_POINT('Ctrl Pts',(-23.2949741157067,20.3376289165113,-10.1073878350923));
#36942=CARTESIAN_POINT('Ctrl Pts',(-23.1954894624993,20.3455340705934,-10.1012351367846));
#36943=CARTESIAN_POINT('Ctrl Pts',(-23.0962958311345,20.358070714771,-10.0950824384769));
#36944=CARTESIAN_POINT('Ctrl Pts',(-22.9978552357661,20.3751974471403,-10.0889297401692));
#36945=CARTESIAN_POINT('Ctrl Pts',(-22.8994519692116,20.3923176850284,-10.0827793749734));
#36946=CARTESIAN_POINT('Ctrl Pts',(-22.801801598761,20.4140244782415,-10.0766290097777));
#36947=CARTESIAN_POINT('Ctrl Pts',(-22.7053589614813,20.4402248119604,-10.0704786445819));
#36948=CARTESIAN_POINT('Ctrl Pts',(-22.6089270941431,20.4664222198357,-10.0643289662097));
#36949=CARTESIAN_POINT('Ctrl Pts',(-22.5137031110442,20.49711205668,-10.0581792878375));
#36950=CARTESIAN_POINT('Ctrl Pts',(-22.4201286492632,20.5321508811763,-10.0520296094653));
#36951=CARTESIAN_POINT('Ctrl Pts',(-22.3265396034023,20.5671951666606,-10.0458789726328));
#36952=CARTESIAN_POINT('Ctrl Pts',(-22.2346009963549,20.6065896337603,-10.0397283358004));
#36953=CARTESIAN_POINT('Ctrl Pts',(-22.1447354295089,20.6501423203463,-10.0335776989679));
#36954=CARTESIAN_POINT('Ctrl Pts',(-22.0547737253841,20.6937415991579,-10.0274204822461));
#36955=CARTESIAN_POINT('Ctrl Pts',(-21.9668898817002,20.7415077906915,-10.0212632655243));
#36956=CARTESIAN_POINT('Ctrl Pts',(-21.8814826652363,20.7932025329996,-10.0151060488025));
#36957=CARTESIAN_POINT('Ctrl Pts',(-21.7960278004361,20.8449261155927,-10.0089453969947));
#36958=CARTESIAN_POINT('Ctrl Pts',(-21.713052675266,20.900582371749,-10.0027847451869));
#36959=CARTESIAN_POINT('Ctrl Pts',(-21.6329260282908,20.9598902709579,-9.99662409337905));
#36960=CARTESIAN_POINT('Ctrl Pts',(-21.5526653009419,21.0192974133723,-9.99045313261002));
#36961=CARTESIAN_POINT('Ctrl Pts',(-21.4752629097114,21.0823681298745,-9.98428217184101));
#36962=CARTESIAN_POINT('Ctrl Pts',(-21.4010536452309,21.1487817929749,-9.97811121107198));
#36963=CARTESIAN_POINT('Ctrl Pts',(-21.3444083203067,21.1994765889962,-9.9734008008516));
#36964=CARTESIAN_POINT('Ctrl Pts',(-21.2896227871122,21.2521183516899,-9.96869039063121));
#36965=CARTESIAN_POINT('Ctrl Pts',(-21.2368303253655,21.3065512909393,-9.96397998041083));
#36966=CARTESIAN_POINT('Ctrl Pts',(-21.1676559054618,21.3778752427241,-9.9578078890985));
#36967=CARTESIAN_POINT('Ctrl Pts',(-21.1016611745336,21.4525268308881,-9.95163579778617));
#36968=CARTESIAN_POINT('Ctrl Pts',(-21.0391833294155,21.5301908930634,-9.94546370647384));
#36969=CARTESIAN_POINT('Ctrl Pts',(-20.9767901356009,21.6077497281126,-9.93929997773506));
#36970=CARTESIAN_POINT('Ctrl Pts',(-20.9179046264757,21.6883125890606,-9.93313624899627));
#36971=CARTESIAN_POINT('Ctrl Pts',(-20.8628271084798,21.7715276633796,-9.92697252025748));
#36972=CARTESIAN_POINT('Ctrl Pts',(-20.8078079399448,21.8546545791375,-9.9208153214108));
#36973=CARTESIAN_POINT('Ctrl Pts',(-20.7565889806,21.9404277619421,-9.91465812256414));
#36974=CARTESIAN_POINT('Ctrl Pts',(-20.7094295761867,22.0284632894002,-9.90850092371745));
#36975=CARTESIAN_POINT('Ctrl Pts',(-20.6623046424382,22.1164344682264,-9.90234822540975));
#36976=CARTESIAN_POINT('Ctrl Pts',(-20.6192335686585,22.2066643222329,-9.896195527102));
#36977=CARTESIAN_POINT('Ctrl Pts',(-20.5804312609677,22.2987417716763,-9.89004282879429));
#36978=CARTESIAN_POINT('Ctrl Pts',(-20.5416436671672,22.3907843052198,-9.88389246359854));
#36979=CARTESIAN_POINT('Ctrl Pts',(-20.5071217915778,22.4846726422299,-9.87774209840284));
#36980=CARTESIAN_POINT('Ctrl Pts',(-20.4770332379878,22.5799738421977,-9.87159173320708));
#36981=CARTESIAN_POINT('Ctrl Pts',(-20.4469480444467,22.6752643996906,-9.86544205483487));
#36982=CARTESIAN_POINT('Ctrl Pts',(-20.4212953194093,22.7719670922121,-9.85929237646264));
#36983=CARTESIAN_POINT('Ctrl Pts',(-20.4001931068524,22.8696328269653,-9.85314269809042));
#36984=CARTESIAN_POINT('Ctrl Pts',(-20.3790876054029,22.9673137834452,-9.84699206125797));
#36985=CARTESIAN_POINT('Ctrl Pts',(-20.3625341168807,23.0659576556402,-9.84084142442551));
#36986=CARTESIAN_POINT('Ctrl Pts',(-20.3505995742911,23.1651051382437,-9.83469078759306));
#36987=CARTESIAN_POINT('Ctrl Pts',(-20.3386522642481,23.2643586878258,-9.82853357087125));
#36988=CARTESIAN_POINT('Ctrl Pts',(-20.3313338194465,23.3641164915305,-9.82237635414945));
#36989=CARTESIAN_POINT('Ctrl Pts',(-20.3286592523298,23.4639142154381,-9.81621913742764));
#36990=CARTESIAN_POINT('Ctrl Pts',(-20.325983193083,23.5637676160871,-9.81005848561984));
#36991=CARTESIAN_POINT('Ctrl Pts',(-20.327956162482,23.6636605469585,-9.80389783381202));
#36992=CARTESIAN_POINT('Ctrl Pts',(-20.3345410436693,23.7631308732061,-9.79773718200421));
#36993=CARTESIAN_POINT('Ctrl Pts',(-20.3411369437044,23.8627676486816,-9.79156622123518));
#36994=CARTESIAN_POINT('Ctrl Pts',(-20.3523601219335,23.9619799751271,-9.78539526046612));
#36995=CARTESIAN_POINT('Ctrl Pts',(-20.3681217975989,24.0603128748168,-9.77922429969709));
#36996=CARTESIAN_POINT('Ctrl Pts',(-20.3801529805741,24.1353722234393,-9.7745138894767));
#36997=CARTESIAN_POINT('Ctrl Pts',(-20.3948274755497,24.2099193160998,-9.76980347925633));
#36998=CARTESIAN_POINT('Ctrl Pts',(-20.4120862570241,24.2837578111728,-9.76509306903594));
#36999=CARTESIAN_POINT('Ctrl Pts',(-20.4347027313341,24.3805182012034,-9.75892039271475));
#37000=CARTESIAN_POINT('Ctrl Pts',(-20.4618384160323,24.4764020278299,-9.75274771639359));
#37001=CARTESIAN_POINT('Ctrl Pts',(-20.4934104028952,24.5709551142811,-9.7465750400724));
#37002=CARTESIAN_POINT('Ctrl Pts',(-20.5261462377295,24.6689937405667,-9.74017481846411));
#37003=CARTESIAN_POINT('Ctrl Pts',(-20.5636517547069,24.7656011521383,-9.73377459685581));
#37004=CARTESIAN_POINT('Ctrl Pts',(-20.6057762256289,24.860281861717,-9.72737437524752));
#37005=CARTESIAN_POINT('Ctrl Pts',(-20.6462960525434,24.9513559068099,-9.72121795675476));
#37006=CARTESIAN_POINT('Ctrl Pts',(-20.6910891794856,25.0406469057963,-9.71506153826197));
#37007=CARTESIAN_POINT('Ctrl Pts',(-20.7399709965839,25.1277300294476,-9.70890511976921));
#37008=CARTESIAN_POINT('Ctrl Pts',(-20.7888200647944,25.2147548108437,-9.70275282583381));
#37009=CARTESIAN_POINT('Ctrl Pts',(-20.8417521675508,25.2995742789073,-9.6966005318984));
#37010=CARTESIAN_POINT('Ctrl Pts',(-20.898535909008,25.3817864558872,-9.690448237963));
#37011=CARTESIAN_POINT('Ctrl Pts',(-20.9552967994043,25.463965548829,-9.68429841984973));
#37012=CARTESIAN_POINT('Ctrl Pts',(-21.0159060003052,25.5435390798167,-9.67814860173648));
#37013=CARTESIAN_POINT('Ctrl Pts',(-21.0800883176759,25.6201332814678,-9.67199878362321));
#37014=CARTESIAN_POINT('Ctrl Pts',(-21.1442619770477,25.6967171507946,-9.66584979510166));
#37015=CARTESIAN_POINT('Ctrl Pts',(-21.2120075140709,25.7703221584116,-9.6597008065801));
#37016=CARTESIAN_POINT('Ctrl Pts',(-21.2830095503844,25.8406077063781,-9.65355181805855));
#37017=CARTESIAN_POINT('Ctrl Pts',(-21.3540485173879,25.9109298123634,-9.64739963122888));
#37018=CARTESIAN_POINT('Ctrl Pts',(-21.4283470578706,25.9779287042374,-9.64124744439921));
#37019=CARTESIAN_POINT('Ctrl Pts',(-21.5055533802708,26.0413010945826,-9.63509525756955));
#37020=CARTESIAN_POINT('Ctrl Pts',(-21.5827839279436,26.1046933694837,-9.62894114034871));
#37021=CARTESIAN_POINT('Ctrl Pts',(-21.662923729402,26.1644566129475,-9.6227870231279));
#37022=CARTESIAN_POINT('Ctrl Pts',(-21.7455897448107,26.2203292699431,-9.61663290590707));
#37023=CARTESIAN_POINT('Ctrl Pts',(-21.8283399051361,26.2762587991618,-9.61047252447139));
#37024=CARTESIAN_POINT('Ctrl Pts',(-21.913621043207,26.3282896083141,-9.60431214303569));
#37025=CARTESIAN_POINT('Ctrl Pts',(-22.0010234910573,26.3762049272853,-9.59815176160001));
#37026=CARTESIAN_POINT('Ctrl Pts',(-22.0255307934407,26.3896401941424,-9.59642441489114));
#37027=CARTESIAN_POINT('Ctrl Pts',(-22.0502047432709,26.4027521781315,-9.59469706818227));
#37028=CARTESIAN_POINT('Ctrl Pts',(-22.0750360153461,26.4155367745563,-9.59296972147339));
#37029=CARTESIAN_POINT('Origin',(-23.5502525316942,23.5502525316942,-77.3107734492734));
#37030=CARTESIAN_POINT('',(-22.0750359919087,26.4155367624894,-8.09328852648195));
#37031=CARTESIAN_POINT('',(-22.0750360458934,26.4155367902838,-8.34120882940695));
#37032=CARTESIAN_POINT('',(-22.0750360153461,26.4155367745563,-77.3107734492734));
#37033=CARTESIAN_POINT('',(-26.773001214148,23.5531666769314,-8.93957441054318));
#37034=CARTESIAN_POINT('Ctrl Pts',(-22.0750359919087,26.4155367624894,-8.09328852648195));
#37035=CARTESIAN_POINT('Ctrl Pts',(-21.9573065708424,26.354922744756,-8.10161611668175));
#37036=CARTESIAN_POINT('Ctrl Pts',(-21.8434252301781,26.2871108196349,-8.11019806025512));
#37037=CARTESIAN_POINT('Ctrl Pts',(-21.5403771928706,26.0803666436431,-8.13450590777129));
#37038=CARTESIAN_POINT('Ctrl Pts',(-21.3617299474878,25.927526736386,-8.15061384987241));
#37039=CARTESIAN_POINT('Ctrl Pts',(-21.1273775541537,25.678029700849,-8.1734080311854));
#37040=CARTESIAN_POINT('Ctrl Pts',(-21.0574951103024,25.5957170105429,-8.18046132516641));
#37041=CARTESIAN_POINT('Ctrl Pts',(-20.9878143459113,25.5047531131256,-8.18764675290268));
#37042=CARTESIAN_POINT('Ctrl Pts',(-20.9837779343401,25.4994498335995,-8.18806356127619));
#37043=CARTESIAN_POINT('Ctrl Pts',(-20.978238786992,25.492125133863,-8.18863629861809));
#37044=CARTESIAN_POINT('Ctrl Pts',(-20.9767219627746,25.4901144641352,-8.18879321376207));
#37045=CARTESIAN_POINT('Ctrl Pts',(-20.9741306040372,25.4866710256537,-8.18906142062471));
#37046=CARTESIAN_POINT('Ctrl Pts',(-20.9730549070567,25.4852391397878,-8.18917279464785));
#37047=CARTESIAN_POINT('Ctrl Pts',(-20.9709600497518,25.4824457796315,-8.18938976372299));
#37048=CARTESIAN_POINT('Ctrl Pts',(-20.9699407763217,25.4810843990186,-8.18949536655215));
#37049=CARTESIAN_POINT('Ctrl Pts',(-20.9674807358536,25.4777932479724,-8.18975032594651));
#37050=CARTESIAN_POINT('Ctrl Pts',(-20.9660410502544,25.4758626639862,-8.18989960572073));
#37051=CARTESIAN_POINT('Ctrl Pts',(-20.9616965984248,25.470023210618,-8.19035029706649));
#37052=CARTESIAN_POINT('Ctrl Pts',(-20.9587985101012,25.4661093462885,-8.19065123989692));
#37053=CARTESIAN_POINT('Ctrl Pts',(-20.9302781950621,25.4274095819416,-8.19361594253352));
#37054=CARTESIAN_POINT('Ctrl Pts',(-20.905347512274,25.392116262991,-8.19623230094382));
#37055=CARTESIAN_POINT('Ctrl Pts',(-20.834113323417,25.2868424997952,-8.20381716082002));
#37056=CARTESIAN_POINT('Ctrl Pts',(-20.7898217525837,25.215539596482,-8.20867762667879));
#37057=CARTESIAN_POINT('Ctrl Pts',(-20.6533529590857,24.9754069385022,-8.22442973516083));
#37058=CARTESIAN_POINT('Ctrl Pts',(-20.5734954248659,24.8000583860983,-8.23499146268696));
#37059=CARTESIAN_POINT('Ctrl Pts',(-20.4473888278571,24.4411705566913,-8.25646728967847));
#37060=CARTESIAN_POINT('Ctrl Pts',(-20.4006973012122,24.2586196390261,-8.2673313588744));
#37061=CARTESIAN_POINT('Ctrl Pts',(-20.3681718124855,24.0607764969554,-8.27951619730709));
#37062=CARTESIAN_POINT('Ctrl Pts',(-20.3662242296477,24.0484855972591,-8.28027469742689));
#37063=CARTESIAN_POINT('Ctrl Pts',(-20.3636550050387,24.0316410266239,-8.28131639530575));
#37064=CARTESIAN_POINT('Ctrl Pts',(-20.3629718279045,24.0270967356345,-8.28159763911032));
#37065=CARTESIAN_POINT('Ctrl Pts',(-20.3618239169232,24.0193484838624,-8.28207754946121));
#37066=CARTESIAN_POINT('Ctrl Pts',(-20.3613542858122,24.0161452458761,-8.2822760604407));
#37067=CARTESIAN_POINT('Ctrl Pts',(-20.3604539345899,24.0099390290277,-8.28266088552741));
#37068=CARTESIAN_POINT('Ctrl Pts',(-20.3600226263091,24.0069361383715,-8.28284718072536));
#37069=CARTESIAN_POINT('Ctrl Pts',(-20.3590071832156,23.9997946956526,-8.28329045818412));
#37070=CARTESIAN_POINT('Ctrl Pts',(-20.3584268590817,23.9956556151497,-8.28354756093572));
#37071=CARTESIAN_POINT('Ctrl Pts',(-20.3567437746367,23.9834790299398,-8.28430447201234));
#37072=CARTESIAN_POINT('Ctrl Pts',(-20.3556633166317,23.9754385207178,-8.28480498596277));
#37073=CARTESIAN_POINT('Ctrl Pts',(-20.3475239854818,23.9130847062843,-8.28869203985816));
#37074=CARTESIAN_POINT('Ctrl Pts',(-20.3418207263208,23.8586063568136,-8.29212123062283));
#37075=CARTESIAN_POINT('Ctrl Pts',(-20.3271819304938,23.6732703987473,-8.30390953093639));
#37076=CARTESIAN_POINT('Ctrl Pts',(-20.3248467159278,23.5420364197295,-8.31246908498272));
#37077=CARTESIAN_POINT('Ctrl Pts',(-20.3383294394444,23.2302087255335,-8.3332499117462));
#37078=CARTESIAN_POINT('Ctrl Pts',(-20.3613681783913,23.0503636642574,-8.34560086238983));
#37079=CARTESIAN_POINT('Ctrl Pts',(-20.4290269267916,22.7353915105678,-8.36726555311397));
#37080=CARTESIAN_POINT('Ctrl Pts',(-20.4677177665171,22.5994435144559,-8.37661941945852));
#37081=CARTESIAN_POINT('Ctrl Pts',(-20.5182674765082,22.4578849084121,-8.38606982996712));
#37082=CARTESIAN_POINT('Ctrl Pts',(-20.5213646003374,22.4493264200469,-8.3866400139683));
#37083=CARTESIAN_POINT('Ctrl Pts',(-20.5255948755178,22.4377895986684,-8.38740691651851));
#37084=CARTESIAN_POINT('Ctrl Pts',(-20.5266962084174,22.4347997650539,-8.38760550880069));
#37085=CARTESIAN_POINT('Ctrl Pts',(-20.5284346180392,22.4301019247316,-8.38791730191848));
#37086=CARTESIAN_POINT('Ctrl Pts',(-20.5290687092669,22.4283928271372,-8.38803068187137));
#37087=CARTESIAN_POINT('Ctrl Pts',(-20.5302931807261,22.4251010154478,-8.38824895624923));
#37088=CARTESIAN_POINT('Ctrl Pts',(-20.5308833512837,22.4235182380774,-8.38835386212594));
#37089=CARTESIAN_POINT('Ctrl Pts',(-20.5322897679984,22.419755411725,-8.38860315382899));
#37090=CARTESIAN_POINT('Ctrl Pts',(-20.5331071311787,22.4175757845403,-8.38874747141705));
#37091=CARTESIAN_POINT('Ctrl Pts',(-20.5355047382168,22.4112031990482,-8.38916916910932));
#37092=CARTESIAN_POINT('Ctrl Pts',(-20.5370913742377,22.4070126267532,-8.38944616531073));
#37093=CARTESIAN_POINT('Ctrl Pts',(-20.5492608158052,22.3750724093487,-8.39155514455531));
#37094=CARTESIAN_POINT('Ctrl Pts',(-20.5602184625373,22.3474657605841,-8.39336493263201));
#37095=CARTESIAN_POINT('Ctrl Pts',(-20.5988637072362,22.2538966127567,-8.39946710842424));
#37096=CARTESIAN_POINT('Ctrl Pts',(-20.6283666745114,22.1887022173879,-8.40366441416358));
#37097=CARTESIAN_POINT('Ctrl Pts',(-20.7354038888723,21.9717141908156,-8.41762300153342));
#37098=CARTESIAN_POINT('Ctrl Pts',(-20.8227972346321,21.8251001143924,-8.42704664337351));
#37099=CARTESIAN_POINT('Ctrl Pts',(-21.0082678604624,21.5635480779807,-8.44499673029432));
#37100=CARTESIAN_POINT('Ctrl Pts',(-21.1036102626014,21.4472506895518,-8.4534747028518));
#37101=CARTESIAN_POINT('Ctrl Pts',(-21.2246285027271,21.319048370053,-8.46377675624882));
#37102=CARTESIAN_POINT('Ctrl Pts',(-21.2427789758806,21.3002825605042,-8.46531059699426));
#37103=CARTESIAN_POINT('Ctrl Pts',(-21.2644155381146,21.2784496669926,-8.46712720679567));
#37104=CARTESIAN_POINT('Ctrl Pts',(-21.2676830592542,21.2751666826622,-8.46740123571817));
#37105=CARTESIAN_POINT('Ctrl Pts',(-21.2737931508909,21.2690540885643,-8.46791308342342));
#37106=CARTESIAN_POINT('Ctrl Pts',(-21.2766339506186,21.2662227164401,-8.46815083037824));
#37107=CARTESIAN_POINT('Ctrl Pts',(-21.2829969721644,21.2599044457422,-8.46868284880503));
#37108=CARTESIAN_POINT('Ctrl Pts',(-21.2865219620928,21.2564203593448,-8.46897723318948));
#37109=CARTESIAN_POINT('Ctrl Pts',(-21.2949976781262,21.2480815593424,-8.46968426381833));
#37110=CARTESIAN_POINT('Ctrl Pts',(-21.2999560479873,21.2432346785305,-8.47009722668026));
#37111=CARTESIAN_POINT('Ctrl Pts',(-21.3063472510161,21.2370273897882,-8.47062870592974));
#37112=CARTESIAN_POINT('Ctrl Pts',(-21.3077657718126,21.2356522211586,-8.4707466156265));
#37113=CARTESIAN_POINT('Ctrl Pts',(-21.3130255933399,21.2305625217665,-8.47118363091039));
#37114=CARTESIAN_POINT('Ctrl Pts',(-21.3168748513546,21.2268562563436,-8.47150307504396));
#37115=CARTESIAN_POINT('Ctrl Pts',(-21.3226728131037,21.2213013998617,-8.47198369030811));
#37116=CARTESIAN_POINT('Ctrl Pts',(-21.3246146518515,21.2194456317378,-8.47214456468561));
#37117=CARTESIAN_POINT('Ctrl Pts',(-21.3323351459601,21.2120857882112,-8.47278381842538));
#37118=CARTESIAN_POINT('Ctrl Pts',(-21.3381318822736,21.2066007911476,-8.47326298323059));
#37119=CARTESIAN_POINT('Ctrl Pts',(-21.3647996812133,21.1815542272336,-8.4754638154192));
#37120=CARTESIAN_POINT('Ctrl Pts',(-21.3859097364079,21.1622500185959,-8.47719605813919));
#37121=CARTESIAN_POINT('Ctrl Pts',(-21.4126077977254,21.1384806594419,-8.47937578269444));
#37122=CARTESIAN_POINT('Ctrl Pts',(-21.4179578802664,21.1337492540945,-8.47981203633124));
#37123=CARTESIAN_POINT('Ctrl Pts',(-21.4265892119216,21.1261670216064,-8.48051499253071));
#37124=CARTESIAN_POINT('Ctrl Pts',(-21.4298605986814,21.1233049619914,-8.48078122566481));
#37125=CARTESIAN_POINT('Ctrl Pts',(-21.4356861102275,21.1182291280112,-8.4812549758304));
#37126=CARTESIAN_POINT('Ctrl Pts',(-21.4382379512898,21.1160127327267,-8.48146238342603));
#37127=CARTESIAN_POINT('Ctrl Pts',(-21.443562457163,21.1114028214842,-8.48189490640814));
#37128=CARTESIAN_POINT('Ctrl Pts',(-21.4463357239177,21.109010010989,-8.48212005061243));
#37129=CARTESIAN_POINT('Ctrl Pts',(-21.4535337327445,21.1028208510722,-8.48270406599189));
#37130=CARTESIAN_POINT('Ctrl Pts',(-21.457964693641,21.09903178374,-8.48306323732909));
#37131=CARTESIAN_POINT('Ctrl Pts',(-21.4764944432798,21.0832732049138,-8.48456386754899));
#37132=CARTESIAN_POINT('Ctrl Pts',(-21.4906856323746,21.0714133331376,-8.48570981834527));
#37133=CARTESIAN_POINT('Ctrl Pts',(-21.5272907129781,21.0413530413518,-8.48865767838952));
#37134=CARTESIAN_POINT('Ctrl Pts',(-21.5498481627544,21.0233307984716,-8.4904666840662));
#37135=CARTESIAN_POINT('Ctrl Pts',(-21.6277837373006,20.9627618506007,-8.49669261457061));
#37136=CARTESIAN_POINT('Ctrl Pts',(-21.6842979353195,20.921715573079,-8.50116691565166));
#37137=CARTESIAN_POINT('Ctrl Pts',(-21.9160538687353,20.7646331999288,-8.51936029325104));
#37138=CARTESIAN_POINT('Ctrl Pts',(-22.1011077055038,20.6640371537043,-8.53358897655656));
#37139=CARTESIAN_POINT('Ctrl Pts',(-22.3192744424469,20.5717414982212,-8.54961281572385));
#37140=CARTESIAN_POINT('Ctrl Pts',(-22.3440726763337,20.5616131744564,-8.55142306099604));
#37141=CARTESIAN_POINT('Ctrl Pts',(-22.515829278821,20.4939487563055,-8.56387478419597));
#37142=CARTESIAN_POINT('Ctrl Pts',(-22.6667360821941,20.4469580885852,-8.57439230469254));
#37143=CARTESIAN_POINT('Ctrl Pts',(-22.8296221596707,20.409090772024,-8.58490909751607));
#37144=CARTESIAN_POINT('Ctrl Pts',(-22.8387567737052,20.4070091231993,-8.5854961181882));
#37145=CARTESIAN_POINT('Ctrl Pts',(-22.8510460918294,20.4042648798913,-8.58628204590355));
#37146=CARTESIAN_POINT('Ctrl Pts',(-22.8541927827349,20.4035671681822,-8.58648294693222));
#37147=CARTESIAN_POINT('Ctrl Pts',(-22.8591280460063,20.4024806438571,-8.58679750654798));
#37148=CARTESIAN_POINT('Ctrl Pts',(-22.8609159009117,20.4020886347414,-8.5869113497083));
#37149=CARTESIAN_POINT('Ctrl Pts',(-22.8643525294807,20.4013381796707,-8.5871299679914));
#37150=CARTESIAN_POINT('Ctrl Pts',(-22.8660012398631,20.4009795077951,-8.58723475546849));
#37151=CARTESIAN_POINT('Ctrl Pts',(-22.8699096467533,20.40013246,-8.58748294142765));
#37152=CARTESIAN_POINT('Ctrl Pts',(-22.8721695852919,20.399645221181,-8.58762627344358));
#37153=CARTESIAN_POINT('Ctrl Pts',(-22.8768518407422,20.3986410063383,-8.58792287663201));
#37154=CARTESIAN_POINT('Ctrl Pts',(-22.8792742344445,20.3981243899385,-8.58807612702932));
#37155=CARTESIAN_POINT('Ctrl Pts',(-22.8927668705227,20.3952631156596,-8.58892862941443));
#37156=CARTESIAN_POINT('Ctrl Pts',(-22.9038489912569,20.3929739437583,-8.5896247210007));
#37157=CARTESIAN_POINT('Ctrl Pts',(-23.0004243588922,20.3735547139665,-8.5956569219187));
#37158=CARTESIAN_POINT('Ctrl Pts',(-23.0865768106257,20.3598406542811,-8.60080737010682));
#37159=CARTESIAN_POINT('Ctrl Pts',(-23.3167410700854,20.3327249795871,-8.61420924637417));
#37160=CARTESIAN_POINT('Ctrl Pts',(-23.4612787620586,20.3254889682529,-8.62226231399615));
#37161=CARTESIAN_POINT('Ctrl Pts',(-23.8682045332157,20.3325065145344,-8.64500334971389));
#37162=CARTESIAN_POINT('Ctrl Pts',(-24.1290080314134,20.3690580132611,-8.65974601734649));
#37163=CARTESIAN_POINT('Ctrl Pts',(-24.3979730123308,20.4409528177106,-8.67662673108713));
#37164=CARTESIAN_POINT('Ctrl Pts',(-24.4134340220905,20.4452094684198,-8.67760274171195));
#37165=CARTESIAN_POINT('Ctrl Pts',(-24.4343240366428,20.4511288876333,-8.67892934456185));
#37166=CARTESIAN_POINT('Ctrl Pts',(-24.4397815426165,20.4526909221188,-8.67927664902685));
#37167=CARTESIAN_POINT('Ctrl Pts',(-24.4483722792125,20.4551743182147,-8.67982450664443));
#37168=CARTESIAN_POINT('Ctrl Pts',(-24.4515083031492,20.4560860425198,-8.6800247445866));
#37169=CARTESIAN_POINT('Ctrl Pts',(-24.4575469129457,20.4578515838417,-8.68041078782019));
#37170=CARTESIAN_POINT('Ctrl Pts',(-24.4604496943736,20.4587047249344,-8.68059657082713));
#37171=CARTESIAN_POINT('Ctrl Pts',(-24.4672976965006,20.4607278656806,-8.681035354133));
#37172=CARTESIAN_POINT('Ctrl Pts',(-24.4712418792818,20.4619013344399,-8.68128846783668));
#37173=CARTESIAN_POINT('Ctrl Pts',(-24.4793838911243,20.464340720936,-8.68181178637204));
#37174=CARTESIAN_POINT('Ctrl Pts',(-24.4835814038687,20.4656076570103,-8.68208202419808));
#37175=CARTESIAN_POINT('Ctrl Pts',(-24.5064330502439,20.4725558876646,-8.6835556762369));
#37176=CARTESIAN_POINT('Ctrl Pts',(-24.5250375885064,20.478397736488,-8.6847643556774));
#37177=CARTESIAN_POINT('Ctrl Pts',(-24.5729895746836,20.4939342030055,-8.68790323684717));
#37178=CARTESIAN_POINT('Ctrl Pts',(-24.6022520858705,20.5038826237384,-8.68984173337229));
#37179=CARTESIAN_POINT('Ctrl Pts',(-24.7256388101766,20.5478203595679,-8.69811559399015));
#37180=CARTESIAN_POINT('Ctrl Pts',(-24.8182876701456,20.5857601077218,-8.70457961761168));
#37181=CARTESIAN_POINT('Ctrl Pts',(-24.9864607687752,20.6639541957462,-8.71677962722367));
#37182=CARTESIAN_POINT('Ctrl Pts',(-25.0624407533349,20.7030262536865,-8.72247834415721));
#37183=CARTESIAN_POINT('Ctrl Pts',(-25.2065238551658,20.7845150538289,-8.73361391763236));
#37184=CARTESIAN_POINT('Ctrl Pts',(-25.2747756541109,20.826549520247,-8.73904131277138));
#37185=CARTESIAN_POINT('Ctrl Pts',(-25.5018475751631,20.9783565377205,-8.75752755849726));
#37186=CARTESIAN_POINT('Ctrl Pts',(-25.65236623206,21.0998425384074,-8.77055009609657));
#37187=CARTESIAN_POINT('Ctrl Pts',(-25.7993405518816,21.2420386158584,-8.78343687558731));
#37188=CARTESIAN_POINT('Ctrl Pts',(-25.8075191290508,21.2500360371797,-8.78415451414662));
#37189=CARTESIAN_POINT('Ctrl Pts',(-25.8181385178986,21.2605313898076,-8.78508681638621));
#37190=CARTESIAN_POINT('Ctrl Pts',(-25.8206179620484,21.2629898517747,-8.78530452816382));
#37191=CARTESIAN_POINT('Ctrl Pts',(-25.8244294142267,21.2667813537328,-8.7856392463875));
#37192=CARTESIAN_POINT('Ctrl Pts',(-25.8257642467635,21.2681115307367,-8.78575647910237));
#37193=CARTESIAN_POINT('Ctrl Pts',(-25.8284179200658,21.2707605917007,-8.78598955640326));
#37194=CARTESIAN_POINT('Ctrl Pts',(-25.8297367749204,21.2720794420927,-8.78610540182543));
#37195=CARTESIAN_POINT('Ctrl Pts',(-25.8326783833245,21.2750261523001,-8.78636380467813));
#37196=CARTESIAN_POINT('Ctrl Pts',(-25.8343005368991,21.2766545998514,-8.78650631388841));
#37197=CARTESIAN_POINT('Ctrl Pts',(-25.8376540028831,21.2800282882857,-8.78680095192132));
#37198=CARTESIAN_POINT('Ctrl Pts',(-25.839385064168,21.2817737782952,-8.78695306075394));
#37199=CARTESIAN_POINT('Ctrl Pts',(-25.8438710275129,21.2863074966391,-8.78734729198076));
#37200=CARTESIAN_POINT('Ctrl Pts',(-25.8466228533236,21.2890987836193,-8.78758917282893));
#37201=CARTESIAN_POINT('Ctrl Pts',(-25.8816200111191,21.3247275825165,-8.79066608053887));
#37202=CARTESIAN_POINT('Ctrl Pts',(-25.9131654859177,21.3582492172115,-8.79344729495734));
#37203=CARTESIAN_POINT('Ctrl Pts',(-26.0107764462834,21.466532081651,-8.80212277202728));
#37204=CARTESIAN_POINT('Ctrl Pts',(-26.0740984511117,21.5436947878039,-8.80785712787751));
#37205=CARTESIAN_POINT('Ctrl Pts',(-26.1569451001805,21.6547901149668,-8.81570628027586));
#37206=CARTESIAN_POINT('Ctrl Pts',(-26.1795834093834,21.6863203586925,-8.81789108470322));
#37207=CARTESIAN_POINT('Ctrl Pts',(-26.225230556148,21.7523839905228,-8.82239677430283));
#37208=CARTESIAN_POINT('Ctrl Pts',(-26.2481530125848,21.7869681634627,-8.82471623617704));
#37209=CARTESIAN_POINT('Ctrl Pts',(-26.4170307378308,22.0527676888526,-8.84231400873226));
#37210=CARTESIAN_POINT('Ctrl Pts',(-26.5336731708421,22.3012315860595,-8.85759716777871));
#37211=CARTESIAN_POINT('Ctrl Pts',(-26.6229787502142,22.5782525921642,-8.87522725900439));
#37212=CARTESIAN_POINT('Ctrl Pts',(-26.6282660744616,22.5951279808995,-8.8763028989983));
#37213=CARTESIAN_POINT('Ctrl Pts',(-26.6351342406631,22.6176983432464,-8.87774402651722));
#37214=CARTESIAN_POINT('Ctrl Pts',(-26.6368387618405,22.6233556033042,-8.87810545254564));
#37215=CARTESIAN_POINT('Ctrl Pts',(-26.639474550055,22.6321916103325,-8.87867029404943));
#37216=CARTESIAN_POINT('Ctrl Pts',(-26.6404164961137,22.6353671798997,-8.87887335954752));
#37217=CARTESIAN_POINT('Ctrl Pts',(-26.6422067852974,22.6414370647849,-8.87926163619824));
#37218=CARTESIAN_POINT('Ctrl Pts',(-26.6430559648271,22.6443311315879,-8.87944681976235));
#37219=CARTESIAN_POINT('Ctrl Pts',(-26.6450287232469,22.6510895418458,-8.87987940668242));
#37220=CARTESIAN_POINT('Ctrl Pts',(-26.6461491271297,22.6549548000691,-8.8801269135044));
#37221=CARTESIAN_POINT('Ctrl Pts',(-26.6484402906067,22.6629147660326,-8.88063683451766));
#37222=CARTESIAN_POINT('Ctrl Pts',(-26.64961017888,22.6670097143465,-8.88089927663189));
#37223=CARTESIAN_POINT('Ctrl Pts',(-26.6525882202093,22.6775124970252,-8.88157269708334));
#37224=CARTESIAN_POINT('Ctrl Pts',(-26.6543846323421,22.6839236143609,-8.88198405775232));
#37225=CARTESIAN_POINT('Ctrl Pts',(-26.6690070553294,22.7367381963858,-8.88537529190522));
#37226=CARTESIAN_POINT('Ctrl Pts',(-26.6808110645855,22.7834160307172,-8.8883882253994));
#37227=CARTESIAN_POINT('Ctrl Pts',(-26.7459135208793,23.0674877492968,-8.90683162709606));
#37228=CARTESIAN_POINT('Ctrl Pts',(-26.7732211168377,23.3099766345803,-8.92311349304411));
#37229=CARTESIAN_POINT('Ctrl Pts',(-26.773001214148,23.5531666769314,-8.93957441054318));
#37230=CARTESIAN_POINT('Ctrl Pts',(-26.7730012132604,23.5531676583652,-8.93957447697395));
#37231=CARTESIAN_POINT('Ctrl Pts',(-26.7728078658805,23.7669182373274,-8.95404271192202));
#37232=CARTESIAN_POINT('Ctrl Pts',(-26.7513493600371,23.980153034217,-8.96854767402835));
#37233=CARTESIAN_POINT('Ctrl Pts',(-26.7076087245426,24.1962117567834,-8.98241629501119));
#37234=CARTESIAN_POINT('Ctrl Pts',(-26.7062742060583,24.2027007225553,-8.98283199846243));
#37235=CARTESIAN_POINT('Ctrl Pts',(-26.7041939028601,24.2126602533808,-8.9834687320389));
#37236=CARTESIAN_POINT('Ctrl Pts',(-26.7034623869286,24.2161337310392,-8.98369055458102));
#37237=CARTESIAN_POINT('Ctrl Pts',(-26.7022468014455,24.2218588076012,-8.98405575755601));
#37238=CARTESIAN_POINT('Ctrl Pts',(-26.7017660569191,24.2241110975567,-8.98419932637149));
#37239=CARTESIAN_POINT('Ctrl Pts',(-26.7008240282472,24.2285014473913,-8.98447897540248));
#37240=CARTESIAN_POINT('Ctrl Pts',(-26.7003629811254,24.2306395561073,-8.98461506914724));
#37241=CARTESIAN_POINT('Ctrl Pts',(-26.6995445395715,24.2344164191022,-8.98485530054972));
#37242=CARTESIAN_POINT('Ctrl Pts',(-26.6991880443372,24.2360553553674,-8.98495948961635));
#37243=CARTESIAN_POINT('Ctrl Pts',(-26.6984240067506,24.2395547538723,-8.9851818283776));
#37244=CARTESIAN_POINT('Ctrl Pts',(-26.698016095785,24.2414151279678,-8.98529995612276));
#37245=CARTESIAN_POINT('Ctrl Pts',(-26.6968342144602,24.2467826280248,-8.98564056575428));
#37246=CARTESIAN_POINT('Ctrl Pts',(-26.6960560271926,24.2502888374825,-8.98586280407847));
#37247=CARTESIAN_POINT('Ctrl Pts',(-26.692587552028,24.2657938589516,-8.98684446565155));
#37248=CARTESIAN_POINT('Ctrl Pts',(-26.6898344180992,24.2777787243962,-8.98760030966766));
#37249=CARTESIAN_POINT('Ctrl Pts',(-26.6390311639475,24.49327385812,-9.00114252270274));
#37250=CARTESIAN_POINT('Ctrl Pts',(-26.5713463842603,24.6916831419501,-9.01285124716831));
#37251=CARTESIAN_POINT('Ctrl Pts',(-26.464828963232,24.9263774657351,-9.02725887432765));
#37252=CARTESIAN_POINT('Ctrl Pts',(-26.4437632472755,24.9701367998647,-9.02996950052121));
#37253=CARTESIAN_POINT('Ctrl Pts',(-26.399649666394,25.056710635031,-9.0354071566973));
#37254=CARTESIAN_POINT('Ctrl Pts',(-26.376605841805,25.0995126448388,-9.03813348394425));
#37255=CARTESIAN_POINT('Ctrl Pts',(-26.2838173315237,25.2628943667709,-9.04873352151199));
#37256=CARTESIAN_POINT('Ctrl Pts',(-26.2072588814237,25.3794134888963,-9.05671690527982));
#37257=CARTESIAN_POINT('Ctrl Pts',(-26.0899619278102,25.5349640794995,-9.06827346276721));
#37258=CARTESIAN_POINT('Ctrl Pts',(-26.0553746749621,25.5784453768402,-9.07160982174604));
#37259=CARTESIAN_POINT('Ctrl Pts',(-26.0152241238418,25.6263259305737,-9.07541410948211));
#37260=CARTESIAN_POINT('Ctrl Pts',(-26.0107485965919,25.6316282356625,-9.07583724079194));
#37261=CARTESIAN_POINT('Ctrl Pts',(-26.003421959669,25.6402516892807,-9.07652843851192));
#37262=CARTESIAN_POINT('Ctrl Pts',(-26.0005811297096,25.6435815747527,-9.07679608200145));
#37263=CARTESIAN_POINT('Ctrl Pts',(-25.9950598925253,25.6500266671777,-9.0773155614169));
#37264=CARTESIAN_POINT('Ctrl Pts',(-25.9923802916666,25.6531425562419,-9.07756736374422));
#37265=CARTESIAN_POINT('Ctrl Pts',(-25.9877180204353,25.6585430012168,-9.07800493676978));
#37266=CARTESIAN_POINT('Ctrl Pts',(-25.9857380754591,25.6608299121036,-9.07819059415372));
#37267=CARTESIAN_POINT('Ctrl Pts',(-25.9816121138658,25.665582016023,-9.07857713320096));
#37268=CARTESIAN_POINT('Ctrl Pts',(-25.9794655617997,25.6680467377801,-9.07877803705164));
#37269=CARTESIAN_POINT('Ctrl Pts',(-25.9735721735892,25.6747929162054,-9.07932909074726));
#37270=CARTESIAN_POINT('Ctrl Pts',(-25.9698177565168,25.6790677078844,-9.07967955711122));
#37271=CARTESIAN_POINT('Ctrl Pts',(-25.9553795957711,25.6954195100647,-9.08102510925123));
#37272=CARTESIAN_POINT('Ctrl Pts',(-25.9446167306384,25.7074260590344,-9.08202351509584));
#37273=CARTESIAN_POINT('Ctrl Pts',(-25.7568582072712,25.9137443230065,-9.09936318920441));
#37274=CARTESIAN_POINT('Ctrl Pts',(-25.5568754223864,26.0857225123447,-9.1167758909787));
#37275=CARTESIAN_POINT('Ctrl Pts',(-25.2737376435289,26.2745391199642,-9.13979081734646));
#37276=CARTESIAN_POINT('Ctrl Pts',(-25.2076479312285,26.3152442045469,-9.14505203024023));
#37277=CARTESIAN_POINT('Ctrl Pts',(-25.0641567443149,26.3966265173592,-9.15617563231805));
#37278=CARTESIAN_POINT('Ctrl Pts',(-24.9864343343809,26.4366229864699,-9.1620260472387));
#37279=CARTESIAN_POINT('Ctrl Pts',(-24.8605846304507,26.4950421937532,-9.17113274904898));
#37280=CARTESIAN_POINT('Ctrl Pts',(-24.8134772370519,26.5155552756975,-9.17446304808412));
#37281=CARTESIAN_POINT('Ctrl Pts',(-24.7509119592197,26.5410377622456,-9.17876570665235));
#37282=CARTESIAN_POINT('Ctrl Pts',(-24.7358810454088,26.5470282004189,-9.17979039023191));
#37283=CARTESIAN_POINT('Ctrl Pts',(-24.7112636828298,26.5566250215961,-9.18145319655281));
#37284=CARTESIAN_POINT('Ctrl Pts',(-24.7017042361781,26.5602992788561,-9.18209513238091));
#37285=CARTESIAN_POINT('Ctrl Pts',(-24.6898792421018,26.5647797421613,-9.18288441629445));
#37286=CARTESIAN_POINT('Ctrl Pts',(-24.6876302385443,26.5656290079855,-9.18303431745502));
#37287=CARTESIAN_POINT('Ctrl Pts',(-24.6832655598858,26.5672716144754,-9.18332481661476));
#37288=CARTESIAN_POINT('Ctrl Pts',(-24.6811499974788,26.5680652478638,-9.18346543213911));
#37289=CARTESIAN_POINT('Ctrl Pts',(-24.6773046698804,26.5695031750614,-9.1837206736744));
#37290=CARTESIAN_POINT('Ctrl Pts',(-24.6755751928137,26.5701482050711,-9.18383534382065));
#37291=CARTESIAN_POINT('Ctrl Pts',(-24.6720609766479,26.5714554376694,-9.18406808936415));
#37292=CARTESIAN_POINT('Ctrl Pts',(-24.6702762119692,26.572117542232,-9.18418615858885));
#37293=CARTESIAN_POINT('Ctrl Pts',(-24.6651269111073,26.5740226197903,-9.18452641809959));
#37294=CARTESIAN_POINT('Ctrl Pts',(-24.6617608714587,26.5752615628324,-9.1847483656156));
#37295=CARTESIAN_POINT('Ctrl Pts',(-24.6468850206994,26.5807087566014,-9.1857271658962));
#37296=CARTESIAN_POINT('Ctrl Pts',(-24.6353531305201,26.5848570279695,-9.18648046492864));
#37297=CARTESIAN_POINT('Ctrl Pts',(-24.4374462254037,26.6547760398833,-9.19931931277185));
#37298=CARTESIAN_POINT('Ctrl Pts',(-24.245401182448,26.7033419201677,-9.21044159575959));
#37299=CARTESIAN_POINT('Ctrl Pts',(-23.8767040662614,26.7612259883571,-9.23132255251582));
#37300=CARTESIAN_POINT('Ctrl Pts',(-23.7013883070317,26.7742369283798,-9.24106370529646));
#37301=CARTESIAN_POINT('Ctrl Pts',(-23.4097268643695,26.772032440428,-9.25785337287125));
#37302=CARTESIAN_POINT('Ctrl Pts',(-23.2937035648919,26.7648740164228,-9.26468166520517));
#37303=CARTESIAN_POINT('Ctrl Pts',(-23.1595200641905,26.7492842963919,-9.27285945600781));
#37304=CARTESIAN_POINT('Ctrl Pts',(-23.1407316302965,26.7469334197694,-9.27401084508389));
#37305=CARTESIAN_POINT('Ctrl Pts',(-23.116137701976,26.7436357609215,-9.27552664793765));
#37306=CARTESIAN_POINT('Ctrl Pts',(-23.1103122736418,26.7428384275961,-9.27588632421064));
#37307=CARTESIAN_POINT('Ctrl Pts',(-23.1008504631222,26.7415169897278,-9.27647156531165));
#37308=CARTESIAN_POINT('Ctrl Pts',(-23.0972127196351,26.7410025985057,-9.27669682190857));
#37309=CARTESIAN_POINT('Ctrl Pts',(-23.0902333866196,26.7400035172467,-9.2771294821972));
#37310=CARTESIAN_POINT('Ctrl Pts',(-23.0868916618299,26.7395197935914,-9.27733685496387));
#37311=CARTESIAN_POINT('Ctrl Pts',(-23.0792728966128,26.7384047296838,-9.2778101324272));
#37312=CARTESIAN_POINT('Ctrl Pts',(-23.0749963606751,26.7377700337362,-9.27807614332407));
#37313=CARTESIAN_POINT('Ctrl Pts',(-23.0616750714806,26.7357655691576,-9.2789058664102));
#37314=CARTESIAN_POINT('Ctrl Pts',(-23.0526349239343,26.7343659028161,-9.27947052715836));
#37315=CARTESIAN_POINT('Ctrl Pts',(-22.9824787258578,26.7231977039833,-9.28386511231251));
#37316=CARTESIAN_POINT('Ctrl Pts',(-22.9216532304913,26.711709509106,-9.28774949674526));
#37317=CARTESIAN_POINT('Ctrl Pts',(-22.856311438363,26.6974081297277,-9.29200721751513));
#37318=CARTESIAN_POINT('Ctrl Pts',(-22.8514259926214,26.6963269216426,-9.29232607112002));
#37319=CARTESIAN_POINT('Ctrl Pts',(-22.8317451799987,26.6919232162596,-9.29361263621379));
#37320=CARTESIAN_POINT('Ctrl Pts',(-22.8169710086694,26.6885077316994,-9.2945831825999));
#37321=CARTESIAN_POINT('Ctrl Pts',(-22.7744183989526,26.6783535533502,-9.29739226507565));
#37322=CARTESIAN_POINT('Ctrl Pts',(-22.746705307041,26.6713495154611,-9.29923865653612));
#37323=CARTESIAN_POINT('Ctrl Pts',(-22.598495483465,26.6317871005532,-9.30920377958813));
#37324=CARTESIAN_POINT('Ctrl Pts',(-22.4798841145426,26.5926205362366,-9.31750789520908));
#37325=CARTESIAN_POINT('Ctrl Pts',(-22.2654847629832,26.5077315882893,-9.33303371024729));
#37326=CARTESIAN_POINT('Ctrl Pts',(-22.1690958172653,26.4639642817613,-9.34021715872359));
#37327=CARTESIAN_POINT('Ctrl Pts',(-22.075036015341,26.4155367745536,-9.34735996012824));
#37328=CARTESIAN_POINT('',(-26.7730021134982,23.5486107394123,-9.18577344932659));
#37329=CARTESIAN_POINT('Ctrl Pts',(-22.0750360153461,26.4155367745563,-9.59296972147339));
#37330=CARTESIAN_POINT('Ctrl Pts',(-22.1637577963692,26.4612159552698,-9.58679793631509));
#37331=CARTESIAN_POINT('Ctrl Pts',(-22.2544891503987,26.5027117903437,-9.58062615115677));
#37332=CARTESIAN_POINT('Ctrl Pts',(-22.346794125753,26.5398687993228,-9.57445436599846));
#37333=CARTESIAN_POINT('Ctrl Pts',(-22.3879140852554,26.5564214791603,-9.57170496321933));
#37334=CARTESIAN_POINT('Ctrl Pts',(-22.4293461334093,26.5721137747017,-9.56895556044019));
#37335=CARTESIAN_POINT('Ctrl Pts',(-22.4710509224819,26.5869351705575,-9.56620615766106));
#37336=CARTESIAN_POINT('Ctrl Pts',(-22.5646733514219,26.6202074903835,-9.56003406634873));
#37337=CARTESIAN_POINT('Ctrl Pts',(-22.6600008140785,26.6492047142014,-9.5538619750364));
#37338=CARTESIAN_POINT('Ctrl Pts',(-22.7566065109273,26.6737511400212,-9.54768988372408));
#37339=CARTESIAN_POINT('Ctrl Pts',(-22.8530813166075,26.6982643078607,-9.54152615498529));
#37340=CARTESIAN_POINT('Ctrl Pts',(-22.95083049687,26.7183385577121,-9.5353624262465));
#37341=CARTESIAN_POINT('Ctrl Pts',(-23.0494092502704,26.7338469735088,-9.52919869750771));
#37342=CARTESIAN_POINT('Ctrl Pts',(-23.1478835687336,26.7493389595945,-9.52304149866104));
#37343=CARTESIAN_POINT('Ctrl Pts',(-23.2471852863367,26.7602746610277,-9.51688429981437));
#37344=CARTESIAN_POINT('Ctrl Pts',(-23.3468574210034,26.7665777626755,-9.5107271009677));
#37345=CARTESIAN_POINT('Ctrl Pts',(-23.4464567013842,26.7728762571383,-9.50457440266));
#37346=CARTESIAN_POINT('Ctrl Pts',(-23.5464254283002,26.7745488567173,-9.4984217043523));
#37347=CARTESIAN_POINT('Ctrl Pts',(-23.6463003894648,26.7715709530114,-9.49226900604459));
#37348=CARTESIAN_POINT('Ctrl Pts',(-23.7461374779021,26.7685941785308,-9.48611864084884));
#37349=CARTESIAN_POINT('Ctrl Pts',(-23.8458804375116,26.7609704177089,-9.47996827565307));
#37350=CARTESIAN_POINT('Ctrl Pts',(-23.9450658330466,26.7487271712021,-9.47381791045731));
#37351=CARTESIAN_POINT('Ctrl Pts',(-24.0442401523507,26.7364852919231,-9.4676682320851));
#37352=CARTESIAN_POINT('Ctrl Pts',(-24.1428566002399,26.719625005791,-9.46151855371289));
#37353=CARTESIAN_POINT('Ctrl Pts',(-24.2404576488375,26.6982256031751,-9.45536887534068));
#37354=CARTESIAN_POINT('Ctrl Pts',(-24.3380739090803,26.676822865348,-9.44921823850822));
#37355=CARTESIAN_POINT('Ctrl Pts',(-24.4346740313327,26.6508796989122,-9.44306760167575));
#37356=CARTESIAN_POINT('Ctrl Pts',(-24.5298124422281,26.6205261260462,-9.43691696484329));
#37357=CARTESIAN_POINT('Ctrl Pts',(-24.6250526312376,26.5901400812334,-9.43075974812147));
#37358=CARTESIAN_POINT('Ctrl Pts',(-24.7188275716294,26.5553343404886,-9.42460253139967));
#37359=CARTESIAN_POINT('Ctrl Pts',(-24.8107086959699,26.5162882395776,-9.41844531467785));
#37360=CARTESIAN_POINT('Ctrl Pts',(-24.9026410804132,26.4772203550069,-9.41228466287005));
#37361=CARTESIAN_POINT('Ctrl Pts',(-24.9926771532215,26.4339075873789,-9.40612401106223));
#37362=CARTESIAN_POINT('Ctrl Pts',(-25.0804120134834,26.3865757718752,-9.39996335925443));
#37363=CARTESIAN_POINT('Ctrl Pts',(-25.1682936853654,26.3391647534127,-9.39379239848539));
#37364=CARTESIAN_POINT('Ctrl Pts',(-25.2538660804435,26.2877214773809,-9.38762143771638));
#37365=CARTESIAN_POINT('Ctrl Pts',(-25.3367522804116,26.2325157943761,-9.38145047694735));
#37366=CARTESIAN_POINT('Ctrl Pts',(-25.400020873111,26.1903762600016,-9.37674006672694));
#37367=CARTESIAN_POINT('Ctrl Pts',(-25.4617249171379,26.1460454492973,-9.37202965650652));
#37368=CARTESIAN_POINT('Ctrl Pts',(-25.5217103655992,26.0996586530556,-9.36731924628612));
#37369=CARTESIAN_POINT('Ctrl Pts',(-25.5994036959404,26.0395783373067,-9.36121830903075));
#37370=CARTESIAN_POINT('Ctrl Pts',(-25.6745002405137,25.9758253033282,-9.35511737177537));
#37371=CARTESIAN_POINT('Ctrl Pts',(-25.7466261173724,25.9086546675979,-9.34901643452001));
#37372=CARTESIAN_POINT('Ctrl Pts',(-25.8186539201148,25.8415753680292,-9.34292379309488));
#37373=CARTESIAN_POINT('Ctrl Pts',(-25.8877187567366,25.77108799903,-9.33683115166976));
#37374=CARTESIAN_POINT('Ctrl Pts',(-25.9534776244252,25.6974895275026,-9.33073851024463));
#37375=CARTESIAN_POINT('Ctrl Pts',(-26.0191620495435,25.623974373398,-9.32465276601684));
#37376=CARTESIAN_POINT('Ctrl Pts',(-26.0815476510511,25.547355448728,-9.31856702178908));
#37377=CARTESIAN_POINT('Ctrl Pts',(-26.1403272040665,25.4679675141761,-9.31248127756129));
#37378=CARTESIAN_POINT('Ctrl Pts',(-26.1990701315555,25.3886290462285,-9.30639932535937));
#37379=CARTESIAN_POINT('Ctrl Pts',(-26.2542112077898,25.3065253510947,-9.30031737315742));
#37380=CARTESIAN_POINT('Ctrl Pts',(-26.3054831090182,25.2220246538086,-9.2942354209555));
#37381=CARTESIAN_POINT('Ctrl Pts',(-26.3567375395523,25.1375527497956,-9.28815554115435));
#37382=CARTESIAN_POINT('Ctrl Pts',(-26.4041251830893,25.0506858464732,-9.28207566135319));
#37383=CARTESIAN_POINT('Ctrl Pts',(-26.4474223844702,24.9618205983017,-9.27599578155204));
#37384=CARTESIAN_POINT('Ctrl Pts',(-26.4907170569699,24.8729605405267,-9.26991625686144));
#37385=CARTESIAN_POINT('Ctrl Pts',(-26.5299215681555,24.7821027708259,-9.26383673217088));
#37386=CARTESIAN_POINT('Ctrl Pts',(-26.5648590466163,24.6896669087711,-9.25775720748028));
#37387=CARTESIAN_POINT('Ctrl Pts',(-26.5998254795955,24.5971544402755,-9.25167264436913));
#37388=CARTESIAN_POINT('Ctrl Pts',(-26.6305176570152,24.5030616840487,-9.24558808125795));
#37389=CARTESIAN_POINT('Ctrl Pts',(-26.6568076885387,24.4078262136498,-9.23950351814679));
#37390=CARTESIAN_POINT('Ctrl Pts',(-26.6831081413057,24.312552992363,-9.23341654314373));
#37391=CARTESIAN_POINT('Ctrl Pts',(-26.7050028737611,24.2161365894468,-9.22732956814067));
#37392=CARTESIAN_POINT('Ctrl Pts',(-26.7224150143323,24.1190255499041,-9.2212425931376));
#37393=CARTESIAN_POINT('Ctrl Pts',(-26.739854639304,24.0217612242846,-9.21514601007636));
#37394=CARTESIAN_POINT('Ctrl Pts',(-26.7527974776387,23.9238005137262,-9.20904942701514));
#37395=CARTESIAN_POINT('Ctrl Pts',(-26.7612185047024,23.8255979196766,-9.2029528439539));
#37396=CARTESIAN_POINT('Ctrl Pts',(-26.7691282986336,23.7333571185777,-9.19722637907812));
#37397=CARTESIAN_POINT('Ctrl Pts',(-26.7730491308417,23.6409032453324,-9.19149991420236));
#37398=CARTESIAN_POINT('Ctrl Pts',(-26.7730021134982,23.5486107394123,-9.18577344932659));
#37399=CARTESIAN_POINT('Ctrl Pts',(-26.7730021922999,23.5487734894733,-9.18330474046535));
#37400=CARTESIAN_POINT('Ctrl Pts',(-26.7729649266428,23.4675737224467,-9.17795163051465));
#37401=CARTESIAN_POINT('Ctrl Pts',(-26.7698588128614,23.3863948059531,-9.17269397152322));
#37402=CARTESIAN_POINT('Ctrl Pts',(-26.7633169126019,23.3005351682824,-9.16729179848125));
#37403=CARTESIAN_POINT('Ctrl Pts',(-26.7629342824696,23.2956598247637,-9.16698559405237));
#37404=CARTESIAN_POINT('Ctrl Pts',(-26.7623102620737,23.2879342499821,-9.16650126107428));
#37405=CARTESIAN_POINT('Ctrl Pts',(-26.7620761738631,23.2850834611615,-9.16632273006705));
#37406=CARTESIAN_POINT('Ctrl Pts',(-26.7616705729007,23.2802232849545,-9.1660186911729));
#37407=CARTESIAN_POINT('Ctrl Pts',(-26.7615009694366,23.2782137465336,-9.16589307641493));
#37408=CARTESIAN_POINT('Ctrl Pts',(-26.761180922018,23.2744636872304,-9.16565884438339));
#37409=CARTESIAN_POINT('Ctrl Pts',(-26.7610309489815,23.2727231285041,-9.16555020048642));
#37410=CARTESIAN_POINT('Ctrl Pts',(-26.7607160796995,23.2691032323758,-9.16532440321754));
#37411=CARTESIAN_POINT('Ctrl Pts',(-26.7605509489693,23.2672239224816,-9.16520726401055));
#37412=CARTESIAN_POINT('Ctrl Pts',(-26.7601674312223,23.2629027261268,-9.16493811570678));
#37413=CARTESIAN_POINT('Ctrl Pts',(-26.7599479073948,23.2604609371394,-9.16478617129267));
#37414=CARTESIAN_POINT('Ctrl Pts',(-26.7592423597792,23.2527122058869,-9.1643044434345));
#37415=CARTESIAN_POINT('Ctrl Pts',(-26.7587459556855,23.2474061821959,-9.1639752452407));
#37416=CARTESIAN_POINT('Ctrl Pts',(-26.7544055259695,23.2022204741573,-9.16117733973073));
#37417=CARTESIAN_POINT('Ctrl Pts',(-26.7498310951871,23.1624122281876,-9.15874905338377));
#37418=CARTESIAN_POINT('Ctrl Pts',(-26.7435922082235,23.1158015235292,-9.15593805988852));
#37419=CARTESIAN_POINT('Ctrl Pts',(-26.7426468465274,23.1089085519481,-9.1555231895877));
#37420=CARTESIAN_POINT('Ctrl Pts',(-26.7403632336336,23.0926492215005,-9.15454642879065));
#37421=CARTESIAN_POINT('Ctrl Pts',(-26.739006036729,23.0832855434019,-9.15398536417351));
#37422=CARTESIAN_POINT('Ctrl Pts',(-26.7347395263774,23.0547359327775,-9.15227874412316));
#37423=CARTESIAN_POINT('Ctrl Pts',(-26.7316981041866,23.0355698926794,-9.15113863751684));
#37424=CARTESIAN_POINT('Ctrl Pts',(-26.7264224409202,23.0041599339501,-9.14927767978094));
#37425=CARTESIAN_POINT('Ctrl Pts',(-26.7242901010063,22.9918996564146,-9.14855316945212));
#37426=CARTESIAN_POINT('Ctrl Pts',(-26.6687491844894,22.6831608109983,-9.13034912425828));
#37427=CARTESIAN_POINT('Ctrl Pts',(-26.574104119805,22.3956005397989,-9.11419674428456));
#37428=CARTESIAN_POINT('Ctrl Pts',(-26.4044584708247,22.0514481553201,-9.09205387220421));
#37429=CARTESIAN_POINT('Ctrl Pts',(-26.365211361839,21.9789755759874,-9.08722616546257));
#37430=CARTESIAN_POINT('Ctrl Pts',(-26.3014680966286,21.8713377242562,-9.07974840919229));
#37431=CARTESIAN_POINT('Ctrl Pts',(-26.278975578972,21.8350230194398,-9.0771701361137));
#37432=CARTESIAN_POINT('Ctrl Pts',(-26.2516358852398,21.7927817935061,-9.07410109388587));
#37433=CARTESIAN_POINT('Ctrl Pts',(-26.2474804236841,21.7864109527796,-9.07363631364378));
#37434=CARTESIAN_POINT('Ctrl Pts',(-26.2410751656187,21.7766664588255,-9.07292245884629));
#37435=CARTESIAN_POINT('Ctrl Pts',(-26.2388414710478,21.77328221116,-9.07267398967577));
#37436=CARTESIAN_POINT('Ctrl Pts',(-26.2349335340921,21.7673855728142,-9.07224010058451));
#37437=CARTESIAN_POINT('Ctrl Pts',(-26.2332621336659,21.7648712969623,-9.07205478796363));
#37438=CARTESIAN_POINT('Ctrl Pts',(-26.2294935717123,21.7592195185919,-9.07163753711554));
#37439=CARTESIAN_POINT('Ctrl Pts',(-26.2273944299449,21.7560833476492,-9.0714055242391));
#37440=CARTESIAN_POINT('Ctrl Pts',(-26.2217620660332,21.7477003456505,-9.07078406090117));
#37441=CARTESIAN_POINT('Ctrl Pts',(-26.2182189099997,21.7424602375427,-9.07039423440136));
#37442=CARTESIAN_POINT('Ctrl Pts',(-26.202851021567,21.719875666319,-9.06870819765479));
#37443=CARTESIAN_POINT('Ctrl Pts',(-26.1908726219754,21.7026368457372,-9.06740614724789));
#37444=CARTESIAN_POINT('Ctrl Pts',(-25.9737854548101,21.3966374588687,-9.04401825098519));
#37445=CARTESIAN_POINT('Ctrl Pts',(-25.7226547628741,21.1435739184067,-9.01985039402449));
#37446=CARTESIAN_POINT('Ctrl Pts',(-25.3900387374496,20.9036598339824,-8.99229640199206));
#37447=CARTESIAN_POINT('Ctrl Pts',(-25.343677956174,20.872027012824,-8.98854996608669));
#37448=CARTESIAN_POINT('Ctrl Pts',(-25.2460959987815,20.8091157424671,-8.98088864145837));
#37449=CARTESIAN_POINT('Ctrl Pts',(-25.1947775592959,20.7780233945862,-8.97698133965448));
#37450=CARTESIAN_POINT('Ctrl Pts',(-25.1267771519296,20.7393772849319,-8.97198858415305));
#37451=CARTESIAN_POINT('Ctrl Pts',(-25.1108601166761,20.7305090093033,-8.97083278581258));
#37452=CARTESIAN_POINT('Ctrl Pts',(-25.0883189643709,20.7181994077409,-8.96921495456499));
#37453=CARTESIAN_POINT('Ctrl Pts',(-25.0817571402663,20.7146455623265,-8.96874624401838));
#37454=CARTESIAN_POINT('Ctrl Pts',(-25.0702870907136,20.7084848799883,-8.9679309312077));
#37455=CARTESIAN_POINT('Ctrl Pts',(-25.0653843883001,20.7058679049089,-8.96758370437275));
#37456=CARTESIAN_POINT('Ctrl Pts',(-25.0582540130377,20.702085504463,-8.96708057006287));
#37457=CARTESIAN_POINT('Ctrl Pts',(-25.0560317416068,20.7009100015937,-8.96692402421141));
#37458=CARTESIAN_POINT('Ctrl Pts',(-25.0522399119569,20.6989099329514,-8.9666573622799));
#37459=CARTESIAN_POINT('Ctrl Pts',(-25.0506710473117,20.6980840612277,-8.96654716242713));
#37460=CARTESIAN_POINT('Ctrl Pts',(-25.0475485934068,20.6964436482609,-8.96632809766881));
#37461=CARTESIAN_POINT('Ctrl Pts',(-25.0459950223811,20.6956290817145,-8.96621923114136));
#37462=CARTESIAN_POINT('Ctrl Pts',(-25.042333267798,20.6937129647931,-8.96596293492282));
#37463=CARTESIAN_POINT('Ctrl Pts',(-25.0402245247658,20.6926124773362,-8.96581557329073));
#37464=CARTESIAN_POINT('Ctrl Pts',(-25.0339914062557,20.6893683816372,-8.96538068336349));
#37465=CARTESIAN_POINT('Ctrl Pts',(-25.029863586841,20.6872313487374,-8.96509357111276));
#37466=CARTESIAN_POINT('Ctrl Pts',(-24.9938442019695,20.6686822868985,-8.96259584311043));
#37467=CARTESIAN_POINT('Ctrl Pts',(-24.9616837346014,20.6527939541939,-8.96041767060814));
#37468=CARTESIAN_POINT('Ctrl Pts',(-24.9207730841527,20.6334256232266,-8.95770351342188));
#37469=CARTESIAN_POINT('Ctrl Pts',(-24.9122654365868,20.6294432860069,-8.9571421401036));
#37470=CARTESIAN_POINT('Ctrl Pts',(-24.9001979581806,20.6238588219682,-8.95635001941079));
#37471=CARTESIAN_POINT('Ctrl Pts',(-24.8966525242109,20.6222259165062,-8.95611779853653));
#37472=CARTESIAN_POINT('Ctrl Pts',(-24.8906626029107,20.6194803438804,-8.95572630425528));
#37473=CARTESIAN_POINT('Ctrl Pts',(-24.8882196842982,20.6183642878274,-8.95556687249244));
#37474=CARTESIAN_POINT('Ctrl Pts',(-24.8727428252294,20.6113170018099,-8.95455827579723));
#37475=CARTESIAN_POINT('Ctrl Pts',(-24.8596706704911,20.6054695556475,-8.95371297050655));
#37476=CARTESIAN_POINT('Ctrl Pts',(-24.7046465692939,20.5373604476481,-8.94376106003376));
#37477=CARTESIAN_POINT('Ctrl Pts',(-24.5584067237617,20.4853254409156,-8.93508396744657));
#37478=CARTESIAN_POINT('Ctrl Pts',(-24.3920097949483,20.4393246630043,-8.92543455881836));
#37479=CARTESIAN_POINT('Ctrl Pts',(-24.3750032243837,20.4347728270614,-8.92445097898462));
#37480=CARTESIAN_POINT('Ctrl Pts',(-24.338385557134,20.4252928927794,-8.92233748122336));
#37481=CARTESIAN_POINT('Ctrl Pts',(-24.3187636758423,20.4204095596233,-8.92120757663564));
#37482=CARTESIAN_POINT('Ctrl Pts',(-24.2761361980358,20.410225818253,-8.91875661257138));
#37483=CARTESIAN_POINT('Ctrl Pts',(-24.2531157422147,20.4049928990619,-8.91743531402306));
#37484=CARTESIAN_POINT('Ctrl Pts',(-24.2024403855555,20.3940577067689,-8.91452871945726));
#37485=CARTESIAN_POINT('Ctrl Pts',(-24.1747639545671,20.3884650266642,-8.91294257605036));
#37486=CARTESIAN_POINT('Ctrl Pts',(-24.1124570050957,20.3767244391647,-8.90936962071323));
#37487=CARTESIAN_POINT('Ctrl Pts',(-24.0777924086686,20.3707783564588,-8.90738032007583));
#37488=CARTESIAN_POINT('Ctrl Pts',(-23.8808558805949,20.3403067809584,-8.89604786125396));
#37489=CARTESIAN_POINT('Ctrl Pts',(-23.7170172113642,20.3276405363788,-8.88648452576365));
#37490=CARTESIAN_POINT('Ctrl Pts',(-23.5424676569154,20.3274949155151,-8.87586075863551));
#37491=CARTESIAN_POINT('Ctrl Pts',(-23.5319942686975,20.327537234204,-8.8752217168117));
#37492=CARTESIAN_POINT('Ctrl Pts',(-23.5169019141914,20.3276717895139,-8.87429849408435));
#37493=CARTESIAN_POINT('Ctrl Pts',(-23.5122825724061,20.3277229064775,-8.87401560439957));
#37494=CARTESIAN_POINT('Ctrl Pts',(-23.5042518243662,20.3278290433645,-8.87352324180883));
#37495=CARTESIAN_POINT('Ctrl Pts',(-23.5008403574974,20.3278795489205,-8.8733139109486));
#37496=CARTESIAN_POINT('Ctrl Pts',(-23.4942710364588,20.3279872400047,-8.87291047184784));
#37497=CARTESIAN_POINT('Ctrl Pts',(-23.491113171878,20.3280436505325,-8.87271638817393));
#37498=CARTESIAN_POINT('Ctrl Pts',(-23.4836590482543,20.3281877688383,-8.87225789589132));
#37499=CARTESIAN_POINT('Ctrl Pts',(-23.4793628789961,20.328279427378,-8.87199336344817));
#37500=CARTESIAN_POINT('Ctrl Pts',(-23.4644339130206,20.3286278096574,-8.87107314097701));
#37501=CARTESIAN_POINT('Ctrl Pts',(-23.4538023014709,20.3289285750448,-8.8704160693096));
#37502=CARTESIAN_POINT('Ctrl Pts',(-23.3248658067932,20.3332150243829,-8.8624258434317));
#37503=CARTESIAN_POINT('Ctrl Pts',(-23.2068800103227,20.343662610776,-8.85488955474929));
#37504=CARTESIAN_POINT('Ctrl Pts',(-22.8190818270482,20.399650403051,-8.82933627767633));
#37505=CARTESIAN_POINT('Ctrl Pts',(-22.5545049586475,20.4730207294435,-8.81052096007095));
#37506=CARTESIAN_POINT('Ctrl Pts',(-22.2389584925178,20.6055345853877,-8.78767410165781));
#37507=CARTESIAN_POINT('Ctrl Pts',(-22.1763585486276,20.6342154297348,-8.78312788799295));
#37508=CARTESIAN_POINT('Ctrl Pts',(-22.0934938065402,20.6754423225323,-8.77713375490202));
#37509=CARTESIAN_POINT('Ctrl Pts',(-22.0723825397473,20.6862378532114,-8.77560881045344));
#37510=CARTESIAN_POINT('Ctrl Pts',(-22.0357566163987,20.7054798495902,-8.7729694239255));
#37511=CARTESIAN_POINT('Ctrl Pts',(-22.0201889132558,20.7138225843706,-8.77184955930556));
#37512=CARTESIAN_POINT('Ctrl Pts',(-21.9982907497336,20.7257905696615,-8.77027798104856));
#37513=CARTESIAN_POINT('Ctrl Pts',(-21.99190313113,20.7293097999446,-8.76982000190449));
#37514=CARTESIAN_POINT('Ctrl Pts',(-21.982200691393,20.7346983287807,-8.76912509926341));
#37515=CARTESIAN_POINT('Ctrl Pts',(-21.9788771960467,20.7365518371841,-8.76888719883389));
#37516=CARTESIAN_POINT('Ctrl Pts',(-21.9727505856843,20.7399828793852,-8.76844890443323));
#37517=CARTESIAN_POINT('Ctrl Pts',(-21.9699465398368,20.741558728399,-8.76824840407281));
#37518=CARTESIAN_POINT('Ctrl Pts',(-21.9653888494244,20.7441290961766,-8.76792267924017));
#37519=CARTESIAN_POINT('Ctrl Pts',(-21.9636337793284,20.7451210621488,-8.76779729011604));
#37520=CARTESIAN_POINT('Ctrl Pts',(-21.9602399627658,20.7470434520324,-8.76755490284713));
#37521=CARTESIAN_POINT('Ctrl Pts',(-21.9586011065491,20.7479736636127,-8.7674378918529));
#37522=CARTESIAN_POINT('Ctrl Pts',(-21.9548440797919,20.7501105037488,-8.76716973002253));
#37523=CARTESIAN_POINT('Ctrl Pts',(-21.9527264569436,20.7513181012987,-8.7670186423069));
#37524=CARTESIAN_POINT('Ctrl Pts',(-21.9460476718936,20.7551368002395,-8.76654230830306));
#37525=CARTESIAN_POINT('Ctrl Pts',(-21.9414914958475,20.7577566740606,-8.76621762880174));
#37526=CARTESIAN_POINT('Ctrl Pts',(-21.9039093894471,20.7794894900426,-8.7635415280146));
#37527=CARTESIAN_POINT('Ctrl Pts',(-21.8712171353014,20.7991774642645,-8.76122673372378));
#37528=CARTESIAN_POINT('Ctrl Pts',(-21.8358320149225,20.8213529736959,-8.75872702475207));
#37529=CARTESIAN_POINT('Ctrl Pts',(-21.832786674081,20.8232685687535,-8.75851194021225));
#37530=CARTESIAN_POINT('Ctrl Pts',(-21.5974611074795,20.9718447595649,-8.74189465095875));
#37531=CARTESIAN_POINT('Ctrl Pts',(-21.3848504492797,21.1476168511753,-8.72704117392225));
#37532=CARTESIAN_POINT('Ctrl Pts',(-21.17094083591,21.3762104220449,-8.7093772359835));
#37533=CARTESIAN_POINT('Ctrl Pts',(-21.1452832006768,21.4046277603611,-8.70720780803039));
#37534=CARTESIAN_POINT('Ctrl Pts',(-21.0477981627449,21.5165441077007,-8.69874533626598));
#37535=CARTESIAN_POINT('Ctrl Pts',(-20.9797689921945,21.6032397648594,-8.69235779787456));
#37536=CARTESIAN_POINT('Ctrl Pts',(-20.8879039828806,21.7335387954449,-8.68285902140014));
#37537=CARTESIAN_POINT('Ctrl Pts',(-20.8604229900186,21.7744808053182,-8.6798884549838));
#37538=CARTESIAN_POINT('Ctrl Pts',(-20.8296407511343,21.8226960066454,-8.67640018374703));
#37539=CARTESIAN_POINT('Ctrl Pts',(-20.825412967101,21.8293721310754,-8.67591740191258));
#37540=CARTESIAN_POINT('Ctrl Pts',(-20.8190196150783,21.8395505492243,-8.67518166370546));
#37541=CARTESIAN_POINT('Ctrl Pts',(-20.8168361135681,21.8430415891038,-8.67492937227818));
#37542=CARTESIAN_POINT('Ctrl Pts',(-20.8130596050866,21.8491053887934,-8.67449124392545));
#37543=CARTESIAN_POINT('Ctrl Pts',(-20.8114635163459,21.8516762312068,-8.67430552118253));
#37544=CARTESIAN_POINT('Ctrl Pts',(-20.8081528405154,21.8570255811424,-8.67391913113606));
#37545=CARTESIAN_POINT('Ctrl Pts',(-20.8064388508895,21.8598044528305,-8.67371844207044));
#37546=CARTESIAN_POINT('Ctrl Pts',(-20.8022705686145,21.8665854820809,-8.67322879453893));
#37547=CARTESIAN_POINT('Ctrl Pts',(-20.7998207978715,21.8705903988286,-8.67293967001375));
#37548=CARTESIAN_POINT('Ctrl Pts',(-20.7905727563062,21.885783698563,-8.67184306086649));
#37549=CARTESIAN_POINT('Ctrl Pts',(-20.7838340048356,21.8970079988815,-8.67103339671671));
#37550=CARTESIAN_POINT('Ctrl Pts',(-20.7752603920573,21.9114877085041,-8.66998943357831));
#37551=CARTESIAN_POINT('Ctrl Pts',(-20.773362472356,21.9147057977453,-8.66975744816343));
#37552=CARTESIAN_POINT('Ctrl Pts',(-20.6470196179209,22.1297850367443,-8.65425498018703));
#37553=CARTESIAN_POINT('Ctrl Pts',(-20.5472322348576,22.3551332982661,-8.63805520786541));
#37554=CARTESIAN_POINT('Ctrl Pts',(-20.4260600444248,22.7431450255997,-8.610610334163));
#37555=CARTESIAN_POINT('Ctrl Pts',(-20.3896676012117,22.9000934431723,-8.59964691034359));
#37556=CARTESIAN_POINT('Ctrl Pts',(-20.3547623498811,23.1264556237512,-8.58447374104671));
#37557=CARTESIAN_POINT('Ctrl Pts',(-20.3465150117206,23.1941224702675,-8.58001965843767));
#37558=CARTESIAN_POINT('Ctrl Pts',(-20.3387039558049,23.281103825335,-8.57443927157725));
#37559=CARTESIAN_POINT('Ctrl Pts',(-20.3371592757012,23.3002184327026,-8.57322190673327));
#37560=CARTESIAN_POINT('Ctrl Pts',(-20.3352300448756,23.3270754254476,-8.57152507317009));
#37561=CARTESIAN_POINT('Ctrl Pts',(-20.3347027012597,23.3348067093109,-8.57103819179324));
#37562=CARTESIAN_POINT('Ctrl Pts',(-20.333946910245,23.3465087482352,-8.57030372265756));
#37563=CARTESIAN_POINT('Ctrl Pts',(-20.3336979232892,23.3504780803416,-8.57005502096063));
#37564=CARTESIAN_POINT('Ctrl Pts',(-20.3332537264107,23.3577756133679,-8.569598591661));
#37565=CARTESIAN_POINT('Ctrl Pts',(-20.3330563323339,23.3611036687701,-8.56939074321588));
#37566=CARTESIAN_POINT('Ctrl Pts',(-20.3327463020616,23.3664716871997,-8.56905599391635));
#37567=CARTESIAN_POINT('Ctrl Pts',(-20.3326304414011,23.3685114503679,-8.56892891124367));
#37568=CARTESIAN_POINT('Ctrl Pts',(-20.332411856029,23.3724254476783,-8.56868528475797));
#37569=CARTESIAN_POINT('Ctrl Pts',(-20.3323088298298,23.3742996475945,-8.56856872495959));
#37570=CARTESIAN_POINT('Ctrl Pts',(-20.3320764925918,23.3785946717369,-8.56830183675906));
#37571=CARTESIAN_POINT('Ctrl Pts',(-20.3319482758093,23.3810155493771,-8.5681515710246));
#37572=CARTESIAN_POINT('Ctrl Pts',(-20.3316204993157,23.3873394386585,-8.56775946799688));
#37573=CARTESIAN_POINT('Ctrl Pts',(-20.3314253065119,23.3912426875247,-8.56751787649659));
#37574=CARTESIAN_POINT('Ctrl Pts',(-20.3302409229788,23.4158229306692,-8.56599909490031));
#37575=CARTESIAN_POINT('Ctrl Pts',(-20.3294438425893,23.4365093157595,-8.56473254664616));
#37576=CARTESIAN_POINT('Ctrl Pts',(-20.3185429121785,23.8139015320953,-8.54181511589748));
#37577=CARTESIAN_POINT('Ctrl Pts',(-20.3675489362896,24.1698974975159,-8.5230433003129));
#37578=CARTESIAN_POINT('Ctrl Pts',(-20.5140220449611,24.6390657404455,-8.49482237236206));
#37579=CARTESIAN_POINT('Ctrl Pts',(-20.5621006297161,24.7648104456572,-8.48691579698403));
#37580=CARTESIAN_POINT('Ctrl Pts',(-20.6222434830932,24.8967259915526,-8.47809196986474));
#37581=CARTESIAN_POINT('Ctrl Pts',(-20.6266449914798,24.9062564820922,-8.47745145180394));
#37582=CARTESIAN_POINT('Ctrl Pts',(-20.6330521925172,24.919953639674,-8.47652647867717));
#37583=CARTESIAN_POINT('Ctrl Pts',(-20.6350204434143,24.9241378308387,-8.47624332168835));
#37584=CARTESIAN_POINT('Ctrl Pts',(-20.6384569330991,24.9314026322919,-8.47575064549745));
#37585=CARTESIAN_POINT('Ctrl Pts',(-20.6399210762166,24.9344851810315,-8.47554126885818));
#37586=CARTESIAN_POINT('Ctrl Pts',(-20.6427492535757,24.9404151908375,-8.4751378495098));
#37587=CARTESIAN_POINT('Ctrl Pts',(-20.6441125822772,24.9432629858655,-8.47494383154049));
#37588=CARTESIAN_POINT('Ctrl Pts',(-20.6473395078644,24.9499782078909,-8.47448566046984));
#37589=CARTESIAN_POINT('Ctrl Pts',(-20.6492066487092,24.9538439170566,-8.47422138395562));
#37590=CARTESIAN_POINT('Ctrl Pts',(-20.6557160464583,24.9672524307703,-8.47330289073489));
#37591=CARTESIAN_POINT('Ctrl Pts',(-20.6603976715419,24.9767759494027,-8.47264729926198));
#37592=CARTESIAN_POINT('Ctrl Pts',(-20.7173638708062,25.0912271931706,-8.46472924671945));
#37593=CARTESIAN_POINT('Ctrl Pts',(-20.7752828837738,25.193237254939,-8.45726761195228));
#37594=CARTESIAN_POINT('Ctrl Pts',(-20.9532991613371,25.4704036605692,-8.43579394209326));
#37595=CARTESIAN_POINT('Ctrl Pts',(-21.0853186879591,25.6371710089734,-8.42139094525753));
#37596=CARTESIAN_POINT('Ctrl Pts',(-21.307130334386,25.8667108106903,-8.39981710513638));
#37597=CARTESIAN_POINT('Ctrl Pts',(-21.3853093310627,25.9399386835752,-8.39262118884812));
#37598=CARTESIAN_POINT('Ctrl Pts',(-21.5171575050814,26.0516451680143,-8.38128579137249));
#37599=CARTESIAN_POINT('Ctrl Pts',(-21.5686159624712,26.0926054699292,-8.37704142669657));
#37600=CARTESIAN_POINT('Ctrl Pts',(-21.6269998832273,26.1362276889279,-8.37245287315672));
#37601=CARTESIAN_POINT('Ctrl Pts',(-21.632718198057,26.1404707358687,-8.37200580361167));
#37602=CARTESIAN_POINT('Ctrl Pts',(-21.6414613784863,26.1469134419703,-8.37132587728777));
#37603=CARTESIAN_POINT('Ctrl Pts',(-21.6444760429572,26.1491268119993,-8.37109209300309));
#37604=CARTESIAN_POINT('Ctrl Pts',(-21.6494178719409,26.152741885631,-8.37070994024614));
#37605=CARTESIAN_POINT('Ctrl Pts',(-21.6513427398438,26.1541467007375,-8.37056135755736));
#37606=CARTESIAN_POINT('Ctrl Pts',(-21.6549895370837,26.1568020272018,-8.37028036656029));
#37607=CARTESIAN_POINT('Ctrl Pts',(-21.6567111488156,26.158052969354,-8.37014792828654));
#37608=CARTESIAN_POINT('Ctrl Pts',(-21.65991505099,26.1603761146527,-8.36990186237836));
#37609=CARTESIAN_POINT('Ctrl Pts',(-21.6613970114198,26.1614487581109,-8.36978820408598));
#37610=CARTESIAN_POINT('Ctrl Pts',(-21.664400019948,26.1636184424435,-8.3695582120069));
#37611=CARTESIAN_POINT('Ctrl Pts',(-21.665921106489,26.1647154133497,-8.36944188313231));
#37612=CARTESIAN_POINT('Ctrl Pts',(-21.6702401852203,26.1678245014663,-8.36911204151877));
#37613=CARTESIAN_POINT('Ctrl Pts',(-21.6730404594887,26.1698334668937,-8.36889874852059));
#37614=CARTESIAN_POINT('Ctrl Pts',(-21.6848447517796,26.1782734232808,-8.36800196147861));
#37615=CARTESIAN_POINT('Ctrl Pts',(-21.6938787745485,26.18466261256,-8.36732133145051));
#37616=CARTESIAN_POINT('Ctrl Pts',(-21.8217959020194,26.2741455027789,-8.35776127910911));
#37617=CARTESIAN_POINT('Ctrl Pts',(-21.9461104232022,26.34915831371,-8.3494057343621));
#37618=CARTESIAN_POINT('Ctrl Pts',(-22.0750360458934,26.4155367902838,-8.34120882940695));
#37619=CARTESIAN_POINT('Origin',(-23.5502525316942,23.5502525316942,-77.3107734492734));
#37620=CARTESIAN_POINT('',(-22.075035924178,26.4155367276176,-6.84592209196326));
#37621=CARTESIAN_POINT('',(-22.075036226743,26.4155368833958,-7.0956801988874));
#37622=CARTESIAN_POINT('',(-22.0750360153461,26.4155367745563,-77.3107734492734));
#37623=CARTESIAN_POINT('Ctrl Pts',(-22.075035924178,26.4155367276176,-6.84592209196326));
#37624=CARTESIAN_POINT('Ctrl Pts',(-22.0197506382596,26.3870726150335,-6.84940421266326));
#37625=CARTESIAN_POINT('Ctrl Pts',(-21.9652843228088,26.3570059330645,-6.85289943478171));
#37626=CARTESIAN_POINT('Ctrl Pts',(-21.8038988509854,26.2617172186274,-6.86352482352683));
#37627=CARTESIAN_POINT('Ctrl Pts',(-21.6999020120603,26.1918410910454,-6.87074395872825));
#37628=CARTESIAN_POINT('Ctrl Pts',(-21.572290617936,26.0948579079331,-6.88027526220047));
#37629=CARTESIAN_POINT('Ctrl Pts',(-21.5446917621018,26.0731626981938,-6.88237931436025));
#37630=CARTESIAN_POINT('Ctrl Pts',(-21.5007550814826,26.0374479098907,-6.88580194001471));
#37631=CARTESIAN_POINT('Ctrl Pts',(-21.4841932801137,26.0237075609599,-6.88710931998957));
#37632=CARTESIAN_POINT('Ctrl Pts',(-21.4643247682997,26.0068850468856,-6.888699210864));
#37633=CARTESIAN_POINT('Ctrl Pts',(-21.4608850527187,26.0039602335748,-6.88897524716701));
#37634=CARTESIAN_POINT('Ctrl Pts',(-21.4542504303379,25.9982947030201,-6.88950920555597));
#37635=CARTESIAN_POINT('Ctrl Pts',(-21.4510547227587,25.9955549342969,-6.88976708820377));
#37636=CARTESIAN_POINT('Ctrl Pts',(-21.4455620125885,25.9908271791084,-6.8902115255778));
#37637=CARTESIAN_POINT('Ctrl Pts',(-21.4432624306481,25.9888421865571,-6.89039795599639));
#37638=CARTESIAN_POINT('Ctrl Pts',(-21.4385269923097,25.9847428710865,-6.89078261380928));
#37639=CARTESIAN_POINT('Ctrl Pts',(-21.4360914972207,25.982628137245,-6.8909808581898));
#37640=CARTESIAN_POINT('Ctrl Pts',(-21.4295321007336,25.9769153366405,-6.89151588988145));
#37641=CARTESIAN_POINT('Ctrl Pts',(-21.4254141969134,25.9733104273415,-6.89185296248503));
#37642=CARTESIAN_POINT('Ctrl Pts',(-21.4102843447907,25.9599971731114,-6.89309581957962));
#37643=CARTESIAN_POINT('Ctrl Pts',(-21.399329716625,25.9502242210989,-6.89400431104689));
#37644=CARTESIAN_POINT('Ctrl Pts',(-21.2139024053876,25.7825096665218,-6.90953118559948));
#37645=CARTESIAN_POINT('Ctrl Pts',(-21.0572171822121,25.6060335685424,-6.92499416384261));
#37646=CARTESIAN_POINT('Ctrl Pts',(-20.8157582651171,25.2654413734203,-6.95313835147831));
#37647=CARTESIAN_POINT('Ctrl Pts',(-20.7231559656683,25.1080907292221,-6.96558853688841));
#37648=CARTESIAN_POINT('Ctrl Pts',(-20.6183177297916,24.8894688417338,-6.98158933334656));
#37649=CARTESIAN_POINT('Ctrl Pts',(-20.5938104608102,24.8344617404839,-6.98551108119075));
#37650=CARTESIAN_POINT('Ctrl Pts',(-20.5603612115512,24.7533425272335,-6.99111226674759));
#37651=CARTESIAN_POINT('Ctrl Pts',(-20.5501914478024,24.7277538103183,-6.99285326781846));
#37652=CARTESIAN_POINT('Ctrl Pts',(-20.5387792108028,24.6979307657937,-6.99484990377457));
#37653=CARTESIAN_POINT('Ctrl Pts',(-20.537216340677,24.6938214205829,-6.99512431197436));
#37654=CARTESIAN_POINT('Ctrl Pts',(-20.5348451523088,24.6875481110061,-6.99554212578306));
#37655=CARTESIAN_POINT('Ctrl Pts',(-20.5340307513058,24.6853864753176,-6.99568589634604));
#37656=CARTESIAN_POINT('Ctrl Pts',(-20.5326255826229,24.6816445967516,-6.99593442365807));
#37657=CARTESIAN_POINT('Ctrl Pts',(-20.5320337327216,24.6800647684011,-6.9960392458678));
#37658=CARTESIAN_POINT('Ctrl Pts',(-20.5308020361722,24.6767691187852,-6.99625769101337));
#37659=CARTESIAN_POINT('Ctrl Pts',(-20.530162413194,24.6750532216286,-6.99637130018789));
#37660=CARTESIAN_POINT('Ctrl Pts',(-20.5283994701698,24.6703114830802,-6.99668490570288));
#37661=CARTESIAN_POINT('Ctrl Pts',(-20.5272792287174,24.6672844872493,-6.99688471620227));
#37662=CARTESIAN_POINT('Ctrl Pts',(-20.5229148609401,24.6554369128365,-6.99766527596204));
#37663=CARTESIAN_POINT('Ctrl Pts',(-20.5197047355893,24.6466037298956,-6.99824400337414));
#37664=CARTESIAN_POINT('Ctrl Pts',(-20.4664739988406,24.4981103754237,-7.00792072266327));
#37665=CARTESIAN_POINT('Ctrl Pts',(-20.426109069612,24.355153085545,-7.01646644584718));
#37666=CARTESIAN_POINT('Ctrl Pts',(-20.3557668695526,24.0187701365367,-7.03588540385704));
#37667=CARTESIAN_POINT('Ctrl Pts',(-20.3332521300111,23.824400750828,-7.04661858973753));
#37668=CARTESIAN_POINT('Ctrl Pts',(-20.3266296876275,23.5540997883859,-7.06201081572699));
#37669=CARTESIAN_POINT('Ctrl Pts',(-20.3274156543961,23.4789750112605,-7.06633481668244));
#37670=CARTESIAN_POINT('Ctrl Pts',(-20.3347504468316,23.3175715008311,-7.07579181989363));
#37671=CARTESIAN_POINT('Ctrl Pts',(-20.3421501523385,23.2313933673544,-7.08094463815676));
#37672=CARTESIAN_POINT('Ctrl Pts',(-20.3542178895786,23.1360382679982,-7.08679761800651));
#37673=CARTESIAN_POINT('Ctrl Pts',(-20.3554738983943,23.12645969213,-7.08738725065456));
#37674=CARTESIAN_POINT('Ctrl Pts',(-20.3573806062749,23.1124091225686,-7.08825469845875));
#37675=CARTESIAN_POINT('Ctrl Pts',(-20.3579976824625,23.1079325567065,-7.08853144814527));
#37676=CARTESIAN_POINT('Ctrl Pts',(-20.3590948388877,23.1000951504755,-7.08901663786526));
#37677=CARTESIAN_POINT('Ctrl Pts',(-20.3595708193274,23.0967337355577,-7.08922494762439));
#37678=CARTESIAN_POINT('Ctrl Pts',(-20.3605035622708,23.0902207768709,-7.08962898023459));
#37679=CARTESIAN_POINT('Ctrl Pts',(-20.3609596864279,23.0870691442607,-7.08982468261714));
#37680=CARTESIAN_POINT('Ctrl Pts',(-20.3620568822459,23.0795664300672,-7.09029102334248));
#37681=CARTESIAN_POINT('Ctrl Pts',(-20.3627021898156,23.0752159824504,-7.09056179591816));
#37682=CARTESIAN_POINT('Ctrl Pts',(-20.365026545223,23.059763956866,-7.09152483864947));
#37683=CARTESIAN_POINT('Ctrl Pts',(-20.3667546862896,23.0486699461733,-7.09221866646543));
#37684=CARTESIAN_POINT('Ctrl Pts',(-20.3928278715281,22.8868547251071,-7.10237429446663));
#37685=CARTESIAN_POINT('Ctrl Pts',(-20.427791235932,22.7380640149529,-7.11217798675893));
#37686=CARTESIAN_POINT('Ctrl Pts',(-20.5252808423197,22.4249029218801,-7.13383252295159));
#37687=CARTESIAN_POINT('Ctrl Pts',(-20.5909763216272,22.2620207263261,-7.14574006749728));
#37688=CARTESIAN_POINT('Ctrl Pts',(-20.7474093510081,21.950153773769,-7.16932237688817));
#37689=CARTESIAN_POINT('Ctrl Pts',(-20.8376517130569,21.8015219036287,-7.18095570685641));
#37690=CARTESIAN_POINT('Ctrl Pts',(-20.945575906127,21.6523887903515,-7.19254352937989));
#37691=CARTESIAN_POINT('Ctrl Pts',(-20.9517532577081,21.6439396940987,-7.19319967725875));
#37692=CARTESIAN_POINT('Ctrl Pts',(-20.9598976667474,21.632913296235,-7.1940553426875));
#37693=CARTESIAN_POINT('Ctrl Pts',(-20.961827514737,21.6303087819983,-7.19425741046668));
#37694=CARTESIAN_POINT('Ctrl Pts',(-20.9649856065937,21.6260600516107,-7.19458696040033));
#37695=CARTESIAN_POINT('Ctrl Pts',(-20.966211491198,21.6244140972671,-7.19471460755793));
#37696=CARTESIAN_POINT('Ctrl Pts',(-20.9685669067823,21.6212578574159,-7.19495933987909));
#37697=CARTESIAN_POINT('Ctrl Pts',(-20.9696961878354,21.619747396903,-7.19507644167272));
#37698=CARTESIAN_POINT('Ctrl Pts',(-20.9722944729898,21.6162784357642,-7.1953453406027));
#37699=CARTESIAN_POINT('Ctrl Pts',(-20.973764386886,21.6143206124558,-7.19549707343382));
#37700=CARTESIAN_POINT('Ctrl Pts',(-20.9784303462376,21.6081206052783,-7.19597749288437));
#37701=CARTESIAN_POINT('Ctrl Pts',(-20.9816346698303,21.6038846184055,-7.19630559873236));
#37702=CARTESIAN_POINT('Ctrl Pts',(-21.0088082724573,21.5681461859778,-7.19907288303556));
#37703=CARTESIAN_POINT('Ctrl Pts',(-21.0333469272029,21.5370781687739,-7.20147261345067));
#37704=CARTESIAN_POINT('Ctrl Pts',(-21.0632559300916,21.5006128508458,-7.20429272162335));
#37705=CARTESIAN_POINT('Ctrl Pts',(-21.0680794030325,21.494774125299,-7.20474437797953));
#37706=CARTESIAN_POINT('Ctrl Pts',(-21.0737292604161,21.4879839661316,-7.20526983213132));
#37707=CARTESIAN_POINT('Ctrl Pts',(-21.0745356326535,21.4870160000518,-7.20534474259972));
#37708=CARTESIAN_POINT('Ctrl Pts',(-21.0799257114599,21.4805534800953,-7.20584490777962));
#37709=CARTESIAN_POINT('Ctrl Pts',(-21.0845271753434,21.475073688391,-7.20626917733858));
#37710=CARTESIAN_POINT('Ctrl Pts',(-21.0916158313022,21.4666888147799,-7.20691870115627));
#37711=CARTESIAN_POINT('Ctrl Pts',(-21.094089979903,21.4637727914657,-7.20714464888504));
#37712=CARTESIAN_POINT('Ctrl Pts',(-21.1010885294476,21.455554023175,-7.20778167580901));
#37713=CARTESIAN_POINT('Ctrl Pts',(-21.1056249756417,21.4502615162066,-7.20819212348645));
#37714=CARTESIAN_POINT('Ctrl Pts',(-21.1180648996286,21.4358432460453,-7.20931106403037));
#37715=CARTESIAN_POINT('Ctrl Pts',(-21.1260026016387,21.426747036419,-7.21001782580518));
#37716=CARTESIAN_POINT('Ctrl Pts',(-21.16087804168,21.3872319505114,-7.21309287327705));
#37717=CARTESIAN_POINT('Ctrl Pts',(-21.1883393786652,21.3572785318332,-7.21543633550219));
#37718=CARTESIAN_POINT('Ctrl Pts',(-21.3861382269197,21.1495567426904,-7.23184310489584));
#37719=CARTESIAN_POINT('Ctrl Pts',(-21.5757884018109,20.99130110841,-7.24522923172906));
#37720=CARTESIAN_POINT('Ctrl Pts',(-21.8911457996345,20.784271763947,-7.26681328629581));
#37721=CARTESIAN_POINT('Ctrl Pts',(-22.0049463669217,20.7191207183738,-7.27447409707262));
#37722=CARTESIAN_POINT('Ctrl Pts',(-22.1411842022026,20.651790240033,-7.28366306122662));
#37723=CARTESIAN_POINT('Ctrl Pts',(-22.1600715920662,20.6426841083983,-7.28493717098252));
#37724=CARTESIAN_POINT('Ctrl Pts',(-22.1845685552583,20.6311667026796,-7.28659039846189));
#37725=CARTESIAN_POINT('Ctrl Pts',(-22.1900982878482,20.6285860153399,-7.28696362944073));
#37726=CARTESIAN_POINT('Ctrl Pts',(-22.1990140955313,20.6244558679939,-7.28756549057098));
#37727=CARTESIAN_POINT('Ctrl Pts',(-22.2023956031186,20.6228965354769,-7.28779377891341));
#37728=CARTESIAN_POINT('Ctrl Pts',(-22.2088368209808,20.6199397893123,-7.28822867175003));
#37729=CARTESIAN_POINT('Ctrl Pts',(-22.2118960333682,20.618541297557,-7.28843523867168));
#37730=CARTESIAN_POINT('Ctrl Pts',(-22.2188691111407,20.6153668060595,-7.288906123826));
#37731=CARTESIAN_POINT('Ctrl Pts',(-22.2227843451248,20.6135938439303,-7.28917054632108));
#37732=CARTESIAN_POINT('Ctrl Pts',(-22.234710283656,20.6082220629274,-7.2899760866223));
#37733=CARTESIAN_POINT('Ctrl Pts',(-22.2427321127085,20.6046481731605,-7.29051806040932));
#37734=CARTESIAN_POINT('Ctrl Pts',(-22.3001249174809,20.5793591385182,-7.29439677051276));
#37735=CARTESIAN_POINT('Ctrl Pts',(-22.3500170202423,20.5588547392091,-7.29777467380651));
#37736=CARTESIAN_POINT('Ctrl Pts',(-22.4140850643546,20.5343852073421,-7.30212364495926));
#37737=CARTESIAN_POINT('Ctrl Pts',(-22.427807655864,20.5292510882263,-7.30305577531793));
#37738=CARTESIAN_POINT('Ctrl Pts',(-22.4541202511102,20.5196106208432,-7.30484435547272));
#37739=CARTESIAN_POINT('Ctrl Pts',(-22.4667042585437,20.5150886976141,-7.30570028841363));
#37740=CARTESIAN_POINT('Ctrl Pts',(-22.6214451007938,20.460569273658,-7.31623211236412));
#37741=CARTESIAN_POINT('Ctrl Pts',(-22.7668943240279,20.4205295562629,-7.32621457925477));
#37742=CARTESIAN_POINT('Ctrl Pts',(-23.18050251441,20.3373143667379,-7.35460461532516));
#37743=CARTESIAN_POINT('Ctrl Pts',(-23.4521131899202,20.3175949923935,-7.3733196068634));
#37744=CARTESIAN_POINT('Ctrl Pts',(-23.7309523673661,20.3325625793388,-7.39092232678801));
#37745=CARTESIAN_POINT('Ctrl Pts',(-23.7389079372943,20.3330192170007,-7.3914231132945));
#37746=CARTESIAN_POINT('Ctrl Pts',(-23.7527091742675,20.3338627559439,-7.39228928236897));
#37747=CARTESIAN_POINT('Ctrl Pts',(-23.7585555888035,20.3342360952689,-7.39265539792252));
#37748=CARTESIAN_POINT('Ctrl Pts',(-23.7669648089511,20.3347961171837,-7.39318080944741));
#37749=CARTESIAN_POINT('Ctrl Pts',(-23.7695284161657,20.3349699233796,-7.39334082516806));
#37750=CARTESIAN_POINT('Ctrl Pts',(-23.7739949365616,20.3352781091137,-7.39361933608096));
#37751=CARTESIAN_POINT('Ctrl Pts',(-23.775897941036,20.3354111124483,-7.39373790937933));
#37752=CARTESIAN_POINT('Ctrl Pts',(-23.7795585595508,20.3356702239663,-7.39396582441047));
#37753=CARTESIAN_POINT('Ctrl Pts',(-23.7813161848357,20.3357960837386,-7.39407518015229));
#37754=CARTESIAN_POINT('Ctrl Pts',(-23.7854773149363,20.3360974838674,-7.39433389793387));
#37755=CARTESIAN_POINT('Ctrl Pts',(-23.7878807319196,20.3362742790192,-7.3944831887201));
#37756=CARTESIAN_POINT('Ctrl Pts',(-23.795041475257,20.3368090988884,-7.39492757054652));
#37757=CARTESIAN_POINT('Ctrl Pts',(-23.7997982342611,20.3371749936078,-7.39522221948764));
#37758=CARTESIAN_POINT('Ctrl Pts',(-23.8436990209247,20.3406499646627,-7.39793667612935));
#37759=CARTESIAN_POINT('Ctrl Pts',(-23.8827861173088,20.3444638244165,-7.40031753622912));
#37760=CARTESIAN_POINT('Ctrl Pts',(-23.9271533944665,20.3496131593299,-7.40298896122832));
#37761=CARTESIAN_POINT('Ctrl Pts',(-23.9325093924793,20.3502484152217,-7.40331093826421));
#37762=CARTESIAN_POINT('Ctrl Pts',(-23.9425168420203,20.3514608470295,-7.40391161523707));
#37763=CARTESIAN_POINT('Ctrl Pts',(-23.9471686688015,20.3520347292997,-7.40419045865739));
#37764=CARTESIAN_POINT('Ctrl Pts',(-24.2425503414586,20.3891294865829,-7.42187368644489));
#37765=CARTESIAN_POINT('Ctrl Pts',(-24.5269783353454,20.4651222169242,-7.43760761054507));
#37766=CARTESIAN_POINT('Ctrl Pts',(-24.9486833558827,20.6420776723167,-7.46358547699101));
#37767=CARTESIAN_POINT('Ctrl Pts',(-25.095022855106,20.7170983133602,-7.47313919013141));
#37768=CARTESIAN_POINT('Ctrl Pts',(-25.2460882058468,20.8097364834987,-7.4839058316975));
#37769=CARTESIAN_POINT('Ctrl Pts',(-25.2571382063596,20.8166051275862,-7.48469876807435));
#37770=CARTESIAN_POINT('Ctrl Pts',(-25.2724533744258,20.8262540486807,-7.48580540277979));
#37771=CARTESIAN_POINT('Ctrl Pts',(-25.2767541071204,20.8289778693815,-7.48611700589174));
#37772=CARTESIAN_POINT('Ctrl Pts',(-25.2840026889409,20.8335927773749,-7.48664362388413));
#37773=CARTESIAN_POINT('Ctrl Pts',(-25.2869539519705,20.8354785070013,-7.48685843900778));
#37774=CARTESIAN_POINT('Ctrl Pts',(-25.2927871866065,20.83921909678,-7.48728382543547));
#37775=CARTESIAN_POINT('Ctrl Pts',(-25.2956692852238,20.8410737511152,-7.48749438886363));
#37776=CARTESIAN_POINT('Ctrl Pts',(-25.3020141427269,20.8451710466387,-7.48795879574178));
#37777=CARTESIAN_POINT('Ctrl Pts',(-25.3054755612075,20.8474157443358,-7.48821271598116));
#37778=CARTESIAN_POINT('Ctrl Pts',(-25.3175450081941,20.8552756312968,-7.48910007805005));
#37779=CARTESIAN_POINT('Ctrl Pts',(-25.3261304092142,20.860925301442,-7.48973481326279));
#37780=CARTESIAN_POINT('Ctrl Pts',(-25.413565981602,20.9190640163075,-7.49623552414669));
#37781=CARTESIAN_POINT('Ctrl Pts',(-25.4900851824079,20.9749591011713,-7.50223060793621));
#37782=CARTESIAN_POINT('Ctrl Pts',(-25.7356449412205,21.1714929827473,-7.52254726398655));
#37783=CARTESIAN_POINT('Ctrl Pts',(-25.8927392268272,21.326029592222,-7.53740209862361));
#37784=CARTESIAN_POINT('Ctrl Pts',(-26.1492131399061,21.6358815829431,-7.56461858375501));
#37785=CARTESIAN_POINT('Ctrl Pts',(-26.2534282644208,21.7860899306891,-7.57690935315236));
#37786=CARTESIAN_POINT('Ctrl Pts',(-26.352307292686,21.9581281661657,-7.58946062933366));
#37787=CARTESIAN_POINT('Ctrl Pts',(-26.3601361930593,21.9719861684285,-7.59046139373923));
#37788=CARTESIAN_POINT('Ctrl Pts',(-26.3696845813405,21.9891841240345,-7.59169018059009));
#37789=CARTESIAN_POINT('Ctrl Pts',(-26.3715011413099,21.9924695111648,-7.59192432955634));
#37790=CARTESIAN_POINT('Ctrl Pts',(-26.374350000288,21.9976432177906,-7.59229212133506));
#37791=CARTESIAN_POINT('Ctrl Pts',(-26.3753861483857,21.9995293966235,-7.59242601162495));
#37792=CARTESIAN_POINT('Ctrl Pts',(-26.3773174125475,22.0030533830525,-7.59267579449355));
#37793=CARTESIAN_POINT('Ctrl Pts',(-26.378212989173,22.0046909195042,-7.59279171630674));
#37794=CARTESIAN_POINT('Ctrl Pts',(-26.380217959043,22.0083645270797,-7.593051441398));
#37795=CARTESIAN_POINT('Ctrl Pts',(-26.3813265753743,22.0104010135094,-7.59319519412834));
#37796=CARTESIAN_POINT('Ctrl Pts',(-26.3841342640669,22.0155719132131,-7.59355962845327));
#37797=CARTESIAN_POINT('Ctrl Pts',(-26.3858303396969,22.0187079620325,-7.59378011783683));
#37798=CARTESIAN_POINT('Ctrl Pts',(-26.3950859172378,22.0358896307477,-7.5949852484635));
#37799=CARTESIAN_POINT('Ctrl Pts',(-26.4025464417509,22.0499887340122,-7.59596365069495));
#37800=CARTESIAN_POINT('Ctrl Pts',(-26.5529329359238,22.3393702831933,-7.61584297323554));
#37801=CARTESIAN_POINT('Ctrl Pts',(-26.6555090180112,22.6338560405513,-7.63246398170144));
#37802=CARTESIAN_POINT('Ctrl Pts',(-26.7399041983485,23.0703783247074,-7.6575939504278));
#37803=CARTESIAN_POINT('Ctrl Pts',(-26.7571283042137,23.2036992391386,-7.66531158182004));
#37804=CARTESIAN_POINT('Ctrl Pts',(-26.7696547453009,23.3932105825505,-7.67659269883225));
#37805=CARTESIAN_POINT('Ctrl Pts',(-26.7718858166746,23.4488070625984,-7.67993861777374));
#37806=CARTESIAN_POINT('Ctrl Pts',(-26.7727925374772,23.5125726428198,-7.68382669574348));
#37807=CARTESIAN_POINT('Ctrl Pts',(-26.7728774518515,23.5207146752901,-7.68432409111798));
#37808=CARTESIAN_POINT('Ctrl Pts',(-26.7729591778445,23.5330244982713,-7.68507754346163));
#37809=CARTESIAN_POINT('Ctrl Pts',(-26.772978762445,23.5371921469856,-7.68533288522144));
#37810=CARTESIAN_POINT('Ctrl Pts',(-26.7729986293156,23.5443919324392,-7.6857744360295));
#37811=CARTESIAN_POINT('Ctrl Pts',(-26.7730027168634,23.5474240604204,-7.68596052537403));
#37812=CARTESIAN_POINT('Ctrl Pts',(-26.7730022913777,23.554157356275,-7.68637406427218));
#37813=CARTESIAN_POINT('Ctrl Pts',(-26.7729956815624,23.5578585155528,-7.68660157939536));
#37814=CARTESIAN_POINT('Ctrl Pts',(-26.7729616393149,23.5675611686293,-7.68719854520762));
#37815=CARTESIAN_POINT('Ctrl Pts',(-26.7729238183149,23.5735625909949,-7.68756832155159));
#37816=CARTESIAN_POINT('Ctrl Pts',(-26.7726832764717,23.6000088397494,-7.68920017633913));
#37817=CARTESIAN_POINT('Ctrl Pts',(-26.7723027654457,23.6204512157058,-7.69046782381564));
#37818=CARTESIAN_POINT('Ctrl Pts',(-26.7682127307511,23.765823822046,-7.69952853735467));
#37819=CARTESIAN_POINT('Ctrl Pts',(-26.7574333737421,23.8904334371617,-7.70754346589177));
#37820=CARTESIAN_POINT('Ctrl Pts',(-26.6994066306839,24.2894063658884,-7.73401941320084));
#37821=CARTESIAN_POINT('Ctrl Pts',(-26.6238915515564,24.5583370477323,-7.75323741828679));
#37822=CARTESIAN_POINT('Ctrl Pts',(-26.4786668372663,24.8989532675592,-7.77775052409668));
#37823=CARTESIAN_POINT('Ctrl Pts',(-26.438915609643,24.9821161406006,-7.78373663547824));
#37824=CARTESIAN_POINT('Ctrl Pts',(-26.3926238417019,25.0691615020145,-7.7899174289953));
#37825=CARTESIAN_POINT('Ctrl Pts',(-26.3895796813747,25.0748444321249,-7.79032055367208));
#37826=CARTESIAN_POINT('Ctrl Pts',(-26.3853393278583,25.0827037013147,-7.79087746267443));
#37827=CARTESIAN_POINT('Ctrl Pts',(-26.3841576677842,25.0848878006752,-7.79103216427989));
#37828=CARTESIAN_POINT('Ctrl Pts',(-26.3821239833831,25.0886363645064,-7.79129756535256));
#37829=CARTESIAN_POINT('Ctrl Pts',(-26.38127318656,25.0902014878961,-7.79140834339378));
#37830=CARTESIAN_POINT('Ctrl Pts',(-26.37951470566,25.0934300017869,-7.79163678357562));
#37831=CARTESIAN_POINT('Ctrl Pts',(-26.3786068540261,25.0950932939077,-7.79175443400751));
#37832=CARTESIAN_POINT('Ctrl Pts',(-26.3764747507924,25.0989913811621,-7.79203006913802));
#37833=CARTESIAN_POINT('Ctrl Pts',(-26.375249311568,25.1012255325506,-7.79218797732003));
#37834=CARTESIAN_POINT('Ctrl Pts',(-26.3712725304487,25.1084554248686,-7.79269876347109));
#37835=CARTESIAN_POINT('Ctrl Pts',(-26.3685105568399,25.1134453523507,-7.7930509614482));
#37836=CARTESIAN_POINT('Ctrl Pts',(-26.2978424483562,25.2403220009214,-7.80199824231367));
#37837=CARTESIAN_POINT('Ctrl Pts',(-26.2220948805304,25.3576968327753,-7.81009165701611));
#37838=CARTESIAN_POINT('Ctrl Pts',(-25.9473056772875,25.7282780764366,-7.83627406680274));
#37839=CARTESIAN_POINT('Ctrl Pts',(-25.7180348489133,25.9565739906241,-7.85366426335849));
#37840=CARTESIAN_POINT('Ctrl Pts',(-25.4532069504515,26.1512002860662,-7.87321721883335));
#37841=CARTESIAN_POINT('Ctrl Pts',(-25.4476592596371,26.1552501225843,-7.8736265016008));
#37842=CARTESIAN_POINT('Ctrl Pts',(-25.4056992213984,26.1856759698745,-7.87671984819572));
#37843=CARTESIAN_POINT('Ctrl Pts',(-25.3687528844549,26.2113040670552,-7.87943082517805));
#37844=CARTESIAN_POINT('Ctrl Pts',(-25.3250612315886,26.2402762097737,-7.88262669192885));
#37845=CARTESIAN_POINT('Ctrl Pts',(-25.3188243091784,26.2443808093116,-7.88308266007551));
#37846=CARTESIAN_POINT('Ctrl Pts',(-25.3088535872105,26.2508931275467,-7.88381124397058));
#37847=CARTESIAN_POINT('Ctrl Pts',(-25.3051289491521,26.2533148801365,-7.88408333344342));
#37848=CARTESIAN_POINT('Ctrl Pts',(-25.2985490993852,26.2575737540745,-7.8845638665275));
#37849=CARTESIAN_POINT('Ctrl Pts',(-25.2956959639203,26.2594140836341,-7.88477218986558));
#37850=CARTESIAN_POINT('Ctrl Pts',(-25.2897937799584,26.2632079166924,-7.8852030529357));
#37851=CARTESIAN_POINT('Ctrl Pts',(-25.2867443376308,26.2651607959174,-7.88542561554537));
#37852=CARTESIAN_POINT('Ctrl Pts',(-25.2789348527636,26.2701434914903,-7.88599546805452));
#37853=CARTESIAN_POINT('Ctrl Pts',(-25.2741701472862,26.273165944633,-7.88634303111829));
#37854=CARTESIAN_POINT('Ctrl Pts',(-25.2550594874822,26.2852183730295,-7.88773662985761));
#37855=CARTESIAN_POINT('Ctrl Pts',(-25.2406505271045,26.2941474839875,-7.88878639194285));
#37856=CARTESIAN_POINT('Ctrl Pts',(-25.0548172088165,26.4072875156468,-7.90231438686564));
#37857=CARTESIAN_POINT('Ctrl Pts',(-24.8741291155528,26.4953650136986,-7.91539267488797));
#37858=CARTESIAN_POINT('Ctrl Pts',(-24.5447992712856,26.6194397566855,-7.93897908384512));
#37859=CARTESIAN_POINT('Ctrl Pts',(-24.3995563021428,26.6627619006147,-7.9492910574008));
#37860=CARTESIAN_POINT('Ctrl Pts',(-24.1116559232222,26.7269749093367,-7.96913804888836));
#37861=CARTESIAN_POINT('Ctrl Pts',(-23.9695460862155,26.7488370239252,-7.97866132521248));
#37862=CARTESIAN_POINT('Ctrl Pts',(-23.8172415832172,26.7619373784979,-7.98827349681488));
#37863=CARTESIAN_POINT('Ctrl Pts',(-23.8080445648108,26.7626886760308,-7.98885162159681));
#37864=CARTESIAN_POINT('Ctrl Pts',(-23.7956501934097,26.7636475919997,-7.98962750126572));
#37865=CARTESIAN_POINT('Ctrl Pts',(-23.7924556900058,26.7638899499927,-7.98982718615744));
#37866=CARTESIAN_POINT('Ctrl Pts',(-23.7874394195505,26.7642629981604,-7.99014028838149));
#37867=CARTESIAN_POINT('Ctrl Pts',(-23.785617904823,26.7643969029845,-7.99025388740391));
#37868=CARTESIAN_POINT('Ctrl Pts',(-23.7821124283426,26.7646516047907,-7.99047232271217));
#37869=CARTESIAN_POINT('Ctrl Pts',(-23.7804284966404,26.7647726261987,-7.99057717087911));
#37870=CARTESIAN_POINT('Ctrl Pts',(-23.7764301239966,26.7650568247182,-7.99082593146917));
#37871=CARTESIAN_POINT('Ctrl Pts',(-23.7741156036194,26.7652188255789,-7.99096977650383));
#37872=CARTESIAN_POINT('Ctrl Pts',(-23.7676471865481,26.7656645522312,-7.99137135684123));
#37873=CARTESIAN_POINT('Ctrl Pts',(-23.763492893043,26.7659427292301,-7.99162877910082));
#37874=CARTESIAN_POINT('Ctrl Pts',(-23.7539584901334,26.766562607997,-7.99221848180003));
#37875=CARTESIAN_POINT('Ctrl Pts',(-23.7485780214928,26.7668988637463,-7.99255046027932));
#37876=CARTESIAN_POINT('Ctrl Pts',(-23.6130730692217,26.7750260443758,-8.0008915455931));
#37877=CARTESIAN_POINT('Ctrl Pts',(-23.4825772420055,26.7749292501573,-8.00846945790495));
#37878=CARTESIAN_POINT('Ctrl Pts',(-23.1124961815171,26.7521696128154,-8.02955546359413));
#37879=CARTESIAN_POINT('Ctrl Pts',(-22.8749682800439,26.7106164944346,-8.04265843381471));
#37880=CARTESIAN_POINT('Ctrl Pts',(-22.6064156240064,26.6319476654169,-8.05872055546388));
#37881=CARTESIAN_POINT('Ctrl Pts',(-22.5687747460608,26.6201668962918,-8.06099980100116));
#37882=CARTESIAN_POINT('Ctrl Pts',(-22.4400182187364,26.577258860684,-8.06890834115567));
#37883=CARTESIAN_POINT('Ctrl Pts',(-22.3500939693104,26.5427438278393,-8.07462874202298));
#37884=CARTESIAN_POINT('Ctrl Pts',(-22.2525197660991,26.5001865929291,-8.08110846909325));
#37885=CARTESIAN_POINT('Ctrl Pts',(-22.2432035391128,26.4960706224428,-8.08172993158481));
#37886=CARTESIAN_POINT('Ctrl Pts',(-22.2300920101339,26.4902034205509,-8.08260856349652));
#37887=CARTESIAN_POINT('Ctrl Pts',(-22.2262802964774,26.4884888311914,-8.08286447258066));
#37888=CARTESIAN_POINT('Ctrl Pts',(-22.2196210801126,26.4854777856802,-8.0833123966375));
#37889=CARTESIAN_POINT('Ctrl Pts',(-22.216772103348,26.4841845858986,-8.08350429921969));
#37890=CARTESIAN_POINT('Ctrl Pts',(-22.2107986401567,26.4814626297133,-8.08390723045006));
#37891=CARTESIAN_POINT('Ctrl Pts',(-22.2076745481897,26.4800330225075,-8.08411828826566));
#37892=CARTESIAN_POINT('Ctrl Pts',(-22.2002336828003,26.4766136276573,-8.08462176163667));
#37893=CARTESIAN_POINT('Ctrl Pts',(-22.1959190229425,26.4746192841759,-8.08491433448232));
#37894=CARTESIAN_POINT('Ctrl Pts',(-22.1816604714197,26.4679903019738,-8.08588328568245));
#37895=CARTESIAN_POINT('Ctrl Pts',(-22.171735915897,26.4633144704031,-8.08656109076988));
#37896=CARTESIAN_POINT('Ctrl Pts',(-22.1483337541556,26.4521424585935,-8.08816743889533));
#37897=CARTESIAN_POINT('Ctrl Pts',(-22.1348772185798,26.445602962558,-8.08909748247897));
#37898=CARTESIAN_POINT('Ctrl Pts',(-22.1059249527286,26.4312829118854,-8.09111248113288));
#37899=CARTESIAN_POINT('Ctrl Pts',(-22.0904475042375,26.4234715138296,-8.09219839320965));
#37900=CARTESIAN_POINT('Ctrl Pts',(-22.0750359919087,26.4155367624894,-8.09328852648195));
#37901=CARTESIAN_POINT('Ctrl Pts',(-22.0750360458934,26.4155367902838,-8.34120882940695));
#37902=CARTESIAN_POINT('Ctrl Pts',(-22.1027733724074,26.4298175937409,-8.33944533023278));
#37903=CARTESIAN_POINT('Ctrl Pts',(-22.1307241352365,26.4436987562337,-8.33768934506599));
#37904=CARTESIAN_POINT('Ctrl Pts',(-22.3476372887855,26.5475223062275,-8.3241934062341));
#37905=CARTESIAN_POINT('Ctrl Pts',(-22.5447352738616,26.6192655287509,-8.31265322975392));
#37906=CARTESIAN_POINT('Ctrl Pts',(-22.8253182995639,26.6914405061735,-8.29590793569271));
#37907=CARTESIAN_POINT('Ctrl Pts',(-22.9039606430498,26.7085585341609,-8.29118666463588));
#37908=CARTESIAN_POINT('Ctrl Pts',(-23.0232776285371,26.7298871220935,-8.28393417183107));
#37909=CARTESIAN_POINT('Ctrl Pts',(-23.063529386419,26.7362969482822,-8.2814726218952));
#37910=CARTESIAN_POINT('Ctrl Pts',(-23.111325765456,26.7429813364168,-8.27852870352594));
#37911=CARTESIAN_POINT('Ctrl Pts',(-23.1187645719593,26.7439951740693,-8.27806992833723));
#37912=CARTESIAN_POINT('Ctrl Pts',(-23.1302055508545,26.7455137679747,-8.27736338577484));
#37913=CARTESIAN_POINT('Ctrl Pts',(-23.1342052763479,26.746037023063,-8.27711620448954));
#37914=CARTESIAN_POINT('Ctrl Pts',(-23.1414896408188,26.7469760767165,-8.27666570870248));
#37915=CARTESIAN_POINT('Ctrl Pts',(-23.1447739628976,26.7473943262309,-8.27646247207792));
#37916=CARTESIAN_POINT('Ctrl Pts',(-23.1514181899543,26.7482300478159,-8.27605107607443));
#37917=CARTESIAN_POINT('Ctrl Pts',(-23.1547781194514,26.7486472876449,-8.27584290962085));
#37918=CARTESIAN_POINT('Ctrl Pts',(-23.1643643270776,26.7498223773121,-8.27524862485351));
#37919=CARTESIAN_POINT('Ctrl Pts',(-23.170592143216,26.7505673430807,-8.27486209960974));
#37920=CARTESIAN_POINT('Ctrl Pts',(-23.1972255750654,26.7536743739525,-8.27320720374329));
#37921=CARTESIAN_POINT('Ctrl Pts',(-23.2176509900816,26.7558594499879,-8.27193325524694));
#37922=CARTESIAN_POINT('Ctrl Pts',(-23.5899597744425,26.7920918109801,-8.24862094955779));
#37923=CARTESIAN_POINT('Ctrl Pts',(-23.9449984266275,26.7681926273704,-8.2245088086386));
#37924=CARTESIAN_POINT('Ctrl Pts',(-24.4257627108239,26.6549847105705,-8.19131576487943));
#37925=CARTESIAN_POINT('Ctrl Pts',(-24.5603639068937,26.613839598801,-8.1820141438776));
#37926=CARTESIAN_POINT('Ctrl Pts',(-24.6964988782546,26.5622720290513,-8.17288020746082));
#37927=CARTESIAN_POINT('Ctrl Pts',(-24.7011309094968,26.5605051954651,-8.17256976572695));
#37928=CARTESIAN_POINT('Ctrl Pts',(-24.708454681879,26.5576922536549,-8.17207948617992));
#37929=CARTESIAN_POINT('Ctrl Pts',(-24.7111491018783,26.5566532128094,-8.17189923318364));
#37930=CARTESIAN_POINT('Ctrl Pts',(-24.7162421479843,26.5546813294385,-8.1715587495781));
#37931=CARTESIAN_POINT('Ctrl Pts',(-24.7186410579687,26.5537492335058,-8.1713984744974));
#37932=CARTESIAN_POINT('Ctrl Pts',(-24.722785731101,26.552133104656,-8.17112173553792));
#37933=CARTESIAN_POINT('Ctrl Pts',(-24.7245320161185,26.5514504209651,-8.1710051897376));
#37934=CARTESIAN_POINT('Ctrl Pts',(-24.7279114709179,26.5501258731141,-8.1707797518536));
#37935=CARTESIAN_POINT('Ctrl Pts',(-24.7295447098551,26.5494842000154,-8.17067084832795));
#37936=CARTESIAN_POINT('Ctrl Pts',(-24.7333928010328,26.5479687181692,-8.17041436896415));
#37937=CARTESIAN_POINT('Ctrl Pts',(-24.7356072142842,26.5470937867713,-8.17026686142423));
#37938=CARTESIAN_POINT('Ctrl Pts',(-24.7421502952598,26.544500179238,-8.16983125760568));
#37939=CARTESIAN_POINT('Ctrl Pts',(-24.7464762330029,26.5427745634737,-8.16954357930158));
#37940=CARTESIAN_POINT('Ctrl Pts',(-24.7843097420465,26.5275876363343,-8.16703029531971));
#37941=CARTESIAN_POINT('Ctrl Pts',(-24.817594308191,26.5135727326101,-8.16483757924104));
#37942=CARTESIAN_POINT('Ctrl Pts',(-24.8555208779295,26.4968472759093,-8.16235252470389));
#37943=CARTESIAN_POINT('Ctrl Pts',(-24.8603984751865,26.4946817887547,-8.16203318907669));
#37944=CARTESIAN_POINT('Ctrl Pts',(-24.867854026195,26.491349583959,-8.16154543728902));
#37945=CARTESIAN_POINT('Ctrl Pts',(-24.8704358360506,26.4901915807496,-8.16137659855134));
#37946=CARTESIAN_POINT('Ctrl Pts',(-24.8752382587369,26.4880299779789,-8.16106265973373));
#37947=CARTESIAN_POINT('Ctrl Pts',(-24.8774592624939,26.4870272582532,-8.1609175177101));
#37948=CARTESIAN_POINT('Ctrl Pts',(-24.8809398237862,26.4854511294757,-8.16069013448838));
#37949=CARTESIAN_POINT('Ctrl Pts',(-24.8822001484765,26.4848794285781,-8.16060781266769));
#37950=CARTESIAN_POINT('Ctrl Pts',(-24.8859878549434,26.4831583292754,-8.16036044999131));
#37951=CARTESIAN_POINT('Ctrl Pts',(-24.8885141261842,26.4820064736332,-8.16019552446968));
#37952=CARTESIAN_POINT('Ctrl Pts',(-24.8973672231942,26.477956068701,-8.15961774651599));
#37953=CARTESIAN_POINT('Ctrl Pts',(-24.9036861878226,26.4750402731629,-8.15920569221256));
#37954=CARTESIAN_POINT('Ctrl Pts',(-24.9144233997497,26.4700434926081,-8.15850602393743));
#37955=CARTESIAN_POINT('Ctrl Pts',(-24.918846425972,26.4679729031039,-8.15821795035371));
#37956=CARTESIAN_POINT('Ctrl Pts',(-25.0411406844188,26.4103829649947,-8.15025639976279));
#37957=CARTESIAN_POINT('Ctrl Pts',(-25.1555524840572,26.3477713371421,-8.14289564430797));
#37958=CARTESIAN_POINT('Ctrl Pts',(-25.3455622371713,26.2282823326868,-8.13031624572085));
#37959=CARTESIAN_POINT('Ctrl Pts',(-25.4230228408465,26.1746976060524,-8.12507691590084));
#37960=CARTESIAN_POINT('Ctrl Pts',(-25.5849292193896,26.0518733257388,-8.11367516110724));
#37961=CARTESIAN_POINT('Ctrl Pts',(-25.6684245288969,25.9815815925956,-8.10750465582291));
#37962=CARTESIAN_POINT('Ctrl Pts',(-25.805707866571,25.853559662363,-8.0966435515795));
#37963=CARTESIAN_POINT('Ctrl Pts',(-25.8612377607683,25.7978397593696,-8.09202481811507));
#37964=CARTESIAN_POINT('Ctrl Pts',(-25.9417814537768,25.710877141744,-8.08492938055546));
#37965=CARTESIAN_POINT('Ctrl Pts',(-25.9683446958331,25.6811066698828,-8.08251918563339));
#37966=CARTESIAN_POINT('Ctrl Pts',(-25.9992115915905,25.645192333475,-8.07963038798964));
#37967=CARTESIAN_POINT('Ctrl Pts',(-26.0040559142288,25.6395160881938,-8.07917436229542));
#37968=CARTESIAN_POINT('Ctrl Pts',(-26.0114821111363,25.6307531236746,-8.0784711697199));
#37969=CARTESIAN_POINT('Ctrl Pts',(-26.0140780140244,25.6276782820735,-8.07822458018652));
#37970=CARTESIAN_POINT('Ctrl Pts',(-26.018798952275,25.6220650452144,-8.07777469842422));
#37971=CARTESIAN_POINT('Ctrl Pts',(-26.0209258513901,25.6195282187291,-8.07757148296681));
#37972=CARTESIAN_POINT('Ctrl Pts',(-26.025224120011,25.6143854502174,-8.07715972043681));
#37973=CARTESIAN_POINT('Ctrl Pts',(-26.0273952912495,25.6117793486308,-8.07695116563234));
#37974=CARTESIAN_POINT('Ctrl Pts',(-26.0335893812555,25.6043205409911,-8.07635456976985));
#37975=CARTESIAN_POINT('Ctrl Pts',(-26.037602166206,25.599459473415,-8.07596611668119));
#37976=CARTESIAN_POINT('Ctrl Pts',(-26.0547973185164,25.5785044304303,-8.07429309605373));
#37977=CARTESIAN_POINT('Ctrl Pts',(-26.0678377071591,25.5622950773466,-8.07300279876892));
#37978=CARTESIAN_POINT('Ctrl Pts',(-26.3015945846025,25.2659019857957,-8.04947427850338));
#37979=CARTESIAN_POINT('Ctrl Pts',(-26.4744011216352,24.9511636370712,-8.02511985781829));
#37980=CARTESIAN_POINT('Ctrl Pts',(-26.6181705880062,24.5403062515305,-7.99588921291723));
#37981=CARTESIAN_POINT('Ctrl Pts',(-26.6414632008705,24.4649905915381,-7.99064555231686));
#37982=CARTESIAN_POINT('Ctrl Pts',(-26.6714024691744,24.3539028460264,-7.98314355246942));
#37983=CARTESIAN_POINT('Ctrl Pts',(-26.6802421271728,24.318755057165,-7.9808033403347));
#37984=CARTESIAN_POINT('Ctrl Pts',(-26.6945041685765,24.2577117809356,-7.97680501887104));
#37985=CARTESIAN_POINT('Ctrl Pts',(-26.7002039223492,24.2318853453675,-7.97513365473354));
#37986=CARTESIAN_POINT('Ctrl Pts',(-26.7064731853699,24.2017184082633,-7.9732072616159));
#37987=CARTESIAN_POINT('Ctrl Pts',(-26.7073523713557,24.197444316228,-7.97293493059533));
#37988=CARTESIAN_POINT('Ctrl Pts',(-26.7086785687674,24.1909301015901,-7.97252079842349));
#37989=CARTESIAN_POINT('Ctrl Pts',(-26.7091318793789,24.1886912891946,-7.97237863660468));
#37990=CARTESIAN_POINT('Ctrl Pts',(-26.7099153032998,24.1848008506082,-7.97213189192108));
#37991=CARTESIAN_POINT('Ctrl Pts',(-26.7102465013438,24.1831494515242,-7.9720272465312));
#37992=CARTESIAN_POINT('Ctrl Pts',(-26.7109376417045,24.1796892632944,-7.97180817507932));
#37993=CARTESIAN_POINT('Ctrl Pts',(-26.7112973249707,24.1778804299507,-7.97169376431004));
#37994=CARTESIAN_POINT('Ctrl Pts',(-26.7121819299133,24.1734117357072,-7.97141138397589));
#37995=CARTESIAN_POINT('Ctrl Pts',(-26.7127050494356,24.1707515131819,-7.97124351829627));
#37996=CARTESIAN_POINT('Ctrl Pts',(-26.714749014116,24.1602876008245,-7.970584139389));
#37997=CARTESIAN_POINT('Ctrl Pts',(-26.7162443534286,24.1524788684637,-7.97009407839292));
#37998=CARTESIAN_POINT('Ctrl Pts',(-26.7412387479329,24.0192906178819,-7.96176832121097));
#37999=CARTESIAN_POINT('Ctrl Pts',(-26.7573053855183,23.8926127085319,-7.95434433055858));
#38000=CARTESIAN_POINT('Ctrl Pts',(-26.7705420263195,23.6946878378139,-7.94305245767932));
#38001=CARTESIAN_POINT('Ctrl Pts',(-26.7729373045662,23.6239369448992,-7.93907683542844));
#38002=CARTESIAN_POINT('Ctrl Pts',(-26.7730990812615,23.4447935440941,-7.9290490962535));
#38003=CARTESIAN_POINT('Ctrl Pts',(-26.7677307660088,23.3364887109567,-7.92302063020588));
#38004=CARTESIAN_POINT('Ctrl Pts',(-26.7372827827145,23.0328840570655,-7.90582579634958));
#38005=CARTESIAN_POINT('Ctrl Pts',(-26.6997648651561,22.8393472354877,-7.89448984911841));
#38006=CARTESIAN_POINT('Ctrl Pts',(-26.6414829389786,22.6389036114505,-7.8818003566766));
#38007=CARTESIAN_POINT('Ctrl Pts',(-26.6380595015311,22.6273709595411,-7.88106697024858));
#38008=CARTESIAN_POINT('Ctrl Pts',(-26.6332583336872,22.6115229093171,-7.88005453761369));
#38009=CARTESIAN_POINT('Ctrl Pts',(-26.6319359257343,22.6071907428344,-7.87977730601066));
#38010=CARTESIAN_POINT('Ctrl Pts',(-26.6296579015256,22.59978396452,-7.8793024971622));
#38011=CARTESIAN_POINT('Ctrl Pts',(-26.6287067999128,22.5967079615213,-7.87910506838526));
#38012=CARTESIAN_POINT('Ctrl Pts',(-26.6268486629605,22.5907302284907,-7.87872092206963));
#38013=CARTESIAN_POINT('Ctrl Pts',(-26.625942127876,22.5878283460515,-7.87853422118583));
#38014=CARTESIAN_POINT('Ctrl Pts',(-26.6237659208148,22.5808966316009,-7.87808772728309));
#38015=CARTESIAN_POINT('Ctrl Pts',(-26.6224924299964,22.5768680130396,-7.87782780876598));
#38016=CARTESIAN_POINT('Ctrl Pts',(-26.6186571450679,22.5648178053215,-7.8770490815737));
#38017=CARTESIAN_POINT('Ctrl Pts',(-26.6160718448458,22.5568037870361,-7.8765294985445));
#38018=CARTESIAN_POINT('Ctrl Pts',(-26.5934589102471,22.4876362501003,-7.87203031425878));
#38019=CARTESIAN_POINT('Ctrl Pts',(-26.5716364968613,22.4270889667166,-7.86799155454542));
#38020=CARTESIAN_POINT('Ctrl Pts',(-26.5113142837528,22.274232058428,-7.85752532548827));
#38021=CARTESIAN_POINT('Ctrl Pts',(-26.4703058205187,22.1829923266424,-7.85101822124881));
#38022=CARTESIAN_POINT('Ctrl Pts',(-26.2882392541963,21.8236101232849,-7.82435943025246));
#38023=CARTESIAN_POINT('Ctrl Pts',(-26.1139600849322,21.5740819773777,-7.80328546753548));
#38024=CARTESIAN_POINT('Ctrl Pts',(-25.8761468421943,21.3190113921817,-7.78073651511226));
#38025=CARTESIAN_POINT('Ctrl Pts',(-25.8441538442873,21.2861326855571,-7.77781130067336));
#38026=CARTESIAN_POINT('Ctrl Pts',(-25.807917245031,21.2504498367488,-7.77462689539191));
#38027=CARTESIAN_POINT('Ctrl Pts',(-25.8043585222615,21.2469617168805,-7.77431550393104));
#38028=CARTESIAN_POINT('Ctrl Pts',(-25.7990283903411,21.241761516157,-7.77385113449051));
#38029=CARTESIAN_POINT('Ctrl Pts',(-25.797263106283,21.2400432102181,-7.77369767010195));
#38030=CARTESIAN_POINT('Ctrl Pts',(-25.7942216271018,21.2370894556621,-7.77343383011151));
#38031=CARTESIAN_POINT('Ctrl Pts',(-25.7929463811705,21.2358530383009,-7.77332337800509));
#38032=CARTESIAN_POINT('Ctrl Pts',(-25.7903062185187,21.233297494212,-7.77309506396332));
#38033=CARTESIAN_POINT('Ctrl Pts',(-25.7889411609392,21.2319785213852,-7.77297721452394));
#38034=CARTESIAN_POINT('Ctrl Pts',(-25.7857271012518,21.2288784553251,-7.77270019634926));
#38035=CARTESIAN_POINT('Ctrl Pts',(-25.7838771297016,21.2270983592676,-7.77254110637254));
#38036=CARTESIAN_POINT('Ctrl Pts',(-25.7778350806992,21.2212984139785,-7.77202267395487));
#38037=CARTESIAN_POINT('Ctrl Pts',(-25.773634232397,21.2172876564159,-7.77166404028104));
#38038=CARTESIAN_POINT('Ctrl Pts',(-25.6700462915769,21.1189210485666,-7.76286442144645));
#38039=CARTESIAN_POINT('Ctrl Pts',(-25.5647370106838,21.0309745787545,-7.75490694471442));
#38040=CARTESIAN_POINT('Ctrl Pts',(-25.1642005083345,20.7377065102569,-7.72671156060172));
#38041=CARTESIAN_POINT('Ctrl Pts',(-24.8408384203233,20.5754185193488,-7.70736257398968));
#38042=CARTESIAN_POINT('Ctrl Pts',(-24.4778610643212,20.4638183409789,-7.68439760225522));
#38043=CARTESIAN_POINT('Ctrl Pts',(-24.4583085677271,20.4580093638461,-7.68315817725747));
#38044=CARTESIAN_POINT('Ctrl Pts',(-24.4326901071784,20.4506621375966,-7.6815307184455));
#38045=CARTESIAN_POINT('Ctrl Pts',(-24.4266726514745,20.4489553097915,-7.68114819685265));
#38046=CARTESIAN_POINT('Ctrl Pts',(-24.4173937443339,20.4463525462855,-7.68055794850676));
#38047=CARTESIAN_POINT('Ctrl Pts',(-24.4141357642512,20.4454442022724,-7.68035062643563));
#38048=CARTESIAN_POINT('Ctrl Pts',(-24.4077191618574,20.4436660973486,-7.67994215296765));
#38049=CARTESIAN_POINT('Ctrl Pts',(-24.4045606306618,20.4427960206846,-7.67974101213375));
#38050=CARTESIAN_POINT('Ctrl Pts',(-24.3975983563228,20.440889548928,-7.67929748032723));
#38051=CARTESIAN_POINT('Ctrl Pts',(-24.3937940313525,20.4398553153815,-7.67905501937595));
#38052=CARTESIAN_POINT('Ctrl Pts',(-24.3859093580297,20.4377273387596,-7.67855228159195));
#38053=CARTESIAN_POINT('Ctrl Pts',(-24.3818287397242,20.4366346331685,-7.67829197152332));
#38054=CARTESIAN_POINT('Ctrl Pts',(-24.3713901654202,20.4338613821585,-7.67762575300873));
#38055=CARTESIAN_POINT('Ctrl Pts',(-24.3650292151008,20.432192274808,-7.67721947376594));
#38056=CARTESIAN_POINT('Ctrl Pts',(-24.2365118091935,20.3988895475909,-7.66900463091696));
#38057=CARTESIAN_POINT('Ctrl Pts',(-24.1126226464172,20.3744418970721,-7.66096355652652));
#38058=CARTESIAN_POINT('Ctrl Pts',(-23.6777772341081,20.3148751691724,-7.63227785922372));
#38059=CARTESIAN_POINT('Ctrl Pts',(-23.3634531601954,20.3177626822699,-7.61054704511752));
#38060=CARTESIAN_POINT('Ctrl Pts',(-23.026956487317,20.3701494345289,-7.58820916618623));
#38061=CARTESIAN_POINT('Ctrl Pts',(-22.9994712860129,20.3747943637344,-7.58639314134667));
#38062=CARTESIAN_POINT('Ctrl Pts',(-22.9625873822551,20.3815209662901,-7.58397058567214));
#38063=CARTESIAN_POINT('Ctrl Pts',(-22.9531334561969,20.3832888634942,-7.58335093081142));
#38064=CARTESIAN_POINT('Ctrl Pts',(-22.908650358688,20.3918135347791,-7.58044178940181));
#38065=CARTESIAN_POINT('Ctrl Pts',(-22.8737253039417,20.3991096565588,-7.57817669532825));
#38066=CARTESIAN_POINT('Ctrl Pts',(-22.8344004436264,20.4080089243122,-7.57565325381026));
#38067=CARTESIAN_POINT('Ctrl Pts',(-22.8298762199363,20.4090430400775,-7.5753633444375));
#38068=CARTESIAN_POINT('Ctrl Pts',(-22.8230383767599,20.4106215367747,-7.57492581067109));
#38069=CARTESIAN_POINT('Ctrl Pts',(-22.8207231241657,20.4111587046422,-7.57477777384441));
#38070=CARTESIAN_POINT('Ctrl Pts',(-22.8167005900308,20.4120966740617,-7.57452076661325));
#38071=CARTESIAN_POINT('Ctrl Pts',(-22.814993041676,20.4124963078483,-7.57441172858877));
#38072=CARTESIAN_POINT('Ctrl Pts',(-22.8114218868183,20.4133351743791,-7.5741838148974));
#38073=CARTESIAN_POINT('Ctrl Pts',(-22.8095583467037,20.4137746738455,-7.57406495533706));
#38074=CARTESIAN_POINT('Ctrl Pts',(-22.805106415622,20.4148288114091,-7.57378117606285));
#38075=CARTESIAN_POINT('Ctrl Pts',(-22.8025183842176,20.4154449961598,-7.57361634623355));
#38076=CARTESIAN_POINT('Ctrl Pts',(-22.7937686629748,20.4175396704427,-7.57305954378833));
#38077=CARTESIAN_POINT('Ctrl Pts',(-22.7876105209057,20.4190331398793,-7.57266843402244));
#38078=CARTESIAN_POINT('Ctrl Pts',(-22.7729971040031,20.4226228466437,-7.57174207224171));
#38079=CARTESIAN_POINT('Ctrl Pts',(-22.7645457942233,20.4247352347653,-7.57120772814764));
#38080=CARTESIAN_POINT('Ctrl Pts',(-22.6657505800121,20.4498549461405,-7.56497650322715));
#38081=CARTESIAN_POINT('Ctrl Pts',(-22.5764277707128,20.4767402306257,-7.55949147945837));
#38082=CARTESIAN_POINT('Ctrl Pts',(-22.1143153238479,20.6380070601651,-7.53130129787237));
#38083=CARTESIAN_POINT('Ctrl Pts',(-21.7675303923484,20.8363923443027,-7.510320278491));
#38084=CARTESIAN_POINT('Ctrl Pts',(-21.4512084036797,21.1047513549594,-7.48520708112283));
#38085=CARTESIAN_POINT('Ctrl Pts',(-21.4371552115809,21.1168840947281,-7.48407818197906));
#38086=CARTESIAN_POINT('Ctrl Pts',(-21.4186810127926,21.1331144033881,-7.48257620904785));
#38087=CARTESIAN_POINT('Ctrl Pts',(-21.4141653513498,21.1371040843972,-7.482207644042));
#38088=CARTESIAN_POINT('Ctrl Pts',(-21.4071670854613,21.1433222331838,-7.48163420149487));
#38089=CARTESIAN_POINT('Ctrl Pts',(-21.4046766907698,21.1455419456881,-7.48142969205957));
#38090=CARTESIAN_POINT('Ctrl Pts',(-21.3997447499392,21.1499515922087,-7.48102379880451));
#38091=CARTESIAN_POINT('Ctrl Pts',(-21.3973030910476,21.1521413946996,-7.4808224206613));
#38092=CARTESIAN_POINT('Ctrl Pts',(-21.3918772712116,21.1570225080977,-7.48037395518879));
#38093=CARTESIAN_POINT('Ctrl Pts',(-21.3888947964292,21.1597156775789,-7.48012678938378));
#38094=CARTESIAN_POINT('Ctrl Pts',(-21.3827094557098,21.1653220669865,-7.47961283155348));
#38095=CARTESIAN_POINT('Ctrl Pts',(-21.3795074093389,21.1682361754918,-7.47934600202121));
#38096=CARTESIAN_POINT('Ctrl Pts',(-21.3712723405181,21.1757611166437,-7.47865779238412));
#38097=CARTESIAN_POINT('Ctrl Pts',(-21.366248095886,21.1803814852224,-7.47823600581103));
#38098=CARTESIAN_POINT('Ctrl Pts',(-21.2264437084075,21.3097698042006,-7.46644576468609));
#38099=CARTESIAN_POINT('Ctrl Pts',(-21.1025845550344,21.4457928625825,-7.45457460958322));
#38100=CARTESIAN_POINT('Ctrl Pts',(-20.8003020252485,21.8407675532035,-7.42145620117746));
#38101=CARTESIAN_POINT('Ctrl Pts',(-20.6470248879265,22.1164345263202,-7.3995784102034));
#38102=CARTESIAN_POINT('Ctrl Pts',(-20.5303172132053,22.4249231191531,-7.37870750556253));
#38103=CARTESIAN_POINT('Ctrl Pts',(-20.5247453215897,22.4399905077765,-7.37769706253502));
#38104=CARTESIAN_POINT('Ctrl Pts',(-20.51807148182,22.4584611501325,-7.37646984976302));
#38105=CARTESIAN_POINT('Ctrl Pts',(-20.516862359323,22.4618250409831,-7.37624681140183));
#38106=CARTESIAN_POINT('Ctrl Pts',(-20.5148771614592,22.4673770474963,-7.37587946408081));
#38107=CARTESIAN_POINT('Ctrl Pts',(-20.5140978536367,22.4695639903065,-7.3757349625728));
#38108=CARTESIAN_POINT('Ctrl Pts',(-20.5126961953752,22.4735108955834,-7.37547453005728));
#38109=CARTESIAN_POINT('Ctrl Pts',(-20.5120730124375,22.4752705522759,-7.37535854927597));
#38110=CARTESIAN_POINT('Ctrl Pts',(-20.5107353484412,22.4790581151543,-7.37510918358271));
#38111=CARTESIAN_POINT('Ctrl Pts',(-20.5100213697326,22.481086189529,-7.3749758292263));
#38112=CARTESIAN_POINT('Ctrl Pts',(-20.5080693629404,22.4866486792233,-7.37461053452757));
#38113=CARTESIAN_POINT('Ctrl Pts',(-20.5068354601497,22.4901845545296,-7.37437884104576));
#38114=CARTESIAN_POINT('Ctrl Pts',(-20.500429236452,22.5086456270193,-7.37317177852662));
#38115=CARTESIAN_POINT('Ctrl Pts',(-20.4953604176021,22.5236068910809,-7.37220249846643));
#38116=CARTESIAN_POINT('Ctrl Pts',(-20.446006030417,22.6728852565413,-7.36261456760133));
#38117=CARTESIAN_POINT('Ctrl Pts',(-20.4104915558757,22.8099611024345,-7.35447612640773));
#38118=CARTESIAN_POINT('Ctrl Pts',(-20.3202263773212,23.2852469436229,-7.32714302270412));
#38119=CARTESIAN_POINT('Ctrl Pts',(-20.3103444437043,23.6295386550922,-7.30856965493013));
#38120=CARTESIAN_POINT('Ctrl Pts',(-20.3574729044258,23.9892218926378,-7.28663275899283));
#38121=CARTESIAN_POINT('Ctrl Pts',(-20.3603229031716,24.0094744641432,-7.28539001900837));
#38122=CARTESIAN_POINT('Ctrl Pts',(-20.3642969379311,24.0358899716173,-7.28375881129066));
#38123=CARTESIAN_POINT('Ctrl Pts',(-20.3652464887885,24.0420789993281,-7.28337588744482));
#38124=CARTESIAN_POINT('Ctrl Pts',(-20.3667369299289,24.0516081184797,-7.28278515471257));
#38125=CARTESIAN_POINT('Ctrl Pts',(-20.3672650577443,24.0549502150887,-7.28257775158426));
#38126=CARTESIAN_POINT('Ctrl Pts',(-20.3683146411837,24.0615250086614,-7.2821693016435));
#38127=CARTESIAN_POINT('Ctrl Pts',(-20.3688357624952,24.0647577554809,-7.28196826568818));
#38128=CARTESIAN_POINT('Ctrl Pts',(-20.3699948404363,24.0718789369338,-7.28152496175955));
#38129=CARTESIAN_POINT('Ctrl Pts',(-20.3706350028136,24.0757670027254,-7.28128262387341));
#38130=CARTESIAN_POINT('Ctrl Pts',(-20.3719756651998,24.0838174655993,-7.2807802237549));
#38131=CARTESIAN_POINT('Ctrl Pts',(-20.3726772147983,24.0879796780882,-7.28052012848436));
#38132=CARTESIAN_POINT('Ctrl Pts',(-20.374491327004,24.0986150698178,-7.27985463426606));
#38133=CARTESIAN_POINT('Ctrl Pts',(-20.3756155013793,24.1050862249402,-7.27944886567115));
#38134=CARTESIAN_POINT('Ctrl Pts',(-20.3985112787847,24.2345346827897,-7.27131481831905));
#38135=CARTESIAN_POINT('Ctrl Pts',(-20.4273904825377,24.3561313698521,-7.26335885976496));
#38136=CARTESIAN_POINT('Ctrl Pts',(-20.5518396320275,24.7712397858069,-7.23504924387579));
#38137=CARTESIAN_POINT('Ctrl Pts',(-20.6823820105249,25.0524390524938,-7.2136390709152));
#38138=CARTESIAN_POINT('Ctrl Pts',(-20.8606112213619,25.3257144778976,-7.19218286367889));
#38139=CARTESIAN_POINT('Ctrl Pts',(-20.8704758257952,25.3405687973587,-7.19101501618376));
#38140=CARTESIAN_POINT('Ctrl Pts',(-20.8875747195906,25.3658586643454,-7.18902500362645));
#38141=CARTESIAN_POINT('Ctrl Pts',(-20.8947482518326,25.3763346189272,-7.18820015798606));
#38142=CARTESIAN_POINT('Ctrl Pts',(-20.9045778682259,25.390508998168,-7.18708369444735));
#38143=CARTESIAN_POINT('Ctrl Pts',(-20.9071800611662,25.3942444522974,-7.18678942712698));
#38144=CARTESIAN_POINT('Ctrl Pts',(-20.9105833375204,25.3991078590964,-7.18640626455059));
#38145=CARTESIAN_POINT('Ctrl Pts',(-20.9113772309816,25.4002408083155,-7.18631700261827));
#38146=CARTESIAN_POINT('Ctrl Pts',(-20.9136496699999,25.403479320753,-7.18606184212426));
#38147=CARTESIAN_POINT('Ctrl Pts',(-20.91513001128,25.4055836300355,-7.18589603628198));
#38148=CARTESIAN_POINT('Ctrl Pts',(-20.9393438542113,25.4399162358462,-7.18319074019616));
#38149=CARTESIAN_POINT('Ctrl Pts',(-20.9626658713115,25.4717281792872,-7.18068244356887));
#38150=CARTESIAN_POINT('Ctrl Pts',(-20.9894618910131,25.5069057140191,-7.17791429256693));
#38151=CARTESIAN_POINT('Ctrl Pts',(-20.9923649640141,25.5106993106473,-7.17761584461479));
#38152=CARTESIAN_POINT('Ctrl Pts',(-20.9967462855692,25.5163983118868,-7.17716762433079));
#38153=CARTESIAN_POINT('Ctrl Pts',(-20.9982182392707,25.518308513712,-7.17701741085929));
#38154=CARTESIAN_POINT('Ctrl Pts',(-21.0007697668526,25.5216120374818,-7.17675767054288));
#38155=CARTESIAN_POINT('Ctrl Pts',(-21.0018483394941,25.5230061256575,-7.17664807254734));
#38156=CARTESIAN_POINT('Ctrl Pts',(-21.0040965053413,25.5259070284073,-7.17642004174227));
#38157=CARTESIAN_POINT('Ctrl Pts',(-21.0052662913075,25.5274136877906,-7.17630162355166));
#38158=CARTESIAN_POINT('Ctrl Pts',(-21.008046555063,25.5309880526312,-7.17602072565351));
#38159=CARTESIAN_POINT('Ctrl Pts',(-21.009658223546,25.5330548398034,-7.17585833106925));
#38160=CARTESIAN_POINT('Ctrl Pts',(-21.015034671403,25.53993222416,-7.17531803470594));
#38161=CARTESIAN_POINT('Ctrl Pts',(-21.0188106364079,25.5447341209768,-7.17494092753518));
#38162=CARTESIAN_POINT('Ctrl Pts',(-21.0277613206181,25.5560503443414,-7.17405247575955));
#38163=CARTESIAN_POINT('Ctrl Pts',(-21.0329476853058,25.5625554634222,-7.17354194281066));
#38164=CARTESIAN_POINT('Ctrl Pts',(-21.2231435446671,25.7992270438193,-7.15497157238212));
#38165=CARTESIAN_POINT('Ctrl Pts',(-21.43892396765,26.0029413827232,-7.13903697806157));
#38166=CARTESIAN_POINT('Ctrl Pts',(-21.8054377756668,26.2642292166013,-7.1137044483494));
#38167=CARTESIAN_POINT('Ctrl Pts',(-21.9376365380647,26.3447954713216,-7.10486479826434));
#38168=CARTESIAN_POINT('Ctrl Pts',(-22.0750362267429,26.4155368833958,-7.0956801988874));
#38169=CARTESIAN_POINT('Origin',(-23.5502525316942,23.5502525316942,-77.3107734492734));
#38170=CARTESIAN_POINT('',(-22.0750360126322,26.415536773159,-5.59931610453398));
#38171=CARTESIAN_POINT('',(-22.0750360153462,26.4155367745563,-5.84297427009708));
#38172=CARTESIAN_POINT('',(-22.0750360153461,26.4155367745563,-77.3107734492734));
#38173=CARTESIAN_POINT('',(-26.7730012642694,23.5472912798725,-6.43954486607156));
#38174=CARTESIAN_POINT('Ctrl Pts',(-22.0750360126322,26.415536773159,-5.59931610453398));
#38175=CARTESIAN_POINT('Ctrl Pts',(-22.063724523342,26.4097129544905,-5.60012170027255));
#38176=CARTESIAN_POINT('Ctrl Pts',(-22.0524467684468,26.4038217657381,-5.60092356050259));
#38177=CARTESIAN_POINT('Ctrl Pts',(-22.035388410705,26.3947819421545,-5.6021340599298));
#38178=CARTESIAN_POINT('Ctrl Pts',(-22.0295828565831,26.391682561278,-5.60254561634457));
#38179=CARTESIAN_POINT('Ctrl Pts',(-22.0215807446687,26.3873789659974,-5.60311226489102));
#38180=CARTESIAN_POINT('Ctrl Pts',(-22.0193760875055,26.3861899691922,-5.60326831651584));
#38181=CARTESIAN_POINT('Ctrl Pts',(-22.0156007797741,26.3841482173037,-5.6035354279953));
#38182=CARTESIAN_POINT('Ctrl Pts',(-22.0140294527887,26.3832967262774,-5.60364656869388));
#38183=CARTESIAN_POINT('Ctrl Pts',(-22.0109627599141,26.3816316054116,-5.60386340928337));
#38184=CARTESIAN_POINT('Ctrl Pts',(-22.0094673343102,26.3808180999374,-5.60396911645944));
#38185=CARTESIAN_POINT('Ctrl Pts',(-22.0058484757369,26.3788457379252,-5.60422484709094));
#38186=CARTESIAN_POINT('Ctrl Pts',(-22.003725696766,26.3776856720766,-5.60437479255021));
#38187=CARTESIAN_POINT('Ctrl Pts',(-21.9972864569809,26.3741573059139,-5.60482945192425));
#38188=CARTESIAN_POINT('Ctrl Pts',(-21.9929740897392,26.3717814892022,-5.60513368482178));
#38189=CARTESIAN_POINT('Ctrl Pts',(-21.9518812703501,26.3490192737425,-5.6080304856339));
#38190=CARTESIAN_POINT('Ctrl Pts',(-21.9154955631361,26.3279235049876,-5.61057821400722));
#38191=CARTESIAN_POINT('Ctrl Pts',(-21.8071402780183,26.262234035031,-5.61814493675557));
#38192=CARTESIAN_POINT('Ctrl Pts',(-21.7365008852309,26.2155088454694,-5.62305057754278));
#38193=CARTESIAN_POINT('Ctrl Pts',(-21.4915986841601,26.0392637084911,-5.64026052344134));
#38194=CARTESIAN_POINT('Ctrl Pts',(-21.3286757484282,25.8949988838077,-5.65212942729478));
#38195=CARTESIAN_POINT('Ctrl Pts',(-21.1345504790544,25.684565793705,-5.66839747726744));
#38196=CARTESIAN_POINT('Ctrl Pts',(-21.0892666023558,25.6321884098,-5.67237000093987));
#38197=CARTESIAN_POINT('Ctrl Pts',(-20.9842346285269,25.5024848115661,-5.6820896367509));
#38198=CARTESIAN_POINT('Ctrl Pts',(-20.9262516058788,25.4238253127145,-5.68789078817834));
#38199=CARTESIAN_POINT('Ctrl Pts',(-20.8667487331098,25.3349126754141,-5.69440291406271));
#38200=CARTESIAN_POINT('Ctrl Pts',(-20.8615976667254,25.3271429278105,-5.69497159930759));
#38201=CARTESIAN_POINT('Ctrl Pts',(-20.8539998478598,25.3155738756375,-5.69581783669036));
#38202=CARTESIAN_POINT('Ctrl Pts',(-20.8515272268767,25.3117915495037,-5.69609441788861));
#38203=CARTESIAN_POINT('Ctrl Pts',(-20.8473081291278,25.3053079343158,-5.69656839280282));
#38204=CARTESIAN_POINT('Ctrl Pts',(-20.8455577215627,25.3026092001756,-5.69676563917922));
#38205=CARTESIAN_POINT('Ctrl Pts',(-20.8421603277807,25.2973539671783,-5.69714965953264));
#38206=CARTESIAN_POINT('Ctrl Pts',(-20.8405129137032,25.2947977484659,-5.69733641721698));
#38207=CARTESIAN_POINT('Ctrl Pts',(-20.8365814337363,25.2886784424515,-5.697783412599));
#38208=CARTESIAN_POINT('Ctrl Pts',(-20.8343007682676,25.2851131870638,-5.69804377660317));
#38209=CARTESIAN_POINT('Ctrl Pts',(-20.827763521138,25.2748493366561,-5.6987931428397));
#38210=CARTESIAN_POINT('Ctrl Pts',(-20.8235246748178,25.2681395317649,-5.69928280294182));
#38211=CARTESIAN_POINT('Ctrl Pts',(-20.7903870258501,25.2152532413282,-5.70314062634239));
#38212=CARTESIAN_POINT('Ctrl Pts',(-20.7626399347143,25.1683688426381,-5.70655101200951));
#38213=CARTESIAN_POINT('Ctrl Pts',(-20.6727389245209,25.0072819688946,-5.71824650037768));
#38214=CARTESIAN_POINT('Ctrl Pts',(-20.6163171685644,24.8900418754303,-5.72672830605924));
#38215=CARTESIAN_POINT('Ctrl Pts',(-20.4935755162458,24.5897872262508,-5.7483164924717));
#38216=CARTESIAN_POINT('Ctrl Pts',(-20.4364509153238,24.4035635391301,-5.76160629553261));
#38217=CARTESIAN_POINT('Ctrl Pts',(-20.3752536246944,24.1124974193806,-5.78155445360239));
#38218=CARTESIAN_POINT('Ctrl Pts',(-20.3588974691573,24.0106808575185,-5.78837694683938));
#38219=CARTESIAN_POINT('Ctrl Pts',(-20.3467322294419,23.9018442567204,-5.79539362631764));
#38220=CARTESIAN_POINT('Ctrl Pts',(-20.3460357703165,23.8954394602199,-5.795805526485));
#38221=CARTESIAN_POINT('Ctrl Pts',(-20.3426088837517,23.8630207599918,-5.79788512881315));
#38222=CARTESIAN_POINT('Ctrl Pts',(-20.340175923412,23.8369754166747,-5.79953869060973));
#38223=CARTESIAN_POINT('Ctrl Pts',(-20.3376857283784,23.8062867878733,-5.80146454788215));
#38224=CARTESIAN_POINT('Ctrl Pts',(-20.3373211500304,23.8016703979298,-5.80175364983733));
#38225=CARTESIAN_POINT('Ctrl Pts',(-20.3367849184805,23.7946887907792,-5.80218995257939));
#38226=CARTESIAN_POINT('Ctrl Pts',(-20.3366059256461,23.7923241687189,-5.80233756556574));
#38227=CARTESIAN_POINT('Ctrl Pts',(-20.3362903793652,23.7880935426048,-5.80260137664039));
#38228=CARTESIAN_POINT('Ctrl Pts',(-20.3361528411214,23.7862276197839,-5.80271763038156));
#38229=CARTESIAN_POINT('Ctrl Pts',(-20.3358632126738,23.7822511219033,-5.80296516594238));
#38230=CARTESIAN_POINT('Ctrl Pts',(-20.3357115766012,23.7801405222098,-5.80309642150182));
#38231=CARTESIAN_POINT('Ctrl Pts',(-20.3353132086466,23.7745182321665,-5.80344572604508));
#38232=CARTESIAN_POINT('Ctrl Pts',(-20.3350701508892,23.7710062717047,-5.80366356708278));
#38233=CARTESIAN_POINT('Ctrl Pts',(-20.3339434935503,23.7543304598567,-5.80469629928081));
#38234=CARTESIAN_POINT('Ctrl Pts',(-20.3331349643533,23.7411614148443,-5.80550700483182));
#38235=CARTESIAN_POINT('Ctrl Pts',(-20.3272406890403,23.6344471041889,-5.81203987684769));
#38236=CARTESIAN_POINT('Ctrl Pts',(-20.3261547043276,23.5407157741036,-5.81755050553904));
#38237=CARTESIAN_POINT('Ctrl Pts',(-20.335180784728,23.2589685108632,-5.83378266651929));
#38238=CARTESIAN_POINT('Ctrl Pts',(-20.3576702856288,23.0717553473858,-5.84414029915698));
#38239=CARTESIAN_POINT('Ctrl Pts',(-20.4403388374241,22.6783160947907,-5.8667147990062));
#38240=CARTESIAN_POINT('Ctrl Pts',(-20.5050125597034,22.4739955236306,-5.87895602386481));
#38241=CARTESIAN_POINT('Ctrl Pts',(-20.5946190640516,22.2655264795962,-5.89273967519777));
#38242=CARTESIAN_POINT('Ctrl Pts',(-20.5998817597666,22.2534863522571,-5.89354034775661));
#38243=CARTESIAN_POINT('Ctrl Pts',(-20.6071273374206,22.2371821752148,-5.89463095316069));
#38244=CARTESIAN_POINT('Ctrl Pts',(-20.6090461878465,22.2328896687128,-5.89491868637259));
#38245=CARTESIAN_POINT('Ctrl Pts',(-20.6123141391625,22.2256219279921,-5.89540688198937));
#38246=CARTESIAN_POINT('Ctrl Pts',(-20.6136583869862,22.222644508321,-5.89560717714834));
#38247=CARTESIAN_POINT('Ctrl Pts',(-20.6162562287122,22.2169137115935,-5.8959932628735));
#38248=CARTESIAN_POINT('Ctrl Pts',(-20.6175091774203,22.2141600450138,-5.89617903099987));
#38249=CARTESIAN_POINT('Ctrl Pts',(-20.620474705415,22.2076668292775,-5.89661767558438));
#38250=CARTESIAN_POINT('Ctrl Pts',(-20.6221905668943,22.2039287928653,-5.89687066522584));
#38251=CARTESIAN_POINT('Ctrl Pts',(-20.6271274233568,22.1932278374947,-5.89759625569906));
#38252=CARTESIAN_POINT('Ctrl Pts',(-20.6303661155788,22.1862731568453,-5.89806946860222));
#38253=CARTESIAN_POINT('Ctrl Pts',(-20.6519982108467,22.1402511015888,-5.90121191071184));
#38254=CARTESIAN_POINT('Ctrl Pts',(-20.6711496245791,22.1015467993871,-5.90390740442488));
#38255=CARTESIAN_POINT('Ctrl Pts',(-20.728098030659,21.9920481855956,-5.91169005363148));
#38256=CARTESIAN_POINT('Ctrl Pts',(-20.7677671005214,21.9222691654528,-5.91684185235081));
#38257=CARTESIAN_POINT('Ctrl Pts',(-20.9183734453319,21.6789612794698,-5.93550565588518));
#38258=CARTESIAN_POINT('Ctrl Pts',(-21.0432719840423,21.5146815904178,-5.94946857391438));
#38259=CARTESIAN_POINT('Ctrl Pts',(-21.2846196065572,21.2534137871243,-5.97351840251512));
#38260=CARTESIAN_POINT('Ctrl Pts',(-21.3938335950998,21.1505802439385,-5.98358388905972));
#38261=CARTESIAN_POINT('Ctrl Pts',(-21.5371624265648,21.0333429319211,-5.99547450515909));
#38262=CARTESIAN_POINT('Ctrl Pts',(-21.5648759683189,21.0114248764869,-5.99771730836098));
#38263=CARTESIAN_POINT('Ctrl Pts',(-21.5966219588899,20.987155467447,-6.00021822732889));
#38264=CARTESIAN_POINT('Ctrl Pts',(-21.6003042699486,20.9843529325479,-6.00050729449055));
#38265=CARTESIAN_POINT('Ctrl Pts',(-21.6058842073651,20.9801251002199,-6.00094376853211));
#38266=CARTESIAN_POINT('Ctrl Pts',(-21.6077773730306,20.9786939667895,-6.00109158507234));
#38267=CARTESIAN_POINT('Ctrl Pts',(-21.6110714710975,20.9762095155866,-6.00134831222763));
#38268=CARTESIAN_POINT('Ctrl Pts',(-21.6124716817199,20.9751552496374,-6.00145729011387));
#38269=CARTESIAN_POINT('Ctrl Pts',(-21.6154037770047,20.9729513216398,-6.00168518279387));
#38270=CARTESIAN_POINT('Ctrl Pts',(-21.6169358255962,20.9718018835693,-6.00180408133511));
#38271=CARTESIAN_POINT('Ctrl Pts',(-21.6199914381382,20.9695136275547,-6.00204086807108));
#38272=CARTESIAN_POINT('Ctrl Pts',(-21.6215149892718,20.9683747899856,-6.0021587577056));
#38273=CARTESIAN_POINT('Ctrl Pts',(-21.6268244729824,20.9644133321559,-6.00256899385718));
#38274=CARTESIAN_POINT('Ctrl Pts',(-21.6306156244474,20.9615976671134,-6.00286085150361));
#38275=CARTESIAN_POINT('Ctrl Pts',(-21.6643621075381,20.9366492627511,-6.00544947413248));
#38276=CARTESIAN_POINT('Ctrl Pts',(-21.6946944001577,20.9150278631143,-6.00771112161255));
#38277=CARTESIAN_POINT('Ctrl Pts',(-21.775051020258,20.8598238690149,-6.01355393327951));
#38278=CARTESIAN_POINT('Ctrl Pts',(-21.825655679397,20.8271085018592,-6.01708663232258));
#38279=CARTESIAN_POINT('Ctrl Pts',(-22.0150123232969,20.7120888115148,-6.02988934053061));
#38280=CARTESIAN_POINT('Ctrl Pts',(-22.1589748486629,20.638811515233,-6.03883474407486));
#38281=CARTESIAN_POINT('Ctrl Pts',(-22.5334021454231,20.4823705509512,-6.06152683659764));
#38282=CARTESIAN_POINT('Ctrl Pts',(-22.7689296300542,20.4141093235015,-6.07535300421617));
#38283=CARTESIAN_POINT('Ctrl Pts',(-23.0254904249645,20.3704738189411,-6.09113452621829));
#38284=CARTESIAN_POINT('Ctrl Pts',(-23.0411085526091,20.3679357144448,-6.09209763733198));
#38285=CARTESIAN_POINT('Ctrl Pts',(-23.062323655014,20.3646482172907,-6.0934093610934));
#38286=CARTESIAN_POINT('Ctrl Pts',(-23.0679050204813,20.3637983402095,-6.09375478022829));
#38287=CARTESIAN_POINT('Ctrl Pts',(-23.0767124019181,20.3624809066119,-6.09430037268543));
#38288=CARTESIAN_POINT('Ctrl Pts',(-23.0799369617617,20.3620035682754,-6.09450023532779));
#38289=CARTESIAN_POINT('Ctrl Pts',(-23.0861574309734,20.3610923814813,-6.09488600329405));
#38290=CARTESIAN_POINT('Ctrl Pts',(-23.0891532397423,20.3606578600969,-6.09507188706333));
#38291=CARTESIAN_POINT('Ctrl Pts',(-23.0962361440897,20.3596407210667,-6.09551159565997));
#38292=CARTESIAN_POINT('Ctrl Pts',(-23.1003237485212,20.3590617357452,-6.09576553535798));
#38293=CARTESIAN_POINT('Ctrl Pts',(-23.1087731626088,20.3578814824401,-6.09629082610496));
#38294=CARTESIAN_POINT('Ctrl Pts',(-23.1131351123858,20.357281296172,-6.0965622109116));
#38295=CARTESIAN_POINT('Ctrl Pts',(-23.1371096762377,20.3540325434197,-6.0980549737405));
#38296=CARTESIAN_POINT('Ctrl Pts',(-23.1567447920976,20.351555787205,-6.09928178089781));
#38297=CARTESIAN_POINT('Ctrl Pts',(-23.2903701528085,20.3359493684545,-6.10766082438145));
#38298=CARTESIAN_POINT('Ctrl Pts',(-23.4049555385619,20.3287362512678,-6.11499911898354));
#38299=CARTESIAN_POINT('Ctrl Pts',(-23.6941657212413,20.3259917262129,-6.13391840766884));
#38300=CARTESIAN_POINT('Ctrl Pts',(-23.8684911540879,20.3385112897054,-6.14569976153674));
#38301=CARTESIAN_POINT('Ctrl Pts',(-24.2384028881567,20.3954960500221,-6.17103463608782));
#38302=CARTESIAN_POINT('Ctrl Pts',(-24.4326463636069,20.4442196423082,-6.18454452428901));
#38303=CARTESIAN_POINT('Ctrl Pts',(-24.6321176102573,20.5144954793993,-6.19787402576032));
#38304=CARTESIAN_POINT('Ctrl Pts',(-24.6430703752855,20.5184210556133,-6.19860405301831));
#38305=CARTESIAN_POINT('Ctrl Pts',(-24.6573042499791,20.5236097693767,-6.1995500948583));
#38306=CARTESIAN_POINT('Ctrl Pts',(-24.6606047086928,20.5248190154916,-6.19976926876306));
#38307=CARTESIAN_POINT('Ctrl Pts',(-24.665675975797,20.5266864795396,-6.20010574015303));
#38308=CARTESIAN_POINT('Ctrl Pts',(-24.6674481814717,20.527340853931,-6.20022326769941));
#38309=CARTESIAN_POINT('Ctrl Pts',(-24.6709685207579,20.5286442328724,-6.20045661403557));
#38310=CARTESIAN_POINT('Ctrl Pts',(-24.6727166565766,20.5292931926702,-6.20057243419586));
#38311=CARTESIAN_POINT('Ctrl Pts',(-24.6766109571913,20.5307427193792,-6.20083032261912));
#38312=CARTESIAN_POINT('Ctrl Pts',(-24.6787568271319,20.5315440554394,-6.20097234357785));
#38313=CARTESIAN_POINT('Ctrl Pts',(-24.6831935828207,20.5332062731168,-6.20126581524193));
#38314=CARTESIAN_POINT('Ctrl Pts',(-24.6854843470187,20.5340674781385,-6.2014172464195));
#38315=CARTESIAN_POINT('Ctrl Pts',(-24.6979368805879,20.5387651620218,-6.20223992947922));
#38316=CARTESIAN_POINT('Ctrl Pts',(-24.7080803484192,20.5426504474456,-6.20290827709475));
#38317=CARTESIAN_POINT('Ctrl Pts',(-24.7344815196078,20.5529163343628,-6.20464365123393));
#38318=CARTESIAN_POINT('Ctrl Pts',(-24.7507075798561,20.5593780302172,-6.20570604935727));
#38319=CARTESIAN_POINT('Ctrl Pts',(-24.8016005130155,20.5801260011768,-6.20902754637784));
#38320=CARTESIAN_POINT('Ctrl Pts',(-24.8360722523715,20.5948860095794,-6.21126159755536));
#38321=CARTESIAN_POINT('Ctrl Pts',(-24.9580011324386,20.649630589157,-6.21913398732912));
#38322=CARTESIAN_POINT('Ctrl Pts',(-25.0439221055966,20.6929255204805,-6.22462725559394));
#38323=CARTESIAN_POINT('Ctrl Pts',(-25.1987938595158,20.7798625898991,-6.23465082557216));
#38324=CARTESIAN_POINT('Ctrl Pts',(-25.268268867073,20.822401863889,-6.23919594220282));
#38325=CARTESIAN_POINT('Ctrl Pts',(-25.5543275496574,21.0128222215559,-6.25839756610085));
#38326=CARTESIAN_POINT('Ctrl Pts',(-25.7540132678255,21.1841837558739,-6.27312975266344));
#38327=CARTESIAN_POINT('Ctrl Pts',(-25.9325328898397,21.3797998110134,-6.28918777977869));
#38328=CARTESIAN_POINT('Ctrl Pts',(-25.9343335432908,21.3817778494361,-6.28935007491363));
#38329=CARTESIAN_POINT('Ctrl Pts',(-25.9455147081148,21.3940912477223,-6.29035987219193));
#38330=CARTESIAN_POINT('Ctrl Pts',(-25.9548303431019,21.4044850895927,-6.29121006933741));
#38331=CARTESIAN_POINT('Ctrl Pts',(-25.9676285159456,21.4189525463152,-6.29239061851167));
#38332=CARTESIAN_POINT('Ctrl Pts',(-25.9711689461682,21.4229749309816,-6.29271854318657));
#38333=CARTESIAN_POINT('Ctrl Pts',(-25.9768096314042,21.42941579484,-6.29324315913686));
#38334=CARTESIAN_POINT('Ctrl Pts',(-25.9789163519597,21.4318286197831,-6.29343958054804));
#38335=CARTESIAN_POINT('Ctrl Pts',(-25.9832421302096,21.4367978632578,-6.29384389733176));
#38336=CARTESIAN_POINT('Ctrl Pts',(-25.9854607635615,21.4393546446971,-6.29405180999267));
#38337=CARTESIAN_POINT('Ctrl Pts',(-25.9905904496408,21.4452850107866,-6.29453378858206));
#38338=CARTESIAN_POINT('Ctrl Pts',(-25.993498537112,21.4486611407394,-6.29480797683903));
#38339=CARTESIAN_POINT('Ctrl Pts',(-25.9995612175773,21.4557291717413,-6.29538158684159));
#38340=CARTESIAN_POINT('Ctrl Pts',(-26.0027144844718,21.459422190922,-6.29568106244243));
#38341=CARTESIAN_POINT('Ctrl Pts',(-26.0110943601165,21.4692815086413,-6.29647996562938));
#38342=CARTESIAN_POINT('Ctrl Pts',(-26.0163061113498,21.4754603388099,-6.29698000274442));
#38343=CARTESIAN_POINT('Ctrl Pts',(-26.0577738519428,21.5249997015529,-6.30098415029472));
#38344=CARTESIAN_POINT('Ctrl Pts',(-26.0929047146583,21.5692852378482,-6.30453373693261));
#38345=CARTESIAN_POINT('Ctrl Pts',(-26.2082727622755,21.7228443667021,-6.3167523883879));
#38346=CARTESIAN_POINT('Ctrl Pts',(-26.2827657855241,21.8362351505098,-6.32563382942593));
#38347=CARTESIAN_POINT('Ctrl Pts',(-26.3736137348248,21.9955684839366,-6.33788287018465));
#38348=CARTESIAN_POINT('Ctrl Pts',(-26.3964035121164,22.037693319323,-6.34109979622353));
#38349=CARTESIAN_POINT('Ctrl Pts',(-26.4401216443222,22.1229913843143,-6.34756173858693));
#38350=CARTESIAN_POINT('Ctrl Pts',(-26.4610418595475,22.1661559769787,-6.35080601614751));
#38351=CARTESIAN_POINT('Ctrl Pts',(-26.5682692600392,22.4005907038362,-6.36825539361215));
#38352=CARTESIAN_POINT('Ctrl Pts',(-26.6367132344579,22.5995011482201,-6.38249260988721));
#38353=CARTESIAN_POINT('Ctrl Pts',(-26.6883235926518,22.8162265797965,-6.396550692061));
#38354=CARTESIAN_POINT('Ctrl Pts',(-26.6912376113156,22.8287978729241,-6.39736097356616));
#38355=CARTESIAN_POINT('Ctrl Pts',(-26.6948808735499,22.844955756726,-6.39839550618231));
#38356=CARTESIAN_POINT('Ctrl Pts',(-26.6956795736996,22.8485263223217,-6.3986236840252));
#38357=CARTESIAN_POINT('Ctrl Pts',(-26.6968877156592,22.8539707923373,-6.39897094631893));
#38358=CARTESIAN_POINT('Ctrl Pts',(-26.6973015645529,22.8558436994092,-6.39909028477759));
#38359=CARTESIAN_POINT('Ctrl Pts',(-26.6980740770463,22.8593546427886,-6.39931376911895));
#38360=CARTESIAN_POINT('Ctrl Pts',(-26.6984331330208,22.8609925838192,-6.39941793734522));
#38361=CARTESIAN_POINT('Ctrl Pts',(-26.6992538582189,22.8647505872837,-6.39965672276031));
#38362=CARTESIAN_POINT('Ctrl Pts',(-26.6997146640603,22.8668708322729,-6.39979128935125));
#38363=CARTESIAN_POINT('Ctrl Pts',(-26.7006549725435,22.8712185012591,-6.40006691057121));
#38364=CARTESIAN_POINT('Ctrl Pts',(-26.7011342551285,22.8734459723272,-6.40020795244094));
#38365=CARTESIAN_POINT('Ctrl Pts',(-26.7023419326268,22.8790877538382,-6.40056476235431));
#38366=CARTESIAN_POINT('Ctrl Pts',(-26.7030671448463,22.8825027538046,-6.40078034858068));
#38367=CARTESIAN_POINT('Ctrl Pts',(-26.7051212866385,22.8922535878424,-6.40139480797495));
#38368=CARTESIAN_POINT('Ctrl Pts',(-26.7064366861524,22.8985923013127,-6.40179292063658));
#38369=CARTESIAN_POINT('Ctrl Pts',(-26.7509312414172,23.1163001452387,-6.41542217472304));
#38370=CARTESIAN_POINT('Ctrl Pts',(-26.7728029487694,23.3314996865643,-6.42748399422408));
#38371=CARTESIAN_POINT('Ctrl Pts',(-26.773001172026,23.5472921703334,-6.43954507713563));
#38372=CARTESIAN_POINT('Ctrl Pts',(-26.7730011711998,23.5472912709714,-6.43954502686845));
#38373=CARTESIAN_POINT('Ctrl Pts',(-26.7732230558275,23.7887689553493,-6.45304170831777));
#38374=CARTESIAN_POINT('Ctrl Pts',(-26.7463060136877,24.0294874392209,-6.46649688886903));
#38375=CARTESIAN_POINT('Ctrl Pts',(-26.6820697803317,24.3119354550827,-6.48374203233462));
#38376=CARTESIAN_POINT('Ctrl Pts',(-26.6703299556146,24.3586810346309,-6.48664260123069));
#38377=CARTESIAN_POINT('Ctrl Pts',(-26.655776080884,24.411580349893,-6.48998385616881));
#38378=CARTESIAN_POINT('Ctrl Pts',(-26.6539852996154,24.4180111555374,-6.49039103739883));
#38379=CARTESIAN_POINT('Ctrl Pts',(-26.6510173503438,24.4285425191072,-6.4910595050076));
#38380=CARTESIAN_POINT('Ctrl Pts',(-26.6498519913166,24.4326464075783,-6.49132040669056));
#38381=CARTESIAN_POINT('Ctrl Pts',(-26.6475700316367,24.4406221770286,-6.49182826619843));
#38382=CARTESIAN_POINT('Ctrl Pts',(-26.6464543104562,24.4444943031065,-6.49207519494048));
#38383=CARTESIAN_POINT('Ctrl Pts',(-26.6444906813123,24.4512613749443,-6.49250738781117));
#38384=CARTESIAN_POINT('Ctrl Pts',(-26.6436459638527,24.4541572478825,-6.49269254739924));
#38385=CARTESIAN_POINT('Ctrl Pts',(-26.6418660094643,24.4602275964951,-6.4930811199475));
#38386=CARTESIAN_POINT('Ctrl Pts',(-26.6409299466505,24.4634018245479,-6.49328455976424));
#38387=CARTESIAN_POINT('Ctrl Pts',(-26.6383132212585,24.4722251326235,-6.49385076100227));
#38388=CARTESIAN_POINT('Ctrl Pts',(-26.6366219550606,24.4778710314381,-6.49421386957783));
#38389=CARTESIAN_POINT('Ctrl Pts',(-26.6298254988347,24.5003350626034,-6.49566184684453));
#38390=CARTESIAN_POINT('Ctrl Pts',(-26.6245983262605,24.5171157025802,-6.4967507138592));
#38391=CARTESIAN_POINT('Ctrl Pts',(-26.5361596965184,24.7930577014278,-6.51477785529035));
#38392=CARTESIAN_POINT('Ctrl Pts',(-26.4206005378816,25.0406364163846,-6.53287137644403));
#38393=CARTESIAN_POINT('Ctrl Pts',(-26.2530808927883,25.3059795584539,-6.55410624166824));
#38394=CARTESIAN_POINT('Ctrl Pts',(-26.2301231170608,25.3408256792051,-6.55693208372932));
#38395=CARTESIAN_POINT('Ctrl Pts',(-26.1843397903856,25.4074635120278,-6.56239947988033));
#38396=CARTESIAN_POINT('Ctrl Pts',(-26.1615987168668,25.4393050685869,-6.56504110869971));
#38397=CARTESIAN_POINT('Ctrl Pts',(-26.0782998946827,25.5515586486335,-6.57444253231218));
#38398=CARTESIAN_POINT('Ctrl Pts',(-26.0145572076743,25.6295445760625,-6.58114193440231));
#38399=CARTESIAN_POINT('Ctrl Pts',(-25.9165222236781,25.738631029702,-6.59062696741362));
#38400=CARTESIAN_POINT('Ctrl Pts',(-25.8850500832053,25.7721781934054,-6.59356058400394));
#38401=CARTESIAN_POINT('Ctrl Pts',(-25.8501346087193,25.8078342610322,-6.59668586638776));
#38402=CARTESIAN_POINT('Ctrl Pts',(-25.8473954805612,25.8106213303006,-6.59693020409052));
#38403=CARTESIAN_POINT('Ctrl Pts',(-25.8429284531141,25.8151500350231,-6.59732729717358));
#38404=CARTESIAN_POINT('Ctrl Pts',(-25.8412036326767,25.816894681273,-6.59748029078148));
#38405=CARTESIAN_POINT('Ctrl Pts',(-25.8378614909972,25.8202675269138,-6.59777609575074));
#38406=CARTESIAN_POINT('Ctrl Pts',(-25.8362444202288,25.8218959708893,-6.59791892666539));
#38407=CARTESIAN_POINT('Ctrl Pts',(-25.833310109964,25.8248446126631,-6.59817757390651));
#38408=CARTESIAN_POINT('Ctrl Pts',(-25.8319934681808,25.826165390157,-6.59829343684241));
#38409=CARTESIAN_POINT('Ctrl Pts',(-25.8293426034048,25.8288199690645,-6.59852632064472));
#38410=CARTESIAN_POINT('Ctrl Pts',(-25.8280083610934,25.8301537364171,-6.59864333893968));
#38411=CARTESIAN_POINT('Ctrl Pts',(-25.8241939423418,25.833960106765,-6.59897731736106));
#38412=CARTESIAN_POINT('Ctrl Pts',(-25.8217108958063,25.8364298493745,-6.59919404871169));
#38413=CARTESIAN_POINT('Ctrl Pts',(-25.8110382634302,25.8470107465006,-6.60012273242578));
#38414=CARTESIAN_POINT('Ctrl Pts',(-25.8028090882138,25.8550821113522,-6.60083156192904));
#38415=CARTESIAN_POINT('Ctrl Pts',(-25.6564107619157,25.9971399518233,-6.61331827075779));
#38416=CARTESIAN_POINT('Ctrl Pts',(-25.5065319231081,26.1185507036374,-6.62417822589037));
#38417=CARTESIAN_POINT('Ctrl Pts',(-25.287432125624,26.2656565608257,-6.63895276722549));
#38418=CARTESIAN_POINT('Ctrl Pts',(-25.2268690493698,26.3034632123035,-6.64293159181647));
#38419=CARTESIAN_POINT('Ctrl Pts',(-25.1037968105329,26.374723427399,-6.65089475792966));
#38420=CARTESIAN_POINT('Ctrl Pts',(-25.0413407091383,26.4081873222685,-6.65487662653799));
#38421=CARTESIAN_POINT('Ctrl Pts',(-24.8711861190572,26.4922590682175,-6.66566099626532));
#38422=CARTESIAN_POINT('Ctrl Pts',(-24.7617121414733,26.5390030068505,-6.67253673072892));
#38423=CARTESIAN_POINT('Ctrl Pts',(-24.6179701255674,26.59118190569,-6.68163753340397));
#38424=CARTESIAN_POINT('Ctrl Pts',(-24.5858474294374,26.6022707810536,-6.68367548845767));
#38425=CARTESIAN_POINT('Ctrl Pts',(-24.533612988942,26.6193827331942,-6.68699905541715));
#38426=CARTESIAN_POINT('Ctrl Pts',(-24.5136067364435,26.6257210531457,-6.68827427018309));
#38427=CARTESIAN_POINT('Ctrl Pts',(-24.4892547224055,26.6331752579444,-6.68982965075675));
#38428=CARTESIAN_POINT('Ctrl Pts',(-24.4849663627025,26.6344781563839,-6.69010366968577));
#38429=CARTESIAN_POINT('Ctrl Pts',(-24.4766681380678,26.6369804439564,-6.69063414685645));
#38430=CARTESIAN_POINT('Ctrl Pts',(-24.4726586250458,26.6381809762597,-6.69089056708677));
#38431=CARTESIAN_POINT('Ctrl Pts',(-24.4657381235725,26.6402384380939,-6.69133334013744));
#38432=CARTESIAN_POINT('Ctrl Pts',(-24.4628282355226,26.6410990751779,-6.69151957130211));
#38433=CARTESIAN_POINT('Ctrl Pts',(-24.4568135995572,26.6428687475485,-6.69190462368179));
#38434=CARTESIAN_POINT('Ctrl Pts',(-24.4537086905922,26.6437772199989,-6.69210346308038));
#38435=CARTESIAN_POINT('Ctrl Pts',(-24.4461984547915,26.6459623860381,-6.69258458190853));
#38436=CARTESIAN_POINT('Ctrl Pts',(-24.441791768956,26.6472343507369,-6.69286701556923));
#38437=CARTESIAN_POINT('Ctrl Pts',(-24.4254727360672,26.6519070297736,-6.69391344129753));
#38438=CARTESIAN_POINT('Ctrl Pts',(-24.4135436439128,26.6552484222353,-6.69467936607175));
#38439=CARTESIAN_POINT('Ctrl Pts',(-24.3967198561104,26.6598563953244,-6.69576103317268));
#38440=CARTESIAN_POINT('Ctrl Pts',(-24.3918408839094,26.6611803940777,-6.69607489502089));
#38441=CARTESIAN_POINT('Ctrl Pts',(-24.1480899071814,26.7267113156639,-6.71176409380519));
#38442=CARTESIAN_POINT('Ctrl Pts',(-23.9026746005692,26.7632027887211,-6.72808190413251));
#38443=CARTESIAN_POINT('Ctrl Pts',(-23.6418869964452,26.7717285467714,-6.74570271557174));
#38444=CARTESIAN_POINT('Ctrl Pts',(-23.6282158027444,26.7720883929734,-6.74662695704583));
#38445=CARTESIAN_POINT('Ctrl Pts',(-23.4682901123197,26.7752793658229,-6.75744302728201));
#38446=CARTESIAN_POINT('Ctrl Pts',(-23.3220038552415,26.768236592781,-6.76738836316686));
#38447=CARTESIAN_POINT('Ctrl Pts',(-23.0852428170791,26.7406069782184,-6.78317298490582));
#38448=CARTESIAN_POINT('Ctrl Pts',(-22.9942764340936,26.7260185553216,-6.78915862237911));
#38449=CARTESIAN_POINT('Ctrl Pts',(-22.8971237741738,26.7061344022,-6.79537939939735));
#38450=CARTESIAN_POINT('Ctrl Pts',(-22.8902014730163,26.7046938699783,-6.79582168698848));
#38451=CARTESIAN_POINT('Ctrl Pts',(-22.8811813799679,26.7027857947686,-6.79639671399809));
#38452=CARTESIAN_POINT('Ctrl Pts',(-22.8790793067976,26.7023389332874,-6.79653062843239));
#38453=CARTESIAN_POINT('Ctrl Pts',(-22.8749451391846,26.7014557634545,-6.79679381644827));
#38454=CARTESIAN_POINT('Ctrl Pts',(-22.8729130170935,26.7010195913567,-6.79692309780114));
#38455=CARTESIAN_POINT('Ctrl Pts',(-22.8690449847572,26.7001854467596,-6.79716901030501));
#38456=CARTESIAN_POINT('Ctrl Pts',(-22.8672090141582,26.6997878378281,-6.79728566115296));
#38457=CARTESIAN_POINT('Ctrl Pts',(-22.8630315150596,26.698879308643,-6.79755092148407));
#38458=CARTESIAN_POINT('Ctrl Pts',(-22.8606902112822,26.6983673822963,-6.79769947198312));
#38459=CARTESIAN_POINT('Ctrl Pts',(-22.8534252176272,26.6967703970234,-6.79816006501327));
#38460=CARTESIAN_POINT('Ctrl Pts',(-22.8485034709469,26.6956763885098,-6.79847159287229));
#38461=CARTESIAN_POINT('Ctrl Pts',(-22.8112758581231,26.6873096870835,-6.80082426945411));
#38462=CARTESIAN_POINT('Ctrl Pts',(-22.7790797355391,26.6795506714261,-6.80283792887449));
#38463=CARTESIAN_POINT('Ctrl Pts',(-22.6005994097372,26.6336162164452,-6.81391228267647));
#38464=CARTESIAN_POINT('Ctrl Pts',(-22.4570056797223,26.5856758862014,-6.82249425602943));
#38465=CARTESIAN_POINT('Ctrl Pts',(-22.2349997944474,26.4937472977537,-6.83597994670178));
#38466=CARTESIAN_POINT('Ctrl Pts',(-22.15417869041,26.4562840724277,-6.84093731780547));
#38467=CARTESIAN_POINT('Ctrl Pts',(-22.075035924178,26.4155367276176,-6.84592209196326));
#38468=CARTESIAN_POINT('',(-26.7730025170003,23.5505602810918,-6.6857734492733));
#38469=CARTESIAN_POINT('Ctrl Pts',(-22.075036226743,26.4155368833958,-7.0956801988874));
#38470=CARTESIAN_POINT('Ctrl Pts',(-22.1173458186021,26.4373203408489,-7.09285197813402));
#38471=CARTESIAN_POINT('Ctrl Pts',(-22.1601486433663,26.4581722041659,-7.08999223830819));
#38472=CARTESIAN_POINT('Ctrl Pts',(-22.2147476759432,26.4832884943005,-7.08633994433301));
#38473=CARTESIAN_POINT('Ctrl Pts',(-22.2261107026674,26.4884359138944,-7.08557960749034));
#38474=CARTESIAN_POINT('Ctrl Pts',(-22.2417045345805,26.495391045298,-7.08453576350786));
#38475=CARTESIAN_POINT('Ctrl Pts',(-22.2459098549835,26.497255909096,-7.08425422069601));
#38476=CARTESIAN_POINT('Ctrl Pts',(-22.2530828130088,26.5004184209584,-7.08377392225219));
#38477=CARTESIAN_POINT('Ctrl Pts',(-22.2560484493447,26.5017206149314,-7.08357532270844));
#38478=CARTESIAN_POINT('Ctrl Pts',(-22.2620424372228,26.5043417696139,-7.08317387774061));
#38479=CARTESIAN_POINT('Ctrl Pts',(-22.2650708626406,26.505660549294,-7.08297102645723));
#38480=CARTESIAN_POINT('Ctrl Pts',(-22.2719802971711,26.5086567523792,-7.08250815920913));
#38481=CARTESIAN_POINT('Ctrl Pts',(-22.2758625844821,26.5103311963064,-7.08224804178803));
#38482=CARTESIAN_POINT('Ctrl Pts',(-22.2839930208616,26.5138189217937,-7.08170320411444));
#38483=CARTESIAN_POINT('Ctrl Pts',(-22.2882417928383,26.5156307186978,-7.08141843382931));
#38484=CARTESIAN_POINT('Ctrl Pts',(-22.2994130414969,26.5203660986127,-7.08066954887109));
#38485=CARTESIAN_POINT('Ctrl Pts',(-22.3063418441918,26.5232746020145,-7.08020492136146));
#38486=CARTESIAN_POINT('Ctrl Pts',(-22.3269976508562,26.5318604405088,-7.07881933870097));
#38487=CARTESIAN_POINT('Ctrl Pts',(-22.3407536603263,26.5374670692928,-7.07789599024569));
#38488=CARTESIAN_POINT('Ctrl Pts',(-22.4918210495548,26.59782408541,-7.06774844861374));
#38489=CARTESIAN_POINT('Ctrl Pts',(-22.6326849268887,26.6431521720975,-7.05820692834398));
#38490=CARTESIAN_POINT('Ctrl Pts',(-23.0794918091771,26.7537124533823,-7.02772847224717));
#38491=CARTESIAN_POINT('Ctrl Pts',(-23.3921120053161,26.7842508786824,-7.00594346111637));
#38492=CARTESIAN_POINT('Ctrl Pts',(-23.7389510308225,26.7676613073852,-6.98365442570308));
#38493=CARTESIAN_POINT('Ctrl Pts',(-23.7736516356324,26.7654382866165,-6.98144781362781));
#38494=CARTESIAN_POINT('Ctrl Pts',(-23.8129022421721,26.7622852068095,-6.97898346116106));
#38495=CARTESIAN_POINT('Ctrl Pts',(-23.8174925478907,26.7619065527234,-6.97869574878871));
#38496=CARTESIAN_POINT('Ctrl Pts',(-23.8244413447299,26.7613183459396,-6.97826096903672));
#38497=CARTESIAN_POINT('Ctrl Pts',(-23.8268004181085,26.7611160347441,-6.97811349646143));
#38498=CARTESIAN_POINT('Ctrl Pts',(-23.8309041055925,26.7607595514616,-6.97785719593905));
#38499=CARTESIAN_POINT('Ctrl Pts',(-23.8326488167634,26.7606065570504,-6.97774830127719));
#38500=CARTESIAN_POINT('Ctrl Pts',(-23.8363026138706,26.760283152516,-6.97752040736914));
#38501=CARTESIAN_POINT('Ctrl Pts',(-23.8382116715723,26.7601124616459,-6.97740142462477));
#38502=CARTESIAN_POINT('Ctrl Pts',(-23.8427808745358,26.7596998152658,-6.97711685715279));
#38503=CARTESIAN_POINT('Ctrl Pts',(-23.8454408814307,26.7594562546907,-6.97695136361522));
#38504=CARTESIAN_POINT('Ctrl Pts',(-23.8544728812748,26.7586179250484,-6.97639000251614));
#38505=CARTESIAN_POINT('Ctrl Pts',(-23.8608434572983,26.7580074782208,-6.97599501717646));
#38506=CARTESIAN_POINT('Ctrl Pts',(-23.8759898556084,26.7565105620833,-6.97505811564336));
#38507=CARTESIAN_POINT('Ctrl Pts',(-23.8847639934306,26.7556070281214,-6.97451713523652));
#38508=CARTESIAN_POINT('Ctrl Pts',(-23.9883944473509,26.7445053264176,-6.96814726139866));
#38509=CARTESIAN_POINT('Ctrl Pts',(-24.0827668335682,26.7301348630574,-6.96254010048603));
#38510=CARTESIAN_POINT('Ctrl Pts',(-24.3929908300243,26.6686935193108,-6.94434540273821));
#38511=CARTESIAN_POINT('Ctrl Pts',(-24.6046358150256,26.6036390121805,-6.93228259038697));
#38512=CARTESIAN_POINT('Ctrl Pts',(-24.9751005463444,26.4466080155529,-6.90952257288052));
#38513=CARTESIAN_POINT('Ctrl Pts',(-25.1359171801091,26.3617858744673,-6.89901059125812));
#38514=CARTESIAN_POINT('Ctrl Pts',(-25.2984602616419,26.2576536687111,-6.8872721525688));
#38515=CARTESIAN_POINT('Ctrl Pts',(-25.3081599031581,26.2513657932325,-6.88656730899386));
#38516=CARTESIAN_POINT('Ctrl Pts',(-25.3215491030216,26.2425834642626,-6.8855882177711));
#38517=CARTESIAN_POINT('Ctrl Pts',(-25.3252677163734,26.2401332888831,-6.88531563252637));
#38518=CARTESIAN_POINT('Ctrl Pts',(-25.3316490224655,26.2359096840775,-6.88484672337184));
#38519=CARTESIAN_POINT('Ctrl Pts',(-25.3343141823218,26.2341399779425,-6.88465053984573));
#38520=CARTESIAN_POINT('Ctrl Pts',(-25.3397394681644,26.2305258548636,-6.88425048038202));
#38521=CARTESIAN_POINT('Ctrl Pts',(-25.3424993872764,26.2286811365328,-6.88404659324187));
#38522=CARTESIAN_POINT('Ctrl Pts',(-25.3488623193335,26.2244139412664,-6.88357567561285));
#38523=CARTESIAN_POINT('Ctrl Pts',(-25.352463290908,26.2219884452374,-6.88330853104305));
#38524=CARTESIAN_POINT('Ctrl Pts',(-25.3600152409071,26.2168794853742,-6.88274692846537));
#38525=CARTESIAN_POINT('Ctrl Pts',(-25.3639651744142,26.2141945023446,-6.88245241312538));
#38526=CARTESIAN_POINT('Ctrl Pts',(-25.3744251400753,26.2070502513257,-6.88167042246911));
#38527=CARTESIAN_POINT('Ctrl Pts',(-25.3809247578297,26.2025758579281,-6.88118237125483));
#38528=CARTESIAN_POINT('Ctrl Pts',(-25.5150022003369,26.1095481574146,-6.87107001317482));
#38529=CARTESIAN_POINT('Ctrl Pts',(-25.6360105228576,26.011925932001,-6.86109065822348));
#38530=CARTESIAN_POINT('Ctrl Pts',(-25.9989603615316,25.6730849136204,-6.82827863802334));
#38531=CARTESIAN_POINT('Ctrl Pts',(-26.2098220653563,25.4020771125344,-6.80434910546385));
#38532=CARTESIAN_POINT('Ctrl Pts',(-26.3755670094173,25.1006470714388,-6.78260606012956));
#38533=CARTESIAN_POINT('Ctrl Pts',(-26.3768891157322,25.098235331595,-6.78243239603754));
#38534=CARTESIAN_POINT('Ctrl Pts',(-26.3841887555581,25.0848790514434,-6.78147232153988));
#38535=CARTESIAN_POINT('Ctrl Pts',(-26.3901059238388,25.0739013755126,-6.7806894689974));
#38536=CARTESIAN_POINT('Ctrl Pts',(-26.3976542763349,25.0597007446438,-6.77968507617528));
#38537=CARTESIAN_POINT('Ctrl Pts',(-26.3993438663491,25.0565092063878,-6.77945988059685));
#38538=CARTESIAN_POINT('Ctrl Pts',(-26.4019182442709,25.0516265253749,-6.77911618704658));
#38539=CARTESIAN_POINT('Ctrl Pts',(-26.4028068930261,25.0499374388918,-6.77899744311836));
#38540=CARTESIAN_POINT('Ctrl Pts',(-26.4044736379315,25.0467625557868,-6.77877453249247));
#38541=CARTESIAN_POINT('Ctrl Pts',(-26.4052520716591,25.0452769469915,-6.77867034449198));
#38542=CARTESIAN_POINT('Ctrl Pts',(-26.4070406500133,25.0418570273374,-6.77843077062982));
#38543=CARTESIAN_POINT('Ctrl Pts',(-26.4080499881461,25.0399223012596,-6.77829543676777));
#38544=CARTESIAN_POINT('Ctrl Pts',(-26.4108532613012,25.0345355783827,-6.77791918406981));
#38545=CARTESIAN_POINT('Ctrl Pts',(-26.4126429196638,25.0310813415682,-6.77767853743976));
#38546=CARTESIAN_POINT('Ctrl Pts',(-26.4225778265608,25.0118205777699,-6.77634012993693));
#38547=CARTESIAN_POINT('Ctrl Pts',(-26.4305986098101,24.9959496843555,-6.77525014625295));
#38548=CARTESIAN_POINT('Ctrl Pts',(-26.558006874156,24.7385743345285,-6.75776792089081));
#38549=CARTESIAN_POINT('Ctrl Pts',(-26.6468022420777,24.4830583426913,-6.7430948502729));
#38550=CARTESIAN_POINT('Ctrl Pts',(-26.7413246266661,24.0377640916672,-6.71756414570334));
#38551=CARTESIAN_POINT('Ctrl Pts',(-26.7641076630816,23.8531243596407,-6.70699749982585));
#38552=CARTESIAN_POINT('Ctrl Pts',(-26.7722890630402,23.628514714336,-6.69357089656174));
#38553=CARTESIAN_POINT('Ctrl Pts',(-26.7730010593588,23.5894451301886,-6.69121578420057));
#38554=CARTESIAN_POINT('Ctrl Pts',(-26.7730025294131,23.5503737872535,-6.68883834809843));
#38555=CARTESIAN_POINT('Ctrl Pts',(-26.7730025170003,23.5505602810918,-6.6857734492733));
#38556=CARTESIAN_POINT('Ctrl Pts',(-26.7730124690381,23.4463425963718,-6.67937532444307));
#38557=CARTESIAN_POINT('Ctrl Pts',(-26.7679627933299,23.3422071110475,-6.67297719961285));
#38558=CARTESIAN_POINT('Ctrl Pts',(-26.757903268745,23.2386529302868,-6.66657907478262));
#38559=CARTESIAN_POINT('Ctrl Pts',(-26.747831610793,23.1349738469139,-6.66017323280859));
#38560=CARTESIAN_POINT('Ctrl Pts',(-26.732738095894,23.0318778447628,-6.65376739083454));
#38561=CARTESIAN_POINT('Ctrl Pts',(-26.7127238958344,22.9298555350112,-6.64736154886052));
#38562=CARTESIAN_POINT('Ctrl Pts',(-26.6926648822893,22.8276047886852,-6.64094136366489));
#38563=CARTESIAN_POINT('Ctrl Pts',(-26.6676632424978,22.7264329132961,-6.63452117846929));
#38564=CARTESIAN_POINT('Ctrl Pts',(-26.6378707209527,22.6268179211993,-6.62810099327366));
#38565=CARTESIAN_POINT('Ctrl Pts',(-26.6080410340008,22.5270786619534,-6.62167279906159));
#38566=CARTESIAN_POINT('Ctrl Pts',(-26.5734086736759,22.4289005179355,-6.6152446048495));
#38567=CARTESIAN_POINT('Ctrl Pts',(-26.5341737343046,22.3327420310774,-6.60881641063743));
#38568=CARTESIAN_POINT('Ctrl Pts',(-26.4948529598919,22.2363731764238,-6.60237415333963));
#38569=CARTESIAN_POINT('Ctrl Pts',(-26.4509096472389,22.1420331531882,-6.59593189604183));
#38570=CARTESIAN_POINT('Ctrl Pts',(-26.4025903952307,22.0501571098174,-6.58948963874403));
#38571=CARTESIAN_POINT('Ctrl Pts',(-26.3861217244632,22.0188429597257,-6.5872939215086));
#38572=CARTESIAN_POINT('Ctrl Pts',(-26.3691450929648,21.9878147911742,-6.58509820427316));
#38573=CARTESIAN_POINT('Ctrl Pts',(-26.3516713914095,21.9570890325732,-6.58290248703773));
#38574=CARTESIAN_POINT('Ctrl Pts',(-26.3025533721021,21.870719902402,-6.5767303957254));
#38575=CARTESIAN_POINT('Ctrl Pts',(-26.2493508985205,21.7864722856375,-6.57055830441309));
#38576=CARTESIAN_POINT('Ctrl Pts',(-26.1922721870792,21.7047580984706,-6.56438621310076));
#38577=CARTESIAN_POINT('Ctrl Pts',(-26.1352708116489,21.6231546259487,-6.55822248436198));
#38578=CARTESIAN_POINT('Ctrl Pts',(-26.0744038836727,21.5440781134574,-6.55205875562318));
#38579=CARTESIAN_POINT('Ctrl Pts',(-26.0099251284088,21.4679153160946,-6.54589502688439));
#38580=CARTESIAN_POINT('Ctrl Pts',(-25.9455146823345,21.3918332060673,-6.53973782803771));
#38581=CARTESIAN_POINT('Ctrl Pts',(-25.8775002953205,21.3186590040293,-6.53358062919102));
#38582=CARTESIAN_POINT('Ctrl Pts',(-25.80617798152,21.2487491258031,-6.52742343034434));
#38583=CARTESIAN_POINT('Ctrl Pts',(-25.7349078000058,21.1788903474585,-6.52127073203664));
#38584=CARTESIAN_POINT('Ctrl Pts',(-25.6603348081736,21.1122914522744,-6.51511803372894));
#38585=CARTESIAN_POINT('Ctrl Pts',(-25.5827935278875,21.0492737910221,-6.50896533542124));
#38586=CARTESIAN_POINT('Ctrl Pts',(-25.5052816513651,20.9862800261566,-6.50281497022548));
#38587=CARTESIAN_POINT('Ctrl Pts',(-25.4248040596408,20.9268650705392,-6.49666460502974));
#38588=CARTESIAN_POINT('Ctrl Pts',(-25.3417294983502,20.8713109794312,-6.49051423983398));
#38589=CARTESIAN_POINT('Ctrl Pts',(-25.2586642141615,20.8157630921595,-6.48436456146178));
#38590=CARTESIAN_POINT('Ctrl Pts',(-25.1730028980841,20.7640754536891,-6.47821488308955));
#38591=CARTESIAN_POINT('Ctrl Pts',(-25.0851436707897,20.7164870591072,-6.47206520471734));
#38592=CARTESIAN_POINT('Ctrl Pts',(-24.997270750165,20.6688912476196,-6.46591456788488));
#38593=CARTESIAN_POINT('Ctrl Pts',(-24.9071996199251,20.6253961559289,-6.45976393105243));
#38594=CARTESIAN_POINT('Ctrl Pts',(-24.8153525073361,20.586194567664,-6.45361329421998));
#38595=CARTESIAN_POINT('Ctrl Pts',(-24.7234071376307,20.5469510419346,-6.44745607749816));
#38596=CARTESIAN_POINT('Ctrl Pts',(-24.62968239192,20.5120103625511,-6.44129886077633));
#38597=CARTESIAN_POINT('Ctrl Pts',(-24.5346198538001,20.4815168738589,-6.43514164405451));
#38598=CARTESIAN_POINT('Ctrl Pts',(-24.4395042806794,20.4510063729741,-6.42898099224669));
#38599=CARTESIAN_POINT('Ctrl Pts',(-24.3430498481901,20.4249481170937,-6.42282034043888));
#38600=CARTESIAN_POINT('Ctrl Pts',(-24.2457106157175,20.4034357884016,-6.41665968863106));
#38601=CARTESIAN_POINT('Ctrl Pts',(-24.148208500095,20.3818874619337,-6.41048872786202));
#38602=CARTESIAN_POINT('Ctrl Pts',(-24.0498190553298,20.3649003313019,-6.40431776709301));
#38603=CARTESIAN_POINT('Ctrl Pts',(-23.9510039263868,20.3525164759585,-6.39814680632398));
#38604=CARTESIAN_POINT('Ctrl Pts',(-23.8755764831212,20.3430636466568,-6.3934363961036));
#38605=CARTESIAN_POINT('Ctrl Pts',(-23.7999011706109,20.336291874113,-6.38872598588321));
#38606=CARTESIAN_POINT('Ctrl Pts',(-23.7241830036435,20.3321994318483,-6.38401557566283));
#38607=CARTESIAN_POINT('Ctrl Pts',(-23.6249688336115,20.3268370693011,-6.3778434843505));
#38608=CARTESIAN_POINT('Ctrl Pts',(-23.5253317077164,20.3260577945984,-6.37167139303816));
#38609=CARTESIAN_POINT('Ctrl Pts',(-23.4257307277596,20.3299090899407,-6.36549930172583));
#38610=CARTESIAN_POINT('Ctrl Pts',(-23.3262646972838,20.3337551671586,-6.35933557298705));
#38611=CARTESIAN_POINT('Ctrl Pts',(-23.2268351456562,20.3422193276125,-6.35317184424825));
#38612=CARTESIAN_POINT('Ctrl Pts',(-23.127904605688,20.3552971655117,-6.34700811550947));
#38613=CARTESIAN_POINT('Ctrl Pts',(-23.0290788733417,20.3683611486691,-6.34085091666278));
#38614=CARTESIAN_POINT('Ctrl Pts',(-22.9307515299165,20.3860290353501,-6.33469371781609));
#38615=CARTESIAN_POINT('Ctrl Pts',(-22.8333824422229,20.4082444417426,-6.3285365189694));
#38616=CARTESIAN_POINT('Ctrl Pts',(-22.7360845254279,20.4304436100201,-6.32238382066169));
#38617=CARTESIAN_POINT('Ctrl Pts',(-22.6397438940379,20.4571835930782,-6.31623112235399));
#38618=CARTESIAN_POINT('Ctrl Pts',(-22.5448117290975,20.4883566557745,-6.31007842404628));
#38619=CARTESIAN_POINT('Ctrl Pts',(-22.4499155625693,20.5195178976012,-6.30392805885053));
#38620=CARTESIAN_POINT('Ctrl Pts',(-22.3564272135155,20.5551087435017,-6.29777769365479));
#38621=CARTESIAN_POINT('Ctrl Pts',(-22.2647833024081,20.5949714244121,-6.29162732845904));
#38622=CARTESIAN_POINT('Ctrl Pts',(-22.1731496253589,20.6348296537774,-6.28547765008684));
#38623=CARTESIAN_POINT('Ctrl Pts',(-22.0833603751052,20.6789585964522,-6.27932797171462));
#38624=CARTESIAN_POINT('Ctrl Pts',(-21.9958318233241,20.7271524938121,-6.27317829334241));
#38625=CARTESIAN_POINT('Ctrl Pts',(-21.9082896297502,20.7753539024485,-6.26702765650995));
#38626=CARTESIAN_POINT('Ctrl Pts',(-21.8230092150584,20.8276213146083,-6.26087701967752));
#38627=CARTESIAN_POINT('Ctrl Pts',(-21.7403810030875,20.8837037111326,-6.25472638284506));
#38628=CARTESIAN_POINT('Ctrl Pts',(-21.6576643962871,20.93984610404,-6.24856916612324));
#38629=CARTESIAN_POINT('Ctrl Pts',(-21.5776060181478,20.999811386696,-6.24241194940142));
#38630=CARTESIAN_POINT('Ctrl Pts',(-21.5005660026429,21.0633060716501,-6.2362547326796));
#38631=CARTESIAN_POINT('Ctrl Pts',(-21.423483006829,21.1268361800289,-6.23009408087179));
#38632=CARTESIAN_POINT('Ctrl Pts',(-21.3494220491909,21.1938993204271,-6.22393342906399));
#38633=CARTESIAN_POINT('Ctrl Pts',(-21.2787073844689,21.2641641242574,-6.21777277725619));
#38634=CARTESIAN_POINT('Ctrl Pts',(-21.2078743889662,21.3345465060909,-6.21160181648715));
#38635=CARTESIAN_POINT('Ctrl Pts',(-21.1403991650312,21.4081409325322,-6.20543085571809));
#38636=CARTESIAN_POINT('Ctrl Pts',(-21.0765666534871,21.4845817596546,-6.19925989494905));
#38637=CARTESIAN_POINT('Ctrl Pts',(-21.0278420989123,21.5429304782428,-6.19454948472867));
#38638=CARTESIAN_POINT('Ctrl Pts',(-20.9812391785367,21.6029369582211,-6.18983907450831));
#38639=CARTESIAN_POINT('Ctrl Pts',(-20.9368672590285,21.664427783974,-6.18512866428793));
#38640=CARTESIAN_POINT('Ctrl Pts',(-20.8787263485569,21.7449997455783,-6.1789565729756));
#38641=CARTESIAN_POINT('Ctrl Pts',(-20.8242126412108,21.8284049003175,-6.17278448166328));
#38642=CARTESIAN_POINT('Ctrl Pts',(-20.7736142485484,21.9142826642855,-6.16661239035095));
#38643=CARTESIAN_POINT('Ctrl Pts',(-20.7230844117058,22.0000440723734,-6.16044866161216));
#38644=CARTESIAN_POINT('Ctrl Pts',(-20.6764595641369,22.0882710599578,-6.15428493287338));
#38645=CARTESIAN_POINT('Ctrl Pts',(-20.6339860177686,22.1785721089075,-6.1481212041346));
#38646=CARTESIAN_POINT('Ctrl Pts',(-20.5915574681364,22.268777492371,-6.14196400528791));
#38647=CARTESIAN_POINT('Ctrl Pts',(-20.553271660124,22.361052177901,-6.13580680644121));
#38648=CARTESIAN_POINT('Ctrl Pts',(-20.5193297345906,22.4549787939932,-6.12964960759453));
#38649=CARTESIAN_POINT('Ctrl Pts',(-20.4854126185464,22.5488367554249,-6.12349690928682));
#38650=CARTESIAN_POINT('Ctrl Pts',(-20.4558332195076,22.6443438394715,-6.1173442109791));
#38651=CARTESIAN_POINT('Ctrl Pts',(-20.430744780573,22.7410622245384,-6.1111915126714));
#38652=CARTESIAN_POINT('Ctrl Pts',(-20.4056658552102,22.8377439338561,-6.10504114747564));
#38653=CARTESIAN_POINT('Ctrl Pts',(-20.3850746151023,22.9356356114981,-6.09889078227992));
#38654=CARTESIAN_POINT('Ctrl Pts',(-20.3690743383633,23.0342846404682,-6.09274041708416));
#38655=CARTESIAN_POINT('Ctrl Pts',(-20.3530758484072,23.1329226531044,-6.08659073871195));
#38656=CARTESIAN_POINT('Ctrl Pts',(-20.3416673720872,23.2323174201236,-6.08044106033971));
#38657=CARTESIAN_POINT('Ctrl Pts',(-20.3349008137088,23.3320075039202,-6.0742913819675));
#38658=CARTESIAN_POINT('Ctrl Pts',(-20.328133200726,23.4317131249495,-6.06814074513503));
#38659=CARTESIAN_POINT('Ctrl Pts',(-20.3260089720974,23.531713720731,-6.06199010830256));
#38660=CARTESIAN_POINT('Ctrl Pts',(-20.3285279818287,23.6315451346419,-6.05583947147009));
#38661=CARTESIAN_POINT('Ctrl Pts',(-20.3310496863713,23.7314833471941,-6.04968225474828));
#38662=CARTESIAN_POINT('Ctrl Pts',(-20.3382245374823,23.8312515813462,-6.04352503802647));
#38663=CARTESIAN_POINT('Ctrl Pts',(-20.3500002869252,23.9303882079353,-6.03736782130466));
#38664=CARTESIAN_POINT('Ctrl Pts',(-20.3617826060106,24.0295801424424,-6.03120716949684));
#38665=CARTESIAN_POINT('Ctrl Pts',(-20.3781708639595,24.1281393391101,-6.02504651768902));
#38666=CARTESIAN_POINT('Ctrl Pts',(-20.3990615482524,24.2256138782157,-6.0188858658812));
#38667=CARTESIAN_POINT('Ctrl Pts',(-20.419987190089,24.3232515268875,-6.01271490511217));
#38668=CARTESIAN_POINT('Ctrl Pts',(-20.4454301968249,24.4198004722806,-6.00654394434313));
#38669=CARTESIAN_POINT('Ctrl Pts',(-20.4752369686842,24.5148233428566,-6.0003729835741));
#38670=CARTESIAN_POINT('Ctrl Pts',(-20.4979890372935,24.5873560841074,-5.99566257335373));
#38671=CARTESIAN_POINT('Ctrl Pts',(-20.5232826416016,24.6589999492179,-5.99095216313338));
#38672=CARTESIAN_POINT('Ctrl Pts',(-20.5510310014623,24.7295691876834,-5.98624175291302));
#38673=CARTESIAN_POINT('Ctrl Pts',(-20.5873810882621,24.8220142171011,-5.9800711604444));
#38674=CARTESIAN_POINT('Ctrl Pts',(-20.628073333324,24.9129398194747,-5.97390056797578));
#38675=CARTESIAN_POINT('Ctrl Pts',(-20.6729602214789,25.0019090076126,-5.96772997550717));
#38676=CARTESIAN_POINT('Ctrl Pts',(-20.7177909247422,25.09076683307,-5.96156710676552));
#38677=CARTESIAN_POINT('Ctrl Pts',(-20.7668056465855,25.1776727252841,-5.95540423802388));
#38678=CARTESIAN_POINT('Ctrl Pts',(-20.8198082354744,25.2622079948243,-5.94924136928223));
#38679=CARTESIAN_POINT('Ctrl Pts',(-20.8727586662569,25.346660075983,-5.94308456521724));
#38680=CARTESIAN_POINT('Ctrl Pts',(-20.929688936328,25.4287458044922,-5.93692776115223));
#38681=CARTESIAN_POINT('Ctrl Pts',(-20.9903566946544,25.5080704154634,-5.93077095708723));
#38682=CARTESIAN_POINT('Ctrl Pts',(-21.0509809855592,25.5873381916938,-5.92461856426812));
#38683=CARTESIAN_POINT('Ctrl Pts',(-21.1153371783464,25.6638484391644,-5.91846617144903));
#38684=CARTESIAN_POINT('Ctrl Pts',(-21.1831398230338,25.7372356105036,-5.91231377862992));
#38685=CARTESIAN_POINT('Ctrl Pts',(-21.2509238758966,25.8106026587128,-5.90616307282773));
#38686=CARTESIAN_POINT('Ctrl Pts',(-21.3221522135677,25.8808480089752,-5.90001236702551));
#38687=CARTESIAN_POINT('Ctrl Pts',(-21.3964998316802,25.9476400409806,-5.89386166122331));
#38688=CARTESIAN_POINT('Ctrl Pts',(-21.4708333489373,26.0144194051317,-5.88771212197111));
#38689=CARTESIAN_POINT('Ctrl Pts',(-21.5482846440256,26.0777464664712,-5.88156258271889));
#38690=CARTESIAN_POINT('Ctrl Pts',(-21.628493597557,26.1373281319742,-5.87541304346668));
#38691=CARTESIAN_POINT('Ctrl Pts',(-21.7087412223504,26.1969385236741,-5.86926053932797));
#38692=CARTESIAN_POINT('Ctrl Pts',(-21.7917488118925,26.2527996536019,-5.86310803518927));
#38693=CARTESIAN_POINT('Ctrl Pts',(-21.8771254373785,26.3046605059723,-5.85695553105056));
#38694=CARTESIAN_POINT('Ctrl Pts',(-21.9417968217631,26.3439442455095,-5.85229511073273));
#38695=CARTESIAN_POINT('Ctrl Pts',(-22.0078268524888,26.3809335524348,-5.8476346904149));
#38696=CARTESIAN_POINT('Ctrl Pts',(-22.0750360153462,26.4155367745563,-5.84297427009707));
#38697=CARTESIAN_POINT('Origin',(-23.5502525316942,23.5502525316942,-77.3107734492734));
#38698=CARTESIAN_POINT('',(-22.0750357159536,26.4155366204114,-4.34479105736985));
#38699=CARTESIAN_POINT('',(-22.075036015346,26.4155367745563,-4.58978870905188));
#38700=CARTESIAN_POINT('',(-22.0750360153461,26.4155367745563,-77.3107734492734));
#38701=CARTESIAN_POINT('Ctrl Pts',(-22.0750357159536,26.4155366204114,-4.34479105736985));
#38702=CARTESIAN_POINT('Ctrl Pts',(-21.9262750432132,26.3389458743798,-4.35595082401482));
#38703=CARTESIAN_POINT('Ctrl Pts',(-21.7835993653722,26.2508318199401,-4.36736202386383));
#38704=CARTESIAN_POINT('Ctrl Pts',(-21.5651824007717,26.091162495296,-4.38558079714581));
#38705=CARTESIAN_POINT('Ctrl Pts',(-21.484985327817,26.0264192458182,-4.39245034300398));
#38706=CARTESIAN_POINT('Ctrl Pts',(-21.3821897363889,25.9349572982021,-4.40136935074242));
#38707=CARTESIAN_POINT('Ctrl Pts',(-21.3567281602756,25.9115581367451,-4.40358831303293));
#38708=CARTESIAN_POINT('Ctrl Pts',(-21.3184678707426,25.8752439182116,-4.40693121407691));
#38709=CARTESIAN_POINT('Ctrl Pts',(-21.3053944240849,25.862623573236,-4.40807504047152));
#38710=CARTESIAN_POINT('Ctrl Pts',(-21.2896333466181,25.8471490905159,-4.40945514163395));
#38711=CARTESIAN_POINT('Ctrl Pts',(-21.286843621777,25.8444000877064,-4.40969946418793));
#38712=CARTESIAN_POINT('Ctrl Pts',(-21.2825033126537,25.840107511556,-4.41007964358257));
#38713=CARTESIAN_POINT('Ctrl Pts',(-21.280949289184,25.8385674450875,-4.41021577623225));
#38714=CARTESIAN_POINT('Ctrl Pts',(-21.2782066756503,25.8358439220824,-4.41045604789312));
#38715=CARTESIAN_POINT('Ctrl Pts',(-21.2770174472398,25.8346611261924,-4.41056023838447));
#38716=CARTESIAN_POINT('Ctrl Pts',(-21.2744801340551,25.8321335939409,-4.41078255000614));
#38717=CARTESIAN_POINT('Ctrl Pts',(-21.2731323214131,25.8307885950075,-4.41090064923559));
#38718=CARTESIAN_POINT('Ctrl Pts',(-21.2692473427699,25.8269048488036,-4.41124108825666));
#38719=CARTESIAN_POINT('Ctrl Pts',(-21.2667132145419,25.8243630462068,-4.41146318487159));
#38720=CARTESIAN_POINT('Ctrl Pts',(-21.2555303040508,25.8131087288927,-4.41244345124847));
#38721=CARTESIAN_POINT('Ctrl Pts',(-21.2469269497937,25.8043509205023,-4.41319805422413));
#38722=CARTESIAN_POINT('Ctrl Pts',(-21.2362602408905,25.7933678748662,-4.41413453696177));
#38723=CARTESIAN_POINT('Ctrl Pts',(-21.2341498583204,25.7911887581915,-4.41431986223902));
#38724=CARTESIAN_POINT('Ctrl Pts',(-21.0574828389286,25.6082516307316,-4.42983811429788));
#38725=CARTESIAN_POINT('Ctrl Pts',(-20.9046305775353,25.4076674774721,-4.44364048320928));
#38726=CARTESIAN_POINT('Ctrl Pts',(-20.6948242768788,25.0530679601789,-4.46669088191714));
#38727=CARTESIAN_POINT('Ctrl Pts',(-20.6234784176463,24.9088958036751,-4.47574346375745));
#38728=CARTESIAN_POINT('Ctrl Pts',(-20.5409574008587,24.7051402815441,-4.48860886784834));
#38729=CARTESIAN_POINT('Ctrl Pts',(-20.5202501028765,24.6496648884683,-4.49211674646901));
#38730=CARTESIAN_POINT('Ctrl Pts',(-20.4942901748366,24.5738012020162,-4.49693603736281));
#38731=CARTESIAN_POINT('Ctrl Pts',(-20.4876911807252,24.5538838120083,-4.49820330736758));
#38732=CARTESIAN_POINT('Ctrl Pts',(-20.4783269438013,24.5246676455887,-4.50006571791261));
#38733=CARTESIAN_POINT('Ctrl Pts',(-20.4754083611208,24.5154182973626,-4.50065583396195));
#38734=CARTESIAN_POINT('Ctrl Pts',(-20.4702426686145,24.4987863250049,-4.50171794011711));
#38735=CARTESIAN_POINT('Ctrl Pts',(-20.4679802308474,24.4914085100104,-4.5021894246017));
#38736=CARTESIAN_POINT('Ctrl Pts',(-20.4645683970457,24.4801382533538,-4.50291020457211));
#38737=CARTESIAN_POINT('Ctrl Pts',(-20.4633998082474,24.4762516125134,-4.50315887037394));
#38738=CARTESIAN_POINT('Ctrl Pts',(-20.4612911866887,24.4691901437063,-4.50361084392879));
#38739=CARTESIAN_POINT('Ctrl Pts',(-20.4603486975989,24.4660160500881,-4.50381407090868));
#38740=CARTESIAN_POINT('Ctrl Pts',(-20.4583327392942,24.4591882071515,-4.50425138260158));
#38741=CARTESIAN_POINT('Ctrl Pts',(-20.4572608522821,24.4555339993288,-4.50448551873203));
#38742=CARTESIAN_POINT('Ctrl Pts',(-20.45438261327,24.4456569084762,-4.5051186223079));
#38743=CARTESIAN_POINT('Ctrl Pts',(-20.4525885551965,24.4394304877248,-4.50551799081654));
#38744=CARTESIAN_POINT('Ctrl Pts',(-20.4446926389493,24.4117131562315,-4.50729702493826));
#38745=CARTESIAN_POINT('Ctrl Pts',(-20.4387956834593,24.3901649653051,-4.5086833526809));
#38746=CARTESIAN_POINT('Ctrl Pts',(-20.4299250072768,24.3563743370221,-4.51086281973684));
#38747=CARTESIAN_POINT('Ctrl Pts',(-20.4267981545735,24.3441725348637,-4.51165094095547));
#38748=CARTESIAN_POINT('Ctrl Pts',(-20.4206339025865,24.3195178272176,-4.51324572502392));
#38749=CARTESIAN_POINT('Ctrl Pts',(-20.4175991068951,24.307064510331,-4.51405245538387));
#38750=CARTESIAN_POINT('Ctrl Pts',(-20.4142687973821,24.293035236027,-4.51496264904633));
#38751=CARTESIAN_POINT('Ctrl Pts',(-20.4139000393392,24.2914766350597,-4.515063787235));
#38752=CARTESIAN_POINT('Ctrl Pts',(-20.4119244060162,24.2830985087457,-4.51560754934112));
#38753=CARTESIAN_POINT('Ctrl Pts',(-20.4103386203709,24.2762740732067,-4.51605083754183));
#38754=CARTESIAN_POINT('Ctrl Pts',(-20.3409299126837,23.9730923382897,-4.5357606624861));
#38755=CARTESIAN_POINT('Ctrl Pts',(-20.3153732059476,23.6686757863615,-4.5564623440001));
#38756=CARTESIAN_POINT('Ctrl Pts',(-20.3410321661644,23.222350528484,-4.5865825014972));
#38757=CARTESIAN_POINT('Ctrl Pts',(-20.3587660258892,23.0801044970532,-4.59610701916792));
#38758=CARTESIAN_POINT('Ctrl Pts',(-20.3889091452484,22.9239325242353,-4.60616713173035));
#38759=CARTESIAN_POINT('Ctrl Pts',(-20.3920276257648,22.9083925571327,-4.60716366477209));
#38760=CARTESIAN_POINT('Ctrl Pts',(-20.3960254110478,22.8892057190212,-4.608387949339));
#38761=CARTESIAN_POINT('Ctrl Pts',(-20.396796531256,22.8855369001591,-4.60862177443541));
#38762=CARTESIAN_POINT('Ctrl Pts',(-20.398020139552,22.8797652948784,-4.60898917145241));
#38763=CARTESIAN_POINT('Ctrl Pts',(-20.3984683307174,22.877661616396,-4.6091229899705));
#38764=CARTESIAN_POINT('Ctrl Pts',(-20.3993093989759,22.8737331891022,-4.60937270778546));
#38765=CARTESIAN_POINT('Ctrl Pts',(-20.3997017526959,22.8719083450851,-4.6094886361724));
#38766=CARTESIAN_POINT('Ctrl Pts',(-20.4005853848317,22.8678158606784,-4.60974846386691));
#38767=CARTESIAN_POINT('Ctrl Pts',(-20.4010775258029,22.8655484143314,-4.6098923124477));
#38768=CARTESIAN_POINT('Ctrl Pts',(-20.4023331689835,22.8597932676649,-4.61025715051243));
#38769=CARTESIAN_POINT('Ctrl Pts',(-20.4031000212082,22.8563062906672,-4.6104779470459));
#38770=CARTESIAN_POINT('Ctrl Pts',(-20.4073379388359,22.8371874381868,-4.61168719781219));
#38771=CARTESIAN_POINT('Ctrl Pts',(-20.4109197558028,22.8215799627082,-4.6126693631131));
#38772=CARTESIAN_POINT('Ctrl Pts',(-20.4861820873531,22.5044900038483,-4.63253379393759));
#38773=CARTESIAN_POINT('Ctrl Pts',(-20.6008718645076,22.2148217555728,-4.64914110241523));
#38774=CARTESIAN_POINT('Ctrl Pts',(-20.8460382011245,21.7876848467198,-4.67697644883709));
#38775=CARTESIAN_POINT('Ctrl Pts',(-20.950146647486,21.63743928333,-4.6875304527898));
#38776=CARTESIAN_POINT('Ctrl Pts',(-21.0721647966423,21.4898446398552,-4.69916290923268));
#38777=CARTESIAN_POINT('Ctrl Pts',(-21.0779618341603,21.4828923290103,-4.69971394672064));
#38778=CARTESIAN_POINT('Ctrl Pts',(-21.0884788797387,21.4703868716219,-4.70071079186515));
#38779=CARTESIAN_POINT('Ctrl Pts',(-21.0931885962287,21.4648251191314,-4.70115617715199));
#38780=CARTESIAN_POINT('Ctrl Pts',(-21.1004914424257,21.4562601938459,-4.70184524054527));
#38781=CARTESIAN_POINT('Ctrl Pts',(-21.1030713417328,21.4532457294312,-4.70208837234911));
#38782=CARTESIAN_POINT('Ctrl Pts',(-21.1078350103882,21.4477004186262,-4.70253676435695));
#38783=CARTESIAN_POINT('Ctrl Pts',(-21.1100171657592,21.4451681877176,-4.70274195751098));
#38784=CARTESIAN_POINT('Ctrl Pts',(-21.1144164638288,21.4400791582594,-4.70315521917378));
#38785=CARTESIAN_POINT('Ctrl Pts',(-21.1166337018437,21.4375224480524,-4.70336329150082));
#38786=CARTESIAN_POINT('Ctrl Pts',(-21.1229672352777,21.4302424123633,-4.70395705293874));
#38787=CARTESIAN_POINT('Ctrl Pts',(-21.1270932661719,21.4255276108418,-4.704343147857));
#38788=CARTESIAN_POINT('Ctrl Pts',(-21.1447688486275,21.4054482343117,-4.70599413223463));
#38789=CARTESIAN_POINT('Ctrl Pts',(-21.1584507481569,21.3902012775273,-4.70726456723108));
#38790=CARTESIAN_POINT('Ctrl Pts',(-21.4104795717445,21.1146736658287,-4.73053503945799));
#38791=CARTESIAN_POINT('Ctrl Pts',(-21.6898020763137,20.8952079582543,-4.75460081916076));
#38792=CARTESIAN_POINT('Ctrl Pts',(-22.1140844665184,20.6622111813712,-4.78713558041646));
#38793=CARTESIAN_POINT('Ctrl Pts',(-22.2329577440848,20.6060880611204,-4.79583583709514));
#38794=CARTESIAN_POINT('Ctrl Pts',(-22.3692751074134,20.5516448146644,-4.80511680044956));
#38795=CARTESIAN_POINT('Ctrl Pts',(-22.383653961665,20.5460215624655,-4.80608731914136));
#38796=CARTESIAN_POINT('Ctrl Pts',(-22.4015440219804,20.5391729685263,-4.80728388699194));
#38797=CARTESIAN_POINT('Ctrl Pts',(-22.4050173503216,20.5378502086811,-4.80751568909807));
#38798=CARTESIAN_POINT('Ctrl Pts',(-22.4104976494858,20.5357739753785,-4.8078806197986));
#38799=CARTESIAN_POINT('Ctrl Pts',(-22.4125030833258,20.5350164960235,-4.80801398952256));
#38800=CARTESIAN_POINT('Ctrl Pts',(-22.4162567761788,20.5336029538071,-4.80826330348295));
#38801=CARTESIAN_POINT('Ctrl Pts',(-22.4180048376903,20.5329464138562,-4.80837927590459));
#38802=CARTESIAN_POINT('Ctrl Pts',(-22.4219355383993,20.5314740113963,-4.80863975890777));
#38803=CARTESIAN_POINT('Ctrl Pts',(-22.4241184877748,20.5306589982547,-4.80878421762349));
#38804=CARTESIAN_POINT('Ctrl Pts',(-22.429678242136,20.5285901086195,-4.80915162805047));
#38805=CARTESIAN_POINT('Ctrl Pts',(-22.433056279022,20.527339520914,-4.80937438206729));
#38806=CARTESIAN_POINT('Ctrl Pts',(-22.4518342381622,20.5204234822103,-4.81061000825419));
#38807=CARTESIAN_POINT('Ctrl Pts',(-22.4672755241837,20.5148699125292,-4.81161626718249));
#38808=CARTESIAN_POINT('Ctrl Pts',(-22.7823357146298,20.404266542287,-4.83196164689188));
#38809=CARTESIAN_POINT('Ctrl Pts',(-23.0958648649883,20.3439251613509,-4.8489239496657));
#38810=CARTESIAN_POINT('Ctrl Pts',(-23.5876807533102,20.3229914005357,-4.87680349048989));
#38811=CARTESIAN_POINT('Ctrl Pts',(-23.762447907284,20.3297595615514,-4.88692890678008));
#38812=CARTESIAN_POINT('Ctrl Pts',(-23.9446881490625,20.3517187417719,-4.89807994762353));
#38813=CARTESIAN_POINT('Ctrl Pts',(-23.9535801870283,20.3528278396286,-4.89862547577618));
#38814=CARTESIAN_POINT('Ctrl Pts',(-23.9696454134781,20.3548997258443,-4.89961372583772));
#38815=CARTESIAN_POINT('Ctrl Pts',(-23.9768202274092,20.3558496230479,-4.90005603863156));
#38816=CARTESIAN_POINT('Ctrl Pts',(-23.9879077508608,20.3573555572028,-4.90074105970012));
#38817=CARTESIAN_POINT('Ctrl Pts',(-23.9918227712544,20.3578946407468,-4.90098323057203));
#38818=CARTESIAN_POINT('Ctrl Pts',(-23.999015638813,20.3588985562542,-4.90142869364828));
#38819=CARTESIAN_POINT('Ctrl Pts',(-24.0022937843447,20.3593612410609,-4.90163191751159));
#38820=CARTESIAN_POINT('Ctrl Pts',(-24.0089231181076,20.3603073409678,-4.90204330908025));
#38821=CARTESIAN_POINT('Ctrl Pts',(-24.0122742685986,20.3607909876138,-4.90225148389443));
#38822=CARTESIAN_POINT('Ctrl Pts',(-24.0218323906047,20.3621858203471,-4.90284585514284));
#38823=CARTESIAN_POINT('Ctrl Pts',(-24.0280374468001,20.3631098468846,-4.90323245872544));
#38824=CARTESIAN_POINT('Ctrl Pts',(-24.05456090029,20.3671387872321,-4.90488819944509));
#38825=CARTESIAN_POINT('Ctrl Pts',(-24.0748516835591,20.3704198727079,-4.90616292163981));
#38826=CARTESIAN_POINT('Ctrl Pts',(-24.4334012536843,20.4319237026631,-4.92883464387146));
#38827=CARTESIAN_POINT('Ctrl Pts',(-24.7601862213466,20.5436161585164,-4.95216928779469));
#38828=CARTESIAN_POINT('Ctrl Pts',(-25.198225977516,20.7764962408265,-4.98557670102779));
#38829=CARTESIAN_POINT('Ctrl Pts',(-25.3280917825407,20.8578853082174,-4.99573715686729));
#38830=CARTESIAN_POINT('Ctrl Pts',(-25.4563262540549,20.9515926029174,-5.00568447582307));
#38831=CARTESIAN_POINT('Ctrl Pts',(-25.4609482330473,20.9549890771403,-5.00604287650497));
#38832=CARTESIAN_POINT('Ctrl Pts',(-25.4676152467896,20.9599158152456,-5.00655963313597));
#38833=CARTESIAN_POINT('Ctrl Pts',(-25.4696675348971,20.9614361744745,-5.00671867442246));
#38834=CARTESIAN_POINT('Ctrl Pts',(-25.4732400807271,20.964089342112,-5.00699547120869));
#38835=CARTESIAN_POINT('Ctrl Pts',(-25.4747611479507,20.9652210535657,-5.0071133039019));
#38836=CARTESIAN_POINT('Ctrl Pts',(-25.4777081617398,20.9674177471659,-5.0073415647418));
#38837=CARTESIAN_POINT('Ctrl Pts',(-25.4791342210247,20.9684825654563,-5.00745200399998));
#38838=CARTESIAN_POINT('Ctrl Pts',(-25.4825428912996,20.9710321719752,-5.00771594730981));
#38839=CARTESIAN_POINT('Ctrl Pts',(-25.4845246776288,20.9725180683774,-5.0078693731546));
#38840=CARTESIAN_POINT('Ctrl Pts',(-25.4916277505714,20.9778565877993,-5.00841917986982));
#38841=CARTESIAN_POINT('Ctrl Pts',(-25.4967393001716,20.9817222331667,-5.00881465031076));
#38842=CARTESIAN_POINT('Ctrl Pts',(-25.5732289574676,21.0399275404345,-5.01473030203032));
#38843=CARTESIAN_POINT('Ctrl Pts',(-25.642327047265,21.0972150550783,-5.02004571108081));
#38844=CARTESIAN_POINT('Ctrl Pts',(-25.9304148951288,21.3571029489143,-5.04252439438099));
#38845=CARTESIAN_POINT('Ctrl Pts',(-26.1230815483506,21.5866699005502,-5.05853233708837));
#38846=CARTESIAN_POINT('Ctrl Pts',(-26.3252470887504,21.909419241752,-5.08051184444434));
#38847=CARTESIAN_POINT('Ctrl Pts',(-26.3663515527543,21.9810127932429,-5.08534804757117));
#38848=CARTESIAN_POINT('Ctrl Pts',(-26.4243610719716,22.0916853103813,-5.09281834347135));
#38849=CARTESIAN_POINT('Ctrl Pts',(-26.4433161068319,22.1296536689628,-5.09537996966839));
#38850=CARTESIAN_POINT('Ctrl Pts',(-26.4647716943873,22.1748423183364,-5.09843116073839));
#38851=CARTESIAN_POINT('Ctrl Pts',(-26.4680038142218,22.1817121937915,-5.09889508562148));
#38852=CARTESIAN_POINT('Ctrl Pts',(-26.4729235547115,22.192265760456,-5.09960789076394));
#38853=CARTESIAN_POINT('Ctrl Pts',(-26.4746285693484,22.1959413526076,-5.09985616838796));
#38854=CARTESIAN_POINT('Ctrl Pts',(-26.4777276056931,22.2026552520006,-5.10030972086817));
#38855=CARTESIAN_POINT('Ctrl Pts',(-26.4791238422937,22.2056925356599,-5.1005149188255));
#38856=CARTESIAN_POINT('Ctrl Pts',(-26.4819235353749,22.2118078624067,-5.10092810403071));
#38857=CARTESIAN_POINT('Ctrl Pts',(-26.4833268759036,22.2148859536462,-5.1011360949586));
#38858=CARTESIAN_POINT('Ctrl Pts',(-26.4873127350398,22.2236651442848,-5.10172937209268));
#38859=CARTESIAN_POINT('Ctrl Pts',(-26.4898834854236,22.2293715417857,-5.10211506304213));
#38860=CARTESIAN_POINT('Ctrl Pts',(-26.5007753394305,22.2537379118671,-5.10376227840026));
#38861=CARTESIAN_POINT('Ctrl Pts',(-26.5089353716632,22.2724689741585,-5.10502931713618));
#38862=CARTESIAN_POINT('Ctrl Pts',(-26.6543177808281,22.6150494472894,-5.12822077501145));
#38863=CARTESIAN_POINT('Ctrl Pts',(-26.7377597233024,22.9590757790159,-5.15219486594882));
#38864=CARTESIAN_POINT('Ctrl Pts',(-26.7700306246897,23.3900790454445,-5.18125307643998));
#38865=CARTESIAN_POINT('Ctrl Pts',(-26.7730316194701,23.470734894779,-5.18663061556587));
#38866=CARTESIAN_POINT('Ctrl Pts',(-26.773000885856,23.5553700292207,-5.19215940808207));
#38867=CARTESIAN_POINT('Ctrl Pts',(-26.772992200676,23.5593172587968,-5.19241699913911));
#38868=CARTESIAN_POINT('Ctrl Pts',(-26.7729306837212,23.5745534210412,-5.19341025665531));
#38869=CARTESIAN_POINT('Ctrl Pts',(-26.7728257872373,23.5858421957659,-5.19414398873007));
#38870=CARTESIAN_POINT('Ctrl Pts',(-26.7726107844339,23.6006216213051,-5.19510153879008));
#38871=CARTESIAN_POINT('Ctrl Pts',(-26.7725543210756,23.6041128372488,-5.19532750878273));
#38872=CARTESIAN_POINT('Ctrl Pts',(-26.7716801497736,23.6532273763693,-5.19850325178169));
#38873=CARTESIAN_POINT('Ctrl Pts',(-26.7698991853338,23.6988313936406,-5.20141308110938));
#38874=CARTESIAN_POINT('Ctrl Pts',(-26.766850391112,23.7493518345502,-5.2045821843114));
#38875=CARTESIAN_POINT('Ctrl Pts',(-26.7665391500096,23.7543179899248,-5.20489312234184));
#38876=CARTESIAN_POINT('Ctrl Pts',(-26.766056743353,23.7617398700845,-5.20535692274102));
#38877=CARTESIAN_POINT('Ctrl Pts',(-26.7658942657873,23.7641961225763,-5.20551026990623));
#38878=CARTESIAN_POINT('Ctrl Pts',(-26.7656097422638,23.7684238494932,-5.20577395776365));
#38879=CARTESIAN_POINT('Ctrl Pts',(-26.7654890465304,23.7701954087584,-5.20588437477081));
#38880=CARTESIAN_POINT('Ctrl Pts',(-26.7652362862405,23.7738607252785,-5.20611266439916));
#38881=CARTESIAN_POINT('Ctrl Pts',(-26.7651040127942,23.7757544623268,-5.2062305244568));
#38882=CARTESIAN_POINT('Ctrl Pts',(-26.7647888091015,23.780210533792,-5.20650764853177));
#38883=CARTESIAN_POINT('Ctrl Pts',(-26.7646044878273,23.7827727753503,-5.2066668336005));
#38884=CARTESIAN_POINT('Ctrl Pts',(-26.7639927858379,23.7911362765147,-5.20718591643801));
#38885=CARTESIAN_POINT('Ctrl Pts',(-26.763552758912,23.7969366427267,-5.20754510292771));
#38886=CARTESIAN_POINT('Ctrl Pts',(-26.7624839937884,23.8105366552394,-5.20838543631905));
#38887=CARTESIAN_POINT('Ctrl Pts',(-26.7618425460042,23.8183353061449,-5.20886588491718));
#38888=CARTESIAN_POINT('Ctrl Pts',(-26.7545638965526,23.9030505377378,-5.21407018181042));
#38889=CARTESIAN_POINT('Ctrl Pts',(-26.7451926698301,23.9797143632219,-5.21864806539345));
#38890=CARTESIAN_POINT('Ctrl Pts',(-26.7200182753869,24.138152583034,-5.227970506302));
#38891=CARTESIAN_POINT('Ctrl Pts',(-26.7037823657742,24.219798938637,-5.23269705143083));
#38892=CARTESIAN_POINT('Ctrl Pts',(-26.6418306540216,24.4785225379532,-5.24767286638111));
#38893=CARTESIAN_POINT('Ctrl Pts',(-26.5842075287858,24.652367482908,-5.25775142085251));
#38894=CARTESIAN_POINT('Ctrl Pts',(-26.5049317543387,24.8372351377853,-5.26921086046796));
#38895=CARTESIAN_POINT('Ctrl Pts',(-26.4975642503108,24.8540190588416,-5.27025803610446));
#38896=CARTESIAN_POINT('Ctrl Pts',(-26.4673510152363,24.9212828381584,-5.27448416730267));
#38897=CARTESIAN_POINT('Ctrl Pts',(-26.44334916078,24.9712307587618,-5.27768968353585));
#38898=CARTESIAN_POINT('Ctrl Pts',(-26.4085814255507,25.0390461023386,-5.28215230478788));
#38899=CARTESIAN_POINT('Ctrl Pts',(-26.3989114385256,25.0574661087759,-5.2833758812833));
#38900=CARTESIAN_POINT('Ctrl Pts',(-26.3581550576753,25.1333079753947,-5.28846361160344));
#38901=CARTESIAN_POINT('Ctrl Pts',(-26.3255071523835,25.1898689500585,-5.29237754452833));
#38902=CARTESIAN_POINT('Ctrl Pts',(-26.2867672102419,25.2525083589832,-5.29686403173555));
#38903=CARTESIAN_POINT('Ctrl Pts',(-26.2823411666535,25.2596030446374,-5.29737442467612));
#38904=CARTESIAN_POINT('Ctrl Pts',(-26.2756094076501,25.2703007165445,-5.29814744679312));
#38905=CARTESIAN_POINT('Ctrl Pts',(-26.2733240247171,25.2739165079744,-5.29840932187725));
#38906=CARTESIAN_POINT('Ctrl Pts',(-26.2693414388832,25.2801898196372,-5.29886470863792));
#38907=CARTESIAN_POINT('Ctrl Pts',(-26.267647517608,25.2828494253302,-5.29905809807799));
#38908=CARTESIAN_POINT('Ctrl Pts',(-26.2641107924049,25.2883844505253,-5.2994612506838));
#38909=CARTESIAN_POINT('Ctrl Pts',(-26.2622673166121,25.2912594336717,-5.29967103872305));
#38910=CARTESIAN_POINT('Ctrl Pts',(-26.2579084261283,25.2980335965865,-5.30016626005236));
#38911=CARTESIAN_POINT('Ctrl Pts',(-26.255389158454,25.3019302770749,-5.30045183715298));
#38912=CARTESIAN_POINT('Ctrl Pts',(-26.2470935474671,25.3147009475393,-5.30139011619081));
#38913=CARTESIAN_POINT('Ctrl Pts',(-26.2412819312013,25.3235518418011,-5.3020441400594));
#38914=CARTESIAN_POINT('Ctrl Pts',(-26.1563762627122,25.4514816963234,-5.31155215632337));
#38915=CARTESIAN_POINT('Ctrl Pts',(-26.0695000848169,25.5651805089211,-5.32070500183791));
#38916=CARTESIAN_POINT('Ctrl Pts',(-25.7591269186931,25.919810698572,-5.35170692088824));
#38917=CARTESIAN_POINT('Ctrl Pts',(-25.5064237377026,26.1323624188969,-5.37464979995359));
#38918=CARTESIAN_POINT('Ctrl Pts',(-25.1926477066409,26.3233699070541,-5.39829770559522));
#38919=CARTESIAN_POINT('Ctrl Pts',(-25.1589301247863,26.3430644895458,-5.40078032831415));
#38920=CARTESIAN_POINT('Ctrl Pts',(-25.1202456072937,26.3647271342287,-5.40355569020661));
#38921=CARTESIAN_POINT('Ctrl Pts',(-25.1156236904286,26.3673003981839,-5.40388611478902));
#38922=CARTESIAN_POINT('Ctrl Pts',(-25.1088570172833,26.3710459650826,-5.40436814095746));
#38923=CARTESIAN_POINT('Ctrl Pts',(-25.1067172606642,26.3722272098077,-5.40452031514336));
#38924=CARTESIAN_POINT('Ctrl Pts',(-25.1029246019762,26.3743153070385,-5.404789590547));
#38925=CARTESIAN_POINT('Ctrl Pts',(-25.1012722470377,26.3752231438615,-5.40490675546279));
#38926=CARTESIAN_POINT('Ctrl Pts',(-25.097817838878,26.3771171202993,-5.40515138402798));
#38927=CARTESIAN_POINT('Ctrl Pts',(-25.0960156430802,26.378102984926,-5.40527882975497));
#38928=CARTESIAN_POINT('Ctrl Pts',(-25.0913606202502,26.3806436668404,-5.40560755945363));
#38929=CARTESIAN_POINT('Ctrl Pts',(-25.0885063735002,26.3821958992278,-5.40580867677183));
#38930=CARTESIAN_POINT('Ctrl Pts',(-25.0763265595334,26.3887958322473,-5.40666502333722));
#38931=CARTESIAN_POINT('Ctrl Pts',(-25.0669783183422,26.393801881204,-5.40731760938806));
#38932=CARTESIAN_POINT('Ctrl Pts',(-24.9160307816441,26.4736791714868,-5.41778267063301));
#38933=CARTESIAN_POINT('Ctrl Pts',(-24.7690454485814,26.5379494228179,-5.42695541724512));
#38934=CARTESIAN_POINT('Ctrl Pts',(-24.3529053209454,26.6840563980972,-5.4517926255825));
#38935=CARTESIAN_POINT('Ctrl Pts',(-24.0769423114776,26.7420497390921,-5.467144767834));
#38936=CARTESIAN_POINT('Ctrl Pts',(-23.7860933963628,26.7643799962144,-5.48439319326439));
#38937=CARTESIAN_POINT('Ctrl Pts',(-23.7752259301992,26.7651589436305,-5.48503899268572));
#38938=CARTESIAN_POINT('Ctrl Pts',(-23.7107189443913,26.7694539315506,-5.48888056175493));
#38939=CARTESIAN_POINT('Ctrl Pts',(-23.6570047554342,26.7716824255818,-5.49211338935558));
#38940=CARTESIAN_POINT('Ctrl Pts',(-23.5944897572586,26.7727108492281,-5.49592349902234));
#38941=CARTESIAN_POINT('Ctrl Pts',(-23.5857167574082,26.772819338863,-5.49645927227084));
#38942=CARTESIAN_POINT('Ctrl Pts',(-23.57264732087,26.7729275842348,-5.49725908209659));
#38943=CARTESIAN_POINT('Ctrl Pts',(-23.568351099801,26.7729545753834,-5.49752226337158));
#38944=CARTESIAN_POINT('Ctrl Pts',(-23.5606913623404,26.7729873806383,-5.49799196775458));
#38945=CARTESIAN_POINT('Ctrl Pts',(-23.5573278603499,26.7729965201878,-5.4981983861593));
#38946=CARTESIAN_POINT('Ctrl Pts',(-23.5502397263787,26.7730046840094,-5.49863373452073));
#38947=CARTESIAN_POINT('Ctrl Pts',(-23.5465151003408,26.7730025168524,-5.49886270158218));
#38948=CARTESIAN_POINT('Ctrl Pts',(-23.5366841725237,26.7729797540248,-5.49946758662873));
#38949=CARTESIAN_POINT('Ctrl Pts',(-23.5305779326432,26.7729482603121,-5.49984384624813));
#38950=CARTESIAN_POINT('Ctrl Pts',(-23.503464402862,26.7727313562464,-5.501517023538));
#38951=CARTESIAN_POINT('Ctrl Pts',(-23.4824595116011,26.7723578956534,-5.50281983113482));
#38952=CARTESIAN_POINT('Ctrl Pts',(-23.3300707220396,26.7681577250595,-5.51232112681596));
#38953=CARTESIAN_POINT('Ctrl Pts',(-23.1990432324052,26.7565023653579,-5.52076560422306));
#38954=CARTESIAN_POINT('Ctrl Pts',(-22.8105136512479,26.697838718788,-5.54663305154377));
#38955=CARTESIAN_POINT('Ctrl Pts',(-22.5576691741607,26.6274701178797,-5.56465311847542));
#38956=CARTESIAN_POINT('Ctrl Pts',(-22.2342596456139,26.4934027281094,-5.58791243245908));
#38957=CARTESIAN_POINT('Ctrl Pts',(-22.1538293697159,26.4561042185385,-5.59370450105131));
#38958=CARTESIAN_POINT('Ctrl Pts',(-22.0750360126322,26.415536773159,-5.59931610453398));
#38959=CARTESIAN_POINT('',(-26.773001157643,23.5472765537013,-5.43577344933047));
#38960=CARTESIAN_POINT('Ctrl Pts',(-22.0750360153462,26.4155367745563,-5.84297427009707));
#38961=CARTESIAN_POINT('Ctrl Pts',(-22.1638664037002,26.4612718726988,-5.8368145899415));
#38962=CARTESIAN_POINT('Ctrl Pts',(-22.2547570412907,26.5028369104112,-5.83065490978592));
#38963=CARTESIAN_POINT('Ctrl Pts',(-22.3472759868601,26.5400627255157,-5.82449522963034));
#38964=CARTESIAN_POINT('Ctrl Pts',(-22.4402513107283,26.5774721684606,-5.8183051649483));
#38965=CARTESIAN_POINT('Ctrl Pts',(-22.5348706286827,26.6104993280361,-5.81211510026625));
#38966=CARTESIAN_POINT('Ctrl Pts',(-22.6306812321648,26.6390235150437,-5.80592503558421));
#38967=CARTESIAN_POINT('Ctrl Pts',(-22.7264918356468,26.6675477020513,-5.79973497090217));
#38968=CARTESIAN_POINT('Ctrl Pts',(-22.8234932841265,26.6915688712652,-5.7935449062201));
#38969=CARTESIAN_POINT('Ctrl Pts',(-22.9212250381291,26.7110185741021,-5.78735484153806));
#38970=CARTESIAN_POINT('Ctrl Pts',(-23.0186730198225,26.7304118031027,-5.78118275022576));
#38971=CARTESIAN_POINT('Ctrl Pts',(-23.1171903225698,26.7453284107951,-5.77501065891346));
#38972=CARTESIAN_POINT('Ctrl Pts',(-23.2163292355858,26.7556562184108,-5.76883856760114));
#38973=CARTESIAN_POINT('Ctrl Pts',(-23.3153338251759,26.7659700328681,-5.76267483886235));
#38974=CARTESIAN_POINT('Ctrl Pts',(-23.4149579227767,26.7717073603206,-5.75651111012354));
#38975=CARTESIAN_POINT('Ctrl Pts',(-23.5147430549401,26.7728068973428,-5.75034738138476));
#38976=CARTESIAN_POINT('Ctrl Pts',(-23.6144224741215,26.7739052695087,-5.74419018253806));
#38977=CARTESIAN_POINT('Ctrl Pts',(-23.7142621567178,26.7703756145777,-5.73803298369135));
#38978=CARTESIAN_POINT('Ctrl Pts',(-23.813798889093,26.762208459163,-5.73187578484465));
#38979=CARTESIAN_POINT('Ctrl Pts',(-23.9132628661526,26.7540472734436,-5.72572308653695));
#38980=CARTESIAN_POINT('Ctrl Pts',(-24.0124239016077,26.7412553620142,-5.71957038822927));
#38981=CARTESIAN_POINT('Ctrl Pts',(-24.1108200893969,26.723875315793,-5.71341768992157));
#38982=CARTESIAN_POINT('Ctrl Pts',(-24.2091789652119,26.7065018601101,-5.70726732472582));
#38983=CARTESIAN_POINT('Ctrl Pts',(-24.306773142346,26.6845438021302,-5.70111695953007));
#38984=CARTESIAN_POINT('Ctrl Pts',(-24.4031480246445,26.6580953270436,-5.69496659433432));
#38985=CARTESIAN_POINT('Ctrl Pts',(-24.4995121445675,26.6316498055109,-5.68881691596212));
#38986=CARTESIAN_POINT('Ctrl Pts',(-24.5946568214479,26.6007149787936,-5.6826672375899));
#38987=CARTESIAN_POINT('Ctrl Pts',(-24.6881407888652,26.5654354244376,-5.6765175592177));
#38988=CARTESIAN_POINT('Ctrl Pts',(-24.7816393262585,26.5301503715744,-5.67036692238525));
#38989=CARTESIAN_POINT('Ctrl Pts',(-24.8734762336229,26.4905193994746,-5.66421628555281));
#38990=CARTESIAN_POINT('Ctrl Pts',(-24.963229405051,26.4467355573408,-5.65806564872037));
#38991=CARTESIAN_POINT('Ctrl Pts',(-25.0530785935183,26.4029048756934,-5.65190843199856));
#38992=CARTESIAN_POINT('Ctrl Pts',(-25.1408392034506,26.3549126432117,-5.64575121527673));
#38993=CARTESIAN_POINT('Ctrl Pts',(-25.2261130828956,26.3029982474164,-5.63959399855491));
#38994=CARTESIAN_POINT('Ctrl Pts',(-25.3114345362888,26.2510548887922,-5.6334333467471));
#38995=CARTESIAN_POINT('Ctrl Pts',(-25.3942661361837,26.1951852520902,-5.6272726949393));
#38996=CARTESIAN_POINT('Ctrl Pts',(-25.474239868565,26.1356713159651,-5.62111204313149));
#38997=CARTESIAN_POINT('Ctrl Pts',(-25.5543474254393,26.0760577918616,-5.61494108236246));
#38998=CARTESIAN_POINT('Ctrl Pts',(-25.6315872262005,26.0127880627121,-5.60877012159343));
#38999=CARTESIAN_POINT('Ctrl Pts',(-25.7056253065707,25.9461836166424,-5.6025991608244));
#39000=CARTESIAN_POINT('Ctrl Pts',(-25.762139963449,25.8953431923989,-5.59788875060405));
#39001=CARTESIAN_POINT('Ctrl Pts',(-25.8167898235724,25.8425605947428,-5.59317834038368));
#39002=CARTESIAN_POINT('Ctrl Pts',(-25.8694420086437,25.787991956316,-5.58846793016333));
#39003=CARTESIAN_POINT('Ctrl Pts',(-25.9405584090568,25.7142870353311,-5.58210566012863));
#39004=CARTESIAN_POINT('Ctrl Pts',(-26.008305078855,25.6370355103818,-5.57574339009394));
#39005=CARTESIAN_POINT('Ctrl Pts',(-26.072303925268,25.5565860858852,-5.56938112005923));
#39006=CARTESIAN_POINT('Ctrl Pts',(-26.1334909052143,25.4796713038342,-5.56329838402811));
#39007=CARTESIAN_POINT('Ctrl Pts',(-26.1912520703198,25.3998340623105,-5.55721564799696));
#39008=CARTESIAN_POINT('Ctrl Pts',(-26.2452931100523,25.3174180144669,-5.55113291196584));
#39009=CARTESIAN_POINT('Ctrl Pts',(-26.2992838720878,25.2350786433324,-5.54505583507748));
#39010=CARTESIAN_POINT('Ctrl Pts',(-26.3495611375826,25.1501656008213,-5.53897875818915));
#39011=CARTESIAN_POINT('Ctrl Pts',(-26.395871428336,25.0630547849894,-5.5329016813008));
#39012=CARTESIAN_POINT('Ctrl Pts',(-26.4421517837701,24.9760002782423,-5.52682853268054));
#39013=CARTESIAN_POINT('Ctrl Pts',(-26.4844700490081,24.886751213229,-5.52075538406026));
#39014=CARTESIAN_POINT('Ctrl Pts',(-26.5226172132757,24.7957105848565,-5.51468223543999));
#39015=CARTESIAN_POINT('Ctrl Pts',(-26.5607505474694,24.7047029628331,-5.50861128861103));
#39016=CARTESIAN_POINT('Ctrl Pts',(-26.5947156143592,24.6119054800709,-5.50254034178209));
#39017=CARTESIAN_POINT('Ctrl Pts',(-26.6243508388008,24.5177426663954,-5.49646939495312));
#39018=CARTESIAN_POINT('Ctrl Pts',(-26.6539931010491,24.4235574908282,-5.49039700638883));
#39019=CARTESIAN_POINT('Ctrl Pts',(-26.6793033267433,24.3280067610761,-5.48432461782454));
#39020=CARTESIAN_POINT('Ctrl Pts',(-26.7001695323316,24.2315310735517,-5.47825222926025));
#39021=CARTESIAN_POINT('Ctrl Pts',(-26.7210387565873,24.1350414291047,-5.47217896221705));
#39022=CARTESIAN_POINT('Ctrl Pts',(-26.7374625987345,24.0376269996952,-5.46610569517386));
#39023=CARTESIAN_POINT('Ctrl Pts',(-26.7493803441058,23.9397378361081,-5.46003242813066));
#39024=CARTESIAN_POINT('Ctrl Pts',(-26.761308029878,23.8417670247347,-5.45395409547252));
#39025=CARTESIAN_POINT('Ctrl Pts',(-26.7687220787112,23.7433211337576,-5.4478757628144));
#39026=CARTESIAN_POINT('Ctrl Pts',(-26.7716137554282,23.6448539519952,-5.44179743015627));
#39027=CARTESIAN_POINT('Ctrl Pts',(-26.7725690286409,23.6123250525822,-5.43978943654768));
#39028=CARTESIAN_POINT('Ctrl Pts',(-26.7730311850157,23.5797938217113,-5.43778144293905));
#39029=CARTESIAN_POINT('Ctrl Pts',(-26.773001157643,23.5472765537013,-5.43577344933045));
#39030=CARTESIAN_POINT('Ctrl Pts',(-26.7730011581167,23.547277066739,-5.43576586302522));
#39031=CARTESIAN_POINT('Ctrl Pts',(-26.7728017003367,23.3312428347102,-5.42115614110461));
#39032=CARTESIAN_POINT('Ctrl Pts',(-26.7508804635188,23.1157498323663,-5.40642471359264));
#39033=CARTESIAN_POINT('Ctrl Pts',(-26.7042487805336,22.8879107697878,-5.39160782088756));
#39034=CARTESIAN_POINT('Ctrl Pts',(-26.7008218005194,22.8717967439381,-5.3905642810244));
#39035=CARTESIAN_POINT('Ctrl Pts',(-26.6957783552933,22.8489445777544,-5.38909131329109));
#39036=CARTESIAN_POINT('Ctrl Pts',(-26.6942635608367,22.8421845943516,-5.3886564537183));
#39037=CARTESIAN_POINT('Ctrl Pts',(-26.6919137736767,22.8318545609168,-5.38799331642536));
#39038=CARTESIAN_POINT('Ctrl Pts',(-26.6910944784316,22.8282810158282,-5.38776416502595));
#39039=CARTESIAN_POINT('Ctrl Pts',(-26.6897395642714,22.8224172022104,-5.3873885752252));
#39040=CARTESIAN_POINT('Ctrl Pts',(-26.6892075358411,22.8201261203171,-5.38724193279483));
#39041=CARTESIAN_POINT('Ctrl Pts',(-26.6881679470201,22.8156714623836,-5.38695701853772));
#39042=CARTESIAN_POINT('Ctrl Pts',(-26.6876606561421,22.8135078256737,-5.38681873127108));
#39043=CARTESIAN_POINT('Ctrl Pts',(-26.6867661552835,22.8097103851889,-5.38657619164215));
#39044=CARTESIAN_POINT('Ctrl Pts',(-26.6863799080287,22.8080763658457,-5.38647188383003));
#39045=CARTESIAN_POINT('Ctrl Pts',(-26.6854934141952,22.8043391017161,-5.38623344272216));
#39046=CARTESIAN_POINT('Ctrl Pts',(-26.6849923290821,22.8022360619118,-5.38609935892889));
#39047=CARTESIAN_POINT('Ctrl Pts',(-26.683627916442,22.7965351105121,-5.38573612872367));
#39048=CARTESIAN_POINT('Ctrl Pts',(-26.6827605050167,22.7929381649124,-5.38550721900772));
#39049=CARTESIAN_POINT('Ctrl Pts',(-26.678649819353,22.7760200440742,-5.38443176691326));
#39050=CARTESIAN_POINT('Ctrl Pts',(-26.6753276915483,22.7627179004519,-5.38358972973967));
#39051=CARTESIAN_POINT('Ctrl Pts',(-26.6159122931846,22.5311100329855,-5.36898436109109));
#39052=CARTESIAN_POINT('Ctrl Pts',(-26.5371437407903,22.3192217469999,-5.35646055239281));
#39053=CARTESIAN_POINT('Ctrl Pts',(-26.4167171715861,22.0766325775321,-5.34132759708626));
#39054=CARTESIAN_POINT('Ctrl Pts',(-26.3956914038968,22.0364319065887,-5.33879298767271));
#39055=CARTESIAN_POINT('Ctrl Pts',(-26.3522304509475,21.9574424810711,-5.33373865440602));
#39056=CARTESIAN_POINT('Ctrl Pts',(-26.3298211103849,21.9186513174497,-5.33121970989232));
#39057=CARTESIAN_POINT('Ctrl Pts',(-26.24028727996,21.7708667053919,-5.32144573235574));
#39058=CARTESIAN_POINT('Ctrl Pts',(-26.1675070609782,21.6654515586953,-5.3140879175494));
#39059=CARTESIAN_POINT('Ctrl Pts',(-26.0543920849133,21.5208448396623,-5.30319900321725));
#39060=CARTESIAN_POINT('Ctrl Pts',(-26.0190007297739,21.4779368606392,-5.29985949201865));
#39061=CARTESIAN_POINT('Ctrl Pts',(-25.9778900924732,21.4306433201386,-5.29604493205236));
#39062=CARTESIAN_POINT('Ctrl Pts',(-25.9732441860066,21.4253339972309,-5.29561474859756));
#39063=CARTESIAN_POINT('Ctrl Pts',(-25.9656552853289,21.4167186813138,-5.29491349866213));
#39064=CARTESIAN_POINT('Ctrl Pts',(-25.9627228310524,21.4134034009899,-5.29464287253148));
#39065=CARTESIAN_POINT('Ctrl Pts',(-25.9570308823807,21.4069950307853,-5.29411824554769));
#39066=CARTESIAN_POINT('Ctrl Pts',(-25.9542722304672,21.4039012016013,-5.29386428033336));
#39067=CARTESIAN_POINT('Ctrl Pts',(-25.9494871613744,21.3985555429547,-5.29342427407203));
#39068=CARTESIAN_POINT('Ctrl Pts',(-25.9474635190695,21.3963012273436,-5.29323835022815));
#39069=CARTESIAN_POINT('Ctrl Pts',(-25.9432605972093,21.3916324772015,-5.29285252886805));
#39070=CARTESIAN_POINT('Ctrl Pts',(-25.9410808358468,21.3892184826289,-5.2926526110712));
#39071=CARTESIAN_POINT('Ctrl Pts',(-25.935132155612,21.3826505844619,-5.29210751386498));
#39072=CARTESIAN_POINT('Ctrl Pts',(-25.9313560538938,21.3785032279863,-5.2917620297103));
#39073=CARTESIAN_POINT('Ctrl Pts',(-25.9170560785965,21.3628794511765,-5.29045567777744));
#39074=CARTESIAN_POINT('Ctrl Pts',(-25.9064600370686,21.3514696408815,-5.28949173224048));
#39075=CARTESIAN_POINT('Ctrl Pts',(-25.7280179470477,21.1620943821326,-5.27332377836745));
#39076=CARTESIAN_POINT('Ctrl Pts',(-25.5405649662978,21.0037706143978,-5.25720247528504));
#39077=CARTESIAN_POINT('Ctrl Pts',(-25.2711385023251,20.8242769072443,-5.23534843579562));
#39078=CARTESIAN_POINT('Ctrl Pts',(-25.2036221445284,20.7828059752931,-5.22997701626038));
#39079=CARTESIAN_POINT('Ctrl Pts',(-25.0619657674111,20.7028314202572,-5.21898369269443));
#39080=CARTESIAN_POINT('Ctrl Pts',(-24.9877145582437,20.6646350937566,-5.21336774464087));
#39081=CARTESIAN_POINT('Ctrl Pts',(-24.8505649054669,20.6006916894435,-5.20334435881736));
#39082=CARTESIAN_POINT('Ctrl Pts',(-24.7881735276325,20.5739671925596,-5.19891002702729));
#39083=CARTESIAN_POINT('Ctrl Pts',(-24.7071649191778,20.5422569667112,-5.19335146602427));
#39084=CARTESIAN_POINT('Ctrl Pts',(-24.6892870854578,20.5354417719173,-5.19213694424257));
#39085=CARTESIAN_POINT('Ctrl Pts',(-24.6604289659922,20.5247341439105,-5.19019725187474));
#39086=CARTESIAN_POINT('Ctrl Pts',(-24.6494867141667,20.520741440434,-5.18946653965968));
#39087=CARTESIAN_POINT('Ctrl Pts',(-24.6361704269276,20.515964125247,-5.18858328187162));
#39088=CARTESIAN_POINT('Ctrl Pts',(-24.6338170052042,20.515122906697,-5.18842740805631));
#39089=CARTESIAN_POINT('Ctrl Pts',(-24.6292695410634,20.5135034022,-5.18812665738464));
#39090=CARTESIAN_POINT('Ctrl Pts',(-24.6270756303461,20.5127247546551,-5.18798175904151));
#39091=CARTESIAN_POINT('Ctrl Pts',(-24.623120514524,20.5113258559694,-5.18772089975285));
#39092=CARTESIAN_POINT('Ctrl Pts',(-24.6213596181994,20.5107047596875,-5.18760488828299));
#39093=CARTESIAN_POINT('Ctrl Pts',(-24.6175742511704,20.5093732982051,-5.18735577647971));
#39094=CARTESIAN_POINT('Ctrl Pts',(-24.6155496162233,20.5086634260968,-5.18722270612757));
#39095=CARTESIAN_POINT('Ctrl Pts',(-24.610097892291,20.5067580683867,-5.18686483964569));
#39096=CARTESIAN_POINT('Ctrl Pts',(-24.6066694771679,20.5055663452071,-5.18664026857999));
#39097=CARTESIAN_POINT('Ctrl Pts',(-24.5909222334664,20.500122375653,-5.18561094811414));
#39098=CARTESIAN_POINT('Ctrl Pts',(-24.5785794693659,20.4959390049154,-5.1848102504434));
#39099=CARTESIAN_POINT('Ctrl Pts',(-24.3633691379464,20.4244495734823,-5.17094934600652));
#39100=CARTESIAN_POINT('Ctrl Pts',(-24.1542904686654,20.377403406481,-5.15900948745388));
#39101=CARTESIAN_POINT('Ctrl Pts',(-23.7777529224431,20.3312830887449,-5.13780880633432));
#39102=CARTESIAN_POINT('Ctrl Pts',(-23.6121413032126,20.323847999034,-5.12858393289394));
#39103=CARTESIAN_POINT('Ctrl Pts',(-23.3382913393247,20.3326517545762,-5.11277056133077));
#39104=CARTESIAN_POINT('Ctrl Pts',(-23.2301373464575,20.3416072119602,-5.10638363243123));
#39105=CARTESIAN_POINT('Ctrl Pts',(-23.1033555528975,20.3585790630121,-5.09864248888314));
#39106=CARTESIAN_POINT('Ctrl Pts',(-23.0840869987578,20.3613363975877,-5.09745909881912));
#39107=CARTESIAN_POINT('Ctrl Pts',(-23.0605136184476,20.3649279712969,-5.09600254877397));
#39108=CARTESIAN_POINT('Ctrl Pts',(-23.0561836761207,20.3655967066683,-5.0957346473616));
#39109=CARTESIAN_POINT('Ctrl Pts',(-23.0477918528838,20.3669103032346,-5.09521471985265));
#39110=CARTESIAN_POINT('Ctrl Pts',(-23.0437298143259,20.3675541146612,-5.09496272752393));
#39111=CARTESIAN_POINT('Ctrl Pts',(-23.0366818087502,20.3686850204978,-5.09452493343813));
#39112=CARTESIAN_POINT('Ctrl Pts',(-23.0336952678335,20.3691685483925,-5.09433924532489));
#39113=CARTESIAN_POINT('Ctrl Pts',(-23.0274849046246,20.3701829969954,-5.09395274801992));
#39114=CARTESIAN_POINT('Ctrl Pts',(-23.0242612012359,20.3707146159615,-5.09375191679583));
#39115=CARTESIAN_POINT('Ctrl Pts',(-23.0163991096025,20.3720234328168,-5.09326161550997));
#39116=CARTESIAN_POINT('Ctrl Pts',(-23.0117616132844,20.3728058819997,-5.09297197847111));
#39117=CARTESIAN_POINT('Ctrl Pts',(-22.9941670918377,20.3758140955516,-5.09187145911698));
#39118=CARTESIAN_POINT('Ctrl Pts',(-22.9812221544401,20.3781089626214,-5.09105837737816));
#39119=CARTESIAN_POINT('Ctrl Pts',(-22.7578611386389,20.419117415314,-5.07696924404707));
#39120=CARTESIAN_POINT('Ctrl Pts',(-22.5518439070098,20.478601725119,-5.06300310952108));
#39121=CARTESIAN_POINT('Ctrl Pts',(-22.2488643231098,20.599803142625,-5.0410936459051));
#39122=CARTESIAN_POINT('Ctrl Pts',(-22.1467163058612,20.6470047092895,-5.03346083206489));
#39123=CARTESIAN_POINT('Ctrl Pts',(-21.9524996474792,20.7493998625349,-5.01862247536965));
#39124=CARTESIAN_POINT('Ctrl Pts',(-21.8602951858603,20.8040484304449,-5.01142331252134));
#39125=CARTESIAN_POINT('Ctrl Pts',(-21.731845526678,20.8891030831865,-5.00132085702342));
#39126=CARTESIAN_POINT('Ctrl Pts',(-21.6932808483685,20.9158689052912,-4.99827806649798));
#39127=CARTESIAN_POINT('Ctrl Pts',(-21.6409243019268,20.9539282665429,-4.99414816115956));
#39128=CARTESIAN_POINT('Ctrl Pts',(-21.6266225226523,20.9645066818396,-4.99302015277972));
#39129=CARTESIAN_POINT('Ctrl Pts',(-21.6036061860228,20.9818275409794,-4.99120598757277));
#39130=CARTESIAN_POINT('Ctrl Pts',(-21.5948375454561,20.9884970460886,-4.99051511732783));
#39131=CARTESIAN_POINT('Ctrl Pts',(-21.5841546482203,20.9967093628273,-4.98967394797627));
#39132=CARTESIAN_POINT('Ctrl Pts',(-21.5822078753946,20.9982094612163,-4.98952068080459));
#39133=CARTESIAN_POINT('Ctrl Pts',(-21.5784440597433,21.0011165616672,-4.98922440447182));
#39134=CARTESIAN_POINT('Ctrl Pts',(-21.5766268030156,21.0025232825548,-4.98908137557956));
#39135=CARTESIAN_POINT('Ctrl Pts',(-21.573337323056,21.0050752688324,-4.98882251289654));
#39136=CARTESIAN_POINT('Ctrl Pts',(-21.5718645939768,21.006219864946,-4.98870663212928));
#39137=CARTESIAN_POINT('Ctrl Pts',(-21.568905599152,21.0085237011212,-4.98847383448321));
#39138=CARTESIAN_POINT('Ctrl Pts',(-21.567419362718,21.0096829618314,-4.98835691997815));
#39139=CARTESIAN_POINT('Ctrl Pts',(-21.5631814255541,21.0129945263142,-4.98802358213339));
#39140=CARTESIAN_POINT('Ctrl Pts',(-21.560432195431,21.0151500098245,-4.98780738614676));
#39141=CARTESIAN_POINT('Ctrl Pts',(-21.5486850904564,21.0243909942745,-4.98688378193596));
#39142=CARTESIAN_POINT('Ctrl Pts',(-21.5397213710201,21.0315200748215,-4.98617945447827));
#39143=CARTESIAN_POINT('Ctrl Pts',(-21.3891023450939,21.1526277343998,-4.97434824413224));
#39144=CARTESIAN_POINT('Ctrl Pts',(-21.257280791091,21.2783642699907,-4.96404086225563));
#39145=CARTESIAN_POINT('Ctrl Pts',(-21.0308774231787,21.5342186070111,-4.94488652539501));
#39146=CARTESIAN_POINT('Ctrl Pts',(-20.9340468847667,21.6615729830931,-4.93603832258459));
#39147=CARTESIAN_POINT('Ctrl Pts',(-20.7851740077278,21.8909219170241,-4.92046990296279));
#39148=CARTESIAN_POINT('Ctrl Pts',(-20.7283800413686,21.9894613179422,-4.91388661078038));
#39149=CARTESIAN_POINT('Ctrl Pts',(-20.6541990567995,22.1355061078755,-4.90413136933178));
#39150=CARTESIAN_POINT('Ctrl Pts',(-20.6325333751819,22.1807461722552,-4.90111038486596));
#39151=CARTESIAN_POINT('Ctrl Pts',(-20.6086924112458,22.233664569667,-4.89757125327117));
#39152=CARTESIAN_POINT('Ctrl Pts',(-20.6054782281746,22.2408694313171,-4.89708928850533));
#39153=CARTESIAN_POINT('Ctrl Pts',(-20.6006098044179,22.2518910076405,-4.89635181226217));
#39154=CARTESIAN_POINT('Ctrl Pts',(-20.5989364283181,22.2556992792507,-4.89609695764449));
#39155=CARTESIAN_POINT('Ctrl Pts',(-20.5960563972188,22.262288265906,-4.89565594867708));
#39156=CARTESIAN_POINT('Ctrl Pts',(-20.594846280828,22.2650674698699,-4.89546991313726));
#39157=CARTESIAN_POINT('Ctrl Pts',(-20.5923483757165,22.2708264478474,-4.89508437297264));
#39158=CARTESIAN_POINT('Ctrl Pts',(-20.5910611649026,22.2738064675952,-4.894884848832));
#39159=CARTESIAN_POINT('Ctrl Pts',(-20.5879502827344,22.2810384625064,-4.89440057752821));
#39160=CARTESIAN_POINT('Ctrl Pts',(-20.586131264607,22.285292421149,-4.8941156718022));
#39161=CARTESIAN_POINT('Ctrl Pts',(-20.5793751237427,22.3011869340001,-4.89305094855348));
#39162=CARTESIAN_POINT('Ctrl Pts',(-20.574497411347,22.3128524764073,-4.89226911022169));
#39163=CARTESIAN_POINT('Ctrl Pts',(-20.4970181477516,22.5012596949878,-4.87963452661291));
#39164=CARTESIAN_POINT('Ctrl Pts',(-20.4402205282917,22.6840519723448,-4.86723778386786));
#39165=CARTESIAN_POINT('Ctrl Pts',(-20.3625729258513,23.0440509627052,-4.84264097773425));
#39166=CARTESIAN_POINT('Ctrl Pts',(-20.3395594746795,23.2201200858849,-4.83053831832784));
#39167=CARTESIAN_POINT('Ctrl Pts',(-20.3268531186829,23.4873279871111,-4.81258149196924));
#39168=CARTESIAN_POINT('Ctrl Pts',(-20.3263548312428,23.5776272335715,-4.80658807722797));
#39169=CARTESIAN_POINT('Ctrl Pts',(-20.3304785236612,23.6905763818779,-4.79927228883979));
#39170=CARTESIAN_POINT('Ctrl Pts',(-20.3315496995399,23.7133095333237,-4.79780910730074));
#39171=CARTESIAN_POINT('Ctrl Pts',(-20.3343997583616,23.7626683108481,-4.79465502020018));
#39172=CARTESIAN_POINT('Ctrl Pts',(-20.3362687215171,23.7892874759925,-4.79296846193282));
#39173=CARTESIAN_POINT('Ctrl Pts',(-20.3388276713078,23.8202283714001,-4.79102728418031));
#39174=CARTESIAN_POINT('Ctrl Pts',(-20.3391960126509,23.8245746415895,-4.79075504824071));
#39175=CARTESIAN_POINT('Ctrl Pts',(-20.3397722862302,23.8312141983763,-4.7903398569693));
#39176=CARTESIAN_POINT('Ctrl Pts',(-20.3399738524266,23.8335080103328,-4.79019654367755));
#39177=CARTESIAN_POINT('Ctrl Pts',(-20.3403272895627,23.8374812663057,-4.78994852164491));
#39178=CARTESIAN_POINT('Ctrl Pts',(-20.3404780199327,23.8391608039072,-4.78984374828197));
#39179=CARTESIAN_POINT('Ctrl Pts',(-20.3407955213803,23.8426676962074,-4.78962512317792));
#39180=CARTESIAN_POINT('Ctrl Pts',(-20.3409625344194,23.8444950216962,-4.78951128563158));
#39181=CARTESIAN_POINT('Ctrl Pts',(-20.3414292903606,23.8495542243269,-4.78919633184865));
#39182=CARTESIAN_POINT('Ctrl Pts',(-20.3417323562048,23.8527858043011,-4.78899540416604));
#39183=CARTESIAN_POINT('Ctrl Pts',(-20.3429435580294,23.8654942570319,-4.78820620342639));
#39184=CARTESIAN_POINT('Ctrl Pts',(-20.3438888150326,23.8749676680965,-4.78762000878183));
#39185=CARTESIAN_POINT('Ctrl Pts',(-20.3603017654807,24.0323948000153,-4.77791175520961));
#39186=CARTESIAN_POINT('Ctrl Pts',(-20.3859558691113,24.1791297114637,-4.7693445829478));
#39187=CARTESIAN_POINT('Ctrl Pts',(-20.4699443666183,24.5189131341003,-4.74956994853492));
#39188=CARTESIAN_POINT('Ctrl Pts',(-20.5364111285628,24.7092879196807,-4.73851792459834));
#39189=CARTESIAN_POINT('Ctrl Pts',(-20.6497377678543,24.95672499005,-4.72299344350883));
#39190=CARTESIAN_POINT('Ctrl Pts',(-20.681399754507,25.0202299236836,-4.71890164379641));
#39191=CARTESIAN_POINT('Ctrl Pts',(-20.7551536077435,25.1566848238478,-4.7098136680943));
#39192=CARTESIAN_POINT('Ctrl Pts',(-20.7980596886749,25.2291317219921,-4.70479441932454));
#39193=CARTESIAN_POINT('Ctrl Pts',(-20.8489765755297,25.3078982541905,-4.69908291239882));
#39194=CARTESIAN_POINT('Ctrl Pts',(-20.8542400305717,25.3159611338673,-4.69849521174591));
#39195=CARTESIAN_POINT('Ctrl Pts',(-20.8620251109924,25.3277708277269,-4.69762987249399));
#39196=CARTESIAN_POINT('Ctrl Pts',(-20.8645186394031,25.3315361749172,-4.69735329077408));
#39197=CARTESIAN_POINT('Ctrl Pts',(-20.8689003316166,25.3381226235672,-4.6968682864994));
#39198=CARTESIAN_POINT('Ctrl Pts',(-20.8707850578404,25.3409460126372,-4.69665999388323));
#39199=CARTESIAN_POINT('Ctrl Pts',(-20.8744470243656,25.3464130470483,-4.6962559145485));
#39200=CARTESIAN_POINT('Ctrl Pts',(-20.8762237310688,25.3490570467182,-4.6960601481742));
#39201=CARTESIAN_POINT('Ctrl Pts',(-20.8804647161472,25.3553480848593,-4.69559352825165));
#39202=CARTESIAN_POINT('Ctrl Pts',(-20.8829325472206,25.3589927109983,-4.69532254011838));
#39203=CARTESIAN_POINT('Ctrl Pts',(-20.8917332322331,25.3719328573335,-4.69435805126446));
#39204=CARTESIAN_POINT('Ctrl Pts',(-20.8981072182819,25.3812001840885,-4.6936629868024));
#39205=CARTESIAN_POINT('Ctrl Pts',(-20.9924683148742,25.5168679688499,-4.68342330206693));
#39206=CARTESIAN_POINT('Ctrl Pts',(-21.0893429300488,25.6368161151319,-4.67353061019756));
#39207=CARTESIAN_POINT('Ctrl Pts',(-21.3509961588839,25.9171174288147,-4.64820327432532));
#39208=CARTESIAN_POINT('Ctrl Pts',(-21.5250519611933,26.0676571186219,-4.63246638691006));
#39209=CARTESIAN_POINT('Ctrl Pts',(-21.785709120985,26.2484384182394,-4.61124474181449));
#39210=CARTESIAN_POINT('Ctrl Pts',(-21.859847220844,26.2954944066382,-4.60544623001482));
#39211=CARTESIAN_POINT('Ctrl Pts',(-21.9688630818831,26.3585941492496,-4.59734582894304));
#39212=CARTESIAN_POINT('Ctrl Pts',(-22.0022456392596,26.3771324753666,-4.59492029370877));
#39213=CARTESIAN_POINT('Ctrl Pts',(-22.0401442256527,26.3973059252628,-4.59223450943404));
#39214=CARTESIAN_POINT('Ctrl Pts',(-22.0443418622225,26.3995284358611,-4.59193795819502));
#39215=CARTESIAN_POINT('Ctrl Pts',(-22.0506536488911,26.402852474883,-4.59149345415158));
#39216=CARTESIAN_POINT('Ctrl Pts',(-22.0527641090184,26.4039609381761,-4.59134506170654));
#39217=CARTESIAN_POINT('Ctrl Pts',(-22.0563790721916,26.4058544873845,-4.59109128889231));
#39218=CARTESIAN_POINT('Ctrl Pts',(-22.0578829648923,26.4066407263354,-4.59098583466185));
#39219=CARTESIAN_POINT('Ctrl Pts',(-22.0609832742274,26.4082584591111,-4.59076868628164));
#39220=CARTESIAN_POINT('Ctrl Pts',(-22.0625797626786,26.4090898014168,-4.59065700193718));
#39221=CARTESIAN_POINT('Ctrl Pts',(-22.0664411735423,26.4110964503846,-4.59038719657879));
#39222=CARTESIAN_POINT('Ctrl Pts',(-22.0687068014021,26.4122704077472,-4.59022916171983));
#39223=CARTESIAN_POINT('Ctrl Pts',(-22.0723273939412,26.4141410020936,-4.58997704018022));
#39224=CARTESIAN_POINT('Ctrl Pts',(-22.0736814559545,26.4148393678708,-4.58988284461916));
#39225=CARTESIAN_POINT('Ctrl Pts',(-22.075036015346,26.4155367745563,-4.58978870905188));
#39226=CARTESIAN_POINT('Origin',(-23.5502525316942,23.5502525316942,-77.3107734492734));
#39227=CARTESIAN_POINT('',(-22.0750359182337,26.4155367245571,-3.09374624221682));
#39228=CARTESIAN_POINT('',(-22.0750361667496,26.4155368525077,-3.34376876818698));
#39229=CARTESIAN_POINT('',(-22.0750360153461,26.4155367745563,-77.3107734492734));
#39230=CARTESIAN_POINT('',(-26.7730016161112,23.552681809173,-3.93718354728755));
#39231=CARTESIAN_POINT('Ctrl Pts',(-22.0750359182355,26.4155367245581,-3.0937462422167));
#39232=CARTESIAN_POINT('Ctrl Pts',(-22.0146133082446,26.3844276156225,-3.09773139462589));
#39233=CARTESIAN_POINT('Ctrl Pts',(-21.95512803832,26.3513832493889,-3.10177819823092));
#39234=CARTESIAN_POINT('Ctrl Pts',(-21.879463016644,26.3061520264815,-3.10711032437475));
#39235=CARTESIAN_POINT('Ctrl Pts',(-21.8623488067689,26.2957034265546,-3.10832890551739));
#39236=CARTESIAN_POINT('Ctrl Pts',(-21.8400613104548,26.2818092578009,-3.10993276080145));
#39237=CARTESIAN_POINT('Ctrl Pts',(-21.834798655112,26.2785073140795,-3.11031271969719));
#39238=CARTESIAN_POINT('Ctrl Pts',(-21.8266930875078,26.2733889194499,-3.11089987464221));
#39239=CARTESIAN_POINT('Ctrl Pts',(-21.8238434043007,26.2715831747213,-3.11110667282468));
#39240=CARTESIAN_POINT('Ctrl Pts',(-21.818175141691,26.267978908031,-3.11151875488951));
#39241=CARTESIAN_POINT('Ctrl Pts',(-21.8153565151765,26.2661804676553,-3.11172403556082));
#39242=CARTESIAN_POINT('Ctrl Pts',(-21.8091851600086,26.2622292729161,-3.11217430293987));
#39243=CARTESIAN_POINT('Ctrl Pts',(-21.805833618262,26.2600746830372,-3.11241935795831));
#39244=CARTESIAN_POINT('Ctrl Pts',(-21.7962801454155,26.2539080185247,-3.11311938189167));
#39245=CARTESIAN_POINT('Ctrl Pts',(-21.7900880304783,26.2498808487965,-3.11357491540667));
#39246=CARTESIAN_POINT('Ctrl Pts',(-21.7762252664494,26.2407969438803,-3.11459885101972));
#39247=CARTESIAN_POINT('Ctrl Pts',(-21.7685623096419,26.2357286387576,-3.11516768640381));
#39248=CARTESIAN_POINT('Ctrl Pts',(-21.627106895636,26.1412976014961,-3.12572112375304));
#39249=CARTESIAN_POINT('Ctrl Pts',(-21.5001915959202,26.0420870881447,-3.13608712839143));
#39250=CARTESIAN_POINT('Ctrl Pts',(-21.1487327651533,25.7222642416072,-3.16757106908893));
#39251=CARTESIAN_POINT('Ctrl Pts',(-20.9484621960914,25.477842528873,-3.18949428733414));
#39252=CARTESIAN_POINT('Ctrl Pts',(-20.7844139327084,25.2044215027958,-3.20991184700231));
#39253=CARTESIAN_POINT('Ctrl Pts',(-20.7820882678076,25.2005266753592,-3.2102018854314));
#39254=CARTESIAN_POINT('Ctrl Pts',(-20.7770892269645,25.1921144021374,-3.21082657022639));
#39255=CARTESIAN_POINT('Ctrl Pts',(-20.7744186424213,25.1875952985944,-3.2111610639708));
#39256=CARTESIAN_POINT('Ctrl Pts',(-20.7672855715749,25.1754572641211,-3.2120565351764));
#39257=CARTESIAN_POINT('Ctrl Pts',(-20.762843297079,25.1678264206413,-3.21261637659596));
#39258=CARTESIAN_POINT('Ctrl Pts',(-20.7511616381436,25.1475688961617,-3.21409415249107));
#39259=CARTESIAN_POINT('Ctrl Pts',(-20.7439762248941,25.1349110777381,-3.21500890636815));
#39260=CARTESIAN_POINT('Ctrl Pts',(-20.7350311059628,25.1189016966401,-3.21615461940451));
#39261=CARTESIAN_POINT('Ctrl Pts',(-20.7331913672111,25.1155953933362,-3.21639063419207));
#39262=CARTESIAN_POINT('Ctrl Pts',(-20.7303002054151,25.1103779106149,-3.21676211907669));
#39263=CARTESIAN_POINT('Ctrl Pts',(-20.7292449000755,25.1084689039789,-3.21689783901887));
#39264=CARTESIAN_POINT('Ctrl Pts',(-20.7272912516306,25.1049263396863,-3.2171493205975));
#39265=CARTESIAN_POINT('Ctrl Pts',(-20.7263923932336,25.1032930837859,-3.21726511511223));
#39266=CARTESIAN_POINT('Ctrl Pts',(-20.7243966665359,25.0996593204121,-3.21752241317762));
#39267=CARTESIAN_POINT('Ctrl Pts',(-20.7233005077514,25.0976584325419,-3.21766387048355));
#39268=CARTESIAN_POINT('Ctrl Pts',(-20.7201201376017,25.0918384436021,-3.21807469137683));
#39269=CARTESIAN_POINT('Ctrl Pts',(-20.7180415236932,25.0880162647072,-3.21834369531924));
#39270=CARTESIAN_POINT('Ctrl Pts',(-20.7035197927782,25.0611842174393,-3.22022663717745));
#39271=CARTESIAN_POINT('Ctrl Pts',(-20.6913490266913,25.0380269435037,-3.22182342936607));
#39272=CARTESIAN_POINT('Ctrl Pts',(-20.6572660754931,24.9712143752057,-3.22635728895278));
#39273=CARTESIAN_POINT('Ctrl Pts',(-20.6360617185373,24.9272041099921,-3.22925544303751));
#39274=CARTESIAN_POINT('Ctrl Pts',(-20.5978124873225,24.8429712576515,-3.23466833505986));
#39275=CARTESIAN_POINT('Ctrl Pts',(-20.580569210251,24.8028518967939,-3.23719052580586));
#39276=CARTESIAN_POINT('Ctrl Pts',(-20.4372565046046,24.4498012524041,-3.25900292560566));
#39277=CARTESIAN_POINT('Ctrl Pts',(-20.3602356242372,24.1192378336382,-3.27707850944475));
#39278=CARTESIAN_POINT('Ctrl Pts',(-20.3349082663448,23.7690379877467,-3.29789718906894));
#39279=CARTESIAN_POINT('Ctrl Pts',(-20.3340059498439,23.755346990209,-3.29871323895835));
#39280=CARTESIAN_POINT('Ctrl Pts',(-20.3327820150424,23.7347748422324,-3.29994286698378));
#39281=CARTESIAN_POINT('Ctrl Pts',(-20.3323949795844,23.7278976325604,-3.3003545029345));
#39282=CARTESIAN_POINT('Ctrl Pts',(-20.3318858803563,23.7183032900765,-3.30092959730288));
#39283=CARTESIAN_POINT('Ctrl Pts',(-20.3317452022062,23.7155871312244,-3.30109249865328));
#39284=CARTESIAN_POINT('Ctrl Pts',(-20.3313007998519,23.7067912363577,-3.30162033290429));
#39285=CARTESIAN_POINT('Ctrl Pts',(-20.33101086416,23.7007108423363,-3.30198567841849));
#39286=CARTESIAN_POINT('Ctrl Pts',(-20.3301520313107,23.6815594429559,-3.3031379071427));
#39287=CARTESIAN_POINT('Ctrl Pts',(-20.3296455078209,23.668485892618,-3.30392666898512));
#39288=CARTESIAN_POINT('Ctrl Pts',(-20.3285546351352,23.6350717582092,-3.30594850691942));
#39289=CARTESIAN_POINT('Ctrl Pts',(-20.3280833113431,23.6147282928021,-3.30718502200711));
#39290=CARTESIAN_POINT('Ctrl Pts',(-20.3277191156577,23.5881338330159,-3.30880917625656));
#39291=CARTESIAN_POINT('Ctrl Pts',(-20.3276517229676,23.5818853815036,-3.30919133088));
#39292=CARTESIAN_POINT('Ctrl Pts',(-20.3275758739647,23.5722560035519,-3.30978112991998));
#39293=CARTESIAN_POINT('Ctrl Pts',(-20.32755456411,23.5688751694983,-3.30998837062342));
#39294=CARTESIAN_POINT('Ctrl Pts',(-20.3275227640037,23.5621513746698,-3.31040086059076));
#39295=CARTESIAN_POINT('Ctrl Pts',(-20.3275121551373,23.5588084184645,-3.31060610587258));
#39296=CARTESIAN_POINT('Ctrl Pts',(-20.3275003209145,23.5514922467953,-3.31105564982359));
#39297=CARTESIAN_POINT('Ctrl Pts',(-20.3275012417615,23.5475190375955,-3.31130001556216));
#39298=CARTESIAN_POINT('Ctrl Pts',(-20.3275247463536,23.5362244341546,-3.31199533357431));
#39299=CARTESIAN_POINT('Ctrl Pts',(-20.3275649315981,23.5289031360081,-3.31244683776656));
#39300=CARTESIAN_POINT('Ctrl Pts',(-20.3277109917855,23.5124856427681,-3.31346110224683));
#39301=CARTESIAN_POINT('Ctrl Pts',(-20.3278304329106,23.5033896585709,-3.31402428567378));
#39302=CARTESIAN_POINT('Ctrl Pts',(-20.3283225417495,23.475052329362,-3.31578272725679));
#39303=CARTESIAN_POINT('Ctrl Pts',(-20.3288290466735,23.4558140080136,-3.31698217247114));
#39304=CARTESIAN_POINT('Ctrl Pts',(-20.3313671587614,23.3838992385282,-3.32148745558336));
#39305=CARTESIAN_POINT('Ctrl Pts',(-20.3345187272752,23.3312730004496,-3.32482797106629));
#39306=CARTESIAN_POINT('Ctrl Pts',(-20.3474770468649,23.1780037861943,-3.33468856151785));
#39307=CARTESIAN_POINT('Ctrl Pts',(-20.3607302291696,23.0777229822386,-3.34130845058533));
#39308=CARTESIAN_POINT('Ctrl Pts',(-20.4352670071636,22.6644476900113,-3.36922967613078));
#39309=CARTESIAN_POINT('Ctrl Pts',(-20.5381086912875,22.3608119369038,-3.39148629748535));
#39310=CARTESIAN_POINT('Ctrl Pts',(-20.6913116872759,22.0626901771717,-3.41270112515197));
#39311=CARTESIAN_POINT('Ctrl Pts',(-20.6988901774037,22.0482148284786,-3.4137289867691));
#39312=CARTESIAN_POINT('Ctrl Pts',(-20.7082709259173,22.0306239423479,-3.41497476906555));
#39313=CARTESIAN_POINT('Ctrl Pts',(-20.7099685574379,22.0274533187226,-3.41519918000799));
#39314=CARTESIAN_POINT('Ctrl Pts',(-20.7127739886504,22.0222346974916,-3.41556831866835));
#39315=CARTESIAN_POINT('Ctrl Pts',(-20.7138787003547,22.0201850583981,-3.41571324218781));
#39316=CARTESIAN_POINT('Ctrl Pts',(-20.7158732940226,22.0164939503574,-3.41597412263115));
#39317=CARTESIAN_POINT('Ctrl Pts',(-20.7167623791621,22.0148520613506,-3.41609013013811));
#39318=CARTESIAN_POINT('Ctrl Pts',(-20.718675903383,22.0113256454033,-3.41633920652058));
#39319=CARTESIAN_POINT('Ctrl Pts',(-20.7197007942789,22.0094413734963,-3.41647224546646));
#39320=CARTESIAN_POINT('Ctrl Pts',(-20.7225093737042,22.0042900320959,-3.41683582226988));
#39321=CARTESIAN_POINT('Ctrl Pts',(-20.724296849491,22.0010250144202,-3.41706611712103));
#39322=CARTESIAN_POINT('Ctrl Pts',(-20.7335612041514,21.9841720538984,-3.41825410245119));
#39323=CARTESIAN_POINT('Ctrl Pts',(-20.7411306077314,21.9706348131623,-3.41920593085081));
#39324=CARTESIAN_POINT('Ctrl Pts',(-20.7857276633813,21.8922112162942,-3.42470898596819));
#39325=CARTESIAN_POINT('Ctrl Pts',(-20.8249079685812,21.8285679748215,-3.42913075517134));
#39326=CARTESIAN_POINT('Ctrl Pts',(-20.8896091848416,21.7312218711983,-3.43591656849854));
#39327=CARTESIAN_POINT('Ctrl Pts',(-20.9136375557161,21.6965650566027,-3.43833708242893));
#39328=CARTESIAN_POINT('Ctrl Pts',(-21.1016072789672,21.4365036556913,-3.45661451012401));
#39329=CARTESIAN_POINT('Ctrl Pts',(-21.2934811807223,21.2327562144385,-3.47171171900096));
#39330=CARTESIAN_POINT('Ctrl Pts',(-21.5878872878923,20.9918187389081,-3.49382923461142));
#39331=CARTESIAN_POINT('Ctrl Pts',(-21.6695898250489,20.9311753419974,-3.49986232380336));
#39332=CARTESIAN_POINT('Ctrl Pts',(-21.7618346328459,20.869251291161,-3.50662448700155));
#39333=CARTESIAN_POINT('Ctrl Pts',(-21.7696757563003,20.8640372431082,-3.5071988954544));
#39334=CARTESIAN_POINT('Ctrl Pts',(-21.7813326589687,20.8563593126052,-3.50805228764202));
#39335=CARTESIAN_POINT('Ctrl Pts',(-21.78513102622,20.8538689791287,-3.50833027770117));
#39336=CARTESIAN_POINT('Ctrl Pts',(-21.791633664599,20.8496252656295,-3.50880604434361));
#39337=CARTESIAN_POINT('Ctrl Pts',(-21.7943353326222,20.8478678921942,-3.50900367111503));
#39338=CARTESIAN_POINT('Ctrl Pts',(-21.7997582040599,20.8443520034477,-3.50940027325574));
#39339=CARTESIAN_POINT('Ctrl Pts',(-21.8024794316459,20.8425935335055,-3.50959924996803));
#39340=CARTESIAN_POINT('Ctrl Pts',(-21.8087625460157,20.8385467741265,-3.51005858173033));
#39341=CARTESIAN_POINT('Ctrl Pts',(-21.8123262934419,20.8362613975957,-3.51031904497681));
#39342=CARTESIAN_POINT('Ctrl Pts',(-21.823101247575,20.8293815102322,-3.51110635732045));
#39343=CARTESIAN_POINT('Ctrl Pts',(-21.8303262030297,20.8248086971283,-3.51163401189023));
#39344=CARTESIAN_POINT('Ctrl Pts',(-21.8468849982811,20.8144203824624,-3.51284277622807));
#39345=CARTESIAN_POINT('Ctrl Pts',(-21.8562305402623,20.8086238204403,-3.5135245801558));
#39346=CARTESIAN_POINT('Ctrl Pts',(-21.8867866361249,20.7898873194417,-3.51575259289498));
#39347=CARTESIAN_POINT('Ctrl Pts',(-21.9081167897839,20.777145061713,-3.51730601536662));
#39348=CARTESIAN_POINT('Ctrl Pts',(-21.9935337498009,20.7274495393203,-3.523520494314));
#39349=CARTESIAN_POINT('Ctrl Pts',(-22.0587331900814,20.6924633987414,-3.52825097890112));
#39350=CARTESIAN_POINT('Ctrl Pts',(-22.2307490273806,20.6076499521125,-3.54070189462505));
#39351=CARTESIAN_POINT('Ctrl Pts',(-22.3391920540689,20.5613852669244,-3.54852587884169));
#39352=CARTESIAN_POINT('Ctrl Pts',(-22.6902340144543,20.4338668914472,-3.57363499264321));
#39353=CARTESIAN_POINT('Ctrl Pts',(-22.9400928691539,20.3754756776395,-3.59125660907819));
#39354=CARTESIAN_POINT('Ctrl Pts',(-23.1971128654555,20.3469076653475,-3.60780299921877));
#39355=CARTESIAN_POINT('Ctrl Pts',(-23.1999928352131,20.3465914850515,-3.60798819783091));
#39356=CARTESIAN_POINT('Ctrl Pts',(-23.2101054723464,20.3454950587212,-3.60863776074529));
#39357=CARTESIAN_POINT('Ctrl Pts',(-23.2173404156002,20.3447354115217,-3.60910115674214));
#39358=CARTESIAN_POINT('Ctrl Pts',(-23.2255919180676,20.3438972664085,-3.60962810657254));
#39359=CARTESIAN_POINT('Ctrl Pts',(-23.2266059376766,20.3437947534865,-3.60969283617012));
#39360=CARTESIAN_POINT('Ctrl Pts',(-23.2475368661123,20.3416887586883,-3.61102839964508));
#39361=CARTESIAN_POINT('Ctrl Pts',(-23.2674725764781,20.3398703417643,-3.61229008565064));
#39362=CARTESIAN_POINT('Ctrl Pts',(-23.2912750506689,20.3379226680949,-3.61378308714745));
#39363=CARTESIAN_POINT('Ctrl Pts',(-23.2951261556685,20.337614515843,-3.61402422814353));
#39364=CARTESIAN_POINT('Ctrl Pts',(-23.3013810731477,20.3371253368053,-3.61441519715343));
#39365=CARTESIAN_POINT('Ctrl Pts',(-23.3037845350202,20.3369400818839,-3.61456526240293));
#39366=CARTESIAN_POINT('Ctrl Pts',(-23.3080581077314,20.3366155048692,-3.61483179555489));
#39367=CARTESIAN_POINT('Ctrl Pts',(-23.3099281311343,20.3364751184709,-3.61494832372249));
#39368=CARTESIAN_POINT('Ctrl Pts',(-23.3138852191887,20.3361815251161,-3.61519469025364));
#39369=CARTESIAN_POINT('Ctrl Pts',(-23.3159723054859,20.3360287191051,-3.61532450541527));
#39370=CARTESIAN_POINT('Ctrl Pts',(-23.3215385056725,20.335626640068,-3.61567038658308));
#39371=CARTESIAN_POINT('Ctrl Pts',(-23.3250178903064,20.33538098132,-3.61588624792674));
#39372=CARTESIAN_POINT('Ctrl Pts',(-23.3412907449379,20.334258599004,-3.61689422781572));
#39373=CARTESIAN_POINT('Ctrl Pts',(-23.3540892090944,20.3334525740801,-3.61768240206108));
#39374=CARTESIAN_POINT('Ctrl Pts',(-23.6611964437418,20.3159511889739,-3.63649228160364));
#39375=CARTESIAN_POINT('Ctrl Pts',(-23.9564674332818,20.3396340472565,-3.65240117808815));
#39376=CARTESIAN_POINT('Ctrl Pts',(-24.3476659219888,20.4259248960626,-3.67494596206755));
#39377=CARTESIAN_POINT('Ctrl Pts',(-24.4497018342685,20.4537577470525,-3.6809568410531));
#39378=CARTESIAN_POINT('Ctrl Pts',(-24.645272535807,20.5175879495613,-3.69292569721338));
#39379=CARTESIAN_POINT('Ctrl Pts',(-24.7388593186507,20.5530314768552,-3.69886238225315));
#39380=CARTESIAN_POINT('Ctrl Pts',(-24.8392460979695,20.5964920316765,-3.70552057819909));
#39381=CARTESIAN_POINT('Ctrl Pts',(-24.8478356248044,20.60025530815,-3.70609263808224));
#39382=CARTESIAN_POINT('Ctrl Pts',(-24.8605520787762,20.6058929743546,-3.70694309492361));
#39383=CARTESIAN_POINT('Ctrl Pts',(-24.8646917274236,20.6077386903727,-3.70722050756741));
#39384=CARTESIAN_POINT('Ctrl Pts',(-24.8717659533681,20.6109107329723,-3.70769553968746));
#39385=CARTESIAN_POINT('Ctrl Pts',(-24.8747024701196,20.6122327404283,-3.70789301036694));
#39386=CARTESIAN_POINT('Ctrl Pts',(-24.8805877349573,20.6148928782297,-3.70828934730965));
#39387=CARTESIAN_POINT('Ctrl Pts',(-24.8835364569966,20.6162310555221,-3.7084882149881));
#39388=CARTESIAN_POINT('Ctrl Pts',(-24.8894590481103,20.6189295942829,-3.70888822992542));
#39389=CARTESIAN_POINT('Ctrl Pts',(-24.8924328730145,20.6202900424715,-3.70908937998969));
#39390=CARTESIAN_POINT('Ctrl Pts',(-24.9018905781676,20.6246341190074,-3.70973004810133));
#39391=CARTESIAN_POINT('Ctrl Pts',(-24.9083665861363,20.627634746362,-3.71017015381869));
#39392=CARTESIAN_POINT('Ctrl Pts',(-24.9461944677564,20.6453149925964,-3.71274928837823));
#39393=CARTESIAN_POINT('Ctrl Pts',(-24.9773171476909,20.6604770342075,-3.71490501928254));
#39394=CARTESIAN_POINT('Ctrl Pts',(-25.0668504056003,20.7058940556585,-3.72120790096503));
#39395=CARTESIAN_POINT('Ctrl Pts',(-25.1245837032092,20.7374381753716,-3.72539967381491));
#39396=CARTESIAN_POINT('Ctrl Pts',(-25.2500102038357,20.8110397494385,-3.7347965314476));
#39397=CARTESIAN_POINT('Ctrl Pts',(-25.3171892415055,20.8538853576992,-3.74002578551684));
#39398=CARTESIAN_POINT('Ctrl Pts',(-25.6473207923854,21.0820759649078,-3.76669041093025));
#39399=CARTESIAN_POINT('Ctrl Pts',(-25.8830427121671,21.3035497250365,-3.7891568339535));
#39400=CARTESIAN_POINT('Ctrl Pts',(-26.0919767670113,21.5688358196982,-3.81052410863379));
#39401=CARTESIAN_POINT('Ctrl Pts',(-26.1017964136027,21.5814970570262,-3.81153190292591));
#39402=CARTESIAN_POINT('Ctrl Pts',(-26.1136888918762,21.5970694009323,-3.81275628041603));
#39403=CARTESIAN_POINT('Ctrl Pts',(-26.1158516133871,21.5999111084258,-3.81297909889448));
#39404=CARTESIAN_POINT('Ctrl Pts',(-26.119411874759,21.6046052828185,-3.81334615421583));
#39405=CARTESIAN_POINT('Ctrl Pts',(-26.120812137393,21.6064556645459,-3.81349058309648));
#39406=CARTESIAN_POINT('Ctrl Pts',(-26.1233351498344,21.6097972019338,-3.81375093165768));
#39407=CARTESIAN_POINT('Ctrl Pts',(-26.1244585998637,21.611287816897,-3.81386690098521));
#39408=CARTESIAN_POINT('Ctrl Pts',(-26.1268737377152,21.6144980667079,-3.81411629420121));
#39409=CARTESIAN_POINT('Ctrl Pts',(-26.1281649957672,21.6162180139894,-3.81424968744386));
#39410=CARTESIAN_POINT('Ctrl Pts',(-26.1317018685611,21.6209389407278,-3.81461521773985));
#39411=CARTESIAN_POINT('Ctrl Pts',(-26.1339439802461,21.6239425592036,-3.81484710738031));
#39412=CARTESIAN_POINT('Ctrl Pts',(-26.1456332589118,21.6396590873752,-3.81605700183655));
#39413=CARTESIAN_POINT('Ctrl Pts',(-26.1549920669126,21.6524378920063,-3.81702888344381));
#39414=CARTESIAN_POINT('Ctrl Pts',(-26.247794629572,21.7811331219167,-3.82670425956788));
#39415=CARTESIAN_POINT('Ctrl Pts',(-26.3235509252817,21.9024224874691,-3.83491801903236));
#39416=CARTESIAN_POINT('Ctrl Pts',(-26.4900429549156,22.2131951527951,-3.85482929947714));
#39417=CARTESIAN_POINT('Ctrl Pts',(-26.5707907319383,22.4072564477704,-3.86633771881029));
#39418=CARTESIAN_POINT('Ctrl Pts',(-26.6377133469624,22.6260936063406,-3.87943350280407));
#39419=CARTESIAN_POINT('Ctrl Pts',(-26.6431481818419,22.6444487526349,-3.88053246862601));
#39420=CARTESIAN_POINT('Ctrl Pts',(-26.6628868599382,22.7133619924785,-3.88466255817534));
#39421=CARTESIAN_POINT('Ctrl Pts',(-26.6761166333174,22.7642172531722,-3.88771877644782));
#39422=CARTESIAN_POINT('Ctrl Pts',(-26.7049169487885,22.8871907650272,-3.89515260637662));
#39423=CARTESIAN_POINT('Ctrl Pts',(-26.7192652026212,22.9595615236503,-3.89956336771272));
#39424=CARTESIAN_POINT('Ctrl Pts',(-26.7325085047014,23.0409005732024,-3.90458222000383));
#39425=CARTESIAN_POINT('Ctrl Pts',(-26.7338651442123,23.0494499493567,-3.90511048440937));
#39426=CARTESIAN_POINT('Ctrl Pts',(-26.7358521422731,23.062306193363,-3.9059060205549));
#39427=CARTESIAN_POINT('Ctrl Pts',(-26.7365082541625,23.0666090899459,-3.90617247456588));
#39428=CARTESIAN_POINT('Ctrl Pts',(-26.7376275223649,23.0740505822616,-3.90663362328748));
#39429=CARTESIAN_POINT('Ctrl Pts',(-26.7380947660825,23.0771885652604,-3.90682818807761));
#39430=CARTESIAN_POINT('Ctrl Pts',(-26.7390247983188,23.0834985601429,-3.90721963910655));
#39431=CARTESIAN_POINT('Ctrl Pts',(-26.7394874892114,23.0866705821023,-3.90741652817207));
#39432=CARTESIAN_POINT('Ctrl Pts',(-26.7404176493971,23.0931146866533,-3.90781673732065));
#39433=CARTESIAN_POINT('Ctrl Pts',(-26.7408848188975,23.0963868078259,-3.90802006664926));
#39434=CARTESIAN_POINT('Ctrl Pts',(-26.7419493485436,23.1039257961634,-3.90848880665395));
#39435=CARTESIAN_POINT('Ctrl Pts',(-26.7425431866619,23.1081931471619,-3.90875432871478));
#39436=CARTESIAN_POINT('Ctrl Pts',(-26.7440489305974,23.1191747684734,-3.90943813860956));
#39437=CARTESIAN_POINT('Ctrl Pts',(-26.744948218134,23.125890722023,-3.90985682567316));
#39438=CARTESIAN_POINT('Ctrl Pts',(-26.7640325227331,23.2719132513757,-3.91897110692897));
#39439=CARTESIAN_POINT('Ctrl Pts',(-26.7731074835901,23.4122349794034,-3.92795586024967));
#39440=CARTESIAN_POINT('Ctrl Pts',(-26.7730016161112,23.552681809173,-3.93718354728755));
#39441=CARTESIAN_POINT('Ctrl Pts',(-26.7730016191972,23.5526777117792,-3.93718327807921));
#39442=CARTESIAN_POINT('Ctrl Pts',(-26.7728336327151,23.7759099102419,-3.95185015161121));
#39443=CARTESIAN_POINT('Ctrl Pts',(-26.7494711541764,23.9985172774985,-3.96710418728231));
#39444=CARTESIAN_POINT('Ctrl Pts',(-26.6831336232011,24.3122736075055,-3.9886734987549));
#39445=CARTESIAN_POINT('Ctrl Pts',(-26.6586505654969,24.4066897277443,-3.99516388714361));
#39446=CARTESIAN_POINT('Ctrl Pts',(-26.6198690538734,24.5324623615074,-4.00369214877209));
#39447=CARTESIAN_POINT('Ctrl Pts',(-26.6092977090653,24.5649074278942,-4.00588116977758));
#39448=CARTESIAN_POINT('Ctrl Pts',(-26.5923670199883,24.6141983959673,-4.00918351284334));
#39449=CARTESIAN_POINT('Ctrl Pts',(-26.5863788383415,24.6311680916985,-4.0103161718275));
#39450=CARTESIAN_POINT('Ctrl Pts',(-26.5789185356788,24.6517583398107,-4.01168452098841));
#39451=CARTESIAN_POINT('Ctrl Pts',(-26.5775817221573,24.6554270798815,-4.01192809984516));
#39452=CARTESIAN_POINT('Ctrl Pts',(-26.575486360734,24.6611452436578,-4.01230737459805));
#39453=CARTESIAN_POINT('Ctrl Pts',(-26.5747323962068,24.663196325013,-4.01244334418726));
#39454=CARTESIAN_POINT('Ctrl Pts',(-26.5733960723866,24.6668202671541,-4.01268344726817));
#39455=CARTESIAN_POINT('Ctrl Pts',(-26.5728145744723,24.6683934320668,-4.01278763193865));
#39456=CARTESIAN_POINT('Ctrl Pts',(-26.571569606587,24.6717534583432,-4.01301005793523));
#39457=CARTESIAN_POINT('Ctrl Pts',(-26.5709057813275,24.6735401800909,-4.01312827715612));
#39458=CARTESIAN_POINT('Ctrl Pts',(-26.56898398563,24.6786987747581,-4.01346943416195));
#39459=CARTESIAN_POINT('Ctrl Pts',(-26.5677219465601,24.682069144541,-4.01369212714684));
#39460=CARTESIAN_POINT('Ctrl Pts',(-26.5620998063961,24.697007247705,-4.01467827671479));
#39461=CARTESIAN_POINT('Ctrl Pts',(-26.5576787376439,24.7085521527988,-4.01543811386994));
#39462=CARTESIAN_POINT('Ctrl Pts',(-26.552136447766,24.7227792739579,-4.01637196251905));
#39463=CARTESIAN_POINT('Ctrl Pts',(-26.5510779664004,24.7254855798491,-4.01654948769521));
#39464=CARTESIAN_POINT('Ctrl Pts',(-26.4255609228959,25.0451301122219,-4.03750422129371));
#39465=CARTESIAN_POINT('Ctrl Pts',(-26.2516423830581,25.3404052804288,-4.05553471311839));
#39466=CARTESIAN_POINT('Ctrl Pts',(-25.993266798087,25.6531133875712,-4.07864825391055));
#39467=CARTESIAN_POINT('Ctrl Pts',(-25.9503603187814,25.7019552149541,-4.08238877604869));
#39468=CARTESIAN_POINT('Ctrl Pts',(-25.8453083372892,25.8144849659556,-4.09137260309972));
#39469=CARTESIAN_POINT('Ctrl Pts',(-25.7819476879176,25.8769592539073,-4.09665841262858));
#39470=CARTESIAN_POINT('Ctrl Pts',(-25.7065369247427,25.9453979466044,-4.1028460980298));
#39471=CARTESIAN_POINT('Ctrl Pts',(-25.6969333744224,25.9540090281287,-4.10363223842742));
#39472=CARTESIAN_POINT('Ctrl Pts',(-25.6843842381346,25.9651261045282,-4.10465719925248));
#39473=CARTESIAN_POINT('Ctrl Pts',(-25.6814853778949,25.9676848613109,-4.10489380754055));
#39474=CARTESIAN_POINT('Ctrl Pts',(-25.6761988332345,25.9723342721304,-4.10532501686365));
#39475=CARTESIAN_POINT('Ctrl Pts',(-25.6738126489147,25.9744266308095,-4.10551954644499));
#39476=CARTESIAN_POINT('Ctrl Pts',(-25.6691569182061,25.9784969235143,-4.10589889441023));
#39477=CARTESIAN_POINT('Ctrl Pts',(-25.6668876825266,25.9804752095058,-4.10608369787106));
#39478=CARTESIAN_POINT('Ctrl Pts',(-25.6617052249204,25.9849804341673,-4.10650553937267));
#39479=CARTESIAN_POINT('Ctrl Pts',(-25.6587902366496,25.9875053255973,-4.1067426620319));
#39480=CARTESIAN_POINT('Ctrl Pts',(-25.6509304698171,25.9942886090889,-4.10738162032149));
#39481=CARTESIAN_POINT('Ctrl Pts',(-25.6459772968533,25.9985372077518,-4.10778386033387));
#39482=CARTESIAN_POINT('Ctrl Pts',(-25.6231479266305,26.0179991249098,-4.10963587847788));
#39483=CARTESIAN_POINT('Ctrl Pts',(-25.6051191192121,26.0330315849323,-4.11109306572182));
#39484=CARTESIAN_POINT('Ctrl Pts',(-25.5776413846346,26.0554382717038,-4.11330637656465));
#39485=CARTESIAN_POINT('Ctrl Pts',(-25.5683126254925,26.0629591609153,-4.11405650155353));
#39486=CARTESIAN_POINT('Ctrl Pts',(-25.5550517343898,26.0735286701699,-4.11512102350802));
#39487=CARTESIAN_POINT('Ctrl Pts',(-25.5511540714221,26.0766205456614,-4.11543369294684));
#39488=CARTESIAN_POINT('Ctrl Pts',(-25.5458511497258,26.0808071925165,-4.11585880087854));
#39489=CARTESIAN_POINT('Ctrl Pts',(-25.5444521045998,26.0819098542997,-4.11597092770353));
#39490=CARTESIAN_POINT('Ctrl Pts',(-25.5394136428434,26.0858741656935,-4.11637463817346));
#39491=CARTESIAN_POINT('Ctrl Pts',(-25.5357689880651,26.0887291217053,-4.11666648442644));
#39492=CARTESIAN_POINT('Ctrl Pts',(-25.5305069230252,26.0928327729702,-4.11708758166432));
#39493=CARTESIAN_POINT('Ctrl Pts',(-25.5288944451092,26.0940878086254,-4.11721658482149));
#39494=CARTESIAN_POINT('Ctrl Pts',(-25.5218101597198,26.0995908906593,-4.11778319386628));
#39495=CARTESIAN_POINT('Ctrl Pts',(-25.5163258889227,26.1038227974034,-4.11822142543565));
#39496=CARTESIAN_POINT('Ctrl Pts',(-25.5068573150424,26.1110805842291,-4.11897733872554));
#39497=CARTESIAN_POINT('Ctrl Pts',(-25.5028795153936,26.1141149412143,-4.11929469295917));
#39498=CARTESIAN_POINT('Ctrl Pts',(-25.4957007129822,26.1195646997647,-4.11986705364709));
#39499=CARTESIAN_POINT('Ctrl Pts',(-25.4925022307709,26.1219834175526,-4.12012193320673));
#39500=CARTESIAN_POINT('Ctrl Pts',(-25.4856156562066,26.1271709252496,-4.12067042354279));
#39501=CARTESIAN_POINT('Ctrl Pts',(-25.4819261218426,26.1299377782967,-4.12096410651717));
#39502=CARTESIAN_POINT('Ctrl Pts',(-25.461684519251,26.1450495735585,-4.12257436355939));
#39503=CARTESIAN_POINT('Ctrl Pts',(-25.4450203319108,26.1572429198352,-4.12389655355184));
#39504=CARTESIAN_POINT('Ctrl Pts',(-25.407532310553,26.1841239599864,-4.12686330842022));
#39505=CARTESIAN_POINT('Ctrl Pts',(-25.3866492795549,26.1987263953671,-4.12851077996509));
#39506=CARTESIAN_POINT('Ctrl Pts',(-25.2862664408559,26.267160925678,-4.13640511988243));
#39507=CARTESIAN_POINT('Ctrl Pts',(-25.2045658889655,26.3176665511896,-4.14275875411517));
#39508=CARTESIAN_POINT('Ctrl Pts',(-24.862725719322,26.5084334380641,-4.1689722350157));
#39509=CARTESIAN_POINT('Ctrl Pts',(-24.5861379701052,26.616255291323,-4.18948368793534));
#39510=CARTESIAN_POINT('Ctrl Pts',(-24.2906713409112,26.6868057614825,-4.20864143254407));
#39511=CARTESIAN_POINT('Ctrl Pts',(-24.2826069971575,26.6886985033127,-4.2091621794511));
#39512=CARTESIAN_POINT('Ctrl Pts',(-24.2686036342257,26.6919282490206,-4.21006262182683));
#39513=CARTESIAN_POINT('Ctrl Pts',(-24.2626680033923,26.6932795466074,-4.21044310878972));
#39514=CARTESIAN_POINT('Ctrl Pts',(-24.2541751033628,26.6951877336779,-4.21098579338859));
#39515=CARTESIAN_POINT('Ctrl Pts',(-24.2516209760631,26.6957583283732,-4.21114877527473));
#39516=CARTESIAN_POINT('Ctrl Pts',(-24.2472048157776,26.696739256868,-4.21143018635761));
#39517=CARTESIAN_POINT('Ctrl Pts',(-24.2453431111723,26.6971510499783,-4.21154870025574));
#39518=CARTESIAN_POINT('Ctrl Pts',(-24.2417589335762,26.6979405035482,-4.21177663336352));
#39519=CARTESIAN_POINT('Ctrl Pts',(-24.2400365195256,26.6983184017432,-4.21188606636495));
#39520=CARTESIAN_POINT('Ctrl Pts',(-24.2359547161622,26.6992104399149,-4.21214516109982));
#39521=CARTESIAN_POINT('Ctrl Pts',(-24.2335950534028,26.6997233430598,-4.21229475108248));
#39522=CARTESIAN_POINT('Ctrl Pts',(-24.2253285333156,26.7015104502032,-4.21281814276097));
#39523=CARTESIAN_POINT('Ctrl Pts',(-24.2194186231444,26.7027707029954,-4.2131911442657));
#39524=CARTESIAN_POINT('Ctrl Pts',(-24.2014132749565,26.7065573219616,-4.21432404328435));
#39525=CARTESIAN_POINT('Ctrl Pts',(-24.189306652564,26.7090307899159,-4.21508098890193));
#39526=CARTESIAN_POINT('Ctrl Pts',(-23.8961781515021,26.7671647498285,-4.23329884765875));
#39527=CARTESIAN_POINT('Ctrl Pts',(-23.6089416045226,26.7851877217823,-4.24879961257162));
#39528=CARTESIAN_POINT('Ctrl Pts',(-23.2201739368802,26.7577134448672,-4.27071409289777));
#39529=CARTESIAN_POINT('Ctrl Pts',(-23.1176948338158,26.7455066969607,-4.27656964599048));
#39530=CARTESIAN_POINT('Ctrl Pts',(-22.9430996190028,26.7161560231207,-4.28684125176797));
#39531=CARTESIAN_POINT('Ctrl Pts',(-22.8706643773789,26.7014012601985,-4.29119110434243));
#39532=CARTESIAN_POINT('Ctrl Pts',(-22.7746610488359,26.6783816545602,-4.29710684683183));
#39533=CARTESIAN_POINT('Ctrl Pts',(-22.7505863152861,26.6723140057396,-4.29860308581414));
#39534=CARTESIAN_POINT('Ctrl Pts',(-22.7159585223496,26.6631598340035,-4.30077460580838));
#39535=CARTESIAN_POINT('Ctrl Pts',(-22.7053470008415,26.6602964230362,-4.30144270126641));
#39536=CARTESIAN_POINT('Ctrl Pts',(-22.6865217621372,26.6551131669631,-4.30263272039935));
#39537=CARTESIAN_POINT('Ctrl Pts',(-22.6783021842503,26.6528148592079,-4.30315394199495));
#39538=CARTESIAN_POINT('Ctrl Pts',(-22.6660160917138,26.6493268179649,-4.30393550318894));
#39539=CARTESIAN_POINT('Ctrl Pts',(-22.6619425900287,26.6481616589734,-4.30419504052507));
#39540=CARTESIAN_POINT('Ctrl Pts',(-22.6547591392241,26.646091616199,-4.30465344800714));
#39541=CARTESIAN_POINT('Ctrl Pts',(-22.6516482281152,26.6451900687973,-4.30485220887214));
#39542=CARTESIAN_POINT('Ctrl Pts',(-22.6454458940905,26.6433824819026,-4.30524896652729));
#39543=CARTESIAN_POINT('Ctrl Pts',(-22.6423544598315,26.6424764937171,-4.30544696145242));
#39544=CARTESIAN_POINT('Ctrl Pts',(-22.63491294079,26.6402835307959,-4.30592414076378));
#39545=CARTESIAN_POINT('Ctrl Pts',(-22.6305642133307,26.6389920057879,-4.30620347398674));
#39546=CARTESIAN_POINT('Ctrl Pts',(-22.6172186258811,26.6349978276751,-4.30706217593535));
#39547=CARTESIAN_POINT('Ctrl Pts',(-22.6082309047132,26.6322650335787,-4.30764253239619));
#39548=CARTESIAN_POINT('Ctrl Pts',(-22.5030125558045,26.5997692426221,-4.31446109410309));
#39549=CARTESIAN_POINT('Ctrl Pts',(-22.4082260683628,26.5655527880011,-4.3208458640486));
#39550=CARTESIAN_POINT('Ctrl Pts',(-22.2335879730295,26.4930947004337,-4.33308977919066));
#39551=CARTESIAN_POINT('Ctrl Pts',(-22.1534662401888,26.4559172684158,-4.33890733600597));
#39552=CARTESIAN_POINT('Ctrl Pts',(-22.0750357159536,26.4155366204114,-4.34479105736985));
#39553=CARTESIAN_POINT('Ctrl Pts',(-22.075036015346,26.4155367745563,-4.58978870905188));
#39554=CARTESIAN_POINT('Ctrl Pts',(-22.0797990834668,26.4179890816101,-4.589457698007));
#39555=CARTESIAN_POINT('Ctrl Pts',(-22.0845683014347,26.4204295299504,-4.58912742875724));
#39556=CARTESIAN_POINT('Ctrl Pts',(-22.1841440218444,26.4710703344603,-4.58225567891223));
#39557=CARTESIAN_POINT('Ctrl Pts',(-22.2812847583401,26.514566169619,-4.57600230409775));
#39558=CARTESIAN_POINT('Ctrl Pts',(-22.6088403691738,26.6421710623346,-4.55580530523899));
#39559=CARTESIAN_POINT('Ctrl Pts',(-22.8466846975347,26.7048083170721,-4.54248217815563));
#39560=CARTESIAN_POINT('Ctrl Pts',(-23.1988294621773,26.7556943264301,-4.52219936221725));
#39561=CARTESIAN_POINT('Ctrl Pts',(-23.3090489820097,26.7658664078369,-4.51578477715329));
#39562=CARTESIAN_POINT('Ctrl Pts',(-23.4688897361643,26.7723534718767,-4.50625409460115));
#39563=CARTESIAN_POINT('Ctrl Pts',(-23.5182504502743,26.7732216335089,-4.5032801468792));
#39564=CARTESIAN_POINT('Ctrl Pts',(-23.5754924223601,26.7729133345418,-4.49978960689193));
#39565=CARTESIAN_POINT('Ctrl Pts',(-23.5833749495089,26.7728419572942,-4.499308026359));
#39566=CARTESIAN_POINT('Ctrl Pts',(-23.5954040168434,26.772688893479,-4.49857169267415));
#39567=CARTESIAN_POINT('Ctrl Pts',(-23.5995508318443,26.7726281211795,-4.49831759641202));
#39568=CARTESIAN_POINT('Ctrl Pts',(-23.6067267313381,26.7725091021779,-4.49787744261328));
#39569=CARTESIAN_POINT('Ctrl Pts',(-23.6097558794429,26.7724545881699,-4.49769150251613));
#39570=CARTESIAN_POINT('Ctrl Pts',(-23.6160358822205,26.7723327116264,-4.49730572344989));
#39571=CARTESIAN_POINT('Ctrl Pts',(-23.6192867197137,26.7722647004907,-4.49710586431211));
#39572=CARTESIAN_POINT('Ctrl Pts',(-23.6271825093837,26.7720875567335,-4.49662004330929));
#39573=CARTESIAN_POINT('Ctrl Pts',(-23.6318273296969,26.7719732989266,-4.49633392073081));
#39574=CARTESIAN_POINT('Ctrl Pts',(-23.6492396578501,26.7715072941398,-4.49526006356324));
#39575=CARTESIAN_POINT('Ctrl Pts',(-23.662005153204,26.7710896961222,-4.49447026334825));
#39576=CARTESIAN_POINT('Ctrl Pts',(-23.8706145710358,26.7630237765639,-4.48152144685554));
#39577=CARTESIAN_POINT('Ctrl Pts',(-24.0653244861559,26.7376035150987,-4.46878868858443));
#39578=CARTESIAN_POINT('Ctrl Pts',(-24.3713388746256,26.6688724783629,-4.44781533513045));
#39579=CARTESIAN_POINT('Ctrl Pts',(-24.484684633235,26.6368053072332,-4.43983538719622));
#39580=CARTESIAN_POINT('Ctrl Pts',(-24.774942584346,26.5372298740477,-4.4190751410826));
#39581=CARTESIAN_POINT('Ctrl Pts',(-24.9481412767853,26.4602054204499,-4.40634864615721));
#39582=CARTESIAN_POINT('Ctrl Pts',(-25.120419607617,26.3646358994787,-4.39398056731649));
#39583=CARTESIAN_POINT('Ctrl Pts',(-25.1272258670839,26.3608278268348,-4.39349246757406));
#39584=CARTESIAN_POINT('Ctrl Pts',(-25.1365610677554,26.3555602358763,-4.39282381034444));
#39585=CARTESIAN_POINT('Ctrl Pts',(-25.1391018772499,26.3541219730222,-4.39264190035741));
#39586=CARTESIAN_POINT('Ctrl Pts',(-25.1433511688566,26.351708967859,-4.39233781282694));
#39587=CARTESIAN_POINT('Ctrl Pts',(-25.1450607129072,26.3507361143357,-4.39221551300868));
#39588=CARTESIAN_POINT('Ctrl Pts',(-25.1484269167665,26.3488164202625,-4.39197477414275));
#39589=CARTESIAN_POINT('Ctrl Pts',(-25.1500836263822,26.347869673478,-4.39185632929509));
#39590=CARTESIAN_POINT('Ctrl Pts',(-25.153735825363,26.3457782750215,-4.39159529856463));
#39591=CARTESIAN_POINT('Ctrl Pts',(-25.1557309354049,26.3446329549681,-4.39145275618068));
#39592=CARTESIAN_POINT('Ctrl Pts',(-25.1627026792051,26.3406207994701,-4.39095483152919));
#39593=CARTESIAN_POINT('Ctrl Pts',(-25.167672912484,26.337742775808,-4.39060017247096));
#39594=CARTESIAN_POINT('Ctrl Pts',(-25.2181198452733,26.3083510230434,-4.38700339913134));
#39595=CARTESIAN_POINT('Ctrl Pts',(-25.2629513524647,26.2807382393759,-4.38383139171528));
#39596=CARTESIAN_POINT('Ctrl Pts',(-25.5687756302272,26.081875882708,-4.3622194557549));
#39597=CARTESIAN_POINT('Ctrl Pts',(-25.8043812766291,25.874582329617,-4.34556050899947));
#39598=CARTESIAN_POINT('Ctrl Pts',(-26.0635865407976,25.5694210551125,-4.32265276985209));
#39599=CARTESIAN_POINT('Ctrl Pts',(-26.1178737533197,25.499921430596,-4.31753537093236));
#39600=CARTESIAN_POINT('Ctrl Pts',(-26.2042266936628,25.3794991066975,-4.308752083828));
#39601=CARTESIAN_POINT('Ctrl Pts',(-26.2378401991909,25.3297450685115,-4.30514591011375));
#39602=CARTESIAN_POINT('Ctrl Pts',(-26.2744901674349,25.2720874804144,-4.30098102958072));
#39603=CARTESIAN_POINT('Ctrl Pts',(-26.2789102603196,25.2650741797409,-4.30047466473154));
#39604=CARTESIAN_POINT('Ctrl Pts',(-26.285527976235,25.2544835697009,-4.29971034502765));
#39605=CARTESIAN_POINT('Ctrl Pts',(-26.2877457728553,25.2509188548589,-4.29945313705026));
#39606=CARTESIAN_POINT('Ctrl Pts',(-26.2915555595553,25.2447685368471,-4.29900945985568));
#39607=CARTESIAN_POINT('Ctrl Pts',(-26.2931508765982,25.2421849924323,-4.29882311370921));
#39608=CARTESIAN_POINT('Ctrl Pts',(-26.2964357599669,25.2368484148579,-4.29843825223085));
#39609=CARTESIAN_POINT('Ctrl Pts',(-26.2981248427757,25.2340950891277,-4.29823971935126));
#39610=CARTESIAN_POINT('Ctrl Pts',(-26.3026766331881,25.2266502569967,-4.29770297759967));
#39611=CARTESIAN_POINT('Ctrl Pts',(-26.3055314742636,25.2219539751102,-4.29736448018439));
#39612=CARTESIAN_POINT('Ctrl Pts',(-26.3160444717676,25.2045597558923,-4.29611104044488));
#39613=CARTESIAN_POINT('Ctrl Pts',(-26.3236268839384,25.1918164623113,-4.29519333112648));
#39614=CARTESIAN_POINT('Ctrl Pts',(-26.4477505196712,24.9798947491,-4.27993994259104));
#39615=CARTESIAN_POINT('Ctrl Pts',(-26.5426305894621,24.7688601285093,-4.2647945691676));
#39616=CARTESIAN_POINT('Ctrl Pts',(-26.6616210091264,24.4040282169322,-4.23894265356162));
#39617=CARTESIAN_POINT('Ctrl Pts',(-26.6986553303595,24.2553107148667,-4.2285091352454));
#39618=CARTESIAN_POINT('Ctrl Pts',(-26.732555814328,24.0611372282712,-4.21534249098413));
#39619=CARTESIAN_POINT('Ctrl Pts',(-26.739240739655,24.0175980659007,-4.21241999084546));
#39620=CARTESIAN_POINT('Ctrl Pts',(-26.7540046924746,23.9062701927076,-4.20504359664744));
#39621=CARTESIAN_POINT('Ctrl Pts',(-26.7608269565842,23.8383322897388,-4.20063247990639));
#39622=CARTESIAN_POINT('Ctrl Pts',(-26.7662361143637,23.7592686292224,-4.19564183160193));
#39623=CARTESIAN_POINT('Ctrl Pts',(-26.7669296135479,23.7483098274811,-4.19495327324181));
#39624=CARTESIAN_POINT('Ctrl Pts',(-26.7677585821542,23.7340547532595,-4.19406192926262));
#39625=CARTESIAN_POINT('Ctrl Pts',(-26.7679450101344,23.7307616888622,-4.19385631984731));
#39626=CARTESIAN_POINT('Ctrl Pts',(-26.7682391236181,23.7254211937342,-4.19352336750498));
#39627=CARTESIAN_POINT('Ctrl Pts',(-26.7683499108297,23.7233739469517,-4.19339584961283));
#39628=CARTESIAN_POINT('Ctrl Pts',(-26.7685589002173,23.7194424861783,-4.19315119596635));
#39629=CARTESIAN_POINT('Ctrl Pts',(-26.7686574010694,23.717558297197,-4.19303404388137));
#39630=CARTESIAN_POINT('Ctrl Pts',(-26.7688801581254,23.7132242533887,-4.19276479795247));
#39631=CARTESIAN_POINT('Ctrl Pts',(-26.7690032722777,23.710774336405,-4.19261276894541));
#39632=CARTESIAN_POINT('Ctrl Pts',(-26.769385334552,23.7029942664259,-4.19213050651392));
#39633=CARTESIAN_POINT('Ctrl Pts',(-26.769633842675,23.6976635741591,-4.1918008601863));
#39634=CARTESIAN_POINT('Ctrl Pts',(-26.7716439370443,23.6521135582221,-4.18899061305948));
#39635=CARTESIAN_POINT('Ctrl Pts',(-26.7726651043539,23.6118628633773,-4.18655082835764));
#39636=CARTESIAN_POINT('Ctrl Pts',(-26.7729762871449,23.5648887716828,-4.18374330021972));
#39637=CARTESIAN_POINT('Ctrl Pts',(-26.7729997826694,23.5581759949475,-4.18334304171166));
#39638=CARTESIAN_POINT('Ctrl Pts',(-26.7730352005879,23.4638902064783,-4.17773382955586));
#39639=CARTESIAN_POINT('Ctrl Pts',(-26.7694985965574,23.3763453175803,-4.17267913867162));
#39640=CARTESIAN_POINT('Ctrl Pts',(-26.7330214650367,22.9277716066589,-4.14708892265759));
#39641=CARTESIAN_POINT('Ctrl Pts',(-26.6429182559604,22.574072100136,-4.12760012635231));
#39642=CARTESIAN_POINT('Ctrl Pts',(-26.4875583442566,22.2240660387918,-4.10444298478342));
#39643=CARTESIAN_POINT('Ctrl Pts',(-26.4790811376852,22.2054480785495,-4.10319994645464));
#39644=CARTESIAN_POINT('Ctrl Pts',(-26.4677783248097,22.1812382796036,-4.1015684013831));
#39645=CARTESIAN_POINT('Ctrl Pts',(-26.4651127280699,22.1755719103747,-4.10118544138217));
#39646=CARTESIAN_POINT('Ctrl Pts',(-26.4609813743745,22.1668557642111,-4.10059466511295));
#39647=CARTESIAN_POINT('Ctrl Pts',(-26.4595272904305,22.1638004445542,-4.10038725469932));
#39648=CARTESIAN_POINT('Ctrl Pts',(-26.4566270511556,22.1577311168639,-4.09997459461927));
#39649=CARTESIAN_POINT('Ctrl Pts',(-26.4551810124597,22.1547170575343,-4.09976934920925));
#39650=CARTESIAN_POINT('Ctrl Pts',(-26.4519722757289,22.1480555052654,-4.0993150213823));
#39651=CARTESIAN_POINT('Ctrl Pts',(-26.4502073867011,22.1444090793393,-4.09906586277491));
#39652=CARTESIAN_POINT('Ctrl Pts',(-26.4451168713067,22.1339419727684,-4.09834930169176));
#39653=CARTESIAN_POINT('Ctrl Pts',(-26.4417740408908,22.1271297315254,-4.09788129837131));
#39654=CARTESIAN_POINT('Ctrl Pts',(-26.41961775824,22.082378534663,-4.09479592768817));
#39655=CARTESIAN_POINT('Ctrl Pts',(-26.400082885085,22.0448032448244,-4.09215331248392));
#39656=CARTESIAN_POINT('Ctrl Pts',(-26.3403090337582,21.9351631643943,-4.08428305681629));
#39657=CARTESIAN_POINT('Ctrl Pts',(-26.2980382631075,21.8642511767335,-4.07898433132942));
#39658=CARTESIAN_POINT('Ctrl Pts',(-26.0907800909265,21.5450945605374,-4.05415252330508));
#39659=CARTESIAN_POINT('Ctrl Pts',(-25.894612645465,21.3189139456743,-4.03352932944031));
#39660=CARTESIAN_POINT('Ctrl Pts',(-25.6023429951045,21.0636569134999,-4.00786187434773));
#39661=CARTESIAN_POINT('Ctrl Pts',(-25.5320287122559,21.0072622161041,-4.00201267575824));
#39662=CARTESIAN_POINT('Ctrl Pts',(-25.4542682034371,20.9500827228878,-3.99596179866068));
#39663=CARTESIAN_POINT('Ctrl Pts',(-25.4490887651295,20.9462979097507,-3.99556068299996));
#39664=CARTESIAN_POINT('Ctrl Pts',(-25.4418928488262,20.9410724662449,-3.99500609747454));
#39665=CARTESIAN_POINT('Ctrl Pts',(-25.4398860028496,20.9396186913926,-3.99485172025148));
#39666=CARTESIAN_POINT('Ctrl Pts',(-25.4364346787909,20.9371245900839,-3.9945867257879));
#39667=CARTESIAN_POINT('Ctrl Pts',(-25.4349910159461,20.9360831459684,-3.99447603052115));
#39668=CARTESIAN_POINT('Ctrl Pts',(-25.432008033712,20.933935007505,-3.99424761604955));
#39669=CARTESIAN_POINT('Ctrl Pts',(-25.4304686035824,20.9328284774414,-3.99412990876358));
#39670=CARTESIAN_POINT('Ctrl Pts',(-25.426853597266,20.9302348747746,-3.99385389814171));
#39671=CARTESIAN_POINT('Ctrl Pts',(-25.4247772231676,20.92874890533,-3.99369567191777));
#39672=CARTESIAN_POINT('Ctrl Pts',(-25.4180346489997,20.9239356488915,-3.99318285648074));
#39673=CARTESIAN_POINT('Ctrl Pts',(-25.4133613052385,20.9206183164923,-3.99282895481266));
#39674=CARTESIAN_POINT('Ctrl Pts',(-25.2855445550673,20.8304004894742,-3.98319078770374));
#39675=CARTESIAN_POINT('Ctrl Pts',(-25.1564449971852,20.7522187494271,-3.9744921697016));
#39676=CARTESIAN_POINT('Ctrl Pts',(-24.7151557101342,20.5256285403925,-3.94643849774397));
#39677=CARTESIAN_POINT('Ctrl Pts',(-24.384668685978,20.4183050047682,-3.9277304383771));
#39678=CARTESIAN_POINT('Ctrl Pts',(-24.0229605670322,20.3622917079563,-3.90559981502139));
#39679=CARTESIAN_POINT('Ctrl Pts',(-24.0024496603143,20.3593177429465,-3.90434059196153));
#39680=CARTESIAN_POINT('Ctrl Pts',(-23.9756744755184,20.3556988307987,-3.90269075525043));
#39681=CARTESIAN_POINT('Ctrl Pts',(-23.9694346691237,20.3548740700774,-3.90230584429812));
#39682=CARTESIAN_POINT('Ctrl Pts',(-23.9598303164005,20.3536332090516,-3.90171271876441));
#39683=CARTESIAN_POINT('Ctrl Pts',(-23.95646743828,20.3532041265015,-3.90150491527495));
#39684=CARTESIAN_POINT('Ctrl Pts',(-23.949819283781,20.352366521674,-3.90109385227066));
#39685=CARTESIAN_POINT('Ctrl Pts',(-23.9465340421302,20.3519577537207,-3.90089060079857));
#39686=CARTESIAN_POINT('Ctrl Pts',(-23.9393316361947,20.3510728581137,-3.90044473387189));
#39687=CARTESIAN_POINT('Ctrl Pts',(-23.9354142197083,20.3505988617989,-3.9002020513401));
#39688=CARTESIAN_POINT('Ctrl Pts',(-23.9243390675044,20.3492794336721,-3.89951545329457));
#39689=CARTESIAN_POINT('Ctrl Pts',(-23.9171793855118,20.34845082123,-3.89907100688035));
#39690=CARTESIAN_POINT('Ctrl Pts',(-23.9011557486698,20.3466508073824,-3.89807498506227));
#39691=CARTESIAN_POINT('Ctrl Pts',(-23.8922904462955,20.3456921658871,-3.89752300951158));
#39692=CARTESIAN_POINT('Ctrl Pts',(-23.7133926031724,20.3270980263835,-3.88636561931689));
#39693=CARTESIAN_POINT('Ctrl Pts',(-23.5422566705809,20.3229845631223,-3.87532777304698));
#39694=CARTESIAN_POINT('Ctrl Pts',(-23.0502725751672,20.3502957859667,-3.84259033391797));
#39695=CARTESIAN_POINT('Ctrl Pts',(-22.7334270007086,20.416167060159,-3.82011092006373));
#39696=CARTESIAN_POINT('Ctrl Pts',(-22.4165915220138,20.5334352597712,-3.79873398439484));
#39697=CARTESIAN_POINT('Ctrl Pts',(-22.4016224429598,20.5391028041678,-3.7977272553634));
#39698=CARTESIAN_POINT('Ctrl Pts',(-22.3833668039644,20.5461706412306,-3.79650400697162));
#39699=CARTESIAN_POINT('Ctrl Pts',(-22.3800398875701,20.5474650477008,-3.79628126576141));
#39700=CARTESIAN_POINT('Ctrl Pts',(-22.3745542427759,20.5496098540189,-3.79591430726386));
#39701=CARTESIAN_POINT('Ctrl Pts',(-22.3723942817149,20.5504570572196,-3.79576989812885));
#39702=CARTESIAN_POINT('Ctrl Pts',(-22.3684982173198,20.5519900703166,-3.79550956473558));
#39703=CARTESIAN_POINT('Ctrl Pts',(-22.3667617993054,20.5526750542541,-3.79539359087805));
#39704=CARTESIAN_POINT('Ctrl Pts',(-22.3630255631325,20.5541526810375,-3.7951441650494));
#39705=CARTESIAN_POINT('Ctrl Pts',(-22.3610259487391,20.5549458154391,-3.79501074376876));
#39706=CARTESIAN_POINT('Ctrl Pts',(-22.3555428367392,20.5571270133287,-3.79464507987255));
#39707=CARTESIAN_POINT('Ctrl Pts',(-22.352060951305,20.5585191610653,-3.79441308495365));
#39708=CARTESIAN_POINT('Ctrl Pts',(-22.3338662600028,20.5658307274141,-3.79320184258342));
#39709=CARTESIAN_POINT('Ctrl Pts',(-22.319194530257,20.5718527450191,-3.79222873446555));
#39710=CARTESIAN_POINT('Ctrl Pts',(-22.1722495732096,20.633437715581,-3.78251312207513));
#39711=CARTESIAN_POINT('Ctrl Pts',(-22.0437635840609,20.6976742278776,-3.77426476093259));
#39712=CARTESIAN_POINT('Ctrl Pts',(-21.6267526061687,20.9422241995619,-3.74696759628441));
#39713=CARTESIAN_POINT('Ctrl Pts',(-21.3626139583364,21.1594589909255,-3.72850667866777));
#39714=CARTESIAN_POINT('Ctrl Pts',(-21.1235919601499,21.4294358612213,-3.70670416997352));
#39715=CARTESIAN_POINT('Ctrl Pts',(-21.1100386460553,21.4450444563176,-3.70544818310043));
#39716=CARTESIAN_POINT('Ctrl Pts',(-21.0925600250056,21.4655691887136,-3.70380200237777));
#39717=CARTESIAN_POINT('Ctrl Pts',(-21.0884974217569,21.4703681897785,-3.70341747986854));
#39718=CARTESIAN_POINT('Ctrl Pts',(-21.0822668792514,21.4777719247301,-3.70282482207802));
#39719=CARTESIAN_POINT('Ctrl Pts',(-21.0800889449977,21.4803682591501,-3.70261709684376));
#39720=CARTESIAN_POINT('Ctrl Pts',(-21.0757914412457,21.485507793277,-3.70220610707547));
#39721=CARTESIAN_POINT('Ctrl Pts',(-21.0736716871212,21.4880508337198,-3.70200285044926));
#39722=CARTESIAN_POINT('Ctrl Pts',(-21.0690330794048,21.4936331760292,-3.70155689138208));
#39723=CARTESIAN_POINT('Ctrl Pts',(-21.066515886424,21.4966738452943,-3.7013141217089));
#39724=CARTESIAN_POINT('Ctrl Pts',(-21.0594289312271,21.5052666971676,-3.70062845468206));
#39725=CARTESIAN_POINT('Ctrl Pts',(-21.0548721775985,21.5108295350825,-3.70018503007203));
#39726=CARTESIAN_POINT('Ctrl Pts',(-21.0447124636344,21.5233174366792,-3.69919060342048));
#39727=CARTESIAN_POINT('Ctrl Pts',(-21.0391195368424,21.5302505535615,-3.69863920011983));
#39728=CARTESIAN_POINT('Ctrl Pts',(-20.9272495564966,21.6701096904999,-3.68752938780932));
#39729=CARTESIAN_POINT('Ctrl Pts',(-20.8316561569087,21.8112014951871,-3.67654249566736));
#39730=CARTESIAN_POINT('Ctrl Pts',(-20.5883397552585,22.2397855599911,-3.64380605066535));
#39731=CARTESIAN_POINT('Ctrl Pts',(-20.4720815894401,22.5427275385657,-3.62126333245579));
#39732=CARTESIAN_POINT('Ctrl Pts',(-20.3993304900804,22.8734496917229,-3.59983763236267));
#39733=CARTESIAN_POINT('Ctrl Pts',(-20.3960204589618,22.8890476822934,-3.59883475592369));
#39734=CARTESIAN_POINT('Ctrl Pts',(-20.3921121155843,22.9081626753874,-3.59761561700886));
#39735=CARTESIAN_POINT('Ctrl Pts',(-20.3914037730136,22.9116565784314,-3.59739318103359));
#39736=CARTESIAN_POINT('Ctrl Pts',(-20.3902442949107,22.9174248441887,-3.59702662196992));
#39737=CARTESIAN_POINT('Ctrl Pts',(-20.3897898163113,22.9196985186562,-3.59688230775134));
#39738=CARTESIAN_POINT('Ctrl Pts',(-20.3889739068327,22.9238034097067,-3.5966220761213));
#39739=CARTESIAN_POINT('Ctrl Pts',(-20.3886116140037,22.9256344451101,-3.59650610929064));
#39740=CARTESIAN_POINT('Ctrl Pts',(-20.3878349876222,22.9295775187021,-3.59625662125887));
#39741=CARTESIAN_POINT('Ctrl Pts',(-20.3874211801551,22.9316896516296,-3.59612313088746));
#39742=CARTESIAN_POINT('Ctrl Pts',(-20.3862912455956,22.9374877792008,-3.59575708575434));
#39743=CARTESIAN_POINT('Ctrl Pts',(-20.3855794412158,22.9411746281617,-3.5955247795546));
#39744=CARTESIAN_POINT('Ctrl Pts',(-20.3818827416378,22.9605034197248,-3.59430920405122));
#39745=CARTESIAN_POINT('Ctrl Pts',(-20.3790072989027,22.9761664408064,-3.5933321265163));
#39746=CARTESIAN_POINT('Ctrl Pts',(-20.3446353925671,23.1715392765327,-3.58123631951792));
#39747=CARTESIAN_POINT('Ctrl Pts',(-20.3283338742798,23.3536172110083,-3.57092003762428));
#39748=CARTESIAN_POINT('Ctrl Pts',(-20.3264155662258,23.7910437246479,-3.546414951305));
#39749=CARTESIAN_POINT('Ctrl Pts',(-20.3555465001149,24.0451730283263,-3.53233784307375));
#39750=CARTESIAN_POINT('Ctrl Pts',(-20.4152279643893,24.2970820721114,-3.51701193552946));
#39751=CARTESIAN_POINT('Ctrl Pts',(-20.4161525807257,24.3009528028979,-3.51677612997515));
#39752=CARTESIAN_POINT('Ctrl Pts',(-20.4194497917377,24.3146436819744,-3.51594095560996));
#39753=CARTESIAN_POINT('Ctrl Pts',(-20.4218613740993,24.3244543070197,-3.51534043769612));
#39754=CARTESIAN_POINT('Ctrl Pts',(-20.4256159599233,24.3394244260853,-3.51442088676505));
#39755=CARTESIAN_POINT('Ctrl Pts',(-20.4269257166613,24.3445922515533,-3.51410286240769));
#39756=CARTESIAN_POINT('Ctrl Pts',(-20.4287787146652,24.3518280700543,-3.51365674188052));
#39757=CARTESIAN_POINT('Ctrl Pts',(-20.429311204817,24.3538988271829,-3.51352897472617));
#39758=CARTESIAN_POINT('Ctrl Pts',(-20.4315377732023,24.362521958183,-3.51299652069353));
#39759=CARTESIAN_POINT('Ctrl Pts',(-20.433250420032,24.369069483708,-3.51259126493477));
#39760=CARTESIAN_POINT('Ctrl Pts',(-20.436820080891,24.382542958108,-3.5117553123687));
#39761=CARTESIAN_POINT('Ctrl Pts',(-20.4386796100524,24.3894681962741,-3.51132453939361));
#39762=CARTESIAN_POINT('Ctrl Pts',(-20.4482211809661,24.4245351119534,-3.50913758772434));
#39763=CARTESIAN_POINT('Ctrl Pts',(-20.456261761692,24.452577063105,-3.50737019098676));
#39764=CARTESIAN_POINT('Ctrl Pts',(-20.4665415219874,24.4866741701049,-3.50519719693621));
#39765=CARTESIAN_POINT('Ctrl Pts',(-20.4684198248075,24.4928374043096,-3.50480345615348));
#39766=CARTESIAN_POINT('Ctrl Pts',(-20.4715469573693,24.5029891251625,-3.50415330900261));
#39767=CARTESIAN_POINT('Ctrl Pts',(-20.4727850920539,24.5069809088238,-3.50389725422928));
#39768=CARTESIAN_POINT('Ctrl Pts',(-20.4750300715203,24.5141693409945,-3.50343540763567));
#39769=CARTESIAN_POINT('Ctrl Pts',(-20.4760341461147,24.5173668540156,-3.50322970722053));
#39770=CARTESIAN_POINT('Ctrl Pts',(-20.4781629643227,24.5241093407096,-3.50279539247604));
#39771=CARTESIAN_POINT('Ctrl Pts',(-20.4792888596168,24.5276539430982,-3.50256674045236));
#39772=CARTESIAN_POINT('Ctrl Pts',(-20.4821900936578,24.5367332581924,-3.50198021557083));
#39773=CARTESIAN_POINT('Ctrl Pts',(-20.4839742691022,24.5422651138169,-3.50162205160463));
#39774=CARTESIAN_POINT('Ctrl Pts',(-20.4879801556456,24.5545713484214,-3.5008234680341));
#39775=CARTESIAN_POINT('Ctrl Pts',(-20.4902093957214,24.5613432276342,-3.50038280070358));
#39776=CARTESIAN_POINT('Ctrl Pts',(-20.4968278079865,24.5812259446431,-3.49908534428002));
#39777=CARTESIAN_POINT('Ctrl Pts',(-20.5012788601949,24.5943158738596,-3.49822650917489));
#39778=CARTESIAN_POINT('Ctrl Pts',(-20.516897735719,24.6392970723253,-3.49525902731987));
#39779=CARTESIAN_POINT('Ctrl Pts',(-20.5284825005611,24.6710402317541,-3.49313660688906));
#39780=CARTESIAN_POINT('Ctrl Pts',(-20.5827162007208,24.8126879077974,-3.48353531152221));
#39781=CARTESIAN_POINT('Ctrl Pts',(-20.6308727650596,24.9203734392677,-3.47587559667729));
#39782=CARTESIAN_POINT('Ctrl Pts',(-20.8286714649276,25.3046525981251,-3.44723972970496));
#39783=CARTESIAN_POINT('Ctrl Pts',(-21.0126263332655,25.561560694453,-3.42531753112927));
#39784=CARTESIAN_POINT('Ctrl Pts',(-21.2339531419561,25.790987839493,-3.40490572696321));
#39785=CARTESIAN_POINT('Ctrl Pts',(-21.2370663655839,25.7942015827925,-3.40461965517891));
#39786=CARTESIAN_POINT('Ctrl Pts',(-21.2438387697025,25.8011635827133,-3.40399962691574));
#39787=CARTESIAN_POINT('Ctrl Pts',(-21.2475004250445,25.8049094318148,-3.40366583269406));
#39788=CARTESIAN_POINT('Ctrl Pts',(-21.2572754629531,25.814860577897,-3.4027786076108));
#39789=CARTESIAN_POINT('Ctrl Pts',(-21.2634049492402,25.8210500962439,-3.4022262684138));
#39790=CARTESIAN_POINT('Ctrl Pts',(-21.270674587486,25.8283316456735,-3.4015759771239));
#39791=CARTESIAN_POINT('Ctrl Pts',(-21.2717904645627,25.8294477102464,-3.40147629106471));
#39792=CARTESIAN_POINT('Ctrl Pts',(-21.2823384999536,25.8399820301659,-3.40053524515658));
#39793=CARTESIAN_POINT('Ctrl Pts',(-21.2918283779793,25.849342696996,-3.39969807371846));
#39794=CARTESIAN_POINT('Ctrl Pts',(-21.3039984438396,25.8611989908464,-3.39863679023316));
#39795=CARTESIAN_POINT('Ctrl Pts',(-21.3066249994441,25.863749119355,-3.39840846800066));
#39796=CARTESIAN_POINT('Ctrl Pts',(-21.3108030025703,25.8677917446093,-3.39804643896065));
#39797=CARTESIAN_POINT('Ctrl Pts',(-21.3123516000185,25.8692871620874,-3.39791250285376));
#39798=CARTESIAN_POINT('Ctrl Pts',(-21.3152456604843,25.8720762398894,-3.3976626710656));
#39799=CARTESIAN_POINT('Ctrl Pts',(-21.3165907400274,25.8733702744633,-3.39754674606989));
#39800=CARTESIAN_POINT('Ctrl Pts',(-21.3196088053085,25.8762687615408,-3.39728706029532));
#39801=CARTESIAN_POINT('Ctrl Pts',(-21.3212823946222,25.8778725745053,-3.39714334997494));
#39802=CARTESIAN_POINT('Ctrl Pts',(-21.3262279120883,25.882601675097,-3.39671953549956));
#39803=CARTESIAN_POINT('Ctrl Pts',(-21.3295047106563,25.885721895932,-3.3964398268374));
#39804=CARTESIAN_POINT('Ctrl Pts',(-21.3549189839264,25.9098199307345,-3.39427886627923));
#39805=CARTESIAN_POINT('Ctrl Pts',(-21.3773476225397,25.9304903595793,-3.39242103874771));
#39806=CARTESIAN_POINT('Ctrl Pts',(-21.4557033991246,26.0006729390814,-3.38608421457666));
#39807=CARTESIAN_POINT('Ctrl Pts',(-21.5130595459458,26.0485605045044,-3.38170916989849));
#39808=CARTESIAN_POINT('Ctrl Pts',(-21.6789319459723,26.1775350233767,-3.36961023167016));
#39809=CARTESIAN_POINT('Ctrl Pts',(-21.7909699180333,26.2538395365431,-3.36206294142898));
#39810=CARTESIAN_POINT('Ctrl Pts',(-21.96242393445,26.3554256659843,-3.35092737772661));
#39811=CARTESIAN_POINT('Ctrl Pts',(-22.0183009156529,26.3863262187569,-3.34735930310875));
#39812=CARTESIAN_POINT('Ctrl Pts',(-22.0750361667496,26.4155368525077,-3.34376876818698));
#39813=CARTESIAN_POINT('Origin',(-23.5502525316942,23.5502525316942,-77.3107734492734));
#39814=CARTESIAN_POINT('',(-22.0750359636318,26.4155367479307,-1.84841977781535));
#39815=CARTESIAN_POINT('',(-22.0750363389647,26.4155369411741,-2.09574775951102));
#39816=CARTESIAN_POINT('',(-22.0750360153461,26.4155367745563,-77.3107734492734));
#39817=CARTESIAN_POINT('Ctrl Pts',(-22.0750359636318,26.4155367479307,-1.84841977781534));
#39818=CARTESIAN_POINT('Ctrl Pts',(-22.0147494710243,26.3844977214282,-1.85229280629613));
#39819=CARTESIAN_POINT('Ctrl Pts',(-21.9554363723595,26.3515528266262,-1.85611401846149));
#39820=CARTESIAN_POINT('Ctrl Pts',(-21.7891319966047,26.2521808848818,-1.86697516491533));
#39821=CARTESIAN_POINT('Ctrl Pts',(-21.6849533142671,26.1813399344116,-1.87396327472071));
#39822=CARTESIAN_POINT('Ctrl Pts',(-21.431080192038,25.9860336499376,-1.89203649308758));
#39823=CARTESIAN_POINT('Ctrl Pts',(-21.288044137719,25.8537969097466,-1.9032641130977));
#39824=CARTESIAN_POINT('Ctrl Pts',(-21.1511518557094,25.7021196591162,-1.91570441433683));
#39825=CARTESIAN_POINT('Ctrl Pts',(-21.1445322562156,25.6947166000034,-1.91631051088979));
#39826=CARTESIAN_POINT('Ctrl Pts',(-21.134949831241,25.683899844989,-1.91719456263574));
#39827=CARTESIAN_POINT('Ctrl Pts',(-21.1319597578092,25.6805102747366,-1.91747137504461));
#39828=CARTESIAN_POINT('Ctrl Pts',(-21.1267362191044,25.674563660496,-1.91795663752941));
#39829=CARTESIAN_POINT('Ctrl Pts',(-21.1244996402559,25.6720093506712,-1.91816495721126));
#39830=CARTESIAN_POINT('Ctrl Pts',(-21.120173268853,25.6670525878746,-1.91856898180749));
#39831=CARTESIAN_POINT('Ctrl Pts',(-21.1180829913787,25.6646505615306,-1.91876466621032));
#39832=CARTESIAN_POINT('Ctrl Pts',(-21.1131147864482,25.6589242715424,-1.91923092094093));
#39833=CARTESIAN_POINT('Ctrl Pts',(-21.1102401007902,25.6555972142755,-1.91950162538642));
#39834=CARTESIAN_POINT('Ctrl Pts',(-21.100053254489,25.6437584384739,-1.92046419478591));
#39835=CARTESIAN_POINT('Ctrl Pts',(-21.0927788153043,25.6352144996606,-1.92115761539434));
#39836=CARTESIAN_POINT('Ctrl Pts',(-20.98748006118,25.5102228551447,-1.93128419140052));
#39837=CARTESIAN_POINT('Ctrl Pts',(-20.8977963235191,25.3870296474176,-1.94105711520603));
#39838=CARTESIAN_POINT('Ctrl Pts',(-20.6899568360752,25.0543974038987,-1.96694913272589));
#39839=CARTESIAN_POINT('Ctrl Pts',(-20.5859015751572,24.8372451535808,-1.98343988181253));
#39840=CARTESIAN_POINT('Ctrl Pts',(-20.4925954809956,24.5694431279525,-2.00236342484556));
#39841=CARTESIAN_POINT('Ctrl Pts',(-20.4790948647286,24.5280086250873,-2.00525107353723));
#39842=CARTESIAN_POINT('Ctrl Pts',(-20.451792775599,24.4380628359811,-2.01141648684609));
#39843=CARTESIAN_POINT('Ctrl Pts',(-20.4382807966536,24.3894739220751,-2.01468348435445));
#39844=CARTESIAN_POINT('Ctrl Pts',(-20.4220161424861,24.3251765732929,-2.01890624316303));
#39845=CARTESIAN_POINT('Ctrl Pts',(-20.4182323544617,24.3097390754593,-2.01991256150456));
#39846=CARTESIAN_POINT('Ctrl Pts',(-20.4130052999681,24.2877095713463,-2.02133724389597));
#39847=CARTESIAN_POINT('Ctrl Pts',(-20.4114683575524,24.2811403400346,-2.02176065372164));
#39848=CARTESIAN_POINT('Ctrl Pts',(-20.4091436878043,24.2710616113708,-2.02240801681774));
#39849=CARTESIAN_POINT('Ctrl Pts',(-20.4083411991506,24.26755558985,-2.02263279473431));
#39850=CARTESIAN_POINT('Ctrl Pts',(-20.4070301156251,24.2617831359981,-2.02300218520011));
#39851=CARTESIAN_POINT('Ctrl Pts',(-20.4065181013511,24.2595174957921,-2.02314699237782));
#39852=CARTESIAN_POINT('Ctrl Pts',(-20.4055579057269,24.2552472063919,-2.02341959239409));
#39853=CARTESIAN_POINT('Ctrl Pts',(-20.405109191057,24.2532426801614,-2.02354741591625));
#39854=CARTESIAN_POINT('Ctrl Pts',(-20.4042649330627,24.2494541698359,-2.02378873653539));
#39855=CARTESIAN_POINT('Ctrl Pts',(-20.4038689918767,24.2476702845046,-2.02390225621014));
#39856=CARTESIAN_POINT('Ctrl Pts',(-20.4030655257328,24.2440357132869,-2.0241333218128));
#39857=CARTESIAN_POINT('Ctrl Pts',(-20.4026581174377,24.2421850117388,-2.02425086064171));
#39858=CARTESIAN_POINT('Ctrl Pts',(-20.4014934609144,24.2368721038966,-2.02458794877002));
#39859=CARTESIAN_POINT('Ctrl Pts',(-20.4007402880225,24.2334089925422,-2.02480726241004));
#39860=CARTESIAN_POINT('Ctrl Pts',(-20.3974867472199,24.21832937255,-2.02576047410109));
#39861=CARTESIAN_POINT('Ctrl Pts',(-20.395044882047,24.2067001343429,-2.02649104213994));
#39862=CARTESIAN_POINT('Ctrl Pts',(-20.3918912978707,24.1912571523086,-2.02745550344502));
#39863=CARTESIAN_POINT('Ctrl Pts',(-20.3911221039985,24.1874554413979,-2.02769247516465));
#39864=CARTESIAN_POINT('Ctrl Pts',(-20.3235565072747,23.8503854879869,-2.04866330793441));
#39865=CARTESIAN_POINT('Ctrl Pts',(-20.3098811304207,23.5085855880593,-2.06666543409453));
#39866=CARTESIAN_POINT('Ctrl Pts',(-20.3613807979946,23.0741031048338,-2.09159407772048));
#39867=CARTESIAN_POINT('Ctrl Pts',(-20.3772414981934,22.9778716755029,-2.09723151325793));
#39868=CARTESIAN_POINT('Ctrl Pts',(-20.4105758942607,22.8204793688928,-2.10675239907097));
#39869=CARTESIAN_POINT('Ctrl Pts',(-20.4255411068997,22.7588512948536,-2.11055760018341));
#39870=CARTESIAN_POINT('Ctrl Pts',(-20.4445337607476,22.689613862309,-2.11493398504481));
#39871=CARTESIAN_POINT('Ctrl Pts',(-20.4467856102481,22.6815287154898,-2.11544660748937));
#39872=CARTESIAN_POINT('Ctrl Pts',(-20.4502169249906,22.6693923826968,-2.11621848540238));
#39873=CARTESIAN_POINT('Ctrl Pts',(-20.4513728178548,22.6653345220406,-2.1164769714898));
#39874=CARTESIAN_POINT('Ctrl Pts',(-20.4533750193501,22.6583576539857,-2.11692209784983));
#39875=CARTESIAN_POINT('Ctrl Pts',(-20.4542174965111,22.6554375451413,-2.11710861271907));
#39876=CARTESIAN_POINT('Ctrl Pts',(-20.4559615280675,22.6494245090397,-2.11749311752306));
#39877=CARTESIAN_POINT('Ctrl Pts',(-20.4568635919321,22.646331733861,-2.11769112396119));
#39878=CARTESIAN_POINT('Ctrl Pts',(-20.459047229259,22.6388865643088,-2.11816835715027));
#39879=CARTESIAN_POINT('Ctrl Pts',(-20.4603333569777,22.634535522076,-2.11844773281111));
#39880=CARTESIAN_POINT('Ctrl Pts',(-20.4643113746801,22.6211814695238,-2.11930665046801));
#39881=CARTESIAN_POINT('Ctrl Pts',(-20.4670334380588,22.6121875655245,-2.11988718087699));
#39882=CARTESIAN_POINT('Ctrl Pts',(-20.499430669127,22.5068091344996,-2.12671343279464));
#39883=CARTESIAN_POINT('Ctrl Pts',(-20.533571918748,22.4118665830744,-2.13310607655239));
#39884=CARTESIAN_POINT('Ctrl Pts',(-20.6829344098437,22.050680663392,-2.1584179011844));
#39885=CARTESIAN_POINT('Ctrl Pts',(-20.8294304198555,21.7988796130966,-2.17837549436561));
#39886=CARTESIAN_POINT('Ctrl Pts',(-21.0346001927308,21.5354210626815,-2.20067816442014));
#39887=CARTESIAN_POINT('Ctrl Pts',(-21.0623363300044,21.5012708833047,-2.20359658498709));
#39888=CARTESIAN_POINT('Ctrl Pts',(-21.1346569859304,21.4158604723975,-2.21094631091168));
#39889=CARTESIAN_POINT('Ctrl Pts',(-21.1801818715847,21.3654189108885,-2.21533534267922));
#39890=CARTESIAN_POINT('Ctrl Pts',(-21.2323016317085,21.3112183946938,-2.22007052553823));
#39891=CARTESIAN_POINT('Ctrl Pts',(-21.2373501413318,21.3060037093855,-2.22052630197605));
#39892=CARTESIAN_POINT('Ctrl Pts',(-21.2450631522409,21.2980904887591,-2.2212181790071));
#39893=CARTESIAN_POINT('Ctrl Pts',(-21.2477148300794,21.2953795694694,-2.22145524646465));
#39894=CARTESIAN_POINT('Ctrl Pts',(-21.2520559274166,21.2909571296145,-2.22184204634748));
#39895=CARTESIAN_POINT('Ctrl Pts',(-21.2537424791541,21.2892428182157,-2.22199200033308));
#39896=CARTESIAN_POINT('Ctrl Pts',(-21.2569957405921,21.2859434053518,-2.22228063237449));
#39897=CARTESIAN_POINT('Ctrl Pts',(-21.2585621779397,21.2843580389708,-2.22241933167617));
#39898=CARTESIAN_POINT('Ctrl Pts',(-21.2614162990792,21.2814754153301,-2.22267154358612));
#39899=CARTESIAN_POINT('Ctrl Pts',(-21.2627034375136,21.2801776330993,-2.22278509850839));
#39900=CARTESIAN_POINT('Ctrl Pts',(-21.2653228527705,21.277541047108,-2.22301581170385));
#39901=CARTESIAN_POINT('Ctrl Pts',(-21.2666551973533,21.2762023245896,-2.22313296356487));
#39902=CARTESIAN_POINT('Ctrl Pts',(-21.2704689601419,21.2723770369018,-2.22346773970981));
#39903=CARTESIAN_POINT('Ctrl Pts',(-21.272953277985,21.2698933467783,-2.22368513346133));
#39904=CARTESIAN_POINT('Ctrl Pts',(-21.2836705569123,21.2592137568224,-2.22462005712921));
#39905=CARTESIAN_POINT('Ctrl Pts',(-21.2919438729133,21.2510582102517,-2.22533441216096));
#39906=CARTESIAN_POINT('Ctrl Pts',(-21.4337118112802,21.1128118098934,-2.23745419650848));
#39907=CARTESIAN_POINT('Ctrl Pts',(-21.578223806049,20.9944773510963,-2.24799918387846));
#39908=CARTESIAN_POINT('Ctrl Pts',(-21.8704444700303,20.7948207535242,-2.26782783903187));
#39909=CARTESIAN_POINT('Ctrl Pts',(-22.0158580193115,20.711275460077,-2.2771040514605));
#39910=CARTESIAN_POINT('Ctrl Pts',(-22.2608480388759,20.5948631976761,-2.29260916806692));
#39911=CARTESIAN_POINT('Ctrl Pts',(-22.3566830066463,20.554876284831,-2.29864281321902));
#39912=CARTESIAN_POINT('Ctrl Pts',(-22.4992202695564,20.5033306253284,-2.30768024299628));
#39913=CARTESIAN_POINT('Ctrl Pts',(-22.5445206006651,20.488079311462,-2.31056103798599));
#39914=CARTESIAN_POINT('Ctrl Pts',(-22.5976242230304,20.4715063077072,-2.31395350221476));
#39915=CARTESIAN_POINT('Ctrl Pts',(-22.6051153311819,20.4691983814596,-2.31443241370109));
#39916=CARTESIAN_POINT('Ctrl Pts',(-22.6165413100471,20.4657237571691,-2.31516344317922));
#39917=CARTESIAN_POINT('Ctrl Pts',(-22.6204701500044,20.4645371966779,-2.3154149092318));
#39918=CARTESIAN_POINT('Ctrl Pts',(-22.6276057801377,20.4623970092866,-2.31587181281953));
#39919=CARTESIAN_POINT('Ctrl Pts',(-22.630811813879,20.4614408634777,-2.31607716748746));
#39920=CARTESIAN_POINT('Ctrl Pts',(-22.6377095436108,20.4593954219885,-2.31651913388153));
#39921=CARTESIAN_POINT('Ctrl Pts',(-22.6414017107691,20.4583077451857,-2.31675579823457));
#39922=CARTESIAN_POINT('Ctrl Pts',(-22.6513284088281,20.4554027524761,-2.31739234113963));
#39923=CARTESIAN_POINT('Ctrl Pts',(-22.6575664746471,20.4535976692398,-2.31779261888205));
#39924=CARTESIAN_POINT('Ctrl Pts',(-22.6860906322902,20.4454371045188,-2.31962417754935));
#39925=CARTESIAN_POINT('Ctrl Pts',(-22.7084389705096,20.4393033986791,-2.32106267069402));
#39926=CARTESIAN_POINT('Ctrl Pts',(-22.7441404480199,20.4299176642449,-2.32336668488871));
#39927=CARTESIAN_POINT('Ctrl Pts',(-22.7574518789417,20.4265090255754,-2.32422706871126));
#39928=CARTESIAN_POINT('Ctrl Pts',(-22.7746922098383,20.4222116163076,-2.32534316680685));
#39929=CARTESIAN_POINT('Ctrl Pts',(-22.7786016904003,20.4212448998623,-2.32559637461803));
#39930=CARTESIAN_POINT('Ctrl Pts',(-22.8719335985539,20.3983518153624,-2.33164408398727));
#39931=CARTESIAN_POINT('Ctrl Pts',(-22.9622451083185,20.380262111649,-2.3375597882004));
#39932=CARTESIAN_POINT('Ctrl Pts',(-23.2535104046101,20.3347955608054,-2.35684083989997));
#39933=CARTESIAN_POINT('Ctrl Pts',(-23.4563070529969,20.3225013816433,-2.37060292748258));
#39934=CARTESIAN_POINT('Ctrl Pts',(-23.8323688226921,20.3351852175872,-2.39603546999539));
#39935=CARTESIAN_POINT('Ctrl Pts',(-24.0051180095531,20.3550434753913,-2.40766911660469));
#39936=CARTESIAN_POINT('Ctrl Pts',(-24.182300219831,20.3900813168716,-2.41903825277547));
#39937=CARTESIAN_POINT('Ctrl Pts',(-24.1891505841266,20.3914591437376,-2.41947690417789));
#39938=CARTESIAN_POINT('Ctrl Pts',(-24.1996107846104,20.3935984436739,-2.42014525489775));
#39939=CARTESIAN_POINT('Ctrl Pts',(-24.2032238314059,20.3943438425652,-2.42037584445405));
#39940=CARTESIAN_POINT('Ctrl Pts',(-24.2091476753078,20.3955765848886,-2.42075346881158));
#39941=CARTESIAN_POINT('Ctrl Pts',(-24.2114592183555,20.3960602646897,-2.42090071078288));
#39942=CARTESIAN_POINT('Ctrl Pts',(-24.2159194783303,20.3969986722074,-2.42118460620677));
#39943=CARTESIAN_POINT('Ctrl Pts',(-24.2180682651042,20.3974530562293,-2.42132127928002));
#39944=CARTESIAN_POINT('Ctrl Pts',(-24.2220033838607,20.3982893828075,-2.42157139146125));
#39945=CARTESIAN_POINT('Ctrl Pts',(-24.2237898478976,20.3986706458708,-2.42168486909836));
#39946=CARTESIAN_POINT('Ctrl Pts',(-24.2274425893842,20.3994534532963,-2.4219167547322));
#39947=CARTESIAN_POINT('Ctrl Pts',(-24.2293088271958,20.3998551354513,-2.42203515415357));
#39948=CARTESIAN_POINT('Ctrl Pts',(-24.2347065620429,20.401021943173,-2.42237738979209));
#39949=CARTESIAN_POINT('Ctrl Pts',(-24.2382371450628,20.4017913533707,-2.42260097875961));
#39950=CARTESIAN_POINT('Ctrl Pts',(-24.2539674364746,20.4052471351741,-2.42359602486919));
#39951=CARTESIAN_POINT('Ctrl Pts',(-24.2661529730728,20.4079985347341,-2.42436378219493));
#39952=CARTESIAN_POINT('Ctrl Pts',(-24.2809707024383,20.4114349345807,-2.42529399432965));
#39953=CARTESIAN_POINT('Ctrl Pts',(-24.2836182002076,20.4120524505353,-2.42546006426578));
#39954=CARTESIAN_POINT('Ctrl Pts',(-24.6186463471903,20.4906432530917,-2.44645907733329));
#39955=CARTESIAN_POINT('Ctrl Pts',(-24.9365912207545,20.6209460095237,-2.46453112471705));
#39956=CARTESIAN_POINT('Ctrl Pts',(-25.3094915595013,20.8483526109719,-2.48942519613442));
#39957=CARTESIAN_POINT('Ctrl Pts',(-25.3885475015473,20.9015066867624,-2.49493227117917));
#39958=CARTESIAN_POINT('Ctrl Pts',(-25.5170412457105,20.996426968454,-2.5043811475226));
#39959=CARTESIAN_POINT('Ctrl Pts',(-25.5677856147155,21.0363228954142,-2.50825295102506));
#39960=CARTESIAN_POINT('Ctrl Pts',(-25.6237599961517,21.0831174822532,-2.51270010475568));
#39961=CARTESIAN_POINT('Ctrl Pts',(-25.6302031545065,21.0885470330856,-2.51321472964418));
#39962=CARTESIAN_POINT('Ctrl Pts',(-25.6398458023128,21.0967376274924,-2.51398902745751));
#39963=CARTESIAN_POINT('Ctrl Pts',(-25.6430613093975,21.0994798287585,-2.51424792373933));
#39964=CARTESIAN_POINT('Ctrl Pts',(-25.6485807468954,21.104205617486,-2.51469351916355));
#39965=CARTESIAN_POINT('Ctrl Pts',(-25.6508872869714,21.1061861598389,-2.5148800921569));
#39966=CARTESIAN_POINT('Ctrl Pts',(-25.6556303148301,21.1102704999486,-2.51526449607886));
#39967=CARTESIAN_POINT('Ctrl Pts',(-25.658066459394,21.1123746899984,-2.51546234318443));
#39968=CARTESIAN_POINT('Ctrl Pts',(-25.6639214649186,21.1174472162411,-2.51593883032677));
#39969=CARTESIAN_POINT('Ctrl Pts',(-25.6673372245128,21.1204191083331,-2.51621761825719));
#39970=CARTESIAN_POINT('Ctrl Pts',(-25.6777936842519,21.1295555700323,-2.51707355044855));
#39971=CARTESIAN_POINT('Ctrl Pts',(-25.6848137586981,21.1357435751503,-2.51765167376828));
#39972=CARTESIAN_POINT('Ctrl Pts',(-25.7659289690192,21.2078746646212,-2.52437255498367));
#39973=CARTESIAN_POINT('Ctrl Pts',(-25.8369612907692,21.2771674689656,-2.53065737607574));
#39974=CARTESIAN_POINT('Ctrl Pts',(-26.1037372978666,21.5625874765751,-2.55594096521853));
#39975=CARTESIAN_POINT('Ctrl Pts',(-26.2729617071288,21.8015669520083,-2.5760008784623));
#39976=CARTESIAN_POINT('Ctrl Pts',(-26.4280808220543,22.0989911635446,-2.59840672463539));
#39977=CARTESIAN_POINT('Ctrl Pts',(-26.4476353990424,22.1384352522685,-2.60132742165609));
#39978=CARTESIAN_POINT('Ctrl Pts',(-26.4953716663972,22.2398977403806,-2.60869198233823));
#39979=CARTESIAN_POINT('Ctrl Pts',(-26.5224085178665,22.3024357249117,-2.6130932923653));
#39980=CARTESIAN_POINT('Ctrl Pts',(-26.5514753314337,22.3759870090907,-2.61807366895531));
#39981=CARTESIAN_POINT('Ctrl Pts',(-26.5554536057793,22.3862060017614,-2.6187613018492));
#39982=CARTESIAN_POINT('Ctrl Pts',(-26.5605599486011,22.3995233343494,-2.61965161921877));
#39983=CARTESIAN_POINT('Ctrl Pts',(-26.5617354694051,22.4026032185262,-2.61985711955954));
#39984=CARTESIAN_POINT('Ctrl Pts',(-26.5636342496168,22.4076010598323,-2.62018993402235));
#39985=CARTESIAN_POINT('Ctrl Pts',(-26.5643604047698,22.4095179027913,-2.62031742285892));
#39986=CARTESIAN_POINT('Ctrl Pts',(-26.5657514575433,22.4132004877643,-2.6205620478331));
#39987=CARTESIAN_POINT('Ctrl Pts',(-26.5664166313607,22.4149661157185,-2.6206792002514));
#39988=CARTESIAN_POINT('Ctrl Pts',(-26.5679432483283,22.419029157905,-2.62094848388521));
#39989=CARTESIAN_POINT('Ctrl Pts',(-26.5688036207641,22.4213269781532,-2.62110055018736));
#39990=CARTESIAN_POINT('Ctrl Pts',(-26.5714610080558,22.4284488920648,-2.6215711780463));
#39991=CARTESIAN_POINT('Ctrl Pts',(-26.5732491002714,22.4332763409159,-2.62188920425452));
#39992=CARTESIAN_POINT('Ctrl Pts',(-26.5878355494606,22.4729480756384,-2.62449485293776));
#39993=CARTESIAN_POINT('Ctrl Pts',(-26.6000432457672,22.5080086201089,-2.62674781694578));
#39994=CARTESIAN_POINT('Ctrl Pts',(-26.7182993195313,22.8675277574703,-2.64942044096342));
#39995=CARTESIAN_POINT('Ctrl Pts',(-26.7727812658795,23.2067101508008,-2.66747027613089));
#39996=CARTESIAN_POINT('Ctrl Pts',(-26.7730375089227,23.6033534261096,-2.69026412956738));
#39997=CARTESIAN_POINT('Ctrl Pts',(-26.7716558194149,23.6585259170155,-2.69346620726019));
#39998=CARTESIAN_POINT('Ctrl Pts',(-26.768433196616,23.7220114806858,-2.69720044260653));
#39999=CARTESIAN_POINT('Ctrl Pts',(-26.7679752288546,23.7303874007087,-2.69769410891723));
#40000=CARTESIAN_POINT('Ctrl Pts',(-26.7633890991607,23.8086576948525,-2.70231687388276));
#40001=CARTESIAN_POINT('Ctrl Pts',(-26.7570171911784,23.8783974946396,-2.70650808168359));
#40002=CARTESIAN_POINT('Ctrl Pts',(-26.7472251429439,23.9571570088781,-2.71134202467801));
#40003=CARTESIAN_POINT('Ctrl Pts',(-26.7460301619426,23.9664381462107,-2.71191324542094));
#40004=CARTESIAN_POINT('Ctrl Pts',(-26.744209844536,23.9801058530803,-2.71275681846786));
#40005=CARTESIAN_POINT('Ctrl Pts',(-26.743615849142,23.9844966066453,-2.71302817796419));
#40006=CARTESIAN_POINT('Ctrl Pts',(-26.7425509698524,23.9922477331081,-2.71350786046206));
#40007=CARTESIAN_POINT('Ctrl Pts',(-26.7420838289907,23.995608620458,-2.71371606454762));
#40008=CARTESIAN_POINT('Ctrl Pts',(-26.741106514098,24.0025594779948,-2.71414710919673));
#40009=CARTESIAN_POINT('Ctrl Pts',(-26.7405955875958,24.0061493360075,-2.71436997334935));
#40010=CARTESIAN_POINT('Ctrl Pts',(-26.7392709848073,24.0153449470342,-2.71494148511913));
#40011=CARTESIAN_POINT('Ctrl Pts',(-26.7384485880384,24.0209494137298,-2.71529040901676));
#40012=CARTESIAN_POINT('Ctrl Pts',(-26.7350247798169,24.043861287917,-2.7167193516256));
#40013=CARTESIAN_POINT('Ctrl Pts',(-26.7322972153144,24.0611492811752,-2.71780336947734));
#40014=CARTESIAN_POINT('Ctrl Pts',(-26.7134677529929,24.1744899833767,-2.72494938209993));
#40015=CARTESIAN_POINT('Ctrl Pts',(-26.6931611394368,24.269783717082,-2.73114481910676));
#40016=CARTESIAN_POINT('Ctrl Pts',(-26.6316782401347,24.5053879987416,-2.74695124763146));
#40017=CARTESIAN_POINT('Ctrl Pts',(-26.5852141185865,24.6440844777718,-2.75670789053095));
#40018=CARTESIAN_POINT('Ctrl Pts',(-26.4358911206073,25.006096566825,-2.783146228409));
#40019=CARTESIAN_POINT('Ctrl Pts',(-26.3166401197718,25.2216330422663,-2.7999791957612));
#40020=CARTESIAN_POINT('Ctrl Pts',(-26.1658445077554,25.4330686060118,-2.81638506190913));
#40021=CARTESIAN_POINT('Ctrl Pts',(-26.1575529433625,25.4445340144293,-2.81727412190962));
#40022=CARTESIAN_POINT('Ctrl Pts',(-26.1469721090427,25.4589638812027,-2.81839193755103));
#40023=CARTESIAN_POINT('Ctrl Pts',(-26.1447529877117,25.4619792284769,-2.81862546053773));
#40024=CARTESIAN_POINT('Ctrl Pts',(-26.1412381292602,25.4667378338647,-2.81899388240071));
#40025=CARTESIAN_POINT('Ctrl Pts',(-26.1399458845009,25.4684836488243,-2.81912902438785));
#40026=CARTESIAN_POINT('Ctrl Pts',(-26.1375408885669,25.4717259242929,-2.81937996135543));
#40027=CARTESIAN_POINT('Ctrl Pts',(-26.1364286104118,25.4732227160637,-2.81949578806962));
#40028=CARTESIAN_POINT('Ctrl Pts',(-26.1339459130093,25.4765576296768,-2.81975381531637));
#40029=CARTESIAN_POINT('Ctrl Pts',(-26.1325748343275,25.4783952506251,-2.81989596829689));
#40030=CARTESIAN_POINT('Ctrl Pts',(-26.1285642346391,25.4837586016909,-2.82031078905726));
#40031=CARTESIAN_POINT('Ctrl Pts',(-26.1259194322612,25.4872804040098,-2.82058308632838));
#40032=CARTESIAN_POINT('Ctrl Pts',(-26.1067641607551,25.5126788446631,-2.8225462594122));
#40033=CARTESIAN_POINT('Ctrl Pts',(-26.0899817859081,25.5343503567916,-2.82421828213052));
#40034=CARTESIAN_POINT('Ctrl Pts',(-26.0364471629167,25.6016885181801,-2.82941318009864));
#40035=CARTESIAN_POINT('Ctrl Pts',(-25.9987225735468,25.6465704262292,-2.83287505864796));
#40036=CARTESIAN_POINT('Ctrl Pts',(-25.9048215732454,25.7522912125675,-2.84109725080491));
#40037=CARTESIAN_POINT('Ctrl Pts',(-25.8474837298069,25.8120438590498,-2.84580200400116));
#40038=CARTESIAN_POINT('Ctrl Pts',(-25.6274551384789,26.0243292548041,-2.8630193164219));
#40039=CARTESIAN_POINT('Ctrl Pts',(-25.4513809742409,26.1620594148432,-2.875260611496));
#40040=CARTESIAN_POINT('Ctrl Pts',(-25.1616018363719,26.3437907261885,-2.89500747817153));
#40041=CARTESIAN_POINT('Ctrl Pts',(-25.0572836209951,26.4014197397457,-2.90203705754552));
#40042=CARTESIAN_POINT('Ctrl Pts',(-24.9404305573871,26.4577662561175,-2.90993069201774));
#40043=CARTESIAN_POINT('Ctrl Pts',(-24.9308141331345,26.4623446767304,-2.91058039641108));
#40044=CARTESIAN_POINT('Ctrl Pts',(-24.9172841026905,26.4687043015373,-2.91149470924142));
#40045=CARTESIAN_POINT('Ctrl Pts',(-24.9133892842406,26.4705255056757,-2.91175793048819));
#40046=CARTESIAN_POINT('Ctrl Pts',(-24.9066266716694,26.4736712039743,-2.91221500839286));
#40047=CARTESIAN_POINT('Ctrl Pts',(-24.9037605459633,26.474999289318,-2.91240874056708));
#40048=CARTESIAN_POINT('Ctrl Pts',(-24.8978574182098,26.4777241039893,-2.91280778544201));
#40049=CARTESIAN_POINT('Ctrl Pts',(-24.8948201877655,26.4791203257183,-2.9130131153483));
#40050=CARTESIAN_POINT('Ctrl Pts',(-24.8877125887241,26.4823743193437,-2.91349366106644));
#40051=CARTESIAN_POINT('Ctrl Pts',(-24.8836405202389,26.4842283416561,-2.91376900578269));
#40052=CARTESIAN_POINT('Ctrl Pts',(-24.8750399258782,26.4881226093017,-2.91435063225017));
#40053=CARTESIAN_POINT('Ctrl Pts',(-24.8705105216409,26.4901608758828,-2.91465698136322));
#40054=CARTESIAN_POINT('Ctrl Pts',(-24.8583533418804,26.4955979389077,-2.91547936233691));
#40055=CARTESIAN_POINT('Ctrl Pts',(-24.8507170760723,26.498977555176,-2.91599605195103));
#40056=CARTESIAN_POINT('Ctrl Pts',(-24.6670811050053,26.5793980725762,-2.92842480170463));
#40057=CARTESIAN_POINT('Ctrl Pts',(-24.4845890141806,26.6405631951537,-2.9408885364234));
#40058=CARTESIAN_POINT('Ctrl Pts',(-24.0042889811236,26.7550918308312,-2.97386858086621));
#40059=CARTESIAN_POINT('Ctrl Pts',(-23.702445504781,26.783515040905,-2.99485014069555));
#40060=CARTESIAN_POINT('Ctrl Pts',(-23.3849598488456,26.7688011934813,-3.01496249244831));
#40061=CARTESIAN_POINT('Ctrl Pts',(-23.3688705336006,26.7679345787353,-3.01597598091149));
#40062=CARTESIAN_POINT('Ctrl Pts',(-23.3492164031156,26.76672806275,-3.01720643545685));
#40063=CARTESIAN_POINT('Ctrl Pts',(-23.3456451526113,26.7665028620643,-3.01742970866661));
#40064=CARTESIAN_POINT('Ctrl Pts',(-23.3397563797149,26.7661216720056,-3.01779735897987));
#40065=CARTESIAN_POINT('Ctrl Pts',(-23.3374386506163,26.765969125192,-3.01794192919325));
#40066=CARTESIAN_POINT('Ctrl Pts',(-23.3332585126869,26.7656894604644,-3.01820242948673));
#40067=CARTESIAN_POINT('Ctrl Pts',(-23.3313960539708,26.7655632304294,-3.01831840948071));
#40068=CARTESIAN_POINT('Ctrl Pts',(-23.3273896882546,26.7652881977364,-3.0185677110303));
#40069=CARTESIAN_POINT('Ctrl Pts',(-23.3252458260677,26.7651388692491,-3.01870100214614));
#40070=CARTESIAN_POINT('Ctrl Pts',(-23.3193707299076,26.764723739964,-3.01906596911516));
#40071=CARTESIAN_POINT('Ctrl Pts',(-23.3156397918937,26.7644535860547,-3.0192973988299));
#40072=CARTESIAN_POINT('Ctrl Pts',(-23.2962094457437,26.7630126401227,-3.02050092957759));
#40073=CARTESIAN_POINT('Ctrl Pts',(-23.280517945837,26.7617332930951,-3.02146698387324));
#40074=CARTESIAN_POINT('Ctrl Pts',(-23.1255891668766,26.7479582051925,-3.03095257659426));
#40075=CARTESIAN_POINT('Ctrl Pts',(-22.9872758710674,26.7265283740593,-3.0390029099222));
#40076=CARTESIAN_POINT('Ctrl Pts',(-22.5809545265929,26.636185394098,-3.06253153655113));
#40077=CARTESIAN_POINT('Ctrl Pts',(-22.320271996219,26.5417986630288,-3.07757178124686));
#40078=CARTESIAN_POINT('Ctrl Pts',(-22.0750359182355,26.4155367245581,-3.0937462422167));
#40079=CARTESIAN_POINT('',(-26.7730011298473,23.5526187726184,-2.93758573339873));
#40080=CARTESIAN_POINT('Ctrl Pts',(-22.0750361667496,26.4155368525077,-3.34376876818698));
#40081=CARTESIAN_POINT('Ctrl Pts',(-22.1688943408046,26.4638605435787,-3.3378288799319));
#40082=CARTESIAN_POINT('Ctrl Pts',(-22.2651012992214,26.5075592847051,-3.33182564982117));
#40083=CARTESIAN_POINT('Ctrl Pts',(-22.4572788829981,26.5836897363742,-3.31980480788063));
#40084=CARTESIAN_POINT('Ctrl Pts',(-22.5529345878195,26.6164694787834,-3.31380812174433));
#40085=CARTESIAN_POINT('Ctrl Pts',(-22.6589933387836,26.6473258303721,-3.30708520147718));
#40086=CARTESIAN_POINT('Ctrl Pts',(-22.6680327218927,26.6499128631793,-3.30651165196124));
#40087=CARTESIAN_POINT('Ctrl Pts',(-22.6814520928204,26.6536899741265,-3.3056593254318));
#40088=CARTESIAN_POINT('Ctrl Pts',(-22.6858235386818,26.6549104319104,-3.30538153864854));
#40089=CARTESIAN_POINT('Ctrl Pts',(-22.6933028319005,26.6569815441514,-3.30490602365386));
#40090=CARTESIAN_POINT('Ctrl Pts',(-22.6964094127031,26.6578367820177,-3.30470844488574));
#40091=CARTESIAN_POINT('Ctrl Pts',(-22.7026418186639,26.6595425046275,-3.30431192085007));
#40092=CARTESIAN_POINT('Ctrl Pts',(-22.7057676533225,26.6603929379636,-3.30411297421242));
#40093=CARTESIAN_POINT('Ctrl Pts',(-22.7120507913711,26.6620921956407,-3.30371293168302));
#40094=CARTESIAN_POINT('Ctrl Pts',(-22.7152081143956,26.6629409312299,-3.30351183318725));
#40095=CARTESIAN_POINT('Ctrl Pts',(-22.7252528880012,26.6656247333638,-3.30287181502195));
#40096=CARTESIAN_POINT('Ctrl Pts',(-22.7321451019116,26.667441746204,-3.30243230962323));
#40097=CARTESIAN_POINT('Ctrl Pts',(-22.7723843216199,26.6779074734242,-3.29986417558199));
#40098=CARTESIAN_POINT('Ctrl Pts',(-22.8058612053786,26.6860436266896,-3.29771901156181));
#40099=CARTESIAN_POINT('Ctrl Pts',(-22.9032067568754,26.708055662676,-3.29145374148205));
#40100=CARTESIAN_POINT('Ctrl Pts',(-22.9673721276543,26.7205266983352,-3.28728963235783));
#40101=CARTESIAN_POINT('Ctrl Pts',(-23.145642830397,26.7495801041324,-3.27562146042933));
#40102=CARTESIAN_POINT('Ctrl Pts',(-23.2603194225701,26.7620028817506,-3.26800160186077));
#40103=CARTESIAN_POINT('Ctrl Pts',(-23.6616752211399,26.7838101247049,-3.24105942298021));
#40104=CARTESIAN_POINT('Ctrl Pts',(-23.948742506596,26.7610978109878,-3.2211910774191));
#40105=CARTESIAN_POINT('Ctrl Pts',(-24.2415967046084,26.6980019208678,-3.20223802942282));
#40106=CARTESIAN_POINT('Ctrl Pts',(-24.254153687607,26.6952177394838,-3.20142820987855));
#40107=CARTESIAN_POINT('Ctrl Pts',(-24.2718131105254,26.6911911592768,-3.20029366698206));
#40108=CARTESIAN_POINT('Ctrl Pts',(-24.2769294928991,26.6900113960249,-3.19996547557595));
#40109=CARTESIAN_POINT('Ctrl Pts',(-24.2845064884599,26.688244738203,-3.19948023378188));
#40110=CARTESIAN_POINT('Ctrl Pts',(-24.2869692982333,26.6876674496073,-3.19932263507599));
#40111=CARTESIAN_POINT('Ctrl Pts',(-24.2911775537826,26.6866757959197,-3.19905355648742));
#40112=CARTESIAN_POINT('Ctrl Pts',(-24.2929233327316,26.6862628732036,-3.19894199314404));
#40113=CARTESIAN_POINT('Ctrl Pts',(-24.2963223017574,26.6854559300348,-3.19872490705267));
#40114=CARTESIAN_POINT('Ctrl Pts',(-24.297975520261,26.6850620607003,-3.19861937614539));
#40115=CARTESIAN_POINT('Ctrl Pts',(-24.3019628353981,26.6841087732498,-3.19836498819468));
#40116=CARTESIAN_POINT('Ctrl Pts',(-24.3042966249379,26.6835480538187,-3.19821620703586));
#40117=CARTESIAN_POINT('Ctrl Pts',(-24.3114207402016,26.6818279837734,-3.19776237740747));
#40118=CARTESIAN_POINT('Ctrl Pts',(-24.3162090632844,26.6806602441475,-3.19745781377138));
#40119=CARTESIAN_POINT('Ctrl Pts',(-24.3646782151912,26.668722089187,-3.19437948094654));
#40120=CARTESIAN_POINT('Ctrl Pts',(-24.4081343625763,26.6570484447148,-3.19165715215846));
#40121=CARTESIAN_POINT('Ctrl Pts',(-24.5309914502857,26.621270617972,-3.18403105931695));
#40122=CARTESIAN_POINT('Ctrl Pts',(-24.6097291853234,26.5950041171786,-3.17922784467167));
#40123=CARTESIAN_POINT('Ctrl Pts',(-24.7945841085958,26.5252963517135,-3.16796451724521));
#40124=CARTESIAN_POINT('Ctrl Pts',(-24.8995688105568,26.4791762694943,-3.16157672544629));
#40125=CARTESIAN_POINT('Ctrl Pts',(-25.1168980558848,26.3695319707076,-3.14797462472122));
#40126=CARTESIAN_POINT('Ctrl Pts',(-25.2283319684792,26.3046602445977,-3.14076668697122));
#40127=CARTESIAN_POINT('Ctrl Pts',(-25.3828567008539,26.201837770413,-3.13012641416181));
#40128=CARTESIAN_POINT('Ctrl Pts',(-25.4292920356733,26.169136337539,-3.12683950056204));
#40129=CARTESIAN_POINT('Ctrl Pts',(-25.4905088274792,26.1235587300766,-3.12236638170538));
#40130=CARTESIAN_POINT('Ctrl Pts',(-25.506073385003,26.1117489793259,-3.1212165402572));
#40131=CARTESIAN_POINT('Ctrl Pts',(-25.5256327317084,26.0966259393591,-3.11975504412438));
#40132=CARTESIAN_POINT('Ctrl Pts',(-25.5297284094047,26.0934433847364,-3.11944808324342));
#40133=CARTESIAN_POINT('Ctrl Pts',(-25.5370532965627,26.087723152366,-3.11889742250627));
#40134=CARTESIAN_POINT('Ctrl Pts',(-25.540285377806,26.0851891583637,-3.11865385687884));
#40135=CARTESIAN_POINT('Ctrl Pts',(-25.5461453740895,26.0805767302907,-3.1182111778378));
#40136=CARTESIAN_POINT('Ctrl Pts',(-25.5487749119699,26.0785003604769,-3.11801214051021));
#40137=CARTESIAN_POINT('Ctrl Pts',(-25.5927391309593,26.0436733179728,-3.11467770188953));
#40138=CARTESIAN_POINT('Ctrl Pts',(-25.6332650533486,26.0099185791214,-3.1115051547378));
#40139=CARTESIAN_POINT('Ctrl Pts',(-25.6795060496545,25.9694410528153,-3.10776003941509));
#40140=CARTESIAN_POINT('Ctrl Pts',(-25.6860458240265,25.9636693325271,-3.10722737893163));
#40141=CARTESIAN_POINT('Ctrl Pts',(-25.69576412987,25.9550219418757,-3.10643131011997));
#40142=CARTESIAN_POINT('Ctrl Pts',(-25.6989605236228,25.9521663309785,-3.10616874527303));
#40143=CARTESIAN_POINT('Ctrl Pts',(-25.7046542744291,25.9470591571308,-3.10569972000538));
#40144=CARTESIAN_POINT('Ctrl Pts',(-25.7071538270086,25.9448100421689,-3.10549336312122));
#40145=CARTESIAN_POINT('Ctrl Pts',(-25.7119789536941,25.9404546745151,-3.10509412920712));
#40146=CARTESIAN_POINT('Ctrl Pts',(-25.7143049817363,25.9383489285077,-3.1049012737757));
#40147=CARTESIAN_POINT('Ctrl Pts',(-25.7193365550757,25.9337804729937,-3.10448323014683));
#40148=CARTESIAN_POINT('Ctrl Pts',(-25.7220409870032,25.9313165486108,-3.10425799043073));
#40149=CARTESIAN_POINT('Ctrl Pts',(-25.732673302807,25.9215965897878,-3.10337032069829));
#40150=CARTESIAN_POINT('Ctrl Pts',(-25.7405689961006,25.9143055863651,-3.10270639984789));
#40151=CARTESIAN_POINT('Ctrl Pts',(-25.8241802385079,25.8363192468397,-3.09562495571878));
#40152=CARTESIAN_POINT('Ctrl Pts',(-25.8964738505739,25.7620594381685,-3.08905269378531));
#40153=CARTESIAN_POINT('Ctrl Pts',(-26.0088972307174,25.6348545530367,-3.07804408436624));
#40154=CARTESIAN_POINT('Ctrl Pts',(-26.0511926417979,25.5839184422617,-3.07369619662488));
#40155=CARTESIAN_POINT('Ctrl Pts',(-26.252167109403,25.3261276206479,-3.05200658102386));
#40156=CARTESIAN_POINT('Ctrl Pts',(-26.3868968346137,25.1018682632967,-3.034004808293));
#40157=CARTESIAN_POINT('Ctrl Pts',(-26.4977419915785,24.8535371469987,-3.01611516702053));
#40158=CARTESIAN_POINT('Ctrl Pts',(-26.5022874803899,24.8432082820346,-3.01537472828653));
#40159=CARTESIAN_POINT('Ctrl Pts',(-26.5129664315766,24.8185922505983,-3.01361908472154));
#40160=CARTESIAN_POINT('Ctrl Pts',(-26.5190509981154,24.8042840216131,-3.01260576557898));
#40161=CARTESIAN_POINT('Ctrl Pts',(-26.52820989302,24.7823060099169,-3.01106078071371));
#40162=CARTESIAN_POINT('Ctrl Pts',(-26.5313585971773,24.7746676770487,-3.01052594657956));
#40163=CARTESIAN_POINT('Ctrl Pts',(-26.5354856424881,24.7645457255392,-3.00982008300289));
#40164=CARTESIAN_POINT('Ctrl Pts',(-26.53649029267,24.7620729480165,-3.00964786786068));
#40165=CARTESIAN_POINT('Ctrl Pts',(-26.5393134591315,24.7550993678874,-3.00916283999665));
#40166=CARTESIAN_POINT('Ctrl Pts',(-26.5411248880731,24.7505956805718,-3.00885035282926));
#40167=CARTESIAN_POINT('Ctrl Pts',(-26.5565328525252,24.7120360173548,-3.00618144869453));
#40168=CARTESIAN_POINT('Ctrl Pts',(-26.5695581193038,24.6777525490764,-3.00385214420757));
#40169=CARTESIAN_POINT('Ctrl Pts',(-26.5835826892461,24.6388514496286,-3.00126393461964));
#40170=CARTESIAN_POINT('Ctrl Pts',(-26.5851597624699,24.6344469561789,-3.00097167673504));
#40171=CARTESIAN_POINT('Ctrl Pts',(-26.5875268006212,24.6277905924981,-3.00053120100323));
#40172=CARTESIAN_POINT('Ctrl Pts',(-26.5883238558558,24.6255412773642,-3.0003825629187));
#40173=CARTESIAN_POINT('Ctrl Pts',(-26.5897031323159,24.6216351397674,-3.0001248017762));
#40174=CARTESIAN_POINT('Ctrl Pts',(-26.5902864975567,24.6199787270067,-3.00001561012724));
#40175=CARTESIAN_POINT('Ctrl Pts',(-26.5915023717629,24.6165173350041,-2.99978767040763));
#40176=CARTESIAN_POINT('Ctrl Pts',(-26.5921346273865,24.6147122709151,-2.9996689380268));
#40177=CARTESIAN_POINT('Ctrl Pts',(-26.5936387919884,24.6104056579456,-2.99938597940423));
#40178=CARTESIAN_POINT('Ctrl Pts',(-26.5945092266958,24.6079035873391,-2.99922184168739));
#40179=CARTESIAN_POINT('Ctrl Pts',(-26.5974298148769,24.5994748606458,-2.99866976533848));
#40180=CARTESIAN_POINT('Ctrl Pts',(-26.5994657707283,24.5935432462982,-2.99828266971334));
#40181=CARTESIAN_POINT('Ctrl Pts',(-26.6387551171952,24.4779790255854,-2.99076792548357));
#40182=CARTESIAN_POINT('Ctrl Pts',(-26.6700955626545,24.3664087776341,-2.98398354023975));
#40183=CARTESIAN_POINT('Ctrl Pts',(-26.7467938389344,24.0233349666376,-2.96385955048933));
#40184=CARTESIAN_POINT('Ctrl Pts',(-26.772828298777,23.7883472203177,-2.95102022401773));
#40185=CARTESIAN_POINT('Ctrl Pts',(-26.7730016601459,23.5526226717751,-2.93758688024679));
#40186=CARTESIAN_POINT('Ctrl Pts',(-26.7730016630494,23.5526187204738,-2.9375866550721));
#40187=CARTESIAN_POINT('Ctrl Pts',(-26.7731176149863,23.394692181726,-2.92858681874837));
#40188=CARTESIAN_POINT('Ctrl Pts',(-26.761625434773,23.2369872380094,-2.91936317422375));
#40189=CARTESIAN_POINT('Ctrl Pts',(-26.7376222489929,23.0739763744628,-2.90933099846862));
#40190=CARTESIAN_POINT('Ctrl Pts',(-26.7366004539343,23.0671877223873,-2.90891232305038));
#40191=CARTESIAN_POINT('Ctrl Pts',(-26.7348963751076,23.0561067614394,-2.90822746956691));
#40192=CARTESIAN_POINT('Ctrl Pts',(-26.7342270822599,23.0518124523366,-2.90796170356339));
#40193=CARTESIAN_POINT('Ctrl Pts',(-26.7330314354178,23.0442416374893,-2.90749252431895));
#40194=CARTESIAN_POINT('Ctrl Pts',(-26.7325087024492,23.0409645595176,-2.90728922628265));
#40195=CARTESIAN_POINT('Ctrl Pts',(-26.7314725822137,23.0345328715813,-2.90688981167449));
#40196=CARTESIAN_POINT('Ctrl Pts',(-26.7309595618014,23.0313782057139,-2.9066937069765));
#40197=CARTESIAN_POINT('Ctrl Pts',(-26.7299303083534,23.0251080066467,-2.90630353713853));
#40198=CARTESIAN_POINT('Ctrl Pts',(-26.7294141869646,23.0219924583332,-2.90610947574212));
#40199=CARTESIAN_POINT('Ctrl Pts',(-26.7281851937343,23.0146407211812,-2.90565109233367));
#40200=CARTESIAN_POINT('Ctrl Pts',(-26.7274684309178,23.0104051963617,-2.90538664662962));
#40201=CARTESIAN_POINT('Ctrl Pts',(-26.7249489607696,22.9956958652806,-2.90446701045664));
#40202=CARTESIAN_POINT('Ctrl Pts',(-26.7231029283755,22.9852296392551,-2.90381044068062));
#40203=CARTESIAN_POINT('Ctrl Pts',(-26.7001368033008,22.858683914779,-2.89584471742151));
#40204=CARTESIAN_POINT('Ctrl Pts',(-26.6727119668798,22.7438535494066,-2.88833377872145));
#40205=CARTESIAN_POINT('Ctrl Pts',(-26.6320720080184,22.6073284679076,-2.8790452970354));
#40206=CARTESIAN_POINT('Ctrl Pts',(-26.6248193302774,22.5839420066789,-2.87744142069908));
#40207=CARTESIAN_POINT('Ctrl Pts',(-26.6113050750688,22.5420580250215,-2.8745463312326));
#40208=CARTESIAN_POINT('Ctrl Pts',(-26.6051404628003,22.5235302985516,-2.87325763101354));
#40209=CARTESIAN_POINT('Ctrl Pts',(-26.5111682092076,22.2494376214018,-2.85407602357772));
#40210=CARTESIAN_POINT('Ctrl Pts',(-26.3917370846445,22.0058787904027,-2.8353921177336));
#40211=CARTESIAN_POINT('Ctrl Pts',(-26.205054281669,21.7218652959204,-2.81305161463466));
#40212=CARTESIAN_POINT('Ctrl Pts',(-26.1649020365322,21.6648926518335,-2.8085459738846));
#40213=CARTESIAN_POINT('Ctrl Pts',(-26.1162340942652,21.6003859170614,-2.80345654554986));
#40214=CARTESIAN_POINT('Ctrl Pts',(-26.1094913692146,21.5915443412106,-2.80275924387021));
#40215=CARTESIAN_POINT('Ctrl Pts',(-26.100679942838,21.5801133074973,-2.80185827764924));
#40216=CARTESIAN_POINT('Ctrl Pts',(-26.0986529256779,21.5774920357362,-2.80165171361203));
#40217=CARTESIAN_POINT('Ctrl Pts',(-26.0953630790357,21.5732512464698,-2.8013175951957));
#40218=CARTESIAN_POINT('Ctrl Pts',(-26.0941027446444,21.5716298101785,-2.80118986358982));
#40219=CARTESIAN_POINT('Ctrl Pts',(-26.0916822041781,21.5685218895532,-2.80094506447933));
#40220=CARTESIAN_POINT('Ctrl Pts',(-26.0905222468452,21.5670352232575,-2.80082798017312));
#40221=CARTESIAN_POINT('Ctrl Pts',(-26.0878547983203,21.5636226515896,-2.80055925096354));
#40222=CARTESIAN_POINT('Ctrl Pts',(-26.0863464155372,21.5616974390352,-2.80040767007954));
#40223=CARTESIAN_POINT('Ctrl Pts',(-26.0823237394377,21.5565751494944,-2.80000442558831));
#40224=CARTESIAN_POINT('Ctrl Pts',(-26.0798055725806,21.5533810988895,-2.7997530380818));
#40225=CARTESIAN_POINT('Ctrl Pts',(-26.0680043113549,21.5384704880372,-2.79857973190425));
#40226=CARTESIAN_POINT('Ctrl Pts',(-26.0586456231145,21.5268135940502,-2.79766313070836));
#40227=CARTESIAN_POINT('Ctrl Pts',(-25.8514212802897,21.2723486282651,-2.77765839200026));
#40228=CARTESIAN_POINT('Ctrl Pts',(-25.6192499451273,21.0595597780481,-2.76089459607937));
#40229=CARTESIAN_POINT('Ctrl Pts',(-25.2736455937428,20.8250149967025,-2.73726906027501));
#40230=CARTESIAN_POINT('Ctrl Pts',(-25.1845262947236,20.7706572387589,-2.73129002872255));
#40231=CARTESIAN_POINT('Ctrl Pts',(-25.0449716760142,20.6945711349221,-2.72196114427025));
#40232=CARTESIAN_POINT('Ctrl Pts',(-24.9963559554664,20.6696473989967,-2.71871778927306));
#40233=CARTESIAN_POINT('Ctrl Pts',(-24.9199963960683,20.6329205290624,-2.71361995107313));
#40234=CARTESIAN_POINT('Ctrl Pts',(-24.8926796055842,20.6202501897048,-2.71179561139613));
#40235=CARTESIAN_POINT('Ctrl Pts',(-24.8589483314576,20.6051753501253,-2.7095407486087));
#40236=CARTESIAN_POINT('Ctrl Pts',(-24.8526978620025,20.6024057815837,-2.70912283016058));
#40237=CARTESIAN_POINT('Ctrl Pts',(-24.8434716930708,20.5983527595356,-2.70850580483268));
#40238=CARTESIAN_POINT('Ctrl Pts',(-24.8405027655238,20.5970538593723,-2.70830722747293));
#40239=CARTESIAN_POINT('Ctrl Pts',(-24.8347453924039,20.5945453588049,-2.70792209917661));
#40240=CARTESIAN_POINT('Ctrl Pts',(-24.831957183881,20.593335220449,-2.70773556689757));
#40241=CARTESIAN_POINT('Ctrl Pts',(-24.8262102715081,20.5908506010729,-2.70735105212164));
#40242=CARTESIAN_POINT('Ctrl Pts',(-24.8232513609295,20.5895766086329,-2.70715305315777));
#40243=CARTESIAN_POINT('Ctrl Pts',(-24.8161213595973,20.5865193704512,-2.7066758805604));
#40244=CARTESIAN_POINT('Ctrl Pts',(-24.8119484124001,20.5847404941549,-2.70639655811985));
#40245=CARTESIAN_POINT('Ctrl Pts',(-24.7991234994463,20.579305360625,-2.70553794292718));
#40246=CARTESIAN_POINT('Ctrl Pts',(-24.7904593519459,20.5756781373682,-2.70495766275381));
#40247=CARTESIAN_POINT('Ctrl Pts',(-24.7584650396152,20.5624478839631,-2.70281393941075));
#40248=CARTESIAN_POINT('Ctrl Pts',(-24.7350386820786,20.5530812324948,-2.70124251294084));
#40249=CARTESIAN_POINT('Ctrl Pts',(-24.7058746754377,20.5418158184188,-2.69928357162428));
#40250=CARTESIAN_POINT('Ctrl Pts',(-24.7002379907897,20.5396566704131,-2.69890483582364));
#40251=CARTESIAN_POINT('Ctrl Pts',(-24.6881773104612,20.5350756059123,-2.69809419824144));
#40252=CARTESIAN_POINT('Ctrl Pts',(-24.6817515836279,20.5326583591457,-2.69766214363788));
#40253=CARTESIAN_POINT('Ctrl Pts',(-24.6738973158571,20.5297323346583,-2.69713383475595));
#40254=CARTESIAN_POINT('Ctrl Pts',(-24.6724760385455,20.5292039947892,-2.69703822601826));
#40255=CARTESIAN_POINT('Ctrl Pts',(-24.6647618547135,20.5263425503163,-2.69651925215158));
#40256=CARTESIAN_POINT('Ctrl Pts',(-24.658462081175,20.5240281183499,-2.69609527459557));
#40257=CARTESIAN_POINT('Ctrl Pts',(-24.643715625694,20.5186627376629,-2.69510245271877));
#40258=CARTESIAN_POINT('Ctrl Pts',(-24.6352633598522,20.5156273954722,-2.69453310441106));
#40259=CARTESIAN_POINT('Ctrl Pts',(-24.623045016367,20.5112971673876,-2.69370964352609));
#40260=CARTESIAN_POINT('Ctrl Pts',(-24.619288998891,20.5099738515407,-2.69345644681485));
#40261=CARTESIAN_POINT('Ctrl Pts',(-24.6105862289025,20.5069258226277,-2.69286964906068));
#40262=CARTESIAN_POINT('Ctrl Pts',(-24.6056377143004,20.5052062063694,-2.69253588639295));
#40263=CARTESIAN_POINT('Ctrl Pts',(-24.5805808568521,20.496567327377,-2.69084535846534));
#40264=CARTESIAN_POINT('Ctrl Pts',(-24.5604089340155,20.4898352735553,-2.68948271805058));
#40265=CARTESIAN_POINT('Ctrl Pts',(-24.4885166777385,20.4666305970646,-2.68462026064215));
#40266=CARTESIAN_POINT('Ctrl Pts',(-24.4364505785761,20.4512661898824,-2.68108751583845));
#40267=CARTESIAN_POINT('Ctrl Pts',(-24.2350708168662,20.3973300842698,-2.66738713078729));
#40268=CARTESIAN_POINT('Ctrl Pts',(-24.0834583137772,20.3681808258822,-2.65698375479044));
#40269=CARTESIAN_POINT('Ctrl Pts',(-23.9121277515839,20.3478314443187,-2.64530460500259));
#40270=CARTESIAN_POINT('Ctrl Pts',(-23.8938819539107,20.3458222676983,-2.64406200363223));
#40271=CARTESIAN_POINT('Ctrl Pts',(-23.8544243989858,20.3418181913229,-2.64137823439547));
#40272=CARTESIAN_POINT('Ctrl Pts',(-23.8332079350134,20.3398775243552,-2.63993729511466));
#40273=CARTESIAN_POINT('Ctrl Pts',(-23.7867649652777,20.3360933677338,-2.6367892804878));
#40274=CARTESIAN_POINT('Ctrl Pts',(-23.7615326892881,20.3343361802749,-2.63508297323784));
#40275=CARTESIAN_POINT('Ctrl Pts',(-23.7050297385417,20.3310691637154,-2.6312738230857));
#40276=CARTESIAN_POINT('Ctrl Pts',(-23.6737521200838,20.3297175669739,-2.6291733103008));
#40277=CARTESIAN_POINT('Ctrl Pts',(-23.5243564463918,20.3254414272693,-2.61919144697101));
#40278=CARTESIAN_POINT('Ctrl Pts',(-23.4061410277907,20.3285578987412,-2.61144270076675));
#40279=CARTESIAN_POINT('Ctrl Pts',(-23.2822617950769,20.3386585590301,-2.60365485502659));
#40280=CARTESIAN_POINT('Ctrl Pts',(-23.2761745462321,20.3391723178865,-2.60327302501202));
#40281=CARTESIAN_POINT('Ctrl Pts',(-23.2674777418531,20.3399312315853,-2.60272876328481));
#40282=CARTESIAN_POINT('Ctrl Pts',(-23.2648670156037,20.3401622620871,-2.602565541114));
#40283=CARTESIAN_POINT('Ctrl Pts',(-23.2603567323792,20.3405669354946,-2.60228384194877));
#40284=CARTESIAN_POINT('Ctrl Pts',(-23.25845704514,20.3407390802483,-2.60216527980001));
#40285=CARTESIAN_POINT('Ctrl Pts',(-23.2548022372927,20.3410735412371,-2.60193734641992));
#40286=CARTESIAN_POINT('Ctrl Pts',(-23.253047100458,20.341235610434,-2.60182796124331));
#40287=CARTESIAN_POINT('Ctrl Pts',(-23.2488909940216,20.3416228239484,-2.60156911542913));
#40288=CARTESIAN_POINT('Ctrl Pts',(-23.246490138292,20.341849223776,-2.60141972620068));
#40289=CARTESIAN_POINT('Ctrl Pts',(-23.2393343561126,20.3425321155418,-2.60097487528912));
#40290=CARTESIAN_POINT('Ctrl Pts',(-23.2345801611178,20.3429964871514,-2.60067985699347));
#40291=CARTESIAN_POINT('Ctrl Pts',(-23.1905864580744,20.3473923926164,-2.59795465659187));
#40292=CARTESIAN_POINT('Ctrl Pts',(-23.151419023337,20.352033506553,-2.59556375998345));
#40293=CARTESIAN_POINT('Ctrl Pts',(-23.1097927875592,20.3577426397597,-2.59305109765782));
#40294=CARTESIAN_POINT('Ctrl Pts',(-23.1072414710324,20.3580956751912,-2.5928972075835));
#40295=CARTESIAN_POINT('Ctrl Pts',(-23.1032624598652,20.3586511284116,-2.59265737550673));
#40296=CARTESIAN_POINT('Ctrl Pts',(-23.1018344788232,20.3588514457097,-2.59257133984019));
#40297=CARTESIAN_POINT('Ctrl Pts',(-23.0973154604185,20.3594884669021,-2.59229917862654));
#40298=CARTESIAN_POINT('Ctrl Pts',(-23.0942249137604,20.3599287049436,-2.59211320966619));
#40299=CARTESIAN_POINT('Ctrl Pts',(-22.8591971861004,20.3937561156087,-2.57798272765505));
#40300=CARTESIAN_POINT('Ctrl Pts',(-22.6315625206171,20.4523396940686,-2.56514371546771));
#40301=CARTESIAN_POINT('Ctrl Pts',(-22.2951364481622,20.5793138391578,-2.54498732163228));
#40302=CARTESIAN_POINT('Ctrl Pts',(-22.1806821305994,20.6303096017905,-2.5379095919147));
#40303=CARTESIAN_POINT('Ctrl Pts',(-22.0125182632425,20.7173025989869,-2.52691196314952));
#40304=CARTESIAN_POINT('Ctrl Pts',(-21.956441749928,20.7484676710725,-2.52313877769711));
#40305=CARTESIAN_POINT('Ctrl Pts',(-21.8764573241606,20.7960982995331,-2.5175780344988));
#40306=CARTESIAN_POINT('Ctrl Pts',(-21.8517811110839,20.8112471131967,-2.51583698431417));
#40307=CARTESIAN_POINT('Ctrl Pts',(-21.8168978247166,20.8333147501416,-2.51333756788259));
#40308=CARTESIAN_POINT('Ctrl Pts',(-21.8065206909193,20.839963117269,-2.51258914448544));
#40309=CARTESIAN_POINT('Ctrl Pts',(-21.7883134903224,20.8517758589677,-2.51126722198594));
#40310=CARTESIAN_POINT('Ctrl Pts',(-21.7804673143244,20.8569152300902,-2.51069465801427));
#40311=CARTESIAN_POINT('Ctrl Pts',(-21.7689735850154,20.8645157171566,-2.50985160759914));
#40312=CARTESIAN_POINT('Ctrl Pts',(-21.7653084082743,20.8669502008324,-2.50958212390627));
#40313=CARTESIAN_POINT('Ctrl Pts',(-21.7589897724524,20.8711658397017,-2.50911641906948));
#40314=CARTESIAN_POINT('Ctrl Pts',(-21.7563339493032,20.8729434543759,-2.50892033183641));
#40315=CARTESIAN_POINT('Ctrl Pts',(-21.7510593569301,20.8764852544787,-2.5085302063753));
#40316=CARTESIAN_POINT('Ctrl Pts',(-21.7484405273014,20.8782493442834,-2.50833617190397));
#40317=CARTESIAN_POINT('Ctrl Pts',(-21.7422664238528,20.8824215334286,-2.507877920129));
#40318=CARTESIAN_POINT('Ctrl Pts',(-21.7387133680811,20.8848328912111,-2.50761357930658));
#40319=CARTESIAN_POINT('Ctrl Pts',(-21.726391320236,20.8932315331307,-2.50669465175795));
#40320=CARTESIAN_POINT('Ctrl Pts',(-21.7176471786981,20.8992549984428,-2.50603868854075));
#40321=CARTESIAN_POINT('Ctrl Pts',(-21.6124850570262,20.9724656273743,-2.49810254509883));
#40322=CARTESIAN_POINT('Ctrl Pts',(-21.5197934187683,21.0448267924307,-2.4906222022246));
#40323=CARTESIAN_POINT('Ctrl Pts',(-21.2492041527251,21.2809609310822,-2.46720822712583));
#40324=CARTESIAN_POINT('Ctrl Pts',(-21.0856022918418,21.4598027245708,-2.45070297005883));
#40325=CARTESIAN_POINT('Ctrl Pts',(-20.855796525491,21.7759095638967,-2.42440150153338));
#40326=CARTESIAN_POINT('Ctrl Pts',(-20.7765246019652,21.9025778177085,-2.41450535977724));
#40327=CARTESIAN_POINT('Ctrl Pts',(-20.7034337725026,22.0396970354984,-2.40476921081609));
#40328=CARTESIAN_POINT('Ctrl Pts',(-20.7005727057971,22.0451014276156,-2.40438699748589));
#40329=CARTESIAN_POINT('Ctrl Pts',(-20.6965068436451,22.0528347592433,-2.40384228731023));
#40330=CARTESIAN_POINT('Ctrl Pts',(-20.6952895039893,22.0551570337856,-2.40367899822689));
#40331=CARTESIAN_POINT('Ctrl Pts',(-20.6931913730637,22.0591714683421,-2.40339722022666));
#40332=CARTESIAN_POINT('Ctrl Pts',(-20.6923092489605,22.0608629270598,-2.4032786460284));
#40333=CARTESIAN_POINT('Ctrl Pts',(-20.6906150823782,22.0641185112139,-2.40305071622753));
#40334=CARTESIAN_POINT('Ctrl Pts',(-20.6898028226109,22.0656825164364,-2.40294134663571));
#40335=CARTESIAN_POINT('Ctrl Pts',(-20.6878826016505,22.0693873262565,-2.40268257690375));
#40336=CARTESIAN_POINT('Ctrl Pts',(-20.6867757567197,22.0715287128677,-2.40253324807361));
#40337=CARTESIAN_POINT('Ctrl Pts',(-20.6834844793722,22.0779138215105,-2.40208869517871));
#40338=CARTESIAN_POINT('Ctrl Pts',(-20.6813070583736,22.0821611806112,-2.40179391366958));
#40339=CARTESIAN_POINT('Ctrl Pts',(-20.6612771948877,22.1214469254029,-2.39907582122423));
#40340=CARTESIAN_POINT('Ctrl Pts',(-20.6440570504599,22.1568063990951,-2.39669157176947));
#40341=CARTESIAN_POINT('Ctrl Pts',(-20.6263661435936,22.1948879917478,-2.39418024030171));
#40342=CARTESIAN_POINT('Ctrl Pts',(-20.6252477667475,22.1973032452106,-2.39402120398089));
#40343=CARTESIAN_POINT('Ctrl Pts',(-20.623591879861,22.2008909585587,-2.39378531744662));
#40344=CARTESIAN_POINT('Ctrl Pts',(-20.6230520823235,22.2020623539902,-2.3937083557285));
#40345=CARTESIAN_POINT('Ctrl Pts',(-20.621122672737,22.2062559184626,-2.39343303301176));
#40346=CARTESIAN_POINT('Ctrl Pts',(-20.6197370318817,22.2092799247597,-2.39323486423478));
#40347=CARTESIAN_POINT('Ctrl Pts',(-20.6166912817363,22.2159542009116,-2.39279828637573));
#40348=CARTESIAN_POINT('Ctrl Pts',(-20.6150332961677,22.219605440056,-2.39255997817797));
#40349=CARTESIAN_POINT('Ctrl Pts',(-20.6098935239963,22.2309806678423,-2.39181915209135));
#40350=CARTESIAN_POINT('Ctrl Pts',(-20.6064353528896,22.2387153551639,-2.39131772699228));
#40351=CARTESIAN_POINT('Ctrl Pts',(-20.601215461718,22.2505150396821,-2.39055614991386));
#40352=CARTESIAN_POINT('Ctrl Pts',(-20.5994315792356,22.2545701264949,-2.39029503054349));
#40353=CARTESIAN_POINT('Ctrl Pts',(-20.525382030641,22.4238442327912,-2.37941963746448));
#40354=CARTESIAN_POINT('Ctrl Pts',(-20.4670954225866,22.5948509486062,-2.36939932415109));
#40355=CARTESIAN_POINT('Ctrl Pts',(-20.3807777369471,22.9406995407201,-2.34947999964717));
#40356=CARTESIAN_POINT('Ctrl Pts',(-20.3522136450669,23.1147465513395,-2.3396121710883));
#40357=CARTESIAN_POINT('Ctrl Pts',(-20.3329914298302,23.3522237270046,-2.32569396876936));
#40358=CARTESIAN_POINT('Ctrl Pts',(-20.3297696829819,23.4143338821655,-2.32201463906848));
#40359=CARTESIAN_POINT('Ctrl Pts',(-20.3278485211888,23.4982554413895,-2.31697246291183));
#40360=CARTESIAN_POINT('Ctrl Pts',(-20.3275708490225,23.5200194193565,-2.31565846253371));
#40361=CARTESIAN_POINT('Ctrl Pts',(-20.3274874682947,23.5517508715871,-2.31373274017173));
#40362=CARTESIAN_POINT('Ctrl Pts',(-20.3275075141571,23.5617175807045,-2.31312645120896));
#40363=CARTESIAN_POINT('Ctrl Pts',(-20.3276262436872,23.5795711416655,-2.31203776898023));
#40364=CARTESIAN_POINT('Ctrl Pts',(-20.3277076491381,23.5874580583314,-2.31155591945637));
#40365=CARTESIAN_POINT('Ctrl Pts',(-20.3278753287331,23.5994410352372,-2.31082240163502));
#40366=CARTESIAN_POINT('Ctrl Pts',(-20.3279404627672,23.6035374005176,-2.31057139729893));
#40367=CARTESIAN_POINT('Ctrl Pts',(-20.3280674291221,23.6106672058305,-2.31013407630906));
#40368=CARTESIAN_POINT('Ctrl Pts',(-20.3281257345852,23.6137007100587,-2.30994787063113));
#40369=CARTESIAN_POINT('Ctrl Pts',(-20.328255101367,23.6199705374554,-2.3095627192955));
#40370=CARTESIAN_POINT('Ctrl Pts',(-20.3283267551518,23.6232068440057,-2.30936375522643));
#40371=CARTESIAN_POINT('Ctrl Pts',(-20.3285118830378,23.6310353026153,-2.30888208204943));
#40372=CARTESIAN_POINT('Ctrl Pts',(-20.328630299307,23.635627321483,-2.30859921796791));
#40373=CARTESIAN_POINT('Ctrl Pts',(-20.3291055775386,23.652645940715,-2.30754967485815));
#40374=CARTESIAN_POINT('Ctrl Pts',(-20.329524520711,23.6650705737708,-2.30678104831934));
#40375=CARTESIAN_POINT('Ctrl Pts',(-20.3379816248501,23.8791064406994,-2.29349794352499));
#40376=CARTESIAN_POINT('Ctrl Pts',(-20.3648620601589,24.0794869527433,-2.28037339375336));
#40377=CARTESIAN_POINT('Ctrl Pts',(-20.4236061685339,24.3336420660302,-2.26290823416026));
#40378=CARTESIAN_POINT('Ctrl Pts',(-20.4385112440124,24.3908966259931,-2.25892174635905));
#40379=CARTESIAN_POINT('Ctrl Pts',(-20.4974510269398,24.5941765230381,-2.24461605241875));
#40380=CARTESIAN_POINT('Ctrl Pts',(-20.5502629787708,24.7374509518412,-2.23423924383234));
#40381=CARTESIAN_POINT('Ctrl Pts',(-20.6402857982026,24.9368311220768,-2.21976011585997));
#40382=CARTESIAN_POINT('Ctrl Pts',(-20.6694057410358,24.9963609794146,-2.21543355863218));
#40383=CARTESIAN_POINT('Ctrl Pts',(-20.7136696199261,25.0801968853942,-2.2093774677648));
#40384=CARTESIAN_POINT('Ctrl Pts',(-20.7273323107288,25.1052618259698,-2.20757175820088));
#40385=CARTESIAN_POINT('Ctrl Pts',(-20.7435086155479,25.134022072848,-2.20550845704056));
#40386=CARTESIAN_POINT('Ctrl Pts',(-20.745698482774,25.1378966850119,-2.20523066964242));
#40387=CARTESIAN_POINT('Ctrl Pts',(-20.7490334630524,25.1437689557223,-2.20480995398076));
#40388=CARTESIAN_POINT('Ctrl Pts',(-20.7501726907364,25.1457699237998,-2.20466664733498));
#40389=CARTESIAN_POINT('Ctrl Pts',(-20.7521499520022,25.1492341949848,-2.20441863270622));
#40390=CARTESIAN_POINT('Ctrl Pts',(-20.7529869879875,25.1506980584326,-2.20431386011394));
#40391=CARTESIAN_POINT('Ctrl Pts',(-20.7547372826998,25.1537535208805,-2.20409523256723));
#40392=CARTESIAN_POINT('Ctrl Pts',(-20.7556507492884,25.1553449924254,-2.20398139181379));
#40393=CARTESIAN_POINT('Ctrl Pts',(-20.758183851802,25.1597495294493,-2.20366641880998));
#40394=CARTESIAN_POINT('Ctrl Pts',(-20.7598063850163,25.1625609394529,-2.20346547515328));
#40395=CARTESIAN_POINT('Ctrl Pts',(-20.7662052859165,25.1736099065285,-2.20267614444537));
#40396=CARTESIAN_POINT('Ctrl Pts',(-20.7710139672587,25.1818288371414,-2.20208983667212));
#40397=CARTESIAN_POINT('Ctrl Pts',(-20.8591912596,25.3310192219314,-2.19146034439946));
#40398=CARTESIAN_POINT('Ctrl Pts',(-20.9531635276924,25.4654772805208,-2.18209038457099));
#40399=CARTESIAN_POINT('Ctrl Pts',(-21.1776464334114,25.7395752964639,-2.16214986507381));
#40400=CARTESIAN_POINT('Ctrl Pts',(-21.3111478874068,25.875936023859,-2.15165689472751));
#40401=CARTESIAN_POINT('Ctrl Pts',(-21.5109245317899,26.0467497432315,-2.13664271577017));
#40402=CARTESIAN_POINT('Ctrl Pts',(-21.5675065351425,26.0919201679988,-2.13245995069935));
#40403=CARTESIAN_POINT('Ctrl Pts',(-21.6831327051265,26.1780146269689,-2.12399293140257));
#40404=CARTESIAN_POINT('Ctrl Pts',(-21.7421190237322,26.218945488239,-2.11971224727104));
#40405=CARTESIAN_POINT('Ctrl Pts',(-21.8105818006328,26.2631398676686,-2.11476567787262));
#40406=CARTESIAN_POINT('Ctrl Pts',(-21.8187679266023,26.2683719200408,-2.11417457120599));
#40407=CARTESIAN_POINT('Ctrl Pts',(-21.8335103672825,26.27770072931,-2.11311062104568));
#40408=CARTESIAN_POINT('Ctrl Pts',(-21.8400580270385,26.2818110766187,-2.11263828467855));
#40409=CARTESIAN_POINT('Ctrl Pts',(-21.8500668353751,26.288044095211,-2.11191655165509));
#40410=CARTESIAN_POINT('Ctrl Pts',(-21.8535173425892,26.2901838711706,-2.11166778764856));
#40411=CARTESIAN_POINT('Ctrl Pts',(-21.8595492099242,26.2939086719544,-2.11123300638141));
#40412=CARTESIAN_POINT('Ctrl Pts',(-21.8621287838072,26.2954965918736,-2.11104709614873));
#40413=CARTESIAN_POINT('Ctrl Pts',(-21.8674834557875,26.2987823903019,-2.110661238918));
#40414=CARTESIAN_POINT('Ctrl Pts',(-21.8702588927957,26.3004797076954,-2.11046127154123));
#40415=CARTESIAN_POINT('Ctrl Pts',(-21.8770097493999,26.3045941591153,-2.10997495048036));
#40416=CARTESIAN_POINT('Ctrl Pts',(-21.8809878342355,26.3070068875463,-2.10968843538709));
#40417=CARTESIAN_POINT('Ctrl Pts',(-21.8959417165296,26.3160322562407,-2.10861161956689));
#40418=CARTESIAN_POINT('Ctrl Pts',(-21.9069515820608,26.3225879621923,-2.10781923858378));
#40419=CARTESIAN_POINT('Ctrl Pts',(-21.9695602388023,26.3593636217945,-2.10331539435115));
#40420=CARTESIAN_POINT('Ctrl Pts',(-22.0219266568068,26.3881929669247,-2.09955607985897));
#40421=CARTESIAN_POINT('Ctrl Pts',(-22.0750363389647,26.4155369411741,-2.09574775951102));
#40422=CARTESIAN_POINT('Origin',(-23.5502525316942,23.5502525316942,-77.3107734492734));
#40423=CARTESIAN_POINT('',(-22.0750358767111,26.4155367031789,-0.597455529348901));
#40424=CARTESIAN_POINT('',(-22.0750363147453,26.4155369287046,-0.841310143832834));
#40425=CARTESIAN_POINT('',(-22.0750360153461,26.4155367745563,-77.3107734492734));
#40426=CARTESIAN_POINT('',(-26.7730021324148,23.5486483013339,-1.44183060332433));
#40427=CARTESIAN_POINT('Ctrl Pts',(-22.0750358767111,26.4155367031789,-0.597455529348901));
#40428=CARTESIAN_POINT('Ctrl Pts',(-21.9406891892397,26.3463671342851,-0.607650048982882));
#40429=CARTESIAN_POINT('Ctrl Pts',(-21.8111950680103,26.2677429624805,-0.617743844345608));
#40430=CARTESIAN_POINT('Ctrl Pts',(-21.6745161179815,26.1709367096955,-0.628341425636105));
#40431=CARTESIAN_POINT('Ctrl Pts',(-21.6615510212869,26.1616083642588,-0.629346007056065));
#40432=CARTESIAN_POINT('Ctrl Pts',(-21.6457756861704,26.1500791086699,-0.630566952953863));
#40433=CARTESIAN_POINT('Ctrl Pts',(-21.6428993559169,26.147969634968,-0.630789512356329));
#40434=CARTESIAN_POINT('Ctrl Pts',(-21.6381586429986,26.1444807217255,-0.631156228657627));
#40435=CARTESIAN_POINT('Ctrl Pts',(-21.63629224693,26.1431040449044,-0.631300576985442));
#40436=CARTESIAN_POINT('Ctrl Pts',(-21.6329601776115,26.1406407111871,-0.63155823229359));
#40437=CARTESIAN_POINT('Ctrl Pts',(-21.6314939444935,26.139554826827,-0.631671592924775));
#40438=CARTESIAN_POINT('Ctrl Pts',(-21.6283474816425,26.1372204331125,-0.631914821877224));
#40439=CARTESIAN_POINT('Ctrl Pts',(-21.6266675505145,26.1359715351094,-0.63204466191687));
#40440=CARTESIAN_POINT('Ctrl Pts',(-21.6221353912845,26.132595366367,-0.63239489012542));
#40441=CARTESIAN_POINT('Ctrl Pts',(-21.6192854567953,26.1304649994716,-0.632615060841247));
#40442=CARTESIAN_POINT('Ctrl Pts',(-21.6129963617318,26.1257475549872,-0.633100801028384));
#40443=CARTESIAN_POINT('Ctrl Pts',(-21.6095588361024,26.1231582943404,-0.63336621869832));
#40444=CARTESIAN_POINT('Ctrl Pts',(-21.5992409644101,26.1153540815471,-0.634162672166856));
#40445=CARTESIAN_POINT('Ctrl Pts',(-21.5923763096048,26.1101183093534,-0.634692286789618));
#40446=CARTESIAN_POINT('Ctrl Pts',(-21.5128320890189,26.0489416237836,-0.640827019622044));
#40447=CARTESIAN_POINT('Ctrl Pts',(-21.4425437125946,25.9899443682486,-0.646227012852222));
#40448=CARTESIAN_POINT('Ctrl Pts',(-21.0814050572507,25.6595433205295,-0.674441126662648));
#40449=CARTESIAN_POINT('Ctrl Pts',(-20.8401848157741,25.339078088967,-0.695486817408777));
#40450=CARTESIAN_POINT('Ctrl Pts',(-20.6550703130174,24.9660158531481,-0.720698091940841));
#40451=CARTESIAN_POINT('Ctrl Pts',(-20.6469204039708,24.9492265825701,-0.721832839008516));
#40452=CARTESIAN_POINT('Ctrl Pts',(-20.6363274092861,24.9269131295968,-0.723341464278263));
#40453=CARTESIAN_POINT('Ctrl Pts',(-20.6337532577105,24.9214512790999,-0.723710783115514));
#40454=CARTESIAN_POINT('Ctrl Pts',(-20.629779734269,24.9129584233236,-0.724285125859934));
#40455=CARTESIAN_POINT('Ctrl Pts',(-20.628369687679,24.9099324033173,-0.724489779711153));
#40456=CARTESIAN_POINT('Ctrl Pts',(-20.625555315277,24.9038680452123,-0.724899951916874));
#40457=CARTESIAN_POINT('Ctrl Pts',(-20.6241510159881,24.9008296993541,-0.725105470878797));
#40458=CARTESIAN_POINT('Ctrl Pts',(-20.6210253847441,24.8940393171884,-0.72556482186619));
#40459=CARTESIAN_POINT('Ctrl Pts',(-20.6193065255384,24.8902861551695,-0.725818738859921));
#40460=CARTESIAN_POINT('Ctrl Pts',(-20.6142975237022,24.8792931608235,-0.726562542065408));
#40461=CARTESIAN_POINT('Ctrl Pts',(-20.6110269792714,24.8720444793915,-0.727053102533168));
#40462=CARTESIAN_POINT('Ctrl Pts',(-20.5871629283512,24.8186267815638,-0.7306690533251));
#40463=CARTESIAN_POINT('Ctrl Pts',(-20.5676324657403,24.7719932194257,-0.733830681566581));
#40464=CARTESIAN_POINT('Ctrl Pts',(-20.5073010873557,24.6178586070316,-0.744304580837282));
#40465=CARTESIAN_POINT('Ctrl Pts',(-20.4711581791909,24.5086413524432,-0.751767525059768));
#40466=CARTESIAN_POINT('Ctrl Pts',(-20.3526157163248,24.0737225703439,-0.781600810601189));
#40467=CARTESIAN_POINT('Ctrl Pts',(-20.315494250577,23.7379292830332,-0.805123472645065));
#40468=CARTESIAN_POINT('Ctrl Pts',(-20.3312613925392,23.3944373816574,-0.826868117253289));
#40469=CARTESIAN_POINT('Ctrl Pts',(-20.3316604864376,23.3864002680407,-0.827375460647435));
#40470=CARTESIAN_POINT('Ctrl Pts',(-20.3325564618243,23.3696254120253,-0.828431242859504));
#40471=CARTESIAN_POINT('Ctrl Pts',(-20.3330588423977,23.3608880043832,-0.828979386343283));
#40472=CARTESIAN_POINT('Ctrl Pts',(-20.3337894704851,23.3490243991397,-0.829721142296514));
#40473=CARTESIAN_POINT('Ctrl Pts',(-20.3339866890196,23.3458964334275,-0.829916477037895));
#40474=CARTESIAN_POINT('Ctrl Pts',(-20.3343051639504,23.3409599716785,-0.830224368877319));
#40475=CARTESIAN_POINT('Ctrl Pts',(-20.3344233828609,23.3391512921675,-0.83033709750462));
#40476=CARTESIAN_POINT('Ctrl Pts',(-20.3346648922272,23.3355036260952,-0.830564280117797));
#40477=CARTESIAN_POINT('Ctrl Pts',(-20.3347882335411,23.3336646583821,-0.83067872994329));
#40478=CARTESIAN_POINT('Ctrl Pts',(-20.3350746513123,23.3294484607367,-0.830940937423881));
#40479=CARTESIAN_POINT('Ctrl Pts',(-20.3352387865152,23.3270713079165,-0.831088634373186));
#40480=CARTESIAN_POINT('Ctrl Pts',(-20.3355888746903,23.322081554044,-0.831398368553348));
#40481=CARTESIAN_POINT('Ctrl Pts',(-20.3357753766395,23.3194689914439,-0.831560374770081));
#40482=CARTESIAN_POINT('Ctrl Pts',(-20.3362768529567,23.3125627469246,-0.831988201876065));
#40483=CARTESIAN_POINT('Ctrl Pts',(-20.3365972477742,23.3082694456398,-0.832253720882407));
#40484=CARTESIAN_POINT('Ctrl Pts',(-20.3375863336016,23.2953641744624,-0.833050552740466));
#40485=CARTESIAN_POINT('Ctrl Pts',(-20.3382810523757,23.2867541541111,-0.833580442814485));
#40486=CARTESIAN_POINT('Ctrl Pts',(-20.3408866088912,23.2560047962555,-0.835467002141052));
#40487=CARTESIAN_POINT('Ctrl Pts',(-20.3429918478851,23.233881983798,-0.836813438138309));
#40488=CARTESIAN_POINT('Ctrl Pts',(-20.354412246798,23.1257439264778,-0.843349452674268));
#40489=CARTESIAN_POINT('Ctrl Pts',(-20.3669604263103,23.0400990174421,-0.848385321555301));
#40490=CARTESIAN_POINT('Ctrl Pts',(-20.4356552978211,22.6745422818763,-0.869663373985702));
#40491=CARTESIAN_POINT('Ctrl Pts',(-20.5253974447585,22.4022763627015,-0.885077981120781));
#40492=CARTESIAN_POINT('Ctrl Pts',(-20.6605133533898,22.1233238076916,-0.903067437832979));
#40493=CARTESIAN_POINT('Ctrl Pts',(-20.6714470862214,22.1013918524545,-0.904496619908667));
#40494=CARTESIAN_POINT('Ctrl Pts',(-20.6909882385076,22.0632889276861,-0.907007288038405));
#40495=CARTESIAN_POINT('Ctrl Pts',(-20.6994854571633,22.0470625482935,-0.908085382973898));
#40496=CARTESIAN_POINT('Ctrl Pts',(-20.7102045944783,22.0270109813662,-0.909429191375002));
#40497=CARTESIAN_POINT('Ctrl Pts',(-20.7122967813345,22.0231165635955,-0.909690731045899));
#40498=CARTESIAN_POINT('Ctrl Pts',(-20.7162993374321,22.0157027962459,-0.910189670847715));
#40499=CARTESIAN_POINT('Ctrl Pts',(-20.718208267084,22.012182676025,-0.91042702391303));
#40500=CARTESIAN_POINT('Ctrl Pts',(-20.72269401461,22.003947494906,-0.91098337019839));
#40501=CARTESIAN_POINT('Ctrl Pts',(-20.7252760685309,21.9992353117997,-0.911302534550945));
#40502=CARTESIAN_POINT('Ctrl Pts',(-20.7311938006479,21.9884993996366,-0.912031593763147));
#40503=CARTESIAN_POINT('Ctrl Pts',(-20.7345370160915,21.9824798732024,-0.912441738014669));
#40504=CARTESIAN_POINT('Ctrl Pts',(-20.7394294034469,21.9737371592558,-0.913039446104469));
#40505=CARTESIAN_POINT('Ctrl Pts',(-20.7409633103103,21.9710054172945,-0.913226493134887));
#40506=CARTESIAN_POINT('Ctrl Pts',(-20.7431076351569,21.9671995892408,-0.913487488154249));
#40507=CARTESIAN_POINT('Ctrl Pts',(-20.7437146943713,21.9661236049858,-0.913561321737854));
#40508=CARTESIAN_POINT('Ctrl Pts',(-20.747695947375,21.9590764905902,-0.914045187491566));
#40509=CARTESIAN_POINT('Ctrl Pts',(-20.7510885576144,21.9531158289558,-0.914455847506404));
#40510=CARTESIAN_POINT('Ctrl Pts',(-20.7575034365023,21.9419284018101,-0.915229256616018));
#40511=CARTESIAN_POINT('Ctrl Pts',(-20.7605214202229,21.9366992042798,-0.915591855986747));
#40512=CARTESIAN_POINT('Ctrl Pts',(-20.7763256130222,21.9094924909312,-0.917484170986884));
#40513=CARTESIAN_POINT('Ctrl Pts',(-20.7893566147258,21.8876588530324,-0.919022436824428));
#40514=CARTESIAN_POINT('Ctrl Pts',(-20.8080175080907,21.8572166955915,-0.921195966161289));
#40515=CARTESIAN_POINT('Ctrl Pts',(-20.8134325600513,21.8484770747166,-0.921823334741975));
#40516=CARTESIAN_POINT('Ctrl Pts',(-20.8210792677051,21.8362665682698,-0.922704651194728));
#40517=CARTESIAN_POINT('Ctrl Pts',(-20.8232759508806,21.8327737646856,-0.922957303365962));
#40518=CARTESIAN_POINT('Ctrl Pts',(-20.8273096031884,21.8263873635396,-0.923420280947412));
#40519=CARTESIAN_POINT('Ctrl Pts',(-20.8291444949307,21.8234924551346,-0.923630528991319));
#40520=CARTESIAN_POINT('Ctrl Pts',(-20.8328635724077,21.8176455159188,-0.924055952912407));
#40521=CARTESIAN_POINT('Ctrl Pts',(-20.8347479583385,21.8146936190968,-0.924271136033673));
#40522=CARTESIAN_POINT('Ctrl Pts',(-20.8393828470093,21.8074590782071,-0.924799501662318));
#40523=CARTESIAN_POINT('Ctrl Pts',(-20.8421386842436,21.803179877901,-0.925112883111043));
#40524=CARTESIAN_POINT('Ctrl Pts',(-20.8521345947711,21.7877389390363,-0.92624678959131));
#40525=CARTESIAN_POINT('Ctrl Pts',(-20.8594335547906,21.7766156492251,-0.927069519156938));
#40526=CARTESIAN_POINT('Ctrl Pts',(-20.9638966458085,21.619547598452,-0.938771732582543));
#40527=CARTESIAN_POINT('Ctrl Pts',(-21.0727263883099,21.4817496818975,-0.950105527629853));
#40528=CARTESIAN_POINT('Ctrl Pts',(-21.2162719445651,21.3276641619678,-0.964114602848038));
#40529=CARTESIAN_POINT('Ctrl Pts',(-21.240763950178,21.3022252100691,-0.966474950371078));
#40530=CARTESIAN_POINT('Ctrl Pts',(-21.4640350960089,21.0778219452219,-0.987714141418737));
#40531=CARTESIAN_POINT('Ctrl Pts',(-21.6876485439697,20.9052693749875,-1.00718131785204));
#40532=CARTESIAN_POINT('Ctrl Pts',(-21.9451020023631,20.755635931005,-1.02603150631787));
#40533=CARTESIAN_POINT('Ctrl Pts',(-21.9594407340496,20.7474489319291,-1.02707029475024));
#40534=CARTESIAN_POINT('Ctrl Pts',(-21.9769908604176,20.7376063916341,-1.02832771836351));
#40535=CARTESIAN_POINT('Ctrl Pts',(-21.9801425929372,20.7358457778589,-1.02855298473468));
#40536=CARTESIAN_POINT('Ctrl Pts',(-21.9853356326806,20.7329562918876,-1.0289232421387));
#40537=CARTESIAN_POINT('Ctrl Pts',(-21.9873752073292,20.7318243398283,-1.02906843100839));
#40538=CARTESIAN_POINT('Ctrl Pts',(-21.9909596219089,20.729840097868,-1.02932318390013));
#40539=CARTESIAN_POINT('Ctrl Pts',(-21.9925039301707,20.728986863613,-1.02943280906032));
#40540=CARTESIAN_POINT('Ctrl Pts',(-21.9958558592982,20.7271385054723,-1.02967046320114));
#40541=CARTESIAN_POINT('Ctrl Pts',(-21.9976637312556,20.7261438515941,-1.02979846149781));
#40542=CARTESIAN_POINT('Ctrl Pts',(-22.0024749013599,20.7235028611883,-1.03013861681776));
#40543=CARTESIAN_POINT('Ctrl Pts',(-22.0054798812383,20.7218595690153,-1.03035057745891));
#40544=CARTESIAN_POINT('Ctrl Pts',(-22.0120955278317,20.7182554491524,-1.03081614673436));
#40545=CARTESIAN_POINT('Ctrl Pts',(-22.0157073431359,20.7162967259754,-1.03106962177661));
#40546=CARTESIAN_POINT('Ctrl Pts',(-22.0264533675234,20.7104956177878,-1.03182171458604));
#40547=CARTESIAN_POINT('Ctrl Pts',(-22.0335983977896,20.7066731914664,-1.03231909230179));
#40548=CARTESIAN_POINT('Ctrl Pts',(-22.0587590609275,20.6933346289821,-1.03406140800573));
#40549=CARTESIAN_POINT('Ctrl Pts',(-22.0768508757845,20.6839621967392,-1.03529777707063));
#40550=CARTESIAN_POINT('Ctrl Pts',(-22.1319873841863,20.6560588418074,-1.03901978519361));
#40551=CARTESIAN_POINT('Ctrl Pts',(-22.1693028278144,20.6380692630539,-1.04147649304671));
#40552=CARTESIAN_POINT('Ctrl Pts',(-22.3056852475059,20.5755312400114,-1.05026862483504));
#40553=CARTESIAN_POINT('Ctrl Pts',(-22.4066469985118,20.5352758713674,-1.05642738341751));
#40554=CARTESIAN_POINT('Ctrl Pts',(-22.7189746396144,20.4286976879988,-1.07496349951045));
#40555=CARTESIAN_POINT('Ctrl Pts',(-22.9352908868415,20.3789837441137,-1.08715031691132));
#40556=CARTESIAN_POINT('Ctrl Pts',(-23.1807716990753,20.3486472796386,-1.10148829916147));
#40557=CARTESIAN_POINT('Ctrl Pts',(-23.2065879277729,20.3457733435946,-1.10300162827251));
#40558=CARTESIAN_POINT('Ctrl Pts',(-23.2526112274924,20.3412124463707,-1.10571127670561));
#40559=CARTESIAN_POINT('Ctrl Pts',(-23.2728049353553,20.3394035129084,-1.10690422144167));
#40560=CARTESIAN_POINT('Ctrl Pts',(-23.2976821369309,20.3374114698292,-1.10837941269145));
#40561=CARTESIAN_POINT('Ctrl Pts',(-23.30235100065,20.3370478504293,-1.1086565122514));
#40562=CARTESIAN_POINT('Ctrl Pts',(-23.3110498499032,20.3363894407713,-1.10917325315885));
#40563=CARTESIAN_POINT('Ctrl Pts',(-23.3150796334605,20.336092050651,-1.10941281949309));
#40564=CARTESIAN_POINT('Ctrl Pts',(-23.3229245049975,20.3355279467843,-1.10987955315879));
#40565=CARTESIAN_POINT('Ctrl Pts',(-23.326739530678,20.3352604435634,-1.1101066972761));
#40566=CARTESIAN_POINT('Ctrl Pts',(-23.3833570608287,20.3313917801237,-1.11348020019779));
#40567=CARTESIAN_POINT('Ctrl Pts',(-23.4362374200321,20.3290852448379,-1.11666391026));
#40568=CARTESIAN_POINT('Ctrl Pts',(-23.497878471502,20.3279163042374,-1.12042104157735));
#40569=CARTESIAN_POINT('Ctrl Pts',(-23.5066091630582,20.3277862310213,-1.12095426105015));
#40570=CARTESIAN_POINT('Ctrl Pts',(-23.5196278613997,20.3276451900846,-1.12175099456063));
#40571=CARTESIAN_POINT('Ctrl Pts',(-23.5239155864056,20.3276072962303,-1.1220136629853));
#40572=CARTESIAN_POINT('Ctrl Pts',(-23.5315658050816,20.3275549543021,-1.12248279392042));
#40573=CARTESIAN_POINT('Ctrl Pts',(-23.5349282760058,20.3275372113267,-1.12268915268429));
#40574=CARTESIAN_POINT('Ctrl Pts',(-23.5420200070604,20.3275108890047,-1.12312472780098));
#40575=CARTESIAN_POINT('Ctrl Pts',(-23.545749264336,20.3275035203091,-1.1233539818622));
#40576=CARTESIAN_POINT('Ctrl Pts',(-23.5556055621826,20.3275011530905,-1.12396043196195));
#40577=CARTESIAN_POINT('Ctrl Pts',(-23.561732568387,20.327517154541,-1.124337972828));
#40578=CARTESIAN_POINT('Ctrl Pts',(-23.5895106302914,20.3276689173489,-1.12605216208167));
#40579=CARTESIAN_POINT('Ctrl Pts',(-23.6111596215759,20.3280053904425,-1.12739509630084));
#40580=CARTESIAN_POINT('Ctrl Pts',(-23.7702022688411,20.3320805995236,-1.13731393118291));
#40581=CARTESIAN_POINT('Ctrl Pts',(-23.9072165014444,20.3443866249787,-1.14615936893646));
#40582=CARTESIAN_POINT('Ctrl Pts',(-24.0816243669733,20.3713709488588,-1.15780325421886));
#40583=CARTESIAN_POINT('Ctrl Pts',(-24.1201236074863,20.3780465249892,-1.16039726135637));
#40584=CARTESIAN_POINT('Ctrl Pts',(-24.1887013527223,20.3912262513658,-1.16505732630796));
#40585=CARTESIAN_POINT('Ctrl Pts',(-24.2188265272765,20.3974644495236,-1.16711813021863));
#40586=CARTESIAN_POINT('Ctrl Pts',(-24.2737318902162,20.4096563409319,-1.17089712014989));
#40587=CARTESIAN_POINT('Ctrl Pts',(-24.2985398455746,20.4154745670875,-1.17261324690678));
#40588=CARTESIAN_POINT('Ctrl Pts',(-24.3443584746063,20.4267953253297,-1.17579742845327));
#40589=CARTESIAN_POINT('Ctrl Pts',(-24.3653876833665,20.4322172779897,-1.17726460484576));
#40590=CARTESIAN_POINT('Ctrl Pts',(-24.4045734455441,20.44274404526,-1.18000824153349));
#40591=CARTESIAN_POINT('Ctrl Pts',(-24.4227431777805,20.4477965229126,-1.18128434308218));
#40592=CARTESIAN_POINT('Ctrl Pts',(-24.4568296556016,20.4575981152262,-1.18368494701112));
#40593=CARTESIAN_POINT('Ctrl Pts',(-24.4727561152681,20.4623113794935,-1.18480933968115));
#40594=CARTESIAN_POINT('Ctrl Pts',(-24.6372351010361,20.5123732204015,-1.19644671620746));
#40595=CARTESIAN_POINT('Ctrl Pts',(-24.7823733402676,20.5682854026854,-1.20694128480268));
#40596=CARTESIAN_POINT('Ctrl Pts',(-24.9677942310842,20.6555759029267,-1.22022291435769));
#40597=CARTESIAN_POINT('Ctrl Pts',(-25.0121754102516,20.6777345716642,-1.22339090242088));
#40598=CARTESIAN_POINT('Ctrl Pts',(-25.0609626632634,20.7035169305174,-1.22684658699875));
#40599=CARTESIAN_POINT('Ctrl Pts',(-25.065888267137,20.7061363239429,-1.22719516660556));
#40600=CARTESIAN_POINT('Ctrl Pts',(-25.0728443316413,20.7098587012378,-1.22768697476471));
#40601=CARTESIAN_POINT('Ctrl Pts',(-25.0748804097663,20.7109510797789,-1.22783087322785));
#40602=CARTESIAN_POINT('Ctrl Pts',(-25.0785980496897,20.7129507869062,-1.22809350924025));
#40603=CARTESIAN_POINT('Ctrl Pts',(-25.0802799814418,20.7138574223293,-1.22821229122766));
#40604=CARTESIAN_POINT('Ctrl Pts',(-25.0835018178565,20.7155978339504,-1.22843974754709));
#40605=CARTESIAN_POINT('Ctrl Pts',(-25.0850418488813,20.7164313692279,-1.22854843732257));
#40606=CARTESIAN_POINT('Ctrl Pts',(-25.0889416553437,20.7185462344983,-1.22882358756877));
#40607=CARTESIAN_POINT('Ctrl Pts',(-25.0913005160186,20.7198292624725,-1.22898993873865));
#40608=CARTESIAN_POINT('Ctrl Pts',(-25.0993892850173,20.7242420029142,-1.22956011566033));
#40609=CARTESIAN_POINT('Ctrl Pts',(-25.105111333713,20.7273862052771,-1.22996301802266));
#40610=CARTESIAN_POINT('Ctrl Pts',(-25.1188017422576,20.7349631897336,-1.23092601945571));
#40611=CARTESIAN_POINT('Ctrl Pts',(-25.1267609731641,20.7394124715891,-1.23148509062852));
#40612=CARTESIAN_POINT('Ctrl Pts',(-25.1555292912804,20.7556548551948,-1.23350335149589));
#40613=CARTESIAN_POINT('Ctrl Pts',(-25.1762263928661,20.7676460689092,-1.23495065176322));
#40614=CARTESIAN_POINT('Ctrl Pts',(-25.2659516747629,20.8209729160657,-1.24121279745851));
#40615=CARTESIAN_POINT('Ctrl Pts',(-25.3335566898949,20.8646577918024,-1.24589971744871));
#40616=CARTESIAN_POINT('Ctrl Pts',(-25.5369947641291,21.0071887534181,-1.26013048621562));
#40617=CARTESIAN_POINT('Ctrl Pts',(-25.6667930128477,21.1141532379139,-1.26940474851507));
#40618=CARTESIAN_POINT('Ctrl Pts',(-25.8927779845824,21.3321407140563,-1.2870110877469));
#40619=CARTESIAN_POINT('Ctrl Pts',(-25.9908668450641,21.4405507302487,-1.29528699558577));
#40620=CARTESIAN_POINT('Ctrl Pts',(-26.0915456383318,21.5682780255872,-1.30482584102547));
#40621=CARTESIAN_POINT('Ctrl Pts',(-26.1017294128243,21.5814053289098,-1.30580374199393));
#40622=CARTESIAN_POINT('Ctrl Pts',(-26.1516974453986,21.6468549604466,-1.31066854642246));
#40623=CARTESIAN_POINT('Ctrl Pts',(-26.1899737391699,21.7003041654103,-1.31460798484887));
#40624=CARTESIAN_POINT('Ctrl Pts',(-26.2312545835782,21.761841015329,-1.31912179449434));
#40625=CARTESIAN_POINT('Ctrl Pts',(-26.2358947417348,21.768816686193,-1.31963315486224));
#40626=CARTESIAN_POINT('Ctrl Pts',(-26.2428650542993,21.7793844683761,-1.3204073972785));
#40627=CARTESIAN_POINT('Ctrl Pts',(-26.2452153620788,21.7829632975486,-1.32066952185399));
#40628=CARTESIAN_POINT('Ctrl Pts',(-26.2492847572197,21.7891867868779,-1.32112522185629));
#40629=CARTESIAN_POINT('Ctrl Pts',(-26.2510071109343,21.7918293134111,-1.32131867463097));
#40630=CARTESIAN_POINT('Ctrl Pts',(-26.2545858154601,21.7973376131846,-1.3217218427001));
#40631=CARTESIAN_POINT('Ctrl Pts',(-26.2564414958837,21.8002038148934,-1.3219315826948));
#40632=CARTESIAN_POINT('Ctrl Pts',(-26.2608058199096,21.8069682966453,-1.32242648300178));
#40633=CARTESIAN_POINT('Ctrl Pts',(-26.2633106093111,21.8108690433443,-1.32271178660218));
#40634=CARTESIAN_POINT('Ctrl Pts',(-26.2714956187075,21.823676377488,-1.32364826854078));
#40635=CARTESIAN_POINT('Ctrl Pts',(-26.2771404191291,21.8326054200945,-1.32430076179848));
#40636=CARTESIAN_POINT('Ctrl Pts',(-26.3572880787015,21.9607752441523,-1.33366150852107));
#40637=CARTESIAN_POINT('Ctrl Pts',(-26.4239429853942,22.0847219040408,-1.34265862620585));
#40638=CARTESIAN_POINT('Ctrl Pts',(-26.6040659631666,22.4795408494138,-1.37118337491613));
#40639=CARTESIAN_POINT('Ctrl Pts',(-26.6888076315404,22.7618100676,-1.39152292120949));
#40640=CARTESIAN_POINT('Ctrl Pts',(-26.73606606423,23.0635739890314,-1.41158869683743));
#40641=CARTESIAN_POINT('Ctrl Pts',(-26.7378702580484,23.0755346090853,-1.41238107168448));
#40642=CARTESIAN_POINT('Ctrl Pts',(-26.7410447006124,23.0974135554134,-1.41382482055198));
#40643=CARTESIAN_POINT('Ctrl Pts',(-26.7424361439456,23.107328617316,-1.41447696056039));
#40644=CARTESIAN_POINT('Ctrl Pts',(-26.7449193965863,23.1256433855745,-1.41567744416891));
#40645=CARTESIAN_POINT('Ctrl Pts',(-26.7460243371001,23.1340411967884,-1.41622629886083));
#40646=CARTESIAN_POINT('Ctrl Pts',(-26.7528256392466,23.1873570625371,-1.41970031813369));
#40647=CARTESIAN_POINT('Ctrl Pts',(-26.7576083312586,23.2323894647162,-1.42258720363565));
#40648=CARTESIAN_POINT('Ctrl Pts',(-26.7618608959266,23.2824579619789,-1.42573349632634));
#40649=CARTESIAN_POINT('Ctrl Pts',(-26.762269679851,23.287406459806,-1.42604377223927));
#40650=CARTESIAN_POINT('Ctrl Pts',(-26.762863805056,23.2948070085089,-1.42650674789126));
#40651=CARTESIAN_POINT('Ctrl Pts',(-26.7630577767862,23.2972583296754,-1.42665993006355));
#40652=CARTESIAN_POINT('Ctrl Pts',(-26.7633869324547,23.3014794711676,-1.42692340942656));
#40653=CARTESIAN_POINT('Ctrl Pts',(-26.7635234598359,23.3032491807273,-1.42703378265865));
#40654=CARTESIAN_POINT('Ctrl Pts',(-26.7637944697061,23.3068003458606,-1.42725507940636));
#40655=CARTESIAN_POINT('Ctrl Pts',(-26.7639289326623,23.3085817969736,-1.42736600128482));
#40656=CARTESIAN_POINT('Ctrl Pts',(-26.7641997370059,23.312209778776,-1.42759171088979));
#40657=CARTESIAN_POINT('Ctrl Pts',(-26.7643359686806,23.314056319026,-1.42770649246917));
#40658=CARTESIAN_POINT('Ctrl Pts',(-26.7646473351462,23.3183268615568,-1.42797172582079));
#40659=CARTESIAN_POINT('Ctrl Pts',(-26.7648213197668,23.3207509505021,-1.4281221126366));
#40660=CARTESIAN_POINT('Ctrl Pts',(-26.7652640380277,23.3270185262977,-1.42851051552325));
#40661=CARTESIAN_POINT('Ctrl Pts',(-26.7655286226081,23.3308623163659,-1.42874829986085));
#40662=CARTESIAN_POINT('Ctrl Pts',(-26.7705596293757,23.4059153305016,-1.43338326392699));
#40663=CARTESIAN_POINT('Ctrl Pts',(-26.7729666008245,23.4772686408052,-1.43764991829428));
#40664=CARTESIAN_POINT('Ctrl Pts',(-26.7730021324148,23.5486483013339,-1.44183060332433));
#40665=CARTESIAN_POINT('Ctrl Pts',(-26.7730021302442,23.5486439466878,-1.44183034827392));
#40666=CARTESIAN_POINT('Ctrl Pts',(-26.7731688677631,23.882697335105,-1.4613957704159));
#40667=CARTESIAN_POINT('Ctrl Pts',(-26.7214006904693,24.2147936159358,-1.4791387893778));
#40668=CARTESIAN_POINT('Ctrl Pts',(-26.5997245547146,24.5947803069446,-1.502308737071));
#40669=CARTESIAN_POINT('Ctrl Pts',(-26.5781038952386,24.6558895429473,-1.50612049904104));
#40670=CARTESIAN_POINT('Ctrl Pts',(-26.5386957085977,24.7574273031958,-1.51262655607523));
#40671=CARTESIAN_POINT('Ctrl Pts',(-26.521892637583,24.7982182115299,-1.5152882471269));
#40672=CARTESIAN_POINT('Ctrl Pts',(-26.5011905884798,24.8456833586222,-1.51844656978587));
#40673=CARTESIAN_POINT('Ctrl Pts',(-26.4980978445266,24.8527057755179,-1.51891542690475));
#40674=CARTESIAN_POINT('Ctrl Pts',(-26.4933267199962,24.8634350940985,-1.51963423409926));
#40675=CARTESIAN_POINT('Ctrl Pts',(-26.4916663343527,24.8671500073321,-1.51988356550995));
#40676=CARTESIAN_POINT('Ctrl Pts',(-26.4886287816072,24.8739117613638,-1.52033821790734));
#40677=CARTESIAN_POINT('Ctrl Pts',(-26.487253898034,24.876959626846,-1.5205434600195));
#40678=CARTESIAN_POINT('Ctrl Pts',(-26.4844828434696,24.8830771307915,-1.52095603030087));
#40679=CARTESIAN_POINT('Ctrl Pts',(-26.4830865927558,24.8861467283428,-1.52116336102295));
#40680=CARTESIAN_POINT('Ctrl Pts',(-26.4791071873032,24.8948589726428,-1.52175271090289));
#40681=CARTESIAN_POINT('Ctrl Pts',(-26.4765125588,24.9004963347251,-1.52213512622008));
#40682=CARTESIAN_POINT('Ctrl Pts',(-26.46548954095,24.9242650965224,-1.52375205096208));
#40683=CARTESIAN_POINT('Ctrl Pts',(-26.4569089360643,24.9423250392733,-1.52499182731233));
#40684=CARTESIAN_POINT('Ctrl Pts',(-26.2795236178546,25.3068837479351,-1.55025027321395));
#40685=CARTESIAN_POINT('Ctrl Pts',(-26.05009296358,25.6203481629741,-1.57680513659364));
#40686=CARTESIAN_POINT('Ctrl Pts',(-25.7261133975403,25.9283973336497,-1.60659851310883));
#40687=CARTESIAN_POINT('Ctrl Pts',(-25.6800690334475,25.9697206084309,-1.61067861131474));
#40688=CARTESIAN_POINT('Ctrl Pts',(-25.6064119191038,26.0320920352255,-1.61693537097136));
#40689=CARTESIAN_POINT('Ctrl Pts',(-25.5796017479016,26.0540617753315,-1.61915967689));
#40690=CARTESIAN_POINT('Ctrl Pts',(-25.5430636961239,26.0830305399558,-1.62211471480445));
#40691=CARTESIAN_POINT('Ctrl Pts',(-25.5336447073969,26.090413208489,-1.62286980226507));
#40692=CARTESIAN_POINT('Ctrl Pts',(-25.5198596502624,26.1010946078229,-1.62396494125104));
#40693=CARTESIAN_POINT('Ctrl Pts',(-25.5155260913321,26.1044348540204,-1.62430779354336));
#40694=CARTESIAN_POINT('Ctrl Pts',(-25.5077496738672,26.1103972989696,-1.62492045489268));
#40695=CARTESIAN_POINT('Ctrl Pts',(-25.5043100136147,26.1130236195785,-1.6251905492195));
#40696=CARTESIAN_POINT('Ctrl Pts',(-25.4990630010683,26.1170132220948,-1.62560118456961));
#40697=CARTESIAN_POINT('Ctrl Pts',(-25.4972595025747,26.1183815282102,-1.62574208048134));
#40698=CARTESIAN_POINT('Ctrl Pts',(-25.4939724484223,26.1208699484578,-1.62599842485238));
#40699=CARTESIAN_POINT('Ctrl Pts',(-25.4924893693122,26.1219906763563,-1.6261139168333));
#40700=CARTESIAN_POINT('Ctrl Pts',(-25.4892842238448,26.1244083752498,-1.62636314967497));
#40701=CARTESIAN_POINT('Ctrl Pts',(-25.4875618302637,26.1257048981374,-1.62649685854838));
#40702=CARTESIAN_POINT('Ctrl Pts',(-25.4829003699228,26.1292064661729,-1.62685812255144));
#40703=CARTESIAN_POINT('Ctrl Pts',(-25.4799588197479,26.1314082234219,-1.62708544526047));
#40704=CARTESIAN_POINT('Ctrl Pts',(-25.4662239345746,26.1416522150239,-1.62814389137584));
#40705=CARTESIAN_POINT('Ctrl Pts',(-25.4553838437218,26.1496319642393,-1.62897067962835));
#40706=CARTESIAN_POINT('Ctrl Pts',(-25.4433578199757,26.1583690746709,-1.62987887947253));
#40707=CARTESIAN_POINT('Ctrl Pts',(-25.4422212456592,26.1591936808315,-1.6299646243613));
#40708=CARTESIAN_POINT('Ctrl Pts',(-25.4340174663101,26.1651374976655,-1.63058289324737));
#40709=CARTESIAN_POINT('Ctrl Pts',(-25.4269299474096,26.170228790237,-1.63111362986479));
#40710=CARTESIAN_POINT('Ctrl Pts',(-25.415555145862,26.1783299958641,-1.63196012980029));
#40711=CARTESIAN_POINT('Ctrl Pts',(-25.4112811118018,26.1813583115683,-1.6322770127559));
#40712=CARTESIAN_POINT('Ctrl Pts',(-25.3160731870645,26.2484686922482,-1.63930999773033));
#40713=CARTESIAN_POINT('Ctrl Pts',(-25.221879049007,26.3078172271735,-1.64574545177314));
#40714=CARTESIAN_POINT('Ctrl Pts',(-25.0677921524255,26.3940983649729,-1.65577689716675));
#40715=CARTESIAN_POINT('Ctrl Pts',(-25.0098309996988,26.4242770148866,-1.65944560441169));
#40716=CARTESIAN_POINT('Ctrl Pts',(-24.8384490518839,26.5069877379262,-1.67009704450526));
#40717=CARTESIAN_POINT('Ctrl Pts',(-24.7228437804965,26.5547096218153,-1.67704280289335));
#40718=CARTESIAN_POINT('Ctrl Pts',(-24.4809946756595,26.6384545569573,-1.69152440631513));
#40719=CARTESIAN_POINT('Ctrl Pts',(-24.354741598107,26.6737225150426,-1.69906009168216));
#40720=CARTESIAN_POINT('Ctrl Pts',(-24.1731414815125,26.7127085089994,-1.71009704194022));
#40721=CARTESIAN_POINT('Ctrl Pts',(-24.1192996560617,26.7228387428969,-1.71339236847744));
#40722=CARTESIAN_POINT('Ctrl Pts',(-24.0572202712967,26.7328877732047,-1.71722660705486));
#40723=CARTESIAN_POINT('Ctrl Pts',(-24.0492075501952,26.7341537954143,-1.717722156424));
#40724=CARTESIAN_POINT('Ctrl Pts',(-24.0370773565378,26.7360234697395,-1.71847337212975));
#40725=CARTESIAN_POINT('Ctrl Pts',(-24.0329633126662,26.7366494281045,-1.71872832969818));
#40726=CARTESIAN_POINT('Ctrl Pts',(-24.0258503815691,26.7377175803746,-1.71916944620626));
#40727=CARTESIAN_POINT('Ctrl Pts',(-24.0228520544526,26.7381635157638,-1.71935548613726));
#40728=CARTESIAN_POINT('Ctrl Pts',(-24.0166426101538,26.739078081662,-1.71974096822388));
#40729=CARTESIAN_POINT('Ctrl Pts',(-24.0134314064034,26.7395460934891,-1.71994042979302));
#40730=CARTESIAN_POINT('Ctrl Pts',(-24.005643549946,26.7406691123034,-1.72042443636991));
#40731=CARTESIAN_POINT('Ctrl Pts',(-24.0010661933281,26.7413191213266,-1.72070913959362));
#40732=CARTESIAN_POINT('Ctrl Pts',(-23.9839850241543,26.7437072525439,-1.72177240947607));
#40733=CARTESIAN_POINT('Ctrl Pts',(-23.9714725588401,26.745381732615,-1.72255298992911));
#40734=CARTESIAN_POINT('Ctrl Pts',(-23.7548825809245,26.7730725068247,-1.73609516435349));
#40735=CARTESIAN_POINT('Ctrl Pts',(-23.5488261779048,26.7795575172112,-1.74949223434172));
#40736=CARTESIAN_POINT('Ctrl Pts',(-23.1585547512216,26.754479492105,-1.775700621787));
#40737=CARTESIAN_POINT('Ctrl Pts',(-22.974894936122,26.7266434606477,-1.78838123610047));
#40738=CARTESIAN_POINT('Ctrl Pts',(-22.7524258049084,26.672987974116,-1.80364754112412));
#40739=CARTESIAN_POINT('Ctrl Pts',(-22.7104104384663,26.6619513714923,-1.80652510275852));
#40740=CARTESIAN_POINT('Ctrl Pts',(-22.6230729215237,26.6371115853815,-1.81247862326149));
#40741=CARTESIAN_POINT('Ctrl Pts',(-22.5778047791555,26.6231512822985,-1.81554834664257));
#40742=CARTESIAN_POINT('Ctrl Pts',(-22.5164159832112,26.6027269101449,-1.81967421457841));
#40743=CARTESIAN_POINT('Ctrl Pts',(-22.5000175781196,26.5971237814988,-1.82077267017262));
#40744=CARTESIAN_POINT('Ctrl Pts',(-22.4768789995183,26.5890086149181,-1.82231663301923));
#40745=CARTESIAN_POINT('Ctrl Pts',(-22.4701011524368,26.5866059816586,-1.8227681662272));
#40746=CARTESIAN_POINT('Ctrl Pts',(-22.4597853303753,26.5829102824631,-1.82345421925334));
#40747=CARTESIAN_POINT('Ctrl Pts',(-22.4562415407407,26.5816336859645,-1.82368968666073));
#40748=CARTESIAN_POINT('Ctrl Pts',(-22.4496978566411,26.5792634535825,-1.82412407941771));
#40749=CARTESIAN_POINT('Ctrl Pts',(-22.4466973393016,26.5781715687978,-1.82432310752258));
#40750=CARTESIAN_POINT('Ctrl Pts',(-22.4418114825409,26.5763853839519,-1.82464693117836));
#40751=CARTESIAN_POINT('Ctrl Pts',(-22.4399251701813,26.5756937803868,-1.82477188818677));
#40752=CARTESIAN_POINT('Ctrl Pts',(-22.4362688521869,26.5743493362595,-1.8250139725686));
#40753=CARTESIAN_POINT('Ctrl Pts',(-22.4344987781511,26.5736967073091,-1.82513111186687));
#40754=CARTESIAN_POINT('Ctrl Pts',(-22.430429216126,26.572192193192,-1.82540029617754));
#40755=CARTESIAN_POINT('Ctrl Pts',(-22.4281301210197,26.5713392354122,-1.82555227643369));
#40756=CARTESIAN_POINT('Ctrl Pts',(-22.4208344318647,26.568623078135,-1.82603425795931));
#40757=CARTESIAN_POINT('Ctrl Pts',(-22.4158414544478,26.5667500882374,-1.82636367307461));
#40758=CARTESIAN_POINT('Ctrl Pts',(-22.3732834351261,26.5506649071019,-1.82916789367756));
#40759=CARTESIAN_POINT('Ctrl Pts',(-22.3359803653261,26.5357632328176,-1.83160207573915));
#40760=CARTESIAN_POINT('Ctrl Pts',(-22.2229924279091,26.4881589839944,-1.83893034184878));
#40761=CARTESIAN_POINT('Ctrl Pts',(-22.1482954939807,26.4532550560576,-1.84371331314543));
#40762=CARTESIAN_POINT('Ctrl Pts',(-22.0750359636318,26.4155367479307,-1.84841977781534));
#40763=CARTESIAN_POINT('Ctrl Pts',(-22.0750363389647,26.4155369411741,-2.09574775951102));
#40764=CARTESIAN_POINT('Ctrl Pts',(-22.2011751392929,26.4804805817286,-2.08670276167943));
#40765=CARTESIAN_POINT('Ctrl Pts',(-22.3315060440038,26.53704528402,-2.07737252921282));
#40766=CARTESIAN_POINT('Ctrl Pts',(-22.7433972891215,26.6843228832894,-2.04808129956067));
#40767=CARTESIAN_POINT('Ctrl Pts',(-23.0339622594772,26.7450714813704,-2.02757079915333));
#40768=CARTESIAN_POINT('Ctrl Pts',(-23.3412669817044,26.7662438687843,-2.00814414337565));
#40769=CARTESIAN_POINT('Ctrl Pts',(-23.3537994529027,26.7670337553,-2.00735601078313));
#40770=CARTESIAN_POINT('Ctrl Pts',(-23.3697931694055,26.7679479754731,-2.00635574359657));
#40771=CARTESIAN_POINT('Ctrl Pts',(-23.3732502102837,26.7681399953631,-2.00613986555109));
#40772=CARTESIAN_POINT('Ctrl Pts',(-23.3787915313267,26.7684388288754,-2.00579436834691));
#40773=CARTESIAN_POINT('Ctrl Pts',(-23.3808756052322,26.7685491890665,-2.00566454930556));
#40774=CARTESIAN_POINT('Ctrl Pts',(-23.3848339188845,26.7687549422693,-2.00541821445588));
#40775=CARTESIAN_POINT('Ctrl Pts',(-23.3867081208446,26.7688507219066,-2.00530167781696));
#40776=CARTESIAN_POINT('Ctrl Pts',(-23.3910005366016,26.7690663235438,-2.005035004047));
#40777=CARTESIAN_POINT('Ctrl Pts',(-23.3934187992127,26.7691850573912,-2.00488492922803));
#40778=CARTESIAN_POINT('Ctrl Pts',(-23.4008658940968,26.7695422889126,-2.00442326890558));
#40779=CARTESIAN_POINT('Ctrl Pts',(-23.4058951840868,26.7697717295606,-2.00411219305613));
#40780=CARTESIAN_POINT('Ctrl Pts',(-23.4438430775558,26.7714138467199,-2.00177014959254));
#40781=CARTESIAN_POINT('Ctrl Pts',(-23.47678259673,26.7723334685427,-1.99976639346848));
#40782=CARTESIAN_POINT('Ctrl Pts',(-23.5180310480813,26.7728521382516,-1.99728726580144));
#40783=CARTESIAN_POINT('Ctrl Pts',(-23.526330592207,26.7729244343096,-1.99678996752611));
#40784=CARTESIAN_POINT('Ctrl Pts',(-23.5407225203228,26.7729941992907,-1.99593012100705));
#40785=CARTESIAN_POINT('Ctrl Pts',(-23.5468147471754,26.7730064565099,-1.99556691725262));
#40786=CARTESIAN_POINT('Ctrl Pts',(-23.8550998779148,26.7727525309378,-1.97722537277802));
#40787=CARTESIAN_POINT('Ctrl Pts',(-24.1557922869066,26.7300028437982,-1.96104434394632));
#40788=CARTESIAN_POINT('Ctrl Pts',(-24.5186042529909,26.6250046732449,-1.93954680566064));
#40789=CARTESIAN_POINT('Ctrl Pts',(-24.5902897000707,26.6015026766257,-1.9352057457857));
#40790=CARTESIAN_POINT('Ctrl Pts',(-24.7352376523306,26.5482799390058,-1.9261689890664));
#40791=CARTESIAN_POINT('Ctrl Pts',(-24.8083620267614,26.5183355824813,-1.92146930241151));
#40792=CARTESIAN_POINT('Ctrl Pts',(-24.8896617974048,26.4814989951999,-1.91605416370084));
#40793=CARTESIAN_POINT('Ctrl Pts',(-24.8989948808137,26.4772163310555,-1.91542964236119));
#40794=CARTESIAN_POINT('Ctrl Pts',(-24.915642800184,26.4694805813602,-1.91431043157827));
#40795=CARTESIAN_POINT('Ctrl Pts',(-24.922965434871,26.4660444095235,-1.91381632819794));
#40796=CARTESIAN_POINT('Ctrl Pts',(-24.9340126918647,26.4608096070354,-1.91306812527711));
#40797=CARTESIAN_POINT('Ctrl Pts',(-24.9377469532686,26.459031295977,-1.91281473200034));
#40798=CARTESIAN_POINT('Ctrl Pts',(-24.9442195520279,26.4559336476926,-1.91237468565196));
#40799=CARTESIAN_POINT('Ctrl Pts',(-24.9469594715196,26.454617613048,-1.91218814778618));
#40800=CARTESIAN_POINT('Ctrl Pts',(-24.9525992394811,26.4518989006218,-1.91180364282047));
#40801=CARTESIAN_POINT('Ctrl Pts',(-24.9554988543054,26.4504957476698,-1.9116056592851));
#40802=CARTESIAN_POINT('Ctrl Pts',(-24.9624758865332,26.4471065715472,-1.91112855889887));
#40803=CARTESIAN_POINT('Ctrl Pts',(-24.966551216833,26.4451162877823,-1.91084929333928));
#40804=CARTESIAN_POINT('Ctrl Pts',(-24.9790502952278,26.4389793564025,-1.90999096721693));
#40805=CARTESIAN_POINT('Ctrl Pts',(-24.9874600779658,26.4348045216594,-1.90941092014022));
#40806=CARTESIAN_POINT('Ctrl Pts',(-25.0184049107969,26.4192737828006,-1.90726710386275));
#40807=CARTESIAN_POINT('Ctrl Pts',(-25.0408241335984,26.4076902980701,-1.90569534638959));
#40808=CARTESIAN_POINT('Ctrl Pts',(-25.068436336152,26.3930103409279,-1.90373591879255));
#40809=CARTESIAN_POINT('Ctrl Pts',(-25.0737601520591,26.3901607266833,-1.90335703126427));
#40810=CARTESIAN_POINT('Ctrl Pts',(-25.0851198953671,26.3840391990825,-1.9025462209027));
#40811=CARTESIAN_POINT('Ctrl Pts',(-25.0911534307059,26.3807629306481,-1.90211414560646));
#40812=CARTESIAN_POINT('Ctrl Pts',(-25.0984883947788,26.3767495706759,-1.90158712523887));
#40813=CARTESIAN_POINT('Ctrl Pts',(-25.0997998745581,26.3760308017155,-1.90149282666959));
#40814=CARTESIAN_POINT('Ctrl Pts',(-25.1036283669803,26.3739290933302,-1.90121734950016));
#40815=CARTESIAN_POINT('Ctrl Pts',(-25.1061440271363,26.3725437046083,-1.9010360847221));
#40816=CARTESIAN_POINT('Ctrl Pts',(-25.1146894318349,26.3678228026043,-1.90041949186207));
#40817=CARTESIAN_POINT('Ctrl Pts',(-25.120710297586,26.3644713310074,-1.89998360349084));
#40818=CARTESIAN_POINT('Ctrl Pts',(-25.1313586658994,26.3584991797639,-1.89921011500283));
#40819=CARTESIAN_POINT('Ctrl Pts',(-25.1359905321879,26.3558862991817,-1.89887278921981));
#40820=CARTESIAN_POINT('Ctrl Pts',(-25.1440995884511,26.3512854063983,-1.89828069805135));
#40821=CARTESIAN_POINT('Ctrl Pts',(-25.1475795885699,26.3493023488016,-1.8980261060129));
#40822=CARTESIAN_POINT('Ctrl Pts',(-25.1548406636712,26.3451467167868,-1.89749385711653));
#40823=CARTESIAN_POINT('Ctrl Pts',(-25.1586210417822,26.3429729463794,-1.89721615906713));
#40824=CARTESIAN_POINT('Ctrl Pts',(-25.1853074313872,26.327555740211,-1.89525165842774));
#40825=CARTESIAN_POINT('Ctrl Pts',(-25.2080534647302,26.3140386375315,-1.89355541964498));
#40826=CARTESIAN_POINT('Ctrl Pts',(-25.3127290524877,26.2500767879286,-1.88564750675736));
#40827=CARTESIAN_POINT('Ctrl Pts',(-25.3925338541213,26.1962629882673,-1.8793234610762));
#40828=CARTESIAN_POINT('Ctrl Pts',(-25.5212403850291,26.1008258788836,-1.86864566928385));
#40829=CARTESIAN_POINT('Ctrl Pts',(-25.5715243284565,26.0611641915785,-1.86434310078712));
#40830=CARTESIAN_POINT('Ctrl Pts',(-25.7109822118129,25.9442609857963,-1.85206195737553));
#40831=CARTESIAN_POINT('Ctrl Pts',(-25.7971445526171,25.863584693704,-1.84404495176569));
#40832=CARTESIAN_POINT('Ctrl Pts',(-25.9431886626645,25.7109647395509,-1.82985284903459));
#40833=CARTESIAN_POINT('Ctrl Pts',(-26.0047346873913,25.64078849053,-1.82365067699451));
#40834=CARTESIAN_POINT('Ctrl Pts',(-26.084091307304,25.5419595864191,-1.81544258652913));
#40835=CARTESIAN_POINT('Ctrl Pts',(-26.1046233779342,25.5155580329806,-1.81329800393248));
#40836=CARTESIAN_POINT('Ctrl Pts',(-26.1354081421401,25.4746751628591,-1.81005594771835));
#40837=CARTESIAN_POINT('Ctrl Pts',(-26.1459578348705,25.4604216359595,-1.80893994149941));
#40838=CARTESIAN_POINT('Ctrl Pts',(-26.1586761428049,25.442938172625,-1.80758912512211));
#40839=CARTESIAN_POINT('Ctrl Pts',(-26.1609569854512,25.4397908154816,-1.80734666072015));
#40840=CARTESIAN_POINT('Ctrl Pts',(-26.1645090066659,25.4348706373559,-1.80696873717648));
#40841=CARTESIAN_POINT('Ctrl Pts',(-26.1657840790539,25.4331006524819,-1.80683300750787));
#40842=CARTESIAN_POINT('Ctrl Pts',(-26.1680363061781,25.4299675328271,-1.80659314601665));
#40843=CARTESIAN_POINT('Ctrl Pts',(-26.1690141887757,25.4286049370917,-1.80648896346828));
#40844=CARTESIAN_POINT('Ctrl Pts',(-26.1711029408282,25.4256896381597,-1.80626634776544));
#40845=CARTESIAN_POINT('Ctrl Pts',(-26.1722134911821,25.4241367155044,-1.8061479370324));
#40846=CARTESIAN_POINT('Ctrl Pts',(-26.1754223003678,25.4196412845054,-1.80580565454605));
#40847=CARTESIAN_POINT('Ctrl Pts',(-26.1775169989933,25.4166962202813,-1.80558203013265));
#40848=CARTESIAN_POINT('Ctrl Pts',(-26.1868323180954,25.4035524917458,-1.80458670053755));
#40849=CARTESIAN_POINT('Ctrl Pts',(-26.1939986666674,25.3933152267318,-1.80381869765335));
#40850=CARTESIAN_POINT('Ctrl Pts',(-26.3152436862393,25.2179520936328,-1.79078095830451));
#40851=CARTESIAN_POINT('Ctrl Pts',(-26.4137310232875,25.0425377726757,-1.77950292950655));
#40852=CARTESIAN_POINT('Ctrl Pts',(-26.5612345127091,24.710636417083,-1.7591881289436));
#40853=CARTESIAN_POINT('Ctrl Pts',(-26.6158846970046,24.5574266515223,-1.75016279157195));
#40854=CARTESIAN_POINT('Ctrl Pts',(-26.6915335483904,24.2809387701899,-1.73371922736902));
#40855=CARTESIAN_POINT('Ctrl Pts',(-26.7173582157115,24.159337857078,-1.72643949757995));
#40856=CARTESIAN_POINT('Ctrl Pts',(-26.7391736186868,24.0164228794936,-1.71769444918471));
#40857=CARTESIAN_POINT('Ctrl Pts',(-26.7420563474737,23.9962579847636,-1.71645637202738));
#40858=CARTESIAN_POINT('Ctrl Pts',(-26.7455395984723,23.9701263783485,-1.71484613823199));
#40859=CARTESIAN_POINT('Ctrl Pts',(-26.7463149455236,23.964183120518,-1.71447952559014));
#40860=CARTESIAN_POINT('Ctrl Pts',(-26.7475420487022,23.954567994543,-1.71388577271022));
#40861=CARTESIAN_POINT('Ctrl Pts',(-26.7480040719188,23.9508974316715,-1.71365895770139));
#40862=CARTESIAN_POINT('Ctrl Pts',(-26.7488748480599,23.9438820461965,-1.7132251653749));
#40863=CARTESIAN_POINT('Ctrl Pts',(-26.7492846775162,23.940537360121,-1.71301822241602));
#40864=CARTESIAN_POINT('Ctrl Pts',(-26.7502108949041,23.9328788662033,-1.71254408319146));
#40865=CARTESIAN_POINT('Ctrl Pts',(-26.7507238060361,23.92856465145,-1.71227677736607));
#40866=CARTESIAN_POINT('Ctrl Pts',(-26.7522743046873,23.9152941987828,-1.71145389050412));
#40867=CARTESIAN_POINT('Ctrl Pts',(-26.7532830259138,23.9063346905873,-1.71089739854318));
#40868=CARTESIAN_POINT('Ctrl Pts',(-26.7605977734794,23.8388175297896,-1.70669668215556));
#40869=CARTESIAN_POINT('Ctrl Pts',(-26.7653347541892,23.7801044212592,-1.70300322056571));
#40870=CARTESIAN_POINT('Ctrl Pts',(-26.7692479267539,23.7064781441524,-1.69831664865356));
#40871=CARTESIAN_POINT('Ctrl Pts',(-26.7699331803443,23.6916537499286,-1.69737025914913));
#40872=CARTESIAN_POINT('Ctrl Pts',(-26.7722017411626,23.6339370617008,-1.69367479996766));
#40873=CARTESIAN_POINT('Ctrl Pts',(-26.7730304438053,23.5910210324962,-1.69090365196987));
#40874=CARTESIAN_POINT('Ctrl Pts',(-26.7729009589345,23.3969072731341,-1.6782653603257));
#40875=CARTESIAN_POINT('Ctrl Pts',(-26.762160312742,23.245921019536,-1.6681369661269));
#40876=CARTESIAN_POINT('Ctrl Pts',(-26.708051016869,22.8656459064639,-1.64217120326962));
#40877=CARTESIAN_POINT('Ctrl Pts',(-26.6503278496435,22.6392464702608,-1.62625582676243));
#40878=CARTESIAN_POINT('Ctrl Pts',(-26.5637957857494,22.4079434969898,-1.61065726557838));
#40879=CARTESIAN_POINT('Ctrl Pts',(-26.5588137394052,22.3948857712107,-1.60977919307569));
#40880=CARTESIAN_POINT('Ctrl Pts',(-26.5523956841853,22.3783873759847,-1.60867331656203));
#40881=CARTESIAN_POINT('Ctrl Pts',(-26.5510385354166,22.3749164897838,-1.60844086601903));
#40882=CARTESIAN_POINT('Ctrl Pts',(-26.548882312421,22.369430063493,-1.60807375827423));
#40883=CARTESIAN_POINT('Ctrl Pts',(-26.5480872250465,22.3674129759342,-1.60793886084429));
#40884=CARTESIAN_POINT('Ctrl Pts',(-26.5466043480409,22.3636621077525,-1.6076881450184));
#40885=CARTESIAN_POINT('Ctrl Pts',(-26.54591709312,22.3619281328188,-1.60757229538596));
#40886=CARTESIAN_POINT('Ctrl Pts',(-26.5443797753195,22.3580592202002,-1.6073139244837));
#40887=CARTESIAN_POINT('Ctrl Pts',(-26.5435289361523,22.355924599515,-1.60717145135671));
#40888=CARTESIAN_POINT('Ctrl Pts',(-26.5410316618907,22.3496787648553,-1.60675480721923));
#40889=CARTESIAN_POINT('Ctrl Pts',(-26.5393790262915,22.3455700112375,-1.60648101169907));
#40890=CARTESIAN_POINT('Ctrl Pts',(-26.5272172931887,22.3155128298761,-1.6044801154671));
#40891=CARTESIAN_POINT('Ctrl Pts',(-26.5163785243098,22.2896978732313,-1.60277269959519));
#40892=CARTESIAN_POINT('Ctrl Pts',(-26.4799458170619,22.2059980564678,-1.5972627553313));
#40893=CARTESIAN_POINT('Ctrl Pts',(-26.4529817048122,22.14872218552,-1.59353320328476));
#40894=CARTESIAN_POINT('Ctrl Pts',(-26.3861173932511,22.0169134675127,-1.58496314952343));
#40895=CARTESIAN_POINT('Ctrl Pts',(-26.3449371428071,21.9430818542706,-1.58017215715433));
#40896=CARTESIAN_POINT('Ctrl Pts',(-26.1671499737347,21.6518715629132,-1.56098845376566));
#40897=CARTESIAN_POINT('Ctrl Pts',(-26.0077178421121,21.4495715898968,-1.54690720546562));
#40898=CARTESIAN_POINT('Ctrl Pts',(-25.8171539791868,21.2595254115901,-1.53111138195038));
#40899=CARTESIAN_POINT('Ctrl Pts',(-25.8082777887953,21.2507754511653,-1.53037790260144));
#40900=CARTESIAN_POINT('Ctrl Pts',(-25.7505495017093,21.1945246918028,-1.52562138434387));
#40901=CARTESIAN_POINT('Ctrl Pts',(-25.7002550866962,21.1485347340481,-1.52154038953863));
#40902=CARTESIAN_POINT('Ctrl Pts',(-25.6414048432671,21.0980518802236,-1.51681763112022));
#40903=CARTESIAN_POINT('Ctrl Pts',(-25.6342393539314,21.0919594354463,-1.51624346249569));
#40904=CARTESIAN_POINT('Ctrl Pts',(-25.6237035441359,21.0830805507818,-1.51540045047024));
#40905=CARTESIAN_POINT('Ctrl Pts',(-25.6203540126742,21.0802694259746,-1.51513262045078));
#40906=CARTESIAN_POINT('Ctrl Pts',(-25.6144021684953,21.0752948973606,-1.51465702095385));
#40907=CARTESIAN_POINT('Ctrl Pts',(-25.6118021449282,21.0731287546318,-1.5144493638413));
#40908=CARTESIAN_POINT('Ctrl Pts',(-25.6063898249814,21.0686340426976,-1.51401731212067));
#40909=CARTESIAN_POINT('Ctrl Pts',(-25.603576974891,21.0663061505153,-1.5137928903504));
#40910=CARTESIAN_POINT('Ctrl Pts',(-25.5963032366952,21.0603072610351,-1.51321286680965));
#40911=CARTESIAN_POINT('Ctrl Pts',(-25.5918364368312,21.0566434813612,-1.51285697260819));
#40912=CARTESIAN_POINT('Ctrl Pts',(-25.573071297979,21.0413360686713,-1.5113630748757));
#40913=CARTESIAN_POINT('Ctrl Pts',(-25.5586832366834,21.0298034327893,-1.51022060000891));
#40914=CARTESIAN_POINT('Ctrl Pts',(-25.4610349155357,20.9529012542054,-1.5024856489804));
#40915=CARTESIAN_POINT('Ctrl Pts',(-25.3747051737642,20.8915514704308,-1.49573507548004));
#40916=CARTESIAN_POINT('Ctrl Pts',(-25.1572168827541,20.752580899112,-1.47891845934216));
#40917=CARTESIAN_POINT('Ctrl Pts',(-25.0232759441968,20.6798005496214,-1.46871095979811));
#40918=CARTESIAN_POINT('Ctrl Pts',(-24.6745928147253,20.5211833562646,-1.44280913980538));
#40919=CARTESIAN_POINT('Ctrl Pts',(-24.4547972687646,20.44844309298,-1.42705018909865));
#40920=CARTESIAN_POINT('Ctrl Pts',(-24.2161974415993,20.3970305152307,-1.41164456000963));
#40921=CARTESIAN_POINT('Ctrl Pts',(-24.2032798816226,20.3943300037023,-1.41081579340468));
#40922=CARTESIAN_POINT('Ctrl Pts',(-24.1867715361973,20.3909845120886,-1.40976369733969));
#40923=CARTESIAN_POINT('Ctrl Pts',(-24.1831959887697,20.3902662274114,-1.40953624476675));
#40924=CARTESIAN_POINT('Ctrl Pts',(-24.1775110747314,20.3891342322424,-1.40917528603247));
#40925=CARTESIAN_POINT('Ctrl Pts',(-24.1754025138489,20.3887165627672,-1.40904155284713));
#40926=CARTESIAN_POINT('Ctrl Pts',(-24.1714980719402,20.3879472191013,-1.40879419396643));
#40927=CARTESIAN_POINT('Ctrl Pts',(-24.1697023210212,20.3875949672623,-1.4086805356983));
#40928=CARTESIAN_POINT('Ctrl Pts',(-24.1657777946103,20.3868286087409,-1.40843237693538));
#40929=CARTESIAN_POINT('Ctrl Pts',(-24.1636489062009,20.386415122248,-1.40829791273573));
#40930=CARTESIAN_POINT('Ctrl Pts',(-24.159156195249,20.3855472239108,-1.40801446169817));
#40931=CARTESIAN_POINT('Ctrl Pts',(-24.1567922762052,20.3850933105776,-1.4078655035266));
#40932=CARTESIAN_POINT('Ctrl Pts',(-24.1506977816074,20.3839301405734,-1.40748194025754));
#40933=CARTESIAN_POINT('Ctrl Pts',(-24.1469664436035,20.3832248257312,-1.40724755886948));
#40934=CARTESIAN_POINT('Ctrl Pts',(-24.1360862728115,20.3811881164023,-1.40656542907959));
#40935=CARTESIAN_POINT('Ctrl Pts',(-24.1289341124098,20.3798743096192,-1.4061186615157));
#40936=CARTESIAN_POINT('Ctrl Pts',(-24.0547172706226,20.3665006590652,-1.40149900089485));
#40937=CARTESIAN_POINT('Ctrl Pts',(-23.9872849340557,20.3565454536014,-1.39744013883199));
#40938=CARTESIAN_POINT('Ctrl Pts',(-23.8513455204538,20.3408633707872,-1.38944356119344));
#40939=CARTESIAN_POINT('Ctrl Pts',(-23.7828709959598,20.3351747117281,-1.38550909849417));
#40940=CARTESIAN_POINT('Ctrl Pts',(-23.362455779992,20.3137513059831,-1.36165200210973));
#40941=CARTESIAN_POINT('Ctrl Pts',(-23.0101247566829,20.3536182663799,-1.34262619544138));
#40942=CARTESIAN_POINT('Ctrl Pts',(-22.6512580904904,20.4553604653162,-1.32007313505219));
#40943=CARTESIAN_POINT('Ctrl Pts',(-22.6313553927862,20.4612112686684,-1.31881273758147));
#40944=CARTESIAN_POINT('Ctrl Pts',(-22.6054875482102,20.4690877627669,-1.3171615742955));
#40945=CARTESIAN_POINT('Ctrl Pts',(-22.5994695960322,20.4709394564027,-1.31677652258074));
#40946=CARTESIAN_POINT('Ctrl Pts',(-22.5902194017627,20.4738153962714,-1.31618322754854));
#40947=CARTESIAN_POINT('Ctrl Pts',(-22.5869832615334,20.4748271348103,-1.31597539570229));
#40948=CARTESIAN_POINT('Ctrl Pts',(-22.5805905616292,20.4768368119964,-1.31556430612857));
#40949=CARTESIAN_POINT('Ctrl Pts',(-22.5774339306523,20.4778345113701,-1.31536105649232));
#40950=CARTESIAN_POINT('Ctrl Pts',(-22.5704416515864,20.4800563795656,-1.31491025970654));
#40951=CARTESIAN_POINT('Ctrl Pts',(-22.5666067535526,20.4812828745891,-1.31466263613482));
#40952=CARTESIAN_POINT('Ctrl Pts',(-22.5556611527179,20.484806171233,-1.3139547602697));
#40953=CARTESIAN_POINT('Ctrl Pts',(-22.5485561609215,20.4871205104988,-1.31349392966345));
#40954=CARTESIAN_POINT('Ctrl Pts',(-22.5033881026817,20.5020072506236,-1.3105557402038));
#40955=CARTESIAN_POINT('Ctrl Pts',(-22.4655557668092,20.5152637145138,-1.30805581643115));
#40956=CARTESIAN_POINT('Ctrl Pts',(-22.3538663948609,20.556754755859,-1.30055505315203));
#40957=CARTESIAN_POINT('Ctrl Pts',(-22.2807948901364,20.5870035900472,-1.29548825641569));
#40958=CARTESIAN_POINT('Ctrl Pts',(-22.0714517310497,20.682828450085,-1.28049853754635));
#40959=CARTESIAN_POINT('Ctrl Pts',(-21.9386005323521,20.7553389150149,-1.2703713642156));
#40960=CARTESIAN_POINT('Ctrl Pts',(-21.6314521642055,20.9521814800467,-1.24571000850892));
#40961=CARTESIAN_POINT('Ctrl Pts',(-21.463460463427,21.0850787648623,-1.23112807469708));
#40962=CARTESIAN_POINT('Ctrl Pts',(-21.3066056699675,21.2367731837902,-1.2171557165846));
#40963=CARTESIAN_POINT('Ctrl Pts',(-21.3033678639448,21.2399176590724,-1.21686714446093));
#40964=CARTESIAN_POINT('Ctrl Pts',(-21.2963793619282,21.246733301936,-1.2162439760432));
#40965=CARTESIAN_POINT('Ctrl Pts',(-21.2926309974804,21.250406859404,-1.21590953668217));
#40966=CARTESIAN_POINT('Ctrl Pts',(-21.282618080161,21.2602680149908,-1.21501567259362));
#40967=CARTESIAN_POINT('Ctrl Pts',(-21.2763698307259,21.2664722097875,-1.21445737438463));
#40968=CARTESIAN_POINT('Ctrl Pts',(-21.2598448061077,21.2830157725445,-1.21297965249756));
#40969=CARTESIAN_POINT('Ctrl Pts',(-21.249612468608,21.2933995478286,-1.21206343507456));
#40970=CARTESIAN_POINT('Ctrl Pts',(-21.2368116679226,21.3065673339627,-1.21091612530259));
#40971=CARTESIAN_POINT('Ctrl Pts',(-21.2341773913626,21.3092867038921,-1.21067996069684));
#40972=CARTESIAN_POINT('Ctrl Pts',(-21.2300325397459,21.3135805592881,-1.21030828707244));
#40973=CARTESIAN_POINT('Ctrl Pts',(-21.2285187717058,21.315151936423,-1.21017252780909));
#40974=CARTESIAN_POINT('Ctrl Pts',(-21.225739944152,21.3180423863112,-1.20992328330767));
#40975=CARTESIAN_POINT('Ctrl Pts',(-21.2244744182807,21.3193609901816,-1.20980976147508));
#40976=CARTESIAN_POINT('Ctrl Pts',(-21.2216748958573,21.3222828999342,-1.209558608897));
#40977=CARTESIAN_POINT('Ctrl Pts',(-21.220141436946,21.3238867099194,-1.20942102051637));
#40978=CARTESIAN_POINT('Ctrl Pts',(-21.2169589162153,21.3272221260803,-1.2091354312578));
#40979=CARTESIAN_POINT('Ctrl Pts',(-21.2153101218947,21.3289539873003,-1.20898745126677));
#40980=CARTESIAN_POINT('Ctrl Pts',(-21.2110740128681,21.3334134411331,-1.20860719580412));
#40981=CARTESIAN_POINT('Ctrl Pts',(-21.2084895316137,21.3361437384847,-1.20837513865686));
#40982=CARTESIAN_POINT('Ctrl Pts',(-21.2009886047108,21.3440956921651,-1.20770144187643));
#40983=CARTESIAN_POINT('Ctrl Pts',(-21.1960847656151,21.3493292866326,-1.20726075400568));
#40984=CARTESIAN_POINT('Ctrl Pts',(-21.0696286689402,21.4851950294501,-1.19588882381541));
#40985=CARTESIAN_POINT('Ctrl Pts',(-20.9590965341054,21.6257037763544,-1.18575284308195));
#40986=CARTESIAN_POINT('Ctrl Pts',(-20.6882115155567,22.0360150351246,-1.15816782537698));
#40987=CARTESIAN_POINT('Ctrl Pts',(-20.5547041435692,22.321080676087,-1.14094732402074));
#40988=CARTESIAN_POINT('Ctrl Pts',(-20.458998071584,22.638871702962,-1.12085696781627));
#40989=CARTESIAN_POINT('Ctrl Pts',(-20.4537478671096,22.6568724383445,-1.11971691007044));
#40990=CARTESIAN_POINT('Ctrl Pts',(-20.447011973554,22.6807399100413,-1.11820222218321));
#40991=CARTESIAN_POINT('Ctrl Pts',(-20.4453852243013,22.6865667302628,-1.11783219752102));
#40992=CARTESIAN_POINT('Ctrl Pts',(-20.442885600431,22.6956184120386,-1.1172569975411));
#40993=CARTESIAN_POINT('Ctrl Pts',(-20.4420013117371,22.698840130159,-1.11705219408571));
#40994=CARTESIAN_POINT('Ctrl Pts',(-20.4402411246179,22.705292288061,-1.11664187921063));
#40995=CARTESIAN_POINT('Ctrl Pts',(-20.4393652459643,22.708522728957,-1.11643636743425));
#40996=CARTESIAN_POINT('Ctrl Pts',(-20.4374213860382,22.7157366064281,-1.11597726603841));
#40997=CARTESIAN_POINT('Ctrl Pts',(-20.436356016792,22.7197207351227,-1.11572359191395));
#40998=CARTESIAN_POINT('Ctrl Pts',(-20.4332637107434,22.731374528016,-1.11498122876439));
#40999=CARTESIAN_POINT('Ctrl Pts',(-20.4312574527445,22.7390496036151,-1.11449186950533));
#41000=CARTESIAN_POINT('Ctrl Pts',(-20.416797891624,22.7952123212608,-1.11090759921212));
#41001=CARTESIAN_POINT('Ctrl Pts',(-20.4054481360072,22.8439745709118,-1.10777716520858));
#41002=CARTESIAN_POINT('Ctrl Pts',(-20.3721754995751,23.0036883718675,-1.09745623167664));
#41003=CARTESIAN_POINT('Ctrl Pts',(-20.354957351514,23.1155228636957,-1.09012041782651));
#41004=CARTESIAN_POINT('Ctrl Pts',(-20.309810320198,23.5647912239797,-1.06026011071333));
#41005=CARTESIAN_POINT('Ctrl Pts',(-20.3292301653878,23.9047540870365,-1.03654077099051));
#41006=CARTESIAN_POINT('Ctrl Pts',(-20.4020321778134,24.2393403342527,-1.01489042254365));
#41007=CARTESIAN_POINT('Ctrl Pts',(-20.402885405708,24.2432269690667,-1.01463920028158));
#41008=CARTESIAN_POINT('Ctrl Pts',(-20.4063010843938,24.2586496701697,-1.01364342873332));
#41009=CARTESIAN_POINT('Ctrl Pts',(-20.4089198213766,24.2701733760852,-1.01290187038063));
#41010=CARTESIAN_POINT('Ctrl Pts',(-20.4124045846724,24.2851268958564,-1.0119430522834));
#41011=CARTESIAN_POINT('Ctrl Pts',(-20.4132129092912,24.2885698601455,-1.01172252797463));
#41012=CARTESIAN_POINT('Ctrl Pts',(-20.4144627339557,24.2938542345521,-1.01138443336166));
#41013=CARTESIAN_POINT('Ctrl Pts',(-20.4149001888925,24.2956965836696,-1.01126662947618));
#41014=CARTESIAN_POINT('Ctrl Pts',(-20.4157299907772,24.2991776563292,-1.01104417519294));
#41015=CARTESIAN_POINT('Ctrl Pts',(-20.4161219973826,24.3008164501932,-1.0109395057837));
#41016=CARTESIAN_POINT('Ctrl Pts',(-20.4170196724174,24.3045562383449,-1.01070077387203));
#41017=CARTESIAN_POINT('Ctrl Pts',(-20.4175261678783,24.306657027872,-1.01056676023376));
#41018=CARTESIAN_POINT('Ctrl Pts',(-20.4189414775473,24.3125014973824,-1.01019418078611));
#41019=CARTESIAN_POINT('Ctrl Pts',(-20.4198548957881,24.316244075379,-1.00995588185317));
#41020=CARTESIAN_POINT('Ctrl Pts',(-20.4219089221042,24.3245950663587,-1.00942477655976));
#41021=CARTESIAN_POINT('Ctrl Pts',(-20.4230530095223,24.3292026262787,-1.00913216910047));
#41022=CARTESIAN_POINT('Ctrl Pts',(-20.4266068317581,24.3433808359462,-1.00823302583629));
#41023=CARTESIAN_POINT('Ctrl Pts',(-20.4290503790251,24.3529430659052,-1.00762838123761));
#41024=CARTESIAN_POINT('Ctrl Pts',(-20.4382519380361,24.3882737355535,-1.00540035910864));
#41025=CARTESIAN_POINT('Ctrl Pts',(-20.4452856579359,24.4139701062999,-1.00379177954574));
#41026=CARTESIAN_POINT('Ctrl Pts',(-20.4765220965681,24.5227700353375,-0.997020079348007));
#41027=CARTESIAN_POINT('Ctrl Pts',(-20.5037505359669,24.604973873176,-0.992000840985586));
#41028=CARTESIAN_POINT('Ctrl Pts',(-20.6402645512784,24.9674928058054,-0.969900176978225));
#41029=CARTESIAN_POINT('Ctrl Pts',(-20.7851540369272,25.2327630591764,-0.953670432714227));
#41030=CARTESIAN_POINT('Ctrl Pts',(-20.977078177054,25.4906955230521,-0.934840809804062));
#41031=CARTESIAN_POINT('Ctrl Pts',(-20.9895830599513,25.5071677296483,-0.933624294109055));
#41032=CARTESIAN_POINT('Ctrl Pts',(-21.0052465112645,25.5273933820429,-0.932112465217948));
#41033=CARTESIAN_POINT('Ctrl Pts',(-21.0082564217634,25.5312617095809,-0.931822486799601));
#41034=CARTESIAN_POINT('Ctrl Pts',(-21.0137535321157,25.5382934218109,-0.931293850958268));
#41035=CARTESIAN_POINT('Ctrl Pts',(-21.0162378581375,25.5414590477622,-0.93105529814438));
#41036=CARTESIAN_POINT('Ctrl Pts',(-21.0214071166785,25.5480205789189,-0.930559657802778));
#41037=CARTESIAN_POINT('Ctrl Pts',(-21.0240929744663,25.5514157421107,-0.930302536624922));
#41038=CARTESIAN_POINT('Ctrl Pts',(-21.0595499577223,25.5960513917799,-0.926913448913421));
#41039=CARTESIAN_POINT('Ctrl Pts',(-21.0933189959918,25.6364858348869,-0.923744519564235));
#41040=CARTESIAN_POINT('Ctrl Pts',(-21.1338138871127,25.6826262952294,-0.920003305402341));
#41041=CARTESIAN_POINT('Ctrl Pts',(-21.1395919864224,25.6891562984767,-0.919470833231494));
#41042=CARTESIAN_POINT('Ctrl Pts',(-21.1482494170282,25.6988606778806,-0.918674991332547));
#41043=CARTESIAN_POINT('Ctrl Pts',(-21.1511087288068,25.7020529270631,-0.91841246437401));
#41044=CARTESIAN_POINT('Ctrl Pts',(-21.1562227678772,25.7077395787713,-0.917943481413285));
#41045=CARTESIAN_POINT('Ctrl Pts',(-21.1584750516817,25.7102361784646,-0.917737128877092));
#41046=CARTESIAN_POINT('Ctrl Pts',(-21.1632346883992,25.7154955430007,-0.917301458772015));
#41047=CARTESIAN_POINT('Ctrl Pts',(-21.1657429384674,25.7182574859881,-0.917072103306014));
#41048=CARTESIAN_POINT('Ctrl Pts',(-21.1723875224505,25.7255486456641,-0.916465136922146));
#41049=CARTESIAN_POINT('Ctrl Pts',(-21.1765319857922,25.7300704036202,-0.916087180152197));
#41050=CARTESIAN_POINT('Ctrl Pts',(-21.1954078558245,25.750546986173,-0.914368603810139));
#41051=CARTESIAN_POINT('Ctrl Pts',(-21.2102871076739,25.7663641965461,-0.913021659075345));
#41052=CARTESIAN_POINT('Ctrl Pts',(-21.3209819512588,25.8816792635215,-0.903055598655631));
#41053=CARTESIAN_POINT('Ctrl Pts',(-21.4229334448893,25.9750622798637,-0.894164171201551));
#41054=CARTESIAN_POINT('Ctrl Pts',(-21.6422388991004,26.1514339748723,-0.875591668495027));
#41055=CARTESIAN_POINT('Ctrl Pts',(-21.7597903274098,26.2337019197543,-0.865913501870995));
#41056=CARTESIAN_POINT('Ctrl Pts',(-21.9454058127333,26.3459641497493,-0.851229451117898));
#41057=CARTESIAN_POINT('Ctrl Pts',(-22.0096510653896,26.3818727729581,-0.846249054954694));
#41058=CARTESIAN_POINT('Ctrl Pts',(-22.0750363147453,26.4155369287046,-0.841310143832837));
#41059=CARTESIAN_POINT('Origin',(-23.5502525316942,23.5502525316942,-77.3107734492734));
#41060=CARTESIAN_POINT('',(-22.0750360011372,26.4155367672407,0.656690934610686));
#41061=CARTESIAN_POINT('',(-22.0750360367128,26.4155367855571,0.408876748608879));
#41062=CARTESIAN_POINT('',(-22.0750360153461,26.4155367745563,-77.3107734492734));
#41063=CARTESIAN_POINT('Ctrl Pts',(-22.0750360011372,26.4155367672407,0.656690934610686));
#41064=CARTESIAN_POINT('Ctrl Pts',(-22.0347854868283,26.3948134395739,0.653836575818294));
#41065=CARTESIAN_POINT('Ctrl Pts',(-21.9949738925344,26.3732431361297,0.650952707466448));
#41066=CARTESIAN_POINT('Ctrl Pts',(-21.6767862317566,26.1920704356087,0.627403182791127));
#41067=CARTESIAN_POINT('Ctrl Pts',(-21.4232414642238,25.9925525060078,0.605233911009184));
#41068=CARTESIAN_POINT('Ctrl Pts',(-21.1381756976759,25.6896594749138,0.577578533526645));
#41069=CARTESIAN_POINT('Ctrl Pts',(-21.0760394129289,25.6174849869373,0.571357342939539));
#41070=CARTESIAN_POINT('Ctrl Pts',(-21.0117377680158,25.5357343265099,0.564793087957518));
#41071=CARTESIAN_POINT('Ctrl Pts',(-21.006320034543,25.5287880044894,0.564238981182645));
#41072=CARTESIAN_POINT('Ctrl Pts',(-20.997019697702,25.5167622646266,0.563286106674382));
#41073=CARTESIAN_POINT('Ctrl Pts',(-20.993123634078,25.5116933890586,0.562886419979856));
#41074=CARTESIAN_POINT('Ctrl Pts',(-20.9876218770747,25.504491211832,0.562321321426151));
#41075=CARTESIAN_POINT('Ctrl Pts',(-20.986003744071,25.5023674991691,0.562155034155368));
#41076=CARTESIAN_POINT('Ctrl Pts',(-20.9832287146955,25.4987160181079,0.561869715919636));
#41077=CARTESIAN_POINT('Ctrl Pts',(-20.9820705403344,25.4971892266721,0.561750593893924));
#41078=CARTESIAN_POINT('Ctrl Pts',(-20.9798564189393,25.4942649940674,0.561522783573879));
#41079=CARTESIAN_POINT('Ctrl Pts',(-20.9788002507879,25.4928677270909,0.561414079360236));
#41080=CARTESIAN_POINT('Ctrl Pts',(-20.9763185820844,25.4895790114672,0.561158572940399));
#41081=CARTESIAN_POINT('Ctrl Pts',(-20.9748940241208,25.4876868479115,0.561011837768286));
#41082=CARTESIAN_POINT('Ctrl Pts',(-20.9707034589361,25.4821079575446,0.560579991721011));
#41083=CARTESIAN_POINT('Ctrl Pts',(-20.9679432581271,25.4784168456022,0.560295288733591));
#41084=CARTESIAN_POINT('Ctrl Pts',(-20.9443789238096,25.4467637974791,0.55786238455405));
#41085=CARTESIAN_POINT('Ctrl Pts',(-20.9240207052318,25.4184706337941,0.555744800891914));
#41086=CARTESIAN_POINT('Ctrl Pts',(-20.7258279934546,25.1333849524081,0.534908955592302));
#41087=CARTESIAN_POINT('Ctrl Pts',(-20.5857363473156,24.8523240114919,0.518227634219056));
#41088=CARTESIAN_POINT('Ctrl Pts',(-20.4644387260804,24.4828363782198,0.496108203453257));
#41089=CARTESIAN_POINT('Ctrl Pts',(-20.4431909785306,24.4093956615494,0.491711965062886));
#41090=CARTESIAN_POINT('Ctrl Pts',(-20.4050726640934,24.2576216716744,0.482558403129002));
#41091=CARTESIAN_POINT('Ctrl Pts',(-20.3884723181591,24.1792769723601,0.477797032890339));
#41092=CARTESIAN_POINT('Ctrl Pts',(-20.37216193219,24.0851336079763,0.472000729462033));
#41093=CARTESIAN_POINT('Ctrl Pts',(-20.3696271677712,24.0698484378397,0.471057345330194));
#41094=CARTESIAN_POINT('Ctrl Pts',(-20.3663569315904,24.0492070265632,0.46978010480062));
#41095=CARTESIAN_POINT('Ctrl Pts',(-20.3655245439493,24.0438661698986,0.469449330506847));
#41096=CARTESIAN_POINT('Ctrl Pts',(-20.3642308279089,24.0354257845988,0.468926119387076));
#41097=CARTESIAN_POINT('Ctrl Pts',(-20.3637605743487,24.0323276171166,0.468733966191606));
#41098=CARTESIAN_POINT('Ctrl Pts',(-20.3628136774373,24.0260272620999,0.468343001264512));
#41099=CARTESIAN_POINT('Ctrl Pts',(-20.3623373391534,24.0228250327639,0.468144180079909));
#41100=CARTESIAN_POINT('Ctrl Pts',(-20.3612577706451,24.0154916176718,0.467688609121825));
#41101=CARTESIAN_POINT('Ctrl Pts',(-20.3606577423294,24.0113599730948,0.467431758111159));
#41102=CARTESIAN_POINT('Ctrl Pts',(-20.35890974435,23.9991570205741,0.466672594943795));
#41103=CARTESIAN_POINT('Ctrl Pts',(-20.357784377465,23.9910825542019,0.466169567132753));
#41104=CARTESIAN_POINT('Ctrl Pts',(-20.3505989355672,23.9380563624841,0.46286139372817));
#41105=CARTESIAN_POINT('Ctrl Pts',(-20.3454580638468,23.892987160979,0.460027294462243));
#41106=CARTESIAN_POINT('Ctrl Pts',(-20.3411450070381,23.8464759217142,0.457077673210773));
#41107=CARTESIAN_POINT('Ctrl Pts',(-20.3410206404389,23.8451255039042,0.45699201182157));
#41108=CARTESIAN_POINT('Ctrl Pts',(-20.3369257736191,23.8003525003089,0.454151203607914));
#41109=CARTESIAN_POINT('Ctrl Pts',(-20.3338362481713,23.7568556438337,0.451369095263529));
#41110=CARTESIAN_POINT('Ctrl Pts',(-20.3201322647396,23.486351967586,0.433926681970065));
#41111=CARTESIAN_POINT('Ctrl Pts',(-20.3326739904699,23.2588428614664,0.418576055951041));
#41112=CARTESIAN_POINT('Ctrl Pts',(-20.3982213584296,22.8544729304243,0.390857485635323));
#41113=CARTESIAN_POINT('Ctrl Pts',(-20.4426638453245,22.6771439027861,0.378567211908465));
#41114=CARTESIAN_POINT('Ctrl Pts',(-20.5070500331622,22.489455892002,0.36601620347792));
#41115=CARTESIAN_POINT('Ctrl Pts',(-20.5123269575011,22.4744369394828,0.365015281847339));
#41116=CARTESIAN_POINT('Ctrl Pts',(-20.5189857913965,22.4559246070893,0.36378632773665));
#41117=CARTESIAN_POINT('Ctrl Pts',(-20.5202626848979,22.4523940772207,0.363552166763792));
#41118=CARTESIAN_POINT('Ctrl Pts',(-20.5222812318347,22.4468432689323,0.363184360351415));
#41119=CARTESIAN_POINT('Ctrl Pts',(-20.5230187392951,22.444821502573,0.363050467400887));
#41120=CARTESIAN_POINT('Ctrl Pts',(-20.5243996492584,22.4410476903996,0.362800682117746));
#41121=CARTESIAN_POINT('Ctrl Pts',(-20.525042544358,22.4392954764281,0.362684760546014));
#41122=CARTESIAN_POINT('Ctrl Pts',(-20.526487509072,22.4353677724193,0.36242503924669));
#41123=CARTESIAN_POINT('Ctrl Pts',(-20.5272904026795,22.4331925936731,0.362281290060201));
#41124=CARTESIAN_POINT('Ctrl Pts',(-20.5293337788934,22.4276750682295,0.361916870660934));
#41125=CARTESIAN_POINT('Ctrl Pts',(-20.5305774650981,22.4243339001047,0.361696392631806));
#41126=CARTESIAN_POINT('Ctrl Pts',(-20.5374150247963,22.406057588195,0.36049141931253));
#41127=CARTESIAN_POINT('Ctrl Pts',(-20.5431142873678,22.3911617173432,0.359513161126289));
#41128=CARTESIAN_POINT('Ctrl Pts',(-20.6549957199676,22.1051234590149,0.340791038152935));
#41129=CARTESIAN_POINT('Ctrl Pts',(-20.7973513980028,21.8495146838571,0.325066312705371));
#41130=CARTESIAN_POINT('Ctrl Pts',(-21.0922266244122,21.4563860081436,0.297407822078719));
#41131=CARTESIAN_POINT('Ctrl Pts',(-21.2269414663724,21.3078484597269,0.285904464831211));
#41132=CARTESIAN_POINT('Ctrl Pts',(-21.3850562812297,21.1631526687265,0.272892029846063));
#41133=CARTESIAN_POINT('Ctrl Pts',(-21.3956305867839,21.1536038667641,0.272024105532997));
#41134=CARTESIAN_POINT('Ctrl Pts',(-21.4101727703592,21.1406460213847,0.270833501284561));
#41135=CARTESIAN_POINT('Ctrl Pts',(-21.4140862560114,21.1371759557176,0.270513388538846));
#41136=CARTESIAN_POINT('Ctrl Pts',(-21.4203568645072,21.1316430508825,0.270000930611424));
#41137=CARTESIAN_POINT('Ctrl Pts',(-21.4227085888715,21.1295740844361,0.269808842008652));
#41138=CARTESIAN_POINT('Ctrl Pts',(-21.427558386775,21.1253199253956,0.269412921323217));
#41139=CARTESIAN_POINT('Ctrl Pts',(-21.4300568264868,21.1231351572238,0.269209071864934));
#41140=CARTESIAN_POINT('Ctrl Pts',(-21.4358200753665,21.1181111562002,0.268739105082294));
#41141=CARTESIAN_POINT('Ctrl Pts',(-21.4390872307082,21.1152746356173,0.268472875504281));
#41142=CARTESIAN_POINT('Ctrl Pts',(-21.4490648588767,21.1066473078217,0.267660409089334));
#41143=CARTESIAN_POINT('Ctrl Pts',(-21.4557934763808,21.1008776339632,0.267113298816795));
#41144=CARTESIAN_POINT('Ctrl Pts',(-21.4704117117014,21.088447027717,0.265926344719462));
#41145=CARTESIAN_POINT('Ctrl Pts',(-21.4783096919318,21.081796123191,0.265286096037397));
#41146=CARTESIAN_POINT('Ctrl Pts',(-21.687408763093,20.9074239372215,0.248362150119762));
#41147=CARTESIAN_POINT('Ctrl Pts',(-21.908234965077,20.764853068017,0.231012769475701));
#41148=CARTESIAN_POINT('Ctrl Pts',(-22.2899888093119,20.5796892126811,0.202321042049335));
#41149=CARTESIAN_POINT('Ctrl Pts',(-22.4413207811096,20.5199412724886,0.191269355035347));
#41150=CARTESIAN_POINT('Ctrl Pts',(-22.658252344682,20.4527325469802,0.176339826379156));
#41151=CARTESIAN_POINT('Ctrl Pts',(-22.7205522883347,20.4354663068507,0.172154963881771));
#41152=CARTESIAN_POINT('Ctrl Pts',(-22.79848723561,20.416371566337,0.167080893385526));
#41153=CARTESIAN_POINT('Ctrl Pts',(-22.8136675502153,20.4127688976372,0.166100067640527));
#41154=CARTESIAN_POINT('Ctrl Pts',(-22.8325087148812,20.4084417026453,0.164892510610802));
#41155=CARTESIAN_POINT('Ctrl Pts',(-22.8361451074413,20.4076131856883,0.164659900356568));
#41156=CARTESIAN_POINT('Ctrl Pts',(-22.8418767195626,20.4063177551618,0.164293984302377));
#41157=CARTESIAN_POINT('Ctrl Pts',(-22.8439709668546,20.4058466225381,0.164160435194475));
#41158=CARTESIAN_POINT('Ctrl Pts',(-22.8478875659604,20.4049696345513,0.163910960425778));
#41159=CARTESIAN_POINT('Ctrl Pts',(-22.8497097874238,20.4045632731013,0.163795006218067));
#41160=CARTESIAN_POINT('Ctrl Pts',(-22.8538031789774,20.403654166397,0.163534788016768));
#41161=CARTESIAN_POINT('Ctrl Pts',(-22.8560745359861,20.4031522975487,0.16339057542968));
#41162=CARTESIAN_POINT('Ctrl Pts',(-22.8618519881338,20.4018822966713,0.163024203188053));
#41163=CARTESIAN_POINT('Ctrl Pts',(-22.8653588372245,20.4011175595607,0.162802239307252));
#41164=CARTESIAN_POINT('Ctrl Pts',(-22.884747589944,20.3969233813881,0.161577323578932));
#41165=CARTESIAN_POINT('Ctrl Pts',(-22.9006543486063,20.3936081449619,0.160580852238311));
#41166=CARTESIAN_POINT('Ctrl Pts',(-23.2299989063664,20.3275621716161,0.140111144292248));
#41167=CARTESIAN_POINT('Ctrl Pts',(-23.5510772879119,20.3116763547085,0.123048013008246));
#41168=CARTESIAN_POINT('Ctrl Pts',(-23.9797844309823,20.3543253268618,0.098635244908576));
#41169=CARTESIAN_POINT('Ctrl Pts',(-24.0896323544244,20.3710207793976,0.0922494552223906));
#41170=CARTESIAN_POINT('Ctrl Pts',(-24.2654688057172,20.4071216074122,0.0816516820150702));
#41171=CARTESIAN_POINT('Ctrl Pts',(-24.3320841114588,20.4230261819133,0.0775482675371054));
#41172=CARTESIAN_POINT('Ctrl Pts',(-24.406372700293,20.4432847722791,0.072855041176118));
#41173=CARTESIAN_POINT('Ctrl Pts',(-24.4145975693603,20.4455628443371,0.0723338065685653));
#41174=CARTESIAN_POINT('Ctrl Pts',(-24.4268481571589,20.4490083877383,0.0715549941180591));
#41175=CARTESIAN_POINT('Ctrl Pts',(-24.4308808506585,20.4501510987441,0.0712982240746903));
#41176=CARTESIAN_POINT('Ctrl Pts',(-24.4380406120034,20.4521949987125,0.0708416358861511));
#41177=CARTESIAN_POINT('Ctrl Pts',(-24.4411685715318,20.4530930648537,0.0706419199726562));
#41178=CARTESIAN_POINT('Ctrl Pts',(-24.4477607611836,20.4549965564476,0.0702205060665057));
#41179=CARTESIAN_POINT('Ctrl Pts',(-24.4512246722264,20.456003062741,0.0699987729657552));
#41180=CARTESIAN_POINT('Ctrl Pts',(-24.4601388756374,20.4586094945502,0.0694273817279601));
#41181=CARTESIAN_POINT('Ctrl Pts',(-24.4655866240651,20.4602180130039,0.0690774426830349));
#41182=CARTESIAN_POINT('Ctrl Pts',(-24.4871992506722,20.466661590957,0.0676861664964763));
#41183=CARTESIAN_POINT('Ctrl Pts',(-24.5033300772324,20.4716090936248,0.0666411479314599));
#41184=CARTESIAN_POINT('Ctrl Pts',(-24.7810926326637,20.5591941385627,0.0485298550585272));
#41185=CARTESIAN_POINT('Ctrl Pts',(-25.0310975387023,20.6747648142353,0.0302872386054696));
#41186=CARTESIAN_POINT('Ctrl Pts',(-25.3293758929812,20.8619619106936,0.00645562504132138));
#41187=CARTESIAN_POINT('Ctrl Pts',(-25.3938377808542,20.9057525593612,0.00117653361270985));
#41188=CARTESIAN_POINT('Ctrl Pts',(-25.5434226807009,21.0154995282732,-0.0113055845170199));
#41189=CARTESIAN_POINT('Ctrl Pts',(-25.6269598786956,21.0834751391232,-0.0184678596970956));
#41190=CARTESIAN_POINT('Ctrl Pts',(-25.7279007074455,21.1743818913481,-0.0272249476669519));
#41191=CARTESIAN_POINT('Ctrl Pts',(-25.7486085929477,21.1935294616425,-0.0290271458694069));
#41192=CARTESIAN_POINT('Ctrl Pts',(-25.7804074409697,21.2237161991043,-0.0317998457133827));
#41193=CARTESIAN_POINT('Ctrl Pts',(-25.7916733587597,21.2345679836838,-0.0327832292112673));
#41194=CARTESIAN_POINT('Ctrl Pts',(-25.8055295586595,21.2481106969068,-0.0339935117048435));
#41195=CARTESIAN_POINT('Ctrl Pts',(-25.8081945091748,21.2507244230372,-0.034226321148725));
#41196=CARTESIAN_POINT('Ctrl Pts',(-25.8123853361987,21.254849005488,-0.0345924800485561));
#41197=CARTESIAN_POINT('Ctrl Pts',(-25.8139142434358,21.2563567563384,-0.0347260733503726));
#41198=CARTESIAN_POINT('Ctrl Pts',(-25.8167696111653,21.259178247359,-0.0349755878625767));
#41199=CARTESIAN_POINT('Ctrl Pts',(-25.8180964280798,21.2604916032282,-0.0350915377095388));
#41200=CARTESIAN_POINT('Ctrl Pts',(-25.8210731871779,21.2634432874672,-0.0353516912653111));
#41201=CARTESIAN_POINT('Ctrl Pts',(-25.822722494452,21.2650822454113,-0.0354958436799492));
#41202=CARTESIAN_POINT('Ctrl Pts',(-25.8269110237644,21.2692535108402,-0.0358619622122694));
#41203=CARTESIAN_POINT('Ctrl Pts',(-25.8294478030405,21.2717882818079,-0.0360837330245468));
#41204=CARTESIAN_POINT('Ctrl Pts',(-25.8434271067988,21.2858032265454,-0.037306044894854));
#41205=CARTESIAN_POINT('Ctrl Pts',(-25.8547873957157,21.297365633975,-0.0383001375012151));
#41206=CARTESIAN_POINT('Ctrl Pts',(-26.0846180650061,21.5348430468127,-0.0584402269181293));
#41207=CARTESIAN_POINT('Ctrl Pts',(-26.2690097287303,21.7914686636345,-0.0752522841314742));
#41208=CARTESIAN_POINT('Ctrl Pts',(-26.4950549821759,22.2289121301765,-0.103114262930192));
#41209=CARTESIAN_POINT('Ctrl Pts',(-26.5635170066255,22.3935221853769,-0.113423636470402));
#41210=CARTESIAN_POINT('Ctrl Pts',(-26.6221287606919,22.5756385925777,-0.12504545751006));
#41211=CARTESIAN_POINT('Ctrl Pts',(-26.6261408633413,22.588375793527,-0.125859245529396));
#41212=CARTESIAN_POINT('Ctrl Pts',(-26.6315748634349,22.6060087949187,-0.126987272201844));
#41213=CARTESIAN_POINT('Ctrl Pts',(-26.6330645207062,22.610883708252,-0.127299284210471));
#41214=CARTESIAN_POINT('Ctrl Pts',(-26.6355585478241,22.619115256608,-0.127826396334402));
#41215=CARTESIAN_POINT('Ctrl Pts',(-26.6365690244515,22.6224700439297,-0.128041295836377));
#41216=CARTESIAN_POINT('Ctrl Pts',(-26.6385567882603,22.6291086125849,-0.128466694786657));
#41217=CARTESIAN_POINT('Ctrl Pts',(-26.6395343137876,22.6323923182024,-0.128677186100811));
#41218=CARTESIAN_POINT('Ctrl Pts',(-26.6416761176096,22.6396292514416,-0.129141246939347));
#41219=CARTESIAN_POINT('Ctrl Pts',(-26.6428380519084,22.6435831619635,-0.12939489283442));
#41220=CARTESIAN_POINT('Ctrl Pts',(-26.646863658873,22.657379548205,-0.130280314817266));
#41221=CARTESIAN_POINT('Ctrl Pts',(-26.6496879310761,22.6672333706485,-0.130913376745396));
#41222=CARTESIAN_POINT('Ctrl Pts',(-26.6778635784282,22.7673383186684,-0.137351691139239));
#41223=CARTESIAN_POINT('Ctrl Pts',(-26.6993102963944,22.8586328662693,-0.143283359476885));
#41224=CARTESIAN_POINT('Ctrl Pts',(-26.735140659056,23.0478763022963,-0.155719553475827));
#41225=CARTESIAN_POINT('Ctrl Pts',(-26.7490525265102,23.1458146722644,-0.162231271757614));
#41226=CARTESIAN_POINT('Ctrl Pts',(-26.7682348801184,23.3469133100907,-0.175716306674401));
#41227=CARTESIAN_POINT('Ctrl Pts',(-26.77309380282,23.4500034301552,-0.182689934824677));
#41228=CARTESIAN_POINT('Ctrl Pts',(-26.7728461899883,23.7258964258954,-0.201365712422515));
#41229=CARTESIAN_POINT('Ctrl Pts',(-26.7588011919433,23.8983710442638,-0.213063909669046));
#41230=CARTESIAN_POINT('Ctrl Pts',(-26.7304311277122,24.0723578196513,-0.224431325583277));
#41231=CARTESIAN_POINT('Ctrl Pts',(-26.7298617210067,24.0758143622566,-0.224656975511129));
#41232=CARTESIAN_POINT('Ctrl Pts',(-26.7230044100128,24.1170221251666,-0.227344862316903));
#41233=CARTESIAN_POINT('Ctrl Pts',(-26.7160498075461,24.1546614865963,-0.229777613971489));
#41234=CARTESIAN_POINT('Ctrl Pts',(-26.7073782871479,24.1973245473106,-0.232502702669006));
#41235=CARTESIAN_POINT('Ctrl Pts',(-26.7063179754438,24.2024765306747,-0.232831244323582));
#41236=CARTESIAN_POINT('Ctrl Pts',(-26.7047476509662,24.2100131330414,-0.233311039571711));
#41237=CARTESIAN_POINT('Ctrl Pts',(-26.704247544517,24.2123997719544,-0.233462858298347));
#41238=CARTESIAN_POINT('Ctrl Pts',(-26.7033561502634,24.2166298154194,-0.233731724833956));
#41239=CARTESIAN_POINT('Ctrl Pts',(-26.702965954197,24.2184734452728,-0.233848835686228));
#41240=CARTESIAN_POINT('Ctrl Pts',(-26.702146465012,24.2223287376662,-0.234093578604118));
#41241=CARTESIAN_POINT('Ctrl Pts',(-26.7017168639319,24.224340327319,-0.234221192360505));
#41242=CARTESIAN_POINT('Ctrl Pts',(-26.7005870248269,24.2296060653125,-0.234555023295103));
#41243=CARTESIAN_POINT('Ctrl Pts',(-26.6998836683004,24.2328595532082,-0.234761060351634));
#41244=CARTESIAN_POINT('Ctrl Pts',(-26.6967792709118,24.2471124847494,-0.235662713551194));
#41245=CARTESIAN_POINT('Ctrl Pts',(-26.6943256035827,24.2581005678354,-0.2363553299075));
#41246=CARTESIAN_POINT('Ctrl Pts',(-26.6759513950936,24.3384036380501,-0.241400299574725));
#41247=CARTESIAN_POINT('Ctrl Pts',(-26.6577964796317,24.4071935558015,-0.245630292851446));
#41248=CARTESIAN_POINT('Ctrl Pts',(-26.6146562079719,24.5511589707876,-0.254396239781917));
#41249=CARTESIAN_POINT('Ctrl Pts',(-26.5891467834824,24.6261273795643,-0.258909972711792));
#41250=CARTESIAN_POINT('Ctrl Pts',(-26.4397431226913,25.0173168125652,-0.282545749088872));
#41251=CARTESIAN_POINT('Ctrl Pts',(-26.2692292869155,25.3133720586982,-0.300999264206647));
#41252=CARTESIAN_POINT('Ctrl Pts',(-26.0432001403632,25.592731654574,-0.322738542431323));
#41253=CARTESIAN_POINT('Ctrl Pts',(-26.0306185174856,25.6079923831733,-0.32394063699489));
#41254=CARTESIAN_POINT('Ctrl Pts',(-26.0139229217475,25.6278674995866,-0.325525810478143));
#41255=CARTESIAN_POINT('Ctrl Pts',(-26.009934829622,25.6325874562575,-0.325903727421661));
#41256=CARTESIAN_POINT('Ctrl Pts',(-26.0037528256426,25.6398613960511,-0.326488423432875));
#41257=CARTESIAN_POINT('Ctrl Pts',(-26.0015684294766,25.6424234777562,-0.326694810037525));
#41258=CARTESIAN_POINT('Ctrl Pts',(-25.9972064383223,25.6475234546308,-0.327106516747561));
#41259=CARTESIAN_POINT('Ctrl Pts',(-25.9950289000438,25.6500613929917,-0.327311834363868));
#41260=CARTESIAN_POINT('Ctrl Pts',(-25.9901871588031,25.6556867406035,-0.327767895325005));
#41261=CARTESIAN_POINT('Ctrl Pts',(-25.9875210412345,25.6587724876752,-0.328018717946543));
#41262=CARTESIAN_POINT('Ctrl Pts',(-25.9797939441341,25.6676815416659,-0.328744782312228));
#41263=CARTESIAN_POINT('Ctrl Pts',(-25.9747179268682,25.6734917158124,-0.329220650069114));
#41264=CARTESIAN_POINT('Ctrl Pts',(-25.9398846473205,25.7130752358933,-0.332478865905345));
#41265=CARTESIAN_POINT('Ctrl Pts',(-25.9094447675075,25.746238724928,-0.335289815172548));
#41266=CARTESIAN_POINT('Ctrl Pts',(-25.8288050456904,25.8304814154994,-0.342649284810011));
#41267=CARTESIAN_POINT('Ctrl Pts',(-25.7775816219825,25.8805420338546,-0.347241275070761));
#41268=CARTESIAN_POINT('Ctrl Pts',(-25.6140486675017,26.0300416720214,-0.361655314787619));
#41269=CARTESIAN_POINT('Ctrl Pts',(-25.4964434713283,26.1233714928482,-0.371693085323411));
#41270=CARTESIAN_POINT('Ctrl Pts',(-25.1773924521551,26.342144303118,-0.397836721284272));
#41271=CARTESIAN_POINT('Ctrl Pts',(-24.9678089969649,26.4541808049471,-0.414039348090076));
#41272=CARTESIAN_POINT('Ctrl Pts',(-24.7353086134694,26.5472412323637,-0.429850228012322));
#41273=CARTESIAN_POINT('Ctrl Pts',(-24.7227652056926,26.5521707906457,-0.430696741768996));
#41274=CARTESIAN_POINT('Ctrl Pts',(-24.7067613316152,26.5583446963806,-0.431768219570169));
#41275=CARTESIAN_POINT('Ctrl Pts',(-24.703329398214,26.5596619115826,-0.431997491654009));
#41276=CARTESIAN_POINT('Ctrl Pts',(-24.6978808305264,26.5617424452658,-0.432360684920211));
#41277=CARTESIAN_POINT('Ctrl Pts',(-24.6958656842691,26.5625096117816,-0.432494837905251));
#41278=CARTESIAN_POINT('Ctrl Pts',(-24.6921395247644,26.5639238813658,-0.432742574217777));
#41279=CARTESIAN_POINT('Ctrl Pts',(-24.6904287414695,26.5645715459103,-0.432856190966694));
#41280=CARTESIAN_POINT('Ctrl Pts',(-24.6866150365703,26.5660116185794,-0.433109187484006));
#41281=CARTESIAN_POINT('Ctrl Pts',(-24.6845118419263,26.5668032821118,-0.433248521707288));
#41282=CARTESIAN_POINT('Ctrl Pts',(-24.6801299824222,26.5684474272943,-0.433538424510278));
#41283=CARTESIAN_POINT('Ctrl Pts',(-24.6778511755879,26.5692995303135,-0.43368897025165));
#41284=CARTESIAN_POINT('Ctrl Pts',(-24.6719552802554,26.5714965467324,-0.434077910884803));
#41285=CARTESIAN_POINT('Ctrl Pts',(-24.668336723943,26.5728375501745,-0.434316073145402));
#41286=CARTESIAN_POINT('Ctrl Pts',(-24.6577395903057,26.5767431156185,-0.435011968950935));
#41287=CARTESIAN_POINT('Ctrl Pts',(-24.6507544791301,26.5792900530515,-0.43546867317455));
#41288=CARTESIAN_POINT('Ctrl Pts',(-24.5771981469014,26.6058224094536,-0.440257626357364));
#41289=CARTESIAN_POINT('Ctrl Pts',(-24.5098571976897,26.6276353794079,-0.444467007518637));
#41290=CARTESIAN_POINT('Ctrl Pts',(-24.3664640035169,26.6689173080416,-0.453172340694728));
#41291=CARTESIAN_POINT('Ctrl Pts',(-24.2903094343048,26.6878612195325,-0.457647067955348));
#41292=CARTESIAN_POINT('Ctrl Pts',(-23.8803664704533,26.7740785069709,-0.481299136526181));
#41293=CARTESIAN_POINT('Ctrl Pts',(-23.5382393407314,26.7909125068505,-0.499791292278699));
#41294=CARTESIAN_POINT('Ctrl Pts',(-23.1799547185387,26.7517203365284,-0.52159301522342));
#41295=CARTESIAN_POINT('Ctrl Pts',(-23.1601188314851,26.7493636963513,-0.522806993769418));
#41296=CARTESIAN_POINT('Ctrl Pts',(-23.1341534109168,26.7460337455871,-0.524405635664677));
#41297=CARTESIAN_POINT('Ctrl Pts',(-23.1280026723124,26.7452268822617,-0.524785026784344));
#41298=CARTESIAN_POINT('Ctrl Pts',(-23.1185124949875,26.743954063145,-0.525371498009442));
#41299=CARTESIAN_POINT('Ctrl Pts',(-23.1151713701045,26.7435006138167,-0.525578181753649));
#41300=CARTESIAN_POINT('Ctrl Pts',(-23.1085183921398,26.7425870524723,-0.525990159056699));
#41301=CARTESIAN_POINT('Ctrl Pts',(-23.105206531108,26.7421270279469,-0.526195449604739));
#41302=CARTESIAN_POINT('Ctrl Pts',(-23.0978650973423,26.7410956390393,-0.526650982364138));
#41303=CARTESIAN_POINT('Ctrl Pts',(-23.0938358838619,26.7405217945919,-0.526901302927074));
#41304=CARTESIAN_POINT('Ctrl Pts',(-23.0822095264602,26.7388434813631,-0.527624506576167));
#41305=CARTESIAN_POINT('Ctrl Pts',(-23.0746152667785,26.7377195024483,-0.528098008058565));
#41306=CARTESIAN_POINT('Ctrl Pts',(-23.0233328907344,26.7299421666856,-0.531303048318972));
#41307=CARTESIAN_POINT('Ctrl Pts',(-22.9797834165328,26.7224182206039,-0.534062133465268));
#41308=CARTESIAN_POINT('Ctrl Pts',(-22.8780061887156,26.7026708282401,-0.540602217432489));
#41309=CARTESIAN_POINT('Ctrl Pts',(-22.8199365091347,26.6897260588641,-0.544405174985379));
#41310=CARTESIAN_POINT('Ctrl Pts',(-22.6837477852807,26.6553843177723,-0.553495599609622));
#41311=CARTESIAN_POINT('Ctrl Pts',(-22.6060135927911,26.6326355583656,-0.558820276853013));
#41312=CARTESIAN_POINT('Ctrl Pts',(-22.3729489478991,26.5547858055371,-0.575171464795435));
#41313=CARTESIAN_POINT('Ctrl Pts',(-22.2211232282342,26.4907510558054,-0.586370102522171));
#41314=CARTESIAN_POINT('Ctrl Pts',(-22.0750358767111,26.4155367031789,-0.597455529348902));
#41315=CARTESIAN_POINT('',(-26.7730021510373,23.5486861587587,-0.433369846446908));
#41316=CARTESIAN_POINT('Ctrl Pts',(-22.0750363147453,26.4155369287046,-0.841310143832836));
#41317=CARTESIAN_POINT('Ctrl Pts',(-22.1918959590995,26.4757031176658,-0.832483085698408));
#41318=CARTESIAN_POINT('Ctrl Pts',(-22.3123968422096,26.5286998695453,-0.823785630732621));
#41319=CARTESIAN_POINT('Ctrl Pts',(-22.4469193609948,26.5782736674178,-0.814748539363253));
#41320=CARTESIAN_POINT('Ctrl Pts',(-22.4579852758515,26.5822829299526,-0.814009994337906));
#41321=CARTESIAN_POINT('Ctrl Pts',(-22.4723994529638,26.58741613792,-0.813054511133772));
#41322=CARTESIAN_POINT('Ctrl Pts',(-22.4757277613118,26.588595262268,-0.812834336061839));
#41323=CARTESIAN_POINT('Ctrl Pts',(-22.4808428650176,26.5903979408247,-0.812496660141599));
#41324=CARTESIAN_POINT('Ctrl Pts',(-22.4826282693482,26.5910253904148,-0.812378926626182));
#41325=CARTESIAN_POINT('Ctrl Pts',(-22.4860037179556,26.5922082943084,-0.812156590560344));
#41326=CARTESIAN_POINT('Ctrl Pts',(-22.4875936376374,26.5927640722077,-0.812051969046023));
#41327=CARTESIAN_POINT('Ctrl Pts',(-22.4912258690637,26.5940305732807,-0.811813195049276));
#41328=CARTESIAN_POINT('Ctrl Pts',(-22.4932684569645,26.5947404860865,-0.811679091665356));
#41329=CARTESIAN_POINT('Ctrl Pts',(-22.4989641769027,26.5967136423387,-0.811305620165246));
#41330=CARTESIAN_POINT('Ctrl Pts',(-22.5026188848862,26.5979723754523,-0.811066521380125));
#41331=CARTESIAN_POINT('Ctrl Pts',(-22.5107813783029,26.600767236343,-0.810533705104373));
#41332=CARTESIAN_POINT('Ctrl Pts',(-22.5152903329119,26.6022999575678,-0.810240187568537));
#41333=CARTESIAN_POINT('Ctrl Pts',(-22.5291937717427,26.6069917758105,-0.809337566395588));
#41334=CARTESIAN_POINT('Ctrl Pts',(-22.5385995513683,26.6101175697421,-0.808730371139305));
#41335=CARTESIAN_POINT('Ctrl Pts',(-22.5734856241607,26.6215327072147,-0.806490462878175));
#41336=CARTESIAN_POINT('Ctrl Pts',(-22.5990553661165,26.6295478349863,-0.804872722669587));
#41337=CARTESIAN_POINT('Ctrl Pts',(-22.6897370908625,26.6567356745358,-0.799210185580214));
#41338=CARTESIAN_POINT('Ctrl Pts',(-22.7553552489818,26.6741705685107,-0.795247710534378));
#41339=CARTESIAN_POINT('Ctrl Pts',(-23.2029480943067,26.7780781123869,-0.768826597802522));
#41340=CARTESIAN_POINT('Ctrl Pts',(-23.5973444654112,26.7963734817766,-0.748049077700995));
#41341=CARTESIAN_POINT('Ctrl Pts',(-24.004569985287,26.7408773391201,-0.723179021927088));
#41342=CARTESIAN_POINT('Ctrl Pts',(-24.0236936060035,26.738095773486,-0.722004304385006));
#41343=CARTESIAN_POINT('Ctrl Pts',(-24.0488417516076,26.734206652401,-0.720450186398075));
#41344=CARTESIAN_POINT('Ctrl Pts',(-24.0548900552158,26.7332536347439,-0.720075698370171));
#41345=CARTESIAN_POINT('Ctrl Pts',(-24.0642488285811,26.7317516484153,-0.719495124017312));
#41346=CARTESIAN_POINT('Ctrl Pts',(-24.0675612412363,26.7312147323194,-0.719289421140707));
#41347=CARTESIAN_POINT('Ctrl Pts',(-24.0738440823315,26.7301862598864,-0.718898839913368));
#41348=CARTESIAN_POINT('Ctrl Pts',(-24.0768146742458,26.7296957121158,-0.718713993839199));
#41349=CARTESIAN_POINT('Ctrl Pts',(-24.0836841870394,26.7285514258461,-0.718286128660739));
#41350=CARTESIAN_POINT('Ctrl Pts',(-24.087582595005,26.7278946755377,-0.718043013917701));
#41351=CARTESIAN_POINT('Ctrl Pts',(-24.0985144021371,26.7260323424104,-0.717360420663766));
#41352=CARTESIAN_POINT('Ctrl Pts',(-24.1055449879307,26.7248105751813,-0.716920427092435));
#41353=CARTESIAN_POINT('Ctrl Pts',(-24.1463156897247,26.7175859062542,-0.714363037019959));
#41354=CARTESIAN_POINT('Ctrl Pts',(-24.17996133793,26.7110686710813,-0.712229287059696));
#41355=CARTESIAN_POINT('Ctrl Pts',(-24.2768422934146,26.6906944038584,-0.706015222023742));
#41356=CARTESIAN_POINT('Ctrl Pts',(-24.3397692170871,26.6754677680556,-0.701891876686825));
#41357=CARTESIAN_POINT('Ctrl Pts',(-24.5716825349564,26.6118997727916,-0.686363409808072));
#41358=CARTESIAN_POINT('Ctrl Pts',(-24.7370689247855,26.551661505447,-0.674603697452908));
#41359=CARTESIAN_POINT('Ctrl Pts',(-24.9650191426792,26.4468379667959,-0.65763781899987));
#41360=CARTESIAN_POINT('Ctrl Pts',(-25.0322160082494,26.41304069718,-0.65253955888881));
#41361=CARTESIAN_POINT('Ctrl Pts',(-25.1898793976965,26.3267024649186,-0.640411923944332));
#41362=CARTESIAN_POINT('Ctrl Pts',(-25.2790978469107,26.2720437575327,-0.633411823862365));
#41363=CARTESIAN_POINT('Ctrl Pts',(-25.3753922565699,26.2064011899725,-0.625814748918397));
#41364=CARTESIAN_POINT('Ctrl Pts',(-25.3852407423554,26.1996069785357,-0.625037279936702));
#41365=CARTESIAN_POINT('Ctrl Pts',(-25.3966811073754,26.1916201752299,-0.624133784990768));
#41366=CARTESIAN_POINT('Ctrl Pts',(-25.3983098616422,26.1904808586814,-0.62400514673842));
#41367=CARTESIAN_POINT('Ctrl Pts',(-25.4037912926175,26.1866390304628,-0.62357219995578));
#41368=CARTESIAN_POINT('Ctrl Pts',(-25.4076391223868,26.1839295738487,-0.623268238767382));
#41369=CARTESIAN_POINT('Ctrl Pts',(-25.4135267678604,26.1797644565317,-0.622803091602461));
#41370=CARTESIAN_POINT('Ctrl Pts',(-25.4155708275809,26.1783148401515,-0.622641593623739));
#41371=CARTESIAN_POINT('Ctrl Pts',(-25.4498287265583,26.1539595511138,-0.619934803102744));
#41372=CARTESIAN_POINT('Ctrl Pts',(-25.4816220249929,26.1304641892959,-0.617420831748965));
#41373=CARTESIAN_POINT('Ctrl Pts',(-25.5171873745454,26.103155402757,-0.614613886052682));
#41374=CARTESIAN_POINT('Ctrl Pts',(-25.5213900531472,26.0999118457169,-0.614282281215068));
#41375=CARTESIAN_POINT('Ctrl Pts',(-25.5275188083326,26.095157564381,-0.613798852146006));
#41376=CARTESIAN_POINT('Ctrl Pts',(-25.529451181003,26.0936550285076,-0.613646450621238));
#41377=CARTESIAN_POINT('Ctrl Pts',(-25.5328693675954,26.0909909285638,-0.613376908017485));
#41378=CARTESIAN_POINT('Ctrl Pts',(-25.534355874656,26.0898302611304,-0.613259702829827));
#41379=CARTESIAN_POINT('Ctrl Pts',(-25.5372174959365,26.0875918558252,-0.613034103258723));
#41380=CARTESIAN_POINT('Ctrl Pts',(-25.5385927478522,26.0865143083552,-0.612925695762816));
#41381=CARTESIAN_POINT('Ctrl Pts',(-25.5422968310571,26.0836071935239,-0.612633743570966));
#41382=CARTESIAN_POINT('Ctrl Pts',(-25.5446240250329,26.0817755278301,-0.612450349458289));
#41383=CARTESIAN_POINT('Ctrl Pts',(-25.5534476327734,26.0748110077101,-0.611755117886821));
#41384=CARTESIAN_POINT('Ctrl Pts',(-25.5599268563628,26.0696562754687,-0.611244834929675));
#41385=CARTESIAN_POINT('Ctrl Pts',(-25.576004838508,26.0567634858304,-0.609978953580685));
#41386=CARTESIAN_POINT('Ctrl Pts',(-25.585579285352,26.0489951332312,-0.609225450444682));
#41387=CARTESIAN_POINT('Ctrl Pts',(-25.6230091478245,26.0182680445942,-0.606279984041182));
#41388=CARTESIAN_POINT('Ctrl Pts',(-25.6505237344633,25.9948959982704,-0.604115303526411));
#41389=CARTESIAN_POINT('Ctrl Pts',(-25.7261447007332,25.9284409778457,-0.598148569295593));
#41390=CARTESIAN_POINT('Ctrl Pts',(-25.7733592726218,25.8843657294892,-0.594402894442797));
#41391=CARTESIAN_POINT('Ctrl Pts',(-26.0062861855531,25.6534416356921,-0.575627077735363));
#41392=CARTESIAN_POINT('Ctrl Pts',(-26.169911070631,25.445748978468,-0.561351382405291));
#41393=CARTESIAN_POINT('Ctrl Pts',(-26.3335894777414,25.1756440581429,-0.543184384200481));
#41394=CARTESIAN_POINT('Ctrl Pts',(-26.3596425931045,25.1301858429121,-0.540142650404));
#41395=CARTESIAN_POINT('Ctrl Pts',(-26.3886519017998,25.0765814417388,-0.53656234992002));
#41396=CARTESIAN_POINT('Ctrl Pts',(-26.3926984385456,25.0690323678068,-0.536058291059274));
#41397=CARTESIAN_POINT('Ctrl Pts',(-26.4295299396103,24.9996580601409,-0.531427153743921));
#41398=CARTESIAN_POINT('Ctrl Pts',(-26.4603210531502,24.9368003484797,-0.527238064177088));
#41399=CARTESIAN_POINT('Ctrl Pts',(-26.4929304955564,24.8643506253012,-0.522398981515381));
#41400=CARTESIAN_POINT('Ctrl Pts',(-26.4967825305603,24.8556905276877,-0.521820393960499));
#41401=CARTESIAN_POINT('Ctrl Pts',(-26.5023613613589,24.8429977745731,-0.520972104266465));
#41402=CARTESIAN_POINT('Ctrl Pts',(-26.5041182399141,24.8389783297875,-0.520703433809886));
#41403=CARTESIAN_POINT('Ctrl Pts',(-26.5072167905813,24.831849738715,-0.520226863002594));
#41404=CARTESIAN_POINT('Ctrl Pts',(-26.5085617817672,24.8287420350426,-0.520019076569772));
#41405=CARTESIAN_POINT('Ctrl Pts',(-26.5113443834544,24.8222847225499,-0.519587273469587));
#41406=CARTESIAN_POINT('Ctrl Pts',(-26.5127812134829,24.8189347844821,-0.519363230504296));
#41407=CARTESIAN_POINT('Ctrl Pts',(-26.5164698165109,24.8102944518615,-0.518785283022863));
#41408=CARTESIAN_POINT('Ctrl Pts',(-26.5187131134266,24.8050004726527,-0.518431090052694));
#41409=CARTESIAN_POINT('Ctrl Pts',(-26.5280007512499,24.782918169432,-0.51695331458252));
#41410=CARTESIAN_POINT('Ctrl Pts',(-26.5349168229369,24.7660765651026,-0.515825380618384));
#41411=CARTESIAN_POINT('Ctrl Pts',(-26.6552803236543,24.4657576550718,-0.495693907005689));
#41412=CARTESIAN_POINT('Ctrl Pts',(-26.7279911436311,24.167694796446,-0.475200616383863));
#41413=CARTESIAN_POINT('Ctrl Pts',(-26.7679455708432,23.759182062243,-0.447428429760582));
#41414=CARTESIAN_POINT('Ctrl Pts',(-26.7730533208591,23.6539660190022,-0.440326684895173));
#41415=CARTESIAN_POINT('Ctrl Pts',(-26.7730021510373,23.5486861587587,-0.433369846446908));
#41416=CARTESIAN_POINT('Ctrl Pts',(-26.773002148774,23.5486815090728,-0.433369539198178));
#41417=CARTESIAN_POINT('Ctrl Pts',(-26.7729606909923,23.4636362345256,-0.427749795259021));
#41418=CARTESIAN_POINT('Ctrl Pts',(-26.7695528295525,23.3786153665292,-0.422229805789728));
#41419=CARTESIAN_POINT('Ctrl Pts',(-26.7624563038197,23.2897118072575,-0.416627183339296));
#41420=CARTESIAN_POINT('Ctrl Pts',(-26.7621205403511,23.2856047692772,-0.416368743239842));
#41421=CARTESIAN_POINT('Ctrl Pts',(-26.7614599942432,23.2777114595341,-0.415872796195772));
#41422=CARTESIAN_POINT('Ctrl Pts',(-26.7611363903938,23.273925099402,-0.41563522544598));
#41423=CARTESIAN_POINT('Ctrl Pts',(-26.7605967693513,23.267740164003,-0.415247709940809));
#41424=CARTESIAN_POINT('Ctrl Pts',(-26.7603847606628,23.2653412564105,-0.41509754249434));
#41425=CARTESIAN_POINT('Ctrl Pts',(-26.7600056746364,23.2611059875934,-0.414832663968443));
#41426=CARTESIAN_POINT('Ctrl Pts',(-26.7598397101878,23.2592695317042,-0.414717890268604));
#41427=CARTESIAN_POINT('Ctrl Pts',(-26.7595092345212,23.255647383065,-0.414491675273463));
#41428=CARTESIAN_POINT('Ctrl Pts',(-26.7593448087476,23.253861682207,-0.414380229125421));
#41429=CARTESIAN_POINT('Ctrl Pts',(-26.7590137519495,23.2502989025832,-0.414158028929345));
#41430=CARTESIAN_POINT('Ctrl Pts',(-26.7588471354849,23.2485218292531,-0.414047274311157));
#41431=CARTESIAN_POINT('Ctrl Pts',(-26.7584439880963,23.2442600954756,-0.413781846279013));
#41432=CARTESIAN_POINT('Ctrl Pts',(-26.7582060464848,23.2417755649755,-0.413627253059689));
#41433=CARTESIAN_POINT('Ctrl Pts',(-26.7574718173178,23.2342016425685,-0.413156429265943));
#41434=CARTESIAN_POINT('Ctrl Pts',(-26.7569662998405,23.2291131217427,-0.412840717630414));
#41435=CARTESIAN_POINT('Ctrl Pts',(-26.7513427504129,23.1738441942195,-0.409418039451498));
#41436=CARTESIAN_POINT('Ctrl Pts',(-26.7450590604961,23.1237859262715,-0.406375555810663));
#41437=CARTESIAN_POINT('Ctrl Pts',(-26.7370975668604,23.070515160457,-0.403179706209221));
#41438=CARTESIAN_POINT('Ctrl Pts',(-26.7365874464137,23.06713863731,-0.402977320370541));
#41439=CARTESIAN_POINT('Ctrl Pts',(-26.7340947702606,23.0508151313361,-0.401999748975227));
#41440=CARTESIAN_POINT('Ctrl Pts',(-26.7320386390126,23.037879333752,-0.401227630439692));
#41441=CARTESIAN_POINT('Ctrl Pts',(-26.7275356033897,23.0106221784376,-0.399605448785137));
#41442=CARTESIAN_POINT('Ctrl Pts',(-26.7250705988577,22.9963040789598,-0.398756099422074));
#41443=CARTESIAN_POINT('Ctrl Pts',(-26.7202797440528,22.9695591073477,-0.397173981295573));
#41444=CARTESIAN_POINT('Ctrl Pts',(-26.7179774418262,22.9571283616891,-0.396440412217942));
#41445=CARTESIAN_POINT('Ctrl Pts',(-26.6665346735377,22.6882212334434,-0.380604037349782));
#41446=CARTESIAN_POINT('Ctrl Pts',(-26.5864733051594,22.4386342469413,-0.366468616055812));
#41447=CARTESIAN_POINT('Ctrl Pts',(-26.4314585396456,22.1022559708833,-0.345342863188886));
#41448=CARTESIAN_POINT('Ctrl Pts',(-26.380747996997,22.0054761354431,-0.339007479498481));
#41449=CARTESIAN_POINT('Ctrl Pts',(-26.3002746763841,21.8692101003068,-0.329577500096659));
#41450=CARTESIAN_POINT('Ctrl Pts',(-26.274361485691,21.8275350686512,-0.326620909519834));
#41451=CARTESIAN_POINT('Ctrl Pts',(-26.2431884874025,21.7798639322464,-0.323147545779706));
#41452=CARTESIAN_POINT('Ctrl Pts',(-26.2388447515165,21.7732742739868,-0.322665353759454));
#41453=CARTESIAN_POINT('Ctrl Pts',(-26.2321991935727,21.7632727881937,-0.321930331658308));
#41454=CARTESIAN_POINT('Ctrl Pts',(-26.2299149478962,21.7598492710331,-0.321678164530393));
#41455=CARTESIAN_POINT('Ctrl Pts',(-26.2259399757596,21.7539164218641,-0.321240175141211));
#41456=CARTESIAN_POINT('Ctrl Pts',(-26.2242522578145,21.7514050722311,-0.321054466839019));
#41457=CARTESIAN_POINT('Ctrl Pts',(-26.2207355309599,21.7461880153082,-0.320668032431311));
#41458=CARTESIAN_POINT('Ctrl Pts',(-26.218905941577,21.7434827050592,-0.320467284451658));
#41459=CARTESIAN_POINT('Ctrl Pts',(-26.214434354981,21.736892432846,-0.319977365930073));
#41460=CARTESIAN_POINT('Ctrl Pts',(-26.2117879740945,21.7330104663354,-0.319688028948727));
#41461=CARTESIAN_POINT('Ctrl Pts',(-26.2017222860675,21.7183142965163,-0.318589799752796));
#41462=CARTESIAN_POINT('Ctrl Pts',(-26.1942455597744,21.7075397447535,-0.317778719778919));
#41463=CARTESIAN_POINT('Ctrl Pts',(-26.0641342240194,21.5224612402907,-0.303743093236472));
#41464=CARTESIAN_POINT('Ctrl Pts',(-25.924598474026,21.3607348650812,-0.289834077523667));
#41465=CARTESIAN_POINT('Ctrl Pts',(-25.6523232109758,21.102021266223,-0.264621249295177));
#41466=CARTESIAN_POINT('Ctrl Pts',(-25.5261930773607,20.9991360683353,-0.25353197399763));
#41467=CARTESIAN_POINT('Ctrl Pts',(-25.3336111082468,20.8649291343552,-0.237806305414943));
#41468=CARTESIAN_POINT('Ctrl Pts',(-25.2730066683117,20.825651823641,-0.233015969421886));
#41469=CARTESIAN_POINT('Ctrl Pts',(-25.1768891738189,20.7678493798572,-0.225714613407133));
#41470=CARTESIAN_POINT('Ctrl Pts',(-25.1422659163654,20.7478949923283,-0.223141795897741));
#41471=CARTESIAN_POINT('Ctrl Pts',(-25.0956483341677,20.7221708794438,-0.219762057008459));
#41472=CARTESIAN_POINT('Ctrl Pts',(-25.0839780860035,20.7158249076009,-0.21892289988479));
#41473=CARTESIAN_POINT('Ctrl Pts',(-25.0645224101568,20.7054007731002,-0.217535818154493));
#41474=CARTESIAN_POINT('Ctrl Pts',(-25.056759064754,20.7012820398612,-0.216985456570053));
#41475=CARTESIAN_POINT('Ctrl Pts',(-25.046300475251,20.6957880869343,-0.216248310113245));
#41476=CARTESIAN_POINT('Ctrl Pts',(-25.0436200959089,20.6943848817233,-0.216059767711152));
#41477=CARTESIAN_POINT('Ctrl Pts',(-25.0393871947932,20.6921765046775,-0.21576261785026));
#41478=CARTESIAN_POINT('Ctrl Pts',(-25.0378359954855,20.6913688230869,-0.215653850439024));
#41479=CARTESIAN_POINT('Ctrl Pts',(-25.0346161893533,20.6896956580052,-0.215428347513663));
#41480=CARTESIAN_POINT('Ctrl Pts',(-25.0329474943046,20.6888303776502,-0.215311625825309));
#41481=CARTESIAN_POINT('Ctrl Pts',(-25.029142425741,20.6868615305094,-0.21504580351432));
#41482=CARTESIAN_POINT('Ctrl Pts',(-25.0270055762432,20.6857588958336,-0.214896762760868));
#41483=CARTESIAN_POINT('Ctrl Pts',(-25.0203483191145,20.6823331169821,-0.214433172708095));
#41484=CARTESIAN_POINT('Ctrl Pts',(-25.0158236203729,20.6800182593149,-0.214119147782663));
#41485=CARTESIAN_POINT('Ctrl Pts',(-24.9809757812688,20.6622938252583,-0.211708627685704));
#41486=CARTESIAN_POINT('Ctrl Pts',(-24.9504144273922,20.6473537394199,-0.209641156124055));
#41487=CARTESIAN_POINT('Ctrl Pts',(-24.9130350509513,20.6298083367712,-0.207161627785425));
#41488=CARTESIAN_POINT('Ctrl Pts',(-24.9064387967506,20.6267393528503,-0.206725910309519));
#41489=CARTESIAN_POINT('Ctrl Pts',(-24.8968915329486,20.6223366434032,-0.206097837133921));
#41490=CARTESIAN_POINT('Ctrl Pts',(-24.8939488657874,20.6209850105352,-0.205904604130387));
#41491=CARTESIAN_POINT('Ctrl Pts',(-24.8647444577383,20.6076240398141,-0.203990313010486));
#41492=CARTESIAN_POINT('Ctrl Pts',(-24.8383236295131,20.5959633755776,-0.202286070668944));
#41493=CARTESIAN_POINT('Ctrl Pts',(-24.6717886517483,20.5251231687292,-0.191694371882658));
#41494=CARTESIAN_POINT('Ctrl Pts',(-24.5277773461167,20.4755649326542,-0.183190617012992));
#41495=CARTESIAN_POINT('Ctrl Pts',(-24.3637953957064,20.4318274357486,-0.173706233545412));
#41496=CARTESIAN_POINT('Ctrl Pts',(-24.3467599656239,20.4274328157201,-0.172723371866494));
#41497=CARTESIAN_POINT('Ctrl Pts',(-24.3100304817221,20.418277833018,-0.170608138082399));
#41498=CARTESIAN_POINT('Ctrl Pts',(-24.2903258211528,20.4135632627511,-0.169475741220546));
#41499=CARTESIAN_POINT('Ctrl Pts',(-24.2474521189368,20.4037317182041,-0.167015028185077));
#41500=CARTESIAN_POINT('Ctrl Pts',(-24.2242684329288,20.3986841841782,-0.165686411223758));
#41501=CARTESIAN_POINT('Ctrl Pts',(-24.1731280777455,20.3881400573309,-0.162756943887326));
#41502=CARTESIAN_POINT('Ctrl Pts',(-24.1451501082827,20.3827572922396,-0.16115512864134));
#41503=CARTESIAN_POINT('Ctrl Pts',(-24.0819507219637,20.371465050308,-0.157533556835172));
#41504=CARTESIAN_POINT('Ctrl Pts',(-24.0466953394981,20.3657686994227,-0.155511021752524));
#41505=CARTESIAN_POINT('Ctrl Pts',(-23.8996681658487,20.3445138513874,-0.147049929284097));
#41506=CARTESIAN_POINT('Ctrl Pts',(-23.7872220803534,20.3342467008128,-0.14051203952232));
#41507=CARTESIAN_POINT('Ctrl Pts',(-23.6245140591477,20.3279703070119,-0.130813876715079));
#41508=CARTESIAN_POINT('Ctrl Pts',(-23.5745159432577,20.3272060889082,-0.127802091865754));
#41509=CARTESIAN_POINT('Ctrl Pts',(-23.5165920601263,20.3276685641337,-0.124269864390859));
#41510=CARTESIAN_POINT('Ctrl Pts',(-23.5086621305321,20.3277611520187,-0.123785363146156));
#41511=CARTESIAN_POINT('Ctrl Pts',(-23.4966095657719,20.327946370141,-0.123047537720698));
#41512=CARTESIAN_POINT('Ctrl Pts',(-23.4924865933205,20.328017645363,-0.122794884309092));
#41513=CARTESIAN_POINT('Ctrl Pts',(-23.4850173546148,20.3281611088923,-0.122336705278238));
#41514=CARTESIAN_POINT('Ctrl Pts',(-23.4816710373251,20.3282305976105,-0.12213126472485));
#41515=CARTESIAN_POINT('Ctrl Pts',(-23.4749845096964,20.3283798695983,-0.121720415824829));
#41516=CARTESIAN_POINT('Ctrl Pts',(-23.4716443029979,20.3284596345413,-0.121515008301901));
#41517=CARTESIAN_POINT('Ctrl Pts',(-23.4622551133315,20.3286984606867,-0.120937132145645));
#41518=CARTESIAN_POINT('Ctrl Pts',(-23.4562064690344,20.3288693636494,-0.120564292006981));
#41519=CARTESIAN_POINT('Ctrl Pts',(-23.4314057136373,20.329640012593,-0.119033225328796));
#41520=CARTESIAN_POINT('Ctrl Pts',(-23.4126588266654,20.3303864610752,-0.117870400155611));
#41521=CARTESIAN_POINT('Ctrl Pts',(-23.0819183389212,20.3464492935671,-0.0972554456065239));
#41522=CARTESIAN_POINT('Ctrl Pts',(-22.7738440469038,20.4068806787888,-0.0762363995151968));
#41523=CARTESIAN_POINT('Ctrl Pts',(-22.3796152857574,20.5457705854012,-0.0479704283915766));
#41524=CARTESIAN_POINT('Ctrl Pts',(-22.2816469566217,20.5858055874663,-0.0408486610661869));
#41525=CARTESIAN_POINT('Ctrl Pts',(-22.13592105616,20.6539069480672,-0.0302591077162034));
#41526=CARTESIAN_POINT('Ctrl Pts',(-22.0866246376019,20.6785029892014,-0.0266780766157556));
#41527=CARTESIAN_POINT('Ctrl Pts',(-22.0221187322504,20.7127805459983,-0.0220164701104062));
#41528=CARTESIAN_POINT('Ctrl Pts',(-22.0063278487092,20.7213416483775,-0.0208773052456294));
#41529=CARTESIAN_POINT('Ctrl Pts',(-21.9841472163808,20.7336080337546,-0.0192808708216959));
#41530=CARTESIAN_POINT('Ctrl Pts',(-21.9776977003706,20.7372037600922,-0.0188171159473739));
#41531=CARTESIAN_POINT('Ctrl Pts',(-21.9679131029038,20.7427030237857,-0.0181142938672159));
#41532=CARTESIAN_POINT('Ctrl Pts',(-21.9645690242909,20.7445903777682,-0.0178742230540317));
#41533=CARTESIAN_POINT('Ctrl Pts',(-21.9583909345512,20.7480917842342,-0.0174309557304598));
#41534=CARTESIAN_POINT('Ctrl Pts',(-21.9555559902542,20.7497041675325,-0.0172276535590465));
#41535=CARTESIAN_POINT('Ctrl Pts',(-21.9509720257329,20.7523205288224,-0.0168990924890992));
#41536=CARTESIAN_POINT('Ctrl Pts',(-21.9492215008824,20.7533218446958,-0.0167736613907947));
#41537=CARTESIAN_POINT('Ctrl Pts',(-21.9458372213183,20.7552619011751,-0.0165312450178589));
#41538=CARTESIAN_POINT('Ctrl Pts',(-21.9442033549815,20.7562004285914,-0.0164142468032592));
#41539=CARTESIAN_POINT('Ctrl Pts',(-21.940458775714,20.7583557640099,-0.0161461848339086));
#41540=CARTESIAN_POINT('Ctrl Pts',(-21.9383486140854,20.7595735356987,-0.0159951840417283));
#41541=CARTESIAN_POINT('Ctrl Pts',(-21.9316972056332,20.7634221165197,-0.0155193953020725));
#41542=CARTESIAN_POINT('Ctrl Pts',(-21.9271609735171,20.7660616436338,-0.0151951722920524));
#41543=CARTESIAN_POINT('Ctrl Pts',(-21.8898657684265,20.7878849740743,-0.0125315278559098));
#41544=CARTESIAN_POINT('Ctrl Pts',(-21.8574399267222,20.8076361675548,-0.0102283556399859));
#41545=CARTESIAN_POINT('Ctrl Pts',(-21.819503377101,20.8316732807122,-0.00753963268260769));
#41546=CARTESIAN_POINT('Ctrl Pts',(-21.8136497730548,20.8354087718558,-0.00712493104132523));
#41547=CARTESIAN_POINT('Ctrl Pts',(-21.8036174787606,20.8418566279417,-0.00641439455479403));
#41548=CARTESIAN_POINT('Ctrl Pts',(-21.7994329454138,20.8445598003436,-0.00611808735559252));
#41549=CARTESIAN_POINT('Ctrl Pts',(-21.5738929028098,20.9909990317915,0.00985002264757228));
#41550=CARTESIAN_POINT('Ctrl Pts',(-21.3709980081448,21.1613904828752,0.0241573078071055));
#41551=CARTESIAN_POINT('Ctrl Pts',(-21.0907964774909,21.4624578097231,0.0473488945240556));
#41552=CARTESIAN_POINT('Ctrl Pts',(-20.9979720108129,21.5770146053482,0.0557917091615164));
#41553=CARTESIAN_POINT('Ctrl Pts',(-20.8829194181258,21.7407646519255,0.0676947697538534));
#41554=CARTESIAN_POINT('Ctrl Pts',(-20.8535976927702,21.7847598226973,0.070876619068553));
#41555=CARTESIAN_POINT('Ctrl Pts',(-20.821078358248,21.8362541157659,0.0745900659921645));
#41556=CARTESIAN_POINT('Ctrl Pts',(-20.8168097194374,21.8430698733111,0.0750813585106056));
#41557=CARTESIAN_POINT('Ctrl Pts',(-20.8103786900877,21.8534242870177,0.0758274228257293));
#41558=CARTESIAN_POINT('Ctrl Pts',(-20.8081975228632,21.8569512920616,0.0760815006210693));
#41559=CARTESIAN_POINT('Ctrl Pts',(-20.8042834168736,21.8633078993222,0.0765393262519748));
#41560=CARTESIAN_POINT('Ctrl Pts',(-20.8025480261164,21.8661359911502,0.0767429833833166));
#41561=CARTESIAN_POINT('Ctrl Pts',(-20.7988307736843,21.8722148779074,0.0771806708958416));
#41562=CARTESIAN_POINT('Ctrl Pts',(-20.7968503004982,21.8754665122208,0.077414751914649));
#41563=CARTESIAN_POINT('Ctrl Pts',(-20.7915171513188,21.8842577563836,0.0780475170327083));
#41564=CARTESIAN_POINT('Ctrl Pts',(-20.788175414122,21.889803951972,0.0784466014257982));
#41565=CARTESIAN_POINT('Ctrl Pts',(-20.7734007251989,21.9144931439497,0.080222682535859));
#41566=CARTESIAN_POINT('Ctrl Pts',(-20.7621501275273,21.9337440493622,0.0816063142241604));
#41567=CARTESIAN_POINT('Ctrl Pts',(-20.7448461812775,21.9640709423421,0.0837845240337787));
#41568=CARTESIAN_POINT('Ctrl Pts',(-20.7386564549625,21.9750686315261,0.0845741210455968));
#41569=CARTESIAN_POINT('Ctrl Pts',(-20.7259931352688,21.9978808269861,0.0862114097813076));
#41570=CARTESIAN_POINT('Ctrl Pts',(-20.7195287177338,22.0097001216532,0.0870594082772526));
#41571=CARTESIAN_POINT('Ctrl Pts',(-20.712497128932,22.0227501042612,0.0879954132689088));
#41572=CARTESIAN_POINT('Ctrl Pts',(-20.7118563350316,22.0239411537368,0.0880808381641459));
#41573=CARTESIAN_POINT('Ctrl Pts',(-20.707933641809,22.0312433127476,0.0886045501617664));
#41574=CARTESIAN_POINT('Ctrl Pts',(-20.7046707499575,22.0373645644977,0.0890434979533087));
#41575=CARTESIAN_POINT('Ctrl Pts',(-20.6995482469145,22.0470496836921,0.0897379029601386));
#41576=CARTESIAN_POINT('Ctrl Pts',(-20.6976754845388,22.0506066030456,0.0899929054607688));
#41577=CARTESIAN_POINT('Ctrl Pts',(-20.6939370407133,22.0577393338602,0.0905042220648665));
#41578=CARTESIAN_POINT('Ctrl Pts',(-20.692071407356,22.0613151623035,0.090760537242487));
#41579=CARTESIAN_POINT('Ctrl Pts',(-20.6878847249044,22.0693765716923,0.0913383314264424));
#41580=CARTESIAN_POINT('Ctrl Pts',(-20.6855675015034,22.0738641181666,0.0916599394286235));
#41581=CARTESIAN_POINT('Ctrl Pts',(-20.6738016872162,22.096781840704,0.0933022159163836));
#41582=CARTESIAN_POINT('Ctrl Pts',(-20.6645205345106,22.1152970203391,0.094628475933402));
#41583=CARTESIAN_POINT('Ctrl Pts',(-20.523244912024,22.4040453799413,0.115303911667138));
#41584=CARTESIAN_POINT('Ctrl Pts',(-20.4295517822895,22.6913395638239,0.135972502017653));
#41585=CARTESIAN_POINT('Ctrl Pts',(-20.3619476365231,23.0724483536035,0.161869770918256));
#41586=CARTESIAN_POINT('Ctrl Pts',(-20.3502815014377,23.1581138480114,0.167581050839779));
#41587=CARTESIAN_POINT('Ctrl Pts',(-20.3395303333145,23.2707943782117,0.174868411042409));
#41588=CARTESIAN_POINT('Ctrl Pts',(-20.3373201185951,23.2974694025967,0.176577079332786));
#41589=CARTESIAN_POINT('Ctrl Pts',(-20.3347476705051,23.3340486382462,0.178894817366914));
#41590=CARTESIAN_POINT('Ctrl Pts',(-20.3340984681964,23.3439307401517,0.179518437653203));
#41591=CARTESIAN_POINT('Ctrl Pts',(-20.3332047175873,23.3585663916606,0.180438133814038));
#41592=CARTESIAN_POINT('Ctrl Pts',(-20.3329251380838,23.3633176298209,0.180736090488942));
#41593=CARTESIAN_POINT('Ctrl Pts',(-20.3324378965027,23.371922969269,0.181274620044712));
#41594=CARTESIAN_POINT('Ctrl Pts',(-20.3322266314391,23.3757768458631,0.181515391174598));
#41595=CARTESIAN_POINT('Ctrl Pts',(-20.3319077776034,23.381791009188,0.181890480235989));
#41596=CARTESIAN_POINT('Ctrl Pts',(-20.3317954402618,23.3839510241149,0.182025065213579));
#41597=CARTESIAN_POINT('Ctrl Pts',(-20.3315995171785,23.3877927832435,0.182264202151406));
#41598=CARTESIAN_POINT('Ctrl Pts',(-20.3315150752614,23.3894744725308,0.182368802204134));
#41599=CARTESIAN_POINT('Ctrl Pts',(-20.3313244664818,23.3933308506801,0.182608484144308));
#41600=CARTESIAN_POINT('Ctrl Pts',(-20.3312191856129,23.3955055773835,0.182743515185539));
#41601=CARTESIAN_POINT('Ctrl Pts',(-20.3309378137523,23.4014422743092,0.183111772550395));
#41602=CARTESIAN_POINT('Ctrl Pts',(-20.3307661123531,23.405204464204,0.183344751043484));
#41603=CARTESIAN_POINT('Ctrl Pts',(-20.3299708669236,23.4233267204072,0.184465140923115));
#41604=CARTESIAN_POINT('Ctrl Pts',(-20.329436789307,23.4376908427062,0.185347580614001));
#41605=CARTESIAN_POINT('Ctrl Pts',(-20.3184934158106,23.7966875769334,0.207272649390551));
#41606=CARTESIAN_POINT('Ctrl Pts',(-20.3633561116702,24.14083594934,0.225500527842729));
#41607=CARTESIAN_POINT('Ctrl Pts',(-20.4930395730555,24.5756311930454,0.251384422218675));
#41608=CARTESIAN_POINT('Ctrl Pts',(-20.5293895033194,24.678231105532,0.257696928091187));
#41609=CARTESIAN_POINT('Ctrl Pts',(-20.5895216358816,24.8240609966413,0.26709680078661));
#41610=CARTESIAN_POINT('Ctrl Pts',(-20.609217217609,24.86889817206,0.270047325149324));
#41611=CARTESIAN_POINT('Ctrl Pts',(-20.6332621021985,24.9204155227757,0.273514217745747));
#41612=CARTESIAN_POINT('Ctrl Pts',(-20.6366245559732,24.9275512666281,0.273996152668289));
#41613=CARTESIAN_POINT('Ctrl Pts',(-20.6417807486555,24.9383902701016,0.274730862600814));
#41614=CARTESIAN_POINT('Ctrl Pts',(-20.6435554546391,24.9421025938466,0.274982975525235));
#41615=CARTESIAN_POINT('Ctrl Pts',(-20.6467863810607,24.9488279044599,0.275440577840088));
#41616=CARTESIAN_POINT('Ctrl Pts',(-20.6482401962958,24.9518420458677,0.275645983172878));
#41617=CARTESIAN_POINT('Ctrl Pts',(-20.6511570429987,24.957865442273,0.276057099041058));
#41618=CARTESIAN_POINT('Ctrl Pts',(-20.652620071659,24.960874694082,0.276262809289172));
#41619=CARTESIAN_POINT('Ctrl Pts',(-20.6567526735091,24.969341338997,0.276842485850519));
#41620=CARTESIAN_POINT('Ctrl Pts',(-20.6594329855526,24.9747934483287,0.27721682748922));
#41621=CARTESIAN_POINT('Ctrl Pts',(-20.6705372695402,24.9972206337698,0.278761068367342));
#41622=CARTESIAN_POINT('Ctrl Pts',(-20.6790953356128,25.0141285545181,0.27993566558761));
#41623=CARTESIAN_POINT('Ctrl Pts',(-20.6911030736317,25.0373414879111,0.281562901125425));
#41624=CARTESIAN_POINT('Ctrl Pts',(-20.6944255820869,25.0437121460754,0.282011018027436));
#41625=CARTESIAN_POINT('Ctrl Pts',(-20.7044612436974,25.0627988190192,0.283358216254511));
#41626=CARTESIAN_POINT('Ctrl Pts',(-20.7112381572836,25.0754809399052,0.284259547560253));
#41627=CARTESIAN_POINT('Ctrl Pts',(-20.719204133787,25.0901511934884,0.285309445986835));
#41628=CARTESIAN_POINT('Ctrl Pts',(-20.7203108284034,25.092184072269,0.285455094756321));
#41629=CARTESIAN_POINT('Ctrl Pts',(-20.7238532406541,25.0986744419272,0.2859206283418));
#41630=CARTESIAN_POINT('Ctrl Pts',(-20.7262972982619,25.103127350724,0.286240807177686));
#41631=CARTESIAN_POINT('Ctrl Pts',(-20.7321100284138,25.113658649298,0.286999909910334));
#41632=CARTESIAN_POINT('Ctrl Pts',(-20.7354878445116,25.1197319396299,0.287439154692371));
#41633=CARTESIAN_POINT('Ctrl Pts',(-20.7418796005154,25.1311372701268,0.28826682733365));
#41634=CARTESIAN_POINT('Ctrl Pts',(-20.7448891532083,25.136471744354,0.288655099824032));
#41635=CARTESIAN_POINT('Ctrl Pts',(-20.7499259767119,25.1453404127158,0.289302541225746));
#41636=CARTESIAN_POINT('Ctrl Pts',(-20.7519447846058,25.1488794159496,0.289561413777675));
#41637=CARTESIAN_POINT('Ctrl Pts',(-20.7564365919346,25.1567190481306,0.290136012669184));
#41638=CARTESIAN_POINT('Ctrl Pts',(-20.7589128179452,25.1610178081071,0.290451850837234));
#41639=CARTESIAN_POINT('Ctrl Pts',(-20.7714489344203,25.1826649484732,0.292046171275604));
#41640=CARTESIAN_POINT('Ctrl Pts',(-20.7816605028035,25.1999245839127,0.293329891275744));
#41641=CARTESIAN_POINT('Ctrl Pts',(-20.8055798534322,25.239505489108,0.296302926832801));
#41642=CARTESIAN_POINT('Ctrl Pts',(-20.8193998910517,25.2617569750201,0.297995974332773));
#41643=CARTESIAN_POINT('Ctrl Pts',(-20.8955398283283,25.3810786335741,0.30719232082289));
#41644=CARTESIAN_POINT('Ctrl Pts',(-20.9627611090807,25.4749103588654,0.314853590863943));
#41645=CARTESIAN_POINT('Ctrl Pts',(-21.2084208314198,25.7816245542864,0.341270196479512));
#41646=CARTESIAN_POINT('Ctrl Pts',(-21.4092594525579,25.9749924677834,0.360456044878661));
#41647=CARTESIAN_POINT('Ctrl Pts',(-21.6385145789546,26.1447531278,0.378429061316228));
#41648=CARTESIAN_POINT('Ctrl Pts',(-21.6446395005714,26.149255094502,0.378906580565882));
#41649=CARTESIAN_POINT('Ctrl Pts',(-21.6539485260691,26.1560468560446,0.379628250289522));
#41650=CARTESIAN_POINT('Ctrl Pts',(-21.6571209232754,26.158352540543,0.379873469358838));
#41651=CARTESIAN_POINT('Ctrl Pts',(-21.6622894954946,26.1620946372302,0.380271812759372));
#41652=CARTESIAN_POINT('Ctrl Pts',(-21.6642831080575,26.1635345569476,0.380425177380249));
#41653=CARTESIAN_POINT('Ctrl Pts',(-21.6680851947827,26.1662740602382,0.380717121035346));
#41654=CARTESIAN_POINT('Ctrl Pts',(-21.6698933701589,26.1675740529527,0.38085572839394));
#41655=CARTESIAN_POINT('Ctrl Pts',(-21.6731917108961,26.1699402220138,0.381108138079332));
#41656=CARTESIAN_POINT('Ctrl Pts',(-21.6746814353009,26.1710069998236,0.381221982272932));
#41657=CARTESIAN_POINT('Ctrl Pts',(-21.677681587593,26.173151512718,0.381450932897352));
#41658=CARTESIAN_POINT('Ctrl Pts',(-21.6791920308051,26.1742292098303,0.381566036686877));
#41659=CARTESIAN_POINT('Ctrl Pts',(-21.6834303325868,26.177247706279,0.381888564477951));
#41660=CARTESIAN_POINT('Ctrl Pts',(-21.6861602959656,26.1791855676064,0.382095784304771));
#41661=CARTESIAN_POINT('Ctrl Pts',(-21.6972923874487,26.1870616115606,0.382938655939312));
#41662=CARTESIAN_POINT('Ctrl Pts',(-21.7057200294066,26.1929638807847,0.383571853837511));
#41663=CARTESIAN_POINT('Ctrl Pts',(-21.8296205257403,26.2788557104618,0.392811592072697));
#41664=CARTESIAN_POINT('Ctrl Pts',(-21.9501656510622,26.3512461824876,0.400924583803991));
#41665=CARTESIAN_POINT('Ctrl Pts',(-22.0750360367128,26.4155367855571,0.408876748608877));
#41666=CARTESIAN_POINT('Origin',(-23.5502525316942,23.5502525316942,-77.3107734492734));
#41667=CARTESIAN_POINT('',(-22.0750357750288,26.4155366508268,1.90417269213726));
#41668=CARTESIAN_POINT('',(-22.0750360931093,26.4155368145933,1.65435918102699));
#41669=CARTESIAN_POINT('',(-22.0750360153461,26.4155367745563,-77.3107734492734));
#41670=CARTESIAN_POINT('',(-26.7730025181246,23.5505482728461,1.06385144282923));
#41671=CARTESIAN_POINT('Ctrl Pts',(-22.075035775028,26.4155366508264,1.90417269213721));
#41672=CARTESIAN_POINT('Ctrl Pts',(-21.8814507610379,26.3158677019181,1.8919715089247));
#41673=CARTESIAN_POINT('Ctrl Pts',(-21.6981541108952,26.1966789059609,1.87955594100593));
#41674=CARTESIAN_POINT('Ctrl Pts',(-21.5122014721954,26.0468261874996,1.86511320621351));
#41675=CARTESIAN_POINT('Ctrl Pts',(-21.4964692496334,26.0339003208803,1.8638759470571));
#41676=CARTESIAN_POINT('Ctrl Pts',(-21.4761651150797,26.0168932576151,1.86225858208589));
#41677=CARTESIAN_POINT('Ctrl Pts',(-21.4714806371493,26.0129466848854,1.86188399032297));
#41678=CARTESIAN_POINT('Ctrl Pts',(-21.463917553353,26.0065379933014,1.86127686259327));
#41679=CARTESIAN_POINT('Ctrl Pts',(-21.4610319717169,26.0040840993301,1.86104466549418));
#41680=CARTESIAN_POINT('Ctrl Pts',(-21.4556518048291,25.9994924445066,1.86061068984257));
#41681=CARTESIAN_POINT('Ctrl Pts',(-21.4531561468159,25.9973559434649,1.86040896351885));
#41682=CARTESIAN_POINT('Ctrl Pts',(-21.447572670071,25.9925611860239,1.85995669852832));
#41683=CARTESIAN_POINT('Ctrl Pts',(-21.4444866208581,25.9899008858646,1.85970607529586));
#41684=CARTESIAN_POINT('Ctrl Pts',(-21.4380733653824,25.9843511638366,1.85918388171023));
#41685=CARTESIAN_POINT('Ctrl Pts',(-21.4347470258812,25.9814607572817,1.85891227063435));
#41686=CARTESIAN_POINT('Ctrl Pts',(-21.4161600473663,25.9652426653331,1.85739024326999));
#41687=CARTESIAN_POINT('Ctrl Pts',(-21.4010197058138,25.9517783606637,1.85613412387737));
#41688=CARTESIAN_POINT('Ctrl Pts',(-21.2469753545308,25.8121632478877,1.84318277879368));
#41689=CARTESIAN_POINT('Ctrl Pts',(-21.1192386756393,25.6742759132547,1.83096877135852));
#41690=CARTESIAN_POINT('Ctrl Pts',(-20.8458520919125,25.3219956789153,1.80114358394728));
#41691=CARTESIAN_POINT('Ctrl Pts',(-20.7125860196738,25.099608836659,1.78330301144837));
#41692=CARTESIAN_POINT('Ctrl Pts',(-20.6058403763807,24.8604309288844,1.76631614551117));
#41693=CARTESIAN_POINT('Ctrl Pts',(-20.6043871161431,24.857160074906,1.76608425334781));
#41694=CARTESIAN_POINT('Ctrl Pts',(-20.6024120347641,24.852694724728,1.76576824097735));
#41695=CARTESIAN_POINT('Ctrl Pts',(-20.6018854903421,24.8515023351585,1.76568391062095));
#41696=CARTESIAN_POINT('Ctrl Pts',(-20.6002536604032,24.8478008887473,1.76542230129149));
#41697=CARTESIAN_POINT('Ctrl Pts',(-20.5991508502565,24.8452907339985,1.7652451334981));
#41698=CARTESIAN_POINT('Ctrl Pts',(-20.5972386254719,24.8409231083533,1.76493729225028));
#41699=CARTESIAN_POINT('Ctrl Pts',(-20.5964277584337,24.8390662795687,1.76480655250562));
#41700=CARTESIAN_POINT('Ctrl Pts',(-20.5943047766906,24.8341922721651,1.76446372681533));
#41701=CARTESIAN_POINT('Ctrl Pts',(-20.5929955268357,24.8311738387499,1.76425177353868));
#41702=CARTESIAN_POINT('Ctrl Pts',(-20.576412066822,24.7927802590375,1.76156035885763));
#41703=CARTESIAN_POINT('Ctrl Pts',(-20.5617679947572,24.7571339532501,1.75911076528892));
#41704=CARTESIAN_POINT('Ctrl Pts',(-20.5460418529123,24.7168108355699,1.75640155238525));
#41705=CARTESIAN_POINT('Ctrl Pts',(-20.5443274696509,24.7123861732833,1.75610509825657));
#41706=CARTESIAN_POINT('Ctrl Pts',(-20.5417594905385,24.70571475956,1.75565937520567));
#41707=CARTESIAN_POINT('Ctrl Pts',(-20.5408986347578,24.7034708379108,1.75550967192108));
#41708=CARTESIAN_POINT('Ctrl Pts',(-20.5394115644337,24.6995816105483,1.75525057717783));
#41709=CARTESIAN_POINT('Ctrl Pts',(-20.5387841879807,24.6979367550237,1.75514111539304));
#41710=CARTESIAN_POINT('Ctrl Pts',(-20.5374793221104,24.694507221071,1.75491313012427));
#41711=CARTESIAN_POINT('Ctrl Pts',(-20.5368020712802,24.6927224565483,1.7547946215952));
#41712=CARTESIAN_POINT('Ctrl Pts',(-20.535195681804,24.6884777593945,1.75451309751388));
#41713=CARTESIAN_POINT('Ctrl Pts',(-20.5342679646048,24.6860172820893,1.75435016813333));
#41714=CARTESIAN_POINT('Ctrl Pts',(-20.5311774994348,24.6777903101593,1.75380624468434));
#41715=CARTESIAN_POINT('Ctrl Pts',(-20.5290282527285,24.6720187060592,1.75342605999938));
#41716=CARTESIAN_POINT('Ctrl Pts',(-20.4677757133275,24.5060776487926,1.74253454572671));
#41717=CARTESIAN_POINT('Ctrl Pts',(-20.4214664321042,24.3414423300494,1.73277286198874));
#41718=CARTESIAN_POINT('Ctrl Pts',(-20.3452950612736,23.9552540009159,1.71062918018383));
#41719=CARTESIAN_POINT('Ctrl Pts',(-20.3249662010619,23.7327463799608,1.69838271240373));
#41720=CARTESIAN_POINT('Ctrl Pts',(-20.3291912901761,23.3951501879122,1.67885833496819));
#41721=CARTESIAN_POINT('Ctrl Pts',(-20.3367579337698,23.280548728671,1.67207509539306));
#41722=CARTESIAN_POINT('Ctrl Pts',(-20.3516766017234,23.1561191942171,1.6644491936628));
#41723=CARTESIAN_POINT('Ctrl Pts',(-20.3529851675831,23.1456410319546,1.66380502193365));
#41724=CARTESIAN_POINT('Ctrl Pts',(-20.3548969320148,23.1309215113061,1.66289723313203));
#41725=CARTESIAN_POINT('Ctrl Pts',(-20.3554571373852,23.1266745562569,1.66263497699177));
#41726=CARTESIAN_POINT('Ctrl Pts',(-20.3564446141178,23.1193018371944,1.66217911177237));
#41727=CARTESIAN_POINT('Ctrl Pts',(-20.3568680118607,23.1161755525261,1.66198562556488));
#41728=CARTESIAN_POINT('Ctrl Pts',(-20.357749867041,23.1097352315521,1.66158665232587));
#41729=CARTESIAN_POINT('Ctrl Pts',(-20.3582088956451,23.1064212788867,1.66138114743954));
#41730=CARTESIAN_POINT('Ctrl Pts',(-20.3592962241687,23.0986602630068,1.66089938134118));
#41731=CARTESIAN_POINT('Ctrl Pts',(-20.3599286603854,23.0942137948462,1.66062298928055));
#41732=CARTESIAN_POINT('Ctrl Pts',(-20.3612833380543,23.0848302058941,1.66003890452354));
#41733=CARTESIAN_POINT('Ctrl Pts',(-20.3620077542829,23.0798934154878,1.65973114338011));
#41734=CARTESIAN_POINT('Ctrl Pts',(-20.3673481281932,23.0440787768531,1.6574950172375));
#41735=CARTESIAN_POINT('Ctrl Pts',(-20.372400973753,23.0132686613625,1.6555528195199));
#41736=CARTESIAN_POINT('Ctrl Pts',(-20.3879687546237,22.9262769612286,1.65001452872419));
#41737=CARTESIAN_POINT('Ctrl Pts',(-20.3995313101981,22.8702971542423,1.64638565805902));
#41738=CARTESIAN_POINT('Ctrl Pts',(-20.4284850469749,22.7467952008307,1.6382312942406));
#41739=CARTESIAN_POINT('Ctrl Pts',(-20.4465909700144,22.6794714247532,1.63368589977613));
#41740=CARTESIAN_POINT('Ctrl Pts',(-20.5163122364266,22.4501523903064,1.61786948749574));
#41741=CARTESIAN_POINT('Ctrl Pts',(-20.5785477202612,22.2916912918582,1.60633997128058));
#41742=CARTESIAN_POINT('Ctrl Pts',(-20.7132603561785,22.0151505136336,1.58553650438964));
#41743=CARTESIAN_POINT('Ctrl Pts',(-20.7814095078298,21.8953877412622,1.57627711316599));
#41744=CARTESIAN_POINT('Ctrl Pts',(-20.8620392211563,21.7726950825497,1.56676387830214));
#41745=CARTESIAN_POINT('Ctrl Pts',(-20.8670970243253,21.7650696796998,1.56617253624986));
#41746=CARTESIAN_POINT('Ctrl Pts',(-20.8774591246889,21.7495907714466,1.56497214009515));
#41747=CARTESIAN_POINT('Ctrl Pts',(-20.8827657330968,21.7417389002452,1.5643632119043));
#41748=CARTESIAN_POINT('Ctrl Pts',(-20.8911207591429,21.7294932468399,1.56341365778343));
#41749=CARTESIAN_POINT('Ctrl Pts',(-20.8941455649354,21.7250835150961,1.56307174240534));
#41750=CARTESIAN_POINT('Ctrl Pts',(-20.8999617137211,21.7166494861608,1.56241787521868));
#41751=CARTESIAN_POINT('Ctrl Pts',(-20.9027512799573,21.7126239862143,1.56210582356671));
#41752=CARTESIAN_POINT('Ctrl Pts',(-20.9103929869869,21.7016500948953,1.56125526951302));
#41753=CARTESIAN_POINT('Ctrl Pts',(-20.9152634171564,21.6947144008757,1.56071784491774));
#41754=CARTESIAN_POINT('Ctrl Pts',(-20.9220532448787,21.6851260507455,1.55997516066795));
#41755=CARTESIAN_POINT('Ctrl Pts',(-20.9239493597191,21.6824570583518,1.55976845957951));
#41756=CARTESIAN_POINT('Ctrl Pts',(-20.9328870110855,21.6699168388114,1.5587974409993));
#41757=CARTESIAN_POINT('Ctrl Pts',(-20.9399802782132,21.6600823382348,1.55803640910593));
#41758=CARTESIAN_POINT('Ctrl Pts',(-20.9492348983139,21.6474026708905,1.55705607774178));
#41759=CARTESIAN_POINT('Ctrl Pts',(-20.951345589253,21.6445209066374,1.55683333209414));
#41760=CARTESIAN_POINT('Ctrl Pts',(-20.9545866981573,21.6401111611257,1.5564925788639));
#41761=CARTESIAN_POINT('Ctrl Pts',(-20.955713675064,21.6385806727111,1.55637433184176));
#41762=CARTESIAN_POINT('Ctrl Pts',(-20.9579379101103,21.6355656452746,1.55614142498344));
#41763=CARTESIAN_POINT('Ctrl Pts',(-20.9590350841611,21.6340810597374,1.55602676070396));
#41764=CARTESIAN_POINT('Ctrl Pts',(-20.9614807411735,21.6307777845123,1.55577166664929));
#41765=CARTESIAN_POINT('Ctrl Pts',(-20.96282986209,21.6289595771038,1.55563128281289));
#41766=CARTESIAN_POINT('Ctrl Pts',(-20.966728204985,21.6237173417172,1.55522660132314));
#41767=CARTESIAN_POINT('Ctrl Pts',(-20.9692823278778,21.6202969383116,1.55496264694418));
#41768=CARTESIAN_POINT('Ctrl Pts',(-20.9864669412194,21.5973789531396,1.55319457193935));
#41769=CARTESIAN_POINT('Ctrl Pts',(-21.001311956288,21.5780421482168,1.55170529973201));
#41770=CARTESIAN_POINT('Ctrl Pts',(-21.0479167378743,21.5187410956292,1.54713949584041));
#41771=CARTESIAN_POINT('Ctrl Pts',(-21.0804089892362,21.4793598148726,1.54410938244089));
#41772=CARTESIAN_POINT('Ctrl Pts',(-21.1534790869431,21.3949649195445,1.53757872223916));
#41773=CARTESIAN_POINT('Ctrl Pts',(-21.1944186306777,21.3502900405086,1.53409724814066));
#41774=CARTESIAN_POINT('Ctrl Pts',(-21.2637108287791,21.2788296594606,1.52843695567045));
#41775=CARTESIAN_POINT('Ctrl Pts',(-21.2913318337374,21.2513588386409,1.52623742004462));
#41776=CARTESIAN_POINT('Ctrl Pts',(-21.3431828940148,21.2016267456452,1.52219691617058));
#41777=CARTESIAN_POINT('Ctrl Pts',(-21.3672686580242,21.1792230272889,1.52035366086074));
#41778=CARTESIAN_POINT('Ctrl Pts',(-21.5432873739169,21.0204527926601,1.50709023911515));
#41779=CARTESIAN_POINT('Ctrl Pts',(-21.7075195564533,20.8984372305199,1.49577043300807));
#41780=CARTESIAN_POINT('Ctrl Pts',(-21.9674779889894,20.7411815979433,1.4780917613915));
#41781=CARTESIAN_POINT('Ctrl Pts',(-22.0551119110054,20.6935750583475,1.47217486568356));
#41782=CARTESIAN_POINT('Ctrl Pts',(-22.1539876527791,20.645658569912,1.46548719573802));
#41783=CARTESIAN_POINT('Ctrl Pts',(-22.1631916807759,20.6412520354758,1.46486457902553));
#41784=CARTESIAN_POINT('Ctrl Pts',(-22.176232426546,20.6350845893119,1.46398225281223));
#41785=CARTESIAN_POINT('Ctrl Pts',(-22.180051981342,20.6332873565192,1.46372380430496));
#41786=CARTESIAN_POINT('Ctrl Pts',(-22.1867180047453,20.6301667435638,1.46327271056255));
#41787=CARTESIAN_POINT('Ctrl Pts',(-22.1895629030109,20.6288400051053,1.46308018188672));
#41788=CARTESIAN_POINT('Ctrl Pts',(-22.1954541529114,20.6261030511894,1.46268146277393));
#41789=CARTESIAN_POINT('Ctrl Pts',(-22.1985007771107,20.6246934354981,1.46247525192044));
#41790=CARTESIAN_POINT('Ctrl Pts',(-22.2056951763517,20.6213783596693,1.46198825902148));
#41791=CARTESIAN_POINT('Ctrl Pts',(-22.209844799986,20.6194769500786,1.46170733754462));
#41792=CARTESIAN_POINT('Ctrl Pts',(-22.218626204959,20.6154757512555,1.46111278165286));
#41793=CARTESIAN_POINT('Ctrl Pts',(-22.2232589410106,20.6133780987526,1.46079907440684));
#41794=CARTESIAN_POINT('Ctrl Pts',(-22.2584688064079,20.5975357746459,1.45841447894258));
#41795=CARTESIAN_POINT('Ctrl Pts',(-22.2892528096187,20.5842584311879,1.45632760418596));
#41796=CARTESIAN_POINT('Ctrl Pts',(-22.3783400248555,20.5474721256919,1.45028011420247));
#41797=CARTESIAN_POINT('Ctrl Pts',(-22.4371286079786,20.5251866917094,1.44627913062091));
#41798=CARTESIAN_POINT('Ctrl Pts',(-22.570739136822,20.4789600368383,1.43715935687858));
#41799=CARTESIAN_POINT('Ctrl Pts',(-22.6458589165091,20.4560071030729,1.43201331010333));
#41800=CARTESIAN_POINT('Ctrl Pts',(-22.9999474985609,20.361810859115,1.40770625984286));
#41801=CARTESIAN_POINT('Ctrl Pts',(-23.2867946499104,20.3254157043369,1.38772806999562));
#41802=CARTESIAN_POINT('Ctrl Pts',(-23.6268156828161,20.327989796836,1.36565773507302));
#41803=CARTESIAN_POINT('Ctrl Pts',(-23.6789686312704,20.3296513459005,1.36232180446997));
#41804=CARTESIAN_POINT('Ctrl Pts',(-23.7367816849261,20.3329000086425,1.35869523291549));
#41805=CARTESIAN_POINT('Ctrl Pts',(-23.742500729226,20.3332366762247,1.35833725885135));
#41806=CARTESIAN_POINT('Ctrl Pts',(-23.750512584493,20.3337297578467,1.35783688848985));
#41807=CARTESIAN_POINT('Ctrl Pts',(-23.7528061285321,20.3338733743318,1.35769377652903));
#41808=CARTESIAN_POINT('Ctrl Pts',(-23.7570030923822,20.3341406856257,1.35743213300354));
#41809=CARTESIAN_POINT('Ctrl Pts',(-23.7589065585771,20.3342636172402,1.35731355817461));
#41810=CARTESIAN_POINT('Ctrl Pts',(-23.7627733705782,20.3345167951644,1.35707286158511));
#41811=CARTESIAN_POINT('Ctrl Pts',(-23.7647367067801,20.3346471496794,1.35695074611826));
#41812=CARTESIAN_POINT('Ctrl Pts',(-23.7696165315406,20.3349756317696,1.35664746669998));
#41813=CARTESIAN_POINT('Ctrl Pts',(-23.7725328797192,20.3351759300156,1.35646642590578));
#41814=CARTESIAN_POINT('Ctrl Pts',(-23.783439876142,20.3359399468842,1.35579011161252));
#41815=CARTESIAN_POINT('Ctrl Pts',(-23.7914287730758,20.3365294953536,1.35529628550864));
#41816=CARTESIAN_POINT('Ctrl Pts',(-23.9291236107938,20.3472071628721,1.34681016849553));
#41817=CARTESIAN_POINT('Ctrl Pts',(-24.0581221247887,20.365111936138,1.33924647735657));
#41818=CARTESIAN_POINT('Ctrl Pts',(-24.2610421145562,20.4059240283525,1.32747436309305));
#41819=CARTESIAN_POINT('Ctrl Pts',(-24.335819967173,20.4237676003324,1.32316439338793));
#41820=CARTESIAN_POINT('Ctrl Pts',(-24.5086141231305,20.4715915209475,1.31313662367713));
#41821=CARTESIAN_POINT('Ctrl Pts',(-24.6059784341575,20.5036063466133,1.30743245864895));
#41822=CARTESIAN_POINT('Ctrl Pts',(-24.8831883201678,20.6096441688844,1.29069761408952));
#41823=CARTESIAN_POINT('Ctrl Pts',(-25.0580425704263,20.6953537032487,1.27949016491133));
#41824=CARTESIAN_POINT('Ctrl Pts',(-25.23428174683,20.8024706633733,1.26695209025099));
#41825=CARTESIAN_POINT('Ctrl Pts',(-25.2444313590026,20.8087168874943,1.2662255210112));
#41826=CARTESIAN_POINT('Ctrl Pts',(-25.2583750474245,20.817405044599,1.26522103824138));
#41827=CARTESIAN_POINT('Ctrl Pts',(-25.2621990788703,20.8197989181453,1.26494490235496));
#41828=CARTESIAN_POINT('Ctrl Pts',(-25.2687393142346,20.8239122970226,1.26447149343682));
#41829=CARTESIAN_POINT('Ctrl Pts',(-25.2714580029765,20.8256278561708,1.26427436696575));
#41830=CARTESIAN_POINT('Ctrl Pts',(-25.2769726524914,20.8291192828331,1.26387382477098));
#41831=CARTESIAN_POINT('Ctrl Pts',(-25.2797684505113,20.8308953980956,1.26367040001719));
#41832=CARTESIAN_POINT('Ctrl Pts',(-25.286182069086,20.8349837349184,1.26320291106151));
#41833=CARTESIAN_POINT('Ctrl Pts',(-25.289798010987,20.8372988788058,1.26293873812384));
#41834=CARTESIAN_POINT('Ctrl Pts',(-25.2973708452006,20.8421688281909,1.2623842041558));
#41835=CARTESIAN_POINT('Ctrl Pts',(-25.3013267821481,20.8447250940976,1.26209378887469));
#41836=CARTESIAN_POINT('Ctrl Pts',(-25.3265746622469,20.8611184584719,1.26023555565196));
#41837=CARTESIAN_POINT('Ctrl Pts',(-25.3477075482556,20.8751978071666,1.25865866422172));
#41838=CARTESIAN_POINT('Ctrl Pts',(-25.5800973033549,21.0340197534594,1.24107349919458));
#41839=CARTESIAN_POINT('Ctrl Pts',(-25.7735026921135,21.2031686147822,1.22406272097569));
#41840=CARTESIAN_POINT('Ctrl Pts',(-26.0747637857122,21.5376283685949,1.19361314385912));
#41841=CARTESIAN_POINT('Ctrl Pts',(-26.1914122081893,21.6933464045357,1.18039870522529));
#41842=CARTESIAN_POINT('Ctrl Pts',(-26.2965595046832,21.8638500858632,1.16748648705273));
#41843=CARTESIAN_POINT('Ctrl Pts',(-26.2997648147177,21.8690810931143,1.16709178879035));
#41844=CARTESIAN_POINT('Ctrl Pts',(-26.3212638904364,21.9043931396477,1.16443725254659));
#41845=CARTESIAN_POINT('Ctrl Pts',(-26.3390795319283,21.9347645851838,1.16220232572372));
#41846=CARTESIAN_POINT('Ctrl Pts',(-26.3586680483521,21.9694485533358,1.15970936419581));
#41847=CARTESIAN_POINT('Ctrl Pts',(-26.3609326930063,21.973478621573,1.1594205925036));
#41848=CARTESIAN_POINT('Ctrl Pts',(-26.3643462417632,21.9795839543467,1.15898448882889));
#41849=CARTESIAN_POINT('Ctrl Pts',(-26.3655015268214,21.9816556158356,1.15883674816047));
#41850=CARTESIAN_POINT('Ctrl Pts',(-26.3675063490557,21.9852600198799,1.15858011603939));
#41851=CARTESIAN_POINT('Ctrl Pts',(-26.3683569231326,21.9867921796346,1.15847115743749));
#41852=CARTESIAN_POINT('Ctrl Pts',(-26.3701346428063,21.9900005932772,1.15824326745465));
#41853=CARTESIAN_POINT('Ctrl Pts',(-26.3710615430849,21.9916769790876,1.15812435237936));
#41854=CARTESIAN_POINT('Ctrl Pts',(-26.3732747217799,21.9956881610281,1.15784018993199));
#41855=CARTESIAN_POINT('Ctrl Pts',(-26.3745596029461,21.9980237355239,1.15767503309625));
#41856=CARTESIAN_POINT('Ctrl Pts',(-26.3789041702153,22.0059442646638,1.15711595517815));
#41857=CARTESIAN_POINT('Ctrl Pts',(-26.3819502252139,22.0115367392623,1.15672290662291));
#41858=CARTESIAN_POINT('Ctrl Pts',(-26.3891497823511,22.0248487152359,1.15579126720568));
#41859=CARTESIAN_POINT('Ctrl Pts',(-26.393288430092,22.032576252782,1.15525359819272));
#41860=CARTESIAN_POINT('Ctrl Pts',(-26.441583725735,22.1236423588657,1.14895311202748));
#41861=CARTESIAN_POINT('Ctrl Pts',(-26.4820977764742,22.2088726929073,1.14340705688869));
#41862=CARTESIAN_POINT('Ctrl Pts',(-26.6203476069523,22.5360214612851,1.1229624250592));
#41863=CARTESIAN_POINT('Ctrl Pts',(-26.692339172238,22.7877199375945,1.10883621379078));
#41864=CARTESIAN_POINT('Ctrl Pts',(-26.7549740880502,23.182581709233,1.08596053099294));
#41865=CARTESIAN_POINT('Ctrl Pts',(-26.7678420929857,23.3210539961626,1.0778252309071));
#41866=CARTESIAN_POINT('Ctrl Pts',(-26.7721376785587,23.4742334600604,1.06852386079418));
#41867=CARTESIAN_POINT('Ctrl Pts',(-26.7724437667979,23.4885562361089,1.06765134792028));
#41868=CARTESIAN_POINT('Ctrl Pts',(-26.7727339722753,23.5082969273394,1.06644477344609));
#41869=CARTESIAN_POINT('Ctrl Pts',(-26.7727999425391,23.5137136220729,1.06611328235863));
#41870=CARTESIAN_POINT('Ctrl Pts',(-26.7728832979791,23.5223448267491,1.06558439774986));
#41871=CARTESIAN_POINT('Ctrl Pts',(-26.7729095314212,23.5255592574914,1.0653872822359));
#41872=CARTESIAN_POINT('Ctrl Pts',(-26.7729525099123,23.5320077431331,1.06499154783542));
#41873=CARTESIAN_POINT('Ctrl Pts',(-26.7729691961829,23.5352417947467,1.06479292732375));
#41874=CARTESIAN_POINT('Ctrl Pts',(-26.7729933534064,23.5418525038813,1.06438661654675));
#41875=CARTESIAN_POINT('Ctrl Pts',(-26.7730003856187,23.5452291579355,1.06417891275826));
#41876=CARTESIAN_POINT('Ctrl Pts',(-26.7730024418284,23.5492532957307,1.06393118172865));
#41877=CARTESIAN_POINT('Ctrl Pts',(-26.7730025775425,23.5499007845161,1.06389131534507));
#41878=CARTESIAN_POINT('Ctrl Pts',(-26.7730025181246,23.5505482728461,1.06385144282923));
#41879=CARTESIAN_POINT('Ctrl Pts',(-26.7730025181501,23.5505479950934,1.06385145993333));
#41880=CARTESIAN_POINT('Ctrl Pts',(-26.7730022618683,23.5533433743501,1.0636793196899));
#41881=CARTESIAN_POINT('Ctrl Pts',(-26.7729983685636,23.5561387455046,1.06350706512355));
#41882=CARTESIAN_POINT('Ctrl Pts',(-26.772952457919,23.5731815149597,1.06245616260223));
#41883=CARTESIAN_POINT('Ctrl Pts',(-26.7728195988542,23.5874283294327,1.06157466572968));
#41884=CARTESIAN_POINT('Ctrl Pts',(-26.7695656810077,23.7913374756817,1.04891409998377));
#41885=CARTESIAN_POINT('Ctrl Pts',(-26.7498010758502,23.9803281996212,1.03660008540109));
#41886=CARTESIAN_POINT('Ctrl Pts',(-26.674593879202,24.366405226574,1.01032532656749));
#41887=CARTESIAN_POINT('Ctrl Pts',(-26.6167766994715,24.5622008701433,0.99636727538878));
#41888=CARTESIAN_POINT('Ctrl Pts',(-26.5108996430848,24.8258517894404,0.977440662005678));
#41889=CARTESIAN_POINT('Ctrl Pts',(-26.4781457219519,24.8993368071326,0.972155526978332));
#41890=CARTESIAN_POINT('Ctrl Pts',(-26.4286034850465,25.0001598725442,0.964962154658452));
#41891=CARTESIAN_POINT('Ctrl Pts',(-26.4141077492004,25.0285857121237,0.96294079985228));
#41892=CARTESIAN_POINT('Ctrl Pts',(-26.3970532862464,25.0608365080325,0.960659199583425));
#41893=CARTESIAN_POINT('Ctrl Pts',(-26.3949063666697,25.0648756021193,0.960373664613543));
#41894=CARTESIAN_POINT('Ctrl Pts',(-26.3916537351577,25.0709636100479,0.959943623667648));
#41895=CARTESIAN_POINT('Ctrl Pts',(-26.39055440217,25.0730158972654,0.959798713481767));
#41896=CARTESIAN_POINT('Ctrl Pts',(-26.3885775133581,25.0766968587514,0.959538910703062));
#41897=CARTESIAN_POINT('Ctrl Pts',(-26.3877007810336,25.0783259649825,0.959423965848513));
#41898=CARTESIAN_POINT('Ctrl Pts',(-26.3859382456897,25.0815942850436,0.959193439022753));
#41899=CARTESIAN_POINT('Ctrl Pts',(-26.3850524273688,25.0832334792715,0.959077858737703));
#41900=CARTESIAN_POINT('Ctrl Pts',(-26.3825525971509,25.0878498034163,0.958752464831404));
#41901=CARTESIAN_POINT('Ctrl Pts',(-26.3809353074311,25.0908251700954,0.958542861443316));
#41902=CARTESIAN_POINT('Ctrl Pts',(-26.3742412343576,25.103094286924,0.957679034380685));
#41903=CARTESIAN_POINT('Ctrl Pts',(-26.3691232726928,25.1123656717967,0.957027420142438));
#41904=CARTESIAN_POINT('Ctrl Pts',(-26.2745081225734,25.2817854357539,0.945138252250335));
#41905=CARTESIAN_POINT('Ctrl Pts',(-26.1715274988144,25.4340555425234,0.934739891450258));
#41906=CARTESIAN_POINT('Ctrl Pts',(-25.9499571546216,25.7080394846369,0.914986172828499));
#41907=CARTESIAN_POINT('Ctrl Pts',(-25.8336347860798,25.8307767042791,0.905639993619675));
#41908=CARTESIAN_POINT('Ctrl Pts',(-25.6531283189693,25.9935158917294,0.891760000630903));
#41909=CARTESIAN_POINT('Ctrl Pts',(-25.5963265305947,26.0412769358294,0.887472353013706));
#41910=CARTESIAN_POINT('Ctrl Pts',(-25.4822596851849,26.1306532324259,0.878956564732244));
#41911=CARTESIAN_POINT('Ctrl Pts',(-25.4251723854354,26.1724260217868,0.87473743717121));
#41912=CARTESIAN_POINT('Ctrl Pts',(-25.354900121296,26.2203781473119,0.869572757252184));
#41913=CARTESIAN_POINT('Ctrl Pts',(-25.3429861090755,26.2283918178253,0.868698127091755));
#41914=CARTESIAN_POINT('Ctrl Pts',(-25.3266463597186,26.2392244644244,0.86749979684013));
#41915=CARTESIAN_POINT('Ctrl Pts',(-25.3222665754128,26.2421127278416,0.867178707798934));
#41916=CARTESIAN_POINT('Ctrl Pts',(-25.3152607099786,26.2467082617412,0.866665275473352));
#41917=CARTESIAN_POINT('Ctrl Pts',(-25.3126391457502,26.2484224292354,0.866473191222828));
#41918=CARTESIAN_POINT('Ctrl Pts',(-25.3072367924786,26.2519436443291,0.866077436164229));
#41919=CARTESIAN_POINT('Ctrl Pts',(-25.3044557055198,26.2537502264495,0.865873748228727));
#41920=CARTESIAN_POINT('Ctrl Pts',(-25.298050099156,26.2578972352053,0.865404696401294));
#41921=CARTESIAN_POINT('Ctrl Pts',(-25.2944236645493,26.2602346785548,0.865139221544065));
#41922=CARTESIAN_POINT('Ctrl Pts',(-25.2833818583141,26.2673204060378,0.864331110844406));
#41923=CARTESIAN_POINT('Ctrl Pts',(-25.2759517562986,26.272045558416,0.863787615058523));
#41924=CARTESIAN_POINT('Ctrl Pts',(-25.2192692615357,26.3077672284368,0.859643446730582));
#41925=CARTESIAN_POINT('Ctrl Pts',(-25.1692075360091,26.3374533006186,0.855994675877741));
#41926=CARTESIAN_POINT('Ctrl Pts',(-24.8517879203346,26.5142423148024,0.832907658370451));
#41927=CARTESIAN_POINT('Ctrl Pts',(-24.5655039130546,26.6240806033784,0.812081688067338));
#41928=CARTESIAN_POINT('Ctrl Pts',(-24.1237873074547,26.7250129503782,0.781595007996346));
#41929=CARTESIAN_POINT('Ctrl Pts',(-23.9773026401792,26.7480152345837,0.771778741118466));
#41930=CARTESIAN_POINT('Ctrl Pts',(-23.8236508809171,26.7613906835773,0.762114737343932));
#41931=CARTESIAN_POINT('Ctrl Pts',(-23.8175628977816,26.7619032065772,0.761732867924659));
#41932=CARTESIAN_POINT('Ctrl Pts',(-23.8088611205264,26.7626108600255,0.761188565604464));
#41933=CARTESIAN_POINT('Ctrl Pts',(-23.8062485368686,26.7628201149941,0.761025342050356));
#41934=CARTESIAN_POINT('Ctrl Pts',(-23.8017342101189,26.7631761482825,0.760743646345505));
#41935=CARTESIAN_POINT('Ctrl Pts',(-23.7998325894122,26.7633244256108,0.760625089030307));
#41936=CARTESIAN_POINT('Ctrl Pts',(-23.7961735838451,26.7636064656487,0.760397169277749));
#41937=CARTESIAN_POINT('Ctrl Pts',(-23.7944162243434,26.7637404747215,0.760287792889584));
#41938=CARTESIAN_POINT('Ctrl Pts',(-23.790254382727,26.7640544060914,0.760028974300967));
#41939=CARTESIAN_POINT('Ctrl Pts',(-23.7878498027661,26.7642330719661,0.759879603486389));
#41940=CARTESIAN_POINT('Ctrl Pts',(-23.7806818780102,26.7647575772358,0.759434826830249));
#41941=CARTESIAN_POINT('Ctrl Pts',(-23.7759179355652,26.7650955290496,0.759139864188646));
#41942=CARTESIAN_POINT('Ctrl Pts',(-23.7318307283083,26.768124573698,0.756415993953826));
#41943=CARTESIAN_POINT('Ctrl Pts',(-23.6924597871926,26.7701047893787,0.754026330346571));
#41944=CARTESIAN_POINT('Ctrl Pts',(-23.652582814233,26.7713775376484,0.751640331108725));
#41945=CARTESIAN_POINT('Ctrl Pts',(-23.6521053427244,26.7713926707744,0.751611767058734));
#41946=CARTESIAN_POINT('Ctrl Pts',(-23.647029499083,26.7715524163711,0.751308164806257));
#41947=CARTESIAN_POINT('Ctrl Pts',(-23.6424307999821,26.7716872890298,0.751033563017467));
#41948=CARTESIAN_POINT('Ctrl Pts',(-23.6333411723795,26.7719343938504,0.750491678173563));
#41949=CARTESIAN_POINT('Ctrl Pts',(-23.628850268389,26.7720470843275,0.750224375764226));
#41950=CARTESIAN_POINT('Ctrl Pts',(-23.616321233354,26.7723352635547,0.749479789619918));
#41951=CARTESIAN_POINT('Ctrl Pts',(-23.6082826095365,26.7724900643311,0.749003386789321));
#41952=CARTESIAN_POINT('Ctrl Pts',(-23.4692676032212,26.7746467067939,0.740786371494307));
#41953=CARTESIAN_POINT('Ctrl Pts',(-23.3382772669552,26.7686914472251,0.73337216273358));
#41954=CARTESIAN_POINT('Ctrl Pts',(-23.0392087468997,26.7367503371296,0.716503703248535));
#41955=CARTESIAN_POINT('Ctrl Pts',(-22.8721080548968,26.7054153622454,0.707111732053728));
#41956=CARTESIAN_POINT('Ctrl Pts',(-22.5644942953383,26.6221541235516,0.688922240850701));
#41957=CARTESIAN_POINT('Ctrl Pts',(-22.4236228484983,26.5733296306818,0.680217176689868));
#41958=CARTESIAN_POINT('Ctrl Pts',(-22.2748972972629,26.5099399508598,0.67039245023387));
#41959=CARTESIAN_POINT('Ctrl Pts',(-22.2631813460264,26.5048639018784,0.669614173759584));
#41960=CARTESIAN_POINT('Ctrl Pts',(-22.2469139320065,26.4977007709883,0.668527404569993));
#41961=CARTESIAN_POINT('Ctrl Pts',(-22.2423365931142,26.4956724552219,0.668220928177105));
#41962=CARTESIAN_POINT('Ctrl Pts',(-22.2348988213699,26.4923558645031,0.66772181646321));
#41963=CARTESIAN_POINT('Ctrl Pts',(-22.2320354982717,26.4910740592386,0.667529403823884));
#41964=CARTESIAN_POINT('Ctrl Pts',(-22.2261173419208,26.4884143366996,0.667131149791656));
#41965=CARTESIAN_POINT('Ctrl Pts',(-22.2230627779997,26.487035831624,0.666925288317764));
#41966=CARTESIAN_POINT('Ctrl Pts',(-22.2158988449067,26.4837893351799,0.66644174887494));
#41967=CARTESIAN_POINT('Ctrl Pts',(-22.2117912472008,26.4819174730593,0.666163937618385));
#41968=CARTESIAN_POINT('Ctrl Pts',(-22.1987934838375,26.475961287087,0.665283058514088));
#41969=CARTESIAN_POINT('Ctrl Pts',(-22.189918040534,26.4718451364542,0.664678891084597));
#41970=CARTESIAN_POINT('Ctrl Pts',(-22.1453991597498,26.45095184285,0.661634858846061));
#41971=CARTESIAN_POINT('Ctrl Pts',(-22.1100514947494,26.4335647989318,0.659174052746652));
#41972=CARTESIAN_POINT('Ctrl Pts',(-22.0750360011372,26.4155367672407,0.656690934610686));
#41973=CARTESIAN_POINT('Ctrl Pts',(-22.0750360367128,26.4155367855571,0.408876748608875));
#41974=CARTESIAN_POINT('Ctrl Pts',(-22.0995036376718,26.4281341425135,0.410434927469236));
#41975=CARTESIAN_POINT('Ctrl Pts',(-22.1241373073762,26.4404205190396,0.4119868098433));
#41976=CARTESIAN_POINT('Ctrl Pts',(-22.3097216831781,26.5300314085391,0.42357291862522));
#41977=CARTESIAN_POINT('Ctrl Pts',(-22.4766823563153,26.5941719314614,0.433427277109405));
#41978=CARTESIAN_POINT('Ctrl Pts',(-22.7408020895591,26.6711871429517,0.449108882320199));
#41979=CARTESIAN_POINT('Ctrl Pts',(-22.8346703305267,26.6940373028288,0.454695284139118));
#41980=CARTESIAN_POINT('Ctrl Pts',(-22.9913023769119,26.7247870842978,0.46414302470922));
#41981=CARTESIAN_POINT('Ctrl Pts',(-23.0535269468766,26.735116383894,0.467928013908913));
#41982=CARTESIAN_POINT('Ctrl Pts',(-23.1243180689114,26.7447427371464,0.472282943377488));
#41983=CARTESIAN_POINT('Ctrl Pts',(-23.1326290603348,26.7458398757349,0.472794970898169));
#41984=CARTESIAN_POINT('Ctrl Pts',(-23.1451274559382,26.7474402056085,0.473566138430657));
#41985=CARTESIAN_POINT('Ctrl Pts',(-23.1493117669356,26.7479676303426,0.473824511230317));
#41986=CARTESIAN_POINT('Ctrl Pts',(-23.1565130584911,26.7488609831649,0.474269516692919));
#41987=CARTESIAN_POINT('Ctrl Pts',(-23.1595295509132,26.7492308609055,0.474456024170555));
#41988=CARTESIAN_POINT('Ctrl Pts',(-23.165745790361,26.7499841632206,0.474840582898491));
#41989=CARTESIAN_POINT('Ctrl Pts',(-23.1689455976152,26.7503670561788,0.475038650755829));
#41990=CARTESIAN_POINT('Ctrl Pts',(-23.1766550107426,26.7512778471369,0.475516145693151));
#41991=CARTESIAN_POINT('Ctrl Pts',(-23.1811651595905,26.7518010147242,0.475795722019741));
#41992=CARTESIAN_POINT('Ctrl Pts',(-23.1950255521417,26.7533791129557,0.476655627947201));
#41993=CARTESIAN_POINT('Ctrl Pts',(-23.2043792595696,26.7544026185659,0.4772369490259));
#41994=CARTESIAN_POINT('Ctrl Pts',(-23.3145684451345,26.765971670739,0.484097249267685));
#41995=CARTESIAN_POINT('Ctrl Pts',(-23.4158326476031,26.7717931778601,0.490524737896736));
#41996=CARTESIAN_POINT('Ctrl Pts',(-23.8067120235829,26.7758029328656,0.515845359116236));
#41997=CARTESIAN_POINT('Ctrl Pts',(-24.0952899525238,26.7397403553443,0.535769536277604));
#41998=CARTESIAN_POINT('Ctrl Pts',(-24.4176120450762,26.6544012371775,0.558038621149693));
#41999=CARTESIAN_POINT('Ctrl Pts',(-24.4598928680931,26.6422755672834,0.560956341297723));
#42000=CARTESIAN_POINT('Ctrl Pts',(-24.5667552660202,26.6092467823837,0.568301523436472));
#42001=CARTESIAN_POINT('Ctrl Pts',(-24.6309533289382,26.587160663152,0.572686797668253));
#42002=CARTESIAN_POINT('Ctrl Pts',(-24.7011931172345,26.5604860709049,0.577418185681183));
#42003=CARTESIAN_POINT('Ctrl Pts',(-24.707966508835,26.5578875729754,0.577873746830789));
#42004=CARTESIAN_POINT('Ctrl Pts',(-24.7182659248607,26.5538964265036,0.57856533211947));
#42005=CARTESIAN_POINT('Ctrl Pts',(-24.7217983072182,26.5525204127538,0.578802322128006));
#42006=CARTESIAN_POINT('Ctrl Pts',(-24.7283154188769,26.5499684661719,0.579239174715101));
#42007=CARTESIAN_POINT('Ctrl Pts',(-24.7313008304196,26.548794305625,0.579439142269598));
#42008=CARTESIAN_POINT('Ctrl Pts',(-24.7361569948146,26.5468760015715,0.57976416653539));
#42009=CARTESIAN_POINT('Ctrl Pts',(-24.7380288030023,26.5461345629564,0.579889386761071));
#42010=CARTESIAN_POINT('Ctrl Pts',(-24.7416520469411,26.5446954367826,0.580131655889902));
#42011=CARTESIAN_POINT('Ctrl Pts',(-24.7434035600598,26.5439979684823,0.580248717279999));
#42012=CARTESIAN_POINT('Ctrl Pts',(-24.7474235708563,26.5423930756796,0.580517270115671));
#42013=CARTESIAN_POINT('Ctrl Pts',(-24.749691654668,26.5414846059982,0.580668697821311));
#42014=CARTESIAN_POINT('Ctrl Pts',(-24.7568623185684,26.5386029651769,0.581147168108609));
#42015=CARTESIAN_POINT('Ctrl Pts',(-24.761761111704,26.536620300838,0.581473636627261));
#42016=CARTESIAN_POINT('Ctrl Pts',(-24.8026808536453,26.5199417971001,0.584197393056457));
#42017=CARTESIAN_POINT('Ctrl Pts',(-24.8384398091579,26.5046060827787,0.586556592443559));
#42018=CARTESIAN_POINT('Ctrl Pts',(-25.0081700280381,26.4281469778153,0.597693660707304));
#42019=CARTESIAN_POINT('Ctrl Pts',(-25.1381389519207,26.3585307122643,0.606042386981039));
#42020=CARTESIAN_POINT('Ctrl Pts',(-25.3361263130104,26.2343248617678,0.619154653779421));
#42021=CARTESIAN_POINT('Ctrl Pts',(-25.4074725619995,26.1854609369353,0.6239680617356));
#42022=CARTESIAN_POINT('Ctrl Pts',(-25.5504213732254,26.0788654715814,0.633953103900781));
#42023=CARTESIAN_POINT('Ctrl Pts',(-25.6216896073023,26.020820514944,0.6391238418908));
#42024=CARTESIAN_POINT('Ctrl Pts',(-25.7524727360789,25.9046613876217,0.649129813942959));
#42025=CARTESIAN_POINT('Ctrl Pts',(-25.8124080962872,25.8471342416085,0.65394555122834));
#42026=CARTESIAN_POINT('Ctrl Pts',(-25.9154825435877,25.7402497524828,0.662724490027008));
#42027=CARTESIAN_POINT('Ctrl Pts',(-25.959464799315,25.6917697865474,0.666649754557606));
#42028=CARTESIAN_POINT('Ctrl Pts',(-26.0074243981403,25.6355571663038,0.671153732534353));
#42029=CARTESIAN_POINT('Ctrl Pts',(-26.0128848940787,25.6291057843242,0.671669953436111));
#42030=CARTESIAN_POINT('Ctrl Pts',(-26.0210409740907,25.6193924354149,0.672446188194751));
#42031=CARTESIAN_POINT('Ctrl Pts',(-26.0237556450177,25.6161464825928,0.67270541961517));
#42032=CARTESIAN_POINT('Ctrl Pts',(-26.028410298429,25.6105585512142,0.673151407204916));
#42033=CARTESIAN_POINT('Ctrl Pts',(-26.0303533780605,25.6082191501421,0.673338036627604));
#42034=CARTESIAN_POINT('Ctrl Pts',(-26.0343452702479,25.6033991849126,0.673722385412113));
#42035=CARTESIAN_POINT('Ctrl Pts',(-26.0363936849855,25.6009182965478,0.673920120699752));
#42036=CARTESIAN_POINT('Ctrl Pts',(-26.0413113669479,25.5949441654835,0.674396057980072));
#42037=CARTESIAN_POINT('Ctrl Pts',(-26.0441770003041,25.5914479516696,0.674674407098615));
#42038=CARTESIAN_POINT('Ctrl Pts',(-26.0529336179612,25.5807184798958,0.675528081317239));
#42039=CARTESIAN_POINT('Ctrl Pts',(-26.0588005205612,25.5734657115093,0.676104378391196));
#42040=CARTESIAN_POINT('Ctrl Pts',(-26.0804748243287,25.5464323478187,0.678249695638889));
#42041=CARTESIAN_POINT('Ctrl Pts',(-26.0960800955957,25.5264915517208,0.679826784206252));
#42042=CARTESIAN_POINT('Ctrl Pts',(-26.1152704033688,25.5013651707364,0.681807788966305));
#42043=CARTESIAN_POINT('Ctrl Pts',(-26.1190776862472,25.496349789456,0.682202904628665));
#42044=CARTESIAN_POINT('Ctrl Pts',(-26.1249527398742,25.4885632280032,0.682815870918273));
#42045=CARTESIAN_POINT('Ctrl Pts',(-26.1270308056451,25.4857998042177,0.683033320199309));
#42046=CARTESIAN_POINT('Ctrl Pts',(-26.1299448343687,25.4819117018769,0.683339142683186));
#42047=CARTESIAN_POINT('Ctrl Pts',(-26.1307845224279,25.4807898069154,0.683427371726358));
#42048=CARTESIAN_POINT('Ctrl Pts',(-26.1341437571173,25.4762954749178,0.683780760238077));
#42049=CARTESIAN_POINT('Ctrl Pts',(-26.1366574179843,25.4729186618021,0.684046146283691));
#42050=CARTESIAN_POINT('Ctrl Pts',(-26.1433079615744,25.4639477810893,0.684750826555741));
#42051=CARTESIAN_POINT('Ctrl Pts',(-26.1474333406327,25.458345248114,0.685190559379306));
#42052=CARTESIAN_POINT('Ctrl Pts',(-26.1560465883395,25.4465682127376,0.686114179150925));
#42053=CARTESIAN_POINT('Ctrl Pts',(-26.1605307223886,25.4403910433929,0.686598203694183));
#42054=CARTESIAN_POINT('Ctrl Pts',(-26.1673233637086,25.4309634920476,0.687336282696466));
#42055=CARTESIAN_POINT('Ctrl Pts',(-26.1696478769986,25.427724630274,0.687589738159199));
#42056=CARTESIAN_POINT('Ctrl Pts',(-26.1750790273205,25.4201274143702,0.688183989643753));
#42057=CARTESIAN_POINT('Ctrl Pts',(-26.1781808220264,25.4157656271529,0.68852496364681));
#42058=CARTESIAN_POINT('Ctrl Pts',(-26.1935339793735,25.3940615248334,0.690220634591346));
#42059=CARTESIAN_POINT('Ctrl Pts',(-26.2056243876301,25.3766064645495,0.691581171497676));
#42060=CARTESIAN_POINT('Ctrl Pts',(-26.361722927432,25.1464183602922,0.709482216385985));
#42061=CARTESIAN_POINT('Ctrl Pts',(-26.4799471212204,24.9173518388607,0.726951110880739));
#42062=CARTESIAN_POINT('Ctrl Pts',(-26.598671974789,24.5991184641266,0.749874264365667));
#42063=CARTESIAN_POINT('Ctrl Pts',(-26.6246274815847,24.5204076022534,0.755432953171279));
#42064=CARTESIAN_POINT('Ctrl Pts',(-26.6637379983157,24.3843806488808,0.764766814481929));
#42065=CARTESIAN_POINT('Ctrl Pts',(-26.6784116876,24.327544431243,0.76858738982242));
#42066=CARTESIAN_POINT('Ctrl Pts',(-26.6976514324485,24.243613416311,0.774083463749585));
#42067=CARTESIAN_POINT('Ctrl Pts',(-26.703436044812,24.2168131159379,0.77581685904736));
#42068=CARTESIAN_POINT('Ctrl Pts',(-26.7097524931961,24.1856240434316,0.777806559031801));
#42069=CARTESIAN_POINT('Ctrl Pts',(-26.7106179608429,24.1813050805759,0.778081475091815));
#42070=CARTESIAN_POINT('Ctrl Pts',(-26.7119204846962,24.1747351775414,0.778498727567766));
#42071=CARTESIAN_POINT('Ctrl Pts',(-26.7123639935446,24.1724855450559,0.778641432995534));
#42072=CARTESIAN_POINT('Ctrl Pts',(-26.7131638725067,24.1684053369344,0.778899953956846));
#42073=CARTESIAN_POINT('Ctrl Pts',(-26.7135210533841,24.1665749312589,0.779015815850281));
#42074=CARTESIAN_POINT('Ctrl Pts',(-26.7142366284006,24.1628908937182,0.779248784016214));
#42075=CARTESIAN_POINT('Ctrl Pts',(-26.7145949810986,24.1610372644572,0.779365887576553));
#42076=CARTESIAN_POINT('Ctrl Pts',(-26.7156146598695,24.1557378500577,0.779700354452553));
#42077=CARTESIAN_POINT('Ctrl Pts',(-26.7162719904694,24.1522912847455,0.77991748793278));
#42078=CARTESIAN_POINT('Ctrl Pts',(-26.719074614199,24.1374648235411,0.780849892412955));
#42079=CARTESIAN_POINT('Ctrl Pts',(-26.7211642252107,24.1260742990857,0.781562009672773));
#42080=CARTESIAN_POINT('Ctrl Pts',(-26.7561604236966,23.9293398994024,0.793792840328805));
#42081=CARTESIAN_POINT('Ctrl Pts',(-26.7728324644746,23.7414434010028,0.804433783195011));
#42082=CARTESIAN_POINT('Ctrl Pts',(-26.7732725053934,23.2504829657748,0.831934080181385));
#42083=CARTESIAN_POINT('Ctrl Pts',(-26.7309132814301,22.9493419044259,0.848652270162657));
#42084=CARTESIAN_POINT('Ctrl Pts',(-26.6421112696967,22.6409326161044,0.868084768824089));
#42085=CARTESIAN_POINT('Ctrl Pts',(-26.636892459408,22.6233722267457,0.869198780460152));
#42086=CARTESIAN_POINT('Ctrl Pts',(-26.6297679844223,22.6001272451644,0.870683773263436));
#42087=CARTESIAN_POINT('Ctrl Pts',(-26.627995696984,22.594401867919,0.871050373053453));
#42088=CARTESIAN_POINT('Ctrl Pts',(-26.6252140207211,22.5855036061092,0.871621449631648));
#42089=CARTESIAN_POINT('Ctrl Pts',(-26.6242156619745,22.5823272649716,0.871825563345842));
#42090=CARTESIAN_POINT('Ctrl Pts',(-26.6222129698167,22.5759899234901,0.872233328785831));
#42091=CARTESIAN_POINT('Ctrl Pts',(-26.6212086753772,22.5728289149443,0.87243697902277));
#42092=CARTESIAN_POINT('Ctrl Pts',(-26.6189428274349,22.5657351425572,0.87289458819865));
#42093=CARTESIAN_POINT('Ctrl Pts',(-26.6176785916271,22.5618032475742,0.873148635330487));
#42094=CARTESIAN_POINT('Ctrl Pts',(-26.61395514909,22.5502989206679,0.873893147675802));
#42095=CARTESIAN_POINT('Ctrl Pts',(-26.6114754483081,22.5427331993652,0.874384289069713));
#42096=CARTESIAN_POINT('Ctrl Pts',(-26.5929730385625,22.4869801156199,0.878014921971213));
#42097=CARTESIAN_POINT('Ctrl Pts',(-26.5758421891125,22.4391705981788,0.88119098441538));
#42098=CARTESIAN_POINT('Ctrl Pts',(-26.5159516436911,22.2836966588994,0.89173494847809));
#42099=CARTESIAN_POINT('Ctrl Pts',(-26.4685208557158,22.1779406787224,0.899255995543369));
#42100=CARTESIAN_POINT('Ctrl Pts',(-26.2732713663549,21.7987308700924,0.927493279158542));
#42101=CARTESIAN_POINT('Ctrl Pts',(-26.0918527940358,21.5445332298945,0.949145815305843));
#42102=CARTESIAN_POINT('Ctrl Pts',(-25.8512281201052,21.2934844071552,0.971502463498003));
#42103=CARTESIAN_POINT('Ctrl Pts',(-25.8251229029251,21.2671721312342,0.973856979799311));
#42104=CARTESIAN_POINT('Ctrl Pts',(-25.7948815950805,21.2377248218776,0.976498944525474));
#42105=CARTESIAN_POINT('Ctrl Pts',(-25.7911863278011,21.2341437770783,0.976820348778215));
#42106=CARTESIAN_POINT('Ctrl Pts',(-25.7857166701628,21.2288685336243,0.977293963726078));
#42107=CARTESIAN_POINT('Ctrl Pts',(-25.7839489202103,21.2271675085191,0.977446706642546));
#42108=CARTESIAN_POINT('Ctrl Pts',(-25.7808181539938,21.2241617924712,0.977716642952823));
#42109=CARTESIAN_POINT('Ctrl Pts',(-25.7794559333906,21.2228562791357,0.97783390108372));
#42110=CARTESIAN_POINT('Ctrl Pts',(-25.7766111756814,21.2201347334167,0.97807837006634));
#42111=CARTESIAN_POINT('Ctrl Pts',(-25.7751284368017,21.21871892215,0.978205563595296));
#42112=CARTESIAN_POINT('Ctrl Pts',(-25.7712570521657,21.2150293393294,0.978537070651937));
#42113=CARTESIAN_POINT('Ctrl Pts',(-25.7688662578002,21.2127578102714,0.978741208666828));
#42114=CARTESIAN_POINT('Ctrl Pts',(-25.758503261313,21.2029419963314,0.979623543181706));
#42115=CARTESIAN_POINT('Ctrl Pts',(-25.7504959106077,21.1954346797036,0.980298896795738));
#42116=CARTESIAN_POINT('Ctrl Pts',(-25.6924517009059,21.1415697042424,0.985149760794836));
#42117=CARTESIAN_POINT('Ctrl Pts',(-25.6409884315136,21.0967661943485,0.989212666162239));
#42118=CARTESIAN_POINT('Ctrl Pts',(-25.5540392370581,21.025793425754,0.99577120521706));
#42119=CARTESIAN_POINT('Ctrl Pts',(-25.5193729639377,20.9986608830158,0.998310694409467));
#42120=CARTESIAN_POINT('Ctrl Pts',(-25.2504710055561,20.796942359928,1.0175330764218));
#42121=CARTESIAN_POINT('Ctrl Pts',(-24.9940360356269,20.6542272665234,1.0332961043754));
#42122=CARTESIAN_POINT('Ctrl Pts',(-24.6301602949257,20.5122254939189,1.05603627288238));
#42123=CARTESIAN_POINT('Ctrl Pts',(-24.536867432782,20.4806601969072,1.0618816518633));
#42124=CARTESIAN_POINT('Ctrl Pts',(-24.4333070150722,20.4508300704414,1.06844145339731));
#42125=CARTESIAN_POINT('Ctrl Pts',(-24.4243199920023,20.4482836592074,1.06901127139889));
#42126=CARTESIAN_POINT('Ctrl Pts',(-24.4109645552231,20.4445621354021,1.0698589330914));
#42127=CARTESIAN_POINT('Ctrl Pts',(-24.4066044771938,20.4433570763935,1.07013580137979));
#42128=CARTESIAN_POINT('Ctrl Pts',(-24.3991383037835,20.441310450455,1.0706101482528));
#42129=CARTESIAN_POINT('Ctrl Pts',(-24.3960334495205,20.4404643463857,1.07080747900561));
#42130=CARTESIAN_POINT('Ctrl Pts',(-24.3897343058152,20.4387578977413,1.07120797008468));
#42131=CARTESIAN_POINT('Ctrl Pts',(-24.3865399496019,20.4378978185034,1.07141113872544));
#42132=CARTESIAN_POINT('Ctrl Pts',(-24.3792067321786,20.4359354570795,1.07187772517848));
#42133=CARTESIAN_POINT('Ctrl Pts',(-24.375066993221,20.4348365062635,1.07214125081594));
#42134=CARTESIAN_POINT('Ctrl Pts',(-24.3663845020643,20.4325501379371,1.07269423179524));
#42135=CARTESIAN_POINT('Ctrl Pts',(-24.3618413241777,20.4313643899618,1.07298374069533));
#42136=CARTESIAN_POINT('Ctrl Pts',(-24.3498435550139,20.4282610188535,1.07374870835422));
#42137=CARTESIAN_POINT('Ctrl Pts',(-24.3423846902959,20.4263601755973,1.07422471013595));
#42138=CARTESIAN_POINT('Ctrl Pts',(-24.3200325684135,20.4207490834243,1.07565247907355));
#42139=CARTESIAN_POINT('Ctrl Pts',(-24.3051197038885,20.417118529316,1.07660681603012));
#42140=CARTESIAN_POINT('Ctrl Pts',(-24.1371566286211,20.3774964916496,1.08737616900261));
#42141=CARTESIAN_POINT('Ctrl Pts',(-23.9817189932269,20.3526501841446,1.09755131882267));
#42142=CARTESIAN_POINT('Ctrl Pts',(-23.5033041620485,20.3116987966174,1.12944360520425));
#42143=CARTESIAN_POINT('Ctrl Pts',(-23.1792101991778,20.3326829813672,1.15200749182668));
#42144=CARTESIAN_POINT('Ctrl Pts',(-22.8479126284273,20.4049233161702,1.17346161596833));
#42145=CARTESIAN_POINT('Ctrl Pts',(-22.8321944430288,20.4084744012606,1.17447504536514));
#42146=CARTESIAN_POINT('Ctrl Pts',(-22.8127924252049,20.4130109604647,1.17571991996125));
#42147=CARTESIAN_POINT('Ctrl Pts',(-22.8090832014797,20.4138851888562,1.17595763658883));
#42148=CARTESIAN_POINT('Ctrl Pts',(-22.8032471099614,20.4152716309278,1.17633121721482));
#42149=CARTESIAN_POINT('Ctrl Pts',(-22.8011192133105,20.4157794308965,1.17646733569463));
#42150=CARTESIAN_POINT('Ctrl Pts',(-22.7971964829261,20.4167197716297,1.17671809398807));
#42151=CARTESIAN_POINT('Ctrl Pts',(-22.7954015141997,20.4171516855028,1.17683276923952));
#42152=CARTESIAN_POINT('Ctrl Pts',(-22.7914041247192,20.4181171909027,1.17708800166862));
#42153=CARTESIAN_POINT('Ctrl Pts',(-22.7892019004251,20.4186515618189,1.17722851267862));
#42154=CARTESIAN_POINT('Ctrl Pts',(-22.7828438517557,20.4202014486412,1.17763389692923));
#42155=CARTESIAN_POINT('Ctrl Pts',(-22.7786894631304,20.421222922327,1.17789842506234));
#42156=CARTESIAN_POINT('Ctrl Pts',(-22.7506918013589,20.4281660871219,1.17967885723378));
#42157=CARTESIAN_POINT('Ctrl Pts',(-22.726914039097,20.4343521893578,1.18117967427281));
#42158=CARTESIAN_POINT('Ctrl Pts',(-22.6535690912806,20.4543321044506,1.18578075643764));
#42159=CARTESIAN_POINT('Ctrl Pts',(-22.6042575641248,20.4690419501657,1.18883391144853));
#42160=CARTESIAN_POINT('Ctrl Pts',(-22.5136504203636,20.4984510006402,1.19440483147114));
#42161=CARTESIAN_POINT('Ctrl Pts',(-22.472262836203,20.5128235171879,1.19693411092816));
#42162=CARTESIAN_POINT('Ctrl Pts',(-22.1696842245451,20.6248629702744,1.21539685485603));
#42163=CARTESIAN_POINT('Ctrl Pts',(-21.9218615706629,20.7552160898329,1.23047085079505));
#42164=CARTESIAN_POINT('Ctrl Pts',(-21.6017223833773,20.98080430518,1.25313700096463));
#42165=CARTESIAN_POINT('Ctrl Pts',(-21.513024435206,21.0505463005997,1.25980511608295));
#42166=CARTESIAN_POINT('Ctrl Pts',(-21.4202568261997,21.1317103252983,1.26730596167425));
#42167=CARTESIAN_POINT('Ctrl Pts',(-21.4123778127606,21.1386721802291,1.26794737404487));
#42168=CARTESIAN_POINT('Ctrl Pts',(-21.4013426682423,21.1485193564352,1.26885191577603));
#42169=CARTESIAN_POINT('Ctrl Pts',(-21.3981579373047,21.1513726466451,1.26911369722539));
#42170=CARTESIAN_POINT('Ctrl Pts',(-21.3926347690407,21.1563408595619,1.26956897367359));
#42171=CARTESIAN_POINT('Ctrl Pts',(-21.3902937336231,21.1584528966458,1.26976234660244));
#42172=CARTESIAN_POINT('Ctrl Pts',(-21.3854736737971,21.162814309629,1.27016131976304));
#42173=CARTESIAN_POINT('Ctrl Pts',(-21.3829950481802,21.1650641182147,1.27036693820086));
#42174=CARTESIAN_POINT('Ctrl Pts',(-21.3771874950381,21.1703520671661,1.27084978264821));
#42175=CARTESIAN_POINT('Ctrl Pts',(-21.3738614327931,21.1733933312171,1.27112714138503));
#42176=CARTESIAN_POINT('Ctrl Pts',(-21.3668549686429,21.1798268953869,1.27171316240238));
#42177=CARTESIAN_POINT('Ctrl Pts',(-21.3631760713803,21.1832208099192,1.27202189334804));
#42178=CARTESIAN_POINT('Ctrl Pts',(-21.3533125229077,21.1923629134108,1.27285241373305));
#42179=CARTESIAN_POINT('Ctrl Pts',(-21.3471425619303,21.1981268307249,1.27337487805268));
#42180=CARTESIAN_POINT('Ctrl Pts',(-21.1518670228843,21.3819937535564,1.29000503723837));
#42181=CARTESIAN_POINT('Ctrl Pts',(-20.9850061740106,21.5822451677835,1.30716104934124));
#42182=CARTESIAN_POINT('Ctrl Pts',(-20.7304469300662,21.9759106248341,1.33884275640988));
#42183=CARTESIAN_POINT('Ctrl Pts',(-20.6342415915367,22.1621787398352,1.35312090826121));
#42184=CARTESIAN_POINT('Ctrl Pts',(-20.5424689954772,22.392304198516,1.36906515083092));
#42185=CARTESIAN_POINT('Ctrl Pts',(-20.5288211299047,22.4283974795373,1.37151799739849));
#42186=CARTESIAN_POINT('Ctrl Pts',(-20.5142250428256,22.4691987937817,1.37423048981934));
#42187=CARTESIAN_POINT('Ctrl Pts',(-20.5126359373132,22.4736720546063,1.37452706677275));
#42188=CARTESIAN_POINT('Ctrl Pts',(-20.5102569968641,22.4804158667567,1.37497294768239));
#42189=CARTESIAN_POINT('Ctrl Pts',(-20.5094598178541,22.4826837924642,1.37512268640962));
#42190=CARTESIAN_POINT('Ctrl Pts',(-20.5080831815195,22.4866142909213,1.37538182974064));
#42191=CARTESIAN_POINT('Ctrl Pts',(-20.5075025491421,22.4882764462333,1.37549130472152));
#42192=CARTESIAN_POINT('Ctrl Pts',(-20.5062952119632,22.491741765432,1.37571930469514));
#42193=CARTESIAN_POINT('Ctrl Pts',(-20.5056687478071,22.4935450085134,1.37583781474935));
#42194=CARTESIAN_POINT('Ctrl Pts',(-20.5041832586636,22.4978331954764,1.37611932042017));
#42195=CARTESIAN_POINT('Ctrl Pts',(-20.5033256691886,22.5003186432964,1.37628222991182));
#42196=CARTESIAN_POINT('Ctrl Pts',(-20.5004702000861,22.508627266522,1.37682598785116));
#42197=CARTESIAN_POINT('Ctrl Pts',(-20.4984859489215,22.5144551630033,1.37720602762583));
#42198=CARTESIAN_POINT('Ctrl Pts',(-20.443373652309,22.677857320869,1.38782424444582));
#42199=CARTESIAN_POINT('Ctrl Pts',(-20.4024952843724,22.8393294348641,1.39735128594478));
#42200=CARTESIAN_POINT('Ctrl Pts',(-20.3413817849476,23.1941702484797,1.41762717609679));
#42201=CARTESIAN_POINT('Ctrl Pts',(-20.3257824676052,23.3876533650958,1.42829315917424));
#42202=CARTESIAN_POINT('Ctrl Pts',(-20.3290761249458,23.7287952150526,1.44778715597633));
#42203=CARTESIAN_POINT('Ctrl Pts',(-20.3406142673435,23.8759336824188,1.45641622388821));
#42204=CARTESIAN_POINT('Ctrl Pts',(-20.3638118936337,24.0327854257133,1.46606064882687));
#42205=CARTESIAN_POINT('Ctrl Pts',(-20.3655007381437,24.0438089542738,1.46674078353661));
#42206=CARTESIAN_POINT('Ctrl Pts',(-20.3679333606254,24.0591547701043,1.46769090831552));
#42207=CARTESIAN_POINT('Ctrl Pts',(-20.3686288101472,24.0634847296226,1.46795936236115));
#42208=CARTESIAN_POINT('Ctrl Pts',(-20.3698439935893,24.0709532267092,1.46842304296187));
#42209=CARTESIAN_POINT('Ctrl Pts',(-20.3703595420474,24.074092447437,1.46861813621453));
#42210=CARTESIAN_POINT('Ctrl Pts',(-20.3714234686052,24.0805113431904,1.46901745293488));
#42211=CARTESIAN_POINT('Ctrl Pts',(-20.3719722759146,24.0837909418398,1.46922168981802));
#42212=CARTESIAN_POINT('Ctrl Pts',(-20.3732587372041,24.0914062388109,1.4696964330935));
#42213=CARTESIAN_POINT('Ctrl Pts',(-20.3740001913481,24.0957412805185,1.46996706021925));
#42214=CARTESIAN_POINT('Ctrl Pts',(-20.3755787333402,24.1048581602972,1.4705370066209));
#42215=CARTESIAN_POINT('Ctrl Pts',(-20.3764177561066,24.1096396481787,1.4708363870532));
#42216=CARTESIAN_POINT('Ctrl Pts',(-20.3786819471274,24.122373906398,1.47163495301786));
#42217=CARTESIAN_POINT('Ctrl Pts',(-20.3801262169674,24.1303232058794,1.47213474737738));
#42218=CARTESIAN_POINT('Ctrl Pts',(-20.3845912495906,24.1543840712685,1.47365148282445));
#42219=CARTESIAN_POINT('Ctrl Pts',(-20.387705024626,24.1704779097886,1.47467138785947));
#42220=CARTESIAN_POINT('Ctrl Pts',(-20.450877581508,24.4841404582638,1.49465624932366));
#42221=CARTESIAN_POINT('Ctrl Pts',(-20.5525492667497,24.7717109928437,1.51508762909092));
#42222=CARTESIAN_POINT('Ctrl Pts',(-20.7516736320597,25.1534474304713,1.54420754256351));
#42223=CARTESIAN_POINT('Ctrl Pts',(-20.8170882393964,25.2625887684959,1.55276458740409));
#42224=CARTESIAN_POINT('Ctrl Pts',(-20.8919848809947,25.3722741771886,1.56142524484949));
#42225=CARTESIAN_POINT('Ctrl Pts',(-20.8951980175028,25.3769531932459,1.56179480716745));
#42226=CARTESIAN_POINT('Ctrl Pts',(-20.9027130372604,25.3878349563095,1.56265449773609));
#42227=CARTESIAN_POINT('Ctrl Pts',(-20.9070244030506,25.3940311528536,1.56314418028636));
#42228=CARTESIAN_POINT('Ctrl Pts',(-20.9136054742975,25.4034187931727,1.56388626573679));
#42229=CARTESIAN_POINT('Ctrl Pts',(-20.915859264518,25.4066213022014,1.56413945428967));
#42230=CARTESIAN_POINT('Ctrl Pts',(-20.9198030286529,25.4122035228076,1.56458082793997));
#42231=CARTESIAN_POINT('Ctrl Pts',(-20.9214904038212,25.4145850547557,1.56476914512493));
#42232=CARTESIAN_POINT('Ctrl Pts',(-20.9264334852064,25.4215415804054,1.56531926098659));
#42233=CARTESIAN_POINT('Ctrl Pts',(-20.929697933294,25.4261103861867,1.56568060340826));
#42234=CARTESIAN_POINT('Ctrl Pts',(-20.9538565468341,25.4597357864824,1.56834020210734));
#42235=CARTESIAN_POINT('Ctrl Pts',(-20.9752225772096,25.4884525756113,1.57061266592819));
#42236=CARTESIAN_POINT('Ctrl Pts',(-20.9998981955187,25.520489040454,1.57314354692306));
#42237=CARTESIAN_POINT('Ctrl Pts',(-21.0027407281935,25.5241630545311,1.57343372917156));
#42238=CARTESIAN_POINT('Ctrl Pts',(-21.0070503428838,25.5297084780446,1.57387160487157));
#42239=CARTESIAN_POINT('Ctrl Pts',(-21.0085115533534,25.5315844109675,1.57401971166002));
#42240=CARTESIAN_POINT('Ctrl Pts',(-21.0110541964559,25.5348412682416,1.57427680657262));
#42241=CARTESIAN_POINT('Ctrl Pts',(-21.0121346800249,25.5362229267352,1.57438586242916));
#42242=CARTESIAN_POINT('Ctrl Pts',(-21.0143968449302,25.5391107879311,1.57461377889145));
#42243=CARTESIAN_POINT('Ctrl Pts',(-21.0155787396543,25.5406168188192,1.57473262343937));
#42244=CARTESIAN_POINT('Ctrl Pts',(-21.0184054395778,25.5442121439111,1.57501630621624));
#42245=CARTESIAN_POINT('Ctrl Pts',(-21.0200514948338,25.5463004635342,1.5751810547206));
#42246=CARTESIAN_POINT('Ctrl Pts',(-21.0256240980098,25.5533523517118,1.5757373003784));
#42247=CARTESIAN_POINT('Ctrl Pts',(-21.0295627142124,25.5583064310639,1.57612793703275));
#42248=CARTESIAN_POINT('Ctrl Pts',(-21.0389487908096,25.5700413166878,1.5770530135684));
#42249=CARTESIAN_POINT('Ctrl Pts',(-21.0444091909939,25.5768117760394,1.57758654889389));
#42250=CARTESIAN_POINT('Ctrl Pts',(-21.1085514912436,25.655687473222,1.58380111624698));
#42251=CARTESIAN_POINT('Ctrl Pts',(-21.1703058013761,25.7252507930029,1.58927146175341));
#42252=CARTESIAN_POINT('Ctrl Pts',(-21.3528530117786,25.9137801020719,1.60438821959014));
#42253=CARTESIAN_POINT('Ctrl Pts',(-21.4801406929185,26.026029351804,1.61375622192197));
#42254=CARTESIAN_POINT('Ctrl Pts',(-21.6965110233861,26.1884292900875,1.628905197601));
#42255=CARTESIAN_POINT('Ctrl Pts',(-21.7801575944174,26.245265818469,1.6345967792353));
#42256=CARTESIAN_POINT('Ctrl Pts',(-21.9344422770162,26.3398144572332,1.64498041584185));
#42257=CARTESIAN_POINT('Ctrl Pts',(-22.0040585157554,26.3789933939254,1.64962651365814));
#42258=CARTESIAN_POINT('Ctrl Pts',(-22.0750360931093,26.4155368145933,1.65435918102699));
#42259=CARTESIAN_POINT('Origin',(-23.5502525316942,23.5502525316942,-77.3107734492734));
#42260=CARTESIAN_POINT('',(-22.0750360153455,26.415536774556,3.15065971150053));
#42261=CARTESIAN_POINT('',(-22.0750360171757,26.4155367754983,2.90599376073416));
#42262=CARTESIAN_POINT('',(-22.0750360153461,26.4155367745563,-77.3107734492734));
#42263=CARTESIAN_POINT('Ctrl Pts',(-22.0750360153455,26.415536774556,3.15065971150053));
#42264=CARTESIAN_POINT('Ctrl Pts',(-22.0689721537274,26.4124147426549,3.15022964192226));
#42265=CARTESIAN_POINT('Ctrl Pts',(-22.0629181479893,26.4092734328418,3.14980069220542));
#42266=CARTESIAN_POINT('Ctrl Pts',(-22.0526714943233,26.4039152816198,3.14907545024222));
#42267=CARTESIAN_POINT('Ctrl Pts',(-22.0484737222784,26.4017083812685,3.14877855940214));
#42268=CARTESIAN_POINT('Ctrl Pts',(-22.040876312398,26.3976927540212,3.14824164812645));
#42269=CARTESIAN_POINT('Ctrl Pts',(-22.0374750258636,26.3958871901358,3.14800143178819));
#42270=CARTESIAN_POINT('Ctrl Pts',(-22.0321711014334,26.3930594189751,3.14762709115791));
#42271=CARTESIAN_POINT('Ctrl Pts',(-22.0302662554384,26.3920413956555,3.14749270123395));
#42272=CARTESIAN_POINT('Ctrl Pts',(-22.0268765330157,26.3902254137327,3.1472536426412));
#42273=CARTESIAN_POINT('Ctrl Pts',(-22.0253912658919,26.3894282085682,3.14714892641721));
#42274=CARTESIAN_POINT('Ctrl Pts',(-22.0219857030607,26.3875968569275,3.14690889530204));
#42275=CARTESIAN_POINT('Ctrl Pts',(-22.0200658348211,26.3865619281134,3.14677363152521));
#42276=CARTESIAN_POINT('Ctrl Pts',(-22.0148191415902,26.383726755263,3.14640411680164));
#42277=CARTESIAN_POINT('Ctrl Pts',(-22.0114944197689,26.3819225944676,3.14617011652517));
#42278=CARTESIAN_POINT('Ctrl Pts',(-21.9954016433121,26.3731531348337,3.14503818338911));
#42279=CARTESIAN_POINT('Ctrl Pts',(-21.9826773988296,26.3661071660755,3.14414534600292));
#42280=CARTESIAN_POINT('Ctrl Pts',(-21.7433708370467,26.2314678259684,3.12738619663064));
#42281=CARTESIAN_POINT('Ctrl Pts',(-21.5329637759489,26.0769760630842,3.11315439362061));
#42282=CARTESIAN_POINT('Ctrl Pts',(-21.3141500402638,25.8713672050449,3.09634236253687));
#42283=CARTESIAN_POINT('Ctrl Pts',(-21.285423912797,25.8433462801086,3.09409070725609));
#42284=CARTESIAN_POINT('Ctrl Pts',(-21.2293461717112,25.786563286217,3.08959199488535));
#42285=CARTESIAN_POINT('Ctrl Pts',(-21.2019878466722,25.7578179296223,3.08734556221746));
#42286=CARTESIAN_POINT('Ctrl Pts',(-21.1090899986132,25.6565288653715,3.07951567208062));
#42287=CARTESIAN_POINT('Ctrl Pts',(-21.0463294478684,25.5815184751539,3.07386308807352));
#42288=CARTESIAN_POINT('Ctrl Pts',(-20.9485797025379,25.4532632360276,3.06432045148484));
#42289=CARTESIAN_POINT('Ctrl Pts',(-20.9115851026535,25.401626236491,3.06050921505357));
#42290=CARTESIAN_POINT('Ctrl Pts',(-20.8714560090935,25.3419660256991,3.05612641706771));
#42291=CARTESIAN_POINT('Ctrl Pts',(-20.8667973544679,25.3349811844064,3.05561361119816));
#42292=CARTESIAN_POINT('Ctrl Pts',(-20.8598383058753,25.3244584565067,3.05484151159028));
#42293=CARTESIAN_POINT('Ctrl Pts',(-20.857517454265,25.3209340876618,3.05458298789678));
#42294=CARTESIAN_POINT('Ctrl Pts',(-20.8535369766745,25.3148635412927,3.05413781855784));
#42295=CARTESIAN_POINT('Ctrl Pts',(-20.8518740140117,25.3123195494567,3.05395129838414));
#42296=CARTESIAN_POINT('Ctrl Pts',(-20.848455866772,25.3070742988103,3.0535668029335));
#42297=CARTESIAN_POINT('Ctrl Pts',(-20.8467011290866,25.3043727537227,3.05336881118368));
#42298=CARTESIAN_POINT('Ctrl Pts',(-20.8424851889798,25.2978606565605,3.05289164673333));
#42299=CARTESIAN_POINT('Ctrl Pts',(-20.8400279805272,25.2940475375058,3.052612325216));
#42300=CARTESIAN_POINT('Ctrl Pts',(-20.8325073753402,25.2823226980185,3.051753682763));
#42301=CARTESIAN_POINT('Ctrl Pts',(-20.8274705454366,25.2743940712053,3.05117337427904));
#42302=CARTESIAN_POINT('Ctrl Pts',(-20.8090347183839,25.2450914162827,3.04902978475394));
#42303=CARTESIAN_POINT('Ctrl Pts',(-20.7958524334708,25.2235827397628,3.04745852246808));
#42304=CARTESIAN_POINT('Ctrl Pts',(-20.7798318805004,25.19674072985,3.0454998808657));
#42305=CARTESIAN_POINT('Ctrl Pts',(-20.7767540293872,25.1915508068804,3.04512127903175));
#42306=CARTESIAN_POINT('Ctrl Pts',(-20.7702056904868,25.1804378737726,3.04431080894755));
#42307=CARTESIAN_POINT('Ctrl Pts',(-20.7667395209942,25.1745123652567,3.04387878760487));
#42308=CARTESIAN_POINT('Ctrl Pts',(-20.7625236947278,25.1672521720804,3.04334960651454));
#42309=CARTESIAN_POINT('Ctrl Pts',(-20.7617560017088,25.165927934648,3.0432530915796));
#42310=CARTESIAN_POINT('Ctrl Pts',(-20.7595646366385,25.1621417099947,3.04297715593653));
#42311=CARTESIAN_POINT('Ctrl Pts',(-20.7581432823337,25.1596783890376,3.0427976528693));
#42312=CARTESIAN_POINT('Ctrl Pts',(-20.7532891039878,25.1512399249171,3.04218280947059));
#42313=CARTESIAN_POINT('Ctrl Pts',(-20.7498722027233,25.1452556856467,3.04174690651847));
#42314=CARTESIAN_POINT('Ctrl Pts',(-20.7438546457933,25.1346378075357,3.04097368767491));
#42315=CARTESIAN_POINT('Ctrl Pts',(-20.741246198937,25.1300085945988,3.04063664683799));
#42316=CARTESIAN_POINT('Ctrl Pts',(-20.7366916515578,25.1218786890185,3.04004484873125));
#42317=CARTESIAN_POINT('Ctrl Pts',(-20.7347406011122,25.1183807704364,3.03979026414752));
#42318=CARTESIAN_POINT('Ctrl Pts',(-20.7306790806224,25.1110671044611,3.03925804211906));
#42319=CARTESIAN_POINT('Ctrl Pts',(-20.7285698251872,25.1072506948443,3.03898036350651));
#42320=CARTESIAN_POINT('Ctrl Pts',(-20.7165802888827,25.0854528879501,3.03739462723167));
#42321=CARTESIAN_POINT('Ctrl Pts',(-20.7068643288012,25.0673820617276,3.0360809957412));
#42322=CARTESIAN_POINT('Ctrl Pts',(-20.5571028786504,24.7823464917123,3.01537566723813));
#42323=CARTESIAN_POINT('Ctrl Pts',(-20.4550399136743,24.4971407629173,2.99465608499176));
#42324=CARTESIAN_POINT('Ctrl Pts',(-20.3764571954094,24.1165968855771,2.9686593208174));
#42325=CARTESIAN_POINT('Ctrl Pts',(-20.3622932004324,24.0305030390971,2.96289687013642));
#42326=CARTESIAN_POINT('Ctrl Pts',(-20.3484551062746,23.9180702671479,2.955608582127));
#42327=CARTESIAN_POINT('Ctrl Pts',(-20.3455855043574,23.8921677006739,2.95394576427495));
#42328=CARTESIAN_POINT('Ctrl Pts',(-20.3420781918439,23.8565681674941,2.95168534573581));
#42329=CARTESIAN_POINT('Ctrl Pts',(-20.3411697441133,23.8468996818152,2.95107395396739));
#42330=CARTESIAN_POINT('Ctrl Pts',(-20.3398872601461,23.8325544861959,2.9501707050421));
#42331=CARTESIAN_POINT('Ctrl Pts',(-20.3394797213011,23.8278809361704,2.9498770435787));
#42332=CARTESIAN_POINT('Ctrl Pts',(-20.3388470368081,23.8204377114764,2.94941033903733));
#42333=CARTESIAN_POINT('Ctrl Pts',(-20.3386152677574,23.8176686288011,2.94923693003962));
#42334=CARTESIAN_POINT('Ctrl Pts',(-20.3381868835839,23.8124695755081,2.94891176165231));
#42335=CARTESIAN_POINT('Ctrl Pts',(-20.3379894439835,23.8100396777581,2.94875995612464));
#42336=CARTESIAN_POINT('Ctrl Pts',(-20.3376456538787,23.8057483193702,2.94849215962291));
#42337=CARTESIAN_POINT('Ctrl Pts',(-20.3374981636527,23.8038869528748,2.94837610386146));
#42338=CARTESIAN_POINT('Ctrl Pts',(-20.337214412085,23.8002659697631,2.94815053279951));
#42339=CARTESIAN_POINT('Ctrl Pts',(-20.33707797875,23.7985063728052,2.94804100780829));
#42340=CARTESIAN_POINT('Ctrl Pts',(-20.336757855954,23.7943332363309,2.94778146521344));
#42341=CARTESIAN_POINT('Ctrl Pts',(-20.3365754397179,23.7919195960264,2.94763151995224));
#42342=CARTESIAN_POINT('Ctrl Pts',(-20.3359446471403,23.7834462426487,2.94710570236284));
#42343=CARTESIAN_POINT('Ctrl Pts',(-20.3355106857597,23.7773854200154,2.94673064004958));
#42344=CARTESIAN_POINT('Ctrl Pts',(-20.3302010473401,23.7001643273391,2.94196485483842));
#42345=CARTESIAN_POINT('Ctrl Pts',(-20.3276715073951,23.6288559289507,2.93770334010832));
#42346=CARTESIAN_POINT('Ctrl Pts',(-20.3269424239474,23.3053742697196,2.91876680886396));
#42347=CARTESIAN_POINT('Ctrl Pts',(-20.3559658256038,23.0540158032507,2.90508084240943));
#42348=CARTESIAN_POINT('Ctrl Pts',(-20.4557113981276,22.6322227833925,2.88057621796159));
#42349=CARTESIAN_POINT('Ctrl Pts',(-20.5122153191156,22.4597119715439,2.87009053832727));
#42350=CARTESIAN_POINT('Ctrl Pts',(-20.5881425499942,22.2805273881455,2.85826920850269));
#42351=CARTESIAN_POINT('Ctrl Pts',(-20.5934528877796,22.2682098876806,2.85745182678728));
#42352=CARTESIAN_POINT('Ctrl Pts',(-20.6008907775414,22.2512494979094,2.85631963439452));
#42353=CARTESIAN_POINT('Ctrl Pts',(-20.6029527538395,22.2465778569291,2.85600707222182));
#42354=CARTESIAN_POINT('Ctrl Pts',(-20.6064489628958,22.2387074887493,2.85547929505755));
#42355=CARTESIAN_POINT('Ctrl Pts',(-20.6078773322964,22.2355061541909,2.85526428183323));
#42356=CARTESIAN_POINT('Ctrl Pts',(-20.6107114011699,22.2291820444765,2.85483886488087));
#42357=CARTESIAN_POINT('Ctrl Pts',(-20.6121168606885,22.2260591663374,2.85462846963384));
#42358=CARTESIAN_POINT('Ctrl Pts',(-20.6152221630272,22.2191885842099,2.85416487070892));
#42359=CARTESIAN_POINT('Ctrl Pts',(-20.6169242101374,22.2154418878204,2.8539115912183));
#42360=CARTESIAN_POINT('Ctrl Pts',(-20.6228760376224,22.2024065598085,2.85302875609248));
#42361=CARTESIAN_POINT('Ctrl Pts',(-20.6271627655735,22.1931349548728,2.85239792463933));
#42362=CARTESIAN_POINT('Ctrl Pts',(-20.6423101124016,22.1607780511513,2.85018612422393));
#42363=CARTESIAN_POINT('Ctrl Pts',(-20.6534004946194,22.1378019446303,2.84859719965345));
#42364=CARTESIAN_POINT('Ctrl Pts',(-20.6674548415714,22.1095472902474,2.84661994454605));
#42365=CARTESIAN_POINT('Ctrl Pts',(-20.6701626528781,22.104141746157,2.84624060257306));
#42366=CARTESIAN_POINT('Ctrl Pts',(-20.6759740957533,22.0926215576172,2.84542987653227));
#42367=CARTESIAN_POINT('Ctrl Pts',(-20.6790820603179,22.0865091433128,2.84499834296387));
#42368=CARTESIAN_POINT('Ctrl Pts',(-20.6827674864684,22.0793179394242,2.84448901733501));
#42369=CARTESIAN_POINT('Ctrl Pts',(-20.6833261023039,22.0782294653711,2.84441188075273));
#42370=CARTESIAN_POINT('Ctrl Pts',(-20.6853245553638,22.0743408925264,2.84413615262193));
#42371=CARTESIAN_POINT('Ctrl Pts',(-20.6867678726063,22.0715425928465,2.84393744035542));
#42372=CARTESIAN_POINT('Ctrl Pts',(-20.6913805207197,22.0626316807603,2.84330372661108));
#42373=CARTESIAN_POINT('Ctrl Pts',(-20.6945653254068,22.0565271386129,2.84286818975382));
#42374=CARTESIAN_POINT('Ctrl Pts',(-20.7002716026716,22.0456744615713,2.84209138237212));
#42375=CARTESIAN_POINT('Ctrl Pts',(-20.7027854471277,22.0409223270538,2.84175037633165));
#42376=CARTESIAN_POINT('Ctrl Pts',(-20.7071924493217,22.0326415915818,2.84115465782254));
#42377=CARTESIAN_POINT('Ctrl Pts',(-20.7090803201243,22.0291101775728,2.8409001275841));
#42378=CARTESIAN_POINT('Ctrl Pts',(-20.7130649832219,22.0216898415878,2.84036428920416));
#42379=CARTESIAN_POINT('Ctrl Pts',(-20.7151631993905,22.0178016971348,2.84008293270806));
#42380=CARTESIAN_POINT('Ctrl Pts',(-20.7260501142702,21.9977263531866,2.83862719602005));
#42381=CARTESIAN_POINT('Ctrl Pts',(-20.7349693362382,21.9816106551079,2.83744838088159));
#42382=CARTESIAN_POINT('Ctrl Pts',(-20.772053045677,21.9159410636299,2.83260278937207));
#42383=CARTESIAN_POINT('Ctrl Pts',(-20.8013903677834,21.8670643195113,2.82889720740297));
#42384=CARTESIAN_POINT('Ctrl Pts',(-20.9688285275158,21.6041700932044,2.80842519191634));
#42385=CARTESIAN_POINT('Ctrl Pts',(-21.1306312700497,21.4063318484599,2.79091448301039));
#42386=CARTESIAN_POINT('Ctrl Pts',(-21.3454192871674,21.1993522303183,2.77100760994721));
#42387=CARTESIAN_POINT('Ctrl Pts',(-21.3774550961832,21.1697119523398,2.76811511240939));
#42388=CARTESIAN_POINT('Ctrl Pts',(-21.4593947981516,21.0969320596152,2.76092537542677));
#42389=CARTESIAN_POINT('Ctrl Pts',(-21.5100426272231,21.0546539250662,2.75666744327902));
#42390=CARTESIAN_POINT('Ctrl Pts',(-21.5675703144586,21.0095558413595,2.75206513374346));
#42391=CARTESIAN_POINT('Ctrl Pts',(-21.5731988809698,21.0051734933854,2.7516172509516));
#42392=CARTESIAN_POINT('Ctrl Pts',(-21.581804403983,20.9985190906363,2.75093621106533));
#42393=CARTESIAN_POINT('Ctrl Pts',(-21.5847708022651,20.9962335111466,2.75070212281107));
#42394=CARTESIAN_POINT('Ctrl Pts',(-21.5896329553253,20.9925007596707,2.75031954237935));
#42395=CARTESIAN_POINT('Ctrl Pts',(-21.5915263342834,20.9910505204816,2.75017083531332));
#42396=CARTESIAN_POINT('Ctrl Pts',(-21.5951799212701,20.9882584744809,2.74988441159942));
#42397=CARTESIAN_POINT('Ctrl Pts',(-21.5969399042142,20.9869163772609,2.74974667440132));
#42398=CARTESIAN_POINT('Ctrl Pts',(-21.6001554895538,20.9844695268482,2.7494954555577));
#42399=CARTESIAN_POINT('Ctrl Pts',(-21.6016106433871,20.9833642028217,2.74938193340587));
#42400=CARTESIAN_POINT('Ctrl Pts',(-21.6045788672066,20.9811135407211,2.74915070150007));
#42401=CARTESIAN_POINT('Ctrl Pts',(-21.6060920029518,20.9799683057487,2.74903299910886));
#42402=CARTESIAN_POINT('Ctrl Pts',(-21.610444454988,20.9766801426103,2.74869493333451));
#42403=CARTESIAN_POINT('Ctrl Pts',(-21.6132863203137,20.9745405694263,2.74847480779296));
#42404=CARTESIAN_POINT('Ctrl Pts',(-21.6257274864736,20.9652061443529,2.74751377052465));
#42405=CARTESIAN_POINT('Ctrl Pts',(-21.6353635367135,20.9580600963296,2.74677625640235));
#42406=CARTESIAN_POINT('Ctrl Pts',(-21.7999902990395,20.8373926414277,2.73428785024807));
#42407=CARTESIAN_POINT('Ctrl Pts',(-21.9648133467986,20.737881099687,2.72344874089343));
#42408=CARTESIAN_POINT('Ctrl Pts',(-22.2785489645164,20.5848690740442,2.70390723880978));
#42409=CARTESIAN_POINT('Ctrl Pts',(-22.4243848025181,20.5264884993281,2.69520320136931));
#42410=CARTESIAN_POINT('Ctrl Pts',(-22.7048443569871,20.4373301474084,2.6784045860549));
#42411=CARTESIAN_POINT('Ctrl Pts',(-22.8383155569215,20.4041216671813,2.67038723780692));
#42412=CARTESIAN_POINT('Ctrl Pts',(-22.9947874137189,20.3756588959988,2.66077397949195));
#42413=CARTESIAN_POINT('Ctrl Pts',(-23.0161251445854,20.371999214558,2.65945871810378));
#42414=CARTESIAN_POINT('Ctrl Pts',(-23.0435465004669,20.3675800543144,2.65776242504027));
#42415=CARTESIAN_POINT('Ctrl Pts',(-23.0495980038037,20.3666225055705,2.65738770149755));
#42416=CARTESIAN_POINT('Ctrl Pts',(-23.0593372100511,20.365109894924,2.65678400972904));
#42417=CARTESIAN_POINT('Ctrl Pts',(-23.0630232303135,20.3645439641561,2.65655538709327));
#42418=CARTESIAN_POINT('Ctrl Pts',(-23.070034684972,20.3634799183996,2.65612023372526));
#42419=CARTESIAN_POINT('Ctrl Pts',(-23.07335993512,20.3629806072498,2.65591374127966));
#42420=CARTESIAN_POINT('Ctrl Pts',(-23.0809274023555,20.3618564031667,2.65544354598459));
#42421=CARTESIAN_POINT('Ctrl Pts',(-23.0851700909536,20.3612347718708,2.65517974000688));
#42422=CARTESIAN_POINT('Ctrl Pts',(-23.0980564192259,20.3593729524745,2.65437789225759));
#42423=CARTESIAN_POINT('Ctrl Pts',(-23.1067038173636,20.3581594332991,2.65383900598652));
#42424=CARTESIAN_POINT('Ctrl Pts',(-23.1678064614015,20.3498377700616,2.6500254162419));
#42425=CARTESIAN_POINT('Ctrl Pts',(-23.2204222695272,20.3439881784692,2.64671108664128));
#42426=CARTESIAN_POINT('Ctrl Pts',(-23.2769420682005,20.3391104614585,2.64311542582022));
#42427=CARTESIAN_POINT('Ctrl Pts',(-23.2807288452817,20.338790405659,2.642874350809));
#42428=CARTESIAN_POINT('Ctrl Pts',(-23.2885442600985,20.3381437726874,2.64237645388914));
#42429=CARTESIAN_POINT('Ctrl Pts',(-23.2925729622165,20.3378180750325,2.64211960566326));
#42430=CARTESIAN_POINT('Ctrl Pts',(-23.3020705349442,20.3370682314249,2.64151363919007));
#42431=CARTESIAN_POINT('Ctrl Pts',(-23.3075398844313,20.3366504683894,2.64116432873499));
#42432=CARTESIAN_POINT('Ctrl Pts',(-23.3338180169029,20.3347107444266,2.63948432190373));
#42433=CARTESIAN_POINT('Ctrl Pts',(-23.3546398202615,20.3333769481231,2.63814801259008));
#42434=CARTESIAN_POINT('Ctrl Pts',(-23.6327443200828,20.3182722428812,2.62023095267543));
#42435=CARTESIAN_POINT('Ctrl Pts',(-23.8907314595865,20.3352043635715,2.60271318911965));
#42436=CARTESIAN_POINT('Ctrl Pts',(-24.3019792165563,20.412276625361,2.5744736292064));
#42437=CARTESIAN_POINT('Ctrl Pts',(-24.4576458760638,20.4537001016352,2.5637382030774));
#42438=CARTESIAN_POINT('Ctrl Pts',(-24.6162766012742,20.5089106498502,2.55316376842186));
#42439=CARTESIAN_POINT('Ctrl Pts',(-24.6229602475664,20.5112615942764,2.55271894661977));
#42440=CARTESIAN_POINT('Ctrl Pts',(-24.6331472774998,20.5148826337123,2.55204211241467));
#42441=CARTESIAN_POINT('Ctrl Pts',(-24.6366562486586,20.5161367771185,2.55180918252031));
#42442=CARTESIAN_POINT('Ctrl Pts',(-24.6424002090563,20.5182009713589,2.55142824286814));
#42443=CARTESIAN_POINT('Ctrl Pts',(-24.6446364789671,20.5190074096796,2.55128002079108));
#42444=CARTESIAN_POINT('Ctrl Pts',(-24.6489477360105,20.520567517695,2.55099443812415));
#42445=CARTESIAN_POINT('Ctrl Pts',(-24.6510228439927,20.5213208461536,2.55085705728554));
#42446=CARTESIAN_POINT('Ctrl Pts',(-24.6548418817534,20.5227117181044,2.55060436447167));
#42447=CARTESIAN_POINT('Ctrl Pts',(-24.6565860273068,20.5233486338562,2.5504890155984));
#42448=CARTESIAN_POINT('Ctrl Pts',(-24.6601233928109,20.5246438519276,2.55025518457493));
#42449=CARTESIAN_POINT('Ctrl Pts',(-24.6619165708145,20.5253022386135,2.55013670819908));
#42450=CARTESIAN_POINT('Ctrl Pts',(-24.667105904519,20.5272128019058,2.54979401178729));
#42451=CARTESIAN_POINT('Ctrl Pts',(-24.6705005513344,20.5284691114162,2.54957004005036));
#42452=CARTESIAN_POINT('Ctrl Pts',(-24.6856534748635,20.5341060321116,2.54857117202522));
#42453=CARTESIAN_POINT('Ctrl Pts',(-24.6973884324667,20.53854965026,2.54780001037813));
#42454=CARTESIAN_POINT('Ctrl Pts',(-24.9003443661025,20.6167603306567,2.53449948607699));
#42455=CARTESIAN_POINT('Ctrl Pts',(-25.0841584152696,20.7085479419708,2.52300387903064));
#42456=CARTESIAN_POINT('Ctrl Pts',(-25.3229680226129,20.8577702272276,2.50725855860012));
#42457=CARTESIAN_POINT('Ctrl Pts',(-25.3864398157547,20.9006492952285,2.50298891462022));
#42458=CARTESIAN_POINT('Ctrl Pts',(-25.5144690768732,20.9939525042213,2.49409473620066));
#42459=CARTESIAN_POINT('Ctrl Pts',(-25.5787518894796,21.044657606144,2.48946914396926));
#42460=CARTESIAN_POINT('Ctrl Pts',(-25.7448850891645,21.1862878022225,2.47694431740816));
#42461=CARTESIAN_POINT('Ctrl Pts',(-25.8429963801582,21.2813189440096,2.468928168689));
#42462=CARTESIAN_POINT('Ctrl Pts',(-25.9419952961084,21.3902064499884,2.45997273913193));
#42463=CARTESIAN_POINT('Ctrl Pts',(-25.9491684741101,21.398175668969,2.45931860369201));
#42464=CARTESIAN_POINT('Ctrl Pts',(-25.9594046206718,21.4096625364474,2.45837751119456));
#42465=CARTESIAN_POINT('Ctrl Pts',(-25.9624999830549,21.4131513294537,2.45809191633621));
#42466=CARTESIAN_POINT('Ctrl Pts',(-25.9678515834599,21.4192095757467,2.45759638307381));
#42467=CARTESIAN_POINT('Ctrl Pts',(-25.9701113314562,21.4217759299293,2.45738659197696));
#42468=CARTESIAN_POINT('Ctrl Pts',(-25.9744434021122,21.4267115986118,2.45698335137484));
#42469=CARTESIAN_POINT('Ctrl Pts',(-25.9765163475088,21.4290803636121,2.4567899281768));
#42470=CARTESIAN_POINT('Ctrl Pts',(-25.9813837750523,21.4346588675747,2.45633465160916));
#42471=CARTESIAN_POINT('Ctrl Pts',(-25.9841753716075,21.4378711070522,2.45607267859472));
#42472=CARTESIAN_POINT('Ctrl Pts',(-25.9937667756515,21.4489520163954,2.45516961196423));
#42473=CARTESIAN_POINT('Ctrl Pts',(-26.0005347983614,21.4568480018427,2.45452720404576));
#42474=CARTESIAN_POINT('Ctrl Pts',(-26.0770143390037,21.546952678605,2.44720843883806));
#42475=CARTESIAN_POINT('Ctrl Pts',(-26.142590106918,21.6325672188292,2.44036418546625));
#42476=CARTESIAN_POINT('Ctrl Pts',(-26.3646992842135,21.9548091315217,2.41494661787555));
#42477=CARTESIAN_POINT('Ctrl Pts',(-26.494109373313,22.2085321106504,2.39543037561156));
#42478=CARTESIAN_POINT('Ctrl Pts',(-26.6102744240062,22.5370411598884,2.37216360277266));
#42479=CARTESIAN_POINT('Ctrl Pts',(-26.6300627015075,22.5988842638521,2.3678722440661));
#42480=CARTESIAN_POINT('Ctrl Pts',(-26.6586447740323,22.6984821949141,2.36114326187468));
#42481=CARTESIAN_POINT('Ctrl Pts',(-26.6686488016687,22.7358692992355,2.35865760711562));
#42482=CARTESIAN_POINT('Ctrl Pts',(-26.6821667513215,22.7902966523856,2.35510594295059));
#42483=CARTESIAN_POINT('Ctrl Pts',(-26.686219624897,22.8071979978633,2.35401231520406));
#42484=CARTESIAN_POINT('Ctrl Pts',(-26.6910058652513,22.8278946034136,2.35268511644715));
#42485=CARTESIAN_POINT('Ctrl Pts',(-26.6918692932622,22.8316590425732,2.3524442007248));
#42486=CARTESIAN_POINT('Ctrl Pts',(-26.6932085887111,22.8375467573781,2.35206816665482));
#42487=CARTESIAN_POINT('Ctrl Pts',(-26.6936890728281,22.8396689623556,2.35193278213363));
#42488=CARTESIAN_POINT('Ctrl Pts',(-26.6945360554288,22.8434275908204,2.35169328056941));
#42489=CARTESIAN_POINT('Ctrl Pts',(-26.6949034239572,22.8450638048369,2.35158911343179));
#42490=CARTESIAN_POINT('Ctrl Pts',(-26.695687185334,22.848567372579,2.35136626319743));
#42491=CARTESIAN_POINT('Ctrl Pts',(-26.6961031913151,22.8504348052461,2.35124760295276));
#42492=CARTESIAN_POINT('Ctrl Pts',(-26.6973046546765,22.8558508415949,2.35090380523861));
#42493=CARTESIAN_POINT('Ctrl Pts',(-26.6980857756069,22.8594004195836,2.3506789185853));
#42494=CARTESIAN_POINT('Ctrl Pts',(-26.7015655249497,22.8753415642943,2.34967086322423));
#42495=CARTESIAN_POINT('Ctrl Pts',(-26.7041970484542,22.8877478953697,2.348891513586));
#42496=CARTESIAN_POINT('Ctrl Pts',(-26.7505982872837,23.1130509302846,2.33482674281852));
#42497=CARTESIAN_POINT('Ctrl Pts',(-26.7728007868959,23.3298597703338,2.32270222717392));
#42498=CARTESIAN_POINT('Ctrl Pts',(-26.7732534614922,23.8210445038373,2.29525433934036));
#42499=CARTESIAN_POINT('Ctrl Pts',(-26.7386261652086,24.0936773121162,2.27994883779347));
#42500=CARTESIAN_POINT('Ctrl Pts',(-26.6656921857838,24.3751427893889,2.26233004103553));
#42501=CARTESIAN_POINT('Ctrl Pts',(-26.6612852519656,24.3916107024465,2.26129289263315));
#42502=CARTESIAN_POINT('Ctrl Pts',(-26.6551987142132,24.4136531595913,2.25989592550752));
#42503=CARTESIAN_POINT('Ctrl Pts',(-26.6536343028905,24.4192594488681,2.25953985970554));
#42504=CARTESIAN_POINT('Ctrl Pts',(-26.6511605977192,24.4280324490498,2.25898146788909));
#42505=CARTESIAN_POINT('Ctrl Pts',(-26.6502616153487,24.4312020753012,2.25877947848115));
#42506=CARTESIAN_POINT('Ctrl Pts',(-26.6485295020142,24.4372736662859,2.25839208260559));
#42507=CARTESIAN_POINT('Ctrl Pts',(-26.6476971499433,24.4401758513172,2.25820670174519));
#42508=CARTESIAN_POINT('Ctrl Pts',(-26.6457367888559,24.4469750278694,2.25777190598687));
#42509=CARTESIAN_POINT('Ctrl Pts',(-26.6446054989195,24.4508710610771,2.25752238405177));
#42510=CARTESIAN_POINT('Ctrl Pts',(-26.6413292021852,24.4620752059601,2.25680372128216));
#42511=CARTESIAN_POINT('Ctrl Pts',(-26.6391656517284,24.4693778264411,2.25633397405694));
#42512=CARTESIAN_POINT('Ctrl Pts',(-26.6246364512801,24.5177874262614,2.25321101179727));
#42513=CARTESIAN_POINT('Ctrl Pts',(-26.6114769339192,24.5586498387803,2.25053183787184));
#42514=CARTESIAN_POINT('Ctrl Pts',(-26.57079659377,24.6768245622434,2.242652689255));
#42515=CARTESIAN_POINT('Ctrl Pts',(-26.5411360292892,24.7533589089354,2.23738351289304));
#42516=CARTESIAN_POINT('Ctrl Pts',(-26.3901212993046,25.1028155001723,2.2125409862792));
#42517=CARTESIAN_POINT('Ctrl Pts',(-26.2341490767717,25.3591093719883,2.19187166848193));
#42518=CARTESIAN_POINT('Ctrl Pts',(-25.9886019742628,25.6594112886723,2.16622098097852));
#42519=CARTESIAN_POINT('Ctrl Pts',(-25.9291939559346,25.7261982629153,2.16042209515106));
#42520=CARTESIAN_POINT('Ctrl Pts',(-25.8626303357909,25.7950392583061,2.15441903218325));
#42521=CARTESIAN_POINT('Ctrl Pts',(-25.8581659784763,25.7996289076443,2.15401868144554));
#42522=CARTESIAN_POINT('Ctrl Pts',(-25.8519562591376,25.8059749534546,2.15346498815783));
#42523=CARTESIAN_POINT('Ctrl Pts',(-25.8502225448128,25.8077426494613,2.15331074199663));
#42524=CARTESIAN_POINT('Ctrl Pts',(-25.8472393155269,25.8107773477347,2.15304591733451));
#42525=CARTESIAN_POINT('Ctrl Pts',(-25.8459907886789,25.8120453127617,2.15293526102146));
#42526=CARTESIAN_POINT('Ctrl Pts',(-25.8434097779198,25.814662168129,2.15270687355758));
#42527=CARTESIAN_POINT('Ctrl Pts',(-25.8420771563221,25.8160109141038,2.15258915440102));
#42528=CARTESIAN_POINT('Ctrl Pts',(-25.8389459727108,25.8191743954021,2.15231302680414));
#42529=CARTESIAN_POINT('Ctrl Pts',(-25.8371464367368,25.8209881741131,2.15215469568438));
#42530=CARTESIAN_POINT('Ctrl Pts',(-25.8312965912847,25.8268703118931,2.15164117102741));
#42531=CARTESIAN_POINT('Ctrl Pts',(-25.8272375383268,25.830930018689,2.15128666772739));
#42532=CARTESIAN_POINT('Ctrl Pts',(-25.7129072489442,25.944669258645,2.14135163191842));
#42533=CARTESIAN_POINT('Ctrl Pts',(-25.5948330493108,26.0462517874045,2.1323948248655));
#42534=CARTESIAN_POINT('Ctrl Pts',(-25.1958131932324,26.3421429410736,2.10434042053071));
#42535=CARTESIAN_POINT('Ctrl Pts',(-24.8912647174764,26.5005408384653,2.08581638661141));
#42536=CARTESIAN_POINT('Ctrl Pts',(-24.5484308419812,26.6145898302528,2.0639632193382));
#42537=CARTESIAN_POINT('Ctrl Pts',(-24.5292655875258,26.6207665646138,2.06273954923233));
#42538=CARTESIAN_POINT('Ctrl Pts',(-24.5042221416756,26.6285794700039,2.06113752925753));
#42539=CARTESIAN_POINT('Ctrl Pts',(-24.4983951302862,26.6303792121765,2.06076456463829));
#42540=CARTESIAN_POINT('Ctrl Pts',(-24.4889468617728,26.6332680711803,2.06015946016757));
#42541=CARTESIAN_POINT('Ctrl Pts',(-24.4853287156753,26.6343673791005,2.05992765512354));
#42542=CARTESIAN_POINT('Ctrl Pts',(-24.4785627257672,26.6364101013998,2.05949401460952));
#42543=CARTESIAN_POINT('Ctrl Pts',(-24.4754153546328,26.6373550749208,2.05929223056917));
#42544=CARTESIAN_POINT('Ctrl Pts',(-24.4683586880135,26.6394620229787,2.05883966549198));
#42545=CARTESIAN_POINT('Ctrl Pts',(-24.464448626224,26.6406213924964,2.05858879951207));
#42546=CARTESIAN_POINT('Ctrl Pts',(-24.4562988952391,26.643021042711,2.05806570348264));
#42547=CARTESIAN_POINT('Ctrl Pts',(-24.4520588580831,26.6442600341097,2.05779343180275));
#42548=CARTESIAN_POINT('Ctrl Pts',(-24.4282001298325,26.6511786399603,2.05626065677074));
#42549=CARTESIAN_POINT('Ctrl Pts',(-24.4085306985775,26.6566802664613,2.05499435502827));
#42550=CARTESIAN_POINT('Ctrl Pts',(-24.2683381170094,26.6944596297551,2.04594847663681));
#42551=CARTESIAN_POINT('Ctrl Pts',(-24.1460970596423,26.7198972584676,2.03794781628291));
#42552=CARTESIAN_POINT('Ctrl Pts',(-23.7584308323266,26.7773491101399,2.01221413652531));
#42553=CARTESIAN_POINT('Ctrl Pts',(-23.490355410405,26.7834980069056,1.99380334718602));
#42554=CARTESIAN_POINT('Ctrl Pts',(-23.1219914034802,26.7460857879164,1.9691883103969));
#42555=CARTESIAN_POINT('Ctrl Pts',(-23.0199146007114,26.7307406257783,1.96245715112733));
#42556=CARTESIAN_POINT('Ctrl Pts',(-22.9122619789182,26.7092285118608,1.95557347708528));
#42557=CARTESIAN_POINT('Ctrl Pts',(-22.9057889457377,26.707914305362,1.95516041127388));
#42558=CARTESIAN_POINT('Ctrl Pts',(-22.8968629029976,26.7060734786679,1.95459201663484));
#42559=CARTESIAN_POINT('Ctrl Pts',(-22.8944064573934,26.705563892428,1.95443572067168));
#42560=CARTESIAN_POINT('Ctrl Pts',(-22.8902000522618,26.7046861551426,1.95416829934899));
#42561=CARTESIAN_POINT('Ctrl Pts',(-22.8884498046289,26.7043194160248,1.9540570927335));
#42562=CARTESIAN_POINT('Ctrl Pts',(-22.8850344366407,26.7036008069297,1.95384021641975));
#42563=CARTESIAN_POINT('Ctrl Pts',(-22.8833692941746,26.7032490756889,1.95373453929666));
#42564=CARTESIAN_POINT('Ctrl Pts',(-22.8793409989754,26.7023948372931,1.95347902931546));
#42565=CARTESIAN_POINT('Ctrl Pts',(-22.8769781258753,26.7018909903443,1.95332927410928));
#42566=CARTESIAN_POINT('Ctrl Pts',(-22.8697184968119,26.7003344474774,1.95286952979833));
#42567=CARTESIAN_POINT('Ctrl Pts',(-22.8648235966829,26.6992729864752,1.95256004424274));
#42568=CARTESIAN_POINT('Ctrl Pts',(-22.8120841605379,26.6877076222422,1.94923076499973));
#42569=CARTESIAN_POINT('Ctrl Pts',(-22.7644793674854,26.6761249169372,1.9462720446646));
#42570=CARTESIAN_POINT('Ctrl Pts',(-22.6281962274381,26.6396553728339,1.93788756972047));
#42571=CARTESIAN_POINT('Ctrl Pts',(-22.5402923338682,26.6120462565927,1.93258479790501));
#42572=CARTESIAN_POINT('Ctrl Pts',(-22.3238522786132,26.5337276475404,1.9195241354689));
#42573=CARTESIAN_POINT('Ctrl Pts',(-22.1973892682305,26.478531424086,1.91188432929591));
#42574=CARTESIAN_POINT('Ctrl Pts',(-22.075035775028,26.4155366508264,1.90417269213721));
#42575=CARTESIAN_POINT('',(-26.7730025245988,23.5504663859432,2.06117200133249));
#42576=CARTESIAN_POINT('Ctrl Pts',(-22.0750360931093,26.4155368145933,1.65435918102699));
#42577=CARTESIAN_POINT('Ctrl Pts',(-22.1241974666802,26.4408479737227,1.65763718003993));
#42578=CARTESIAN_POINT('Ctrl Pts',(-22.1740119429965,26.4648947751088,1.66095646117125));
#42579=CARTESIAN_POINT('Ctrl Pts',(-22.2344161870542,26.492158765002,1.66498807657907));
#42580=CARTESIAN_POINT('Ctrl Pts',(-22.2444238915245,26.496614547692,1.66565623777394));
#42581=CARTESIAN_POINT('Ctrl Pts',(-22.2584387265136,26.5027690168378,1.6665922895853));
#42582=CARTESIAN_POINT('Ctrl Pts',(-22.2624269541482,26.504510777653,1.66685870364032));
#42583=CARTESIAN_POINT('Ctrl Pts',(-22.2693286116832,26.5075082762307,1.66731980910595));
#42584=CARTESIAN_POINT('Ctrl Pts',(-22.2722403979568,26.5087678034753,1.66751437067434));
#42585=CARTESIAN_POINT('Ctrl Pts',(-22.2782162902034,26.5113422771571,1.66791372027616));
#42586=CARTESIAN_POINT('Ctrl Pts',(-22.2812805852638,26.5126567713944,1.66811852342681));
#42587=CARTESIAN_POINT('Ctrl Pts',(-22.2884222877264,26.5157072416525,1.66859590509598));
#42588=CARTESIAN_POINT('Ctrl Pts',(-22.2925012394358,26.5174395645444,1.66886860778774));
#42589=CARTESIAN_POINT('Ctrl Pts',(-22.301098561572,26.5210699174754,1.66944349805045));
#42590=CARTESIAN_POINT('Ctrl Pts',(-22.3056177108143,26.5229660636309,1.66974574903111));
#42591=CARTESIAN_POINT('Ctrl Pts',(-22.3177014361431,26.5280037724304,1.67055411087161));
#42592=CARTESIAN_POINT('Ctrl Pts',(-22.3252736566569,26.5311268008594,1.67106085044095));
#42593=CARTESIAN_POINT('Ctrl Pts',(-22.3483201160454,26.5405292603721,1.67260373809438));
#42594=CARTESIAN_POINT('Ctrl Pts',(-22.3638311462971,26.5467172361735,1.67364297168359));
#42595=CARTESIAN_POINT('Ctrl Pts',(-22.6621442879888,26.6630470226429,1.69364751729217));
#42596=CARTESIAN_POINT('Ctrl Pts',(-22.9589992207896,26.7327923065176,1.71407786648253));
#42597=CARTESIAN_POINT('Ctrl Pts',(-23.3942292599906,26.7719964756639,1.74363247458185));
#42598=CARTESIAN_POINT('Ctrl Pts',(-23.5279586530674,26.775696060919,1.75262497783683));
#42599=CARTESIAN_POINT('Ctrl Pts',(-23.6669601883247,26.7708931967524,1.76165985002547));
#42600=CARTESIAN_POINT('Ctrl Pts',(-23.6723794263449,26.770692252122,1.76201158805565));
#42601=CARTESIAN_POINT('Ctrl Pts',(-23.6804115566134,26.7703741181029,1.76253214624319));
#42602=CARTESIAN_POINT('Ctrl Pts',(-23.6830248283657,26.7702674261237,1.76270139006518));
#42603=CARTESIAN_POINT('Ctrl Pts',(-23.731459746752,26.7682309117269,1.76583591361869));
#42604=CARTESIAN_POINT('Ctrl Pts',(-23.7772381995104,26.7653262414096,1.76876080400806));
#42605=CARTESIAN_POINT('Ctrl Pts',(-23.8279069428879,26.7610235325598,1.77194488731095));
#42606=CARTESIAN_POINT('Ctrl Pts',(-23.8328710546547,26.7605903898216,1.77225626951248));
#42607=CARTESIAN_POINT('Ctrl Pts',(-23.8402877999746,26.7599259067,1.77272062742192));
#42608=CARTESIAN_POINT('Ctrl Pts',(-23.8427411758737,26.7597032672864,1.77287408950548));
#42609=CARTESIAN_POINT('Ctrl Pts',(-23.8469630611093,26.7593152576567,1.77313792658219));
#42610=CARTESIAN_POINT('Ctrl Pts',(-23.8487316885717,26.759151238474,1.77324837807625));
#42611=CARTESIAN_POINT('Ctrl Pts',(-23.8523901103427,26.7588089125549,1.77347669187531));
#42612=CARTESIAN_POINT('Ctrl Pts',(-23.8542798794187,26.7586303986923,1.77359454168288));
#42613=CARTESIAN_POINT('Ctrl Pts',(-23.8587252459414,26.7582065117766,1.77387156244463));
#42614=CARTESIAN_POINT('Ctrl Pts',(-23.8612807168373,26.7579597536704,1.77403065463605));
#42615=CARTESIAN_POINT('Ctrl Pts',(-23.8696165116455,26.7571447883298,1.7745491015065));
#42616=CARTESIAN_POINT('Ctrl Pts',(-23.8753956374863,26.7565640042997,1.77490774736355));
#42617=CARTESIAN_POINT('Ctrl Pts',(-24.0170057242009,26.7419458284085,1.78367726898743));
#42618=CARTESIAN_POINT('Ctrl Pts',(-24.1518300673804,26.7193028259447,1.79160809727196));
#42619=CARTESIAN_POINT('Ctrl Pts',(-24.4249212635529,26.6553731242429,1.80754090308574));
#42620=CARTESIAN_POINT('Ctrl Pts',(-24.5626648529085,26.6132319637872,1.81550940469176));
#42621=CARTESIAN_POINT('Ctrl Pts',(-24.7756361188824,26.5321325997473,1.82828423502202));
#42622=CARTESIAN_POINT('Ctrl Pts',(-24.8529363527473,26.4991824495921,1.8330196508188));
#42623=CARTESIAN_POINT('Ctrl Pts',(-25.0585656244851,26.4018663209937,1.84603619954275));
#42624=CARTESIAN_POINT('Ctrl Pts',(-25.1840114563436,26.331894678704,1.85444484685241));
#42625=CARTESIAN_POINT('Ctrl Pts',(-25.3136736328019,26.2477674305825,1.86384665853346));
#42626=CARTESIAN_POINT('Ctrl Pts',(-25.32294789353,26.241681846919,1.86452318141433));
#42627=CARTESIAN_POINT('Ctrl Pts',(-25.3358361859438,26.2331292937447,1.86546906327035));
#42628=CARTESIAN_POINT('Ctrl Pts',(-25.3394769656996,26.230702611648,1.86573690429099));
#42629=CARTESIAN_POINT('Ctrl Pts',(-25.3457541422362,26.2265002094717,1.86619981055906));
#42630=CARTESIAN_POINT('Ctrl Pts',(-25.3483928815189,26.2247279846553,1.86639474354621));
#42631=CARTESIAN_POINT('Ctrl Pts',(-25.3537912016489,26.2210907750093,1.8667942374115));
#42632=CARTESIAN_POINT('Ctrl Pts',(-25.356550520749,26.2192254110213,1.86699881248299));
#42633=CARTESIAN_POINT('Ctrl Pts',(-25.3629565549927,26.2148802982208,1.86747463172042));
#42634=CARTESIAN_POINT('Ctrl Pts',(-25.3666010753379,26.2123973395365,1.8677459976233));
#42635=CARTESIAN_POINT('Ctrl Pts',(-25.3742601441406,26.2071562777888,1.86831768356301));
#42636=CARTESIAN_POINT('Ctrl Pts',(-25.3782735561099,26.2043965406264,1.86861806550848));
#42637=CARTESIAN_POINT('Ctrl Pts',(-25.3889596977429,26.1970127074049,1.86942004781553));
#42638=CARTESIAN_POINT('Ctrl Pts',(-25.3956212047192,26.192372500372,1.86992226389777));
#42639=CARTESIAN_POINT('Ctrl Pts',(-25.415767928832,26.178225532919,1.87144810905059));
#42640=CARTESIAN_POINT('Ctrl Pts',(-25.4291975776097,26.1686404499018,1.87247474411924));
#42641=CARTESIAN_POINT('Ctrl Pts',(-25.5914775779532,26.0509257026233,1.88499782295571));
#42642=CARTESIAN_POINT('Ctrl Pts',(-25.7308522741064,25.9303638848626,1.89699277666627));
#42643=CARTESIAN_POINT('Ctrl Pts',(-26.064470642144,25.5877575811898,1.92899359177089));
#42644=CARTESIAN_POINT('Ctrl Pts',(-26.2399303620716,25.349797395405,1.94942377213292));
#42645=CARTESIAN_POINT('Ctrl Pts',(-26.3881677059003,25.0775382171164,1.96903385076223));
#42646=CARTESIAN_POINT('Ctrl Pts',(-26.3955752751814,25.0636931847023,1.97002130378236));
#42647=CARTESIAN_POINT('Ctrl Pts',(-26.4045310410809,25.0466563276915,1.97122396278808));
#42648=CARTESIAN_POINT('Ctrl Pts',(-26.4061753758983,25.0435156826737,1.97144515061144));
#42649=CARTESIAN_POINT('Ctrl Pts',(-26.4088837466532,25.0383219140542,1.97181007599604));
#42650=CARTESIAN_POINT('Ctrl Pts',(-26.4099507551336,25.0362703582304,1.97195400176455));
#42651=CARTESIAN_POINT('Ctrl Pts',(-26.4117889416649,25.0327267331091,1.97220221923424));
#42652=CARTESIAN_POINT('Ctrl Pts',(-26.4125611601128,25.031235211936,1.97230657737779));
#42653=CARTESIAN_POINT('Ctrl Pts',(-26.4142924996836,25.0278847591941,1.97254073686263));
#42654=CARTESIAN_POINT('Ctrl Pts',(-26.4152509754843,25.0260255003881,1.97267049668115));
#42655=CARTESIAN_POINT('Ctrl Pts',(-26.4178008920491,25.0210673057413,1.97301605412005));
#42656=CARTESIAN_POINT('Ctrl Pts',(-26.4193891250588,25.0179667093932,1.97323164777198));
#42657=CARTESIAN_POINT('Ctrl Pts',(-26.4267789212413,25.0034822938528,1.97423648885563));
#42658=CARTESIAN_POINT('Ctrl Pts',(-26.4325178864234,24.992066406363,1.97502182195642));
#42659=CARTESIAN_POINT('Ctrl Pts',(-26.5690763079747,24.7163519358614,1.99383705143902));
#42660=CARTESIAN_POINT('Ctrl Pts',(-26.6630978776438,24.4353212491886,2.00975184648338));
#42661=CARTESIAN_POINT('Ctrl Pts',(-26.7544403727407,23.9491860270695,2.03758928423975));
#42662=CARTESIAN_POINT('Ctrl Pts',(-26.7729892818748,23.7500321587208,2.04906084790339));
#42663=CARTESIAN_POINT('Ctrl Pts',(-26.7730025245988,23.5504663859432,2.06117200133249));
#42664=CARTESIAN_POINT('Ctrl Pts',(-26.7730025246672,23.5504653522829,2.06117206406279));
#42665=CARTESIAN_POINT('Ctrl Pts',(-26.7730030301775,23.5428103913733,2.06163662479375));
#42666=CARTESIAN_POINT('Ctrl Pts',(-26.7729762615759,23.5351554912076,2.06210202842088));
#42667=CARTESIAN_POINT('Ctrl Pts',(-26.7728668282953,23.5196548135235,2.06304618952845));
#42668=CARTESIAN_POINT('Ctrl Pts',(-26.7727827839904,23.511809114334,2.06352498594758));
#42669=CARTESIAN_POINT('Ctrl Pts',(-26.772614772016,23.500112847161,2.06424014790564));
#42670=CARTESIAN_POINT('Ctrl Pts',(-26.7725525508248,23.4962619554381,2.06447583138215));
#42671=CARTESIAN_POINT('Ctrl Pts',(-26.7724265270868,23.4892414122739,2.06490591453335));
#42672=CARTESIAN_POINT('Ctrl Pts',(-26.7723649500896,23.4860717215934,2.06510024416008));
#42673=CARTESIAN_POINT('Ctrl Pts',(-26.7722357464253,23.479890612096,2.06547949893997));
#42674=CARTESIAN_POINT('Ctrl Pts',(-26.772168574643,23.4768791862025,2.06566440961753));
#42675=CARTESIAN_POINT('Ctrl Pts',(-26.7720173249408,23.4704995935676,2.0660564309928));
#42676=CARTESIAN_POINT('Ctrl Pts',(-26.7719321869442,23.4671314576255,2.06626357477444));
#42677=CARTESIAN_POINT('Ctrl Pts',(-26.7716756398554,23.4575754590055,2.06685177614449));
#42678=CARTESIAN_POINT('Ctrl Pts',(-26.7714916845276,23.4513879728562,2.06723322736863));
#42679=CARTESIAN_POINT('Ctrl Pts',(-26.7705662773994,23.4230135794938,2.06898522331759));
#42680=CARTESIAN_POINT('Ctrl Pts',(-26.7696134331534,23.4008346004517,2.07036239223191));
#42681=CARTESIAN_POINT('Ctrl Pts',(-26.7524925549218,23.0797220527192,2.09041703916769));
#42682=CARTESIAN_POINT('Ctrl Pts',(-26.6949796923149,22.7845191191838,2.11051495921379));
#42683=CARTESIAN_POINT('Ctrl Pts',(-26.5382238389041,22.3290020717458,2.14311126545295));
#42684=CARTESIAN_POINT('Ctrl Pts',(-26.4642778653392,22.161764889373,2.15540449737877));
#42685=CARTESIAN_POINT('Ctrl Pts',(-26.3689169849746,21.9877221193492,2.16795733091916));
#42686=CARTESIAN_POINT('Ctrl Pts',(-26.36117014571,21.9738284828484,2.16895751933203));
#42687=CARTESIAN_POINT('Ctrl Pts',(-26.3514683737279,21.9567276783878,2.17018570240719));
#42688=CARTESIAN_POINT('Ctrl Pts',(-26.3496104693446,21.9534661373944,2.1704198163315));
#42689=CARTESIAN_POINT('Ctrl Pts',(-26.3466784343106,21.9483398110055,2.17078757007863));
#42690=CARTESIAN_POINT('Ctrl Pts',(-26.3456081343642,21.9464728559859,2.17092145727548));
#42691=CARTESIAN_POINT('Ctrl Pts',(-26.3436059964716,21.9429885622767,2.17117124467223));
#42692=CARTESIAN_POINT('Ctrl Pts',(-26.3426746296233,21.9413709718532,2.17128717408809));
#42693=CARTESIAN_POINT('Ctrl Pts',(-26.3405829590522,21.9377454629886,2.1715469294805));
#42694=CARTESIAN_POINT('Ctrl Pts',(-26.3394218956156,21.9357379916791,2.17169070487653));
#42695=CARTESIAN_POINT('Ctrl Pts',(-26.3364698421235,21.9306465982311,2.1720552209492));
#42696=CARTESIAN_POINT('Ctrl Pts',(-26.3346758928518,21.9275643833536,2.17227576928163));
#42697=CARTESIAN_POINT('Ctrl Pts',(-26.3248249072765,21.9107036738795,2.1734816097101));
#42698=CARTESIAN_POINT('Ctrl Pts',(-26.3166705259008,21.8969818851879,2.1744606543097));
#42699=CARTESIAN_POINT('Ctrl Pts',(-26.1463218590701,21.6151171814071,2.19453587248533));
#42700=CARTESIAN_POINT('Ctrl Pts',(-25.9459469521276,21.371938971088,2.21130701930035));
#42701=CARTESIAN_POINT('Ctrl Pts',(-25.5905941411122,21.050122244552,2.23842650704243));
#42702=CARTESIAN_POINT('Ctrl Pts',(-25.4592151151905,20.9484270149588,2.24801405219184));
#42703=CARTESIAN_POINT('Ctrl Pts',(-25.3074308388297,20.8486436632403,2.25897929262195));
#42704=CARTESIAN_POINT('Ctrl Pts',(-25.2941947708239,20.840080667377,2.25993445675901));
#42705=CARTESIAN_POINT('Ctrl Pts',(-25.2742742712252,20.8273995736589,2.26137068151381));
#42706=CARTESIAN_POINT('Ctrl Pts',(-25.2676366186432,20.8232081452492,2.26184902520465));
#42707=CARTESIAN_POINT('Ctrl Pts',(-25.2569504380506,20.8165147116048,2.26261880810875));
#42708=CARTESIAN_POINT('Ctrl Pts',(-25.2529115383619,20.8139973317575,2.2629096789287));
#42709=CARTESIAN_POINT('Ctrl Pts',(-25.2451883699335,20.8092073285982,2.26346574931758));
#42710=CARTESIAN_POINT('Ctrl Pts',(-25.2415050667286,20.8069331620958,2.26373089125598));
#42711=CARTESIAN_POINT('Ctrl Pts',(-25.2349907002316,20.8029291300299,2.26419973103681));
#42712=CARTESIAN_POINT('Ctrl Pts',(-25.2321615208812,20.8011961987287,2.26440331562683));
#42713=CARTESIAN_POINT('Ctrl Pts',(-25.2265957479355,20.7977988548634,2.26480376228176));
#42714=CARTESIAN_POINT('Ctrl Pts',(-25.2238593382915,20.796134146707,2.26500061318987));
#42715=CARTESIAN_POINT('Ctrl Pts',(-25.2173003315207,20.7921573278004,2.26547238703523));
#42716=CARTESIAN_POINT('Ctrl Pts',(-25.2134754067405,20.7898490850476,2.26574745146423));
#42717=CARTESIAN_POINT('Ctrl Pts',(-25.1996623138714,20.7815523748684,2.26674061917723));
#42718=CARTESIAN_POINT('Ctrl Pts',(-25.1896465950827,20.7756101606567,2.26746041062464));
#42719=CARTESIAN_POINT('Ctrl Pts',(-25.0164318900992,20.6741090958042,2.27990352994431));
#42720=CARTESIAN_POINT('Ctrl Pts',(-24.8451964529509,20.5930612703739,2.29215972238692));
#42721=CARTESIAN_POINT('Ctrl Pts',(-24.5765732000631,20.4937416966127,2.31127165786629));
#42722=CARTESIAN_POINT('Ctrl Pts',(-24.4837948118511,20.4641400763565,2.3178464838661));
#42723=CARTESIAN_POINT('Ctrl Pts',(-24.3629448235205,20.4315310276109,2.32631877565821));
#42724=CARTESIAN_POINT('Ctrl Pts',(-24.3359740787569,20.4246271167725,2.32820364717702));
#42725=CARTESIAN_POINT('Ctrl Pts',(-24.135035793073,20.3759565944167,2.34219160710207));
#42726=CARTESIAN_POINT('Ctrl Pts',(-23.9579269078721,20.348386929382,2.35423515292208));
#42727=CARTESIAN_POINT('Ctrl Pts',(-23.7623021109567,20.3344404585691,2.36665353498257));
#42728=CARTESIAN_POINT('Ctrl Pts',(-23.7451673158523,20.3333564233635,2.36773374378712));
#42729=CARTESIAN_POINT('Ctrl Pts',(-23.7241827713985,20.3321971194842,2.36904677632269));
#42730=CARTESIAN_POINT('Ctrl Pts',(-23.7203409126009,20.3319917735538,2.36928676206817));
#42731=CARTESIAN_POINT('Ctrl Pts',(-23.7143288508363,20.3316812268013,2.36966166873918));
#42732=CARTESIAN_POINT('Ctrl Pts',(-23.712158909681,20.3315713408929,2.36979685322604));
#42733=CARTESIAN_POINT('Ctrl Pts',(-23.7083139308726,20.3313805291353,2.37003615616043));
#42734=CARTESIAN_POINT('Ctrl Pts',(-23.7066389504825,20.3312987167394,2.3701403243213));
#42735=CARTESIAN_POINT('Ctrl Pts',(-23.7030501837311,20.331126235511,2.37036334339759));
#42736=CARTESIAN_POINT('Ctrl Pts',(-23.7011363855756,20.3310359661409,2.37048217118767));
#42737=CARTESIAN_POINT('Ctrl Pts',(-23.6955787167573,20.3307787908424,2.37082695198532));
#42738=CARTESIAN_POINT('Ctrl Pts',(-23.6919346266934,20.3306163639932,2.37105265193657));
#42739=CARTESIAN_POINT('Ctrl Pts',(-23.6755008403376,20.3299118209543,2.37206886405149));
#42740=CARTESIAN_POINT('Ctrl Pts',(-23.6627080277553,20.3294397140333,2.37285548144107));
#42741=CARTESIAN_POINT('Ctrl Pts',(-23.6463686288345,20.3289341945299,2.37385488104211));
#42742=CARTESIAN_POINT('Ctrl Pts',(-23.642824570364,20.3288303998719,2.37407133550049));
#42743=CARTESIAN_POINT('Ctrl Pts',(-23.3141547621791,20.3197474984519,2.39411605781885));
#42744=CARTESIAN_POINT('Ctrl Pts',(-22.9894810956702,20.3600291549973,2.41144060698491));
#42745=CARTESIAN_POINT('Ctrl Pts',(-22.5268894787106,20.4903605199775,2.43871206747533));
#42746=CARTESIAN_POINT('Ctrl Pts',(-22.3807405853043,20.543186967019,2.44771408655974));
#42747=CARTESIAN_POINT('Ctrl Pts',(-22.2250494232986,20.6125345806638,2.45800733201461));
#42748=CARTESIAN_POINT('Ctrl Pts',(-22.2111658211919,20.6188370361138,2.45893145772388));
#42749=CARTESIAN_POINT('Ctrl Pts',(-22.1903754059429,20.6284533531939,2.46032492897523));
#42750=CARTESIAN_POINT('Ctrl Pts',(-22.1834346999271,20.6316937692567,2.46079174745395));
#42751=CARTESIAN_POINT('Ctrl Pts',(-22.1722723549476,20.6369536978693,2.46154514523939));
#42752=CARTESIAN_POINT('Ctrl Pts',(-22.168043418693,20.6389577286478,2.46183118822405));
#42753=CARTESIAN_POINT('Ctrl Pts',(-22.1599627298285,20.642808624024,2.46237894163569));
#42754=CARTESIAN_POINT('Ctrl Pts',(-22.1561102520167,20.6446539508235,2.46264059821849));
#42755=CARTESIAN_POINT('Ctrl Pts',(-22.1492797769412,20.6479424424481,2.46310543604126));
#42756=CARTESIAN_POINT('Ctrl Pts',(-22.1463003065786,20.6493825478514,2.46330851039401));
#42757=CARTESIAN_POINT('Ctrl Pts',(-22.1404237765402,20.6522341002824,2.46370965860968));
#42758=CARTESIAN_POINT('Ctrl Pts',(-22.1375266047444,20.6536453089492,2.46390772397547));
#42759=CARTESIAN_POINT('Ctrl Pts',(-22.1305527763274,20.6570552032996,2.46438520725713));
#42760=CARTESIAN_POINT('Ctrl Pts',(-22.126478225148,20.6590581591019,2.4646647744041));
#42761=CARTESIAN_POINT('Ctrl Pts',(-22.1139728333184,20.6652383689544,2.46552463365017));
#42762=CARTESIAN_POINT('Ctrl Pts',(-22.1055560994646,20.6694439113823,2.46610591708006));
#42763=CARTESIAN_POINT('Ctrl Pts',(-22.006785077225,20.7193379931196,2.4729577238437));
#42764=CARTESIAN_POINT('Ctrl Pts',(-21.918623014948,20.7692184950627,2.47937635083919));
#42765=CARTESIAN_POINT('Ctrl Pts',(-21.6614196796813,20.9311833164757,2.49906375337599));
#42766=CARTESIAN_POINT('Ctrl Pts',(-21.5004726790975,21.0551381122436,2.51273749521673));
#42767=CARTESIAN_POINT('Ctrl Pts',(-21.3282386234179,21.2157611491492,2.52867861130471));
#42768=CARTESIAN_POINT('Ctrl Pts',(-21.3045676599009,21.2385225947048,2.53090048542475));
#42769=CARTESIAN_POINT('Ctrl Pts',(-21.2537257234002,21.2889289652941,2.53573575801697));
#42770=CARTESIAN_POINT('Ctrl Pts',(-21.2266969042811,21.3167107269738,2.5383471756131));
#42771=CARTESIAN_POINT('Ctrl Pts',(-21.1107874413812,21.440230787809,2.54970701746402));
#42772=CARTESIAN_POINT('Ctrl Pts',(-21.0272614401654,21.540847990174,2.55832389388032));
#42773=CARTESIAN_POINT('Ctrl Pts',(-20.945328457863,21.6527403625358,2.56703179843677));
#42774=CARTESIAN_POINT('Ctrl Pts',(-20.9406151416111,21.6592277941297,2.56753369910608));
#42775=CARTESIAN_POINT('Ctrl Pts',(-20.9342159169173,21.6681052087411,2.56821637260278));
#42776=CARTESIAN_POINT('Ctrl Pts',(-20.9325090270918,21.670479923258,2.56839858695983));
#42777=CARTESIAN_POINT('Ctrl Pts',(-20.9296589142607,21.6744565598987,2.56870304324721));
#42778=CARTESIAN_POINT('Ctrl Pts',(-20.9285139262551,21.6760572056042,2.56882540808877));
#42779=CARTESIAN_POINT('Ctrl Pts',(-20.9262621228596,21.6792112347541,2.56906616371359));
#42780=CARTESIAN_POINT('Ctrl Pts',(-20.925155220334,21.6807645519431,2.56918456047483));
#42781=CARTESIAN_POINT('Ctrl Pts',(-20.9227180609442,21.6841910520281,2.5694453576293));
#42782=CARTESIAN_POINT('Ctrl Pts',(-20.9213884244894,21.6860646798938,2.56958771481183));
#42783=CARTESIAN_POINT('Ctrl Pts',(-20.9167524946352,21.6926121215739,2.57008432632749));
#42784=CARTESIAN_POINT('Ctrl Pts',(-20.9134566274837,21.6972933580386,2.57043786253606));
#42785=CARTESIAN_POINT('Ctrl Pts',(-20.8803360274832,21.7446030322833,2.57399567977419));
#42786=CARTESIAN_POINT('Ctrl Pts',(-20.8515331255406,21.787941951208,2.57713149454015));
#42787=CARTESIAN_POINT('Ctrl Pts',(-20.6486561715143,22.1098528441634,2.599683805621));
#42788=CARTESIAN_POINT('Ctrl Pts',(-20.5170149165162,22.4129120544996,2.61712865174157));
#42789=CARTESIAN_POINT('Ctrl Pts',(-20.4036561779065,22.8440081789899,2.64277107258762));
#42790=CARTESIAN_POINT('Ctrl Pts',(-20.380061580497,22.9588691076529,2.64965452512963));
#42791=CARTESIAN_POINT('Ctrl Pts',(-20.3608589551612,23.0875920324066,2.65753040407917));
#42792=CARTESIAN_POINT('Ctrl Pts',(-20.3590209950157,23.1004443555903,2.65831848385404));
#42793=CARTESIAN_POINT('Ctrl Pts',(-20.3563375601448,23.1200536444074,2.65952362829603));
#42794=CARTESIAN_POINT('Ctrl Pts',(-20.355435743757,23.1268028670266,2.65993891485386));
#42795=CARTESIAN_POINT('Ctrl Pts',(-20.353996421507,23.1378411769629,2.66061893905677));
#42796=CARTESIAN_POINT('Ctrl Pts',(-20.3534461402716,23.142128600893,2.6608832728024));
#42797=CARTESIAN_POINT('Ctrl Pts',(-20.3524020011353,23.1503955234636,2.66139335310589));
#42798=CARTESIAN_POINT('Ctrl Pts',(-20.3519069413694,23.1543748644296,2.66163906120622));
#42799=CARTESIAN_POINT('Ctrl Pts',(-20.3510203938014,23.1616112421496,2.66208620433249));
#42800=CARTESIAN_POINT('Ctrl Pts',(-20.3506264489566,23.1648679775022,2.66228756139004));
#42801=CARTESIAN_POINT('Ctrl Pts',(-20.3498416541829,23.1714400165466,2.66269414114037));
#42802=CARTESIAN_POINT('Ctrl Pts',(-20.3494509816387,23.1747553365586,2.66289936914962));
#42803=CARTESIAN_POINT('Ctrl Pts',(-20.3483683114657,23.1840675451735,2.6634761775757));
#42804=CARTESIAN_POINT('Ctrl Pts',(-20.3476880139432,23.1900657566035,2.66384812724026));
#42805=CARTESIAN_POINT('Ctrl Pts',(-20.3449748466093,23.2146033605156,2.66537142463432));
#42806=CARTESIAN_POINT('Ctrl Pts',(-20.343086109648,23.233158030996,2.66652731294229));
#42807=CARTESIAN_POINT('Ctrl Pts',(-20.3046911596426,23.6458719081593,2.69233061086009));
#42808=CARTESIAN_POINT('Ctrl Pts',(-20.3409731505091,24.0433509332076,2.71968110425252));
#42809=CARTESIAN_POINT('Ctrl Pts',(-20.4563424003248,24.4528761343452,2.74795188633107));
#42810=CARTESIAN_POINT('Ctrl Pts',(-20.4648389525128,24.4815056715679,2.74992542968048));
#42811=CARTESIAN_POINT('Ctrl Pts',(-20.4935601456592,24.5735716244023,2.75625442161755));
#42812=CARTESIAN_POINT('Ctrl Pts',(-20.5153544236156,24.6365053931723,2.76055393774446));
#42813=CARTESIAN_POINT('Ctrl Pts',(-20.5429388351263,24.7088287525354,2.76542774359601));
#42814=CARTESIAN_POINT('Ctrl Pts',(-20.5468438554051,24.7189145273974,2.7661058667078));
#42815=CARTESIAN_POINT('Ctrl Pts',(-20.5519992655365,24.7320332525235,2.766985710748));
#42816=CARTESIAN_POINT('Ctrl Pts',(-20.5532035568981,24.7350840653105,2.76719016640146));
#42817=CARTESIAN_POINT('Ctrl Pts',(-20.5551666911704,24.7400350987923,2.76752170954256));
#42818=CARTESIAN_POINT('Ctrl Pts',(-20.5559226861174,24.7419364348419,2.76764896927596));
#42819=CARTESIAN_POINT('Ctrl Pts',(-20.5573797961917,24.7455909426591,2.76789345048418));
#42820=CARTESIAN_POINT('Ctrl Pts',(-20.5580806393164,24.7473442132794,2.76801068771679));
#42821=CARTESIAN_POINT('Ctrl Pts',(-20.5596988616986,24.7513821544456,2.76828057298727));
#42822=CARTESIAN_POINT('Ctrl Pts',(-20.5606173207568,24.7536663962459,2.76843315517611));
#42823=CARTESIAN_POINT('Ctrl Pts',(-20.5630806258084,24.7597725027112,2.76884079296712));
#42824=CARTESIAN_POINT('Ctrl Pts',(-20.5646301951342,24.7635924756031,2.76909556283772));
#42825=CARTESIAN_POINT('Ctrl Pts',(-20.5717939282391,24.7811555747387,2.77026582405475));
#42826=CARTESIAN_POINT('Ctrl Pts',(-20.577495798041,24.7948630636545,2.77117609056848));
#42827=CARTESIAN_POINT('Ctrl Pts',(-20.7098117686798,25.1068577774496,2.79183462953358));
#42828=CARTESIAN_POINT('Ctrl Pts',(-20.8806242649835,25.3844533162252,2.80910307819126));
#42829=CARTESIAN_POINT('Ctrl Pts',(-21.1909254291394,25.751183490686,2.83635444299253));
#42830=CARTESIAN_POINT('Ctrl Pts',(-21.300355331277,25.8629294103558,2.84541121905516));
#42831=CARTESIAN_POINT('Ctrl Pts',(-21.4289141943782,25.9764172513883,2.85576724678622));
#42832=CARTESIAN_POINT('Ctrl Pts',(-21.4404545586771,25.9864594377371,2.85669441816827));
#42833=CARTESIAN_POINT('Ctrl Pts',(-21.4578941580385,26.0014181646639,2.85809208796558));
#42834=CARTESIAN_POINT('Ctrl Pts',(-21.4637402927719,26.0063965012704,2.85856004100092));
#42835=CARTESIAN_POINT('Ctrl Pts',(-21.4731838731496,26.0143802320581,2.85931505224242));
#42836=CARTESIAN_POINT('Ctrl Pts',(-21.4767702059011,26.017398773867,2.85960157100954));
#42837=CARTESIAN_POINT('Ctrl Pts',(-21.4836416223597,26.0231567369024,2.86015015210447));
#42838=CARTESIAN_POINT('Ctrl Pts',(-21.4869256015698,26.0258974654156,2.860412160235));
#42839=CARTESIAN_POINT('Ctrl Pts',(-21.4927605425126,26.0307474890549,2.86087739877659));
#42840=CARTESIAN_POINT('Ctrl Pts',(-21.4953093207737,26.0328594113266,2.86108052165847));
#42841=CARTESIAN_POINT('Ctrl Pts',(-21.5003444072504,26.0370184266232,2.86148159538987));
#42842=CARTESIAN_POINT('Ctrl Pts',(-21.5028305398763,26.0390657272043,2.8616795374749));
#42843=CARTESIAN_POINT('Ctrl Pts',(-21.5095300563892,26.0445658672728,2.8622126962302));
#42844=CARTESIAN_POINT('Ctrl Pts',(-21.5137491190402,26.0480117448543,2.86254819459288));
#42845=CARTESIAN_POINT('Ctrl Pts',(-21.5292425432874,26.0606004942123,2.86377928658282));
#42846=CARTESIAN_POINT('Ctrl Pts',(-21.5405697723922,26.0696777562319,2.86467752109661));
#42847=CARTESIAN_POINT('Ctrl Pts',(-21.7151238194768,26.2076333453132,2.87849298664016));
#42848=CARTESIAN_POINT('Ctrl Pts',(-21.8903085799789,26.3204282477399,2.89205552908989));
#42849=CARTESIAN_POINT('Ctrl Pts',(-22.0750360171757,26.4155367754983,2.90599376073416));
#42850=CARTESIAN_POINT('Origin',(-23.5502525316942,23.5502525316942,-77.3107734492734));
#42851=CARTESIAN_POINT('',(-22.07503587195,26.4155367007276,4.4051257859302));
#42852=CARTESIAN_POINT('',(-22.075036015346,26.4155367745563,4.16020796448762));
#42853=CARTESIAN_POINT('',(-22.0750360153461,26.4155367745563,-77.3107734492734));
#42854=CARTESIAN_POINT('',(-26.7730023558368,23.5513171860199,3.55804726516272));
#42855=CARTESIAN_POINT('Ctrl Pts',(-22.07503587195,26.4155367007276,4.4051257859302));
#42856=CARTESIAN_POINT('Ctrl Pts',(-21.9684851210008,26.3606781130149,4.39712134444059));
#42857=CARTESIAN_POINT('Ctrl Pts',(-21.8650503536945,26.299904915894,4.38899729673905));
#42858=CARTESIAN_POINT('Ctrl Pts',(-21.6097021045929,26.1300336496419,4.36824558262081));
#42859=CARTESIAN_POINT('Ctrl Pts',(-21.4634532864716,26.0132371846066,4.35566622781161));
#42860=CARTESIAN_POINT('Ctrl Pts',(-21.3196323257045,25.8763197794498,4.34314960938032));
#42861=CARTESIAN_POINT('Ctrl Pts',(-21.3111748571215,25.8681797354251,4.34241305214061));
#42862=CARTESIAN_POINT('Ctrl Pts',(-21.3002339817327,25.8575337300395,4.34145977720384));
#42863=CARTESIAN_POINT('Ctrl Pts',(-21.2977100907245,25.8550697815696,4.34123984077774));
#42864=CARTESIAN_POINT('Ctrl Pts',(-21.2938388617877,25.8512780619603,4.34090245515943));
#42865=CARTESIAN_POINT('Ctrl Pts',(-21.2924886495425,25.8499532498686,4.34078477391695));
#42866=CARTESIAN_POINT('Ctrl Pts',(-21.2898779221846,25.8473871200297,4.34055721622731));
#42867=CARTESIAN_POINT('Ctrl Pts',(-21.2886172691984,25.8461459594713,4.34044732879512));
#42868=CARTESIAN_POINT('Ctrl Pts',(-21.2857921135897,25.8433599019775,4.34020105505616));
#42869=CARTESIAN_POINT('Ctrl Pts',(-21.2842281731215,25.8418144451571,4.34006471430313));
#42870=CARTESIAN_POINT('Ctrl Pts',(-21.2809866800725,25.8386046989011,4.33978210578601));
#42871=CARTESIAN_POINT('Ctrl Pts',(-21.2793093731152,25.8369401616702,4.33963585774823));
#42872=CARTESIAN_POINT('Ctrl Pts',(-21.2750157536095,25.8326698470069,4.33926145059907));
#42873=CARTESIAN_POINT('Ctrl Pts',(-21.2724020770472,25.8300614061775,4.33903350043176));
#42874=CARTESIAN_POINT('Ctrl Pts',(-21.2648491378509,25.8224976419483,4.33837465183869));
#42875=CARTESIAN_POINT('Ctrl Pts',(-21.2599214835365,25.8175306808459,4.33794465512693));
#42876=CARTESIAN_POINT('Ctrl Pts',(-21.1331400584974,25.688902847659,4.32687620605352));
#42877=CARTESIAN_POINT('Ctrl Pts',(-21.0214404109597,25.5555918889305,4.31699183600734));
#42878=CARTESIAN_POINT('Ctrl Pts',(-20.8041232857785,25.2490020483835,4.29588819625619));
#42879=CARTESIAN_POINT('Ctrl Pts',(-20.7030114081795,25.0734698692578,4.28474389514435));
#42880=CARTESIAN_POINT('Ctrl Pts',(-20.5949945918379,24.837072816971,4.26978152398265));
#42881=CARTESIAN_POINT('Ctrl Pts',(-20.5724004535619,24.7838863563566,4.26642060069734));
#42882=CARTESIAN_POINT('Ctrl Pts',(-20.5440076603403,24.711717361796,4.26184987537096));
#42883=CARTESIAN_POINT('Ctrl Pts',(-20.5369360855625,24.6932454228964,4.26067912160974));
#42884=CARTESIAN_POINT('Ctrl Pts',(-20.5276103885707,24.6681972219883,4.25908982367172));
#42885=CARTESIAN_POINT('Ctrl Pts',(-20.5252067603137,24.6616768142737,4.25867594853426));
#42886=CARTESIAN_POINT('Ctrl Pts',(-20.5221894204981,24.6534092684354,4.25815095405821));
#42887=CARTESIAN_POINT('Ctrl Pts',(-20.521556087151,24.6516692729848,4.25804045081151));
#42888=CARTESIAN_POINT('Ctrl Pts',(-20.5185441137583,24.6433720522773,4.25751345205367));
#42889=CARTESIAN_POINT('Ctrl Pts',(-20.5161852798953,24.6368076973906,4.25709633574458));
#42890=CARTESIAN_POINT('Ctrl Pts',(-20.5119734188067,24.6249659257006,4.25634352337775));
#42891=CARTESIAN_POINT('Ctrl Pts',(-20.5101127794223,24.6196912317304,4.2560080707186));
#42892=CARTESIAN_POINT('Ctrl Pts',(-20.5040679124226,24.6024114822052,4.25490869634127));
#42893=CARTESIAN_POINT('Ctrl Pts',(-20.4999410276381,24.5903866158622,4.25414295294901));
#42894=CARTESIAN_POINT('Ctrl Pts',(-20.488831665434,24.5573815022274,4.25203903651663));
#42895=CARTESIAN_POINT('Ctrl Pts',(-20.4819938869267,24.5363536089928,4.25069623500844));
#42896=CARTESIAN_POINT('Ctrl Pts',(-20.4734405716673,24.5090994333402,4.24895223588301));
#42897=CARTESIAN_POINT('Ctrl Pts',(-20.4715264950855,24.5029356945091,4.24855758112382));
#42898=CARTESIAN_POINT('Ctrl Pts',(-20.4685141847668,24.4931315177131,4.24792944519452));
#42899=CARTESIAN_POINT('Ctrl Pts',(-20.4674038493248,24.4894947915054,4.2476963617164));
#42900=CARTESIAN_POINT('Ctrl Pts',(-20.4653365630964,24.4826805672332,4.24725946497918));
#42901=CARTESIAN_POINT('Ctrl Pts',(-20.4643780779643,24.4795035367812,4.24705570236491));
#42902=CARTESIAN_POINT('Ctrl Pts',(-20.4622310020416,24.4723468032983,4.24659654559194));
#42903=CARTESIAN_POINT('Ctrl Pts',(-20.4610451958679,24.4683662770125,4.24634106058987));
#42904=CARTESIAN_POINT('Ctrl Pts',(-20.4575769820611,24.4566413513681,4.24558819545308));
#42905=CARTESIAN_POINT('Ctrl Pts',(-20.4553159905501,24.4488906969849,4.24509011573967));
#42906=CARTESIAN_POINT('Ctrl Pts',(-20.438233076246,24.3895014277996,4.24127037577921));
#42907=CARTESIAN_POINT('Ctrl Pts',(-20.4246761108608,24.3375106057971,4.23790770460332));
#42908=CARTESIAN_POINT('Ctrl Pts',(-20.3834777317323,24.161617708331,4.2264589136504));
#42909=CARTESIAN_POINT('Ctrl Pts',(-20.3618602941651,24.0364400183458,4.21818605949086));
#42910=CARTESIAN_POINT('Ctrl Pts',(-20.3141832127796,23.6123898454376,4.18981716201159));
#42911=CARTESIAN_POINT('Ctrl Pts',(-20.3224236973037,23.3112574914066,4.16896285271615));
#42912=CARTESIAN_POINT('Ctrl Pts',(-20.3777811622714,22.9821932268002,4.14755649513074));
#42913=CARTESIAN_POINT('Ctrl Pts',(-20.3839300920827,22.9488638059815,4.14540655713465));
#42914=CARTESIAN_POINT('Ctrl Pts',(-20.3916035921698,22.9106587453462,4.14296792047436));
#42915=CARTESIAN_POINT('Ctrl Pts',(-20.3926150382862,22.9056838419814,4.14265087683941));
#42916=CARTESIAN_POINT('Ctrl Pts',(-20.3941278801229,22.8983317941206,4.14218310997013));
#42917=CARTESIAN_POINT('Ctrl Pts',(-20.3946202088096,22.8959528242252,4.14203186947006));
#42918=CARTESIAN_POINT('Ctrl Pts',(-20.3954851614186,22.8917969918221,4.14176787778324));
#42919=CARTESIAN_POINT('Ctrl Pts',(-20.39585659676,22.8900198876365,4.14165505799729));
#42920=CARTESIAN_POINT('Ctrl Pts',(-20.3966447607644,22.8862648243074,4.14141681068948));
#42921=CARTESIAN_POINT('Ctrl Pts',(-20.3970618477952,22.8842869474058,4.14129140439968));
#42922=CARTESIAN_POINT('Ctrl Pts',(-20.3981531259212,22.879135983253,4.14096502576443));
#42923=CARTESIAN_POINT('Ctrl Pts',(-20.3988302496512,22.8759635091456,4.14076422272315));
#42924=CARTESIAN_POINT('Ctrl Pts',(-20.4003200114453,22.8690349092924,4.14032612949517));
#42925=CARTESIAN_POINT('Ctrl Pts',(-20.4011345817016,22.8652791974783,4.14008894959252));
#42926=CARTESIAN_POINT('Ctrl Pts',(-20.403535695419,22.8543032786062,4.13939663259931));
#42927=CARTESIAN_POINT('Ctrl Pts',(-20.4051403790128,22.84708700345,4.13894251211326));
#42928=CARTESIAN_POINT('Ctrl Pts',(-20.4107352579961,22.8223291322585,4.13738791756104));
#42929=CARTESIAN_POINT('Ctrl Pts',(-20.414847575211,22.8048150899971,4.13629407866138));
#42930=CARTESIAN_POINT('Ctrl Pts',(-20.4323282254214,22.7330713749046,4.13183415891107));
#42931=CARTESIAN_POINT('Ctrl Pts',(-20.4469592925563,22.6791561593652,4.1285315097568));
#42932=CARTESIAN_POINT('Ctrl Pts',(-20.4863502278237,22.5476296834416,4.12053489419163));
#42933=CARTESIAN_POINT('Ctrl Pts',(-20.5126652626464,22.4705234320225,4.11589905343451));
#42934=CARTESIAN_POINT('Ctrl Pts',(-20.6273990060186,22.1718778154147,4.09786403039087));
#42935=CARTESIAN_POINT('Ctrl Pts',(-20.7373632809484,21.95945338386,4.08479978116152));
#42936=CARTESIAN_POINT('Ctrl Pts',(-20.8873526593137,21.7347397811048,4.06913506552769));
#42937=CARTESIAN_POINT('Ctrl Pts',(-20.9053373533079,21.7086375101815,4.06728586882316));
#42938=CARTESIAN_POINT('Ctrl Pts',(-20.9284729601965,21.6760974736276,4.06494027841518));
#42939=CARTESIAN_POINT('Ctrl Pts',(-20.9332678221882,21.6694079523006,4.06445589723153));
#42940=CARTESIAN_POINT('Ctrl Pts',(-20.9791092032794,21.6059673015754,4.05984113137371));
#42941=CARTESIAN_POINT('Ctrl Pts',(-21.021967270049,21.5505536607487,4.05564856578748));
#42942=CARTESIAN_POINT('Ctrl Pts',(-21.0725578158683,21.4893706712781,4.05081316189486));
#42943=CARTESIAN_POINT('Ctrl Pts',(-21.0785528926741,21.4821843415746,4.05024188664841));
#42944=CARTESIAN_POINT('Ctrl Pts',(-21.0874323582364,21.4716342432703,4.04939824787638));
#42945=CARTESIAN_POINT('Ctrl Pts',(-21.0902925566819,21.4682501021116,4.04912687738053));
#42946=CARTESIAN_POINT('Ctrl Pts',(-21.0953554119298,21.4622848097421,4.04864718207597));
#42947=CARTESIAN_POINT('Ctrl Pts',(-21.097555187782,21.459701213126,4.04843897620356));
#42948=CARTESIAN_POINT('Ctrl Pts',(-21.1021140503072,21.4543640122092,4.0480079343413));
#42949=CARTESIAN_POINT('Ctrl Pts',(-21.1044737110849,21.4516109065842,4.0477850747729));
#42950=CARTESIAN_POINT('Ctrl Pts',(-21.1105313211834,21.4445673557242,4.04721358821548));
#42951=CARTESIAN_POINT('Ctrl Pts',(-21.114235933065,21.4402826798093,4.04686468499379));
#42952=CARTESIAN_POINT('Ctrl Pts',(-21.1294318728703,21.4228007416184,4.04543593150143));
#42953=CARTESIAN_POINT('Ctrl Pts',(-21.1410191349093,21.409687605871,4.04435208342417));
#42954=CARTESIAN_POINT('Ctrl Pts',(-21.2177784248951,21.3242330451534,4.0372077587366));
#42955=CARTESIAN_POINT('Ctrl Pts',(-21.2860873457146,21.2547894112365,4.03101390739717));
#42956=CARTESIAN_POINT('Ctrl Pts',(-21.4903735151517,21.0651112409568,4.01291800140255));
#42957=CARTESIAN_POINT('Ctrl Pts',(-21.6334889245438,20.9531326171695,4.00071755043467));
#42958=CARTESIAN_POINT('Ctrl Pts',(-21.9160373219171,20.7681859456528,3.97786067675297));
#42959=CARTESIAN_POINT('Ctrl Pts',(-22.0528940420453,20.6921976794464,3.96726058667305));
#42960=CARTESIAN_POINT('Ctrl Pts',(-22.2531088857047,20.5993753504602,3.95283875703214));
#42961=CARTESIAN_POINT('Ctrl Pts',(-22.3122874870389,20.574063401569,3.94870341620471));
#42962=CARTESIAN_POINT('Ctrl Pts',(-22.3777028458145,20.548373139294,3.94430014551669));
#42963=CARTESIAN_POINT('Ctrl Pts',(-22.3832225705398,20.5462229507032,3.94392988749525));
#42964=CARTESIAN_POINT('Ctrl Pts',(-22.3909814932393,20.5432251035114,3.94341126529258));
#42965=CARTESIAN_POINT('Ctrl Pts',(-22.3932157117843,20.5423647193068,3.94326213928935));
#42966=CARTESIAN_POINT('Ctrl Pts',(-22.3970922156404,20.5408768591062,3.94300376979348));
#42967=CARTESIAN_POINT('Ctrl Pts',(-22.3987340553236,20.5402482373622,3.94289445691381));
#42968=CARTESIAN_POINT('Ctrl Pts',(-22.4021257119771,20.5389528330951,3.94266888269686));
#42969=CARTESIAN_POINT('Ctrl Pts',(-22.4038755940033,20.5382862327983,3.94255263284976));
#42970=CARTESIAN_POINT('Ctrl Pts',(-22.4080210920587,20.5367111822111,3.94227754625223));
#42971=CARTESIAN_POINT('Ctrl Pts',(-22.4104172191541,20.5358040602268,3.94211879007372));
#42972=CARTESIAN_POINT('Ctrl Pts',(-22.4154989600927,20.5338871482635,3.94178261340583));
#42973=CARTESIAN_POINT('Ctrl Pts',(-22.4181848482057,20.5328780844679,3.94160523655475));
#42974=CARTESIAN_POINT('Ctrl Pts',(-22.425472555509,20.5301512593923,3.9411247715975));
#42975=CARTESIAN_POINT('Ctrl Pts',(-22.4300769832063,20.5284404212048,3.94082209318514));
#42976=CARTESIAN_POINT('Ctrl Pts',(-22.4443837040294,20.5231617564884,3.93988430692415));
#42977=CARTESIAN_POINT('Ctrl Pts',(-22.4540993800933,20.5196300378459,3.93925128580627));
#42978=CARTESIAN_POINT('Ctrl Pts',(-22.4905488350806,20.5065786098205,3.93689015261329));
#42979=CARTESIAN_POINT('Ctrl Pts',(-22.517391853552,20.4973650771939,3.93517885809896));
#42980=CARTESIAN_POINT('Ctrl Pts',(-22.6102952913908,20.466842807378,3.92933926934609));
#42981=CARTESIAN_POINT('Ctrl Pts',(-22.6769237678563,20.4473130673509,3.92529484949624));
#42982=CARTESIAN_POINT('Ctrl Pts',(-23.1186401387562,20.333197494506,3.89910780465876));
#42983=CARTESIAN_POINT('Ctrl Pts',(-23.5074825751874,20.3046496393114,3.87854463488742));
#42984=CARTESIAN_POINT('Ctrl Pts',(-23.9120893949128,20.3478169068271,3.85393246679386));
#42985=CARTESIAN_POINT('Ctrl Pts',(-23.9320125810545,20.3501308022241,3.85271355764969));
#42986=CARTESIAN_POINT('Ctrl Pts',(-23.9580775243418,20.3534048742732,3.85110933089652));
#42987=CARTESIAN_POINT('Ctrl Pts',(-23.9642402348993,20.3541970956721,3.85072933160547));
#42988=CARTESIAN_POINT('Ctrl Pts',(-23.9737455646093,20.3554469670412,3.85014212801616));
#42989=CARTESIAN_POINT('Ctrl Pts',(-23.977089844355,20.3558920552845,3.84993532169187));
#42990=CARTESIAN_POINT('Ctrl Pts',(-23.9837469936487,20.356788692384,3.84952323216202));
#42991=CARTESIAN_POINT('Ctrl Pts',(-23.9870598718346,20.3572401469715,3.84931795218181));
#42992=CARTESIAN_POINT('Ctrl Pts',(-23.9944005023008,20.3582521119411,3.84886263443916));
#42993=CARTESIAN_POINT('Ctrl Pts',(-23.9984279034157,20.3588150913802,3.84861251870254));
#42994=CARTESIAN_POINT('Ctrl Pts',(-24.0100398701518,20.3604607103131,3.84789048079409));
#42995=CARTESIAN_POINT('Ctrl Pts',(-24.0176216161271,20.361562769794,3.84741794331726));
#42996=CARTESIAN_POINT('Ctrl Pts',(-24.0685830859848,20.3691560325501,3.8442342426152));
#42997=CARTESIAN_POINT('Ctrl Pts',(-24.1118285328456,20.3765049694885,3.84149595049705));
#42998=CARTESIAN_POINT('Ctrl Pts',(-24.2275980481276,20.3986184933433,3.83406210437802));
#42999=CARTESIAN_POINT('Ctrl Pts',(-24.2997822557187,20.4150016902376,3.82931655180012));
#43000=CARTESIAN_POINT('Ctrl Pts',(-24.536687018817,20.4774192998406,3.81337190791578));
#43001=CARTESIAN_POINT('Ctrl Pts',(-24.6982932825663,20.534071529534,3.80187534108136));
#43002=CARTESIAN_POINT('Ctrl Pts',(-24.9258808465114,20.6348046722321,3.78503158142683));
#43003=CARTESIAN_POINT('Ctrl Pts',(-24.9959692541866,20.6689172622727,3.77975163361922));
#43004=CARTESIAN_POINT('Ctrl Pts',(-25.1843308531128,20.7691992530821,3.76539858719322));
#43005=CARTESIAN_POINT('Ctrl Pts',(-25.2997914380041,20.8403462535412,3.75641387261008));
#43006=CARTESIAN_POINT('Ctrl Pts',(-25.4222685305741,20.9269181275548,3.74693620850097));
#43007=CARTESIAN_POINT('Ctrl Pts',(-25.4340384464264,20.9353571337317,3.74602604181142));
#43008=CARTESIAN_POINT('Ctrl Pts',(-25.4488056307422,20.9460966309731,3.74488530647954));
#43009=CARTESIAN_POINT('Ctrl Pts',(-25.451856037607,20.948323260593,3.7446497342712));
#43010=CARTESIAN_POINT('Ctrl Pts',(-25.4566607860887,20.9518434259396,3.74427879331534));
#43011=CARTESIAN_POINT('Ctrl Pts',(-25.4584177292043,20.9531333791771,3.74414317592467));
#43012=CARTESIAN_POINT('Ctrl Pts',(-25.461530568216,20.9554236994271,3.74390294211603));
#43013=CARTESIAN_POINT('Ctrl Pts',(-25.4628869811644,20.9564233421784,3.74379827587307));
#43014=CARTESIAN_POINT('Ctrl Pts',(-25.4659813602872,20.9587075700112,3.74355953549685));
#43015=CARTESIAN_POINT('Ctrl Pts',(-25.4677188153151,20.9599928373065,3.74342551025365));
#43016=CARTESIAN_POINT('Ctrl Pts',(-25.4725554609694,20.9635782371367,3.74305248128033));
#43017=CARTESIAN_POINT('Ctrl Pts',(-25.4756518276613,20.9658822003594,3.74281374583492));
#43018=CARTESIAN_POINT('Ctrl Pts',(-25.4825525205745,20.9710361951404,3.74228183586311));
#43019=CARTESIAN_POINT('Ctrl Pts',(-25.4863547044549,20.9738890994357,3.74198886030146));
#43020=CARTESIAN_POINT('Ctrl Pts',(-25.4980453900141,20.9827015026518,3.741088298431));
#43021=CARTESIAN_POINT('Ctrl Pts',(-25.5059128809542,20.9886889642956,3.74048261036278));
#43022=CARTESIAN_POINT('Ctrl Pts',(-25.5349278253085,21.0109820426369,3.73824969656118));
#43023=CARTESIAN_POINT('Ctrl Pts',(-25.5559005821179,21.0275146065447,3.73663734082592));
#43024=CARTESIAN_POINT('Ctrl Pts',(-25.6293475401673,21.0869069150594,3.73098706078739));
#43025=CARTESIAN_POINT('Ctrl Pts',(-25.6806761207035,21.1311609133904,3.72703126809774));
#43026=CARTESIAN_POINT('Ctrl Pts',(-26.0191739760883,21.4421414335047,3.70059742564631));
#43027=CARTESIAN_POINT('Ctrl Pts',(-26.2569881571294,21.7576765512726,3.67980724021613));
#43028=CARTESIAN_POINT('Ctrl Pts',(-26.4410085701265,22.12546495894,3.65492068913603));
#43029=CARTESIAN_POINT('Ctrl Pts',(-26.4494897027726,22.1428031003409,3.65374739229731));
#43030=CARTESIAN_POINT('Ctrl Pts',(-26.4604540219324,22.1657373456577,3.65219490092532));
#43031=CARTESIAN_POINT('Ctrl Pts',(-26.4630778566817,22.1712660780096,3.65182060606667));
#43032=CARTESIAN_POINT('Ctrl Pts',(-26.4671156799694,22.1798371960958,3.65124027172663));
#43033=CARTESIAN_POINT('Ctrl Pts',(-26.4685407019315,22.1828743933849,3.65103461520077));
#43034=CARTESIAN_POINT('Ctrl Pts',(-26.4713771676027,22.1889444789014,3.65062356434448));
#43035=CARTESIAN_POINT('Ctrl Pts',(-26.4727886368106,22.1919773507137,3.65041817121054));
#43036=CARTESIAN_POINT('Ctrl Pts',(-26.4759188952197,22.1987309115799,3.64996076900529));
#43037=CARTESIAN_POINT('Ctrl Pts',(-26.4776353118819,22.2024526881292,3.64970867832266));
#43038=CARTESIAN_POINT('Ctrl Pts',(-26.482602693946,22.2132779184763,3.64897536726457));
#43039=CARTESIAN_POINT('Ctrl Pts',(-26.4858349192569,22.2203898942174,3.64849350137904));
#43040=CARTESIAN_POINT('Ctrl Pts',(-26.5084050487386,22.2705349643943,3.64509520766727));
#43041=CARTESIAN_POINT('Ctrl Pts',(-26.5268209493351,22.3139744724767,3.64214730061621));
#43042=CARTESIAN_POINT('Ctrl Pts',(-26.5815694784785,22.4514377936207,3.63279965841365));
#43043=CARTESIAN_POINT('Ctrl Pts',(-26.614446234285,22.5467637500771,3.62628775400308));
#43044=CARTESIAN_POINT('Ctrl Pts',(-26.729272943672,22.9383740710023,3.59943465296249));
#43045=CARTESIAN_POINT('Ctrl Pts',(-26.7731038549109,23.2440755629043,3.57805985896633));
#43046=CARTESIAN_POINT('Ctrl Pts',(-26.7730023558368,23.5513171860199,3.55804726516272));
#43047=CARTESIAN_POINT('Ctrl Pts',(-26.7730023545155,23.5513211782174,3.55804700512569));
#43048=CARTESIAN_POINT('Ctrl Pts',(-26.7729832548478,23.6089206270496,3.5542951907194));
#43049=CARTESIAN_POINT('Ctrl Pts',(-26.7714199600787,23.6665144938145,3.55060172167451));
#43050=CARTESIAN_POINT('Ctrl Pts',(-26.7680777749399,23.7284023229884,3.54671699804464));
#43051=CARTESIAN_POINT('Ctrl Pts',(-26.7678333450828,23.7327637753233,3.54644367868682));
#43052=CARTESIAN_POINT('Ctrl Pts',(-26.7674266535249,23.739765671965,3.54600562888445));
#43053=CARTESIAN_POINT('Ctrl Pts',(-26.7672700082726,23.7424064179969,3.54584058828782));
#43054=CARTESIAN_POINT('Ctrl Pts',(-26.7669933752814,23.7469747665552,3.54555537229685));
#43055=CARTESIAN_POINT('Ctrl Pts',(-26.7668749062878,23.748902454426,3.54543511184088));
#43056=CARTESIAN_POINT('Ctrl Pts',(-26.7666457701686,23.7525769283429,3.54520605163458));
#43057=CARTESIAN_POINT('Ctrl Pts',(-26.7665354127903,23.7543237319809,3.54509723438252));
#43058=CARTESIAN_POINT('Ctrl Pts',(-26.7663018245475,23.7579738503119,3.54487000881177));
#43059=CARTESIAN_POINT('Ctrl Pts',(-26.7661783270661,23.7598771461006,3.54475161599882));
#43060=CARTESIAN_POINT('Ctrl Pts',(-26.7659023405037,23.7640728959666,3.54449082009936));
#43061=CARTESIAN_POINT('Ctrl Pts',(-26.7657490891901,23.7663653029111,3.54434846023585));
#43062=CARTESIAN_POINT('Ctrl Pts',(-26.7652053520294,23.774370156927,3.54385180061354));
#43063=CARTESIAN_POINT('Ctrl Pts',(-26.7648020910703,23.7800817692397,3.54349821919257));
#43064=CARTESIAN_POINT('Ctrl Pts',(-26.7605787522617,23.8377126439053,3.53993828545128));
#43065=CARTESIAN_POINT('Ctrl Pts',(-26.7555161226822,23.8895368274097,3.53680048888148));
#43066=CARTESIAN_POINT('Ctrl Pts',(-26.7477668696566,23.952942372934,3.53301462335436));
#43067=CARTESIAN_POINT('Ctrl Pts',(-26.7462696357952,23.9646578010469,3.53231734591374));
#43068=CARTESIAN_POINT('Ctrl Pts',(-26.7006301938124,24.3068050412611,3.51201202278428));
#43069=CARTESIAN_POINT('Ctrl Pts',(-26.6055491089283,24.6284312303505,3.49431771996669));
#43070=CARTESIAN_POINT('Ctrl Pts',(-26.4295177855175,25.000079690047,3.47051216199984));
#43071=CARTESIAN_POINT('Ctrl Pts',(-26.3936918313434,25.0691398716863,3.46594238409155));
#43072=CARTESIAN_POINT('Ctrl Pts',(-26.3359506809717,25.1712290720934,3.45892010181078));
#43073=CARTESIAN_POINT('Ctrl Pts',(-26.3158661236785,25.2052632177996,3.45653259031974));
#43074=CARTESIAN_POINT('Ctrl Pts',(-26.2912621408161,25.2452567398001,3.45366817223913));
#43075=CARTESIAN_POINT('Ctrl Pts',(-26.287340851671,25.2515815621807,3.45321340121067));
#43076=CARTESIAN_POINT('Ctrl Pts',(-26.2812678845662,25.2613015846225,3.45251174615104));
#43077=CARTESIAN_POINT('Ctrl Pts',(-26.2791316843896,25.2647064648459,3.45226543551542));
#43078=CARTESIAN_POINT('Ctrl Pts',(-26.2753816631374,25.2706588423165,3.45183391577181));
#43079=CARTESIAN_POINT('Ctrl Pts',(-26.2737706225249,25.2732080927841,3.45164881009189));
#43080=CARTESIAN_POINT('Ctrl Pts',(-26.2701216319553,25.2789642130425,3.45123017437348));
#43081=CARTESIAN_POINT('Ctrl Pts',(-26.2680815866563,25.2821697432236,3.45099656652647));
#43082=CARTESIAN_POINT('Ctrl Pts',(-26.2625677964255,25.2907998479718,3.45036635249445));
#43083=CARTESIAN_POINT('Ctrl Pts',(-26.2590834623374,25.2962176068667,3.44996935151409));
#43084=CARTESIAN_POINT('Ctrl Pts',(-26.2436273929557,25.3200924699334,3.44821376696568));
#43085=CARTESIAN_POINT('Ctrl Pts',(-26.2314833165106,25.3384368035601,3.44684873394499));
#43086=CARTESIAN_POINT('Ctrl Pts',(-26.2104784106609,25.3694708592442,3.44451134506712));
#43087=CARTESIAN_POINT('Ctrl Pts',(-26.2017121315148,25.3822238817568,3.44354261114887));
#43088=CARTESIAN_POINT('Ctrl Pts',(-26.1864387056822,25.4041041048179,3.44186621106304));
#43089=CARTESIAN_POINT('Ctrl Pts',(-26.1799751085338,25.4132614857394,3.44116020993179));
#43090=CARTESIAN_POINT('Ctrl Pts',(-26.1726465211284,25.4235302224492,3.44036354701902));
#43091=CARTESIAN_POINT('Ctrl Pts',(-26.1718283570184,25.4246750386459,3.44027466059285));
#43092=CARTESIAN_POINT('Ctrl Pts',(-26.1639336096302,25.4357064846877,3.43941747583576));
#43093=CARTESIAN_POINT('Ctrl Pts',(-26.156801959169,25.4455534211798,3.4386470986145));
#43094=CARTESIAN_POINT('Ctrl Pts',(-26.1472639788668,25.4585672124211,3.43762196478568));
#43095=CARTESIAN_POINT('Ctrl Pts',(-26.1449071945639,25.4617703991617,3.43736907415336));
#43096=CARTESIAN_POINT('Ctrl Pts',(-26.1392629926044,25.4694119576199,3.43676441944088));
#43097=CARTESIAN_POINT('Ctrl Pts',(-26.1359700899193,25.473846245894,3.43641245043136));
#43098=CARTESIAN_POINT('Ctrl Pts',(-26.1238802525535,25.4900395244221,3.43512309561724));
#43099=CARTESIAN_POINT('Ctrl Pts',(-26.1150144700019,25.5017466801418,3.4341831497172));
#43100=CARTESIAN_POINT('Ctrl Pts',(-25.9477497217723,25.719509030779,3.41655287160166));
#43101=CARTESIAN_POINT('Ctrl Pts',(-25.765097918075,25.9056895297535,3.39889550684495));
#43102=CARTESIAN_POINT('Ctrl Pts',(-25.4968350405726,26.1200616863566,3.3757115820829));
#43103=CARTESIAN_POINT('Ctrl Pts',(-25.4295365377656,26.1696790947764,3.37009991888696));
#43104=CARTESIAN_POINT('Ctrl Pts',(-25.3102755607003,26.2506421845818,3.36058552815684));
#43105=CARTESIAN_POINT('Ctrl Pts',(-25.2592163476026,26.2832415611422,3.35663984614454));
#43106=CARTESIAN_POINT('Ctrl Pts',(-25.1916005642599,26.3237751593491,3.3516073101922));
#43107=CARTESIAN_POINT('Ctrl Pts',(-25.1758558258971,26.3330326335966,3.35044869122838));
#43108=CARTESIAN_POINT('Ctrl Pts',(-25.1535567872937,26.3458900096894,3.34882724061706));
#43109=CARTESIAN_POINT('Ctrl Pts',(-25.1470677020797,26.3496015200517,3.34835769839622));
#43110=CARTESIAN_POINT('Ctrl Pts',(-25.135722519459,26.3560382482091,3.347540867666));
#43111=CARTESIAN_POINT('Ctrl Pts',(-25.130872195773,26.3587735032618,3.34719295276691));
#43112=CARTESIAN_POINT('Ctrl Pts',(-25.1238216135272,26.3627255054854,3.34668912275339));
#43113=CARTESIAN_POINT('Ctrl Pts',(-25.1216270161875,26.3639522514927,3.34653256611084));
#43114=CARTESIAN_POINT('Ctrl Pts',(-25.1178825228433,26.3660396181315,3.34626590347966));
#43115=CARTESIAN_POINT('Ctrl Pts',(-25.1163333508096,26.366901528881,3.34615571368073));
#43116=CARTESIAN_POINT('Ctrl Pts',(-25.113250046242,26.368613652702,3.34593667115952));
#43117=CARTESIAN_POINT('Ctrl Pts',(-25.1117159325408,26.3694638906995,3.34582781681194));
#43118=CARTESIAN_POINT('Ctrl Pts',(-25.1081001702286,26.3714639652756,3.34557156480758));
#43119=CARTESIAN_POINT('Ctrl Pts',(-25.1060179380628,26.372612752908,3.34542423516249));
#43120=CARTESIAN_POINT('Ctrl Pts',(-25.099863628826,26.3759992647313,3.34498948543377));
#43121=CARTESIAN_POINT('Ctrl Pts',(-25.0957879595578,26.378230500753,3.3447024810362));
#43122=CARTESIAN_POINT('Ctrl Pts',(-25.0602458323582,26.3975883479053,3.34220740698612));
#43123=CARTESIAN_POINT('Ctrl Pts',(-25.0284990660371,26.4141988412201,3.34003170514781));
#43124=CARTESIAN_POINT('Ctrl Pts',(-24.8466973350538,26.5054920537614,3.32783265651303));
#43125=CARTESIAN_POINT('Ctrl Pts',(-24.6912554534103,26.5689171250461,3.31838960395227));
#43126=CARTESIAN_POINT('Ctrl Pts',(-24.5151280379785,26.6252209397543,3.30804020957837));
#43127=CARTESIAN_POINT('Ctrl Pts',(-24.4986461325155,26.6303442565683,3.30707509553081));
#43128=CARTESIAN_POINT('Ctrl Pts',(-24.4633785338458,26.6409970881002,3.3050158436721));
#43129=CARTESIAN_POINT('Ctrl Pts',(-24.4445820072437,26.646488278328,3.30392186136501));
#43130=CARTESIAN_POINT('Ctrl Pts',(-24.4040347995071,26.6579336439278,3.30156767792024));
#43131=CARTESIAN_POINT('Ctrl Pts',(-24.3822693445967,26.663831513458,3.30030748184477));
#43132=CARTESIAN_POINT('Ctrl Pts',(-24.334803316005,26.6761603068449,3.29756410622653));
#43133=CARTESIAN_POINT('Ctrl Pts',(-24.3090817950271,26.6825037168355,3.29608055927804));
#43134=CARTESIAN_POINT('Ctrl Pts',(-24.2520327919579,26.6958291124097,3.2927925860077));
#43135=CARTESIAN_POINT('Ctrl Pts',(-24.220673487355,26.7026616515778,3.29098683570275));
#43136=CARTESIAN_POINT('Ctrl Pts',(-24.1489242629813,26.7171752832638,3.28685166525733));
#43137=CARTESIAN_POINT('Ctrl Pts',(-24.1084793644934,26.7245540661802,3.28451802296216));
#43138=CARTESIAN_POINT('Ctrl Pts',(-23.9654117324493,26.7478365426071,3.27623235892892));
#43139=CARTESIAN_POINT('Ctrl Pts',(-23.8621804969453,26.7595513054382,3.27019585559012));
#43140=CARTESIAN_POINT('Ctrl Pts',(-23.71086418142,26.7693528539763,3.26115476456382));
#43141=CARTESIAN_POINT('Ctrl Pts',(-23.6630972792925,26.7713810106407,3.25827330576143));
#43142=CARTESIAN_POINT('Ctrl Pts',(-23.6074673147068,26.77250414854,3.25488013295656));
#43143=CARTESIAN_POINT('Ctrl Pts',(-23.5996293367874,26.7726337852189,3.25440119245355));
#43144=CARTESIAN_POINT('Ctrl Pts',(-23.5876871381631,26.772787722715,3.25367012772748));
#43145=CARTESIAN_POINT('Ctrl Pts',(-23.5835831760688,26.7728327828326,3.25341865554086));
#43146=CARTESIAN_POINT('Ctrl Pts',(-23.5761337030236,26.7729003437323,3.25296174544063));
#43147=CARTESIAN_POINT('Ctrl Pts',(-23.5727882168216,26.7729254747997,3.25275639040534));
#43148=CARTESIAN_POINT('Ctrl Pts',(-23.5660911285918,26.7729653539649,3.252344979996));
#43149=CARTESIAN_POINT('Ctrl Pts',(-23.5627395306083,26.7729800831176,3.25213892428086));
#43150=CARTESIAN_POINT('Ctrl Pts',(-23.5532843201772,26.7730068855131,3.25155715660602));
#43151=CARTESIAN_POINT('Ctrl Pts',(-23.5471807116872,26.7730068474778,3.25118106483601));
#43152=CARTESIAN_POINT('Ctrl Pts',(-23.521903414878,26.7729348812405,3.24962124909498));
#43153=CARTESIAN_POINT('Ctrl Pts',(-23.5027308682403,26.7727091822049,3.24843270808397));
#43154=CARTESIAN_POINT('Ctrl Pts',(-23.0905919617589,26.7641786631398,3.22276273278232));
#43155=CARTESIAN_POINT('Ctrl Pts',(-22.7024758212538,26.6842111484528,3.19562396212885));
#43156=CARTESIAN_POINT('Ctrl Pts',(-22.2763646369559,26.5113032920142,3.16504511848092));
#43157=CARTESIAN_POINT('Ctrl Pts',(-22.2150410859821,26.4841618004785,3.16064001582726));
#43158=CARTESIAN_POINT('Ctrl Pts',(-22.1306381683155,26.4436103775033,3.15461247963233));
#43159=CARTESIAN_POINT('Ctrl Pts',(-22.1068138473911,26.4317988932988,3.15291518387263));
#43160=CARTESIAN_POINT('Ctrl Pts',(-22.0804351126803,26.4183117238683,3.15104271709831));
#43161=CARTESIAN_POINT('Ctrl Pts',(-22.0777345880461,26.4169261581847,3.15085110340496));
#43162=CARTESIAN_POINT('Ctrl Pts',(-22.0750360153455,26.415536774556,3.15065971150053));
#43163=CARTESIAN_POINT('Ctrl Pts',(-22.0750360171757,26.4155367754983,2.90599376073417));
#43164=CARTESIAN_POINT('Ctrl Pts',(-22.0989936332936,26.4278715625345,2.90780143374778));
#43165=CARTESIAN_POINT('Ctrl Pts',(-22.1231118065676,26.439908887829,2.90961461478517));
#43166=CARTESIAN_POINT('Ctrl Pts',(-22.2949730071992,26.5230063774932,2.92248205540678));
#43167=CARTESIAN_POINT('Ctrl Pts',(-22.4477913926813,26.5830026121293,2.93366489442656));
#43168=CARTESIAN_POINT('Ctrl Pts',(-22.6753219197806,26.652848285626,2.94948805524692));
#43169=CARTESIAN_POINT('Ctrl Pts',(-22.7468652453027,26.6721389103886,2.95434734426875));
#43170=CARTESIAN_POINT('Ctrl Pts',(-22.8504845629538,26.6962796198166,2.96116208954661));
#43171=CARTESIAN_POINT('Ctrl Pts',(-22.8820641421926,26.7031378965749,2.96320960364302));
#43172=CARTESIAN_POINT('Ctrl Pts',(-22.9182408451525,26.7104265526037,2.96551758846153));
#43173=CARTESIAN_POINT('Ctrl Pts',(-22.9227406591764,26.7113231517259,2.96580400383328));
#43174=CARTESIAN_POINT('Ctrl Pts',(-22.9295295812564,26.7126607936927,2.96623510859841));
#43175=CARTESIAN_POINT('Ctrl Pts',(-22.9318172537725,26.7131089628117,2.96638020517512));
#43176=CARTESIAN_POINT('Ctrl Pts',(-22.9359216704411,26.7139084199559,2.96664021603863));
#43177=CARTESIAN_POINT('Ctrl Pts',(-22.9377382269104,26.7142606247488,2.96675518292943));
#43178=CARTESIAN_POINT('Ctrl Pts',(-22.9416533984469,26.7150162234024,2.96700272986064));
#43179=CARTESIAN_POINT('Ctrl Pts',(-22.9437521061084,26.7154190933734,2.96713527922917));
#43180=CARTESIAN_POINT('Ctrl Pts',(-22.9493809484864,26.7164938074274,2.96749039341344));
#43181=CARTESIAN_POINT('Ctrl Pts',(-22.9529118218381,26.7171618376755,2.96771273903431));
#43182=CARTESIAN_POINT('Ctrl Pts',(-22.9689218135657,26.720163150408,2.9687190846058));
#43183=CARTESIAN_POINT('Ctrl Pts',(-22.9814137588918,26.7224286298396,2.96949924911447));
#43184=CARTESIAN_POINT('Ctrl Pts',(-22.9963169188284,26.7250405286924,2.97042434608434));
#43185=CARTESIAN_POINT('Ctrl Pts',(-22.9987153128324,26.7254580660489,2.97057304938576));
#43186=CARTESIAN_POINT('Ctrl Pts',(-23.338424615989,26.7842016761861,2.99161104615214));
#43187=CARTESIAN_POINT('Ctrl Pts',(-23.6829383325917,26.7884295990645,3.00972498877603));
#43188=CARTESIAN_POINT('Ctrl Pts',(-24.1611171660068,26.7177152813727,3.03728306588256));
#43189=CARTESIAN_POINT('Ctrl Pts',(-24.2990017231632,26.6879814838444,3.04549513567131));
#43190=CARTESIAN_POINT('Ctrl Pts',(-24.4483976968447,26.6453554493543,3.0548841515702));
#43191=CARTESIAN_POINT('Ctrl Pts',(-24.462280848853,26.6412929951535,3.05576133633806));
#43192=CARTESIAN_POINT('Ctrl Pts',(-24.4831947751676,26.6350200499408,3.05709000413791));
#43193=CARTESIAN_POINT('Ctrl Pts',(-24.4902462127574,26.6328786441885,3.05753923379858));
#43194=CARTESIAN_POINT('Ctrl Pts',(-24.5016471225592,26.6293736192669,3.05826760596024));
#43195=CARTESIAN_POINT('Ctrl Pts',(-24.5060011828787,26.6280249168593,3.0585462593459));
#43196=CARTESIAN_POINT('Ctrl Pts',(-24.5143424234533,26.6254217488942,3.0590810223188));
#43197=CARTESIAN_POINT('Ctrl Pts',(-24.5183300558334,26.6241687538451,3.0593370831641));
#43198=CARTESIAN_POINT('Ctrl Pts',(-24.5254593581988,26.6219133337678,3.05979562217393));
#43199=CARTESIAN_POINT('Ctrl Pts',(-24.5286019540289,26.6209138358994,3.05999800367246));
#43200=CARTESIAN_POINT('Ctrl Pts',(-24.5348439661779,26.6189180183025,3.06040050024886));
#43201=CARTESIAN_POINT('Ctrl Pts',(-24.5379434182411,26.6179218218997,3.0606006110653));
#43202=CARTESIAN_POINT('Ctrl Pts',(-24.5463935144951,26.6151917383836,3.06114686867473));
#43203=CARTESIAN_POINT('Ctrl Pts',(-24.5517411189934,26.6134485435721,3.06149332248889));
#43204=CARTESIAN_POINT('Ctrl Pts',(-24.5719781460097,26.6067930855152,3.06280730348278));
#43205=CARTESIAN_POINT('Ctrl Pts',(-24.5868360258536,26.6017862499679,3.06377795489912));
#43206=CARTESIAN_POINT('Ctrl Pts',(-24.8327463854409,26.5169157288822,3.07994343978659));
#43207=CARTESIAN_POINT('Ctrl Pts',(-25.0539605128634,26.4111432347182,3.09605415401928));
#43208=CARTESIAN_POINT('Ctrl Pts',(-25.3230185329993,26.2426054918427,3.11748583416924));
#43209=CARTESIAN_POINT('Ctrl Pts',(-25.3836440650742,26.201693485333,3.12244243948128));
#43210=CARTESIAN_POINT('Ctrl Pts',(-25.5016262062503,26.1160927465489,3.13229857733408));
#43211=CARTESIAN_POINT('Ctrl Pts',(-25.5589698419306,26.0714527717369,3.13719555983923));
#43212=CARTESIAN_POINT('Ctrl Pts',(-25.6690725541822,25.9795986749205,3.14675104227998));
#43213=CARTESIAN_POINT('Ctrl Pts',(-25.721885176897,25.9325065096503,3.15140991264535));
#43214=CARTESIAN_POINT('Ctrl Pts',(-25.7937009824346,25.8640946772698,3.15780528426843));
#43215=CARTESIAN_POINT('Ctrl Pts',(-25.8140338233024,25.8442056298425,3.15962306742239));
#43216=CARTESIAN_POINT('Ctrl Pts',(-25.8452067335706,25.8128949073135,3.16241734265421));
#43217=CARTESIAN_POINT('Ctrl Pts',(-25.856230393439,25.8016590773704,3.16340695235446));
#43218=CARTESIAN_POINT('Ctrl Pts',(-25.8697715878855,25.7876534574243,3.16462387567916));
#43219=CARTESIAN_POINT('Ctrl Pts',(-25.8723669515102,25.7849597107478,3.16485717668209));
#43220=CARTESIAN_POINT('Ctrl Pts',(-25.876446058391,25.7807111969685,3.16522393951557));
#43221=CARTESIAN_POINT('Ctrl Pts',(-25.8779329360597,25.7791594647762,3.16535764651394));
#43222=CARTESIAN_POINT('Ctrl Pts',(-25.8807085101094,25.7762570196272,3.16560727086978));
#43223=CARTESIAN_POINT('Ctrl Pts',(-25.881997576392,25.7749066832835,3.16572321708077));
#43224=CARTESIAN_POINT('Ctrl Pts',(-25.8848880389779,25.7718735630103,3.1659832314401));
#43225=CARTESIAN_POINT('Ctrl Pts',(-25.8864887861347,25.7701901709505,3.16612724855639));
#43226=CARTESIAN_POINT('Ctrl Pts',(-25.8905510674399,25.7659088981338,3.16649278303106));
#43227=CARTESIAN_POINT('Ctrl Pts',(-25.8930101042013,25.7633086374679,3.16671410617596));
#43228=CARTESIAN_POINT('Ctrl Pts',(-25.9065191505064,25.7489760099786,3.16793030137597));
#43229=CARTESIAN_POINT('Ctrl Pts',(-25.9174856201728,25.737164702583,3.16891880007298));
#43230=CARTESIAN_POINT('Ctrl Pts',(-26.1448225195932,25.4886002648009,3.18944860111491));
#43231=CARTESIAN_POINT('Ctrl Pts',(-26.3247809329327,25.2208988454348,3.20656226704444));
#43232=CARTESIAN_POINT('Ctrl Pts',(-26.4965209262014,24.858694404708,3.22928268032653));
#43233=CARTESIAN_POINT('Ctrl Pts',(-26.5280903869415,24.7851606868751,3.23386565412394));
#43234=CARTESIAN_POINT('Ctrl Pts',(-26.5768317653921,24.6588569144059,3.24175600984534));
#43235=CARTESIAN_POINT('Ctrl Pts',(-26.5954370196622,24.6066787969809,3.24502057228894));
#43236=CARTESIAN_POINT('Ctrl Pts',(-26.6265686624351,24.5117007622894,3.25098964371017));
#43237=CARTESIAN_POINT('Ctrl Pts',(-26.6395690664385,24.4690706214227,3.25367825951521));
#43238=CARTESIAN_POINT('Ctrl Pts',(-26.6537723117052,24.4187810274552,3.25686540466728));
#43239=CARTESIAN_POINT('Ctrl Pts',(-26.6558371997508,24.4113684593025,3.25733557016836));
#43240=CARTESIAN_POINT('Ctrl Pts',(-26.6589546461619,24.4000203364137,3.25805597734139));
#43241=CARTESIAN_POINT('Ctrl Pts',(-26.6600263320696,24.3960900271323,3.2583055960804));
#43242=CARTESIAN_POINT('Ctrl Pts',(-26.661879781196,24.3892415361533,3.25874075248496));
#43243=CARTESIAN_POINT('Ctrl Pts',(-26.6626649003459,24.3863242611589,3.25892618078188));
#43244=CARTESIAN_POINT('Ctrl Pts',(-26.664295489136,24.3802313394254,3.25931359385866));
#43245=CARTESIAN_POINT('Ctrl Pts',(-26.6651402053918,24.3770554962492,3.25951560287189));
#43246=CARTESIAN_POINT('Ctrl Pts',(-26.6674567397874,24.3682921845604,3.26007323159049));
#43247=CARTESIAN_POINT('Ctrl Pts',(-26.6689183857874,24.36270206147,3.26042918095005));
#43248=CARTESIAN_POINT('Ctrl Pts',(-26.6745557747331,24.3409022637657,3.26181822358134));
#43249=CARTESIAN_POINT('Ctrl Pts',(-26.678620178932,24.3246643084591,3.26285491637539));
#43250=CARTESIAN_POINT('Ctrl Pts',(-26.7428889505068,24.0591347478432,3.27984254051787));
#43251=CARTESIAN_POINT('Ctrl Pts',(-26.7732386265911,23.8036188887567,3.29680855311751));
#43252=CARTESIAN_POINT('Ctrl Pts',(-26.7727849374212,23.3138716996363,3.32991413507576));
#43253=CARTESIAN_POINT('Ctrl Pts',(-26.7472155478491,23.0811683706983,3.345863258448));
#43254=CARTESIAN_POINT('Ctrl Pts',(-26.6936828479454,22.8395052829816,3.36149878070361));
#43255=CARTESIAN_POINT('Ctrl Pts',(-26.6905476061964,22.8257784693161,3.36238346584647));
#43256=CARTESIAN_POINT('Ctrl Pts',(-26.6864664269478,22.8084345404668,3.36349653431896));
#43257=CARTESIAN_POINT('Ctrl Pts',(-26.6856040866437,22.8047982030439,3.36372963668976));
#43258=CARTESIAN_POINT('Ctrl Pts',(-26.6842309005448,22.7990522539057,3.36409754598886));
#43259=CARTESIAN_POINT('Ctrl Pts',(-26.683724248863,22.7969416585863,3.36423259488973));
#43260=CARTESIAN_POINT('Ctrl Pts',(-26.6827782930441,22.7930184890381,3.36448345193259));
#43261=CARTESIAN_POINT('Ctrl Pts',(-26.6823395505057,22.7912057956487,3.36459929161221));
#43262=CARTESIAN_POINT('Ctrl Pts',(-26.681357431404,22.7871634569367,3.36485746433009));
#43263=CARTESIAN_POINT('Ctrl Pts',(-26.6808132479863,22.7849340158538,3.3649997495779));
#43264=CARTESIAN_POINT('Ctrl Pts',(-26.679215391581,22.7784180491853,3.36541530971551));
#43265=CARTESIAN_POINT('Ctrl Pts',(-26.6781552873184,22.7741330828651,3.36568821209387));
#43266=CARTESIAN_POINT('Ctrl Pts',(-26.6703930846981,22.7430323040894,3.36766634000781));
#43267=CARTESIAN_POINT('Ctrl Pts',(-26.6633547838917,22.7163004601444,3.36935238514386));
#43268=CARTESIAN_POINT('Ctrl Pts',(-26.6397348684566,22.6310603779597,3.37469282748858));
#43269=CARTESIAN_POINT('Ctrl Pts',(-26.6218401306455,22.5729266118457,3.37828064645739));
#43270=CARTESIAN_POINT('Ctrl Pts',(-26.5754546339251,22.4361325727833,3.38666882186064));
#43271=CARTESIAN_POINT('Ctrl Pts',(-26.5455255254633,22.3580058285708,3.39141631390109));
#43272=CARTESIAN_POINT('Ctrl Pts',(-26.4102190307824,22.0421790549289,3.41075047897424));
#43273=CARTESIAN_POINT('Ctrl Pts',(-26.2793234251647,21.8165107777194,3.42499384675426));
#43274=CARTESIAN_POINT('Ctrl Pts',(-26.1144895840033,21.5980758638406,3.44105155145121));
#43275=CARTESIAN_POINT('Ctrl Pts',(-26.106164409712,21.5871886338585,3.44185814348597));
#43276=CARTESIAN_POINT('Ctrl Pts',(-26.090901814393,21.5674906867641,3.44332917448825));
#43277=CARTESIAN_POINT('Ctrl Pts',(-26.0839873437853,21.5586624109682,3.44399278938118));
#43278=CARTESIAN_POINT('Ctrl Pts',(-26.0739568549818,21.5459924397679,3.44495155256351));
#43279=CARTESIAN_POINT('Ctrl Pts',(-26.0708777999388,21.5421214891154,3.44524533911121));
#43280=CARTESIAN_POINT('Ctrl Pts',(-26.0634600459117,21.5328399184325,3.44595185960675));
#43281=CARTESIAN_POINT('Ctrl Pts',(-26.0591127814491,21.5274362009849,3.44636491180175));
#43282=CARTESIAN_POINT('Ctrl Pts',(-26.0535114783011,21.5205195270943,3.44689584336933));
#43283=CARTESIAN_POINT('Ctrl Pts',(-26.0522734297748,21.5189935995851,3.44701311519233));
#43284=CARTESIAN_POINT('Ctrl Pts',(-26.0475829044676,21.5132231978584,3.44745711819831));
#43285=CARTESIAN_POINT('Ctrl Pts',(-26.0441210301028,21.5089864025998,3.44778420746588));
#43286=CARTESIAN_POINT('Ctrl Pts',(-26.0388206087923,21.5025331219345,3.44828409255519));
#43287=CARTESIAN_POINT('Ctrl Pts',(-26.0369898410376,21.500310237458,3.44845658730477));
#43288=CARTESIAN_POINT('Ctrl Pts',(-26.0226246224643,21.4829158161413,3.44980878919475));
#43289=CARTESIAN_POINT('Ctrl Pts',(-26.0099546338039,21.4678571817102,3.45099375932787));
#43290=CARTESIAN_POINT('Ctrl Pts',(-25.984304473937,21.4379319668035,3.4533782163696));
#43291=CARTESIAN_POINT('Ctrl Pts',(-25.9713240850451,21.4230667069491,3.45457768286575));
#43292=CARTESIAN_POINT('Ctrl Pts',(-25.9541047369771,21.4037087382997,3.4561598893506));
#43293=CARTESIAN_POINT('Ctrl Pts',(-25.9499880415281,21.3991074496954,3.45653749162365));
#43294=CARTESIAN_POINT('Ctrl Pts',(-25.9436066407195,21.3920159827923,3.45712181611206));
#43295=CARTESIAN_POINT('Ctrl Pts',(-25.9413511980089,21.3895174576939,3.45732814670621));
#43296=CARTESIAN_POINT('Ctrl Pts',(-25.9368469877599,21.3845434908558,3.4577398154555));
#43297=CARTESIAN_POINT('Ctrl Pts',(-25.9345982728858,21.3820680068852,3.45794515124021));
#43298=CARTESIAN_POINT('Ctrl Pts',(-25.9295975943158,21.3765802282549,3.45840136008007));
#43299=CARTESIAN_POINT('Ctrl Pts',(-25.9268437586165,21.3735696540953,3.45865231263446));
#43300=CARTESIAN_POINT('Ctrl Pts',(-25.9188598286573,21.3648746004018,3.45937907795272));
#43301=CARTESIAN_POINT('Ctrl Pts',(-25.9136150316124,21.3592037138624,3.45985551856304));
#43302=CARTESIAN_POINT('Ctrl Pts',(-25.8775357133785,21.320473565285,3.46312634969951));
#43303=CARTESIAN_POINT('Ctrl Pts',(-25.8460302493492,21.288048831281,3.46594959421429));
#43304=CARTESIAN_POINT('Ctrl Pts',(-25.7571780974443,21.200372303213,3.47382793989629));
#43305=CARTESIAN_POINT('Ctrl Pts',(-25.698452900415,21.1465697393773,3.47894351358443));
#43306=CARTESIAN_POINT('Ctrl Pts',(-25.4101861273518,20.9014745697645,3.50363535933499));
#43307=CARTESIAN_POINT('Ctrl Pts',(-25.1568140257935,20.740573695822,3.52431361361684));
#43308=CARTESIAN_POINT('Ctrl Pts',(-24.8037581919339,20.5799333364377,3.54996096298823));
#43309=CARTESIAN_POINT('Ctrl Pts',(-24.7210681482117,20.5463772350149,3.55575003065747));
#43310=CARTESIAN_POINT('Ctrl Pts',(-24.631058342462,20.5141337379637,3.56174377971457));
#43311=CARTESIAN_POINT('Ctrl Pts',(-24.6250262094685,20.5119931495046,3.56214399984));
#43312=CARTESIAN_POINT('Ctrl Pts',(-24.6166520601033,20.5090495234321,3.56269754664557));
#43313=CARTESIAN_POINT('Ctrl Pts',(-24.6143154873417,20.5082312105701,3.56285177628456));
#43314=CARTESIAN_POINT('Ctrl Pts',(-24.6102978352894,20.5068293466376,3.56311658400636));
#43315=CARTESIAN_POINT('Ctrl Pts',(-24.6086172160655,20.5062444955804,3.56322723986907));
#43316=CARTESIAN_POINT('Ctrl Pts',(-24.6051806019271,20.5050517530652,3.56345327711326));
#43317=CARTESIAN_POINT('Ctrl Pts',(-24.6034245691066,20.5044439895902,3.56356865028646));
#43318=CARTESIAN_POINT('Ctrl Pts',(-24.5993235463136,20.5030285950582,3.5638377976133));
#43319=CARTESIAN_POINT('Ctrl Pts',(-24.5969781420184,20.5022221495437,3.56399150063066));
#43320=CARTESIAN_POINT('Ctrl Pts',(-24.592024761747,20.5005253672808,3.56431564532827));
#43321=CARTESIAN_POINT('Ctrl Pts',(-24.5894165679321,20.4996356657809,3.5644860492163));
#43322=CARTESIAN_POINT('Ctrl Pts',(-24.5824183056959,20.4972584500192,3.56494254777384));
#43323=CARTESIAN_POINT('Ctrl Pts',(-24.5780261434918,20.4957770527809,3.56522828388908));
#43324=CARTESIAN_POINT('Ctrl Pts',(-24.4733063868518,20.4607084126243,3.57202303196094));
#43325=CARTESIAN_POINT('Ctrl Pts',(-24.3713759377099,20.4320682803523,3.57824640516057));
#43326=CARTESIAN_POINT('Ctrl Pts',(-23.8874125799282,20.3214726556528,3.60677963174904));
#43327=CARTESIAN_POINT('Ctrl Pts',(-23.4939872160089,20.3043982820673,3.62751379813933));
#43328=CARTESIAN_POINT('Ctrl Pts',(-23.0878489475399,20.3607892981768,3.65232537993949));
#43329=CARTESIAN_POINT('Ctrl Pts',(-23.0686868977944,20.3636262110622,3.65350287765477));
#43330=CARTESIAN_POINT('Ctrl Pts',(-23.0434975922354,20.3675878375705,3.6550601533472));
#43331=CARTESIAN_POINT('Ctrl Pts',(-23.0374460393098,20.3685572878916,3.65543499385223));
#43332=CARTESIAN_POINT('Ctrl Pts',(-23.0280842915022,20.3700844292698,3.65601599264663));
#43333=CARTESIAN_POINT('Ctrl Pts',(-23.0247721180224,20.3706300438108,3.65622176656641));
#43334=CARTESIAN_POINT('Ctrl Pts',(-23.018490897518,20.3716748322579,3.65661241186834));
#43335=CARTESIAN_POINT('Ctrl Pts',(-23.0155216837761,20.3721729941241,3.65679725084986));
#43336=CARTESIAN_POINT('Ctrl Pts',(-23.008657000496,20.3733346136517,3.65722499883446));
#43337=CARTESIAN_POINT('Ctrl Pts',(-23.0047620503207,20.3740010756688,3.65746800329421));
#43338=CARTESIAN_POINT('Ctrl Pts',(-22.993844864898,20.3758897804332,3.65814998215052));
#43339=CARTESIAN_POINT('Ctrl Pts',(-22.9868254764664,20.3771281533579,3.65858947010189));
#43340=CARTESIAN_POINT('Ctrl Pts',(-22.9462081383265,20.384432960337,3.66113838770059));
#43341=CARTESIAN_POINT('Ctrl Pts',(-22.91270522459,20.3910095093719,3.66326404451808));
#43342=CARTESIAN_POINT('Ctrl Pts',(-22.816316937916,20.4115259499161,3.66944929255788));
#43343=CARTESIAN_POINT('Ctrl Pts',(-22.7537398199039,20.4268197149286,3.67355144717675));
#43344=CARTESIAN_POINT('Ctrl Pts',(-22.6152221601491,20.4651065181626,3.68283001773376));
#43345=CARTESIAN_POINT('Ctrl Pts',(-22.5395891295429,20.4890492258005,3.68803245350386));
#43346=CARTESIAN_POINT('Ctrl Pts',(-22.2032172980128,20.60935750785,3.711752463771));
#43347=CARTESIAN_POINT('Ctrl Pts',(-21.9547430153838,20.7364108178673,3.7310071596857));
#43348=CARTESIAN_POINT('Ctrl Pts',(-21.7222791946736,20.8960769848946,3.7493814562276));
#43349=CARTESIAN_POINT('Ctrl Pts',(-21.7189058500562,20.8984034247394,3.74964814709278));
#43350=CARTESIAN_POINT('Ctrl Pts',(-21.7097477079703,20.9047451809933,3.75037230906987));
#43351=CARTESIAN_POINT('Ctrl Pts',(-21.7039715858007,20.9087730562375,3.75082919126555));
#43352=CARTESIAN_POINT('Ctrl Pts',(-21.6971329620578,20.9135752380434,3.75137024776383));
#43353=CARTESIAN_POINT('Ctrl Pts',(-21.6960577209558,20.9143312707183,3.75145532230284));
#43354=CARTESIAN_POINT('Ctrl Pts',(-21.6863305929269,20.9211795886739,3.75222497897567));
#43355=CARTESIAN_POINT('Ctrl Pts',(-21.677708182226,20.9273138746077,3.75290746220585));
#43356=CARTESIAN_POINT('Ctrl Pts',(-21.6392266719494,20.9549774434047,3.75595387394875));
#43357=CARTESIAN_POINT('Ctrl Pts',(-21.6097060318157,20.976975983963,3.75829230266712));
#43358=CARTESIAN_POINT('Ctrl Pts',(-21.5765024389841,21.0026154874384,3.76091800778069));
#43359=CARTESIAN_POINT('Ctrl Pts',(-21.5724450702153,21.0057640597365,3.76123878267264));
#43360=CARTESIAN_POINT('Ctrl Pts',(-21.5664622907775,21.0104297325702,3.76171164353632));
#43361=CARTESIAN_POINT('Ctrl Pts',(-21.5645310822991,21.0119393326553,3.76186425932182));
#43362=CARTESIAN_POINT('Ctrl Pts',(-21.5611510260122,21.0145876960961,3.76213133197922));
#43363=CARTESIAN_POINT('Ctrl Pts',(-21.5597014315771,21.0157254996255,3.76224585769051));
#43364=CARTESIAN_POINT('Ctrl Pts',(-21.5566832311632,21.0180987067509,3.76248428365919));
#43365=CARTESIAN_POINT('Ctrl Pts',(-21.5551148001493,21.0193343225431,3.76260816800031));
#43366=CARTESIAN_POINT('Ctrl Pts',(-21.5519161416613,21.0218590587136,3.76286078834076));
#43367=CARTESIAN_POINT('Ctrl Pts',(-21.5502860104783,21.0231483003624,3.762989515532));
#43368=CARTESIAN_POINT('Ctrl Pts',(-21.5462970605318,21.026309366763,3.76330447734419));
#43369=CARTESIAN_POINT('Ctrl Pts',(-21.5439396100811,21.0281829269951,3.76349058814814));
#43370=CARTESIAN_POINT('Ctrl Pts',(-21.5374700555604,21.0333393522846,3.76400126022353));
#43371=CARTESIAN_POINT('Ctrl Pts',(-21.5333633374887,21.0366290061587,3.76432534243849));
#43372=CARTESIAN_POINT('Ctrl Pts',(-21.3851974835405,21.1559129780184,3.77601572596151));
#43373=CARTESIAN_POINT('Ctrl Pts',(-21.2513569883429,21.2841044578798,3.78651131054078));
#43374=CARTESIAN_POINT('Ctrl Pts',(-20.9243157965346,21.6563241458144,3.81429830373962));
#43375=CARTESIAN_POINT('Ctrl Pts',(-20.7541959166598,21.9179061362556,3.83138930546549));
#43376=CARTESIAN_POINT('Ctrl Pts',(-20.6162521152359,22.2167943651935,3.85131593533221));
#43377=CARTESIAN_POINT('Ctrl Pts',(-20.6085438388796,22.233886674851,3.85245595033117));
#43378=CARTESIAN_POINT('Ctrl Pts',(-20.598546474435,22.2565812012038,3.85397058952886));
#43379=CARTESIAN_POINT('Ctrl Pts',(-20.596123279732,22.2621242299689,3.85434060862077));
#43380=CARTESIAN_POINT('Ctrl Pts',(-20.5923861349425,22.2707389120592,3.85491580189394));
#43381=CARTESIAN_POINT('Ctrl Pts',(-20.5910613209305,22.2738058614927,3.85512060422722));
#43382=CARTESIAN_POINT('Ctrl Pts',(-20.5884187769462,22.2799495856547,3.85553091812981));
#43383=CARTESIAN_POINT('Ctrl Pts',(-20.5871010664563,22.2830263642695,3.8557364300579));
#43384=CARTESIAN_POINT('Ctrl Pts',(-20.5841704247533,22.2898988091019,3.85619553368689));
#43385=CARTESIAN_POINT('Ctrl Pts',(-20.5825599836731,22.2936955248956,3.85644920989676));
#43386=CARTESIAN_POINT('Ctrl Pts',(-20.5778730420384,22.3048045533091,3.85719158505529));
#43387=CARTESIAN_POINT('Ctrl Pts',(-20.5748162648527,22.3121251079005,3.85768095427069));
#43388=CARTESIAN_POINT('Ctrl Pts',(-20.5526661930566,22.3657272080596,3.86126548134028));
#43389=CARTESIAN_POINT('Ctrl Pts',(-20.534627554023,22.4124346033218,3.86439616792427));
#43390=CARTESIAN_POINT('Ctrl Pts',(-20.4794067766693,22.5659681108591,3.87471834383338));
#43391=CARTESIAN_POINT('Ctrl Pts',(-20.4467616862768,22.6743249018979,3.88205519070347));
#43392=CARTESIAN_POINT('Ctrl Pts',(-20.3394064415919,23.1129968649152,3.91192138687688));
#43393=CARTESIAN_POINT('Ctrl Pts',(-20.3112506221036,23.4524204255987,3.93564606072539));
#43394=CARTESIAN_POINT('Ctrl Pts',(-20.3367002153579,23.793587883721,3.95727599795235));
#43395=CARTESIAN_POINT('Ctrl Pts',(-20.3369746884962,23.7971858952935,3.95750383124104));
#43396=CARTESIAN_POINT('Ctrl Pts',(-20.3381917518322,23.812794432353,3.95849095884233));
#43397=CARTESIAN_POINT('Ctrl Pts',(-20.3391956584141,23.8248002882222,3.95924706665686));
#43398=CARTESIAN_POINT('Ctrl Pts',(-20.340583706471,23.8403495697253,3.96022196894315));
#43399=CARTESIAN_POINT('Ctrl Pts',(-20.3409064152843,23.8438981760711,3.96044416319671));
#43400=CARTESIAN_POINT('Ctrl Pts',(-20.3414101259311,23.8493371074322,3.96078425969256));
#43401=CARTESIAN_POINT('Ctrl Pts',(-20.3415869128891,23.851227805113,3.9609023999086));
#43402=CARTESIAN_POINT('Ctrl Pts',(-20.3419370785004,23.8549373748143,3.96113402374322));
#43403=CARTESIAN_POINT('Ctrl Pts',(-20.3421103319471,23.8567562462978,3.96124751349687));
#43404=CARTESIAN_POINT('Ctrl Pts',(-20.3424820801453,23.8606241323027,3.96148868377151));
#43405=CARTESIAN_POINT('Ctrl Pts',(-20.3426809907617,23.862673097843,3.96161634002559));
#43406=CARTESIAN_POINT('Ctrl Pts',(-20.3431081756265,23.8670300891329,3.96188758106753));
#43407=CARTESIAN_POINT('Ctrl Pts',(-20.3433369785467,23.8693380635095,3.96203113585575));
#43408=CARTESIAN_POINT('Ctrl Pts',(-20.3439261173171,23.8752161643368,3.96239643338741));
#43409=CARTESIAN_POINT('Ctrl Pts',(-20.3442899257933,23.8787859515027,3.96261798145719));
#43410=CARTESIAN_POINT('Ctrl Pts',(-20.3453526601469,23.8890439064318,3.96325377255932));
#43411=CARTESIAN_POINT('Ctrl Pts',(-20.3460665631807,23.8957305531389,3.96366718882883));
#43412=CARTESIAN_POINT('Ctrl Pts',(-20.3485304899675,23.9181437007368,3.96504964159991));
#43413=CARTESIAN_POINT('Ctrl Pts',(-20.3503754389167,23.9338598293908,3.96601358795155));
#43414=CARTESIAN_POINT('Ctrl Pts',(-20.3585526188446,23.9993477131949,3.97000998438442));
#43415=CARTESIAN_POINT('Ctrl Pts',(-20.3659312616306,24.0489843886988,3.97299012986646));
#43416=CARTESIAN_POINT('Ctrl Pts',(-20.3818638631928,24.1412873571795,3.97847394052762));
#43417=CARTESIAN_POINT('Ctrl Pts',(-20.3901283274464,24.1839908148912,3.98098757985366));
#43418=CARTESIAN_POINT('Ctrl Pts',(-20.4453666258353,24.4413696441169,3.99606445192876));
#43419=CARTESIAN_POINT('Ctrl Pts',(-20.5133331291118,24.6509502885966,4.00807066484408));
#43420=CARTESIAN_POINT('Ctrl Pts',(-20.6717987308724,25.0098398122419,4.0303154867419));
#43421=CARTESIAN_POINT('Ctrl Pts',(-20.7540493506933,25.1618126135886,4.04033648725274));
#43422=CARTESIAN_POINT('Ctrl Pts',(-20.854311140483,25.3160807320288,4.05152515961816));
#43423=CARTESIAN_POINT('Ctrl Pts',(-20.8606151263234,25.3256679310502,4.05222482607548));
#43424=CARTESIAN_POINT('Ctrl Pts',(-20.8694288159792,25.338917249863,4.0531978547721));
#43425=CARTESIAN_POINT('Ctrl Pts',(-20.871895143431,25.3426082355589,4.05346958144129));
#43426=CARTESIAN_POINT('Ctrl Pts',(-20.8761499152968,25.3489473280607,4.05393740255234));
#43427=CARTESIAN_POINT('Ctrl Pts',(-20.8779346915595,25.3515978996585,4.05413335809062));
#43428=CARTESIAN_POINT('Ctrl Pts',(-20.8816206269563,25.357054348965,4.05453746466929));
#43429=CARTESIAN_POINT('Ctrl Pts',(-20.8835222752581,25.3598598894239,4.05474563407942));
#43430=CARTESIAN_POINT('Ctrl Pts',(-20.8879488883533,25.3663684313172,4.05522947367786));
#43431=CARTESIAN_POINT('Ctrl Pts',(-20.8904771546482,25.3700691690357,4.05550526918002));
#43432=CARTESIAN_POINT('Ctrl Pts',(-20.8985173043973,25.381785352917,4.05638059725024));
#43433=CARTESIAN_POINT('Ctrl Pts',(-20.9040577243792,25.3897810662143,4.05698121768391));
#43434=CARTESIAN_POINT('Ctrl Pts',(-20.9987342331777,25.5251015873525,4.06720202409792));
#43435=CARTESIAN_POINT('Ctrl Pts',(-21.096915653646,25.6458191565422,4.07717744811887));
#43436=CARTESIAN_POINT('Ctrl Pts',(-21.2319959830646,25.7893470291109,4.09019124602269));
#43437=CARTESIAN_POINT('Ctrl Pts',(-21.2611708203737,25.819164678529,4.09296371721845));
#43438=CARTESIAN_POINT('Ctrl Pts',(-21.3172920720689,25.8743380074061,4.09822205952632));
#43439=CARTESIAN_POINT('Ctrl Pts',(-21.3441127154999,25.899812645873,4.10070444321883));
#43440=CARTESIAN_POINT('Ctrl Pts',(-21.5661230513116,26.1035278711038,4.12099008508655));
#43441=CARTESIAN_POINT('Ctrl Pts',(-21.7821357923939,26.2576066670105,4.139206332941));
#43442=CARTESIAN_POINT('Ctrl Pts',(-22.0179677358209,26.3854308282318,4.15616683921355));
#43443=CARTESIAN_POINT('Ctrl Pts',(-22.0213881378354,26.3872767357445,4.15641222829118));
#43444=CARTESIAN_POINT('Ctrl Pts',(-22.0352751995457,26.3947388363725,4.15740607305866));
#43445=CARTESIAN_POINT('Ctrl Pts',(-22.0457697075401,26.4003034254026,4.15815148661553));
#43446=CARTESIAN_POINT('Ctrl Pts',(-22.0594348432145,26.4074526891524,4.15911456945468));
#43447=CARTESIAN_POINT('Ctrl Pts',(-22.0625774768617,26.4090902416001,4.15933553887004));
#43448=CARTESIAN_POINT('Ctrl Pts',(-22.0674047988322,26.4115955301246,4.15967416709459));
#43449=CARTESIAN_POINT('Ctrl Pts',(-22.0690875492545,26.4124669625778,4.15979206065166));
#43450=CARTESIAN_POINT('Ctrl Pts',(-22.0721921739013,26.4140712585016,4.16000929574724));
#43451=CARTESIAN_POINT('Ctrl Pts',(-22.0736138177173,26.414804543736,4.16010866388677));
#43452=CARTESIAN_POINT('Ctrl Pts',(-22.0750360153459,26.4155367745562,4.16020796448761));
#43453=CARTESIAN_POINT('Origin',(-23.5502525316942,23.5502525316942,-77.3107734492734));
#43454=CARTESIAN_POINT('',(-22.0750360153137,26.4155367745396,5.65630390104212));
#43455=CARTESIAN_POINT('',(-22.0750360281848,26.4155367811664,5.40632238256859));
#43456=CARTESIAN_POINT('',(-22.0750360153461,26.4155367745563,-77.3107734492734));
#43457=CARTESIAN_POINT('Ctrl Pts',(-22.0750360153137,26.4155367745396,5.65630390104212));
#43458=CARTESIAN_POINT('Ctrl Pts',(-22.0290555371617,26.3918633253974,5.65326402867864));
#43459=CARTESIAN_POINT('Ctrl Pts',(-21.9836533856863,26.3670874447904,5.65019038681477));
#43460=CARTESIAN_POINT('Ctrl Pts',(-21.9220268220882,26.3315070678986,5.64590801223686));
#43461=CARTESIAN_POINT('Ctrl Pts',(-21.9052737229307,26.3216313311224,5.64473237729546));
#43462=CARTESIAN_POINT('Ctrl Pts',(-21.8770031911469,26.3046195638544,5.64272842066564));
#43463=CARTESIAN_POINT('Ctrl Pts',(-21.8654393787476,26.297561348404,5.64190294107446));
#43464=CARTESIAN_POINT('Ctrl Pts',(-21.8495744331906,26.2877400102614,5.64076231185462));
#43465=CARTESIAN_POINT('Ctrl Pts',(-21.8452347430775,26.2850391833485,5.64044946276797));
#43466=CARTESIAN_POINT('Ctrl Pts',(-21.8382460655568,26.2806666457264,5.63994428065526));
#43467=CARTESIAN_POINT('Ctrl Pts',(-21.8355930457878,26.2790013698037,5.63975218623473));
#43468=CARTESIAN_POINT('Ctrl Pts',(-21.8300692858842,26.2755229205012,5.63935156614846));
#43469=CARTESIAN_POINT('Ctrl Pts',(-21.8271989762515,26.2737090737028,5.6391430156384));
#43470=CARTESIAN_POINT('Ctrl Pts',(-21.8205784774395,26.2695106986353,5.63866111168083));
#43471=CARTESIAN_POINT('Ctrl Pts',(-21.8168303497589,26.2671229465827,5.63838763844325));
#43472=CARTESIAN_POINT('Ctrl Pts',(-21.8067944655993,26.2607003452975,5.63765364663537));
#43473=CARTESIAN_POINT('Ctrl Pts',(-21.80051580883,26.2566513895219,5.63719260179465));
#43474=CARTESIAN_POINT('Ctrl Pts',(-21.7564776375493,26.2280349233244,5.63394578047632));
#43475=CARTESIAN_POINT('Ctrl Pts',(-21.7192244018785,26.2027009408788,5.63113130114599));
#43476=CARTESIAN_POINT('Ctrl Pts',(-21.6813756207168,26.1757845942994,5.62819899730163));
#43477=CARTESIAN_POINT('Ctrl Pts',(-21.6802359199613,26.1749729724241,5.62811063084494));
#43478=CARTESIAN_POINT('Ctrl Pts',(-21.6687946382393,26.166813989787,5.62722283924283));
#43479=CARTESIAN_POINT('Ctrl Pts',(-21.658536002613,26.1594068458606,5.62642115899545));
#43480=CARTESIAN_POINT('Ctrl Pts',(-21.6451110695161,26.1495927143785,5.62536455012179));
#43481=CARTESIAN_POINT('Ctrl Pts',(-21.6419051279042,26.1472399329827,5.6251116611497));
#43482=CARTESIAN_POINT('Ctrl Pts',(-21.6346883916467,26.1419231241593,5.62454111795175));
#43483=CARTESIAN_POINT('Ctrl Pts',(-21.6306801125763,26.1389557131734,5.624223337541));
#43484=CARTESIAN_POINT('Ctrl Pts',(-21.6080008173527,26.1220841307784,5.62242022863408));
#43485=CARTESIAN_POINT('Ctrl Pts',(-21.5894743734467,26.1079875582406,5.62092775291979));
#43486=CARTESIAN_POINT('Ctrl Pts',(-21.3394783174193,25.9134558177032,5.60052000821524));
#43487=CARTESIAN_POINT('Ctrl Pts',(-21.1335827520115,25.7024383207263,5.58036746222942));
#43488=CARTESIAN_POINT('Ctrl Pts',(-20.9327473112214,25.4308780225437,5.55774902135405));
#43489=CARTESIAN_POINT('Ctrl Pts',(-20.907105669774,25.3946659202274,5.55479578657131));
#43490=CARTESIAN_POINT('Ctrl Pts',(-20.8494464113194,25.3095642213742,5.54801767184724));
#43491=CARTESIAN_POINT('Ctrl Pts',(-20.8179929185352,25.2603079844279,5.5442142317708));
#43492=CARTESIAN_POINT('Ctrl Pts',(-20.7737856529536,25.1867425264889,5.53873623290542));
#43493=CARTESIAN_POINT('Ctrl Pts',(-20.7599764333682,25.1630845904282,5.53700438566315));
#43494=CARTESIAN_POINT('Ctrl Pts',(-20.7442987529375,25.1354214014504,5.53501627526534));
#43495=CARTESIAN_POINT('Ctrl Pts',(-20.742135367224,25.1315858126066,5.53474143388893));
#43496=CARTESIAN_POINT('Ctrl Pts',(-20.7388576392711,25.1257466057406,5.53432427637956));
#43497=CARTESIAN_POINT('Ctrl Pts',(-20.7377375732026,25.1237462326153,5.53418159146706));
#43498=CARTESIAN_POINT('Ctrl Pts',(-20.7357103094844,25.120116576581,5.53392309830465));
#43499=CARTESIAN_POINT('Ctrl Pts',(-20.7348023943846,25.1184877067895,5.53380724372401));
#43500=CARTESIAN_POINT('Ctrl Pts',(-20.7329781361281,25.1152081562906,5.5335742823345));
#43501=CARTESIAN_POINT('Ctrl Pts',(-20.7320618333631,25.1135574650815,5.53345717825035));
#43502=CARTESIAN_POINT('Ctrl Pts',(-20.7294465949341,25.1088364219725,5.53312268746577));
#43503=CARTESIAN_POINT('Ctrl Pts',(-20.7277512159577,25.1057640870484,5.53290553066963));
#43504=CARTESIAN_POINT('Ctrl Pts',(-20.7204804460373,25.0925371056361,5.53197284326336));
#43505=CARTESIAN_POINT('Ctrl Pts',(-20.7149547217813,25.0823550421389,5.53126046884061));
#43506=CARTESIAN_POINT('Ctrl Pts',(-20.6208842135392,24.906762571205,5.51906760304813));
#43507=CARTESIAN_POINT('Ctrl Pts',(-20.5468806858322,24.7339325257884,5.50845904945429));
#43508=CARTESIAN_POINT('Ctrl Pts',(-20.3976991786451,24.2795893993786,5.48167090548814));
#43509=CARTESIAN_POINT('Ctrl Pts',(-20.3448158713582,23.9926108723074,5.46562888911613));
#43510=CARTESIAN_POINT('Ctrl Pts',(-20.330186488909,23.6831612581514,5.44698339788424));
#43511=CARTESIAN_POINT('Ctrl Pts',(-20.3294483047411,23.6638754004049,5.44581656451247));
#43512=CARTESIAN_POINT('Ctrl Pts',(-20.3286165705855,23.6354722421496,5.44409062720214));
#43513=CARTESIAN_POINT('Ctrl Pts',(-20.3283884041776,23.6263590761697,5.44353572553851));
#43514=CARTESIAN_POINT('Ctrl Pts',(-20.328046419847,23.6099111138717,5.44253211032834));
#43515=CARTESIAN_POINT('Ctrl Pts',(-20.3279189735424,23.6025766395024,5.44208382596923));
#43516=CARTESIAN_POINT('Ctrl Pts',(-20.3277610720437,23.5912666756295,5.44139137794753));
#43517=CARTESIAN_POINT('Ctrl Pts',(-20.3277129295015,23.5872914247429,5.4411477698532));
#43518=CARTESIAN_POINT('Ctrl Pts',(-20.3276378447444,23.5799732007256,5.44069888250149));
#43519=CARTESIAN_POINT('Ctrl Pts',(-20.3276087483241,23.576630251152,5.44049367116951));
#43520=CARTESIAN_POINT('Ctrl Pts',(-20.327560699023,23.5699079297802,5.44008068751993));
#43521=CARTESIAN_POINT('Ctrl Pts',(-20.3275418599535,23.5665285616103,5.43987291188821));
#43522=CARTESIAN_POINT('Ctrl Pts',(-20.3275033594944,23.5569077395582,5.43928091559561));
#43523=CARTESIAN_POINT('Ctrl Pts',(-20.327496514456,23.5506662749142,5.43889629300001));
#43524=CARTESIAN_POINT('Ctrl Pts',(-20.3275444873398,23.5241369006475,5.43725900987204));
#43525=CARTESIAN_POINT('Ctrl Pts',(-20.3277727487906,23.5038501201218,5.43600091680612));
#43526=CARTESIAN_POINT('Ctrl Pts',(-20.335385436394,23.1360249844661,5.41307611634389));
#43527=CARTESIAN_POINT('Ctrl Pts',(-20.3987641518351,22.7920002538353,5.38941409065657));
#43528=CARTESIAN_POINT('Ctrl Pts',(-20.5617834670544,22.3362375273107,5.35684324650837));
#43529=CARTESIAN_POINT('Ctrl Pts',(-20.6159303714036,22.2106471948495,5.34777554819578));
#43530=CARTESIAN_POINT('Ctrl Pts',(-20.6849828356838,22.0749249104377,5.3381457576323));
#43531=CARTESIAN_POINT('Ctrl Pts',(-20.6921742673289,22.0610411030107,5.33716279019482));
#43532=CARTESIAN_POINT('Ctrl Pts',(-20.7012072815686,22.0439083961411,5.33595295100066));
#43533=CARTESIAN_POINT('Ctrl Pts',(-20.7029536785057,22.0406099471909,5.3357201739217));
#43534=CARTESIAN_POINT('Ctrl Pts',(-20.7057138133191,22.0354186620876,5.33535405447914));
#43535=CARTESIAN_POINT('Ctrl Pts',(-20.7067237126433,22.0335238057401,5.33522046835777));
#43536=CARTESIAN_POINT('Ctrl Pts',(-20.7086152413127,22.0299832930941,5.33497096030692));
#43537=CARTESIAN_POINT('Ctrl Pts',(-20.7094964009972,22.0283374046735,5.33485500975453));
#43538=CARTESIAN_POINT('Ctrl Pts',(-20.7114782940145,22.0246432117581,5.33459484571123));
#43539=CARTESIAN_POINT('Ctrl Pts',(-20.712579811939,22.0225953367582,5.33445068353273));
#43540=CARTESIAN_POINT('Ctrl Pts',(-20.7153859646446,22.017391816128,5.33408452383512));
#43541=CARTESIAN_POINT('Ctrl Pts',(-20.7170936577156,22.0142378112623,5.33386272169738));
#43542=CARTESIAN_POINT('Ctrl Pts',(-20.7265508734569,21.9968403396303,5.33263998770461));
#43543=CARTESIAN_POINT('Ctrl Pts',(-20.7344027253136,21.9826523316972,5.33164550949222));
#43544=CARTESIAN_POINT('Ctrl Pts',(-20.8902436320566,21.7060029390145,5.31229517157563));
#43545=CARTESIAN_POINT('Ctrl Pts',(-21.0742377628744,21.4654685624687,5.29609217544438));
#43546=CARTESIAN_POINT('Ctrl Pts',(-21.4261247533412,21.1189501079005,5.2682346732949));
#43547=CARTESIAN_POINT('Ctrl Pts',(-21.5750374737539,20.9964986457951,5.25713202745246));
#43548=CARTESIAN_POINT('Ctrl Pts',(-21.7408270830447,20.8833880680165,5.24493138213758));
#43549=CARTESIAN_POINT('Ctrl Pts',(-21.7477048423628,20.8787345460701,5.24442557175939));
#43550=CARTESIAN_POINT('Ctrl Pts',(-21.7587089424675,20.8713509639663,5.24361679259769));
#43551=CARTESIAN_POINT('Ctrl Pts',(-21.7628237490258,20.8686037127524,5.24331447231518));
#43552=CARTESIAN_POINT('Ctrl Pts',(-21.7706609175496,20.8633972782554,5.24273886545928));
#43553=CARTESIAN_POINT('Ctrl Pts',(-21.7743820947898,20.8609363254668,5.24246564624699));
#43554=CARTESIAN_POINT('Ctrl Pts',(-21.7808980956154,20.8566464732773,5.24198736743706));
#43555=CARTESIAN_POINT('Ctrl Pts',(-21.7836906810652,20.8548141728779,5.24178243594389));
#43556=CARTESIAN_POINT('Ctrl Pts',(-21.7891329981473,20.8512553933314,5.24138314357982));
#43557=CARTESIAN_POINT('Ctrl Pts',(-21.7917824336377,20.8495284661049,5.24118879979639));
#43558=CARTESIAN_POINT('Ctrl Pts',(-21.7980518671788,20.8454551263698,5.24072901131145));
#43559=CARTESIAN_POINT('Ctrl Pts',(-21.8016740367922,20.8431120810594,5.24046344105088));
#43560=CARTESIAN_POINT('Ctrl Pts',(-21.8124507394307,20.8361716897949,5.23967352376699));
#43561=CARTESIAN_POINT('Ctrl Pts',(-21.8196187351081,20.8315954099799,5.23914839268551));
#43562=CARTESIAN_POINT('Ctrl Pts',(-21.8853170035304,20.7900166304407,5.2343376368014));
#43563=CARTESIAN_POINT('Ctrl Pts',(-21.9450035643996,20.7548836660666,5.22998336277636));
#43564=CARTESIAN_POINT('Ctrl Pts',(-22.0118386474232,20.7183895292736,5.22511951904495));
#43565=CARTESIAN_POINT('Ctrl Pts',(-22.0179161443742,20.7150963563418,5.22467734868954));
#43566=CARTESIAN_POINT('Ctrl Pts',(-22.0524727755572,20.6965149549662,5.22216379944567));
#43567=CARTESIAN_POINT('Ctrl Pts',(-22.0811692712005,20.6816367307315,5.22007889511683));
#43568=CARTESIAN_POINT('Ctrl Pts',(-22.2662981209989,20.5891597080422,5.20664450491016));
#43569=CARTESIAN_POINT('Ctrl Pts',(-22.4285790412283,20.5239601848639,5.19491685783022));
#43570=CARTESIAN_POINT('Ctrl Pts',(-22.7407280959838,20.4271185728184,5.17280071104562));
#43571=CARTESIAN_POINT('Ctrl Pts',(-22.8891555313429,20.3923654013195,5.16246598053466));
#43572=CARTESIAN_POINT('Ctrl Pts',(-23.0912842334221,20.3599206670471,5.14901764564463));
#43573=CARTESIAN_POINT('Ctrl Pts',(-23.1432769257045,20.3528722203996,5.14561404726355));
#43574=CARTESIAN_POINT('Ctrl Pts',(-23.2205167272727,20.3443159519055,5.14066182410012));
#43575=CARTESIAN_POINT('Ctrl Pts',(-23.2456445906256,20.3418309332545,5.1390670054621));
#43576=CARTESIAN_POINT('Ctrl Pts',(-23.2750935517111,20.339267687056,5.13721897508897));
#43577=CARTESIAN_POINT('Ctrl Pts',(-23.2793878802884,20.3389025853482,5.13695001332483));
#43578=CARTESIAN_POINT('Ctrl Pts',(-23.2859479490283,20.3383581038515,5.13653995629943));
#43579=CARTESIAN_POINT('Ctrl Pts',(-23.2882131466422,20.3381725064172,5.13639851110696));
#43580=CARTESIAN_POINT('Ctrl Pts',(-23.2923189361186,20.3378404734495,5.13614240458503));
#43581=CARTESIAN_POINT('Ctrl Pts',(-23.2941594508709,20.3376932239636,5.13602769753121));
#43582=CARTESIAN_POINT('Ctrl Pts',(-23.2981750167691,20.3373754333865,5.13577764915076));
#43583=CARTESIAN_POINT('Ctrl Pts',(-23.3003501090528,20.3372055196531,5.13564234402478));
#43584=CARTESIAN_POINT('Ctrl Pts',(-23.3062997386374,20.3367468248815,5.13527260934664));
#43585=CARTESIAN_POINT('Ctrl Pts',(-23.3100746300795,20.3364624842762,5.13503843095937));
#43586=CARTESIAN_POINT('Ctrl Pts',(-23.3283848193395,20.3351157253471,5.13390448948218));
#43587=CARTESIAN_POINT('Ctrl Pts',(-23.3429270108216,20.3341452398496,5.13300984354642));
#43588=CARTESIAN_POINT('Ctrl Pts',(-23.3662675889,20.3327465596985,5.13158273320885));
#43589=CARTESIAN_POINT('Ctrl Pts',(-23.3750618034998,20.3322557399463,5.13104703607255));
#43590=CARTESIAN_POINT('Ctrl Pts',(-23.3890978778253,20.331530072483,5.13019507672205));
#43591=CARTESIAN_POINT('Ctrl Pts',(-23.3943384161776,20.3312719661663,5.12987766419658));
#43592=CARTESIAN_POINT('Ctrl Pts',(-23.4040760662025,20.3308162043299,5.12928908627256));
#43593=CARTESIAN_POINT('Ctrl Pts',(-23.408572997435,20.3306151708916,5.12901775863018));
#43594=CARTESIAN_POINT('Ctrl Pts',(-23.7270422535201,20.3170466540945,5.10983579494653));
#43595=CARTESIAN_POINT('Ctrl Pts',(-24.0413303099646,20.349661198246,5.0930587851589));
#43596=CARTESIAN_POINT('Ctrl Pts',(-24.5040104236033,20.4675484386213,5.06591717534581));
#43597=CARTESIAN_POINT('Ctrl Pts',(-24.6587521119003,20.5197516086665,5.05642006923913));
#43598=CARTESIAN_POINT('Ctrl Pts',(-24.8164123223943,20.5866357975897,5.04600784111712));
#43599=CARTESIAN_POINT('Ctrl Pts',(-24.8239465692147,20.5898660266766,5.04550848197663));
#43600=CARTESIAN_POINT('Ctrl Pts',(-24.8359676781115,20.595074335915,5.04470885698203));
#43601=CARTESIAN_POINT('Ctrl Pts',(-24.8404625260121,20.5970339863307,5.04440922035229));
#43602=CARTESIAN_POINT('Ctrl Pts',(-24.8490089892762,20.6007832837076,5.04383825446901));
#43603=CARTESIAN_POINT('Ctrl Pts',(-24.8530614252034,20.6025710415036,5.04356699037738));
#43604=CARTESIAN_POINT('Ctrl Pts',(-24.8601584391799,20.6057194283309,5.04309098844088));
#43605=CARTESIAN_POINT('Ctrl Pts',(-24.8632046216483,20.6070764423958,5.04288637504695));
#43606=CARTESIAN_POINT('Ctrl Pts',(-24.8691433252045,20.6097330719735,5.04248687455178));
#43607=CARTESIAN_POINT('Ctrl Pts',(-24.8720360462252,20.6110322339288,5.0422920032373));
#43608=CARTESIAN_POINT('Ctrl Pts',(-24.8788894803211,20.6141223717511,5.04182965689296));
#43609=CARTESIAN_POINT('Ctrl Pts',(-24.8828484896799,20.6159170924753,5.04156205293057));
#43610=CARTESIAN_POINT('Ctrl Pts',(-24.8967453885571,20.622250838815,5.04062086880987));
#43611=CARTESIAN_POINT('Ctrl Pts',(-24.906663731159,20.6268323463075,5.03994582220136));
#43612=CARTESIAN_POINT('Ctrl Pts',(-25.0373620401496,20.6880131703327,5.03100608141913));
#43613=CARTESIAN_POINT('Ctrl Pts',(-25.1545219503958,20.7519994833869,5.02248222370348));
#43614=CARTESIAN_POINT('Ctrl Pts',(-25.3706010190642,20.8880484953357,5.00573566859235));
#43615=CARTESIAN_POINT('Ctrl Pts',(-25.4700511072598,20.9588497801394,4.99756392347781));
#43616=CARTESIAN_POINT('Ctrl Pts',(-25.6460484699152,21.0998489906195,4.98233287291109));
#43617=CARTESIAN_POINT('Ctrl Pts',(-25.7236879971006,21.1684430141461,4.97530196190845));
#43618=CARTESIAN_POINT('Ctrl Pts',(-25.9045459749293,21.3444491977166,4.95831929563578));
#43619=CARTESIAN_POINT('Ctrl Pts',(-26.0038989482285,21.4555216162748,4.94845129954147));
#43620=CARTESIAN_POINT('Ctrl Pts',(-26.0989786277632,21.5779061583656,4.93874057827075));
#43621=CARTESIAN_POINT('Ctrl Pts',(-26.1027151738623,21.5827441096125,4.93835849648739));
#43622=CARTESIAN_POINT('Ctrl Pts',(-26.1080344848724,21.589672027119,4.9378139457162));
#43623=CARTESIAN_POINT('Ctrl Pts',(-26.1096284704087,21.5917533003002,4.93765068508991));
#43624=CARTESIAN_POINT('Ctrl Pts',(-26.112377890287,21.5953523173932,4.93736894570905));
#43625=CARTESIAN_POINT('Ctrl Pts',(-26.1135345182704,21.596869144239,4.93725038171775));
#43626=CARTESIAN_POINT('Ctrl Pts',(-26.1157571557458,21.5997893322908,4.93702246394916));
#43627=CARTESIAN_POINT('Ctrl Pts',(-26.1168233587415,21.6011925382501,4.93691309619673));
#43628=CARTESIAN_POINT('Ctrl Pts',(-26.1193452833312,21.6045172446503,4.93665431976844));
#43629=CARTESIAN_POINT('Ctrl Pts',(-26.1208000035252,21.6064395085581,4.93650498242177));
#43630=CARTESIAN_POINT('Ctrl Pts',(-26.1251290179056,21.6121732165407,4.93606037090477));
#43631=CARTESIAN_POINT('Ctrl Pts',(-26.1279970180763,21.6159894382424,4.93576553947387));
#43632=CARTESIAN_POINT('Ctrl Pts',(-26.1544293316378,21.6513240342288,4.93304560853889));
#43633=CARTESIAN_POINT('Ctrl Pts',(-26.1774242540994,21.6832669056302,4.9306596288548));
#43634=CARTESIAN_POINT('Ctrl Pts',(-26.2013314149635,21.7177937252179,4.92814801068477));
#43635=CARTESIAN_POINT('Ctrl Pts',(-26.2028306307508,21.7199645895263,4.92799037346223));
#43636=CARTESIAN_POINT('Ctrl Pts',(-26.2052099989216,21.7234189783084,4.92773997391076));
#43637=CARTESIAN_POINT('Ctrl Pts',(-26.2060918869853,21.7247012989241,4.9276471182486));
#43638=CARTESIAN_POINT('Ctrl Pts',(-26.2086824577383,21.7284740016877,4.92737421023122));
#43639=CARTESIAN_POINT('Ctrl Pts',(-26.2103885734747,21.7309661541735,4.9271942946592));
#43640=CARTESIAN_POINT('Ctrl Pts',(-26.212699850902,21.7343524791958,4.92695030992237));
#43641=CARTESIAN_POINT('Ctrl Pts',(-26.21330806485,21.7352445549524,4.92688608135389));
#43642=CARTESIAN_POINT('Ctrl Pts',(-26.2211933398391,21.7468224929417,4.92605306897446));
#43643=CARTESIAN_POINT('Ctrl Pts',(-26.2284065802359,21.757551885379,4.92528760026367));
#43644=CARTESIAN_POINT('Ctrl Pts',(-26.3061491382792,21.8747071788135,4.9169963472863));
#43645=CARTESIAN_POINT('Ctrl Pts',(-26.3703653350986,21.9852005364838,4.90977191484756));
#43646=CARTESIAN_POINT('Ctrl Pts',(-26.504256639869,22.250726635808,4.89309453095971));
#43647=CARTESIAN_POINT('Ctrl Pts',(-26.5685665813311,22.4080237845715,4.88370645766961));
#43648=CARTESIAN_POINT('Ctrl Pts',(-26.6620330440601,22.7006365055362,4.86617276207587));
#43649=CARTESIAN_POINT('Ctrl Pts',(-26.69544182781,22.834150200173,4.85815043511401));
#43650=CARTESIAN_POINT('Ctrl Pts',(-26.7241250121101,22.9906811892552,4.84853131314228));
#43651=CARTESIAN_POINT('Ctrl Pts',(-26.7278136820209,23.0120223675674,4.8472155502313));
#43652=CARTESIAN_POINT('Ctrl Pts',(-26.732269638324,23.0394470464099,4.84551869918875));
#43653=CARTESIAN_POINT('Ctrl Pts',(-26.7332351137378,23.0454981436314,4.84514392431726));
#43654=CARTESIAN_POINT('Ctrl Pts',(-26.7347604235763,23.0552364132254,4.84454016959271));
#43655=CARTESIAN_POINT('Ctrl Pts',(-26.7353311287924,23.0589218883134,4.84431153546012));
#43656=CARTESIAN_POINT('Ctrl Pts',(-26.7364042233459,23.0659321143345,4.84387637308583));
#43657=CARTESIAN_POINT('Ctrl Pts',(-26.7369078093782,23.0692566793643,4.84366988315518));
#43658=CARTESIAN_POINT('Ctrl Pts',(-26.7380416995014,23.0768223170557,4.84319971136168));
#43659=CARTESIAN_POINT('Ctrl Pts',(-26.7386687437839,23.0810638652481,4.84293592640924));
#43660=CARTESIAN_POINT('Ctrl Pts',(-26.740546863439,23.0939457703661,4.84213420442753));
#43661=CARTESIAN_POINT('Ctrl Pts',(-26.7417712870527,23.1025899183498,4.8415954232885));
#43662=CARTESIAN_POINT('Ctrl Pts',(-26.7501669242444,23.1636468294434,4.83778402024732));
#43663=CARTESIAN_POINT('Ctrl Pts',(-26.7560814213144,23.2162215726421,4.83447182341248));
#43664=CARTESIAN_POINT('Ctrl Pts',(-26.7609921848854,23.2722602402259,4.8309064196588));
#43665=CARTESIAN_POINT('Ctrl Pts',(-26.7612800494691,23.2756052767537,4.8306934637042));
#43666=CARTESIAN_POINT('Ctrl Pts',(-26.76190666116,23.283022273614,4.83022098144621));
#43667=CARTESIAN_POINT('Ctrl Pts',(-26.7622428919642,23.2870944357958,4.82996137891756));
#43668=CARTESIAN_POINT('Ctrl Pts',(-26.762977164163,23.2961984499482,4.82938055593241));
#43669=CARTESIAN_POINT('Ctrl Pts',(-26.7633711294963,23.3012306119322,4.82905921282184));
#43670=CARTESIAN_POINT('Ctrl Pts',(-26.7652625168005,23.3261414792106,4.82746697708172));
#43671=CARTESIAN_POINT('Ctrl Pts',(-26.7665872666799,23.3460325206587,4.82619092464468));
#43672=CARTESIAN_POINT('Ctrl Pts',(-26.7712907986619,23.4281377467265,4.82090435995079));
#43673=CARTESIAN_POINT('Ctrl Pts',(-26.7730494221322,23.4904281366185,4.81684749405692));
#43674=CARTESIAN_POINT('Ctrl Pts',(-26.7728738638164,23.7190449075866,4.80179839398118));
#43675=CARTESIAN_POINT('Ctrl Pts',(-26.7598714911795,23.8850910761752,4.79054155792165));
#43676=CARTESIAN_POINT('Ctrl Pts',(-26.7046678499917,24.2372295273084,4.76642026884124));
#43677=CARTESIAN_POINT('Ctrl Pts',(-26.6586472059406,24.422132350987,4.75360217753736));
#43678=CARTESIAN_POINT('Ctrl Pts',(-26.5928181251123,24.6128179118957,4.74088904000005));
#43679=CARTESIAN_POINT('Ctrl Pts',(-26.5889959887278,24.6236996842783,4.74016542431284));
#43680=CARTESIAN_POINT('Ctrl Pts',(-26.5839368683926,24.6378596199334,4.73922649037708));
#43681=CARTESIAN_POINT('Ctrl Pts',(-26.5827529032909,24.6411564365647,4.73900807061101));
#43682=CARTESIAN_POINT('Ctrl Pts',(-26.5809229718887,24.6462259826305,4.73867250345071));
#43683=CARTESIAN_POINT('Ctrl Pts',(-26.5802808249788,24.6480000728728,4.7385551279544));
#43684=CARTESIAN_POINT('Ctrl Pts',(-26.5790008517,24.6515266367752,4.738321920794));
#43685=CARTESIAN_POINT('Ctrl Pts',(-26.5783630657773,24.6532791106429,4.73820608803403));
#43686=CARTESIAN_POINT('Ctrl Pts',(-26.5769371308502,24.6571866603517,4.73794793633169));
#43687=CARTESIAN_POINT('Ctrl Pts',(-26.5761482030211,24.6593414434949,4.73780566516316));
#43688=CARTESIAN_POINT('Ctrl Pts',(-26.5738351766597,24.6656381285636,4.73739016317186));
#43689=CARTESIAN_POINT('Ctrl Pts',(-26.5723048627207,24.6697777657684,4.73711730472283));
#43690=CARTESIAN_POINT('Ctrl Pts',(-26.5611331777055,24.6998083560886,4.73514000986864));
#43691=CARTESIAN_POINT('Ctrl Pts',(-26.5511673484998,24.7255785477257,4.73345473584688));
#43692=CARTESIAN_POINT('Ctrl Pts',(-26.5182457692878,24.8075591282002,4.72812076936408));
#43693=CARTESIAN_POINT('Ctrl Pts',(-26.4940314243791,24.8632531294324,4.72453841268557));
#43694=CARTESIAN_POINT('Ctrl Pts',(-26.4327737006213,24.993920367541,4.71615734955104));
#43695=CARTESIAN_POINT('Ctrl Pts',(-26.3943578097896,25.0682023802709,4.71141163070593));
#43696=CARTESIAN_POINT('Ctrl Pts',(-26.2248077437541,25.366960688579,4.69208098872679));
#43697=CARTESIAN_POINT('Ctrl Pts',(-26.0696568834325,25.5766459522074,4.67784024595707));
#43698=CARTESIAN_POINT('Ctrl Pts',(-25.8812510433842,25.7757333938321,4.66175717873313));
#43699=CARTESIAN_POINT('Ctrl Pts',(-25.8714244664303,25.7859805943172,4.66092161527053));
#43700=CARTESIAN_POINT('Ctrl Pts',(-25.8563325505458,25.8015117669704,4.6596430300755));
#43701=CARTESIAN_POINT('Ctrl Pts',(-25.8511159715902,25.8068430190046,4.65920192621688));
#43702=CARTESIAN_POINT('Ctrl Pts',(-25.8430355354815,25.8150439340495,4.65851992207102));
#43703=CARTESIAN_POINT('Ctrl Pts',(-25.8401846714975,25.8179264045258,4.65827954444316));
#43704=CARTESIAN_POINT('Ctrl Pts',(-25.8331939464501,25.8249680075673,4.65769068327534));
#43705=CARTESIAN_POINT('Ctrl Pts',(-25.8290481602912,25.8291212163322,4.65734195924947));
#43706=CARTESIAN_POINT('Ctrl Pts',(-25.8200006873544,25.8381355114466,4.65658197878899));
#43707=CARTESIAN_POINT('Ctrl Pts',(-25.8150946862768,25.842992210096,4.6561705447233));
#43708=CARTESIAN_POINT('Ctrl Pts',(-25.8021284008394,25.8557459634982,4.65508485237189));
#43709=CARTESIAN_POINT('Ctrl Pts',(-25.7940422288221,25.8636164642438,4.65440950463946));
#43710=CARTESIAN_POINT('Ctrl Pts',(-25.7785660685551,25.8785223721214,4.65312008545666));
#43711=CARTESIAN_POINT('Ctrl Pts',(-25.7711836651245,25.8855654797503,4.65250634758203));
#43712=CARTESIAN_POINT('Ctrl Pts',(-25.7587709168142,25.8972956450653,4.65147655987787));
#43713=CARTESIAN_POINT('Ctrl Pts',(-25.7537587613022,25.9020019078812,4.65106132137479));
#43714=CARTESIAN_POINT('Ctrl Pts',(-25.7342222249319,25.9202288413031,4.64944498706106));
#43715=CARTESIAN_POINT('Ctrl Pts',(-25.7195883800787,25.9336310745619,4.64823895972118));
#43716=CARTESIAN_POINT('Ctrl Pts',(-25.7002306869885,25.9510336080784,4.64664932794436));
#43717=CARTESIAN_POINT('Ctrl Pts',(-25.695617547597,25.9551568525902,4.64627092183977));
#43718=CARTESIAN_POINT('Ctrl Pts',(-25.6884746234795,25.9615043218462,4.64568563677741));
#43719=CARTESIAN_POINT('Ctrl Pts',(-25.6859531597954,25.963737923467,4.64547915157451));
#43720=CARTESIAN_POINT('Ctrl Pts',(-25.6809216515002,25.9681809521242,4.64506735530463));
#43721=CARTESIAN_POINT('Ctrl Pts',(-25.6784116606679,25.9703904339737,4.64486204689995));
#43722=CARTESIAN_POINT('Ctrl Pts',(-25.6728350940495,25.9752839616992,4.64440616231671));
#43723=CARTESIAN_POINT('Ctrl Pts',(-25.669766860549,25.9779661021267,4.64415550716968));
#43724=CARTESIAN_POINT('Ctrl Pts',(-25.6608848587447,25.9857007595265,4.64343039759552));
#43725=CARTESIAN_POINT('Ctrl Pts',(-25.6550580835287,25.990738236991,4.64295531970268));
#43726=CARTESIAN_POINT('Ctrl Pts',(-25.6152661146684,26.0248914603937,4.63971498098456));
#43727=CARTESIAN_POINT('Ctrl Pts',(-25.5807173447519,26.0533169021919,4.63692147590551));
#43728=CARTESIAN_POINT('Ctrl Pts',(-25.5133910569373,26.1063992205342,4.63151163056614));
#43729=CARTESIAN_POINT('Ctrl Pts',(-25.4807123533074,26.1311677561835,4.62890046004988));
#43730=CARTESIAN_POINT('Ctrl Pts',(-25.4001135059712,26.1898697143194,4.62249427694327));
#43731=CARTESIAN_POINT('Ctrl Pts',(-25.3517226398677,26.2231291252522,4.61867617752031));
#43732=CARTESIAN_POINT('Ctrl Pts',(-25.1648488703491,26.3441883273632,4.60404347867693));
#43733=CARTESIAN_POINT('Ctrl Pts',(-25.0206538164229,26.4226922844705,4.5929627316583));
#43734=CARTESIAN_POINT('Ctrl Pts',(-24.6914382558783,26.5706199987887,4.56853267147059));
#43735=CARTESIAN_POINT('Ctrl Pts',(-24.5047018269214,26.6347250000079,4.55522316539849));
#43736=CARTESIAN_POINT('Ctrl Pts',(-24.3017498118959,26.6841813365457,4.54205476130365));
#43737=CARTESIAN_POINT('Ctrl Pts',(-24.2902239540649,26.6869227758382,4.54131131455393));
#43738=CARTESIAN_POINT('Ctrl Pts',(-24.2752347193874,26.690400764033,4.54035041488178));
#43739=CARTESIAN_POINT('Ctrl Pts',(-24.271785073716,26.6911952062146,4.54012967996918));
#43740=CARTESIAN_POINT('Ctrl Pts',(-24.2664875482689,26.6924060211721,4.53979133706199));
#43741=CARTESIAN_POINT('Ctrl Pts',(-24.2646406128451,26.6928264480817,4.53967349492698));
#43742=CARTESIAN_POINT('Ctrl Pts',(-24.2610112214233,26.6936492592026,4.53944215822162));
#43743=CARTESIAN_POINT('Ctrl Pts',(-24.2592288033286,26.6940517536276,4.53932865803515));
#43744=CARTESIAN_POINT('Ctrl Pts',(-24.2552815007607,26.6949395809058,4.53907754786697));
#43745=CARTESIAN_POINT('Ctrl Pts',(-24.2531164623426,26.695424193109,4.53893998024437));
#43746=CARTESIAN_POINT('Ctrl Pts',(-24.2486159006409,26.6964266988772,4.53865434704681));
#43747=CARTESIAN_POINT('Ctrl Pts',(-24.2462802964862,26.6969442287092,4.5385063025294));
#43748=CARTESIAN_POINT('Ctrl Pts',(-24.2402701815356,26.6982689482508,4.53812582207067));
#43749=CARTESIAN_POINT('Ctrl Pts',(-24.2365948167534,26.6990723080676,4.53789360482869));
#43750=CARTESIAN_POINT('Ctrl Pts',(-24.2259019861915,26.7013899318327,4.53721931834472));
#43751=CARTESIAN_POINT('Ctrl Pts',(-24.2188808014586,26.7028871979796,4.53677820290706));
#43752=CARTESIAN_POINT('Ctrl Pts',(-24.1466024868981,26.7180482117521,4.53225351255114));
#43753=CARTESIAN_POINT('Ctrl Pts',(-24.0809358601629,26.7297083681593,4.52827915837504));
#43754=CARTESIAN_POINT('Ctrl Pts',(-23.9716544494525,26.7456323605316,4.52181952275864));
#43755=CARTESIAN_POINT('Ctrl Pts',(-23.9282337729237,26.7510590374859,4.51929287418227));
#43756=CARTESIAN_POINT('Ctrl Pts',(-23.6126085754082,26.7839929516179,4.5011314005564));
#43757=CARTESIAN_POINT('Ctrl Pts',(-23.3379951139738,26.7776237154805,4.48632970877388));
#43758=CARTESIAN_POINT('Ctrl Pts',(-22.9505806139728,26.718925663682,4.46370097501754));
#43759=CARTESIAN_POINT('Ctrl Pts',(-22.8347606885478,26.6947973756382,4.45672095188124));
#43760=CARTESIAN_POINT('Ctrl Pts',(-22.7102627019604,26.6616264564022,4.4488812256495));
#43761=CARTESIAN_POINT('Ctrl Pts',(-22.7000022920564,26.6588382453509,4.44823262611958));
#43762=CARTESIAN_POINT('Ctrl Pts',(-22.6856155102209,26.654852158533,4.44731961575147));
#43763=CARTESIAN_POINT('Ctrl Pts',(-22.6814773713433,26.6536967058878,4.44705658683998));
#43764=CARTESIAN_POINT('Ctrl Pts',(-22.6743015504593,26.6516775935641,4.44659975071053));
#43765=CARTESIAN_POINT('Ctrl Pts',(-22.6712627968822,26.6508177353158,4.44640606765432));
#43766=CARTESIAN_POINT('Ctrl Pts',(-22.6649438438396,26.6490196622944,4.44600283966205));
#43767=CARTESIAN_POINT('Ctrl Pts',(-22.6616638623614,26.648080703022,4.4457932706497));
#43768=CARTESIAN_POINT('Ctrl Pts',(-22.6539459394565,26.6458580295738,4.44529951894137));
#43769=CARTESIAN_POINT('Ctrl Pts',(-22.6495092638769,26.6445699800046,4.44501519482447));
#43770=CARTESIAN_POINT('Ctrl Pts',(-22.6350213756625,26.6403300766814,4.44408513023094));
#43771=CARTESIAN_POINT('Ctrl Pts',(-22.6249818624688,26.6373387772528,4.44343809971391));
#43772=CARTESIAN_POINT('Ctrl Pts',(-22.6015601153087,26.6302356892728,4.44192260319975));
#43773=CARTESIAN_POINT('Ctrl Pts',(-22.5881898145426,26.6260855684775,4.44105288657199));
#43774=CARTESIAN_POINT('Ctrl Pts',(-22.447979695722,26.5815609286362,4.43188337308708));
#43775=CARTESIAN_POINT('Ctrl Pts',(-22.3237470330152,26.5334575321492,4.42332742690915));
#43776=CARTESIAN_POINT('Ctrl Pts',(-22.1597826851877,26.4579938422594,4.41143761695813));
#43777=CARTESIAN_POINT('Ctrl Pts',(-22.1171657233614,26.437227623864,4.40829071839276));
#43778=CARTESIAN_POINT('Ctrl Pts',(-22.07503587195,26.4155367007276,4.4051257859302));
#43779=CARTESIAN_POINT('',(-26.7730023406925,23.55136208175,4.56709764253913));
#43780=CARTESIAN_POINT('Ctrl Pts',(-22.0750360153459,26.4155367745562,4.16020796448761));
#43781=CARTESIAN_POINT('Ctrl Pts',(-22.0752387407196,26.4156411494782,4.16022211916697));
#43782=CARTESIAN_POINT('Ctrl Pts',(-22.0754414773459,26.4157455029758,4.16023627247669));
#43783=CARTESIAN_POINT('Ctrl Pts',(-22.0776159214908,26.416864450636,4.1603880501777));
#43784=CARTESIAN_POINT('Ctrl Pts',(-22.0795886715041,26.4178770346465,4.16052554583761));
#43785=CARTESIAN_POINT('Ctrl Pts',(-22.0836906523566,26.4199771757902,4.16081102372231));
#43786=CARTESIAN_POINT('Ctrl Pts',(-22.0858200526079,26.4210644017309,4.16095898492431));
#43787=CARTESIAN_POINT('Ctrl Pts',(-22.0913002370208,26.4238547819672,4.16133917685715));
#43788=CARTESIAN_POINT('Ctrl Pts',(-22.0946528062336,26.4255544515772,4.16157118936666));
#43789=CARTESIAN_POINT('Ctrl Pts',(-22.1044091483979,26.4304792385287,4.16224472436418));
#43790=CARTESIAN_POINT('Ctrl Pts',(-22.1108207707646,26.4336888808583,4.16268529564305));
#43791=CARTESIAN_POINT('Ctrl Pts',(-22.1327027364086,26.4445517629403,4.16418208068455));
#43792=CARTESIAN_POINT('Ctrl Pts',(-22.1482241388819,26.4521022654713,4.1652322024229));
#43793=CARTESIAN_POINT('Ctrl Pts',(-22.2083525987552,26.4807571345579,4.16925860410626));
#43794=CARTESIAN_POINT('Ctrl Pts',(-22.2533836975093,26.5009616750483,4.17218613963835));
#43795=CARTESIAN_POINT('Ctrl Pts',(-22.3391706292074,26.5371089552848,4.17763153981386));
#43796=CARTESIAN_POINT('Ctrl Pts',(-22.3798207474081,26.5532710776522,4.18015753756762));
#43797=CARTESIAN_POINT('Ctrl Pts',(-22.6756495243272,26.663969985544,4.1982352214823));
#43798=CARTESIAN_POINT('Ctrl Pts',(-22.9415623312482,26.7266774940453,4.21296121383391));
#43799=CARTESIAN_POINT('Ctrl Pts',(-23.3312794697115,26.7677834330629,4.23557914435609));
#43800=CARTESIAN_POINT('Ctrl Pts',(-23.4509495709218,26.7736960440887,4.24264498599362));
#43801=CARTESIAN_POINT('Ctrl Pts',(-23.5813261939395,26.7728703687676,4.25057811817322));
#43802=CARTESIAN_POINT('Ctrl Pts',(-23.5919900823455,26.7727498969192,4.25122866390271));
#43803=CARTESIAN_POINT('Ctrl Pts',(-23.6069546422885,26.7725065473661,4.25214397694664));
#43804=CARTESIAN_POINT('Ctrl Pts',(-23.611256046848,26.7724279834203,4.25240735307333));
#43805=CARTESIAN_POINT('Ctrl Pts',(-23.6187162658897,26.7722767809801,4.25286463289879));
#43806=CARTESIAN_POINT('Ctrl Pts',(-23.6218751626426,26.7722081093698,4.25305841186525));
#43807=CARTESIAN_POINT('Ctrl Pts',(-23.6284439736687,26.772055644155,4.25346168635388));
#43808=CARTESIAN_POINT('Ctrl Pts',(-23.6318538642192,26.7719710823206,4.25367120572753));
#43809=CARTESIAN_POINT('Ctrl Pts',(-23.6398763955407,26.7717593869084,4.25416456945638));
#43810=CARTESIAN_POINT('Ctrl Pts',(-23.6444889011699,26.7716277599899,4.25444855457217));
#43811=CARTESIAN_POINT('Ctrl Pts',(-23.659540675307,26.7711658729303,4.25537635210081));
#43812=CARTESIAN_POINT('Ctrl Pts',(-23.6699785423175,26.7707947730481,4.25602144576727));
#43813=CARTESIAN_POINT('Ctrl Pts',(-23.8643721546152,26.7629371100988,4.26806783752885));
#43814=CARTESIAN_POINT('Ctrl Pts',(-24.0473203545893,26.7397533572145,4.27997342002075));
#43815=CARTESIAN_POINT('Ctrl Pts',(-24.260708956705,26.6939031933505,4.29451153138907));
#43816=CARTESIAN_POINT('Ctrl Pts',(-24.2940373918442,26.6861848990009,4.29680047082384));
#43817=CARTESIAN_POINT('Ctrl Pts',(-24.3544600926756,26.6711746147513,4.30098081816748));
#43818=CARTESIAN_POINT('Ctrl Pts',(-24.3815943797773,26.6640564991932,4.30286945473942));
#43819=CARTESIAN_POINT('Ctrl Pts',(-24.4315831867193,26.6502429863717,4.30636795784229));
#43820=CARTESIAN_POINT('Ctrl Pts',(-24.4544632524606,26.6436467035083,4.30797670944009));
#43821=CARTESIAN_POINT('Ctrl Pts',(-24.4970560720837,26.6308543410923,4.31098412268456));
#43822=CARTESIAN_POINT('Ctrl Pts',(-24.5167865045487,26.6247210268544,4.31238235728614));
#43823=CARTESIAN_POINT('Ctrl Pts',(-24.5933426779191,26.6001133294704,4.31782544752065));
#43824=CARTESIAN_POINT('Ctrl Pts',(-24.6497097583347,26.5802495398251,4.32187170621528));
#43825=CARTESIAN_POINT('Ctrl Pts',(-24.7855595310423,26.5280856599102,4.33168074718154));
#43826=CARTESIAN_POINT('Ctrl Pts',(-24.864372231619,26.4941554877538,4.33742074381131));
#43827=CARTESIAN_POINT('Ctrl Pts',(-25.0068983713246,26.4259296193237,4.34778868621606));
#43828=CARTESIAN_POINT('Ctrl Pts',(-25.0709945763356,26.3925546609894,4.35244612598531));
#43829=CARTESIAN_POINT('Ctrl Pts',(-25.1392279096219,26.3540556542697,4.35735575495317));
#43830=CARTESIAN_POINT('Ctrl Pts',(-25.1445270968971,26.3510458682359,4.35773672433705));
#43831=CARTESIAN_POINT('Ctrl Pts',(-25.1519218232155,26.3468180891671,4.35826785556285));
#43832=CARTESIAN_POINT('Ctrl Pts',(-25.1540245311552,26.3456127608034,4.35841882836347));
#43833=CARTESIAN_POINT('Ctrl Pts',(-25.1576568130177,26.343525192353,4.35867952448024));
#43834=CARTESIAN_POINT('Ctrl Pts',(-25.1591870212652,26.3426440674042,4.35878932018916));
#43835=CARTESIAN_POINT('Ctrl Pts',(-25.162333569468,26.3408287760119,4.35901502794548));
#43836=CARTESIAN_POINT('Ctrl Pts',(-25.1639498196787,26.3398944639978,4.35913092972764));
#43837=CARTESIAN_POINT('Ctrl Pts',(-25.1676264146596,26.3377648561393,4.35939450200822));
#43838=CARTESIAN_POINT('Ctrl Pts',(-25.1696862528947,26.3365686765279,4.35954211486434));
#43839=CARTESIAN_POINT('Ctrl Pts',(-25.1741187642971,26.3339880735976,4.35985964395077));
#43840=CARTESIAN_POINT('Ctrl Pts',(-25.1764909996853,26.3326028967634,4.36002951116732));
#43841=CARTESIAN_POINT('Ctrl Pts',(-25.1828429889173,26.3288829948421,4.36048417140519));
#43842=CARTESIAN_POINT('Ctrl Pts',(-25.1868195233418,26.3265427424281,4.36076860966511));
#43843=CARTESIAN_POINT('Ctrl Pts',(-25.1989626343907,26.3193611771279,4.36163665015468));
#43844=CARTESIAN_POINT('Ctrl Pts',(-25.2071129445719,26.3144922590636,4.36221851109815));
#43845=CARTESIAN_POINT('Ctrl Pts',(-25.2368764486304,26.2965328896313,4.36434103613836));
#43846=CARTESIAN_POINT('Ctrl Pts',(-25.2583576327798,26.2832240086095,4.36586840690217));
#43847=CARTESIAN_POINT('Ctrl Pts',(-25.3422431597206,26.2298764239828,4.37182412473616));
#43848=CARTESIAN_POINT('Ctrl Pts',(-25.4034186368347,26.1879393256783,4.37614832515994));
#43849=CARTESIAN_POINT('Ctrl Pts',(-25.7742899928164,25.9144202370695,4.40259814194256));
#43850=CARTESIAN_POINT('Ctrl Pts',(-26.0416315412958,25.6308046367301,4.42315569072723));
#43851=CARTESIAN_POINT('Ctrl Pts',(-26.2633105935426,25.2897454905011,4.44775990615106));
#43852=CARTESIAN_POINT('Ctrl Pts',(-26.27408307747,25.2728281992097,4.44897874543893));
#43853=CARTESIAN_POINT('Ctrl Pts',(-26.2879851189343,25.2505396989263,4.45058290608779));
#43854=CARTESIAN_POINT('Ctrl Pts',(-26.2912581939511,25.2452581744318,4.45096290982296));
#43855=CARTESIAN_POINT('Ctrl Pts',(-26.2962849266399,25.2370942645456,4.45155012616894));
#43856=CARTESIAN_POINT('Ctrl Pts',(-26.2980493786227,25.2342185152141,4.45175694080576));
#43857=CARTESIAN_POINT('Ctrl Pts',(-26.3015534850439,25.2284872610834,4.45216905063818));
#43858=CARTESIAN_POINT('Ctrl Pts',(-26.3032932179168,25.2256318089625,4.4523743426137));
#43859=CARTESIAN_POINT('Ctrl Pts',(-26.3071391088407,25.2192973192572,4.45282969238268));
#43860=CARTESIAN_POINT('Ctrl Pts',(-26.3092431290675,25.2158169962243,4.45307982817002));
#43861=CARTESIAN_POINT('Ctrl Pts',(-26.315292267501,25.20576802035,4.45380194020455));
#43862=CARTESIAN_POINT('Ctrl Pts',(-26.3192205345225,25.199189301694,4.45427453191398));
#43863=CARTESIAN_POINT('Ctrl Pts',(-26.3454841486131,25.1548467930436,4.45745901820239));
#43864=CARTESIAN_POINT('Ctrl Pts',(-26.3670688533068,25.1166458536685,4.46019805651753));
#43865=CARTESIAN_POINT('Ctrl Pts',(-26.4228465547749,25.0130464428213,4.46761920104715));
#43866=CARTESIAN_POINT('Ctrl Pts',(-26.4555827332692,24.9468976066703,4.47235083912952));
#43867=CARTESIAN_POINT('Ctrl Pts',(-26.5382496155191,24.7643459543721,4.48539226600775));
#43868=CARTESIAN_POINT('Ctrl Pts',(-26.5836337378715,24.6460365607246,4.49383098632803));
#43869=CARTESIAN_POINT('Ctrl Pts',(-26.6897355625017,24.3118101376062,4.51746475096486));
#43870=CARTESIAN_POINT('Ctrl Pts',(-26.7350780535578,24.0917502148828,4.53283010359708));
#43871=CARTESIAN_POINT('Ctrl Pts',(-26.7583603920194,23.8573250513762,4.54806094738001));
#43872=CARTESIAN_POINT('Ctrl Pts',(-26.7594347903948,23.8458854359024,4.5488012565424));
#43873=CARTESIAN_POINT('Ctrl Pts',(-26.7635206800514,23.7997310522971,4.55177564940515));
#43874=CARTESIAN_POINT('Ctrl Pts',(-26.7660303940838,23.7649726091436,4.55398723556093));
#43875=CARTESIAN_POINT('Ctrl Pts',(-26.7682332912513,23.7255769033781,4.55645661749159));
#43876=CARTESIAN_POINT('Ctrl Pts',(-26.7684807346502,23.720974640728,4.5567445189483));
#43877=CARTESIAN_POINT('Ctrl Pts',(-26.7688403924344,23.7140064781691,4.55717953579456));
#43878=CARTESIAN_POINT('Ctrl Pts',(-26.7689598715843,23.7116409839352,4.55732705700011));
#43879=CARTESIAN_POINT('Ctrl Pts',(-26.7691631738563,23.7075258872574,4.55758341839791));
#43880=CARTESIAN_POINT('Ctrl Pts',(-26.7692481783294,23.7057763484317,4.55769232538162));
#43881=CARTESIAN_POINT('Ctrl Pts',(-26.7694162766648,23.702257410642,4.55791120266558));
#43882=CARTESIAN_POINT('Ctrl Pts',(-26.7694993380181,23.7004880140099,4.55802117075398));
#43883=CARTESIAN_POINT('Ctrl Pts',(-26.7696672603877,23.6968467951451,4.55824729304731));
#43884=CARTESIAN_POINT('Ctrl Pts',(-26.7697519479626,23.6949749629049,4.55836343750543));
#43885=CARTESIAN_POINT('Ctrl Pts',(-26.7699454729076,23.690613274066,4.55863384858626));
#43886=CARTESIAN_POINT('Ctrl Pts',(-26.7700530548423,23.6881233586781,4.55878804447662));
#43887=CARTESIAN_POINT('Ctrl Pts',(-26.770325804334,23.6816362671151,4.55918933826552));
#43888=CARTESIAN_POINT('Ctrl Pts',(-26.7704864181719,23.6776388884537,4.55943618248145));
#43889=CARTESIAN_POINT('Ctrl Pts',(-26.7722005009939,23.6329021196836,4.56219398104913));
#43890=CARTESIAN_POINT('Ctrl Pts',(-26.7729883030933,23.5921350688961,4.5646628544902));
#43891=CARTESIAN_POINT('Ctrl Pts',(-26.7730023406925,23.55136208175,4.56709764253913));
#43892=CARTESIAN_POINT('Ctrl Pts',(-26.7730023395649,23.5513653520337,4.56709744725173));
#43893=CARTESIAN_POINT('Ctrl Pts',(-26.7731080939755,23.2450984785382,4.58538640618436));
#43894=CARTESIAN_POINT('Ctrl Pts',(-26.7295574972271,22.9403166062594,4.60176991163691));
#43895=CARTESIAN_POINT('Ctrl Pts',(-26.6111710850088,22.5352334404187,4.62578088064272));
#43896=CARTESIAN_POINT('Ctrl Pts',(-26.5727909509155,22.4260889674261,4.63247252524186));
#43897=CARTESIAN_POINT('Ctrl Pts',(-26.5092566950496,22.2723694869662,4.64237579605295));
#43898=CARTESIAN_POINT('Ctrl Pts',(-26.4887774108651,22.2259558102615,4.64543073087777));
#43899=CARTESIAN_POINT('Ctrl Pts',(-26.4638280111813,22.1728423376459,4.64900895928721));
#43900=CARTESIAN_POINT('Ctrl Pts',(-26.460417211027,22.1656506196963,4.64949522900745));
#43901=CARTESIAN_POINT('Ctrl Pts',(-26.4551963705043,22.1547469207156,4.65023520066626));
#43902=CARTESIAN_POINT('Ctrl Pts',(-26.45340576234,22.1510256251301,4.65048822582143));
#43903=CARTESIAN_POINT('Ctrl Pts',(-26.4501641761494,22.1443218729311,4.65094491393233));
#43904=CARTESIAN_POINT('Ctrl Pts',(-26.448715735039,22.1413381902163,4.65114848813569));
#43905=CARTESIAN_POINT('Ctrl Pts',(-26.4455893655727,22.1349233228556,4.65158684577235));
#43906=CARTESIAN_POINT('Ctrl Pts',(-26.4439099395751,22.1314928774113,4.65182168133922));
#43907=CARTESIAN_POINT('Ctrl Pts',(-26.4393428262965,22.1222057988774,4.65245857665054));
#43908=CARTESIAN_POINT('Ctrl Pts',(-26.4364434425008,22.1163549667174,4.65286104571327));
#43909=CARTESIAN_POINT('Ctrl Pts',(-26.4233445728212,22.0901227023089,4.65467107329236));
#43910=CARTESIAN_POINT('Ctrl Pts',(-26.4129470376788,22.069841400333,4.65608558051448));
#43911=CARTESIAN_POINT('Ctrl Pts',(-26.3965802747969,22.0387338524839,4.65827900850527));
#43912=CARTESIAN_POINT('Ctrl Pts',(-26.390762257781,22.0278285342838,4.65905252718635));
#43913=CARTESIAN_POINT('Ctrl Pts',(-26.3823708290075,22.012315158303,4.66015949216328));
#43914=CARTESIAN_POINT('Ctrl Pts',(-26.3798485564664,22.007679437637,4.66049112151599));
#43915=CARTESIAN_POINT('Ctrl Pts',(-26.3760552053937,22.0007481926207,4.66098823812281));
#43916=CARTESIAN_POINT('Ctrl Pts',(-26.374792682584,21.9984479745928,4.66115342236388));
#43917=CARTESIAN_POINT('Ctrl Pts',(-26.371696657672,21.9928235546415,4.66155784054046));
#43918=CARTESIAN_POINT('Ctrl Pts',(-26.3698600916257,21.9895010516831,4.66179718254879));
#43919=CARTESIAN_POINT('Ctrl Pts',(-26.3669776229357,21.9843081152788,4.66217195582481));
#43920=CARTESIAN_POINT('Ctrl Pts',(-26.3659357137498,21.9824354590785,4.66230724606277));
#43921=CARTESIAN_POINT('Ctrl Pts',(-26.3615216328583,21.9745204845051,4.66287966126024));
#43922=CARTESIAN_POINT('Ctrl Pts',(-26.3581318924703,21.9684880303125,4.66331740444321));
#43923=CARTESIAN_POINT('Ctrl Pts',(-26.3522294726293,21.9580627203142,4.66407647487299));
#43924=CARTESIAN_POINT('Ctrl Pts',(-26.3497258156795,21.953664762487,4.6643974843391));
#43925=CARTESIAN_POINT('Ctrl Pts',(-26.3452201086667,21.9457931583913,4.66497346186582));
#43926=CARTESIAN_POINT('Ctrl Pts',(-26.3432219115545,21.9423173091683,4.66522829475053));
#43927=CARTESIAN_POINT('Ctrl Pts',(-26.3390286260118,21.935054519799,4.6657618154092));
#43928=CARTESIAN_POINT('Ctrl Pts',(-26.3368322994535,21.931268307101,4.66604054593631));
#43929=CARTESIAN_POINT('Ctrl Pts',(-26.3243242217837,21.9098066857557,4.66762388829351));
#43930=CARTESIAN_POINT('Ctrl Pts',(-26.31385220005,21.8922256446288,4.6689340419198));
#43931=CARTESIAN_POINT('Ctrl Pts',(-26.14638626599,21.6170687594737,4.68964669635293));
#43932=CARTESIAN_POINT('Ctrl Pts',(-25.9541689463484,21.3827115993336,4.71037918464374));
#43933=CARTESIAN_POINT('Ctrl Pts',(-25.66786394157,21.1193073126764,4.73640666193883));
#43934=CARTESIAN_POINT('Ctrl Pts',(-25.6010836461156,21.0627101714906,4.74218758161736));
#43935=CARTESIAN_POINT('Ctrl Pts',(-25.5117208714353,20.993022406343,4.74947688656816));
#43936=CARTESIAN_POINT('Ctrl Pts',(-25.4911734836251,20.9773922718907,4.75112382488224));
#43937=CARTESIAN_POINT('Ctrl Pts',(-25.4626944688942,20.9562640183415,4.75336437592355));
#43938=CARTESIAN_POINT('Ctrl Pts',(-25.4549232929053,20.9505525744963,4.7539715209549));
#43939=CARTESIAN_POINT('Ctrl Pts',(-25.4433530546489,20.9421287311777,4.75486905867905));
#43940=CARTESIAN_POINT('Ctrl Pts',(-25.4395736358068,20.9393896254826,4.75516122945051));
#43941=CARTESIAN_POINT('Ctrl Pts',(-25.4335425840016,20.9350386190035,4.755625840048));
#43942=CARTESIAN_POINT('Ctrl Pts',(-25.4312948192377,20.9334214055301,4.75579864153974));
#43943=CARTESIAN_POINT('Ctrl Pts',(-25.4270215100568,20.9303552118266,4.75612647664754));
#43944=CARTESIAN_POINT('Ctrl Pts',(-25.4249963667343,20.9289056798118,4.75628154828341));
#43945=CARTESIAN_POINT('Ctrl Pts',(-25.4214559371121,20.9263777562859,4.75655213912213));
#43946=CARTESIAN_POINT('Ctrl Pts',(-25.419941395863,20.9252983277611,4.75666773064404));
#43947=CARTESIAN_POINT('Ctrl Pts',(-25.4169780645063,20.9231901980558,4.75689357568873));
#43948=CARTESIAN_POINT('Ctrl Pts',(-25.4155293615218,20.922161386429,4.75700383701278));
#43949=CARTESIAN_POINT('Ctrl Pts',(-25.4120681777767,20.9197076940537,4.75726691534394));
#43950=CARTESIAN_POINT('Ctrl Pts',(-25.4100549074439,20.9182839213028,4.75741965531588));
#43951=CARTESIAN_POINT('Ctrl Pts',(-25.4039605118889,20.9139844854646,4.75788116134603));
#43952=CARTESIAN_POINT('Ctrl Pts',(-25.3998743122096,20.9111159764467,4.75818943628167));
#43953=CARTESIAN_POINT('Ctrl Pts',(-25.357929543276,20.8818160473244,4.76134220996294));
#43954=CARTESIAN_POINT('Ctrl Pts',(-25.3195113750106,20.8561899606431,4.76413273441913));
#43955=CARTESIAN_POINT('Ctrl Pts',(-25.2090689588493,20.7859035529035,4.77192339098277));
#43956=CARTESIAN_POINT('Ctrl Pts',(-25.1358125902185,20.7432436811638,4.77682029692784));
#43957=CARTESIAN_POINT('Ctrl Pts',(-24.9951903290177,20.6686184002414,4.78588314065134));
#43958=CARTESIAN_POINT('Ctrl Pts',(-24.9282344309275,20.6360069997931,4.7900628209124));
#43959=CARTESIAN_POINT('Ctrl Pts',(-24.7263158052043,20.5461773337232,4.80242896775722));
#43960=CARTESIAN_POINT('Ctrl Pts',(-24.5885191558077,20.4958142286339,4.81056923182446));
#43961=CARTESIAN_POINT('Ctrl Pts',(-24.3542327213456,20.4278784264899,4.8244684736137));
#43962=CARTESIAN_POINT('Ctrl Pts',(-24.2595119543009,20.405009627322,4.83010105944297));
#43963=CARTESIAN_POINT('Ctrl Pts',(-24.1016884949517,20.3743978996075,4.83961505520899));
#43964=CARTESIAN_POINT('Ctrl Pts',(-24.0391317555486,20.3641686469608,4.84341839936489));
#43965=CARTESIAN_POINT('Ctrl Pts',(-23.9679985557683,20.3546811816255,4.84779283323655));
#43966=CARTESIAN_POINT('Ctrl Pts',(-23.9596756331334,20.3536041750684,4.84830542146305));
#43967=CARTESIAN_POINT('Ctrl Pts',(-23.9471621466664,20.3520345712205,4.84907726673279));
#43968=CARTESIAN_POINT('Ctrl Pts',(-23.9429746217936,20.3515176685281,4.84933575453622));
#43969=CARTESIAN_POINT('Ctrl Pts',(-23.935768917811,20.3506425685504,4.84978089139864));
#43970=CARTESIAN_POINT('Ctrl Pts',(-23.9327512174803,20.3502804137718,4.84996741506352));
#43971=CARTESIAN_POINT('Ctrl Pts',(-23.9265335168224,20.3495431472815,4.85035194503044));
#43972=CARTESIAN_POINT('Ctrl Pts',(-23.9233334579622,20.3491685644162,4.85054996784787));
#43973=CARTESIAN_POINT('Ctrl Pts',(-23.9156251172295,20.3482779803983,4.85102725207107));
#43974=CARTESIAN_POINT('Ctrl Pts',(-23.9111163055631,20.3477667019381,4.85130666243616));
#43975=CARTESIAN_POINT('Ctrl Pts',(-23.897265466571,20.3462257029244,4.85216572454044));
#43976=CARTESIAN_POINT('Ctrl Pts',(-23.8879200652376,20.3452273320687,4.85274636510446));
#43977=CARTESIAN_POINT('Ctrl Pts',(-23.7781856945582,20.3339896647524,4.85957647946691));
#43978=CARTESIAN_POINT('Ctrl Pts',(-23.6773837479637,20.3284309457564,4.8659730539542));
#43979=CARTESIAN_POINT('Ctrl Pts',(-23.2865409035751,20.3252481940312,4.89128583744409));
#43980=CARTESIAN_POINT('Ctrl Pts',(-22.9976137569462,20.3620338597635,4.91123962004421));
#43981=CARTESIAN_POINT('Ctrl Pts',(-22.6750831048697,20.4482965495018,4.93353845746264));
#43982=CARTESIAN_POINT('Ctrl Pts',(-22.6328249774174,20.4605309573818,4.93645679553918));
#43983=CARTESIAN_POINT('Ctrl Pts',(-22.5421524571281,20.4888065279282,4.94269421232781));
#43984=CARTESIAN_POINT('Ctrl Pts',(-22.4938398361696,20.5051400135801,4.94600239013901));
#43985=CARTESIAN_POINT('Ctrl Pts',(-22.4298143891178,20.5284930636405,4.95034771735269));
#43986=CARTESIAN_POINT('Ctrl Pts',(-22.4137432030588,20.5345008029068,4.95143512783788));
#43987=CARTESIAN_POINT('Ctrl Pts',(-22.3910540597094,20.5431896088852,4.95296483807384));
#43988=CARTESIAN_POINT('Ctrl Pts',(-22.384396183095,20.5457646392437,4.95341304185703));
#43989=CARTESIAN_POINT('Ctrl Pts',(-22.3742568684834,20.5497249446349,4.95409452629995));
#43990=CARTESIAN_POINT('Ctrl Pts',(-22.3707692521755,20.5510941840463,4.95432873954651));
#43991=CARTESIAN_POINT('Ctrl Pts',(-22.3643266818265,20.5536365154501,4.95476102024104));
#43992=CARTESIAN_POINT('Ctrl Pts',(-22.3613710660457,20.5548079017534,4.95495918885448));
#43993=CARTESIAN_POINT('Ctrl Pts',(-22.3565532056387,20.5567255974054,4.9552819735852));
#43994=CARTESIAN_POINT('Ctrl Pts',(-22.354689925029,20.5574692717613,4.95540674918188));
#43995=CARTESIAN_POINT('Ctrl Pts',(-22.351120013348,20.5588979643192,4.95564569428684));
#43996=CARTESIAN_POINT('Ctrl Pts',(-22.3494132791473,20.5595827013943,4.95575988015435));
#43997=CARTESIAN_POINT('Ctrl Pts',(-22.34545084411,20.5611763582942,4.95602486242271));
#43998=CARTESIAN_POINT('Ctrl Pts',(-22.3431955797708,20.5620863730443,4.95617559198756));
#43999=CARTESIAN_POINT('Ctrl Pts',(-22.3360980435863,20.5649596242419,4.95664968170279));
#44000=CARTESIAN_POINT('Ctrl Pts',(-22.331259483577,20.5669320973745,4.95697248265833));
#44001=CARTESIAN_POINT('Ctrl Pts',(-22.2918400988987,20.5831136004245,4.95959924185949));
#44002=CARTESIAN_POINT('Ctrl Pts',(-22.2575023223602,20.5979123614598,4.9618680555572));
#44003=CARTESIAN_POINT('Ctrl Pts',(-22.0646899096642,20.6850192365989,4.97454020938047));
#44004=CARTESIAN_POINT('Ctrl Pts',(-21.9120063636021,20.7694931697069,4.98432301941116));
#44005=CARTESIAN_POINT('Ctrl Pts',(-21.623098008461,20.9614317679698,5.00372174403504));
#44006=CARTESIAN_POINT('Ctrl Pts',(-21.4872224752447,21.0683539438096,5.0133128744892));
#44007=CARTESIAN_POINT('Ctrl Pts',(-21.2767831364495,21.2632250525258,5.02983228810096));
#44008=CARTESIAN_POINT('Ctrl Pts',(-21.1971875618686,21.3452040824698,5.03654678529588));
#44009=CARTESIAN_POINT('Ctrl Pts',(-21.1094023215744,21.4457949653686,5.04462759438187));
#44010=CARTESIAN_POINT('Ctrl Pts',(-21.0968208691804,21.4604763597784,5.0458031857543));
#44011=CARTESIAN_POINT('Ctrl Pts',(-21.0805866437075,21.4797688832802,5.04734342835977));
#44012=CARTESIAN_POINT('Ctrl Pts',(-21.0768131326725,21.4842782638783,5.04770311781997));
#44013=CARTESIAN_POINT('Ctrl Pts',(-21.0707018240331,21.491622076798,5.04828838332878));
#44014=CARTESIAN_POINT('Ctrl Pts',(-21.0683564837876,21.4944502384527,5.04851365112855));
#44015=CARTESIAN_POINT('Ctrl Pts',(-21.0638649131082,21.4998853511227,5.04894633494477));
#44016=CARTESIAN_POINT('Ctrl Pts',(-21.0617179324301,21.5024916781888,5.04915372003635));
#44017=CARTESIAN_POINT('Ctrl Pts',(-21.0568312514065,21.5084428990832,5.04962702840954));
#44018=CARTESIAN_POINT('Ctrl Pts',(-21.054094182448,21.5117899364984,5.0498930579097));
#44019=CARTESIAN_POINT('Ctrl Pts',(-21.0455866227044,21.5222362729809,5.05072284955111));
#44020=CARTESIAN_POINT('Ctrl Pts',(-21.0398396588414,21.5293545960459,5.05128756042851));
#44021=CARTESIAN_POINT('Ctrl Pts',(-20.9954431332286,21.584826779587,5.05568284231832));
#44022=CARTESIAN_POINT('Ctrl Pts',(-20.9581659837523,21.6342577724026,5.05956789186746));
#44023=CARTESIAN_POINT('Ctrl Pts',(-20.9194046445899,21.6888598748334,5.06383027233894));
#44024=CARTESIAN_POINT('Ctrl Pts',(-20.9164818231186,21.6929978151084,5.06415311152768));
#44025=CARTESIAN_POINT('Ctrl Pts',(-20.9008336227863,21.7152627412434,5.0658892492892));
#44026=CARTESIAN_POINT('Ctrl Pts',(-20.8882858447087,21.7335133084198,5.06730897193122));
#44027=CARTESIAN_POINT('Ctrl Pts',(-20.7103412717672,21.998132931136,5.08784568417336));
#44028=CARTESIAN_POINT('Ctrl Pts',(-20.5795754002199,22.2660443288315,5.10823386816402));
#44029=CARTESIAN_POINT('Ctrl Pts',(-20.4611676440061,22.6278950444826,5.1337139353049));
#44030=CARTESIAN_POINT('Ctrl Pts',(-20.4381513622476,22.7088149110581,5.13927558526879));
#44031=CARTESIAN_POINT('Ctrl Pts',(-20.4115050827481,22.8186658094726,5.14656730794082));
#44032=CARTESIAN_POINT('Ctrl Pts',(-20.405063342118,22.8468751255382,5.14841718946176));
#44033=CARTESIAN_POINT('Ctrl Pts',(-20.3968057065185,22.8854212543739,5.15091072586148));
#44034=CARTESIAN_POINT('Ctrl Pts',(-20.3946592931156,22.8956848681297,5.15157138793824));
#44035=CARTESIAN_POINT('Ctrl Pts',(-20.3915706368785,22.9108224042298,5.1525407578416));
#44036=CARTESIAN_POINT('Ctrl Pts',(-20.3905895268467,22.915688195226,5.15285158767963));
#44037=CARTESIAN_POINT('Ctrl Pts',(-20.3890549132902,22.9233908772446,5.15334241168979));
#44038=CARTESIAN_POINT('Ctrl Pts',(-20.388493982717,22.9262262545653,5.15352282221953));
#44039=CARTESIAN_POINT('Ctrl Pts',(-20.3874403241289,22.9315901534241,5.15386361612869));
#44040=CARTESIAN_POINT('Ctrl Pts',(-20.3869468124292,22.9341185160872,5.15402404402772));
#44041=CARTESIAN_POINT('Ctrl Pts',(-20.3860992079426,22.9384888318793,5.15430097852323));
#44042=CARTESIAN_POINT('Ctrl Pts',(-20.3857436911656,22.94033050479,5.154417567304));
#44043=CARTESIAN_POINT('Ctrl Pts',(-20.3850587304492,22.9438955069804,5.15464303343514));
#44044=CARTESIAN_POINT('Ctrl Pts',(-20.3847290864774,22.9456187924116,5.15475192231905));
#44045=CARTESIAN_POINT('Ctrl Pts',(-20.3839555910239,22.9496803789674,5.15500832922945));
#44046=CARTESIAN_POINT('Ctrl Pts',(-20.3835129214843,22.9520189081473,5.15515577905227));
#44047=CARTESIAN_POINT('Ctrl Pts',(-20.3822123550806,22.9589314183775,5.15559110042031));
#44048=CARTESIAN_POINT('Ctrl Pts',(-20.3813617698474,22.9635067947545,5.15587855475575));
#44049=CARTESIAN_POINT('Ctrl Pts',(-20.3740154361849,23.0035053600588,5.15838567186896));
#44050=CARTESIAN_POINT('Ctrl Pts',(-20.3681036458881,23.0390350721437,5.16057262237117));
#44051=CARTESIAN_POINT('Ctrl Pts',(-20.3619885068992,23.0800191322005,5.16305707973498));
#44052=CARTESIAN_POINT('Ctrl Pts',(-20.3612021363979,23.0853820993563,5.16338143277636));
#44053=CARTESIAN_POINT('Ctrl Pts',(-20.3602251032093,23.092164528227,5.16379071545343));
#44054=CARTESIAN_POINT('Ctrl Pts',(-20.360021856503,23.0935821336061,5.16387620946447));
#44055=CARTESIAN_POINT('Ctrl Pts',(-20.3559557582731,23.1220775497949,5.1655937207561));
#44056=CARTESIAN_POINT('Ctrl Pts',(-20.3524367177889,23.1492041508971,5.16721037273258));
#44057=CARTESIAN_POINT('Ctrl Pts',(-20.3328646643503,23.3167713462156,5.17710172693337));
#44058=CARTESIAN_POINT('Ctrl Pts',(-20.3257193454751,23.4581085851828,5.18503840838501));
#44059=CARTESIAN_POINT('Ctrl Pts',(-20.3308891944683,23.7966018910143,5.20397176602783));
#44060=CARTESIAN_POINT('Ctrl Pts',(-20.3519825270502,23.9930287674631,5.2149198754163));
#44061=CARTESIAN_POINT('Ctrl Pts',(-20.4029031128772,24.2459639053567,5.22992161685348));
#44062=CARTESIAN_POINT('Ctrl Pts',(-20.4166038651409,24.3052810330548,5.23350382593977));
#44063=CARTESIAN_POINT('Ctrl Pts',(-20.4433079402257,24.4075893087749,5.23981747159835));
#44064=CARTESIAN_POINT('Ctrl Pts',(-20.4555455899988,24.4507633201496,5.24252433699204));
#44065=CARTESIAN_POINT('Ctrl Pts',(-20.4709368775036,24.5010375198655,5.24573099980447));
#44066=CARTESIAN_POINT('Ctrl Pts',(-20.4732200156543,24.5084006859377,5.246202030221));
#44067=CARTESIAN_POINT('Ctrl Pts',(-20.476750912479,24.519645114573,5.24692348929501));
#44068=CARTESIAN_POINT('Ctrl Pts',(-20.4779796647221,24.5235323546042,5.24717329217977));
#44069=CARTESIAN_POINT('Ctrl Pts',(-20.4802297731954,24.5306040035871,5.24762845018184));
#44070=CARTESIAN_POINT('Ctrl Pts',(-20.481248717791,24.5337891788284,5.24783372555891));
#44071=CARTESIAN_POINT('Ctrl Pts',(-20.4833037806345,24.5401789247733,5.24824606178775));
#44072=CARTESIAN_POINT('Ctrl Pts',(-20.4843399681574,24.5433834686564,5.24845312471185));
#44073=CARTESIAN_POINT('Ctrl Pts',(-20.4872929233129,24.5524671987314,5.2490408452112));
#44074=CARTESIAN_POINT('Ctrl Pts',(-20.4892215840276,24.5583424770729,5.24942189537926));
#44075=CARTESIAN_POINT('Ctrl Pts',(-20.4974008851893,24.5830191808296,5.25102623102812));
#44076=CARTESIAN_POINT('Ctrl Pts',(-20.5038078272097,24.6017679911236,5.25225468225557));
#44077=CARTESIAN_POINT('Ctrl Pts',(-20.6392167035227,24.9863908158483,5.27765614416623));
#44078=CARTESIAN_POINT('Ctrl Pts',(-20.8330568032805,25.3260032904005,5.3044047976759));
#44079=CARTESIAN_POINT('Ctrl Pts',(-21.1198820019696,25.6675175975626,5.33410447590601));
#44080=CARTESIAN_POINT('Ctrl Pts',(-21.158558640892,25.7111119345917,5.33794637780967));
#44081=CARTESIAN_POINT('Ctrl Pts',(-21.2306153204169,25.7880240276761,5.3447836342117));
#44082=CARTESIAN_POINT('Ctrl Pts',(-21.2635850591232,25.8217037204597,5.34779951131197));
#44083=CARTESIAN_POINT('Ctrl Pts',(-21.301480142212,25.8587530723669,5.3511297741486));
#44084=CARTESIAN_POINT('Ctrl Pts',(-21.3056878527189,25.86284445617,5.35149771469782));
#44085=CARTESIAN_POINT('Ctrl Pts',(-21.3122458929754,25.8691864324528,5.35206829478371));
#44086=CARTESIAN_POINT('Ctrl Pts',(-21.3145884680548,25.8714449721888,5.35227154100182));
#44087=CARTESIAN_POINT('Ctrl Pts',(-21.3189786433865,25.8756648472263,5.35265137103907));
#44088=CARTESIAN_POINT('Ctrl Pts',(-21.3210254163184,25.8776270331644,5.35282802072079));
#44089=CARTESIAN_POINT('Ctrl Pts',(-21.3244688321559,25.8809194331155,5.35312447814667));
#44090=CARTESIAN_POINT('Ctrl Pts',(-21.3258640794771,25.8822510943442,5.35324439936297));
#44091=CARTESIAN_POINT('Ctrl Pts',(-21.3286413582422,25.8848970429266,5.35348270451323));
#44092=CARTESIAN_POINT('Ctrl Pts',(-21.3300233609256,25.8862113560606,5.35360109037877));
#44093=CARTESIAN_POINT('Ctrl Pts',(-21.3330722594389,25.8891057716524,5.35386183452936));
#44094=CARTESIAN_POINT('Ctrl Pts',(-21.3347396823231,25.8906853233141,5.35400414966931));
#44095=CARTESIAN_POINT('Ctrl Pts',(-21.3405662374345,25.8961930194413,5.35450046340097));
#44096=CARTESIAN_POINT('Ctrl Pts',(-21.3447341712098,25.9001119006454,5.35485374501852));
#44097=CARTESIAN_POINT('Ctrl Pts',(-21.3868050166998,25.939458287707,5.35840245567413));
#44098=CARTESIAN_POINT('Ctrl Pts',(-21.4255504040901,25.9739791909452,5.36152979959702));
#44099=CARTESIAN_POINT('Ctrl Pts',(-21.467671404388,26.0097208990934,5.36480424831003));
#44100=CARTESIAN_POINT('Ctrl Pts',(-21.4702310623164,26.0118860318649,5.36500275237122));
#44101=CARTESIAN_POINT('Ctrl Pts',(-21.4801647289094,26.0202620462487,5.36577127554351));
#44102=CARTESIAN_POINT('Ctrl Pts',(-21.4875632817881,26.0264438763656,5.36633974168597));
#44103=CARTESIAN_POINT('Ctrl Pts',(-21.6566820039388,26.1664663787064,5.37924774818872));
#44104=CARTESIAN_POINT('Ctrl Pts',(-21.8310838676421,26.2842351874449,5.39079777184254));
#44105=CARTESIAN_POINT('Ctrl Pts',(-22.0353830798098,26.3948594036574,5.40381141616256));
#44106=CARTESIAN_POINT('Ctrl Pts',(-22.0551571698946,26.4053019781705,5.40506566112819));
#44107=CARTESIAN_POINT('Ctrl Pts',(-22.0750360281848,26.4155367811664,5.40632238256859));
#44108=CARTESIAN_POINT('Origin',(-23.5502525316942,23.5502525316942,-77.3107734492734));
#44109=CARTESIAN_POINT('',(-22.0750360103879,26.4155367720035,6.90165778540197));
#44110=CARTESIAN_POINT('',(-22.0750360194354,26.4155367766617,6.65421995916068));
#44111=CARTESIAN_POINT('',(-22.0750360153461,26.4155367745563,-77.3107734492734));
#44112=CARTESIAN_POINT('',(-26.7730018951938,23.5482270531954,6.06297359389933));
#44113=CARTESIAN_POINT('Ctrl Pts',(-22.0750360103879,26.4155367720035,6.90165778540197));
#44114=CARTESIAN_POINT('Ctrl Pts',(-22.046006365424,26.4005906067135,6.89979682548396));
#44115=CARTESIAN_POINT('Ctrl Pts',(-22.0172022087877,26.3852024195089,6.89794726638968));
#44116=CARTESIAN_POINT('Ctrl Pts',(-21.6939193491592,26.2061239265263,6.87710186694981));
#44117=CARTESIAN_POINT('Ctrl Pts',(-21.4266592779431,25.997693552159,6.85877232401689));
#44118=CARTESIAN_POINT('Ctrl Pts',(-21.1830085908105,25.7371831942219,6.83719381506162));
#44119=CARTESIAN_POINT('Ctrl Pts',(-21.1696175015189,25.7225983660945,6.83599042232142));
#44120=CARTESIAN_POINT('Ctrl Pts',(-21.1522230852041,25.7032993384788,6.83440377706279));
#44121=CARTESIAN_POINT('Ctrl Pts',(-21.1480975297732,25.6986954851709,6.8340256985072));
#44122=CARTESIAN_POINT('Ctrl Pts',(-21.1417452057096,25.6915655313944,6.83344080788177));
#44123=CARTESIAN_POINT('Ctrl Pts',(-21.139509091468,25.6890477456583,6.83323438870156));
#44124=CARTESIAN_POINT('Ctrl Pts',(-21.135281077454,25.684272096585,6.83284308837805));
#44125=CARTESIAN_POINT('Ctrl Pts',(-21.1332883863516,25.6820149359416,6.83265824066074));
#44126=CARTESIAN_POINT('Ctrl Pts',(-21.1287509406063,25.6768607409035,6.83223636082794));
#44127=CARTESIAN_POINT('Ctrl Pts',(-21.1262082198912,25.673961929264,6.8319992441738));
#44128=CARTESIAN_POINT('Ctrl Pts',(-21.1192036793097,25.6659474807564,6.83134410469524));
#44129=CARTESIAN_POINT('Ctrl Pts',(-21.114752828987,25.660822321384,6.83092562641787));
#44130=CARTESIAN_POINT('Ctrl Pts',(-21.1048963070175,25.6493998287103,6.82999399663437));
#44131=CARTESIAN_POINT('Ctrl Pts',(-21.0994987157859,25.6430956151274,6.82948051413785));
#44132=CARTESIAN_POINT('Ctrl Pts',(-20.9698599840793,25.4904924924361,6.81706724212718));
#44133=CARTESIAN_POINT('Ctrl Pts',(-20.8589337269602,25.3334339159391,6.80461688179875));
#44134=CARTESIAN_POINT('Ctrl Pts',(-20.6109767273053,24.9060292105629,6.77161545760273));
#44135=CARTESIAN_POINT('Ctrl Pts',(-20.4968380000018,24.6245603924638,6.750593806451));
#44136=CARTESIAN_POINT('Ctrl Pts',(-20.4199247206499,24.3166683567566,6.73051498775437));
#44137=CARTESIAN_POINT('Ctrl Pts',(-20.4163691721878,24.3019975228268,6.72956528926706));
#44138=CARTESIAN_POINT('Ctrl Pts',(-20.4120045236128,24.2834188922671,6.72837198542093));
#44139=CARTESIAN_POINT('Ctrl Pts',(-20.4110994958829,24.2795341581376,6.72812298540666));
#44140=CARTESIAN_POINT('Ctrl Pts',(-20.4096564429428,24.2732875498949,6.72772343660979));
#44141=CARTESIAN_POINT('Ctrl Pts',(-20.4091138679424,24.2709267475513,6.72757262649262));
#44142=CARTESIAN_POINT('Ctrl Pts',(-20.4081544551746,24.2667305720654,6.7273049163297));
#44143=CARTESIAN_POINT('Ctrl Pts',(-20.40773656335,24.2648954450269,6.72718795509802));
#44144=CARTESIAN_POINT('Ctrl Pts',(-20.40686355856,24.261046165568,6.7269428694706));
#44145=CARTESIAN_POINT('Ctrl Pts',(-20.4064087747535,24.2590319461667,6.72681476450295));
#44146=CARTESIAN_POINT('Ctrl Pts',(-20.4052181371182,24.2537349674164,6.7264782434823));
#44147=CARTESIAN_POINT('Ctrl Pts',(-20.4044854846694,24.2504514795185,6.72627001292226));
#44148=CARTESIAN_POINT('Ctrl Pts',(-20.4012513024476,24.2358494879168,6.72534561955464));
#44149=CARTESIAN_POINT('Ctrl Pts',(-20.3988056664917,24.2245184982396,6.72463264692908));
#44150=CARTESIAN_POINT('Ctrl Pts',(-20.3810712965737,24.1401477477398,6.71935446354672));
#44151=CARTESIAN_POINT('Ctrl Pts',(-20.3682610296761,24.0666033327369,6.71492388573853));
#44152=CARTESIAN_POINT('Ctrl Pts',(-20.3467453892228,23.9113599333451,6.70580221882579));
#44153=CARTESIAN_POINT('Ctrl Pts',(-20.3385862151283,23.8296402424921,6.7011325309346));
#44154=CARTESIAN_POINT('Ctrl Pts',(-20.3134896637612,23.420770136293,6.67805133062961));
#44155=CARTESIAN_POINT('Ctrl Pts',(-20.343374228077,23.0927377950879,6.66019628025002));
#44156=CARTESIAN_POINT('Ctrl Pts',(-20.423322578879,22.7702209584271,6.64014345864616));
#44157=CARTESIAN_POINT('Ctrl Pts',(-20.424477195653,22.7656069216687,6.63985609567741));
#44158=CARTESIAN_POINT('Ctrl Pts',(-20.4305605808731,22.7415232479177,6.63835362648593));
#44159=CARTESIAN_POINT('Ctrl Pts',(-20.4356609703429,22.722097775616,6.63713310076293));
#44160=CARTESIAN_POINT('Ctrl Pts',(-20.4425773981241,22.6967236955165,6.63552704331468));
#44161=CARTESIAN_POINT('Ctrl Pts',(-20.4442296346503,22.6907305877161,6.6351468450622));
#44162=CARTESIAN_POINT('Ctrl Pts',(-20.4468054394549,22.6814918655835,6.6345594018824));
#44163=CARTESIAN_POINT('Ctrl Pts',(-20.4477167883685,22.6782428353272,6.63435255545733));
#44164=CARTESIAN_POINT('Ctrl Pts',(-20.4494522552211,22.6720929207778,6.63396053739416));
#44165=CARTESIAN_POINT('Ctrl Pts',(-20.4502753458729,22.6691917482577,6.6337753994562));
#44166=CARTESIAN_POINT('Ctrl Pts',(-20.4521580718491,22.6625909461244,6.63335369778098));
#44167=CARTESIAN_POINT('Ctrl Pts',(-20.453220262844,22.6588920557281,6.63311705077825));
#44168=CARTESIAN_POINT('Ctrl Pts',(-20.4561680777488,22.6486956964794,6.63246377200874));
#44169=CARTESIAN_POINT('Ctrl Pts',(-20.4580675326544,22.6422022765518,6.63204668838587));
#44170=CARTESIAN_POINT('Ctrl Pts',(-20.46233067982,22.6277969039272,6.63111904959555));
#44171=CARTESIAN_POINT('Ctrl Pts',(-20.4647043561962,22.6198879778117,6.63060816906519));
#44172=CARTESIAN_POINT('Ctrl Pts',(-20.4720239761866,22.5958356445136,6.62904962881855));
#44173=CARTESIAN_POINT('Ctrl Pts',(-20.4770663509738,22.5797221016729,6.62799880953517));
#44174=CARTESIAN_POINT('Ctrl Pts',(-20.495767156126,22.5215686434922,6.62418174911801));
#44175=CARTESIAN_POINT('Ctrl Pts',(-20.5101630248468,22.4797727655538,6.62139141257565));
#44176=CARTESIAN_POINT('Ctrl Pts',(-20.5619399498669,22.3389257912565,6.6118241455995));
#44177=CARTESIAN_POINT('Ctrl Pts',(-20.6033366474104,22.2414334087648,6.60491957556738));
#44178=CARTESIAN_POINT('Ctrl Pts',(-20.7764727540966,21.8837403012387,6.57855809952534));
#44179=CARTESIAN_POINT('Ctrl Pts',(-20.9385025931201,21.6397902497186,6.55831209814716));
#44180=CARTESIAN_POINT('Ctrl Pts',(-21.1342628928692,21.4173825559542,6.53911914339749));
#44181=CARTESIAN_POINT('Ctrl Pts',(-21.1374191502464,21.4138126560536,6.53881089888965));
#44182=CARTESIAN_POINT('Ctrl Pts',(-21.1438745704015,21.40654377433,6.53818292836507));
#44183=CARTESIAN_POINT('Ctrl Pts',(-21.1471743745237,21.4028453741799,6.53786323908622));
#44184=CARTESIAN_POINT('Ctrl Pts',(-21.1769136767446,21.3696681403749,6.53499390903361));
#44185=CARTESIAN_POINT('Ctrl Pts',(-21.2038873820847,21.3406696413679,6.53247532233303));
#44186=CARTESIAN_POINT('Ctrl Pts',(-21.2350786635353,21.3083525045086,6.5296637444229));
#44187=CARTESIAN_POINT('Ctrl Pts',(-21.2387765880974,21.3045400089444,6.52933198245303));
#44188=CARTESIAN_POINT('Ctrl Pts',(-21.2441928024521,21.2989835381699,6.52884837246776));
#44189=CARTESIAN_POINT('Ctrl Pts',(-21.2459036566359,21.2972323768466,6.52869594652076));
#44190=CARTESIAN_POINT('Ctrl Pts',(-21.2489359849817,21.2941356750015,6.52842638112218));
#44191=CARTESIAN_POINT('Ctrl Pts',(-21.2502566455962,21.2927893441246,6.52830917750864));
#44192=CARTESIAN_POINT('Ctrl Pts',(-21.253016950354,21.2899803227989,6.52806462797385));
#44193=CARTESIAN_POINT('Ctrl Pts',(-21.2544568070134,21.2885178511726,6.52793729970334));
#44194=CARTESIAN_POINT('Ctrl Pts',(-21.2582210786203,21.2847017547258,6.5276050331568));
#44195=CARTESIAN_POINT('Ctrl Pts',(-21.2605477295864,21.282350323851,6.5274002719067));
#44196=CARTESIAN_POINT('Ctrl Pts',(-21.2706752821995,21.2721463792809,6.52651159652928));
#44197=CARTESIAN_POINT('Ctrl Pts',(-21.2785131105357,21.2643303788513,6.52583057634219));
#44198=CARTESIAN_POINT('Ctrl Pts',(-21.3356143589554,21.2079719031026,6.52091627001857));
#44199=CARTESIAN_POINT('Ctrl Pts',(-21.3863929366002,21.1609819193639,6.51679873201299));
#44200=CARTESIAN_POINT('Ctrl Pts',(-21.5615722752598,21.0090430687963,6.5032565669248));
#44201=CARTESIAN_POINT('Ctrl Pts',(-21.6924042783877,20.9118812162692,6.49419719150604));
#44202=CARTESIAN_POINT('Ctrl Pts',(-22.0040525793919,20.7151624564374,6.47360437978621));
#44203=CARTESIAN_POINT('Ctrl Pts',(-22.1881820698076,20.622245964243,6.46207669216467));
#44204=CARTESIAN_POINT('Ctrl Pts',(-22.3845953787916,20.5456916108724,6.44962619723221));
#44205=CARTESIAN_POINT('Ctrl Pts',(-22.3892919458963,20.5438737393855,6.44932842394971));
#44206=CARTESIAN_POINT('Ctrl Pts',(-22.3977050305282,20.5406399923075,6.44879489216104));
#44207=CARTESIAN_POINT('Ctrl Pts',(-22.4014199522392,20.5392199706179,6.44855926062721));
#44208=CARTESIAN_POINT('Ctrl Pts',(-22.4161209425321,20.5336317121309,6.44762661789192));
#44209=CARTESIAN_POINT('Ctrl Pts',(-22.4271270498774,20.5295167310265,6.44692797859766));
#44210=CARTESIAN_POINT('Ctrl Pts',(-22.4398224756366,20.524849119214,6.44612154417997));
#44211=CARTESIAN_POINT('Ctrl Pts',(-22.4414901432593,20.5242375476571,6.44601560006298));
#44212=CARTESIAN_POINT('Ctrl Pts',(-22.4548568348715,20.5193482117978,6.44516634533394));
#44213=CARTESIAN_POINT('Ctrl Pts',(-22.4665799446985,20.5151369742952,6.44442095495116));
#44214=CARTESIAN_POINT('Ctrl Pts',(-22.4892224478524,20.50715112033,6.44298001722597));
#44215=CARTESIAN_POINT('Ctrl Pts',(-22.5001383171428,20.5033670448694,6.44228478536496));
#44216=CARTESIAN_POINT('Ctrl Pts',(-22.515501609529,20.4981336008166,6.4413054133809));
#44217=CARTESIAN_POINT('Ctrl Pts',(-22.5199322875163,20.4966350649463,6.4410228657423));
#44218=CARTESIAN_POINT('Ctrl Pts',(-22.5436532586617,20.4886697054947,6.43950958875571));
#44219=CARTESIAN_POINT('Ctrl Pts',(-22.5630008658028,20.4823761298768,6.43827328081423));
#44220=CARTESIAN_POINT('Ctrl Pts',(-22.5883664207331,20.4743897722676,6.43664936089408));
#44221=CARTESIAN_POINT('Ctrl Pts',(-22.5943318245346,20.4725306134498,6.43626723148297));
#44222=CARTESIAN_POINT('Ctrl Pts',(-22.6035331807905,20.4696922801963,6.43567746280351));
#44223=CARTESIAN_POINT('Ctrl Pts',(-22.6067653534869,20.4687008224243,6.43547022718088));
#44224=CARTESIAN_POINT('Ctrl Pts',(-22.6128877026517,20.4668333483331,6.43507755475712));
#44225=CARTESIAN_POINT('Ctrl Pts',(-22.6157775639809,20.4659563044061,6.43489215190516));
#44226=CARTESIAN_POINT('Ctrl Pts',(-22.6223462617721,20.4639728498192,6.43447060327651));
#44227=CARTESIAN_POINT('Ctrl Pts',(-22.6260258473688,20.4628689539228,6.43423437537795));
#44228=CARTESIAN_POINT('Ctrl Pts',(-22.6357165598435,20.4599805635921,6.43361199655701));
#44229=CARTESIAN_POINT('Ctrl Pts',(-22.6417309145564,20.4582070354329,6.43322548726326));
#44230=CARTESIAN_POINT('Ctrl Pts',(-22.6552732148509,20.4542565701417,6.43235463894453));
#44231=CARTESIAN_POINT('Ctrl Pts',(-22.6628039818134,20.4520895209574,6.43186997880298));
#44232=CARTESIAN_POINT('Ctrl Pts',(-22.6854719037923,20.4456560419578,6.43040992685186));
#44233=CARTESIAN_POINT('Ctrl Pts',(-22.7006322903253,20.4414729753752,6.42943182560527));
#44234=CARTESIAN_POINT('Ctrl Pts',(-22.7546296289051,20.4269984643464,6.4259420439738));
#44235=CARTESIAN_POINT('Ctrl Pts',(-22.7936264280118,20.4173228361798,6.42341060107046));
#44236=CARTESIAN_POINT('Ctrl Pts',(-22.9077547074845,20.3912611645688,6.41596715302887));
#44237=CARTESIAN_POINT('Ctrl Pts',(-22.9833001333683,20.3768327116259,6.41099570278561));
#44238=CARTESIAN_POINT('Ctrl Pts',(-23.4107164266459,20.310949195724,6.38263305986548));
#44239=CARTESIAN_POINT('Ctrl Pts',(-23.7686284494603,20.3153150366037,6.35764705120673));
#44240=CARTESIAN_POINT('Ctrl Pts',(-24.1339161056737,20.380757715556,6.33404670373366));
#44241=CARTESIAN_POINT('Ctrl Pts',(-24.1492403069917,20.3836180051432,6.33306084782847));
#44242=CARTESIAN_POINT('Ctrl Pts',(-24.1732676732397,20.3882834178933,6.33152233916795));
#44243=CARTESIAN_POINT('Ctrl Pts',(-24.181984922879,20.39001350061,6.33096566342429));
#44244=CARTESIAN_POINT('Ctrl Pts',(-24.1937862844089,20.3924064587527,6.33021418092985));
#44245=CARTESIAN_POINT('Ctrl Pts',(-24.196876636973,20.3930378133149,6.33001759395106));
#44246=CARTESIAN_POINT('Ctrl Pts',(-24.2017452986749,20.3940399221212,6.32970820275201));
#44247=CARTESIAN_POINT('Ctrl Pts',(-24.2035242193302,20.3944076425355,6.32959522410017));
#44248=CARTESIAN_POINT('Ctrl Pts',(-24.2069586448425,20.3951206004879,6.32937723610095));
#44249=CARTESIAN_POINT('Ctrl Pts',(-24.2086141777296,20.3954656347064,6.32927221609421));
#44250=CARTESIAN_POINT('Ctrl Pts',(-24.2125621814721,20.3962916922006,6.32902191135627));
#44251=CARTESIAN_POINT('Ctrl Pts',(-24.2148543982613,20.3967739114579,6.3288766964779));
#44252=CARTESIAN_POINT('Ctrl Pts',(-24.221688765416,20.3982194567446,6.32844406036627));
#44253=CARTESIAN_POINT('Ctrl Pts',(-24.226229386799,20.3991901055379,6.32815705996215));
#44254=CARTESIAN_POINT('Ctrl Pts',(-24.2640042596012,20.4073506495708,6.3257729118487));
#44255=CARTESIAN_POINT('Ctrl Pts',(-24.2971265048018,20.4150566424196,6.32370497009363));
#44256=CARTESIAN_POINT('Ctrl Pts',(-24.4166090202242,20.4448557399992,6.31630673124075));
#44257=CARTESIAN_POINT('Ctrl Pts',(-24.5021715100984,20.470006467984,6.31112547956491));
#44258=CARTESIAN_POINT('Ctrl Pts',(-24.7080971166735,20.5399401213598,6.29870110993601));
#44259=CARTESIAN_POINT('Ctrl Pts',(-24.8270380848266,20.5884277238055,6.29156098297286));
#44260=CARTESIAN_POINT('Ctrl Pts',(-25.0033060885696,20.6728825366777,6.28063592505208));
#44261=CARTESIAN_POINT('Ctrl Pts',(-25.0629156682402,20.7037682609793,6.27687872971753));
#44262=CARTESIAN_POINT('Ctrl Pts',(-25.2079689090717,20.784769090454,6.26750180382441));
#44263=CARTESIAN_POINT('Ctrl Pts',(-25.2921455854084,20.8370019340267,6.26184941998072));
#44264=CARTESIAN_POINT('Ctrl Pts',(-25.4509608337096,20.9459891620317,6.25061248798056));
#44265=CARTESIAN_POINT('Ctrl Pts',(-25.5257906786898,21.0022874260732,6.24504671241347));
#44266=CARTESIAN_POINT('Ctrl Pts',(-25.6059718734445,21.0682693432697,6.23872563201846));
#44267=CARTESIAN_POINT('Ctrl Pts',(-25.613852930858,21.0748180347975,6.23810035590868));
#44268=CARTESIAN_POINT('Ctrl Pts',(-25.6248591313593,21.0840526213941,6.23722148706006));
#44269=CARTESIAN_POINT('Ctrl Pts',(-25.6280106164732,21.0867071430689,6.23696918037101));
#44270=CARTESIAN_POINT('Ctrl Pts',(-25.633773046982,21.0915798080311,6.23650663879889));
#44271=CARTESIAN_POINT('Ctrl Pts',(-25.6363855666468,21.093796087942,6.23629648074741));
#44272=CARTESIAN_POINT('Ctrl Pts',(-25.641391493376,21.0980565133499,6.23589291386902));
#44273=CARTESIAN_POINT('Ctrl Pts',(-25.6437854503558,21.1001000083162,6.23569953205845));
#44274=CARTESIAN_POINT('Ctrl Pts',(-25.6487794054461,21.1043755387444,6.2352953148756));
#44275=CARTESIAN_POINT('Ctrl Pts',(-25.6513788437711,21.1066082193906,6.23508445290831));
#44276=CARTESIAN_POINT('Ctrl Pts',(-25.6604857135541,21.114455464861,6.23434409883854));
#44277=CARTESIAN_POINT('Ctrl Pts',(-25.6669741978161,21.1200918747641,6.23381369958372));
#44278=CARTESIAN_POINT('Ctrl Pts',(-25.7279363085686,21.1734777585898,6.22880267010499));
#44279=CARTESIAN_POINT('Ctrl Pts',(-25.7808041410448,21.2230217530364,6.22424682819144));
#44280=CARTESIAN_POINT('Ctrl Pts',(-25.8863672380138,21.3288516101607,6.21469116878159));
#44281=CARTESIAN_POINT('Ctrl Pts',(-25.9388021965948,21.3853315238309,6.20968456413662));
#44282=CARTESIAN_POINT('Ctrl Pts',(-26.0984356979744,21.5701447927488,6.19359957542516));
#44283=CARTESIAN_POINT('Ctrl Pts',(-26.1976942936307,21.7049590923145,6.18227917186331));
#44284=CARTESIAN_POINT('Ctrl Pts',(-26.385149767485,22.0060262466604,6.15828133088249));
#44285=CARTESIAN_POINT('Ctrl Pts',(-26.4701908773643,22.1735698217201,6.14565133545971));
#44286=CARTESIAN_POINT('Ctrl Pts',(-26.5444987945367,22.3583043093952,6.13310229821836));
#44287=CARTESIAN_POINT('Ctrl Pts',(-26.5487559332182,22.3690545771117,6.13237685063465));
#44288=CARTESIAN_POINT('Ctrl Pts',(-26.5542286374427,22.383094696012,6.13143588523676));
#44289=CARTESIAN_POINT('Ctrl Pts',(-26.5554967496718,22.3863637707323,6.13121724944211));
#44290=CARTESIAN_POINT('Ctrl Pts',(-26.5574392526297,22.3913957026248,6.13088142325365));
#44291=CARTESIAN_POINT('Ctrl Pts',(-26.5581174291337,22.3931570802963,6.13076400419729));
#44292=CARTESIAN_POINT('Ctrl Pts',(-26.5594626013033,22.3966599705246,6.13053075725797));
#44293=CARTESIAN_POINT('Ctrl Pts',(-26.5601296289103,22.3984014562902,6.13041492819999));
#44294=CARTESIAN_POINT('Ctrl Pts',(-26.5616136323905,22.4022860061321,6.13015685235958));
#44295=CARTESIAN_POINT('Ctrl Pts',(-26.5624298304494,22.4044293588006,6.13001465321585));
#44296=CARTESIAN_POINT('Ctrl Pts',(-26.5648079855288,22.410694543972,6.12959956643231));
#44297=CARTESIAN_POINT('Ctrl Pts',(-26.5663637831,22.4148187329556,6.12932705002879));
#44298=CARTESIAN_POINT('Ctrl Pts',(-26.5775623326941,22.4446898619168,6.12735837866613));
#44299=CARTESIAN_POINT('Ctrl Pts',(-26.5868841043074,22.4705570828485,6.12568119690994));
#44300=CARTESIAN_POINT('Ctrl Pts',(-26.6153313660208,22.5527803750207,6.12042749104709));
#44301=CARTESIAN_POINT('Ctrl Pts',(-26.6332285367491,22.609551269335,6.1169142286083));
#44302=CARTESIAN_POINT('Ctrl Pts',(-26.7312643049135,22.9534719895913,6.09613034252577));
#44303=CARTESIAN_POINT('Ctrl Pts',(-26.7728145267785,23.2501041940918,6.0801402810687));
#44304=CARTESIAN_POINT('Ctrl Pts',(-26.7730018951938,23.5482270531954,6.06297359389933));
#44305=CARTESIAN_POINT('Ctrl Pts',(-26.7730018977802,23.5482311726679,6.06297335668936));
#44306=CARTESIAN_POINT('Ctrl Pts',(-26.7730788051402,23.6708482547567,6.0559127436403));
#44307=CARTESIAN_POINT('Ctrl Pts',(-26.7661579448812,23.7933597209949,6.04869386501434));
#44308=CARTESIAN_POINT('Ctrl Pts',(-26.7512603658681,23.9240797248258,6.0407013465646));
#44309=CARTESIAN_POINT('Ctrl Pts',(-26.7502081414363,23.9329822247001,6.0401556051449));
#44310=CARTESIAN_POINT('Ctrl Pts',(-26.7484845246578,23.9470609549099,6.03929025637791));
#44311=CARTESIAN_POINT('Ctrl Pts',(-26.7478376719193,23.9522401882923,6.03897142324126));
#44312=CARTESIAN_POINT('Ctrl Pts',(-26.7467162760709,23.9610450139207,6.03842855412925));
#44313=CARTESIAN_POINT('Ctrl Pts',(-26.7462481378307,23.9646714235785,6.0382047208235));
#44314=CARTESIAN_POINT('Ctrl Pts',(-26.745366876741,23.971407760695,6.03778847681095));
#44315=CARTESIAN_POINT('Ctrl Pts',(-26.7449553820585,23.974517899833,6.03759611783517));
#44316=CARTESIAN_POINT('Ctrl Pts',(-26.7440934146059,23.9809604197764,6.03719727766523));
#44317=CARTESIAN_POINT('Ctrl Pts',(-26.7436422664471,23.984292705011,6.03699077530287));
#44318=CARTESIAN_POINT('Ctrl Pts',(-26.7426037825683,23.9918739215338,6.03652048747307));
#44319=CARTESIAN_POINT('Ctrl Pts',(-26.7420131787647,23.996122392135,6.03625659872505));
#44320=CARTESIAN_POINT('Ctrl Pts',(-26.7401935549154,24.0090228426967,6.03545425576304));
#44321=CARTESIAN_POINT('Ctrl Pts',(-26.7389378311826,24.0176709612638,6.03491495551422));
#44322=CARTESIAN_POINT('Ctrl Pts',(-26.7298079334654,24.0787987764774,6.03109274104929));
#44323=CARTESIAN_POINT('Ctrl Pts',(-26.7206741577155,24.13107940475,6.02776999844887));
#44324=CARTESIAN_POINT('Ctrl Pts',(-26.7081839411293,24.193446072919,6.02373831377344));
#44325=CARTESIAN_POINT('Ctrl Pts',(-26.7060628935246,24.2037735138671,6.02306845820368));
#44326=CARTESIAN_POINT('Ctrl Pts',(-26.7015340952358,24.22528809917,6.02166829055093));
#44327=CARTESIAN_POINT('Ctrl Pts',(-26.6991173620891,24.236473184748,6.02093771102794));
#44328=CARTESIAN_POINT('Ctrl Pts',(-26.6878525796614,24.2872959023935,6.01760598638686));
#44329=CARTESIAN_POINT('Ctrl Pts',(-26.6783156105871,24.3267756404533,6.01498418704338));
#44330=CARTESIAN_POINT('Ctrl Pts',(-26.6632405694166,24.3843879054442,6.01110901577964));
#44331=CARTESIAN_POINT('Ctrl Pts',(-26.6582842970997,24.4026696060045,6.00987201017383));
#44332=CARTESIAN_POINT('Ctrl Pts',(-26.6333332557562,24.4915923868539,6.00381982056796));
#44333=CARTESIAN_POINT('Ctrl Pts',(-26.6110907155913,24.5615764395919,5.99894671390942));
#44334=CARTESIAN_POINT('Ctrl Pts',(-26.4874676544983,24.9089648013869,5.974255416881));
#44335=CARTESIAN_POINT('Ctrl Pts',(-26.3506847438287,25.1722644190277,5.95375494604774));
#44336=CARTESIAN_POINT('Ctrl Pts',(-26.1726660175558,25.4235448371405,5.93433269184722));
#44337=CARTESIAN_POINT('Ctrl Pts',(-26.1653164863685,25.4337909777991,5.93354126377052));
#44338=CARTESIAN_POINT('Ctrl Pts',(-26.1558694157481,25.4467994565751,5.93253742301117));
#44339=CARTESIAN_POINT('Ctrl Pts',(-26.1538274287666,25.4496017203235,5.93232123426044));
#44340=CARTESIAN_POINT('Ctrl Pts',(-26.1505485077167,25.4540862322637,5.93197536214675));
#44341=CARTESIAN_POINT('Ctrl Pts',(-26.1493144615574,25.4557705733665,5.93184547811886));
#44342=CARTESIAN_POINT('Ctrl Pts',(-26.14696839853,25.4589661796505,5.9315991007346));
#44343=CARTESIAN_POINT('Ctrl Pts',(-26.145856707072,25.4604776618163,5.93148258639653));
#44344=CARTESIAN_POINT('Ctrl Pts',(-26.1433087861723,25.4639355448314,5.93121607391791));
#44345=CARTESIAN_POINT('Ctrl Pts',(-26.1418716868908,25.465881297444,5.93106613783984));
#44346=CARTESIAN_POINT('Ctrl Pts',(-26.1374433668317,25.4718628929275,5.93060529527919));
#44347=CARTESIAN_POINT('Ctrl Pts',(-26.1344448810463,25.4758933861057,5.9302948958556));
#44348=CARTESIAN_POINT('Ctrl Pts',(-26.1118493414853,25.5061179455114,5.92796801147204));
#44349=CARTESIAN_POINT('Ctrl Pts',(-26.0918629922861,25.5320204799883,5.92597834542153));
#44350=CARTESIAN_POINT('Ctrl Pts',(-26.0667296507002,25.5635877626773,5.923552923011));
#44351=CARTESIAN_POINT('Ctrl Pts',(-26.0619532925958,25.5695432816245,5.92309531217441));
#44352=CARTESIAN_POINT('Ctrl Pts',(-26.0526432885964,25.5810675466576,5.92220963121138));
#44353=CARTESIAN_POINT('Ctrl Pts',(-26.0481121105289,25.5866382150697,5.92178142396375));
#44354=CARTESIAN_POINT('Ctrl Pts',(-26.0425885997663,25.5933826910343,5.92126282475652));
#44355=CARTESIAN_POINT('Ctrl Pts',(-26.0416140353925,25.5945709467474,5.92117145069227));
#44356=CARTESIAN_POINT('Ctrl Pts',(-25.849807248885,25.828094074253,5.9032127537389));
#44357=CARTESIAN_POINT('Ctrl Pts',(-25.6273811160765,26.0326105959562,5.8871072642681));
#44358=CARTESIAN_POINT('Ctrl Pts',(-25.2965594964805,26.2607419276318,5.8642336720173));
#44359=CARTESIAN_POINT('Ctrl Pts',(-25.2106731056661,26.3141884399565,5.85839115733837));
#44360=CARTESIAN_POINT('Ctrl Pts',(-25.0859532107066,26.3838873527244,5.84993457362148));
#44361=CARTESIAN_POINT('Ctrl Pts',(-25.0490931158048,26.4035557995752,5.84743889864058));
#44362=CARTESIAN_POINT('Ctrl Pts',(-24.9899479618824,26.4336531679362,5.84343431589864));
#44363=CARTESIAN_POINT('Ctrl Pts',(-24.9679071755853,26.4445533832869,5.84194198948813));
#44364=CARTESIAN_POINT('Ctrl Pts',(-24.9399831596205,26.4579676474108,5.84005059667114));
#44365=CARTESIAN_POINT('Ctrl Pts',(-24.9342138516625,26.4607180402109,5.83965978273793));
#44366=CARTESIAN_POINT('Ctrl Pts',(-24.9255442297187,26.464819488344,5.83907243034146));
#44367=CARTESIAN_POINT('Ctrl Pts',(-24.9226499989544,26.466183427856,5.83887633926477));
#44368=CARTESIAN_POINT('Ctrl Pts',(-24.9167272993387,26.4689637969299,5.83847503589178));
#44369=CARTESIAN_POINT('Ctrl Pts',(-24.9136986486562,26.4703798279657,5.83826981009486));
#44370=CARTESIAN_POINT('Ctrl Pts',(-24.9076074114677,26.4732162142819,5.83785702842776));
#44371=CARTESIAN_POINT('Ctrl Pts',(-24.9045447859199,26.4746364752587,5.83764946961424));
#44372=CARTESIAN_POINT('Ctrl Pts',(-24.8958293382696,26.4786615467764,5.83705876306828));
#44373=CARTESIAN_POINT('Ctrl Pts',(-24.8901712167838,26.4812547866381,5.83667521622037));
#44374=CARTESIAN_POINT('Ctrl Pts',(-24.8661685927903,26.492171682046,5.83504788219857));
#44375=CARTESIAN_POINT('Ctrl Pts',(-24.8477540863078,26.5003394885749,5.83379874376687));
#44376=CARTESIAN_POINT('Ctrl Pts',(-24.8110792609782,26.5161969093896,5.83130920106765));
#44377=CARTESIAN_POINT('Ctrl Pts',(-24.7928221909294,26.5238918350581,5.83006904572971));
#44378=CARTESIAN_POINT('Ctrl Pts',(-24.7671195747605,26.5344468523977,5.82832176093346));
#44379=CARTESIAN_POINT('Ctrl Pts',(-24.7597323330181,26.5374484999179,5.82781941280882));
#44380=CARTESIAN_POINT('Ctrl Pts',(-24.745911335889,26.5430046939857,5.82687924866301));
#44381=CARTESIAN_POINT('Ctrl Pts',(-24.7394803293032,26.5455659919426,5.82644166006604));
#44382=CARTESIAN_POINT('Ctrl Pts',(-24.7274897028574,26.5502968349387,5.82562553793013));
#44383=CARTESIAN_POINT('Ctrl Pts',(-24.7219322019276,26.552471698943,5.82524718128342));
#44384=CARTESIAN_POINT('Ctrl Pts',(-24.7125820818593,26.5561008442503,5.82461045959413));
#44385=CARTESIAN_POINT('Ctrl Pts',(-24.7087926806107,26.5575634209094,5.82435236543096));
#44386=CARTESIAN_POINT('Ctrl Pts',(-24.6918841220338,26.5640528329838,5.82320053090046));
#44387=CARTESIAN_POINT('Ctrl Pts',(-24.678735094805,26.5690009542944,5.82230426010669));
#44388=CARTESIAN_POINT('Ctrl Pts',(-24.6330457337568,26.5858541262252,5.81918803896817));
#44389=CARTESIAN_POINT('Ctrl Pts',(-24.6003469055514,26.5973199453145,5.81695443881186));
#44390=CARTESIAN_POINT('Ctrl Pts',(-24.4155799677924,26.6587810433475,5.80431500092033));
#44391=CARTESIAN_POINT('Ctrl Pts',(-24.2601522704044,26.6979140786884,5.79359712790687));
#44392=CARTESIAN_POINT('Ctrl Pts',(-24.0851301336834,26.7283547260324,5.78158687802584));
#44393=CARTESIAN_POINT('Ctrl Pts',(-24.0677580919096,26.7312296769987,5.78039561856338));
#44394=CARTESIAN_POINT('Ctrl Pts',(-24.030565466361,26.7370720555219,5.77784767530869));
#44395=CARTESIAN_POINT('Ctrl Pts',(-24.0107389562223,26.7399972620547,5.77649092698763));
#44396=CARTESIAN_POINT('Ctrl Pts',(-23.9679475341717,26.7459034303317,5.77356703035208));
#44397=CARTESIAN_POINT('Ctrl Pts',(-23.9449750815039,26.7488221957486,5.77200004290516));
#44398=CARTESIAN_POINT('Ctrl Pts',(-23.894740328477,26.7546553378737,5.76858126917683));
#44399=CARTESIAN_POINT('Ctrl Pts',(-23.8674680785046,26.7574699405713,5.7667302389359));
#44400=CARTESIAN_POINT('Ctrl Pts',(-23.7457701323822,26.7684621488717,5.75849976883083));
#44401=CARTESIAN_POINT('Ctrl Pts',(-23.6510402228595,26.7728205441744,5.75217070720347));
#44402=CARTESIAN_POINT('Ctrl Pts',(-23.514829734828,26.7730740352416,5.74329381802271));
#44403=CARTESIAN_POINT('Ctrl Pts',(-23.473409436445,26.7723525801453,5.74062435334669));
#44404=CARTESIAN_POINT('Ctrl Pts',(-23.4112938818087,26.7700720753166,5.73667713749036));
#44405=CARTESIAN_POINT('Ctrl Pts',(-23.3905824827673,26.7691114800839,5.73537036818875));
#44406=CARTESIAN_POINT('Ctrl Pts',(-23.3658110665697,26.7677228930343,5.73381980122999));
#44407=CARTESIAN_POINT('Ctrl Pts',(-23.3617413896576,26.7674870164535,5.73356545950237));
#44408=CARTESIAN_POINT('Ctrl Pts',(-23.3554533756924,26.7671105938254,5.73317310806402));
#44409=CARTESIAN_POINT('Ctrl Pts',(-23.3532347367553,26.7669754746327,5.73303479334844));
#44410=CARTESIAN_POINT('Ctrl Pts',(-23.3493404521675,26.7667342614434,5.73279222994697));
#44411=CARTESIAN_POINT('Ctrl Pts',(-23.3476647564267,26.7666291537423,5.7326879257588));
#44412=CARTESIAN_POINT('Ctrl Pts',(-23.3441130437561,26.7664035865907,5.73246699653627));
#44413=CARTESIAN_POINT('Ctrl Pts',(-23.3422370554818,26.7662827955598,5.73235039081233));
#44414=CARTESIAN_POINT('Ctrl Pts',(-23.3368995816647,26.7659344368019,5.73201887579972));
#44415=CARTESIAN_POINT('Ctrl Pts',(-23.333438342883,26.7657029206635,5.7318041898975));
#44416=CARTESIAN_POINT('Ctrl Pts',(-23.3187531401536,26.7646968337508,5.73089455385596));
#44417=CARTESIAN_POINT('Ctrl Pts',(-23.3075327229963,26.763869068029,5.73020257061449));
#44418=CARTESIAN_POINT('Ctrl Pts',(-23.2909229678065,26.7625562243158,5.72918241102737));
#44419=CARTESIAN_POINT('Ctrl Pts',(-23.28553029882,26.7621163172079,5.72885185221613));
#44420=CARTESIAN_POINT('Ctrl Pts',(-22.9952102458591,26.7376973084817,5.71108992595839));
#44421=CARTESIAN_POINT('Ctrl Pts',(-22.7146851389304,26.6759147574256,5.69561502083473));
#44422=CARTESIAN_POINT('Ctrl Pts',(-22.3206690118792,26.532202931748,5.67203495157881));
#44423=CARTESIAN_POINT('Ctrl Pts',(-22.1983456332645,26.478775513242,5.66444346522528));
#44424=CARTESIAN_POINT('Ctrl Pts',(-22.0781380349912,26.4171322838288,5.65650890082168));
#44425=CARTESIAN_POINT('Ctrl Pts',(-22.0765866962736,26.4163351561205,5.65640642003244));
#44426=CARTESIAN_POINT('Ctrl Pts',(-22.0750360153137,26.4155367745396,5.65630390104212));
#44427=CARTESIAN_POINT('Ctrl Pts',(-22.0750360281848,26.4155367811664,5.40632238256859));
#44428=CARTESIAN_POINT('Ctrl Pts',(-22.1527963909306,26.4555723798902,5.41123831454265));
#44429=CARTESIAN_POINT('Ctrl Pts',(-22.2321597963147,26.4924287425938,5.41619338139705));
#44430=CARTESIAN_POINT('Ctrl Pts',(-22.3901205810958,26.5581088994348,5.42605094954073));
#44431=CARTESIAN_POINT('Ctrl Pts',(-22.4685253872204,26.5871869715262,5.43094162592195));
#44432=CARTESIAN_POINT('Ctrl Pts',(-22.5910746905245,26.627288871437,5.43863918610307));
#44433=CARTESIAN_POINT('Ctrl Pts',(-22.6344730309378,26.6404826775678,5.44137490383914));
#44434=CARTESIAN_POINT('Ctrl Pts',(-22.685576553372,26.6548479623116,5.44461241544078));
#44435=CARTESIAN_POINT('Ctrl Pts',(-22.6930268245531,26.6569133468898,5.44508479890216));
#44436=CARTESIAN_POINT('Ctrl Pts',(-22.7044215157217,26.6600281046258,5.44580790328134));
#44437=CARTESIAN_POINT('Ctrl Pts',(-22.7083606532161,26.6610968361063,5.44605799397193));
#44438=CARTESIAN_POINT('Ctrl Pts',(-22.7155312108755,26.6630276704382,5.44651345461904));
#44439=CARTESIAN_POINT('Ctrl Pts',(-22.7187619676795,26.6638922330135,5.44671874429687));
#44440=CARTESIAN_POINT('Ctrl Pts',(-22.7252461255434,26.665616606121,5.44713092120141));
#44441=CARTESIAN_POINT('Ctrl Pts',(-22.7284995390503,26.6664763531428,5.44733781020008));
#44442=CARTESIAN_POINT('Ctrl Pts',(-22.7377218001677,26.6688979811658,5.44792449637284));
#44443=CARTESIAN_POINT('Ctrl Pts',(-22.7436937710024,26.6704478130651,5.44830468390117));
#44444=CARTESIAN_POINT('Ctrl Pts',(-22.7687529812387,26.6768743701678,5.44990117477486));
#44445=CARTESIAN_POINT('Ctrl Pts',(-22.7878799616148,26.6815930920325,5.45112258144023));
#44446=CARTESIAN_POINT('Ctrl Pts',(-22.8117416350575,26.6872483045731,5.4526501137397));
#44447=CARTESIAN_POINT('Ctrl Pts',(-22.8164370732838,26.6883499960985,5.45295087890532));
#44448=CARTESIAN_POINT('Ctrl Pts',(-22.8327017304964,26.6921276753268,5.45399334323447));
#44449=CARTESIAN_POINT('Ctrl Pts',(-22.8442831475457,26.694750232922,5.45473675354819));
#44450=CARTESIAN_POINT('Ctrl Pts',(-22.8674822425642,26.6998689357183,5.45622818715308));
#44451=CARTESIAN_POINT('Ctrl Pts',(-22.879099758761,26.7023649518838,5.45697620163019));
#44452=CARTESIAN_POINT('Ctrl Pts',(-22.8923346813743,26.7051319826366,5.45782968213867));
#44453=CARTESIAN_POINT('Ctrl Pts',(-22.8939389266158,26.705466106006,5.45793315724208));
#44454=CARTESIAN_POINT('Ctrl Pts',(-22.9023922451765,26.7072199906981,5.45847851994595));
#44455=CARTESIAN_POINT('Ctrl Pts',(-22.9092456311313,26.7086186663045,5.45892106781193));
#44456=CARTESIAN_POINT('Ctrl Pts',(-22.9194457635329,26.7106657965379,5.45958033363931));
#44457=CARTESIAN_POINT('Ctrl Pts',(-22.9227891057499,26.7113312767301,5.45979652087203));
#44458=CARTESIAN_POINT('Ctrl Pts',(-22.9301837741407,26.7127909650504,5.4602748897395));
#44459=CARTESIAN_POINT('Ctrl Pts',(-22.9342355784513,26.7135826946103,5.46053714761841));
#44460=CARTESIAN_POINT('Ctrl Pts',(-22.9441705717884,26.7155041976366,5.46118055226377));
#44461=CARTESIAN_POINT('Ctrl Pts',(-22.9500553943893,26.7166253534695,5.46156196280872));
#44462=CARTESIAN_POINT('Ctrl Pts',(-22.9763409666862,26.7215572775595,5.46326694734642));
#44463=CARTESIAN_POINT('Ctrl Pts',(-22.9967747673052,26.7251872725367,5.46459599173609));
#44464=CARTESIAN_POINT('Ctrl Pts',(-23.3158327622133,26.7786931515335,5.48540477581826));
#44465=CARTESIAN_POINT('Ctrl Pts',(-23.6199644741039,26.7864322828912,5.50622337556283));
#44466=CARTESIAN_POINT('Ctrl Pts',(-23.9883285605163,26.743816873924,5.53101933811224));
#44467=CARTESIAN_POINT('Ctrl Pts',(-24.0557790674879,26.7338366531908,5.53553233446592));
#44468=CARTESIAN_POINT('Ctrl Pts',(-24.1721153258687,26.7128319837487,5.54321597682523));
#44469=CARTESIAN_POINT('Ctrl Pts',(-24.2211542572648,26.7027933607203,5.5464234193737));
#44470=CARTESIAN_POINT('Ctrl Pts',(-24.2758636829127,26.6902593658756,5.54995150318833));
#44471=CARTESIAN_POINT('Ctrl Pts',(-24.2817809423806,26.6888860954037,5.55033242920677));
#44472=CARTESIAN_POINT('Ctrl Pts',(-24.2909409929071,26.6867329300221,5.55092104367419));
#44473=CARTESIAN_POINT('Ctrl Pts',(-24.2941864768339,26.6859647269023,5.55112938691081));
#44474=CARTESIAN_POINT('Ctrl Pts',(-24.2995835408699,26.6846783959997,5.55147549772328));
#44475=CARTESIAN_POINT('Ctrl Pts',(-24.3017357805697,26.6841630899055,5.55161342630976));
#44476=CARTESIAN_POINT('Ctrl Pts',(-24.3059210532599,26.6831564597769,5.55188145998747));
#44477=CARTESIAN_POINT('Ctrl Pts',(-24.3079541413923,26.6826653729082,5.5520115787169));
#44478=CARTESIAN_POINT('Ctrl Pts',(-24.3117598374919,26.6817421955005,5.55225498514339));
#44479=CARTESIAN_POINT('Ctrl Pts',(-24.3135325446572,26.6813105818019,5.55236829941502));
#44480=CARTESIAN_POINT('Ctrl Pts',(-24.3175602344447,26.6803263075194,5.55262560813788));
#44481=CARTESIAN_POINT('Ctrl Pts',(-24.319814982708,26.6797727164655,5.55276954759721));
#44482=CARTESIAN_POINT('Ctrl Pts',(-24.3255398997912,26.6783605602793,5.55313475482223));
#44483=CARTESIAN_POINT('Ctrl Pts',(-24.3290092522136,26.6774986544286,5.55335582897626));
#44484=CARTESIAN_POINT('Ctrl Pts',(-24.348063417831,26.6727312731513,5.55456868958115));
#44485=CARTESIAN_POINT('Ctrl Pts',(-24.3636206541268,26.6687149771228,5.5555541433478));
#44486=CARTESIAN_POINT('Ctrl Pts',(-24.6806651840772,26.5843319309292,5.57555061034941));
#44487=CARTESIAN_POINT('Ctrl Pts',(-24.9689874130604,26.4607057467485,5.59225749175479));
#44488=CARTESIAN_POINT('Ctrl Pts',(-25.3030797971255,26.2558169366057,5.61442016861978));
#44489=CARTESIAN_POINT('Ctrl Pts',(-25.3695126912894,26.2116006054066,5.61897627918916));
#44490=CARTESIAN_POINT('Ctrl Pts',(-25.5116683487789,26.1091731238215,5.6291510190953));
#44491=CARTESIAN_POINT('Ctrl Pts',(-25.5865794939861,26.0499718022262,5.63479805206794));
#44492=CARTESIAN_POINT('Ctrl Pts',(-25.6718188270182,25.9762312392442,5.64162817813586));
#44493=CARTESIAN_POINT('Ctrl Pts',(-25.6847975151681,25.9648195591982,5.64267973781968));
#44494=CARTESIAN_POINT('Ctrl Pts',(-25.7018872896687,25.9495476809719,5.6440801244155));
#44495=CARTESIAN_POINT('Ctrl Pts',(-25.7060810972827,25.9457801437716,5.64442504913626));
#44496=CARTESIAN_POINT('Ctrl Pts',(-25.7129517103185,25.9395752246995,5.64499223415765));
#44497=CARTESIAN_POINT('Ctrl Pts',(-25.7156343447951,25.9371442912539,5.64521422125183));
#44498=CARTESIAN_POINT('Ctrl Pts',(-25.7208253997667,25.932424338826,5.64564480982305));
#44499=CARTESIAN_POINT('Ctrl Pts',(-25.7233343105921,25.9301358642101,5.64585338800971));
#44500=CARTESIAN_POINT('Ctrl Pts',(-25.7291195391586,25.9248421577146,5.64633542918354));
#44501=CARTESIAN_POINT('Ctrl Pts',(-25.7323932590183,25.9218341082076,5.64660901214717));
#44502=CARTESIAN_POINT('Ctrl Pts',(-25.7411556841848,25.9137492714149,5.64734346012603));
#44503=CARTESIAN_POINT('Ctrl Pts',(-25.7466329399245,25.908660164631,5.6478048524037));
#44504=CARTESIAN_POINT('Ctrl Pts',(-25.7850605141236,25.8727058106497,5.65105823434949));
#44505=CARTESIAN_POINT('Ctrl Pts',(-25.8173753456759,25.8411715095583,5.65387905699424));
#44506=CARTESIAN_POINT('Ctrl Pts',(-25.8538241279906,25.8040765109968,5.65716266604942));
#44507=CARTESIAN_POINT('Ctrl Pts',(-25.8586167535975,25.7991676583308,5.65759650997082));
#44508=CARTESIAN_POINT('Ctrl Pts',(-25.8677171125332,25.7897868658124,5.65842429464836));
#44509=CARTESIAN_POINT('Ctrl Pts',(-25.8720276727756,25.785317700886,5.65881811248597));
#44510=CARTESIAN_POINT('Ctrl Pts',(-25.8868340968147,25.7698774280966,5.66017680174864));
#44511=CARTESIAN_POINT('Ctrl Pts',(-25.8972652073454,25.758844748262,5.66114436789616));
#44512=CARTESIAN_POINT('Ctrl Pts',(-25.9095400846546,25.7456768078444,5.66229536958803));
#44513=CARTESIAN_POINT('Ctrl Pts',(-25.9114596287637,25.7436121817592,5.66247572671434));
#44514=CARTESIAN_POINT('Ctrl Pts',(-25.9399292869548,25.7129100596076,5.66515609662126));
#44515=CARTESIAN_POINT('Ctrl Pts',(-25.9659585242726,25.6837958129243,5.66767674708013));
#44516=CARTESIAN_POINT('Ctrl Pts',(-26.0037643115757,25.6399303097492,5.67144344623523));
#44517=CARTESIAN_POINT('Ctrl Pts',(-26.0159513176634,25.6255363064559,5.67267462499127));
#44518=CARTESIAN_POINT('Ctrl Pts',(-26.167243159694,25.443632386992,5.68817247413242));
#44519=CARTESIAN_POINT('Ctrl Pts',(-26.2891406853652,25.2625610524322,5.70301018125796));
#44520=CARTESIAN_POINT('Ctrl Pts',(-26.4299672463416,24.9993530736216,5.72313861301102));
#44521=CARTESIAN_POINT('Ctrl Pts',(-26.4654021567287,24.9266802334914,5.72855297554233));
#44522=CARTESIAN_POINT('Ctrl Pts',(-26.527387766687,24.7863940628209,5.73864900096001));
#44523=CARTESIAN_POINT('Ctrl Pts',(-26.5544605580201,24.7190622323026,5.74334598832455));
#44524=CARTESIAN_POINT('Ctrl Pts',(-26.5831311666554,24.6401583053523,5.74863486150997));
#44525=CARTESIAN_POINT('Ctrl Pts',(-26.5869659837205,24.6294276006317,5.74934959185833));
#44526=CARTESIAN_POINT('Ctrl Pts',(-26.591852313135,24.6155222208977,5.75026970386431));
#44527=CARTESIAN_POINT('Ctrl Pts',(-26.592955850827,24.6123661099792,5.75047813882302));
#44528=CARTESIAN_POINT('Ctrl Pts',(-26.5947314830746,24.6072623339677,5.75081454277809));
#44529=CARTESIAN_POINT('Ctrl Pts',(-26.5954066212884,24.6053157422107,5.75094269346581));
#44530=CARTESIAN_POINT('Ctrl Pts',(-26.5966954034865,24.6015883197709,5.75118778465723));
#44531=CARTESIAN_POINT('Ctrl Pts',(-26.5973093510205,24.5998076041877,5.75130474287788));
#44532=CARTESIAN_POINT('Ctrl Pts',(-26.598712389226,24.5957265742201,5.75157249039693));
#44533=CARTESIAN_POINT('Ctrl Pts',(-26.5995004393128,24.5934258991435,5.75172321723081));
#44534=CARTESIAN_POINT('Ctrl Pts',(-26.6019733991446,24.5861794639706,5.75219728985586));
#44535=CARTESIAN_POINT('Ctrl Pts',(-26.6036488969936,24.5812304650825,5.75252007651023));
#44536=CARTESIAN_POINT('Ctrl Pts',(-26.6172131458675,24.5408419771263,5.7551464674736));
#44537=CARTESIAN_POINT('Ctrl Pts',(-26.6284971395042,24.5052003253937,5.7574149381736));
#44538=CARTESIAN_POINT('Ctrl Pts',(-26.7276756842679,24.171887398887,5.77824357025283));
#44539=CARTESIAN_POINT('Ctrl Pts',(-26.7727688909504,23.8631384923526,5.79482711162516));
#44540=CARTESIAN_POINT('Ctrl Pts',(-26.7730558073513,23.4803904694763,5.81660196983098));
#44541=CARTESIAN_POINT('Ctrl Pts',(-26.7706784790624,23.4081346848806,5.820757844145));
#44542=CARTESIAN_POINT('Ctrl Pts',(-26.7639330475648,23.3068846978194,5.8266849154569));
#44543=CARTESIAN_POINT('Ctrl Pts',(-26.7615959060808,23.2777749763216,5.8284009460084));
#44544=CARTESIAN_POINT('Ctrl Pts',(-26.7578948780875,23.2383946924825,5.83074071663151));
#44545=CARTESIAN_POINT('Ctrl Pts',(-26.7568765622641,23.2280925445392,5.83135451323139));
#44546=CARTESIAN_POINT('Ctrl Pts',(-26.7502995805126,23.1646771671542,5.83514359689672));
#44547=CARTESIAN_POINT('Ctrl Pts',(-26.7434713374447,23.111706501012,5.83835562339637));
#44548=CARTESIAN_POINT('Ctrl Pts',(-26.7339956421314,23.0502784946369,5.84214330286811));
#44549=CARTESIAN_POINT('Ctrl Pts',(-26.7326254973083,23.0416303375923,5.84267800323797));
#44550=CARTESIAN_POINT('Ctrl Pts',(-26.7305311035279,23.0287506646893,5.8434765296463));
#44551=CARTESIAN_POINT('Ctrl Pts',(-26.7298336073664,23.0245147884245,5.84373950447742));
#44552=CARTESIAN_POINT('Ctrl Pts',(-26.7285745700901,23.0169628408019,5.84420898790239));
#44553=CARTESIAN_POINT('Ctrl Pts',(-26.728016296591,23.0136462248568,5.84441539219418));
#44554=CARTESIAN_POINT('Ctrl Pts',(-26.7268284589082,23.0066563299915,5.84485086267765));
#44555=CARTESIAN_POINT('Ctrl Pts',(-26.7261977130818,23.0029832593101,5.84507996623825));
#44556=CARTESIAN_POINT('Ctrl Pts',(-26.7245151153017,22.9932857343654,5.84568555894803));
#44557=CARTESIAN_POINT('Ctrl Pts',(-26.7234524875928,22.9872631871438,5.84606239114273));
#44558=CARTESIAN_POINT('Ctrl Pts',(-26.7185702282646,22.9600454824409,5.84776876505117));
#44559=CARTESIAN_POINT('Ctrl Pts',(-26.7145554076472,22.9388863072757,5.84910452239508));
#44560=CARTESIAN_POINT('Ctrl Pts',(-26.6835971495884,22.784209527204,5.85893853321938));
#44561=CARTESIAN_POINT('Ctrl Pts',(-26.6484288569967,22.6524969504501,5.86770137465535));
#44562=CARTESIAN_POINT('Ctrl Pts',(-26.5511796703,22.3631850110311,5.88782992172599));
#44563=CARTESIAN_POINT('Ctrl Pts',(-26.4847991295889,22.2074491102723,5.8992892378728));
#44564=CARTESIAN_POINT('Ctrl Pts',(-26.3911234001205,22.0281896964588,5.91297077355295));
#44565=CARTESIAN_POINT('Ctrl Pts',(-26.37527267516,21.9989679695246,5.91521681489622));
#44566=CARTESIAN_POINT('Ctrl Pts',(-26.2848186485942,21.8381965332728,5.92764661797554));
#44567=CARTESIAN_POINT('Ctrl Pts',(-26.2014688471973,21.7117607734551,5.93770294965426));
#44568=CARTESIAN_POINT('Ctrl Pts',(-26.1038037485723,21.5841440177507,5.94780974515509));
#44569=CARTESIAN_POINT('Ctrl Pts',(-26.0980391603917,21.5766796787852,5.94840069764547));
#44570=CARTESIAN_POINT('Ctrl Pts',(-26.0902546704426,21.5666907988375,5.94919113042513));
#44571=CARTESIAN_POINT('Ctrl Pts',(-26.0882636916173,21.5641439331466,5.94939263308698));
#44572=CARTESIAN_POINT('Ctrl Pts',(-26.0851382107318,21.5601581836546,5.94970791797973));
#44573=CARTESIAN_POINT('Ctrl Pts',(-26.0840063149882,21.5587172732633,5.94982188620929));
#44574=CARTESIAN_POINT('Ctrl Pts',(-26.0818299870855,21.5559516528076,5.95004060718245));
#44575=CARTESIAN_POINT('Ctrl Pts',(-26.0807857505092,21.5546268060977,5.9501453725113));
#44576=CARTESIAN_POINT('Ctrl Pts',(-26.0783103137437,21.5514912302543,5.95039330005524));
#44577=CARTESIAN_POINT('Ctrl Pts',(-26.0768782097856,21.5496812201923,5.95053639623526));
#44578=CARTESIAN_POINT('Ctrl Pts',(-26.0726625460843,21.544364866753,5.95095664432539));
#44579=CARTESIAN_POINT('Ctrl Pts',(-26.0698736085411,21.5408627649384,5.95123341075544));
#44580=CARTESIAN_POINT('Ctrl Pts',(-26.0488276057264,21.5145477621958,5.95331263219949));
#44581=CARTESIAN_POINT('Ctrl Pts',(-26.0302675854028,21.491977334311,5.9550936148071));
#44582=CARTESIAN_POINT('Ctrl Pts',(-25.9666352924829,21.4167061224595,5.96103713860791));
#44583=CARTESIAN_POINT('Ctrl Pts',(-25.9201673205921,21.3652053340056,5.96511065761663));
#44584=CARTESIAN_POINT('Ctrl Pts',(-25.7596399773988,21.1984432560415,5.97848242196879));
#44585=CARTESIAN_POINT('Ctrl Pts',(-25.6385497292089,21.0902888794698,5.98747023165775));
#44586=CARTESIAN_POINT('Ctrl Pts',(-25.3162684750233,20.8434560493402,6.01017310538728));
#44587=CARTESIAN_POINT('Ctrl Pts',(-25.1065466313101,20.7176771584164,6.02396960561583));
#44588=CARTESIAN_POINT('Ctrl Pts',(-24.8707975533494,20.6104378088753,6.03968099973521));
#44589=CARTESIAN_POINT('Ctrl Pts',(-24.8568828061011,20.6042268915719,6.04060871319477));
#44590=CARTESIAN_POINT('Ctrl Pts',(-24.837833003299,20.5958854272061,6.04187947151056));
#44591=CARTESIAN_POINT('Ctrl Pts',(-24.8327355529198,20.5936690712461,6.04221957432103));
#44592=CARTESIAN_POINT('Ctrl Pts',(-24.8246555023374,20.5901807175809,6.04275879090372));
#44593=CARTESIAN_POINT('Ctrl Pts',(-24.8216766561265,20.5889000075966,6.04295760664374));
#44594=CARTESIAN_POINT('Ctrl Pts',(-24.8156605137503,20.5863242086915,6.04335919087196));
#44595=CARTESIAN_POINT('Ctrl Pts',(-24.8126231501236,20.5850292877295,6.0435619648091));
#44596=CARTESIAN_POINT('Ctrl Pts',(-24.8057050530171,20.5820924475287,6.04402387882783));
#44597=CARTESIAN_POINT('Ctrl Pts',(-24.8018230845308,20.5804534695467,6.04428311873339));
#44598=CARTESIAN_POINT('Ctrl Pts',(-24.7936930691182,20.5770397259692,6.04482614423634));
#44599=CARTESIAN_POINT('Ctrl Pts',(-24.7894444140477,20.5752664415432,6.0451099795932));
#44600=CARTESIAN_POINT('Ctrl Pts',(-24.7782843266129,20.5706365494942,6.04585569464476));
#44601=CARTESIAN_POINT('Ctrl Pts',(-24.7713667549985,20.5677948969837,6.04631808132575));
#44602=CARTESIAN_POINT('Ctrl Pts',(-24.7507690002305,20.5594172694581,6.04769537947554));
#44603=CARTESIAN_POINT('Ctrl Pts',(-24.7370607556829,20.5539512142618,6.04861265037018));
#44604=CARTESIAN_POINT('Ctrl Pts',(-24.5872650093573,20.4954105719419,6.05864393356026));
#44605=CARTESIAN_POINT('Ctrl Pts',(-24.4477769021305,20.451560295609,6.06806761322516));
#44606=CARTESIAN_POINT('Ctrl Pts',(-24.0095782453884,20.3458810971131,6.09789791554048));
#44607=CARTESIAN_POINT('Ctrl Pts',(-23.7047404822808,20.3168191900896,6.11910705652832));
#44608=CARTESIAN_POINT('Ctrl Pts',(-23.3973217112458,20.3311316797424,6.13898132329279));
#44609=CARTESIAN_POINT('Ctrl Pts',(-23.3942702431048,20.3312780954639,6.13917842830714));
#44610=CARTESIAN_POINT('Ctrl Pts',(-23.3850958304794,20.3317313789008,6.13977051907922));
#44611=CARTESIAN_POINT('Ctrl Pts',(-23.3789735116455,20.3320513811406,6.14016494427671));
#44612=CARTESIAN_POINT('Ctrl Pts',(-23.3376929327138,20.3343271744853,6.14281958040853));
#44613=CARTESIAN_POINT('Ctrl Pts',(-23.3025660670445,20.3368417027629,6.14505487186846));
#44614=CARTESIAN_POINT('Ctrl Pts',(-23.2628804181231,20.3403372362001,6.14754821341587));
#44615=CARTESIAN_POINT('Ctrl Pts',(-23.2582759539783,20.3407527864685,6.14783701028041));
#44616=CARTESIAN_POINT('Ctrl Pts',(-23.2513102548497,20.3413965509994,6.14827314970318));
#44617=CARTESIAN_POINT('Ctrl Pts',(-23.2489483761315,20.3416174643088,6.14842090102293));
#44618=CARTESIAN_POINT('Ctrl Pts',(-23.2448420039836,20.3420061191788,6.14867755056071));
#44619=CARTESIAN_POINT('Ctrl Pts',(-23.2430974037475,20.3421726758826,6.14878651593827));
#44620=CARTESIAN_POINT('Ctrl Pts',(-23.2394460844198,20.342524272532,6.14901441904033));
#44621=CARTESIAN_POINT('Ctrl Pts',(-23.237539395512,20.3427095893821,6.1491333404588));
#44622=CARTESIAN_POINT('Ctrl Pts',(-23.2329798252601,20.3431568520141,6.14941751632879));
#44623=CARTESIAN_POINT('Ctrl Pts',(-23.2303270935925,20.3434203903046,6.14958268023829));
#44624=CARTESIAN_POINT('Ctrl Pts',(-23.221338377157,20.3443246478362,6.1501417740387));
#44625=CARTESIAN_POINT('Ctrl Pts',(-23.2150039131638,20.3449808609985,6.1505348313706));
#44626=CARTESIAN_POINT('Ctrl Pts',(-23.1999547505997,20.3465849662621,6.1514664870729));
#44627=CARTESIAN_POINT('Ctrl Pts',(-23.1912418399859,20.3475496524718,6.15200416358644));
#44628=CARTESIAN_POINT('Ctrl Pts',(-23.0888365076416,20.3593110368342,6.15830456193933));
#44629=CARTESIAN_POINT('Ctrl Pts',(-22.9956475108253,20.3741811543608,6.16385052936836));
#44630=CARTESIAN_POINT('Ctrl Pts',(-22.5166689270653,20.472342077844,6.19199571541734));
#44631=CARTESIAN_POINT('Ctrl Pts',(-22.1479505743331,20.621870525189,6.21290550838715));
#44632=CARTESIAN_POINT('Ctrl Pts',(-21.7994448375427,20.8444907963224,6.23793649323792));
#44633=CARTESIAN_POINT('Ctrl Pts',(-21.7836209265199,20.8547958174311,6.23908457069594));
#44634=CARTESIAN_POINT('Ctrl Pts',(-21.7628342584268,20.8685944094484,6.2406083905364));
#44635=CARTESIAN_POINT('Ctrl Pts',(-21.7577892787743,20.8719639261937,6.24097945730516));
#44636=CARTESIAN_POINT('Ctrl Pts',(-21.7499780537418,20.8772129601438,6.24155591203842));
#44637=CARTESIAN_POINT('Ctrl Pts',(-21.7472051503858,20.8790825843372,6.24176092544901));
#44638=CARTESIAN_POINT('Ctrl Pts',(-21.7417186753603,20.8827942640434,6.24216731749311));
#44639=CARTESIAN_POINT('Ctrl Pts',(-21.7390049951073,20.8846361526466,6.24236868963623));
#44640=CARTESIAN_POINT('Ctrl Pts',(-21.7329877234052,20.888733758312,6.24281602358636));
#44641=CARTESIAN_POINT('Ctrl Pts',(-21.7296855147117,20.8909914875399,6.24306206173605));
#44642=CARTESIAN_POINT('Ctrl Pts',(-21.7228355616794,20.8956935586184,6.2435735727137));
#44643=CARTESIAN_POINT('Ctrl Pts',(-21.7192885000737,20.8981388768035,6.24383908250656));
#44644=CARTESIAN_POINT('Ctrl Pts',(-21.7101759274258,20.9044480118911,6.24452283894024));
#44645=CARTESIAN_POINT('Ctrl Pts',(-21.7046176990124,20.908322265799,6.24494148470431));
#44646=CARTESIAN_POINT('Ctrl Pts',(-21.6885168876838,20.9196206270153,6.24615884101707));
#44647=CARTESIAN_POINT('Ctrl Pts',(-21.6780066848585,20.9270904499103,6.24695930680067));
#44648=CARTESIAN_POINT('Ctrl Pts',(-21.5735151558612,21.0023026823741,6.25497620470894));
#44649=CARTESIAN_POINT('Ctrl Pts',(-21.483217321754,21.0749951593829,6.26238580172256));
#44650=CARTESIAN_POINT('Ctrl Pts',(-21.1566280115007,21.3682627506778,6.29110557425273));
#44651=CARTESIAN_POINT('Ctrl Pts',(-20.9500926625425,21.6190247166904,6.31362026413936));
#44652=CARTESIAN_POINT('Ctrl Pts',(-20.7823272901686,21.8995792651776,6.33491691902024));
#44653=CARTESIAN_POINT('Ctrl Pts',(-20.7803579426909,21.902886044983,6.33516740636562));
#44654=CARTESIAN_POINT('Ctrl Pts',(-20.7761215722387,21.9100285122519,6.3357072962221));
#44655=CARTESIAN_POINT('Ctrl Pts',(-20.7738565669367,21.9138653949012,6.33599660807987));
#44656=CARTESIAN_POINT('Ctrl Pts',(-20.768740919468,21.92257241645,6.33665150736507));
#44657=CARTESIAN_POINT('Ctrl Pts',(-20.7658950891353,21.9274453837391,6.33701687234371));
#44658=CARTESIAN_POINT('Ctrl Pts',(-20.7403143285272,21.9715131727814,6.3403103976156));
#44659=CARTESIAN_POINT('Ctrl Pts',(-20.7183940968227,22.0111784598735,6.3431994638552));
#44660=CARTESIAN_POINT('Ctrl Pts',(-20.6950063540492,22.0556918959894,6.34634793786345));
#44661=CARTESIAN_POINT('Ctrl Pts',(-20.6927064900214,22.0600938658941,6.34665828951856));
#44662=CARTESIAN_POINT('Ctrl Pts',(-20.6892829869668,22.0666835663226,6.34712136384703));
#44663=CARTESIAN_POINT('Ctrl Pts',(-20.6881516748567,22.0688672690902,6.3472745692147));
#44664=CARTESIAN_POINT('Ctrl Pts',(-20.6862080997611,22.0726293708434,6.34753808186566));
#44665=CARTESIAN_POINT('Ctrl Pts',(-20.685394641398,22.0742071455313,6.34764846522299));
#44666=CARTESIAN_POINT('Ctrl Pts',(-20.6837137232085,22.0774740596891,6.34787675235189));
#44667=CARTESIAN_POINT('Ctrl Pts',(-20.6828464541295,22.0791632908539,6.3479946434623));
#44668=CARTESIAN_POINT('Ctrl Pts',(-20.6808082753509,22.0831418221231,6.34827195374635));
#44669=CARTESIAN_POINT('Ctrl Pts',(-20.6796386084345,22.0854317651505,6.34843129368368));
#44670=CARTESIAN_POINT('Ctrl Pts',(-20.6758257718895,22.0929185417324,6.34895135902176));
#44671=CARTESIAN_POINT('Ctrl Pts',(-20.6731939443701,22.0981211870342,6.34931136942247));
#44672=CARTESIAN_POINT('Ctrl Pts',(-20.6187632505012,22.2064496453276,6.35677918888949));
#44673=CARTESIAN_POINT('Ctrl Pts',(-20.5725196660176,22.3122907233276,6.36354489169143));
#44674=CARTESIAN_POINT('Ctrl Pts',(-20.3987921155106,22.7763723759413,6.39192381602653));
#44675=CARTESIAN_POINT('Ctrl Pts',(-20.3295564568571,23.1530899055787,6.41218509498876));
#44676=CARTESIAN_POINT('Ctrl Pts',(-20.327435545196,23.5544120673456,6.43644400443614));
#44677=CARTESIAN_POINT('Ctrl Pts',(-20.3275325714907,23.5756031723385,6.43773132561476));
#44678=CARTESIAN_POINT('Ctrl Pts',(-20.3279302599021,23.6031396574205,6.43941287491131));
#44679=CARTESIAN_POINT('Ctrl Pts',(-20.328040701733,23.6094875998691,6.43980112439245));
#44680=CARTESIAN_POINT('Ctrl Pts',(-20.3282468041674,23.6196134411999,6.44042141415273));
#44681=CARTESIAN_POINT('Ctrl Pts',(-20.328330353619,23.6233915925089,6.44065307382721));
#44682=CARTESIAN_POINT('Ctrl Pts',(-20.3284991958094,23.6304639024051,6.44108712698656));
#44683=CARTESIAN_POINT('Ctrl Pts',(-20.3285828959775,23.633758097068,6.44128947017852));
#44684=CARTESIAN_POINT('Ctrl Pts',(-20.3287818555187,23.6411425105352,6.44174342767195));
#44685=CARTESIAN_POINT('Ctrl Pts',(-20.3288998525165,23.6452326444578,6.44199512765288));
#44686=CARTESIAN_POINT('Ctrl Pts',(-20.3292678196502,23.6571969694445,6.44273215481603));
#44687=CARTESIAN_POINT('Ctrl Pts',(-20.3295388725616,23.6650704401269,6.44321814347493));
#44688=CARTESIAN_POINT('Ctrl Pts',(-20.3302173455139,23.6828792196343,6.44431960564494));
#44689=CARTESIAN_POINT('Ctrl Pts',(-20.3306418827256,23.692813760903,6.44493561347629));
#44690=CARTESIAN_POINT('Ctrl Pts',(-20.3321390734126,23.7244194674938,6.44690043097967));
#44691=CARTESIAN_POINT('Ctrl Pts',(-20.333384592742,23.7460814827299,6.44825465081802));
#44692=CARTESIAN_POINT('Ctrl Pts',(-20.3390275281155,23.8295127085533,6.45350041325461));
#44693=CARTESIAN_POINT('Ctrl Pts',(-20.3449859587357,23.8911595863106,6.45744024440367));
#44694=CARTESIAN_POINT('Ctrl Pts',(-20.3736183205356,24.1187105038635,6.47222588172824));
#44695=CARTESIAN_POINT('Ctrl Pts',(-20.4074311517312,24.2829260760923,6.48339502353272));
#44696=CARTESIAN_POINT('Ctrl Pts',(-20.4933603184843,24.5807122107429,6.50432963492038));
#44697=CARTESIAN_POINT('Ctrl Pts',(-20.541924970244,24.7149001627361,6.51402983396284));
#44698=CARTESIAN_POINT('Ctrl Pts',(-20.642668495061,24.9444416631128,6.53072393770521));
#44699=CARTESIAN_POINT('Ctrl Pts',(-20.6910826124488,25.0412123988521,6.53779279858136));
#44700=CARTESIAN_POINT('Ctrl Pts',(-20.7475560566604,25.1411813446359,6.54499279424933));
#44701=CARTESIAN_POINT('Ctrl Pts',(-20.7508535721495,25.1469765172854,6.54540979239078));
#44702=CARTESIAN_POINT('Ctrl Pts',(-20.7554217573912,25.1549471605623,6.5459827547767));
#44703=CARTESIAN_POINT('Ctrl Pts',(-20.7566769984934,25.1571313850362,6.54613970615585));
#44704=CARTESIAN_POINT('Ctrl Pts',(-20.7588290898082,25.1608660603782,6.54640796293511));
#44705=CARTESIAN_POINT('Ctrl Pts',(-20.7597246711814,25.1624172349514,6.54651935069508));
#44706=CARTESIAN_POINT('Ctrl Pts',(-20.7614731403522,25.1654398153731,6.54673633633047));
#44707=CARTESIAN_POINT('Ctrl Pts',(-20.7623258973667,25.1669112886831,6.5468419419993));
#44708=CARTESIAN_POINT('Ctrl Pts',(-20.7643889091324,25.1704646282566,6.54709689219001));
#44709=CARTESIAN_POINT('Ctrl Pts',(-20.7656003358622,25.1725458188956,6.54724615994889));
#44710=CARTESIAN_POINT('Ctrl Pts',(-20.7693182820324,25.1789166915076,6.54770292636924));
#44711=CARTESIAN_POINT('Ctrl Pts',(-20.7718324044901,25.1832019626115,6.54800993096234));
#44712=CARTESIAN_POINT('Ctrl Pts',(-20.7981838412058,25.2278804127643,6.55120853065695));
#44713=CARTESIAN_POINT('Ctrl Pts',(-20.8228918702673,25.2677570518982,6.55404417511084));
#44714=CARTESIAN_POINT('Ctrl Pts',(-20.8971079950609,25.381892355827,6.56214701615865));
#44715=CARTESIAN_POINT('Ctrl Pts',(-20.9488428926592,25.4546555262145,6.56729628191907));
#44716=CARTESIAN_POINT('Ctrl Pts',(-21.0242540891823,25.5518999839783,6.5742908725811));
#44717=CARTESIAN_POINT('Ctrl Pts',(-21.045392429882,25.5782901538094,6.57620111199282));
#44718=CARTESIAN_POINT('Ctrl Pts',(-21.2476402070929,25.8227992959622,6.5940617134665));
#44719=CARTESIAN_POINT('Ctrl Pts',(-21.4563542578339,26.0164387658367,6.60956868193696));
#44720=CARTESIAN_POINT('Ctrl Pts',(-21.6910908424768,26.1826758605299,6.62661349338064));
#44721=CARTESIAN_POINT('Ctrl Pts',(-21.6944806058583,26.1850666291031,6.62685952638634));
#44722=CARTESIAN_POINT('Ctrl Pts',(-21.7007424301596,26.1894649569934,6.62731382846861));
#44723=CARTESIAN_POINT('Ctrl Pts',(-21.7036131708846,26.1914743914597,6.62752203097897));
#44724=CARTESIAN_POINT('Ctrl Pts',(-21.7121750511035,26.197446674774,6.62814277759251));
#44725=CARTESIAN_POINT('Ctrl Pts',(-21.7178756863467,26.2013958230617,6.62855580498542));
#44726=CARTESIAN_POINT('Ctrl Pts',(-21.7252110792776,26.2064424977994,6.6290869444804));
#44727=CARTESIAN_POINT('Ctrl Pts',(-21.7268341862455,26.2075569885702,6.62920444932175));
#44728=CARTESIAN_POINT('Ctrl Pts',(-21.7329337387332,26.2117369676924,6.6296459501258));
#44729=CARTESIAN_POINT('Ctrl Pts',(-21.7374168840679,26.2147926256837,6.6299702971106));
#44730=CARTESIAN_POINT('Ctrl Pts',(-21.7442329670014,26.2194132211194,6.63046320589802));
#44731=CARTESIAN_POINT('Ctrl Pts',(-21.7465602844139,26.2209864628549,6.63063146802716));
#44732=CARTESIAN_POINT('Ctrl Pts',(-21.7637254476448,26.2325572596121,6.63187220768163));
#44733=CARTESIAN_POINT('Ctrl Pts',(-21.7786440363856,26.2424339883102,6.63294902149212));
#44734=CARTESIAN_POINT('Ctrl Pts',(-21.8114845262292,26.2637845852591,6.63531663869885));
#44735=CARTESIAN_POINT('Ctrl Pts',(-21.8294392805941,26.2752061282996,6.63660928716948));
#44736=CARTESIAN_POINT('Ctrl Pts',(-21.8529046291673,26.2898087183467,6.63829684299885));
#44737=CARTESIAN_POINT('Ctrl Pts',(-21.8583136605233,26.29315261324,6.63868571866198));
#44738=CARTESIAN_POINT('Ctrl Pts',(-21.8669547850541,26.2984593211348,6.6393067763534));
#44739=CARTESIAN_POINT('Ctrl Pts',(-21.8701805163449,26.3004325047901,6.63953857612161));
#44740=CARTESIAN_POINT('Ctrl Pts',(-21.8762248421344,26.304115223277,6.63997284555408));
#44741=CARTESIAN_POINT('Ctrl Pts',(-21.8790426039066,26.3058261211017,6.64017526479139));
#44742=CARTESIAN_POINT('Ctrl Pts',(-21.885361828606,26.3096497907629,6.64062915410262));
#44743=CARTESIAN_POINT('Ctrl Pts',(-21.8888646933687,26.3117602244235,6.64088070945616));
#44744=CARTESIAN_POINT('Ctrl Pts',(-21.8991179127129,26.317911095361,6.64161691353699));
#44745=CARTESIAN_POINT('Ctrl Pts',(-21.9058790208888,26.3219334675595,6.64210222149582));
#44746=CARTESIAN_POINT('Ctrl Pts',(-21.9212037649373,26.3309747766079,6.643201903838));
#44747=CARTESIAN_POINT('Ctrl Pts',(-21.9297759663029,26.3359789693221,6.64381680996049));
#44748=CARTESIAN_POINT('Ctrl Pts',(-21.9571149497055,26.3517697544605,6.64577727768757));
#44749=CARTESIAN_POINT('Ctrl Pts',(-21.9759670438212,26.3624067362789,6.64712822195695));
#44750=CARTESIAN_POINT('Ctrl Pts',(-22.0214287485067,26.387457348192,6.65038429417828));
#44751=CARTESIAN_POINT('Ctrl Pts',(-22.0481352518283,26.4016866825092,6.6522956913974));
#44752=CARTESIAN_POINT('Ctrl Pts',(-22.0750360194354,26.4155367766617,6.65421995916067));
#44753=CARTESIAN_POINT('Origin',(-23.5502525316942,23.5502525316942,-77.3107734492734));
#44754=CARTESIAN_POINT('',(-22.075035838959,26.4155366837419,8.15244980096843));
#44755=CARTESIAN_POINT('',(-22.0750360380806,26.4155367862613,7.90859913775027));
#44756=CARTESIAN_POINT('',(-22.0750360153461,26.4155367745563,-77.3107734492734));
#44757=CARTESIAN_POINT('Ctrl Pts',(-22.075035838959,26.4155366837419,8.15244980096843));
#44758=CARTESIAN_POINT('Ctrl Pts',(-22.0034785551328,26.3786947881442,8.14702447166941));
#44759=CARTESIAN_POINT('Ctrl Pts',(-21.9332984506555,26.3391707970346,8.14163349505117));
#44760=CARTESIAN_POINT('Ctrl Pts',(-21.8252269562421,26.2728511734628,8.13329272431396));
#44761=CARTESIAN_POINT('Ctrl Pts',(-21.786330880127,26.2478139239187,8.1302826068504));
#44762=CARTESIAN_POINT('Ctrl Pts',(-21.7199938119459,26.2030643697733,8.12515193354574));
#44763=CARTESIAN_POINT('Ctrl Pts',(-21.6922994345911,26.183742259056,8.12301095921678));
#44764=CARTESIAN_POINT('Ctrl Pts',(-21.6611656691945,26.1612848432148,8.12060991974254));
#44765=CARTESIAN_POINT('Ctrl Pts',(-21.6574246057767,26.1585740895882,8.12032150571276));
#44766=CARTESIAN_POINT('Ctrl Pts',(-21.6521603880067,26.1547423767257,8.11991581783683));
#44767=CARTESIAN_POINT('Ctrl Pts',(-21.6506323945351,26.1536281237562,8.11979808089806));
#44768=CARTESIAN_POINT('Ctrl Pts',(-21.6475639833635,26.151386418014,8.11956168767697));
#44769=CARTESIAN_POINT('Ctrl Pts',(-21.6460235827623,26.150258938731,8.11944303309373));
#44770=CARTESIAN_POINT('Ctrl Pts',(-21.6430645304162,26.1480890526141,8.11921514048876));
#44771=CARTESIAN_POINT('Ctrl Pts',(-21.641645733673,26.1470468539747,8.11910588816428));
#44772=CARTESIAN_POINT('Ctrl Pts',(-21.6382919891239,26.1445790767582,8.11884767615582));
#44773=CARTESIAN_POINT('Ctrl Pts',(-21.6363577773655,26.1431524927823,8.11869878705824));
#44774=CARTESIAN_POINT('Ctrl Pts',(-21.6306094644303,26.1389028699247,8.11825638475496));
#44775=CARTESIAN_POINT('Ctrl Pts',(-21.6267999789832,26.1360735536261,8.11796330815195));
#44776=CARTESIAN_POINT('Ctrl Pts',(-21.5921129226067,26.1101923056816,8.11529557495283));
#44777=CARTESIAN_POINT('Ctrl Pts',(-21.5616431988227,26.086595493376,8.11295841195184));
#44778=CARTESIAN_POINT('Ctrl Pts',(-21.4450829803222,25.992934989046,8.10401024671193));
#44779=CARTESIAN_POINT('Ctrl Pts',(-21.3622040773661,25.9189832312385,8.09763032769996));
#44780=CARTESIAN_POINT('Ctrl Pts',(-21.1889049707653,25.7474764031931,8.083834188344));
#44781=CARTESIAN_POINT('Ctrl Pts',(-21.1003730628055,25.6483104721367,8.07647111430951));
#44782=CARTESIAN_POINT('Ctrl Pts',(-20.9380246428854,25.4421256121732,8.06175781139711));
#44783=CARTESIAN_POINT('Ctrl Pts',(-20.8640600785651,25.335549326988,8.0544244944145));
#44784=CARTESIAN_POINT('Ctrl Pts',(-20.7654005838118,25.1733205167901,8.04336893801605));
#44785=CARTESIAN_POINT('Ctrl Pts',(-20.7355360632764,25.1209595684009,8.03981695791077));
#44786=CARTESIAN_POINT('Ctrl Pts',(-20.6875052776914,25.0309745404327,8.03371822997947));
#44787=CARTESIAN_POINT('Ctrl Pts',(-20.6685700278105,24.9937778017171,8.03119885074567));
#44788=CARTESIAN_POINT('Ctrl Pts',(-20.6469291462226,24.9491423911917,8.02817387231961));
#44789=CARTESIAN_POINT('Ctrl Pts',(-20.6435211652808,24.9420471578538,8.02769297280075));
#44790=CARTESIAN_POINT('Ctrl Pts',(-20.6383728988901,24.9312273565767,8.02695952871431));
#44791=CARTESIAN_POINT('Ctrl Pts',(-20.6366136734484,24.9275117906461,8.02670764276028));
#44792=CARTESIAN_POINT('Ctrl Pts',(-20.6335722724139,24.9210563027633,8.02626997638259));
#44793=CARTESIAN_POINT('Ctrl Pts',(-20.6322868334148,24.9183179165415,8.02608430942372));
#44794=CARTESIAN_POINT('Ctrl Pts',(-20.6296208548398,24.9126176989727,8.02569780080093));
#44795=CARTESIAN_POINT('Ctrl Pts',(-20.6282409612172,24.9096555707982,8.02549693702364));
#44796=CARTESIAN_POINT('Ctrl Pts',(-20.6248851213634,24.9024230895018,8.02500646143268));
#44797=CARTESIAN_POINT('Ctrl Pts',(-20.6229140218751,24.8981505068359,8.02471668237714));
#44798=CARTESIAN_POINT('Ctrl Pts',(-20.6154643694813,24.8819091212375,8.02361501485377));
#44799=CARTESIAN_POINT('Ctrl Pts',(-20.610049864884,24.869911237329,8.02280092103195));
#44800=CARTESIAN_POINT('Ctrl Pts',(-20.5175003285324,24.6614355439169,8.00864952970832));
#44801=CARTESIAN_POINT('Ctrl Pts',(-20.450179587129,24.4567999048437,7.99461540490779));
#44802=CARTESIAN_POINT('Ctrl Pts',(-20.3678952238628,24.0852160581386,7.96905764102781));
#44803=CARTESIAN_POINT('Ctrl Pts',(-20.3445991609664,23.9208864770235,7.95774659864501));
#44804=CARTESIAN_POINT('Ctrl Pts',(-20.3284826437955,23.6683369826585,7.94081604118686));
#44805=CARTESIAN_POINT('Ctrl Pts',(-20.326465406691,23.5809806549005,7.93504531829204));
#44806=CARTESIAN_POINT('Ctrl Pts',(-20.3286796376527,23.4549433767502,7.92693592404091));
#44807=CARTESIAN_POINT('Ctrl Pts',(-20.3300567223239,23.4162561472129,7.92447636253162));
#44808=CARTESIAN_POINT('Ctrl Pts',(-20.3323856576079,23.3728461708287,7.92175681284996));
#44809=CARTESIAN_POINT('Ctrl Pts',(-20.332651294238,23.3680918508868,7.9214595073092));
#44810=CARTESIAN_POINT('Ctrl Pts',(-20.3330658667313,23.3609558878315,7.92101410200949));
#44811=CARTESIAN_POINT('Ctrl Pts',(-20.3332069106098,23.3585738199304,7.92086555994366));
#44812=CARTESIAN_POINT('Ctrl Pts',(-20.3334528044039,23.354497690627,7.92061162000901));
#44813=CARTESIAN_POINT('Ctrl Pts',(-20.3335563468899,23.3528035559662,7.92050614799976));
#44814=CARTESIAN_POINT('Ctrl Pts',(-20.3337723884344,23.349314017206,7.92028904693828));
#44815=CARTESIAN_POINT('Ctrl Pts',(-20.3338850521282,23.3475186297013,7.92017742756349));
#44816=CARTESIAN_POINT('Ctrl Pts',(-20.3341937695832,23.3426639999473,7.91987582990135));
#44817=CARTESIAN_POINT('Ctrl Pts',(-20.3343926857691,23.3396049316202,7.91968601382583));
#44818=CARTESIAN_POINT('Ctrl Pts',(-20.3351451055483,23.3282832133299,7.91898433742694));
#44819=CARTESIAN_POINT('Ctrl Pts',(-20.3357260972516,23.3200223299647,7.91847401501613));
#44820=CARTESIAN_POINT('Ctrl Pts',(-20.3460981958381,23.1802462894014,7.90986588144374));
#44821=CARTESIAN_POINT('Ctrl Pts',(-20.363922501921,23.0494331319363,7.90220726893785));
#44822=CARTESIAN_POINT('Ctrl Pts',(-20.4330029498787,22.7029789915037,7.88213167768738));
#44823=CARTESIAN_POINT('Ctrl Pts',(-20.4985384198102,22.490930559686,7.87002825248174));
#44824=CARTESIAN_POINT('Ctrl Pts',(-20.627503922865,22.1881733139795,7.85124677101036));
#44825=CARTESIAN_POINT('Ctrl Pts',(-20.6746532251314,22.0912650184146,7.84499425214507));
#44826=CARTESIAN_POINT('Ctrl Pts',(-20.7498366178128,21.954595920712,7.83569787113862));
#44827=CARTESIAN_POINT('Ctrl Pts',(-20.7740581885332,21.9128173735767,7.8327883686596));
#44828=CARTESIAN_POINT('Ctrl Pts',(-20.8033428022954,21.8648245422401,7.82936057211804));
#44829=CARTESIAN_POINT('Ctrl Pts',(-20.807502331411,21.8580640356423,7.82887570745612));
#44830=CARTESIAN_POINT('Ctrl Pts',(-20.8139154804342,21.847726473771,7.82813118407977));
#44831=CARTESIAN_POINT('Ctrl Pts',(-20.8161512545446,21.8441383379702,7.82787218504296));
#44832=CARTESIAN_POINT('Ctrl Pts',(-20.8200070481755,21.8379773182944,7.82742647202648));
#44833=CARTESIAN_POINT('Ctrl Pts',(-20.8216236641268,21.8354023021785,7.82723988438298));
#44834=CARTESIAN_POINT('Ctrl Pts',(-20.8249590426426,21.8301062241432,7.82685550533873));
#44835=CARTESIAN_POINT('Ctrl Pts',(-20.8266782418755,21.8273854420555,7.82665769784231));
#44836=CARTESIAN_POINT('Ctrl Pts',(-20.8308245256808,21.8208453035152,7.82618139630988));
#44837=CARTESIAN_POINT('Ctrl Pts',(-20.8332555800786,21.8170284823127,7.82590275463257));
#44838=CARTESIAN_POINT('Ctrl Pts',(-20.8407333860387,21.8053425182306,7.82504756469418));
#44839=CARTESIAN_POINT('Ctrl Pts',(-20.8458063113168,21.7974902563447,7.82447003969262));
#44840=CARTESIAN_POINT('Ctrl Pts',(-20.9048779277582,21.7069216825903,7.81777505465706));
#44841=CARTESIAN_POINT('Ctrl Pts',(-20.9626126369707,21.6267162736115,7.81151671244625));
#44842=CARTESIAN_POINT('Ctrl Pts',(-21.0663779758242,21.4957068621098,7.80070286483037));
#44843=CARTESIAN_POINT('Ctrl Pts',(-21.1105138772957,21.4434860427505,7.79621962943361));
#44844=CARTESIAN_POINT('Ctrl Pts',(-21.2936074916002,21.2403279544188,7.77809009232828));
#44845=CARTESIAN_POINT('Ctrl Pts',(-21.4451725836988,21.1014105496273,7.76406242178501));
#44846=CARTESIAN_POINT('Ctrl Pts',(-21.671255655043,20.930788390186,7.74505161747657));
#44847=CARTESIAN_POINT('Ctrl Pts',(-21.7353129352484,20.886004522952,7.73985663355557));
#44848=CARTESIAN_POINT('Ctrl Pts',(-21.8462375964566,20.8143139704335,7.73125154447303));
#44849=CARTESIAN_POINT('Ctrl Pts',(-21.8922679606301,20.7861767893041,7.72778841364106));
#44850=CARTESIAN_POINT('Ctrl Pts',(-21.9444788401436,20.7560355324648,7.7239972638394));
#44851=CARTESIAN_POINT('Ctrl Pts',(-21.9499809589547,20.752880786227,7.72359941314159));
#44852=CARTESIAN_POINT('Ctrl Pts',(-21.959726182036,20.7473313356938,7.7228977474691));
#44853=CARTESIAN_POINT('Ctrl Pts',(-21.9639654497386,20.7449299844085,7.72259351488441));
#44854=CARTESIAN_POINT('Ctrl Pts',(-21.9702842871635,20.7413695550443,7.72214154515304));
#44855=CARTESIAN_POINT('Ctrl Pts',(-21.9723596968909,20.740203166967,7.72199333748785));
#44856=CARTESIAN_POINT('Ctrl Pts',(-21.9759228773562,20.7382058382954,7.72173930184025));
#44857=CARTESIAN_POINT('Ctrl Pts',(-21.9774100151513,20.7373737777139,7.72163340097217));
#44858=CARTESIAN_POINT('Ctrl Pts',(-21.9804551039666,20.7356732061318,7.72141681119816));
#44859=CARTESIAN_POINT('Ctrl Pts',(-21.9820131129378,20.7348048107303,7.72130612987596));
#44860=CARTESIAN_POINT('Ctrl Pts',(-21.9857492929873,20.7327264205352,7.7210410348226));
#44861=CARTESIAN_POINT('Ctrl Pts',(-21.9879281519934,20.731517655251,7.72088670084779));
#44862=CARTESIAN_POINT('Ctrl Pts',(-21.9957946668233,20.7271654733145,7.72033043894199));
#44863=CARTESIAN_POINT('Ctrl Pts',(-22.0014904752483,20.7240367071152,7.71992944961804));
#44864=CARTESIAN_POINT('Ctrl Pts',(-22.0911033929641,20.6751636709981,7.71364786378641));
#44865=CARTESIAN_POINT('Ctrl Pts',(-22.1770148744117,20.6331521548447,7.70799980258374));
#44866=CARTESIAN_POINT('Ctrl Pts',(-22.5166598226966,20.4854009270515,7.68660547369846));
#44867=CARTESIAN_POINT('Ctrl Pts',(-22.7816364414664,20.4084569896587,7.67177399100078));
#44868=CARTESIAN_POINT('Ctrl Pts',(-23.1765186499219,20.3468131474472,7.64885285222863));
#44869=CARTESIAN_POINT('Ctrl Pts',(-23.3008592335329,20.334743496168,7.64153882714288));
#44870=CARTESIAN_POINT('Ctrl Pts',(-23.4459210268486,20.3291274172142,7.6327577877768));
#44871=CARTESIAN_POINT('Ctrl Pts',(-23.4662717785913,20.3285326075616,7.63152039310426));
#44872=CARTESIAN_POINT('Ctrl Pts',(-23.492661497411,20.3280114992223,7.62990826175459));
#44873=CARTESIAN_POINT('Ctrl Pts',(-23.4986968412881,20.3279092835938,7.62953905511939));
#44874=CARTESIAN_POINT('Ctrl Pts',(-23.508440969668,20.3277716377274,7.62894212952983));
#44875=CARTESIAN_POINT('Ctrl Pts',(-23.5121496101861,20.3277256526922,7.62871474227271));
#44876=CARTESIAN_POINT('Ctrl Pts',(-23.5192252448072,20.3276501349483,7.62828053829919));
#44877=CARTESIAN_POINT('Ctrl Pts',(-23.522592224077,20.327619476677,7.62807375721324));
#44878=CARTESIAN_POINT('Ctrl Pts',(-23.5302847954498,20.327561487932,7.62760094780115));
#44879=CARTESIAN_POINT('Ctrl Pts',(-23.5346104001501,20.3275375896825,7.62733481205746));
#44880=CARTESIAN_POINT('Ctrl Pts',(-23.547857126271,20.3274910742487,7.62651896217254));
#44881=CARTESIAN_POINT('Ctrl Pts',(-23.5567782481965,20.3274967913346,7.62596835957772));
#44882=CARTESIAN_POINT('Ctrl Pts',(-23.5929260002519,20.3276700493614,7.62373257010375));
#44883=CARTESIAN_POINT('Ctrl Pts',(-23.6201493923751,20.3281455757059,7.62203774741171));
#44884=CARTESIAN_POINT('Ctrl Pts',(-23.6552082448343,20.329202475085,7.61984034476223));
#44885=CARTESIAN_POINT('Ctrl Pts',(-23.663052708489,20.3294676448599,7.61934772067625));
#44886=CARTESIAN_POINT('Ctrl Pts',(-23.6803118992806,20.3301141952762,7.61826174788554));
#44887=CARTESIAN_POINT('Ctrl Pts',(-23.6897260552538,20.3305082129695,7.61766801122811));
#44888=CARTESIAN_POINT('Ctrl Pts',(-23.7007641282942,20.331018698798,7.61697021886843));
#44889=CARTESIAN_POINT('Ctrl Pts',(-23.7023899287517,20.3310951226855,7.61686739919075));
#44890=CARTESIAN_POINT('Ctrl Pts',(-23.7120382858864,20.3315559878299,7.61625696538053));
#44891=CARTESIAN_POINT('Ctrl Pts',(-23.7200593842456,20.3319691845192,7.6157484690072));
#44892=CARTESIAN_POINT('Ctrl Pts',(-23.7399088283264,20.3330661167194,7.61448758696714));
#44893=CARTESIAN_POINT('Ctrl Pts',(-23.7517350376127,20.3337851008907,7.61373413456991));
#44894=CARTESIAN_POINT('Ctrl Pts',(-24.0386171782483,20.3528147147812,7.59540246237311));
#44895=CARTESIAN_POINT('Ctrl Pts',(-24.3101590117772,20.4062748374603,7.57669130377256));
#44896=CARTESIAN_POINT('Ctrl Pts',(-24.7304849340708,20.5467114161775,7.54676948622247));
#44897=CARTESIAN_POINT('Ctrl Pts',(-24.885086287283,20.6121507292481,7.53557449906745));
#44898=CARTESIAN_POINT('Ctrl Pts',(-25.0406574866387,20.6928291511576,7.52457510903283));
#44899=CARTESIAN_POINT('Ctrl Pts',(-25.0473908972771,20.6963513381614,7.52409960162688));
#44900=CARTESIAN_POINT('Ctrl Pts',(-25.05663775305,20.7012300180099,7.5234474439656));
#44901=CARTESIAN_POINT('Ctrl Pts',(-25.05916187744,20.7025660487625,7.52326951088678));
#44902=CARTESIAN_POINT('Ctrl Pts',(-25.0634205836321,20.7048274537639,7.52296945345086));
#44903=CARTESIAN_POINT('Ctrl Pts',(-25.0651560945862,20.7057510599584,7.5228472163844));
#44904=CARTESIAN_POINT('Ctrl Pts',(-25.0685749050392,20.7075745027444,7.52260650520676));
#44905=CARTESIAN_POINT('Ctrl Pts',(-25.070258250415,20.7084742467528,7.52248802544948));
#44906=CARTESIAN_POINT('Ctrl Pts',(-25.0739708545963,20.7104628672172,7.52222680768948));
#44907=CARTESIAN_POINT('Ctrl Pts',(-25.0759997510971,20.7115524262621,7.52208411343012));
#44908=CARTESIAN_POINT('Ctrl Pts',(-25.0830980543048,20.7153741692392,7.52158508097397));
#44909=CARTESIAN_POINT('Ctrl Pts',(-25.0881613431049,20.7181177864706,7.52122947031888));
#44910=CARTESIAN_POINT('Ctrl Pts',(-25.1399375765307,20.7463532914741,7.51759641235279));
#44911=CARTESIAN_POINT('Ctrl Pts',(-25.1860229984064,20.7729867391002,7.51439062244875));
#44912=CARTESIAN_POINT('Ctrl Pts',(-25.3145325510243,20.8515637063047,7.50547020951547));
#44913=CARTESIAN_POINT('Ctrl Pts',(-25.3952946799141,20.9061217097825,7.49988618709235));
#44914=CARTESIAN_POINT('Ctrl Pts',(-25.5264491598719,21.0036618303362,7.49064266265321));
#44915=CARTESIAN_POINT('Ctrl Pts',(-25.5782091334936,21.0446847986799,7.48694526653462));
#44916=CARTESIAN_POINT('Ctrl Pts',(-25.7309918230604,21.1736124847479,7.47576928506367));
#44917=CARTESIAN_POINT('Ctrl Pts',(-25.8278286266458,21.2662456859885,7.46831524581369));
#44918=CARTESIAN_POINT('Ctrl Pts',(-25.9851839517236,21.4367578644358,7.45509907446572));
#44919=CARTESIAN_POINT('Ctrl Pts',(-26.0484124439881,21.5118842151716,7.4494249050375));
#44920=CARTESIAN_POINT('Ctrl Pts',(-26.1468356744202,21.6402981327042,7.43985126312269));
#44921=CARTESIAN_POINT('Ctrl Pts',(-26.1840523075463,21.6919555415958,7.43603141774321));
#44922=CARTESIAN_POINT('Ctrl Pts',(-26.2244194192409,21.7516365127145,7.43163947199003));
#44923=CARTESIAN_POINT('Ctrl Pts',(-26.2290984578448,21.7586128837675,7.43112640516336));
#44924=CARTESIAN_POINT('Ctrl Pts',(-26.236087455396,21.7691219524947,7.43035399016273));
#44925=CARTESIAN_POINT('Ctrl Pts',(-26.2384178621609,21.772641063081,7.43009541297855));
#44926=CARTESIAN_POINT('Ctrl Pts',(-26.2424145132216,21.7787021751243,7.42965018249831));
#44927=CARTESIAN_POINT('Ctrl Pts',(-26.2440840911412,21.7812419806043,7.42946365477132));
#44928=CARTESIAN_POINT('Ctrl Pts',(-26.2475156193518,21.7864782338362,7.42907917262162));
#44929=CARTESIAN_POINT('Ctrl Pts',(-26.2492771246312,21.7891749682608,7.42888120176989));
#44930=CARTESIAN_POINT('Ctrl Pts',(-26.254008415624,21.7964419974879,7.42834783010748));
#44931=CARTESIAN_POINT('Ctrl Pts',(-26.2569706451959,21.8010171778222,7.42801214717339));
#44932=CARTESIAN_POINT('Ctrl Pts',(-26.2677902865465,21.8178214641674,7.42677962210954));
#44933=CARTESIAN_POINT('Ctrl Pts',(-26.2755764511271,21.8300960342168,7.42588013101528));
#44934=CARTESIAN_POINT('Ctrl Pts',(-26.2938036416582,21.8592648641696,7.42374430242491));
#44935=CARTESIAN_POINT('Ctrl Pts',(-26.3041719692178,21.8762036411817,7.42250531922469));
#44936=CARTESIAN_POINT('Ctrl Pts',(-26.5008151727119,22.2042315893919,7.39853399703484));
#44937=CARTESIAN_POINT('Ctrl Pts',(-26.6333925004005,22.5444195078288,7.37361781901645));
#44938=CARTESIAN_POINT('Ctrl Pts',(-26.7309806132763,23.0176419960814,7.34131964240364));
#44939=CARTESIAN_POINT('Ctrl Pts',(-26.7487086678329,23.1372258858783,7.33338983569784));
#44940=CARTESIAN_POINT('Ctrl Pts',(-26.7602543032145,23.2638158975588,7.32542316972101));
#44941=CARTESIAN_POINT('Ctrl Pts',(-26.7608085721551,23.270096805,7.3250290027055));
#44942=CARTESIAN_POINT('Ctrl Pts',(-26.7615700264782,23.2790246594217,7.32447033625397));
#44943=CARTESIAN_POINT('Ctrl Pts',(-26.7617923753193,23.2816702464746,7.32430498810685));
#44944=CARTESIAN_POINT('Ctrl Pts',(-26.7621693599687,23.2862231536489,7.32402078297492));
#44945=CARTESIAN_POINT('Ctrl Pts',(-26.7623255664406,23.2881303392919,7.32390183674331));
#44946=CARTESIAN_POINT('Ctrl Pts',(-26.7626217575744,23.2917866766836,7.32367400424059));
#44947=CARTESIAN_POINT('Ctrl Pts',(-26.7627620121057,23.293535800857,7.32356510264455));
#44948=CARTESIAN_POINT('Ctrl Pts',(-26.7630892205207,23.2976587012696,7.32330861674754));
#44949=CARTESIAN_POINT('Ctrl Pts',(-26.7632749726379,23.3000325758239,7.32316110076436));
#44950=CARTESIAN_POINT('Ctrl Pts',(-26.7638163312105,23.3070510360716,7.3227254393449));
#44951=CARTESIAN_POINT('Ctrl Pts',(-26.7641645008306,23.31169621482,7.32243771205807));
#44952=CARTESIAN_POINT('Ctrl Pts',(-26.7671254205255,23.3523833230073,7.31992277500548));
#44953=CARTESIAN_POINT('Ctrl Pts',(-26.7691420000244,23.3884679040528,7.31772850286132));
#44954=CARTESIAN_POINT('Ctrl Pts',(-26.7707584802383,23.4298896357098,7.3152433469209));
#44955=CARTESIAN_POINT('Ctrl Pts',(-26.7709525373825,23.4351992160073,7.31492542495245));
#44956=CARTESIAN_POINT('Ctrl Pts',(-26.7711818205749,23.4419285036839,7.31452327111515));
#44957=CARTESIAN_POINT('Ctrl Pts',(-26.7712292387856,23.4433477544264,7.31443849798091));
#44958=CARTESIAN_POINT('Ctrl Pts',(-26.771406450904,23.448758966201,7.31411544658448));
#44959=CARTESIAN_POINT('Ctrl Pts',(-26.7715297623108,23.4527511527492,7.31387745428242));
#44960=CARTESIAN_POINT('Ctrl Pts',(-26.7716929991642,23.4583746791862,7.31354268035651));
#44961=CARTESIAN_POINT('Ctrl Pts',(-26.7717391072137,23.4600058198219,7.31344563267206));
#44962=CARTESIAN_POINT('Ctrl Pts',(-26.771984204172,23.468916081101,7.31291580121302));
#44963=CARTESIAN_POINT('Ctrl Pts',(-26.7721597622356,23.476195883072,7.31248401830316));
#44964=CARTESIAN_POINT('Ctrl Pts',(-26.7723898797889,23.4872994130233,7.31182702886601));
#44965=CARTESIAN_POINT('Ctrl Pts',(-26.7724623089478,23.4911227020264,7.31160109420439));
#44966=CARTESIAN_POINT('Ctrl Pts',(-26.7728346105248,23.5128138284192,7.31032085568844));
#44967=CARTESIAN_POINT('Ctrl Pts',(-26.7729926719099,23.5306841023086,7.30927222495788));
#44968=CARTESIAN_POINT('Ctrl Pts',(-26.7730393907041,23.6193840350769,7.30409354850758));
#44969=CARTESIAN_POINT('Ctrl Pts',(-26.7707416864332,23.6901987382377,7.30004191843296));
#44970=CARTESIAN_POINT('Ctrl Pts',(-26.7433386453863,24.1085812604084,7.27630775675397));
#44971=CARTESIAN_POINT('Ctrl Pts',(-26.6643392046655,24.4502482074331,7.2574565837971));
#44972=CARTESIAN_POINT('Ctrl Pts',(-26.5242839521232,24.7918996148428,7.23513201115579));
#44973=CARTESIAN_POINT('Ctrl Pts',(-26.5162068814347,24.8110717623944,7.23386804110642));
#44974=CARTESIAN_POINT('Ctrl Pts',(-26.5054415844893,24.8359488236887,7.23221285620487));
#44975=CARTESIAN_POINT('Ctrl Pts',(-26.5029213184341,24.8417262356189,7.23182739024658));
#44976=CARTESIAN_POINT('Ctrl Pts',(-26.4990188164999,24.8506011252803,7.23123360381595));
#44977=CARTESIAN_POINT('Ctrl Pts',(-26.497648602715,24.8537038992718,7.2310256959427));
#44978=CARTESIAN_POINT('Ctrl Pts',(-26.4949314578639,24.8598305332848,7.23061454735716));
#44979=CARTESIAN_POINT('Ctrl Pts',(-26.4935847608902,24.8628544930381,7.23041131488654));
#44980=CARTESIAN_POINT('Ctrl Pts',(-26.4905907655944,24.8695496263277,7.2299606861103));
#44981=CARTESIAN_POINT('Ctrl Pts',(-26.4889412479145,24.8732197960546,7.22971321364366));
#44982=CARTESIAN_POINT('Ctrl Pts',(-26.4842132736953,24.8836870460961,7.22900615121549));
#44983=CARTESIAN_POINT('Ctrl Pts',(-26.4811180936343,24.8904765040716,7.2285459849923));
#44984=CARTESIAN_POINT('Ctrl Pts',(-26.4613270243664,24.9334929331668,7.22562062467509));
#44985=CARTESIAN_POINT('Ctrl Pts',(-26.4439839503859,24.9694167068045,7.2231330916337));
#44986=CARTESIAN_POINT('Ctrl Pts',(-26.3904858614386,25.0751704749775,7.21567282935285));
#44987=CARTESIAN_POINT('Ctrl Pts',(-26.352439387745,25.144005092115,7.21063488280423));
#44988=CARTESIAN_POINT('Ctrl Pts',(-26.234180849252,25.3406132947755,7.19570086808431));
#44989=CARTESIAN_POINT('Ctrl Pts',(-26.1474766539702,25.4642225875008,7.18560062836074));
#44990=CARTESIAN_POINT('Ctrl Pts',(-25.9845755879772,25.6649125468504,7.16812864592451));
#44991=CARTESIAN_POINT('Ctrl Pts',(-25.9125548914997,25.7450745757454,7.1608162400925));
#44992=CARTESIAN_POINT('Ctrl Pts',(-25.7716525556992,25.8869182971149,7.14739772083273));
#44993=CARTESIAN_POINT('Ctrl Pts',(-25.7038649688071,25.9495401602419,7.14127580285021));
#44994=CARTESIAN_POINT('Ctrl Pts',(-25.5991177561338,26.0382832873199,7.13240364419521));
#44995=CARTESIAN_POINT('Ctrl Pts',(-25.5641476221196,26.0666731700698,7.12953250510165));
#44996=CARTESIAN_POINT('Ctrl Pts',(-25.5243008174668,26.09765914896,7.1263719707721));
#44997=CARTESIAN_POINT('Ctrl Pts',(-25.5200014298373,26.1009850514901,7.12603237490713));
#44998=CARTESIAN_POINT('Ctrl Pts',(-25.5138826580851,26.1056936894792,7.12555110823747));
#44999=CARTESIAN_POINT('Ctrl Pts',(-25.512070216707,26.1070853684322,7.1254088051807));
#45000=CARTESIAN_POINT('Ctrl Pts',(-25.5087448323276,26.1096331396472,7.12514817979121));
#45001=CARTESIAN_POINT('Ctrl Pts',(-25.5072323426977,26.1107898205051,7.12502981540053));
#45002=CARTESIAN_POINT('Ctrl Pts',(-25.5041511525431,26.1131418448668,7.12478904774322));
#45003=CARTESIAN_POINT('Ctrl Pts',(-25.5025823797302,26.1143370889286,7.12466665159665));
#45004=CARTESIAN_POINT('Ctrl Pts',(-25.4986686760882,26.117313255773,7.12436177261338));
#45005=CARTESIAN_POINT('Ctrl Pts',(-25.496322393707,26.1190924109343,7.1241794157452));
#45006=CARTESIAN_POINT('Ctrl Pts',(-25.4874652575031,26.1257895621207,7.12349259090087));
#45007=CARTESIAN_POINT('Ctrl Pts',(-25.4809381003474,26.1306860957576,7.12298962947317));
#45008=CARTESIAN_POINT('Ctrl Pts',(-25.3616965696974,26.2194328188426,7.11385770962764));
#45009=CARTESIAN_POINT('Ctrl Pts',(-25.243620223074,26.2958617517828,7.10572850397359));
#45010=CARTESIAN_POINT('Ctrl Pts',(-24.8131401625233,26.5361306182987,7.07778981894577));
#45011=CARTESIAN_POINT('Ctrl Pts',(-24.4793033421325,26.6562497109241,7.05875248575931));
#45012=CARTESIAN_POINT('Ctrl Pts',(-24.1124581992876,26.7236518410585,7.03619787995373));
#45013=CARTESIAN_POINT('Ctrl Pts',(-24.0922473063135,26.727166131933,7.03495139778635));
#45014=CARTESIAN_POINT('Ctrl Pts',(-24.0658186033756,26.7315020479564,7.03331597216524));
#45015=CARTESIAN_POINT('Ctrl Pts',(-24.0596296974438,26.732498870544,7.03293260849408));
#45016=CARTESIAN_POINT('Ctrl Pts',(-24.0500945604591,26.734006128692,7.03234135354054));
#45017=CARTESIAN_POINT('Ctrl Pts',(-24.0467503436351,26.7345293636791,7.03213386920611));
#45018=CARTESIAN_POINT('Ctrl Pts',(-24.0401680270289,26.735548609184,7.0317252534834));
#45019=CARTESIAN_POINT('Ctrl Pts',(-24.0369299824095,26.7360449531618,7.03152413295271));
#45020=CARTESIAN_POINT('Ctrl Pts',(-24.0297970907488,26.7371271905914,7.0310808524472));
#45021=CARTESIAN_POINT('Ctrl Pts',(-24.0259019193954,26.737710882073,7.03083862289382));
#45022=CARTESIAN_POINT('Ctrl Pts',(-24.0149045596416,26.7393382291663,7.03015427090614));
#45023=CARTESIAN_POINT('Ctrl Pts',(-24.0077999731732,26.74036529308,7.02971162282511));
#45024=CARTESIAN_POINT('Ctrl Pts',(-23.9919081484274,26.7426084913474,7.02872026265327));
#45025=CARTESIAN_POINT('Ctrl Pts',(-23.9831192262033,26.7438120941853,7.02817115624149));
#45026=CARTESIAN_POINT('Ctrl Pts',(-23.8085636046649,26.7669828774427,7.01724844224511));
#45027=CARTESIAN_POINT('Ctrl Pts',(-23.6413686860704,26.7760486290695,7.00646168092928));
#45028=CARTESIAN_POINT('Ctrl Pts',(-23.2601015975465,26.767054353661,6.98115145776986));
#45029=CARTESIAN_POINT('Ctrl Pts',(-23.0469962430431,26.740663942086,6.96647516883323));
#45030=CARTESIAN_POINT('Ctrl Pts',(-22.7871915497385,26.6817986482123,6.94865493893199));
#45031=CARTESIAN_POINT('Ctrl Pts',(-22.7365606340584,26.6690261854752,6.9451883674089));
#45032=CARTESIAN_POINT('Ctrl Pts',(-22.6617747163008,26.648214879732,6.94009718016781));
#45033=CARTESIAN_POINT('Ctrl Pts',(-22.6373698040873,26.6411114314313,6.9384404819557));
#45034=CARTESIAN_POINT('Ctrl Pts',(-22.6030687041969,26.6306858140148,6.93612100312859));
#45035=CARTESIAN_POINT('Ctrl Pts',(-22.5931012663745,26.6276033194611,6.93544807471076));
#45036=CARTESIAN_POINT('Ctrl Pts',(-22.5478950703297,26.6133821250359,6.93240153711876));
#45037=CARTESIAN_POINT('Ctrl Pts',(-22.5128327538376,26.6016856183889,6.93005368677008));
#45038=CARTESIAN_POINT('Ctrl Pts',(-22.4731291530991,26.5876773000436,6.92741847135614));
#45039=CARTESIAN_POINT('Ctrl Pts',(-22.4682847785286,26.5859550497417,6.92709734017924));
#45040=CARTESIAN_POINT('Ctrl Pts',(-22.4611358794341,26.583394218778,6.92662405741832));
#45041=CARTESIAN_POINT('Ctrl Pts',(-22.4588281879092,26.5825645997448,6.9264713746471));
#45042=CARTESIAN_POINT('Ctrl Pts',(-22.454746845817,26.5810920876276,6.92620151308045));
#45043=CARTESIAN_POINT('Ctrl Pts',(-22.4529728116768,26.5804502707391,6.92608426965036));
#45044=CARTESIAN_POINT('Ctrl Pts',(-22.4492718578246,26.5791076491197,6.92583979908717));
#45045=CARTESIAN_POINT('Ctrl Pts',(-22.4473450471248,26.5784065646202,6.92571258932958));
#45046=CARTESIAN_POINT('Ctrl Pts',(-22.4423195062066,26.5765725509815,6.92538097245901));
#45047=CARTESIAN_POINT('Ctrl Pts',(-22.4392218343448,26.5754366976392,6.92517674109285));
#45048=CARTESIAN_POINT('Ctrl Pts',(-22.4258128376956,26.5704965173563,6.9242934032633));
#45049=CARTESIAN_POINT('Ctrl Pts',(-22.4155191077822,26.5666441546895,6.92361714779844));
#45050=CARTESIAN_POINT('Ctrl Pts',(-22.3413421523693,26.5384504478529,6.91875609895471));
#45051=CARTESIAN_POINT('Ctrl Pts',(-22.2782227337624,26.5121324854871,6.91468441294332));
#45052=CARTESIAN_POINT('Ctrl Pts',(-22.1684519854658,26.4622057246811,6.90763841321722));
#45053=CARTESIAN_POINT('Ctrl Pts',(-22.1214557159561,26.4394363613025,6.90463354385769));
#45054=CARTESIAN_POINT('Ctrl Pts',(-22.0750360103879,26.4155367720035,6.90165778540197));
#45055=CARTESIAN_POINT('',(-26.7730018526427,23.548160445141,7.06183203780204));
#45056=CARTESIAN_POINT('Ctrl Pts',(-22.0750360194354,26.4155367766617,6.65421995916067));
#45057=CARTESIAN_POINT('Ctrl Pts',(-22.1030069891242,26.4299378736632,6.656220780701));
#45058=CARTESIAN_POINT('Ctrl Pts',(-22.1311879873181,26.443928955527,6.65823551916694));
#45059=CARTESIAN_POINT('Ctrl Pts',(-22.2698207253827,26.5102438312251,6.66814175552328));
#45060=CARTESIAN_POINT('Ctrl Pts',(-22.3829711956814,26.5566628635125,6.67621724682854));
#45061=CARTESIAN_POINT('Ctrl Pts',(-22.7680281775915,26.6896097419607,6.70353224301071));
#45062=CARTESIAN_POINT('Ctrl Pts',(-23.0487452019916,26.7464912030137,6.72328756031603));
#45063=CARTESIAN_POINT('Ctrl Pts',(-23.3489469742249,26.7667475076122,6.74232093593207));
#45064=CARTESIAN_POINT('Ctrl Pts',(-23.3646130508503,26.7676896895248,6.74330789747096));
#45065=CARTESIAN_POINT('Ctrl Pts',(-23.3838252289674,26.7687043455624,6.74451003094967));
#45066=CARTESIAN_POINT('Ctrl Pts',(-23.3873650250473,26.768885438032,6.7447311786681));
#45067=CARTESIAN_POINT('Ctrl Pts',(-23.3932145388186,26.7691750187581,6.74509605155091));
#45068=CARTESIAN_POINT('Ctrl Pts',(-23.3955240747743,26.7692868610578,6.7452399648297));
#45069=CARTESIAN_POINT('Ctrl Pts',(-23.3995114141946,26.7694756520919,6.74548816904159));
#45070=CARTESIAN_POINT('Ctrl Pts',(-23.4011891545659,26.7695537746745,6.74559252639276));
#45071=CARTESIAN_POINT('Ctrl Pts',(-23.4049566760875,26.7697262546619,6.74582669318417));
#45072=CARTESIAN_POINT('Ctrl Pts',(-23.4070464848073,26.7698198887673,6.74595646108593));
#45073=CARTESIAN_POINT('Ctrl Pts',(-23.4126173142883,26.7700640556095,6.74630206277365));
#45074=CARTESIAN_POINT('Ctrl Pts',(-23.4160985028903,26.7702109785436,6.74651769249859));
#45075=CARTESIAN_POINT('Ctrl Pts',(-23.4323524040536,26.7708705666097,6.74752294484868));
#45076=CARTESIAN_POINT('Ctrl Pts',(-23.4451280883677,26.7713128899038,6.74830864923604));
#45077=CARTESIAN_POINT('Ctrl Pts',(-23.752673581825,26.78012906517,6.76712330162036));
#45078=CARTESIAN_POINT('Ctrl Pts',(-24.0472633585529,26.7480838122956,6.78303742053867));
#45079=CARTESIAN_POINT('Ctrl Pts',(-24.4626704680579,26.6440146834101,6.80713810845837));
#45080=CARTESIAN_POINT('Ctrl Pts',(-24.5897737118816,26.6036541758098,6.81473648374602));
#45081=CARTESIAN_POINT('Ctrl Pts',(-24.7250805930496,26.5512586285551,6.82327708405909));
#45082=CARTESIAN_POINT('Ctrl Pts',(-24.7361300064408,26.5469095319005,6.82397783777911));
#45083=CARTESIAN_POINT('Ctrl Pts',(-24.7589111398375,26.5377970502987,6.82542967620588));
#45084=CARTESIAN_POINT('Ctrl Pts',(-24.7706393121888,26.5330253995509,6.82618100403714));
#45085=CARTESIAN_POINT('Ctrl Pts',(-24.7887419836199,26.5255356202542,6.82734690161485));
#45086=CARTESIAN_POINT('Ctrl Pts',(-24.7951364256011,26.5228658044241,6.82775993839653));
#45087=CARTESIAN_POINT('Ctrl Pts',(-24.8081991576987,26.5173622944666,6.82860620266664));
#45088=CARTESIAN_POINT('Ctrl Pts',(-24.8148665978886,26.5145266958936,6.82903948936594));
#45089=CARTESIAN_POINT('Ctrl Pts',(-24.8271305570639,26.5092620436475,6.82983897282051));
#45090=CARTESIAN_POINT('Ctrl Pts',(-24.8327298605759,26.5068395308615,6.83020495494202));
#45091=CARTESIAN_POINT('Ctrl Pts',(-24.8504286364795,26.4991224997318,6.83136487634342));
#45092=CARTESIAN_POINT('Ctrl Pts',(-24.8625023477292,26.4937695444361,6.83216073471482));
#45093=CARTESIAN_POINT('Ctrl Pts',(-24.8937707336715,26.4796758935613,6.83423404475359));
#45094=CARTESIAN_POINT('Ctrl Pts',(-24.9129128801452,26.4708208212571,6.83551532184514));
#45095=CARTESIAN_POINT('Ctrl Pts',(-24.9376916100922,26.4590616568412,6.83719005411216));
#45096=CARTESIAN_POINT('Ctrl Pts',(-24.9434087761467,26.4563277888824,6.83757759056231));
#45097=CARTESIAN_POINT('Ctrl Pts',(-24.9525199675906,26.4519378803179,6.83819700586523));
#45098=CARTESIAN_POINT('Ctrl Pts',(-24.9559192303687,26.4502926962846,6.83842850599436));
#45099=CARTESIAN_POINT('Ctrl Pts',(-24.9622779110586,26.4472013990284,6.83886231294264));
#45100=CARTESIAN_POINT('Ctrl Pts',(-24.9652380215858,26.4457567149387,6.83906456962158));
#45101=CARTESIAN_POINT('Ctrl Pts',(-24.9710960067254,26.4428865928116,6.83946544654088));
#45102=CARTESIAN_POINT('Ctrl Pts',(-24.9739939641428,26.4414613317436,6.83966406040624));
#45103=CARTESIAN_POINT('Ctrl Pts',(-24.9829153997715,26.4370569633072,6.84027642391676));
#45104=CARTESIAN_POINT('Ctrl Pts',(-24.9889316777197,26.4340633843064,6.84069068060906));
#45105=CARTESIAN_POINT('Ctrl Pts',(-25.0204752879332,26.4182446411655,6.84286954008035));
#45106=CARTESIAN_POINT('Ctrl Pts',(-25.0458399609375,26.405099611612,6.84464537157516));
#45107=CARTESIAN_POINT('Ctrl Pts',(-25.1159263914291,26.3675875340592,6.84962038337753));
#45108=CARTESIAN_POINT('Ctrl Pts',(-25.1602487393301,26.342495874761,6.85284503590439));
#45109=CARTESIAN_POINT('Ctrl Pts',(-25.2741246433576,26.2744158762107,6.8613407358109));
#45110=CARTESIAN_POINT('Ctrl Pts',(-25.3426665149479,26.2298143109516,6.86666639476673));
#45111=CARTESIAN_POINT('Ctrl Pts',(-25.6895010385416,25.9848564471684,6.89471236892197));
#45112=CARTESIAN_POINT('Ctrl Pts',(-25.9361777866325,25.7436554958658,6.91876137477343));
#45113=CARTESIAN_POINT('Ctrl Pts',(-26.1415302250007,25.4663429388757,6.94057118969712));
#45114=CARTESIAN_POINT('Ctrl Pts',(-26.1428550462322,25.4645499834979,6.94071197410278));
#45115=CARTESIAN_POINT('Ctrl Pts',(-26.1518004967781,25.4524172806119,6.94166310765567));
#45116=CARTESIAN_POINT('Ctrl Pts',(-26.1593612614233,25.4420332262551,6.94246961851545));
#45117=CARTESIAN_POINT('Ctrl Pts',(-26.1689670733808,25.4286733420745,6.94349734554793));
#45118=CARTESIAN_POINT('Ctrl Pts',(-26.1710693441006,25.4257390893167,6.94372245854666));
#45119=CARTESIAN_POINT('Ctrl Pts',(-26.1744105776562,25.4210589608274,6.94408053723123));
#45120=CARTESIAN_POINT('Ctrl Pts',(-26.1756527304827,25.419315382895,6.9442137238687));
#45121=CARTESIAN_POINT('Ctrl Pts',(-26.1779650394948,25.4160628010253,6.94446177571425));
#45122=CARTESIAN_POINT('Ctrl Pts',(-26.1790356264383,25.4145541236063,6.9445766705065));
#45123=CARTESIAN_POINT('Ctrl Pts',(-26.1814492720996,25.4111465870285,6.94483581116415));
#45124=CARTESIAN_POINT('Ctrl Pts',(-26.1827915719226,25.4092471991568,6.94498000399539));
#45125=CARTESIAN_POINT('Ctrl Pts',(-26.1867608858833,25.4036175999895,6.94540663040506));
#45126=CARTESIAN_POINT('Ctrl Pts',(-26.1893820503869,25.3998832413927,6.94568866050688));
#45127=CARTESIAN_POINT('Ctrl Pts',(-26.210071087473,25.370274168698,6.94791726924342));
#45128=CARTESIAN_POINT('Ctrl Pts',(-26.2277667503829,25.3441397354224,6.94983874111391));
#45129=CARTESIAN_POINT('Ctrl Pts',(-26.2939536140636,25.2432275087554,6.95710271254078));
#45130=CARTESIAN_POINT('Ctrl Pts',(-26.3397230739466,25.1667044492955,6.9622906748552));
#45131=CARTESIAN_POINT('Ctrl Pts',(-26.5144681800362,24.8449615614837,6.98322986035408));
#45132=CARTESIAN_POINT('Ctrl Pts',(-26.6147389965487,24.5855209979157,6.99821158344184));
#45133=CARTESIAN_POINT('Ctrl Pts',(-26.6850500880035,24.2982581096271,7.01532438669526));
#45134=CARTESIAN_POINT('Ctrl Pts',(-26.6893424577081,24.2800350214749,7.01641158962033));
#45135=CARTESIAN_POINT('Ctrl Pts',(-26.7144923959636,24.1689327230057,7.0230526277392));
#45136=CARTESIAN_POINT('Ctrl Pts',(-26.7313834253881,24.0752121592788,7.02871010949545));
#45137=CARTESIAN_POINT('Ctrl Pts',(-26.7454765203158,23.9706893597865,7.03513016223719));
#45138=CARTESIAN_POINT('Ctrl Pts',(-26.7468027496861,23.9604843733073,7.03575811191759));
#45139=CARTESIAN_POINT('Ctrl Pts',(-26.7485924349922,23.946177353831,7.03664011644885));
#45140=CARTESIAN_POINT('Ctrl Pts',(-26.7490969311021,23.9420804402595,7.03689287292832));
#45141=CARTESIAN_POINT('Ctrl Pts',(-26.7500059797628,23.9345794569039,7.03735599040975));
#45142=CARTESIAN_POINT('Ctrl Pts',(-26.7504129754195,23.9311756842417,7.03756627389787));
#45143=CARTESIAN_POINT('Ctrl Pts',(-26.7511833413595,23.9246446073635,7.03797001547591));
#45144=CARTESIAN_POINT('Ctrl Pts',(-26.7515475614274,23.9215174062543,7.03816344641693));
#45145=CARTESIAN_POINT('Ctrl Pts',(-26.7522983683849,23.9149877078112,7.03856757229151));
#45146=CARTESIAN_POINT('Ctrl Pts',(-26.7526841156237,23.9115851195843,7.03877829351757));
#45147=CARTESIAN_POINT('Ctrl Pts',(-26.753579195574,23.9035757950988,7.0392746255987));
#45148=CARTESIAN_POINT('Ctrl Pts',(-26.754084014079,23.8989685710524,7.03956037876169));
#45149=CARTESIAN_POINT('Ctrl Pts',(-26.7553852946594,23.8868510656411,7.04031259731485));
#45150=CARTESIAN_POINT('Ctrl Pts',(-26.756165294774,23.8793390784422,7.04077958172939));
#45151=CARTESIAN_POINT('Ctrl Pts',(-26.7677055367155,23.7642615450507,7.04794372449195));
#45152=CARTESIAN_POINT('Ctrl Pts',(-26.7730720124202,23.6562378930516,7.05481039927442));
#45153=CARTESIAN_POINT('Ctrl Pts',(-26.7730018526427,23.548160445141,7.06183203780204));
#45154=CARTESIAN_POINT('Ctrl Pts',(-26.7730018552423,23.5481644535157,7.06183177738368));
#45155=CARTESIAN_POINT('Ctrl Pts',(-26.772791063168,23.2228270107721,7.08296847867985));
#45156=CARTESIAN_POINT('Ctrl Pts',(-26.7233244541257,22.8994492477813,7.10558782499766));
#45157=CARTESIAN_POINT('Ctrl Pts',(-26.6058433168695,22.5235175808366,7.13146215824044));
#45158=CARTESIAN_POINT('Ctrl Pts',(-26.5833039843811,22.4587305605738,7.13589430784861));
#45159=CARTESIAN_POINT('Ctrl Pts',(-26.5547643434763,22.3844276793157,7.14090695062496));
#45160=CARTESIAN_POINT('Ctrl Pts',(-26.5507633807697,22.3741685778357,7.14159746206679));
#45161=CARTESIAN_POINT('Ctrl Pts',(-26.5454944464049,22.3608601085036,7.14249095649197));
#45162=CARTESIAN_POINT('Ctrl Pts',(-26.5442743236775,22.3577920613448,7.1426967800971));
#45163=CARTESIAN_POINT('Ctrl Pts',(-26.542288632768,22.3528212230282,7.14302999406615));
#45164=CARTESIAN_POINT('Ctrl Pts',(-26.5415259632994,22.3509172880979,7.14315755990102));
#45165=CARTESIAN_POINT('Ctrl Pts',(-26.5400583018947,22.3472635134997,7.14340224596881));
#45166=CARTESIAN_POINT('Ctrl Pts',(-26.5393535931335,22.3455135699529,7.14351938263826));
#45167=CARTESIAN_POINT('Ctrl Pts',(-26.5377296418131,22.3414911457455,7.14378851167677));
#45168=CARTESIAN_POINT('Ctrl Pts',(-26.5368093404816,22.3392190888751,7.1439404393934));
#45169=CARTESIAN_POINT('Ctrl Pts',(-26.5338806648122,22.3320123623605,7.14442206177389));
#45170=CARTESIAN_POINT('Ctrl Pts',(-26.531862632428,22.3270815889893,7.14475117155195));
#45171=CARTESIAN_POINT('Ctrl Pts',(-26.5145794557455,22.2851495461781,7.14754664845251));
#45172=CARTESIAN_POINT('Ctrl Pts',(-26.4986375841876,22.2484285731391,7.14997267212597));
#45173=CARTESIAN_POINT('Ctrl Pts',(-26.477412891756,22.2019303861763,7.15302804538257));
#45174=CARTESIAN_POINT('Ctrl Pts',(-26.472758922335,22.1918723254186,7.15368795081659));
#45175=CARTESIAN_POINT('Ctrl Pts',(-26.4622496334423,22.1694638987316,7.15515634396711));
#45176=CARTESIAN_POINT('Ctrl Pts',(-26.4563674165113,22.1571263144952,7.15596356984728));
#45177=CARTESIAN_POINT('Ctrl Pts',(-26.4181884256739,22.0783424096899,7.16111262405508));
#45178=CARTESIAN_POINT('Ctrl Pts',(-26.3836914538359,22.0129819421022,7.16535885502875));
#45179=CARTESIAN_POINT('Ctrl Pts',(-26.2318796180292,21.7478525818066,7.18270585633182));
#45180=CARTESIAN_POINT('Ctrl Pts',(-26.095449781197,21.5598393436681,7.19535458264382));
#45181=CARTESIAN_POINT('Ctrl Pts',(-25.8945273563607,21.3377663294674,7.21251886685697));
#45182=CARTESIAN_POINT('Ctrl Pts',(-25.8474388254048,21.2889135564165,7.21645180040281));
#45183=CARTESIAN_POINT('Ctrl Pts',(-25.7632003281092,21.2068670416785,7.22337497614159));
#45184=CARTESIAN_POINT('Ctrl Pts',(-25.7267570650453,21.1729807499142,7.22633608657135));
#45185=CARTESIAN_POINT('Ctrl Pts',(-25.6685523426869,21.1213203891957,7.23102338678131));
#45186=CARTESIAN_POINT('Ctrl Pts',(-25.647317355091,21.1029633187814,7.23272506672825));
#45187=CARTESIAN_POINT('Ctrl Pts',(-25.6207328879937,21.0805818395191,7.23484624173202));
#45188=CARTESIAN_POINT('Ctrl Pts',(-25.6156066298289,21.0762932187978,7.23525484887082));
#45189=CARTESIAN_POINT('Ctrl Pts',(-25.6079863099647,21.069958261286,7.23586165279084));
#45190=CARTESIAN_POINT('Ctrl Pts',(-25.6055024336119,21.0678996537572,7.23605934887651));
#45191=CARTESIAN_POINT('Ctrl Pts',(-25.6004717592207,21.0637430164268,7.23645956084057));
#45192=CARTESIAN_POINT('Ctrl Pts',(-25.5979248220529,21.0616451617776,7.23666208349603));
#45193=CARTESIAN_POINT('Ctrl Pts',(-25.59244772227,21.0571478990857,7.23709739529362));
#45194=CARTESIAN_POINT('Ctrl Pts',(-25.5895165454002,21.0547497391184,7.23733023462969));
#45195=CARTESIAN_POINT('Ctrl Pts',(-25.5816320169285,21.0483221326459,7.2379562114585));
#45196=CARTESIAN_POINT('Ctrl Pts',(-25.5766709246679,21.044302246794,7.23834973459933));
#45197=CARTESIAN_POINT('Ctrl Pts',(-25.5549491596986,21.0268081659813,7.24007124003913));
#45198=CARTESIAN_POINT('Ctrl Pts',(-25.5380661127394,21.013487432581,7.24140536910811));
#45199=CARTESIAN_POINT('Ctrl Pts',(-25.5107542909213,20.9923784572214,7.24355778964545));
#45200=CARTESIAN_POINT('Ctrl Pts',(-25.5004092563132,20.9844825361192,7.2443717561494));
#45201=CARTESIAN_POINT('Ctrl Pts',(-25.4853131159871,20.9731043421235,7.24555770633285));
#45202=CARTESIAN_POINT('Ctrl Pts',(-25.4805997451226,20.9695720224568,7.24592772921284));
#45203=CARTESIAN_POINT('Ctrl Pts',(-25.4701573427388,20.9617908352938,7.24674694579245));
#45204=CARTESIAN_POINT('Ctrl Pts',(-25.464423847832,20.9575480347713,7.24719637102217));
#45205=CARTESIAN_POINT('Ctrl Pts',(-25.457192620297,20.9522339691496,7.24776273567675));
#45206=CARTESIAN_POINT('Ctrl Pts',(-25.4557079568299,20.9511448818179,7.24787899318039));
#45207=CARTESIAN_POINT('Ctrl Pts',(-25.4486138848626,20.9459503111773,7.24843438286161));
#45208=CARTESIAN_POINT('Ctrl Pts',(-25.4429921695411,20.9418617356086,7.24887415666291));
#45209=CARTESIAN_POINT('Ctrl Pts',(-25.4334327576054,20.9349565182575,7.24962138789371));
#45210=CARTESIAN_POINT('Ctrl Pts',(-25.4295018439579,20.9321304904,7.24992849057835));
#45211=CARTESIAN_POINT('Ctrl Pts',(-25.4223009325626,20.926978155672,7.25049076194866));
#45212=CARTESIAN_POINT('Ctrl Pts',(-25.4190329236948,20.9246490747093,7.25074582656327));
#45213=CARTESIAN_POINT('Ctrl Pts',(-25.411653155878,20.9194103373574,7.25132155735793));
#45214=CARTESIAN_POINT('Ctrl Pts',(-25.4075389151891,20.9165042095412,7.25164235287342));
#45215=CARTESIAN_POINT('Ctrl Pts',(-25.3891493270713,20.9035790904507,7.25307544528895));
#45216=CARTESIAN_POINT('Ctrl Pts',(-25.374799809308,20.8936665756671,7.25419160631994));
#45217=CARTESIAN_POINT('Ctrl Pts',(-25.2473073184995,20.8071161352162,7.26409023163786));
#45218=CARTESIAN_POINT('Ctrl Pts',(-25.1294890483084,20.7376386628723,7.27312078295033));
#45219=CARTESIAN_POINT('Ctrl Pts',(-24.9216566857051,20.6322635678398,7.28876505733926));
#45220=CARTESIAN_POINT('Ctrl Pts',(-24.833773279846,20.5925536525158,7.29529729395809));
#45221=CARTESIAN_POINT('Ctrl Pts',(-24.5747085348605,20.4892195492738,7.31416980431325));
#45222=CARTESIAN_POINT('Ctrl Pts',(-24.3997119985493,20.4361125219717,7.32646452255243));
#45223=CARTESIAN_POINT('Ctrl Pts',(-24.2055906109272,20.3947965654028,7.33901815918339));
#45224=CARTESIAN_POINT('Ctrl Pts',(-24.1900148726184,20.3916017872667,7.34001787640688));
#45225=CARTESIAN_POINT('Ctrl Pts',(-24.1707338180533,20.3877954773254,7.34124555817823));
#45226=CARTESIAN_POINT('Ctrl Pts',(-24.1670505963051,20.3870750476945,7.34147963608449));
#45227=CARTESIAN_POINT('Ctrl Pts',(-24.1612535476739,20.385951668715,7.34184734593042));
#45228=CARTESIAN_POINT('Ctrl Pts',(-24.1591405762026,20.3855444026088,7.34198122514609));
#45229=CARTESIAN_POINT('Ctrl Pts',(-24.1551939944578,20.3847878149035,7.34223100530482));
#45230=CARTESIAN_POINT('Ctrl Pts',(-24.1533605008131,20.3844379723382,7.34234693544741));
#45231=CARTESIAN_POINT('Ctrl Pts',(-24.1492481948478,20.3836570196673,7.34260670222978));
#45232=CARTESIAN_POINT('Ctrl Pts',(-24.1469692255103,20.38322677735,7.34275048826914));
#45233=CARTESIAN_POINT('Ctrl Pts',(-24.1411841798565,20.382141095555,7.34311504917113));
#45234=CARTESIAN_POINT('Ctrl Pts',(-24.1376774658678,20.3814890139183,7.34333563160708));
#45235=CARTESIAN_POINT('Ctrl Pts',(-24.1184656232715,20.3779495145529,7.34454194124999));
#45236=CARTESIAN_POINT('Ctrl Pts',(-24.1027399208908,20.3751729642539,7.34552141526681));
#45237=CARTESIAN_POINT('Ctrl Pts',(-23.8016124003484,20.3243105198888,7.36413665936903));
#45238=CARTESIAN_POINT('Ctrl Pts',(-23.5109849449434,20.3147611379025,7.37977718443123));
#45239=CARTESIAN_POINT('Ctrl Pts',(-23.1198590570928,20.354690379954,7.40189722846873));
#45240=CARTESIAN_POINT('Ctrl Pts',(-23.0173415586127,20.3701802405233,7.40778604784257));
#45241=CARTESIAN_POINT('Ctrl Pts',(-22.8457207861161,20.4046436993957,7.41795617196829));
#45242=CARTESIAN_POINT('Ctrl Pts',(-22.7761793150165,20.4210306696376,7.42216505115728));
#45243=CARTESIAN_POINT('Ctrl Pts',(-22.6839097937773,20.4460372913502,7.42789635556053));
#45244=CARTESIAN_POINT('Ctrl Pts',(-22.6606488263648,20.4526232451091,7.42935381937877));
#45245=CARTESIAN_POINT('Ctrl Pts',(-22.6271301356691,20.4625221805971,7.43147318177829));
#45246=CARTESIAN_POINT('Ctrl Pts',(-22.616811118058,20.4656260061574,7.43212828904688));
#45247=CARTESIAN_POINT('Ctrl Pts',(-22.5984715160421,20.4712427715585,7.43329738327003));
#45248=CARTESIAN_POINT('Ctrl Pts',(-22.5904447945101,20.4737354570951,7.43381070445361));
#45249=CARTESIAN_POINT('Ctrl Pts',(-22.5784155645964,20.4775227734509,7.43458249004778));
#45250=CARTESIAN_POINT('Ctrl Pts',(-22.5744056463861,20.4787939019907,7.43484018062508));
#45251=CARTESIAN_POINT('Ctrl Pts',(-22.5673027454038,20.4810608077619,7.43529738127025));
#45252=CARTESIAN_POINT('Ctrl Pts',(-22.5642087523555,20.4820534205339,7.43549678677924));
#45253=CARTESIAN_POINT('Ctrl Pts',(-22.5580362785763,20.4840439702139,7.43589510120443));
#45254=CARTESIAN_POINT('Ctrl Pts',(-22.5549577890841,20.4850418683532,7.43609400865422));
#45255=CARTESIAN_POINT('Ctrl Pts',(-22.546626110986,20.4877564723851,7.43663301586101));
#45256=CARTESIAN_POINT('Ctrl Pts',(-22.5413758443812,20.4894820511101,7.43697340852295));
#45257=CARTESIAN_POINT('Ctrl Pts',(-22.5218651529371,20.4959501868664,7.43824110161262));
#45258=CARTESIAN_POINT('Ctrl Pts',(-22.5076336896107,20.5007789128158,7.43917125108322));
#45259=CARTESIAN_POINT('Ctrl Pts',(-22.2847731716397,20.5781377546223,7.45382458245888));
#45260=CARTESIAN_POINT('Ctrl Pts',(-22.0841519471624,20.6718124009388,7.46828502425969));
#45261=CARTESIAN_POINT('Ctrl Pts',(-21.7916788128761,20.846928895444,7.49121324581711));
#45262=CARTESIAN_POINT('Ctrl Pts',(-21.6921713746734,20.9143325966398,7.49937534582747));
#45263=CARTESIAN_POINT('Ctrl Pts',(-21.5199618668321,21.0455893910299,7.51397777405507));
#45264=CARTESIAN_POINT('Ctrl Pts',(-21.4459209391825,21.1074654745548,7.52043227576709));
#45265=CARTESIAN_POINT('Ctrl Pts',(-21.3444563501271,21.2003018666075,7.52942208454465));
#45266=CARTESIAN_POINT('Ctrl Pts',(-21.3146815527309,21.2286092204901,7.53207905586681));
#45267=CARTESIAN_POINT('Ctrl Pts',(-21.2666815142398,21.27602358869,7.53638221234977));
#45268=CARTESIAN_POINT('Ctrl Pts',(-21.2481360782834,21.2947982931931,7.53804986163973));
#45269=CARTESIAN_POINT('Ctrl Pts',(-21.2267962651321,21.3169393968376,7.53997245828482));
#45270=CARTESIAN_POINT('Ctrl Pts',(-21.2237762594394,21.3200855567527,7.54024463073137));
#45271=CARTESIAN_POINT('Ctrl Pts',(-21.219184523971,21.324888579178,7.54065857141966));
#45272=CARTESIAN_POINT('Ctrl Pts',(-21.2176081689569,21.3265409823117,7.54080069982033));
#45273=CARTESIAN_POINT('Ctrl Pts',(-21.2147480317616,21.3295454889857,7.54105861411945));
#45274=CARTESIAN_POINT('Ctrl Pts',(-21.21346367092,21.3308970263831,7.54117444528726));
#45275=CARTESIAN_POINT('Ctrl Pts',(-21.2106803695851,21.3338309987643,7.54142548840966));
#45276=CARTESIAN_POINT('Ctrl Pts',(-21.2091818655203,21.3354138356717,7.5415606661751));
#45277=CARTESIAN_POINT('Ctrl Pts',(-21.2050915306801,21.3397431554395,7.5419297035508));
#45278=CARTESIAN_POINT('Ctrl Pts',(-21.2025029092365,21.3424926865608,7.54216331358256));
#45279=CARTESIAN_POINT('Ctrl Pts',(-21.1900125993753,21.3558062086021,7.54329082889341));
#45280=CARTESIAN_POINT('Ctrl Pts',(-21.1801771418345,21.3664325143754,7.54417968625659));
#45281=CARTESIAN_POINT('Ctrl Pts',(-21.1693541032826,21.3782850586343,7.54515939428888));
#45282=CARTESIAN_POINT('Ctrl Pts',(-21.1682956349509,21.379445913753,7.54525522460535));
#45283=CARTESIAN_POINT('Ctrl Pts',(-20.9483956034279,21.6209715871171,7.56516794370171));
#45284=CARTESIAN_POINT('Ctrl Pts',(-20.7671362964794,21.8931064338559,7.58248384892978));
#45285=CARTESIAN_POINT('Ctrl Pts',(-20.5842078031875,22.285240926007,7.60703626188439));
#45286=CARTESIAN_POINT('Ctrl Pts',(-20.543664861701,22.3848756432854,7.61322765608586));
#45287=CARTESIAN_POINT('Ctrl Pts',(-20.4934454090403,22.5284700547291,7.62221428672086));
#45288=CARTESIAN_POINT('Ctrl Pts',(-20.4795898239999,22.5708958749271,7.62487657768816));
#45289=CARTESIAN_POINT('Ctrl Pts',(-20.4616778351887,22.6298650736036,7.62859296289825));
#45290=CARTESIAN_POINT('Ctrl Pts',(-20.4568644743225,22.6461745271151,7.62962248085157));
#45291=CARTESIAN_POINT('Ctrl Pts',(-20.4498938562526,22.6705011146268,7.63116082903461));
#45292=CARTESIAN_POINT('Ctrl Pts',(-20.4476380878365,22.6784899017511,7.63166645857372));
#45293=CARTESIAN_POINT('Ctrl Pts',(-20.4435915405834,22.6930353799391,7.63258791464277));
#45294=CARTESIAN_POINT('Ctrl Pts',(-20.4417905856519,22.6995892094318,7.63300340820769));
#45295=CARTESIAN_POINT('Ctrl Pts',(-20.4390007828868,22.7098687049991,7.63365559798318));
#45296=CARTESIAN_POINT('Ctrl Pts',(-20.4379978567359,22.7135905577625,7.63389183603242));
#45297=CARTESIAN_POINT('Ctrl Pts',(-20.4362230810709,22.7202240883364,7.63431307355856));
#45298=CARTESIAN_POINT('Ctrl Pts',(-20.4354486306673,22.7231350707605,7.63449798828024));
#45299=CARTESIAN_POINT('Ctrl Pts',(-20.433816575521,22.7293043933419,7.63489001966726));
#45300=CARTESIAN_POINT('Ctrl Pts',(-20.4329599975829,22.7325629992737,7.63509716942028));
#45301=CARTESIAN_POINT('Ctrl Pts',(-20.4305440606702,22.74181271121,7.63568540630311));
#45302=CARTESIAN_POINT('Ctrl Pts',(-20.4289968585103,22.7478069514308,7.63606688714573));
#45303=CARTESIAN_POINT('Ctrl Pts',(-20.4225564733642,22.7730590311039,7.63767515155898));
#45304=CARTESIAN_POINT('Ctrl Pts',(-20.4178242567538,22.7923571269514,7.63890713229311));
#45305=CARTESIAN_POINT('Ctrl Pts',(-20.3380229966455,23.1313096037672,7.66060010914705));
#45306=CARTESIAN_POINT('Ctrl Pts',(-20.3120797453052,23.4604804535238,7.68281343840332));
#45307=CARTESIAN_POINT('Ctrl Pts',(-20.3486970482049,23.9559671016107,7.71635231250167));
#45308=CARTESIAN_POINT('Ctrl Pts',(-20.3743129427217,24.1229529347272,7.72760977071262));
#45309=CARTESIAN_POINT('Ctrl Pts',(-20.4142074268507,24.2927967300776,7.73853713635104));
#45310=CARTESIAN_POINT('Ctrl Pts',(-20.415540520058,24.2984045159161,7.73889731485976));
#45311=CARTESIAN_POINT('Ctrl Pts',(-20.4174872540215,24.3064970871508,7.73941616979652));
#45312=CARTESIAN_POINT('Ctrl Pts',(-20.4180888110738,24.3089847242288,7.73957553927677));
#45313=CARTESIAN_POINT('Ctrl Pts',(-20.4191413695172,24.3133148165575,7.73985272350553));
#45314=CARTESIAN_POINT('Ctrl Pts',(-20.4195910347076,24.3151575923728,7.73997061606172));
#45315=CARTESIAN_POINT('Ctrl Pts',(-20.4204654446169,24.3187273294728,7.74019885520292));
#45316=CARTESIAN_POINT('Ctrl Pts',(-20.4208899907689,24.3204543317108,7.74030921312419));
#45317=CARTESIAN_POINT('Ctrl Pts',(-20.4219080118957,24.3245807808724,7.74057275327015));
#45318=CARTESIAN_POINT('Ctrl Pts',(-20.422502819285,24.3269799025576,7.74072585784133));
#45319=CARTESIAN_POINT('Ctrl Pts',(-20.4243130952135,24.3342457486364,7.74118919101472));
#45320=CARTESIAN_POINT('Ctrl Pts',(-20.425537174053,24.3391103511272,7.74149892310265));
#45321=CARTESIAN_POINT('Ctrl Pts',(-20.430037727319,24.3568211246066,7.74262490583368));
#45322=CARTESIAN_POINT('Ctrl Pts',(-20.4333821585991,24.3696501225706,7.74343731524509));
#45323=CARTESIAN_POINT('Ctrl Pts',(-20.5206392588227,24.696096208699,7.76403648510837));
#45324=CARTESIAN_POINT('Ctrl Pts',(-20.6513971891129,24.9953256916768,7.78133300032628));
#45325=CARTESIAN_POINT('Ctrl Pts',(-20.9077990984401,25.401685288219,7.80859403049803));
#45326=CARTESIAN_POINT('Ctrl Pts',(-21.0003140821045,25.5271611465319,7.81762297153462));
#45327=CARTESIAN_POINT('Ctrl Pts',(-21.1114546516642,25.6570547772757,7.82794708308797));
#45328=CARTESIAN_POINT('Ctrl Pts',(-21.1214657322099,25.6685880744924,7.82887270982357));
#45329=CARTESIAN_POINT('Ctrl Pts',(-21.1366265325978,25.6858053675442,7.83026825037349));
#45330=CARTESIAN_POINT('Ctrl Pts',(-21.141715280497,25.691542957167,7.83073562810581));
#45331=CARTESIAN_POINT('Ctrl Pts',(-21.1499446739746,25.7007551908365,7.83148982122015));
#45332=CARTESIAN_POINT('Ctrl Pts',(-21.1530725200089,25.7042412712239,7.8317760987448));
#45333=CARTESIAN_POINT('Ctrl Pts',(-21.1590697498251,25.7108961257881,7.83232428373989));
#45334=CARTESIAN_POINT('Ctrl Pts',(-21.1619378630086,25.7140660356886,7.83258613724012));
#45335=CARTESIAN_POINT('Ctrl Pts',(-21.1670376625938,25.7196799685721,7.83305119489872));
#45336=CARTESIAN_POINT('Ctrl Pts',(-21.1692668270736,25.7221262827303,7.83325429180324));
#45337=CARTESIAN_POINT('Ctrl Pts',(-21.1736733537322,25.7269471250379,7.83365540646793));
#45338=CARTESIAN_POINT('Ctrl Pts',(-21.1758505164851,25.7293218311563,7.83385341560884));
#45339=CARTESIAN_POINT('Ctrl Pts',(-21.1811022068799,25.7350328145702,7.83433063583144));
#45340=CARTESIAN_POINT('Ctrl Pts',(-21.1841802199276,25.7383658654079,7.83460999578571));
#45341=CARTESIAN_POINT('Ctrl Pts',(-21.1936539554178,25.7485812114403,7.83546880164589));
#45342=CARTESIAN_POINT('Ctrl Pts',(-21.2000727010021,25.7554420007215,7.83604923557149));
#45343=CARTESIAN_POINT('Ctrl Pts',(-21.2238356547185,25.7806198587517,7.83819289763715));
#45344=CARTESIAN_POINT('Ctrl Pts',(-21.2413643926754,25.7987607932295,7.83976410579842));
#45345=CARTESIAN_POINT('Ctrl Pts',(-21.2633442531961,25.8209802660862,7.84172241657613));
#45346=CARTESIAN_POINT('Ctrl Pts',(-21.2675966128527,25.825254921447,7.8421007416229));
#45347=CARTESIAN_POINT('Ctrl Pts',(-21.2767155100571,25.8343703241402,7.84291088658294));
#45348=CARTESIAN_POINT('Ctrl Pts',(-21.2815855604998,25.8392075009237,7.84334286021126));
#45349=CARTESIAN_POINT('Ctrl Pts',(-21.2875879278709,25.8451313772457,7.84387442701901));
#45350=CARTESIAN_POINT('Ctrl Pts',(-21.2887056619746,25.8462328846594,7.84397337725193));
#45351=CARTESIAN_POINT('Ctrl Pts',(-21.2941561469413,25.8515964005401,7.84445572127461));
#45352=CARTESIAN_POINT('Ctrl Pts',(-21.2985001211947,25.8558469411617,7.84483960903609));
#45353=CARTESIAN_POINT('Ctrl Pts',(-21.3097739136547,25.8668159962973,7.84583452858798));
#45354=CARTESIAN_POINT('Ctrl Pts',(-21.3167219002058,25.8735156761522,7.84644635835668));
#45355=CARTESIAN_POINT('Ctrl Pts',(-21.32657766435,25.8829341413863,7.84731237856716));
#45356=CARTESIAN_POINT('Ctrl Pts',(-21.3294605925896,25.8856789533219,7.84756547620041));
#45357=CARTESIAN_POINT('Ctrl Pts',(-21.336110999795,25.8919873014671,7.84814881498995));
#45358=CARTESIAN_POINT('Ctrl Pts',(-21.3398820022834,25.8955470926088,7.84847921021904));
#45359=CARTESIAN_POINT('Ctrl Pts',(-21.3609714408584,25.9153592813113,7.8503248592468));
#45360=CARTESIAN_POINT('Ctrl Pts',(-21.3784601787074,25.9314286193731,7.85184753991441));
#45361=CARTESIAN_POINT('Ctrl Pts',(-21.5651346063039,26.0991850481535,7.86801869267713));
#45362=CARTESIAN_POINT('Ctrl Pts',(-21.7497122490894,26.2327469140146,7.88337345929642));
#45363=CARTESIAN_POINT('Ctrl Pts',(-21.9889929044795,26.3699965076479,7.90203741202108));
#45364=CARTESIAN_POINT('Ctrl Pts',(-22.0317618329255,26.3932566857474,7.90532646861328));
#45365=CARTESIAN_POINT('Ctrl Pts',(-22.0750360380806,26.4155367862613,7.90859913775027));
#45366=CARTESIAN_POINT('Origin',(-23.5502525316942,23.5502525316942,-77.3107734492734));
#45367=CARTESIAN_POINT('',(-22.0750360149249,26.4155367743394,9.40666775021339));
#45368=CARTESIAN_POINT('',(-22.0750360476606,26.4155367911937,9.15896072794325));
#45369=CARTESIAN_POINT('',(-22.0750360153461,26.4155367745563,-77.3107734492734));
#45370=CARTESIAN_POINT('',(-26.7730012608198,23.553114597239,8.56023136266877));
#45371=CARTESIAN_POINT('Ctrl Pts',(-22.0750360149249,26.4155367743394,9.40666775021339));
#45372=CARTESIAN_POINT('Ctrl Pts',(-22.0693300256039,26.4125989961025,9.4062620900943));
#45373=CARTESIAN_POINT('Ctrl Pts',(-22.0636327609311,26.409644147122,9.40585583565952));
#45374=CARTESIAN_POINT('Ctrl Pts',(-21.9435252406745,26.346895161247,9.39726559129291));
#45375=CARTESIAN_POINT('Ctrl Pts',(-21.8328148432258,26.2803044304993,9.38884597643277));
#45376=CARTESIAN_POINT('Ctrl Pts',(-21.5324258522311,26.074108930731,9.36460508212239));
#45377=CARTESIAN_POINT('Ctrl Pts',(-21.3536239453862,25.920123866776,9.34841892696947));
#45378=CARTESIAN_POINT('Ctrl Pts',(-21.1296348953135,25.6799028791358,9.32666615536534));
#45379=CARTESIAN_POINT('Ctrl Pts',(-21.0690666933332,25.609019407015,9.32060872175227));
#45380=CARTESIAN_POINT('Ctrl Pts',(-21.0076685433264,25.5305116053166,9.31436033330049));
#45381=CARTESIAN_POINT('Ctrl Pts',(-21.0037021700256,25.5254083720678,9.31395617429862));
#45382=CARTESIAN_POINT('Ctrl Pts',(-20.9982314939797,25.5183257939267,9.31339806739935));
#45383=CARTESIAN_POINT('Ctrl Pts',(-20.996714123185,25.5163566334198,9.31324319709865));
#45384=CARTESIAN_POINT('Ctrl Pts',(-20.9941128869307,25.5129728008574,9.31297758244524));
#45385=CARTESIAN_POINT('Ctrl Pts',(-20.9930279167191,25.5115589858508,9.3128667592348));
#45386=CARTESIAN_POINT('Ctrl Pts',(-20.9909073220547,25.5087909068412,9.31265008409845));
#45387=CARTESIAN_POINT('Ctrl Pts',(-20.9898716019989,25.5074367243268,9.31254422556778));
#45388=CARTESIAN_POINT('Ctrl Pts',(-20.9877256744779,25.5046263499756,9.31232482730887));
#45389=CARTESIAN_POINT('Ctrl Pts',(-20.9866156314956,25.5031700311086,9.31221129930498));
#45390=CARTESIAN_POINT('Ctrl Pts',(-20.9830523757719,25.4984869508863,9.31184674776189));
#45391=CARTESIAN_POINT('Ctrl Pts',(-20.9806039966487,25.4952564904199,9.31159606707401));
#45392=CARTESIAN_POINT('Ctrl Pts',(-20.965830058176,25.4756867505273,9.31008220323844));
#45393=CARTESIAN_POINT('Ctrl Pts',(-20.9536539192366,25.4592344985968,9.30882940426677));
#45394=CARTESIAN_POINT('Ctrl Pts',(-20.9176690953964,25.4096308563872,9.30510768633075));
#45395=CARTESIAN_POINT('Ctrl Pts',(-20.8943317034875,25.376140863071,9.30266811575634));
#45396=CARTESIAN_POINT('Ctrl Pts',(-20.8306241714621,25.2809111451613,9.29590641296271));
#45397=CARTESIAN_POINT('Ctrl Pts',(-20.7917266950463,25.2182136249794,9.29165568680662));
#45398=CARTESIAN_POINT('Ctrl Pts',(-20.6633507077381,24.9944941470433,9.2769814377123));
#45399=CARTESIAN_POINT('Ctrl Pts',(-20.5855480221316,24.8271892071836,9.26685123065548));
#45400=CARTESIAN_POINT('Ctrl Pts',(-20.4575583560361,24.4761366516479,9.24576355663737));
#45401=CARTESIAN_POINT('Ctrl Pts',(-20.4084912742498,24.2927743407578,9.23482534984744));
#45402=CARTESIAN_POINT('Ctrl Pts',(-20.3736498714154,24.0938244850829,9.22255146402142));
#45403=CARTESIAN_POINT('Ctrl Pts',(-20.371558099717,24.0814555352083,9.22178688164962));
#45404=CARTESIAN_POINT('Ctrl Pts',(-20.3687963068003,24.0645239705988,9.2207381149868));
#45405=CARTESIAN_POINT('Ctrl Pts',(-20.3680637649673,24.0599715487491,9.22045591918552));
#45406=CARTESIAN_POINT('Ctrl Pts',(-20.3668328530604,24.0522158981095,9.21997479503461));
#45407=CARTESIAN_POINT('Ctrl Pts',(-20.3663295400452,24.049013451043,9.21977602394863));
#45408=CARTESIAN_POINT('Ctrl Pts',(-20.36536478065,24.0428139704086,9.21939102364812));
#45409=CARTESIAN_POINT('Ctrl Pts',(-20.3649027304998,24.0398170336681,9.21920481386912));
#45410=CARTESIAN_POINT('Ctrl Pts',(-20.3638154301726,24.0326979109214,9.21876225364762));
#45411=CARTESIAN_POINT('Ctrl Pts',(-20.3631939494743,24.0285751624877,9.21850578383988));
#45412=CARTESIAN_POINT('Ctrl Pts',(-20.3613812182265,24.0163895687537,9.21774720111604));
#45413=CARTESIAN_POINT('Ctrl Pts',(-20.3602125585587,24.0083234421623,9.21724437240861));
#45414=CARTESIAN_POINT('Ctrl Pts',(-20.3514109870511,23.9459071077258,9.2133479698746));
#45415=CARTESIAN_POINT('Ctrl Pts',(-20.3451373821073,23.89137721419,9.20991157343925));
#45416=CARTESIAN_POINT('Ctrl Pts',(-20.3285629176543,23.7056507099242,9.19808767401274));
#45417=CARTESIAN_POINT('Ctrl Pts',(-20.3249059031371,23.5740076506254,9.18949828178691));
#45418=CARTESIAN_POINT('Ctrl Pts',(-20.335614439619,23.2538394464317,9.16816640502373));
#45419=CARTESIAN_POINT('Ctrl Pts',(-20.3584930227046,23.0660789795015,9.15526830049522));
#45420=CARTESIAN_POINT('Ctrl Pts',(-20.4151134410909,22.7991967900413,9.13695481410728));
#45421=CARTESIAN_POINT('Ctrl Pts',(-20.4357677104259,22.7176853581571,9.13136919100403));
#45422=CARTESIAN_POINT('Ctrl Pts',(-20.4612775668464,22.6313472953767,9.12552111545527));
#45423=CARTESIAN_POINT('Ctrl Pts',(-20.4629842294908,22.6256295825864,9.12513415731335));
#45424=CARTESIAN_POINT('Ctrl Pts',(-20.465247116399,22.6181245074014,9.1246266968221));
#45425=CARTESIAN_POINT('Ctrl Pts',(-20.4657890208632,22.616332879659,9.12450558932912));
#45426=CARTESIAN_POINT('Ctrl Pts',(-20.4796955156024,22.570499789582,9.12140834197518));
#45427=CARTESIAN_POINT('Ctrl Pts',(-20.4940013530364,22.526746251127,9.11847289634632));
#45428=CARTESIAN_POINT('Ctrl Pts',(-20.5108916692095,22.4786052084335,9.11527833924467));
#45429=CARTESIAN_POINT('Ctrl Pts',(-20.5125538006588,22.473902747416,9.11496666862692));
#45430=CARTESIAN_POINT('Ctrl Pts',(-20.5150535622051,22.4668823955026,9.1145019558835));
#45431=CARTESIAN_POINT('Ctrl Pts',(-20.5158829355488,22.4645616040046,9.11434842634014));
#45432=CARTESIAN_POINT('Ctrl Pts',(-20.5173147031102,22.4605696208619,9.1140845079674));
#45433=CARTESIAN_POINT('Ctrl Pts',(-20.5179158167595,22.4588979763322,9.11397404251936));
#45434=CARTESIAN_POINT('Ctrl Pts',(-20.5191619956764,22.4554414398206,9.11374573372434));
#45435=CARTESIAN_POINT('Ctrl Pts',(-20.519807254317,22.453656623776,9.11362790282481));
#45436=CARTESIAN_POINT('Ctrl Pts',(-20.5210918133376,22.4501132650449,9.11339409018688));
#45437=CARTESIAN_POINT('Ctrl Pts',(-20.5217310699706,22.4483547054051,9.11327810567341));
#45438=CARTESIAN_POINT('Ctrl Pts',(-20.5238902199993,22.4424310755551,9.11288760286627));
#45439=CARTESIAN_POINT('Ctrl Pts',(-20.5254171857286,22.438268561178,9.11261350768204));
#45440=CARTESIAN_POINT('Ctrl Pts',(-20.5368118229272,22.4074038839989,9.11058332353545));
#45441=CARTESIAN_POINT('Ctrl Pts',(-20.5470247154046,22.3808292741652,9.10884759892222));
#45442=CARTESIAN_POINT('Ctrl Pts',(-20.5820941431527,22.2930673361856,9.10314533178313));
#45443=CARTESIAN_POINT('Ctrl Pts',(-20.60848047932,22.2325054818348,9.09925901855854));
#45444=CARTESIAN_POINT('Ctrl Pts',(-20.7087806914538,22.0203548928187,9.08567501500552));
#45445=CARTESIAN_POINT('Ctrl Pts',(-20.792707293267,21.8737976715654,9.07633574171811));
#45446=CARTESIAN_POINT('Ctrl Pts',(-20.9628748402892,21.6242759900253,9.05944158206174));
#45447=CARTESIAN_POINT('Ctrl Pts',(-21.0447920665079,21.5188556147609,9.05194001832127));
#45448=CARTESIAN_POINT('Ctrl Pts',(-21.1622847017217,21.3856075767023,9.04166473116141));
#45449=CARTESIAN_POINT('Ctrl Pts',(-21.1922495148485,21.3530043282206,9.03908206765125));
#45450=CARTESIAN_POINT('Ctrl Pts',(-21.2725462309406,21.2691720958402,9.0322434301737));
#45451=CARTESIAN_POINT('Ctrl Pts',(-21.3239328900941,21.2189924467901,9.02794715876865));
#45452=CARTESIAN_POINT('Ctrl Pts',(-21.3839983972756,21.1641360816232,9.0229928859103));
#45453=CARTESIAN_POINT('Ctrl Pts',(-21.3910756550575,21.1577300343084,9.02241017983554));
#45454=CARTESIAN_POINT('Ctrl Pts',(-21.4014558845418,21.1484178401541,9.02155698346243));
#45455=CARTESIAN_POINT('Ctrl Pts',(-21.4047365576394,21.1454868214699,9.02128754206462));
#45456=CARTESIAN_POINT('Ctrl Pts',(-21.4105544469587,21.1403103854906,9.02081008790857));
#45457=CARTESIAN_POINT('Ctrl Pts',(-21.4130892270996,21.1380622300754,9.02060219050962));
#45458=CARTESIAN_POINT('Ctrl Pts',(-21.4183540237514,21.1334075721226,9.02017063559648));
#45459=CARTESIAN_POINT('Ctrl Pts',(-21.4210845795764,21.1310016893307,9.01994695258616));
#45460=CARTESIAN_POINT('Ctrl Pts',(-21.4281204399331,21.1248235566051,9.01937094240777));
#45461=CARTESIAN_POINT('Ctrl Pts',(-21.4324317165647,21.1210581544547,9.01901833044802));
#45462=CARTESIAN_POINT('Ctrl Pts',(-21.4500441560077,21.105758247107,9.01757920980507));
#45463=CARTESIAN_POINT('Ctrl Pts',(-21.4634295049765,21.0943215139235,9.01648865867825));
#45464=CARTESIAN_POINT('Ctrl Pts',(-21.4976616129309,21.0655547678957,9.01370729219794));
#45465=CARTESIAN_POINT('Ctrl Pts',(-21.5186342433715,21.0483773319089,9.01201033876448));
#45466=CARTESIAN_POINT('Ctrl Pts',(-21.6035427254177,20.9806054954448,9.00516674341493));
#45467=CARTESIAN_POINT('Ctrl Pts',(-21.6691669919205,20.9321844912677,8.99993579921483));
#45468=CARTESIAN_POINT('Ctrl Pts',(-21.9118819206311,20.7669363122878,8.98079066413754));
#45469=CARTESIAN_POINT('Ctrl Pts',(-22.0985520839433,20.6651782209173,8.96639241997261));
#45470=CARTESIAN_POINT('Ctrl Pts',(-22.4317794521799,20.5241040243134,8.94193647466219));
#45471=CARTESIAN_POINT('Ctrl Pts',(-22.5736433853384,20.47538653545,8.93188904065837));
#45472=CARTESIAN_POINT('Ctrl Pts',(-22.7218603744945,20.4357867892199,8.92207143605047));
#45473=CARTESIAN_POINT('Ctrl Pts',(-22.725327123705,20.4348667612535,8.92184218289966));
#45474=CARTESIAN_POINT('Ctrl Pts',(-22.7339025768487,20.4326062706231,8.92127604076997));
#45475=CARTESIAN_POINT('Ctrl Pts',(-22.7390130760553,20.4312725695241,8.92093947971316));
#45476=CARTESIAN_POINT('Ctrl Pts',(-22.7529741535043,20.4276657436314,8.92002235152611));
#45477=CARTESIAN_POINT('Ctrl Pts',(-22.7618312377635,20.425417667412,8.91944303763402));
#45478=CARTESIAN_POINT('Ctrl Pts',(-22.7845531374309,20.4197532266932,8.91796354097226));
#45479=CARTESIAN_POINT('Ctrl Pts',(-22.7984315052796,20.4163912355797,8.91706622479146));
#45480=CARTESIAN_POINT('Ctrl Pts',(-22.81598898155,20.4122613407582,8.91593944024253));
#45481=CARTESIAN_POINT('Ctrl Pts',(-22.8196474222199,20.4114075451084,8.91570511278049));
#45482=CARTESIAN_POINT('Ctrl Pts',(-22.8254263324583,20.4100695315962,8.91533570186497));
#45483=CARTESIAN_POINT('Ctrl Pts',(-22.8275457989952,20.409581063396,8.91520037313522));
#45484=CARTESIAN_POINT('Ctrl Pts',(-22.8314831907167,20.4086778192568,8.9149492609704));
#45485=CARTESIAN_POINT('Ctrl Pts',(-22.8333009701613,20.4082624779539,8.9148334454313));
#45486=CARTESIAN_POINT('Ctrl Pts',(-22.8373511078308,20.407340766768,8.91457565739511));
#45487=CARTESIAN_POINT('Ctrl Pts',(-22.8395836402864,20.4068351987393,8.9144337320227));
#45488=CARTESIAN_POINT('Ctrl Pts',(-22.8442020414387,20.4057945106066,8.91414048872522));
#45489=CARTESIAN_POINT('Ctrl Pts',(-22.8465879853694,20.4052597260567,8.91398919023795));
#45490=CARTESIAN_POINT('Ctrl Pts',(-22.8595563643712,20.4023684951574,8.913167886954));
#45491=CARTESIAN_POINT('Ctrl Pts',(-22.8701501992939,20.4000627075052,8.91250077538682));
#45492=CARTESIAN_POINT('Ctrl Pts',(-22.9629288743122,20.3803589251436,8.90669002662913));
#45493=CARTESIAN_POINT('Ctrl Pts',(-23.0457613558124,20.3661253360119,8.90171917797257));
#45494=CARTESIAN_POINT('Ctrl Pts',(-23.2670546327331,20.3369537530503,8.88878692402686));
#45495=CARTESIAN_POINT('Ctrl Pts',(-23.4060887453021,20.3277206224911,8.88101472695495));
#45496=CARTESIAN_POINT('Ctrl Pts',(-23.8151514386645,20.3270909595107,8.85815754936258));
#45497=CARTESIAN_POINT('Ctrl Pts',(-24.0839495696946,20.3605686570519,8.84305050621779));
#45498=CARTESIAN_POINT('Ctrl Pts',(-24.3494520537814,20.4281674904296,8.82645218949149));
#45499=CARTESIAN_POINT('Ctrl Pts',(-24.3534829326035,20.4292020989398,8.82619981888059));
#45500=CARTESIAN_POINT('Ctrl Pts',(-24.3712390374454,20.4337962473421,8.82508646066624));
#45501=CARTESIAN_POINT('Ctrl Pts',(-24.3849425283699,20.4374384970469,8.82422283586093));
#45502=CARTESIAN_POINT('Ctrl Pts',(-24.4038252106915,20.4425909766921,8.82302660953199));
#45503=CARTESIAN_POINT('Ctrl Pts',(-24.4090254547232,20.4440239945641,8.82269652098761));
#45504=CARTESIAN_POINT('Ctrl Pts',(-24.4173145965464,20.446330618598,8.82216931564578));
#45505=CARTESIAN_POINT('Ctrl Pts',(-24.420405845019,20.4471958003253,8.82197247364255));
#45506=CARTESIAN_POINT('Ctrl Pts',(-24.4264256675265,20.4488903369573,8.82158869274214));
#45507=CARTESIAN_POINT('Ctrl Pts',(-24.4293543704854,20.4497192253362,8.82140176923354));
#45508=CARTESIAN_POINT('Ctrl Pts',(-24.4363699305157,20.4517155247679,8.82095349707542));
#45509=CARTESIAN_POINT('Ctrl Pts',(-24.4404556528194,20.452886871872,8.82069202012794));
#45510=CARTESIAN_POINT('Ctrl Pts',(-24.4527487607334,20.4564375498956,8.81990404059399));
#45511=CARTESIAN_POINT('Ctrl Pts',(-24.4609489632615,20.4588414311923,8.81937673591742));
#45512=CARTESIAN_POINT('Ctrl Pts',(-24.5122985095431,20.4741165407056,8.81606412278944));
#45513=CARTESIAN_POINT('Ctrl Pts',(-24.555181880308,20.4878577545529,8.81325039051559));
#45514=CARTESIAN_POINT('Ctrl Pts',(-24.6878813297448,20.5334662896443,8.80438963721416));
#45515=CARTESIAN_POINT('Ctrl Pts',(-24.7765746908378,20.5684192842294,8.7982428594651));
#45516=CARTESIAN_POINT('Ctrl Pts',(-24.9497362750173,20.6456934639883,8.7857932618309));
#45517=CARTESIAN_POINT('Ctrl Pts',(-25.0341547673249,20.6879020549993,8.77949860670387));
#45518=CARTESIAN_POINT('Ctrl Pts',(-25.1923601552144,20.7758849055145,8.7673137328769));
#45519=CARTESIAN_POINT('Ctrl Pts',(-25.2663926880752,20.8210592948337,8.76143716296441));
#45520=CARTESIAN_POINT('Ctrl Pts',(-25.4915762096681,20.9712544362521,8.74312637556821));
#45521=CARTESIAN_POINT('Ctrl Pts',(-25.6356371264473,21.0862806123738,8.73075174116724));
#45522=CARTESIAN_POINT('Ctrl Pts',(-25.7768761663417,21.2203642251367,8.71848811026165));
#45523=CARTESIAN_POINT('Ctrl Pts',(-25.7846089752406,21.2277789317789,8.71781628523167));
#45524=CARTESIAN_POINT('Ctrl Pts',(-25.7947493448923,21.237599682926,8.71693494692813));
#45525=CARTESIAN_POINT('Ctrl Pts',(-25.7971901563625,21.239971065189,8.71672278014685));
#45526=CARTESIAN_POINT('Ctrl Pts',(-25.8009639274506,21.2436491285054,8.71639471181653));
#45527=CARTESIAN_POINT('Ctrl Pts',(-25.8022995063561,21.2449530998311,8.71627859814008));
#45528=CARTESIAN_POINT('Ctrl Pts',(-25.8049689389292,21.2475638917852,8.71604650878675));
#45529=CARTESIAN_POINT('Ctrl Pts',(-25.8063027812085,21.2488707030718,8.71593053433649));
#45530=CARTESIAN_POINT('Ctrl Pts',(-25.8089213861267,21.2514407049622,8.71570284068252));
#45531=CARTESIAN_POINT('Ctrl Pts',(-25.8102062196352,21.2527038081397,8.7155911156034));
#45532=CARTESIAN_POINT('Ctrl Pts',(-25.8131135242264,21.2555667399545,8.71533829030188));
#45533=CARTESIAN_POINT('Ctrl Pts',(-25.8147353614414,21.2571672153153,8.71519724116482));
#45534=CARTESIAN_POINT('Ctrl Pts',(-25.8188380179117,21.2612244313439,8.71484040668034));
#45535=CARTESIAN_POINT('Ctrl Pts',(-25.8213165525828,21.2636834936448,8.71462480318672));
#45536=CARTESIAN_POINT('Ctrl Pts',(-25.855970368343,21.2981769842126,8.71160982936855));
#45537=CARTESIAN_POINT('Ctrl Pts',(-25.8874711995232,21.3308858581414,8.70886314859998));
#45538=CARTESIAN_POINT('Ctrl Pts',(-25.9826650230089,21.434006052176,8.70050218753649));
#45539=CARTESIAN_POINT('Ctrl Pts',(-26.0439497945611,21.5065777453247,8.69503116718976));
#45540=CARTESIAN_POINT('Ctrl Pts',(-26.1244886013955,21.6109773165457,8.68754748319553));
#45541=CARTESIAN_POINT('Ctrl Pts',(-26.1465287066999,21.6405850705771,8.68546582208182));
#45542=CARTESIAN_POINT('Ctrl Pts',(-26.1914757742143,21.7031819615139,8.68113504891112));
#45543=CARTESIAN_POINT('Ctrl Pts',(-26.2142844066333,21.7362337525186,8.67888769499534));
#45544=CARTESIAN_POINT('Ctrl Pts',(-26.3925103800117,22.0051135269178,8.66085334732086));
#45545=CARTESIAN_POINT('Ctrl Pts',(-26.5169070678735,22.2599736962512,8.64512639871806));
#45546=CARTESIAN_POINT('Ctrl Pts',(-26.6122974331258,22.5450995320368,8.62692134050195));
#45547=CARTESIAN_POINT('Ctrl Pts',(-26.6179478791951,22.562478891335,8.62581002499323));
#45548=CARTESIAN_POINT('Ctrl Pts',(-26.6252528671905,22.5856145957235,8.62432812167044));
#45549=CARTESIAN_POINT('Ctrl Pts',(-26.6270396910123,22.5913290799494,8.62396189239165));
#45550=CARTESIAN_POINT('Ctrl Pts',(-26.6297949656264,22.6002277756664,8.62339126926788));
#45551=CARTESIAN_POINT('Ctrl Pts',(-26.6307744322144,22.6034085848176,8.62318723756324));
#45552=CARTESIAN_POINT('Ctrl Pts',(-26.632720139406,22.6097622284839,8.62277955483131));
#45553=CARTESIAN_POINT('Ctrl Pts',(-26.6336864128171,22.6129350488533,8.62257590516293));
#45554=CARTESIAN_POINT('Ctrl Pts',(-26.635845510548,22.6200640531551,8.62211817647134));
#45555=CARTESIAN_POINT('Ctrl Pts',(-26.6370356258624,22.6240210454758,8.62186400901926));
#45556=CARTESIAN_POINT('Ctrl Pts',(-26.6404994314427,22.635618610807,8.62111876172893));
#45557=CARTESIAN_POINT('Ctrl Pts',(-26.6427523742123,22.6432653030972,8.6206270036299));
#45558=CARTESIAN_POINT('Ctrl Pts',(-26.6477628632152,22.6605070748685,8.61951727753619));
#45559=CARTESIAN_POINT('Ctrl Pts',(-26.6505042317609,22.6701067344287,8.61889878542121));
#45560=CARTESIAN_POINT('Ctrl Pts',(-26.6590936589302,22.7007230690444,8.61692412621599));
#45561=CARTESIAN_POINT('Ctrl Pts',(-26.6647728495127,22.7217861084657,8.61556248635779));
#45562=CARTESIAN_POINT('Ctrl Pts',(-26.6858634014066,22.8032902772804,8.61028067296137));
#45563=CARTESIAN_POINT('Ctrl Pts',(-26.6997318346485,22.8641130477225,8.60631148929673));
#45564=CARTESIAN_POINT('Ctrl Pts',(-26.7527053584887,23.1320994880918,8.58869568065027));
#45565=CARTESIAN_POINT('Ctrl Pts',(-26.7731884098208,23.3423807074104,8.57449613895324));
#45566=CARTESIAN_POINT('Ctrl Pts',(-26.7730012608198,23.553114597239,8.56023136266877));
#45567=CARTESIAN_POINT('Ctrl Pts',(-26.7730012594657,23.5531161215966,8.56023125948356));
#45568=CARTESIAN_POINT('Ctrl Pts',(-26.7728196090006,23.7575496561465,8.54639296027699));
#45569=CARTESIAN_POINT('Ctrl Pts',(-26.7531861185436,23.9615361605529,8.53256708739775));
#45570=CARTESIAN_POINT('Ctrl Pts',(-26.7132557045306,24.1679592180812,8.51935782217261));
#45571=CARTESIAN_POINT('Ctrl Pts',(-26.7121486081331,24.1736014105547,8.51899740405998));
#45572=CARTESIAN_POINT('Ctrl Pts',(-26.7104005545642,24.1823856813531,8.51843729125752));
#45573=CARTESIAN_POINT('Ctrl Pts',(-26.7097700043974,24.1855297823828,8.51823701691999));
#45574=CARTESIAN_POINT('Ctrl Pts',(-26.7087070018829,24.1907894821639,8.51790232884377));
#45575=CARTESIAN_POINT('Ctrl Pts',(-26.7082771158951,24.1929055880308,8.51776776959212));
#45576=CARTESIAN_POINT('Ctrl Pts',(-26.7074278434914,24.1970646858325,8.51750348716521));
#45577=CARTESIAN_POINT('Ctrl Pts',(-26.7070086001398,24.199107705484,8.51737375584393));
#45578=CARTESIAN_POINT('Ctrl Pts',(-26.7062083077674,24.2029884848148,8.51712749762943));
#45579=CARTESIAN_POINT('Ctrl Pts',(-26.7058276394067,24.2048263049453,8.51701095007932));
#45580=CARTESIAN_POINT('Ctrl Pts',(-26.704951768458,24.209036381538,8.51674412876978));
#45581=CARTESIAN_POINT('Ctrl Pts',(-26.7044554960813,24.2114084095304,8.51659391758523));
#45582=CARTESIAN_POINT('Ctrl Pts',(-26.7029176085045,24.218717893009,8.51613140177687));
#45583=CARTESIAN_POINT('Ctrl Pts',(-26.7018670656432,24.2236534940032,8.51581960958387));
#45584=CARTESIAN_POINT('Ctrl Pts',(-26.6938150170095,24.261051585203,8.51346084901651));
#45585=CARTESIAN_POINT('Ctrl Pts',(-26.6863233873323,24.293408095687,8.51144152933166));
#45586=CARTESIAN_POINT('Ctrl Pts',(-26.6763962668058,24.3334560034595,8.50896240638243));
#45587=CARTESIAN_POINT('Ctrl Pts',(-26.6744306793447,24.3412602656334,8.50848025050184));
#45588=CARTESIAN_POINT('Ctrl Pts',(-26.6317962774281,24.5078997838623,8.49820398927304));
#45589=CARTESIAN_POINT('Ctrl Pts',(-26.5790890788471,24.663428986897,8.48897307272299));
#45590=CARTESIAN_POINT('Ctrl Pts',(-26.5036208403333,24.8404232976196,8.47820548699661));
#45591=CARTESIAN_POINT('Ctrl Pts',(-26.4921306508403,24.8664128987262,8.47661771679408));
#45592=CARTESIAN_POINT('Ctrl Pts',(-26.4701175416513,24.9144752476664,8.47366394404807));
#45593=CARTESIAN_POINT('Ctrl Pts',(-26.4596842412649,24.9365866976639,8.47229802557481));
#45594=CARTESIAN_POINT('Ctrl Pts',(-26.4273223206903,25.0031970791608,8.46815690135125));
#45595=CARTESIAN_POINT('Ctrl Pts',(-26.404617164617,25.047309934142,8.46537837000793));
#45596=CARTESIAN_POINT('Ctrl Pts',(-26.3152669558422,25.2114762383933,8.45485317602641));
#45597=CARTESIAN_POINT('Ctrl Pts',(-26.2419975088004,25.3277430344337,8.44701098538239));
#45598=CARTESIAN_POINT('Ctrl Pts',(-26.1259809733067,25.4881438030073,8.43532242598728));
#45599=CARTESIAN_POINT('Ctrl Pts',(-26.0890394989321,25.5362937152804,8.43169187632456));
#45600=CARTESIAN_POINT('Ctrl Pts',(-26.0449155060824,25.5905613594779,8.4274442720638));
#45601=CARTESIAN_POINT('Ctrl Pts',(-26.0390373624628,25.5977274477428,8.42688015502983));
#45602=CARTESIAN_POINT('Ctrl Pts',(-26.0283436062351,25.6106501915799,8.42585697534395));
#45603=CARTESIAN_POINT('Ctrl Pts',(-26.0235386256651,25.6164155907117,8.42539834622326));
#45604=CARTESIAN_POINT('Ctrl Pts',(-26.0161206527701,25.625253312027,8.42469199003975));
#45605=CARTESIAN_POINT('Ctrl Pts',(-26.0135219366227,25.6283376279852,8.4244448486151));
#45606=CARTESIAN_POINT('Ctrl Pts',(-26.0089692228177,25.6337205292647,8.42401242361477));
#45607=CARTESIAN_POINT('Ctrl Pts',(-26.0070177704295,25.6360212690553,8.42382724496245));
#45608=CARTESIAN_POINT('Ctrl Pts',(-26.0029201503349,25.6408385868944,8.42343877255174));
#45609=CARTESIAN_POINT('Ctrl Pts',(-26.0007733344801,25.6433546067758,8.42323545215164));
#45610=CARTESIAN_POINT('Ctrl Pts',(-25.9947964162373,25.6503376211207,8.42266996248267));
#45611=CARTESIAN_POINT('Ctrl Pts',(-25.9909579615428,25.6547974208,8.42230744752332));
#45612=CARTESIAN_POINT('Ctrl Pts',(-25.9756516325742,25.6724832458901,8.42086442395779));
#45613=CARTESIAN_POINT('Ctrl Pts',(-25.9640884589165,25.685626058695,8.41977995140539));
#45614=CARTESIAN_POINT('Ctrl Pts',(-25.7714889400267,25.9009730692326,8.40180694506239));
#45615=CARTESIAN_POINT('Ctrl Pts',(-25.5657695117716,26.0795618370056,8.38377041670967));
#45616=CARTESIAN_POINT('Ctrl Pts',(-25.2774714441396,26.2721117113345,8.36031096543834));
#45617=CARTESIAN_POINT('Ctrl Pts',(-25.2133201405861,26.3117754642694,8.35520110835401));
#45618=CARTESIAN_POINT('Ctrl Pts',(-25.0723894771157,26.3922172448623,8.34427388261923));
#45619=CARTESIAN_POINT('Ctrl Pts',(-24.9952273661546,26.432216083076,8.33847120855214));
#45620=CARTESIAN_POINT('Ctrl Pts',(-24.8748410784521,26.4885687895117,8.3297793857843));
#45621=CARTESIAN_POINT('Ctrl Pts',(-24.8327273272608,26.5071928652991,8.3268040515201));
#45622=CARTESIAN_POINT('Ctrl Pts',(-24.7765973542574,26.5305904274676,8.32293719801859));
#45623=CARTESIAN_POINT('Ctrl Pts',(-24.7629288962999,26.5361781253241,8.3220031860775));
#45624=CARTESIAN_POINT('Ctrl Pts',(-24.7403665159098,26.5452211940925,8.32047450659421));
#45625=CARTESIAN_POINT('Ctrl Pts',(-24.7314949607927,26.5487312982271,8.31987673685794));
#45626=CARTESIAN_POINT('Ctrl Pts',(-24.7204165125042,26.5530577792377,8.31913450134647));
#45627=CARTESIAN_POINT('Ctrl Pts',(-24.7182242638808,26.5539111556988,8.3189878309754));
#45628=CARTESIAN_POINT('Ctrl Pts',(-24.7139589944422,26.5555661211502,8.31870287073323));
#45629=CARTESIAN_POINT('Ctrl Pts',(-24.7118860757095,26.5563679672524,8.3185645654007));
#45630=CARTESIAN_POINT('Ctrl Pts',(-24.7082457855265,26.5577717761143,8.3183220119863));
#45631=CARTESIAN_POINT('Ctrl Pts',(-24.7066787795218,26.5583746560185,8.31821770841885));
#45632=CARTESIAN_POINT('Ctrl Pts',(-24.7033561772978,26.5596499928583,8.31799677380087));
#45633=CARTESIAN_POINT('Ctrl Pts',(-24.7016004688582,26.5603221362711,8.31788016207136));
#45634=CARTESIAN_POINT('Ctrl Pts',(-24.6966029714595,26.5622303318655,8.31754861120656));
#45635=CARTESIAN_POINT('Ctrl Pts',(-24.6933597606162,26.5634626907987,8.31733389553557));
#45636=CARTESIAN_POINT('Ctrl Pts',(-24.6795874128415,26.5686704873514,8.31642398458779));
#45637=CARTESIAN_POINT('Ctrl Pts',(-24.6690393142162,26.5725960550055,8.31573175842992));
#45638=CARTESIAN_POINT('Ctrl Pts',(-24.4831411229539,26.6406731183705,8.30361035364273));
#45639=CARTESIAN_POINT('Ctrl Pts',(-24.3025333375933,26.6895321394603,8.29304662955898));
#45640=CARTESIAN_POINT('Ctrl Pts',(-23.971170453199,26.7489092952372,8.27418545002759));
#45641=CARTESIAN_POINT('Ctrl Pts',(-23.821992115627,26.7650205472064,8.26587520129653));
#45642=CARTESIAN_POINT('Ctrl Pts',(-23.6483952946672,26.7715961782197,8.25599952081196));
#45643=CARTESIAN_POINT('Ctrl Pts',(-23.6245427974422,26.7722345023612,8.25463837406028));
#45644=CARTESIAN_POINT('Ctrl Pts',(-23.5061900466449,26.77408684447,8.24785805053681));
#45645=CARTESIAN_POINT('Ctrl Pts',(-23.4116821212831,26.7714084006475,8.2423581229887));
#45646=CARTESIAN_POINT('Ctrl Pts',(-23.2671489964203,26.7609396526013,8.23373010488521));
#45647=CARTESIAN_POINT('Ctrl Pts',(-23.2169587996909,26.7561181329836,8.23069399606373));
#45648=CARTESIAN_POINT('Ctrl Pts',(-23.161210594475,26.7494394312346,8.22727079363634));
#45649=CARTESIAN_POINT('Ctrl Pts',(-23.1555186583866,26.7487421151853,8.22692069138754));
#45650=CARTESIAN_POINT('Ctrl Pts',(-23.1447813887312,26.7473976001791,8.22625913111292));
#45651=CARTESIAN_POINT('Ctrl Pts',(-23.1397356613743,26.7467536400041,8.22594777621598));
#45652=CARTESIAN_POINT('Ctrl Pts',(-23.1312192925016,26.7456462424979,8.22542145811859));
#45653=CARTESIAN_POINT('Ctrl Pts',(-23.1277478315432,26.7451890883082,8.22520669415515));
#45654=CARTESIAN_POINT('Ctrl Pts',(-23.1208792143201,26.7442731747058,8.22478131496989));
#45655=CARTESIAN_POINT('Ctrl Pts',(-23.1174820309084,26.7438146505758,8.2245707074665));
#45656=CARTESIAN_POINT('Ctrl Pts',(-23.109995320567,26.7427919900362,8.22410608938111));
#45657=CARTESIAN_POINT('Ctrl Pts',(-23.1059061373006,26.7422254148125,8.22385200175497));
#45658=CARTESIAN_POINT('Ctrl Pts',(-23.091624156121,26.7402186041142,8.22296345463544));
#45659=CARTESIAN_POINT('Ctrl Pts',(-23.0814372613615,26.7387374020406,8.22232769713919));
#45660=CARTESIAN_POINT('Ctrl Pts',(-22.9769909550334,26.7230392703957,8.21578858793561));
#45661=CARTESIAN_POINT('Ctrl Pts',(-22.8834083168583,26.7046970485344,8.20975445659271));
#45662=CARTESIAN_POINT('Ctrl Pts',(-22.6259677819104,26.6422707573087,8.19263880578794));
#45663=CARTESIAN_POINT('Ctrl Pts',(-22.464583432327,26.5893624159407,8.18130077763559));
#45664=CARTESIAN_POINT('Ctrl Pts',(-22.2289912941689,26.490956817984,8.16404267294249));
#45665=CARTESIAN_POINT('Ctrl Pts',(-22.1512327745749,26.4547673447831,8.15822689933198));
#45666=CARTESIAN_POINT('Ctrl Pts',(-22.075035838959,26.4155366837419,8.15244980096843));
#45667=CARTESIAN_POINT('Ctrl Pts',(-22.0750360380806,26.4155367862613,7.90859913775027));
#45668=CARTESIAN_POINT('Ctrl Pts',(-22.1212966157915,26.4393544466329,7.91209765527108));
#45669=CARTESIAN_POINT('Ctrl Pts',(-22.1681346141975,26.4620520920954,7.91557745044412));
#45670=CARTESIAN_POINT('Ctrl Pts',(-22.2760532281321,26.5111574932639,7.92342594061295));
#45671=CARTESIAN_POINT('Ctrl Pts',(-22.3374401273027,26.5368273991184,7.92777046036409));
#45672=CARTESIAN_POINT('Ctrl Pts',(-22.4262960460565,26.5707917714342,7.93384737801415));
#45673=CARTESIAN_POINT('Ctrl Pts',(-22.453146133568,26.580647418644,7.93565660817201));
#45674=CARTESIAN_POINT('Ctrl Pts',(-22.4843250998948,26.5916232916931,7.93772348727388));
#45675=CARTESIAN_POINT('Ctrl Pts',(-22.4885283088318,26.5930931559785,7.93800141074821));
#45676=CARTESIAN_POINT('Ctrl Pts',(-22.4949100508139,26.5953100211863,7.9384222904637));
#45677=CARTESIAN_POINT('Ctrl Pts',(-22.4970863385605,26.5960633984394,7.93856562553367));
#45678=CARTESIAN_POINT('Ctrl Pts',(-22.501026957483,26.5974228152571,7.93882481273498));
#45679=CARTESIAN_POINT('Ctrl Pts',(-22.5027910020285,26.5980296538823,7.93894071242398));
#45680=CARTESIAN_POINT('Ctrl Pts',(-22.506335780753,26.5992456313266,7.93917335266004));
#45681=CARTESIAN_POINT('Ctrl Pts',(-22.5081165144121,26.5998547395287,7.93929009115026));
#45682=CARTESIAN_POINT('Ctrl Pts',(-22.5131908053321,26.6015854607113,7.93962237803307));
#45683=CARTESIAN_POINT('Ctrl Pts',(-22.5164856596664,26.6027033048531,7.93983770137244));
#45684=CARTESIAN_POINT('Ctrl Pts',(-22.5305223122431,26.6074401813383,7.94075317724377));
#45685=CARTESIAN_POINT('Ctrl Pts',(-22.5412815234598,26.6110079219806,7.94145031559819));
#45686=CARTESIAN_POINT('Ctrl Pts',(-22.7291424839303,26.6722041353058,7.95354662072114));
#45687=CARTESIAN_POINT('Ctrl Pts',(-22.9109227927993,26.7144401359785,7.96408518876877));
#45688=CARTESIAN_POINT('Ctrl Pts',(-23.397850460784,26.7838654443096,7.99164390346882));
#45689=CARTESIAN_POINT('Ctrl Pts',(-23.7048915982453,26.7837557066122,8.00850615539715));
#45690=CARTESIAN_POINT('Ctrl Pts',(-24.0192728476122,26.7387135061588,8.02774124451109));
#45691=CARTESIAN_POINT('Ctrl Pts',(-24.0312189840206,26.7369333610203,8.02847484531774));
#45692=CARTESIAN_POINT('Ctrl Pts',(-24.0495393141961,26.7340980070445,8.02960411431868));
#45693=CARTESIAN_POINT('Ctrl Pts',(-24.0559208992355,26.7330906996195,8.02999826662405));
#45694=CARTESIAN_POINT('Ctrl Pts',(-24.0664219297063,26.7314007757498,8.03064816957189));
#45695=CARTESIAN_POINT('Ctrl Pts',(-24.0705431748086,26.730729326851,8.03090356550762));
#45696=CARTESIAN_POINT('Ctrl Pts',(-24.0785158505415,26.7294144772337,8.03139828886352));
#45697=CARTESIAN_POINT('Ctrl Pts',(-24.0823674414748,26.7287720821422,8.03163758393549));
#45698=CARTESIAN_POINT('Ctrl Pts',(-24.0893945102075,26.7275869282863,8.03207470958279));
#45699=CARTESIAN_POINT('Ctrl Pts',(-24.0925703642361,26.7270464043199,8.03227246875263));
#45700=CARTESIAN_POINT('Ctrl Pts',(-24.099086429782,26.7259273271625,8.03267863856926));
#45701=CARTESIAN_POINT('Ctrl Pts',(-24.1024265483862,26.7253482640167,8.03288706523334));
#45702=CARTESIAN_POINT('Ctrl Pts',(-24.1119646491451,26.7236791753748,8.0334828984526));
#45703=CARTESIAN_POINT('Ctrl Pts',(-24.1181603351732,26.7225762685724,8.03387071535205));
#45704=CARTESIAN_POINT('Ctrl Pts',(-24.1447383103226,26.7177647122339,8.03553773604119));
#45705=CARTESIAN_POINT('Ctrl Pts',(-24.165087449699,26.7138777854465,8.03682261905959));
#45706=CARTESIAN_POINT('Ctrl Pts',(-24.5235110400513,26.6418259365914,8.05960913765149));
#45707=CARTESIAN_POINT('Ctrl Pts',(-24.8484584709887,26.5200325523019,8.08306949723859));
#45708=CARTESIAN_POINT('Ctrl Pts',(-25.2791481093562,26.2742025068544,8.11645299052329));
#45709=CARTESIAN_POINT('Ctrl Pts',(-25.4050566696986,26.1900816702109,8.1264854446279));
#45710=CARTESIAN_POINT('Ctrl Pts',(-25.5291361676184,26.0939054118031,8.1363177889767));
#45711=CARTESIAN_POINT('Ctrl Pts',(-25.5336572801594,26.0903816669915,8.13667596256107));
#45712=CARTESIAN_POINT('Ctrl Pts',(-25.5401788454504,26.0852707463635,8.13719245712185));
#45713=CARTESIAN_POINT('Ctrl Pts',(-25.5421868180476,26.0836932517117,8.13735146244009));
#45714=CARTESIAN_POINT('Ctrl Pts',(-25.5456823625131,26.0809403724056,8.13762822258328));
#45715=CARTESIAN_POINT('Ctrl Pts',(-25.5471707737668,26.0797660603,8.13774605452433));
#45716=CARTESIAN_POINT('Ctrl Pts',(-25.5500546505338,26.0774866357169,8.13797433347576));
#45717=CARTESIAN_POINT('Ctrl Pts',(-25.5514502330247,26.0763816834358,8.13808479156712));
#45718=CARTESIAN_POINT('Ctrl Pts',(-25.5547863077491,26.0737358470659,8.1383488097111));
#45719=CARTESIAN_POINT('Ctrl Pts',(-25.556725943309,26.0721938773412,8.13850229146845));
#45720=CARTESIAN_POINT('Ctrl Pts',(-25.5636796459412,26.0666527288549,8.13905246215529));
#45721=CARTESIAN_POINT('Ctrl Pts',(-25.5686835940055,26.0626407869268,8.13944823911214));
#45722=CARTESIAN_POINT('Ctrl Pts',(-25.6437303150859,26.0021027529293,8.14538250364992));
#45723=CARTESIAN_POINT('Ctrl Pts',(-25.7113946234139,25.9426753803961,8.15071485179274));
#45724=CARTESIAN_POINT('Ctrl Pts',(-25.8470429967791,25.8130809760465,8.16158220323306));
#45725=CARTESIAN_POINT('Ctrl Pts',(-25.9145037108877,25.7425019359737,8.1670914573662));
#45726=CARTESIAN_POINT('Ctrl Pts',(-26.0899562155985,25.5414034256509,8.18205587057764));
#45727=CARTESIAN_POINT('Ctrl Pts',(-26.191023970195,25.4052730702022,8.19142440878584));
#45728=CARTESIAN_POINT('Ctrl Pts',(-26.3376356816523,25.1713672060007,8.20718562660294));
#45729=CARTESIAN_POINT('Ctrl Pts',(-26.3898055229627,25.0781442833416,8.21338574377907));
#45730=CARTESIAN_POINT('Ctrl Pts',(-26.4587947432071,24.9390829319715,8.2226384471591));
#45731=CARTESIAN_POINT('Ctrl Pts',(-26.479355800829,24.8951768150773,8.22555984294994));
#45732=CARTESIAN_POINT('Ctrl Pts',(-26.5020931114405,24.8436266683897,8.22899565790881));
#45733=CARTESIAN_POINT('Ctrl Pts',(-26.5052418694249,24.8364163929021,8.22947634902831));
#45734=CARTESIAN_POINT('Ctrl Pts',(-26.5099953860003,24.8254218124167,8.23020954857767));
#45735=CARTESIAN_POINT('Ctrl Pts',(-26.5116193756198,24.8216458121401,8.23046139911188));
#45736=CARTESIAN_POINT('Ctrl Pts',(-26.5144260280766,24.815085405027,8.23089903487267));
#45737=CARTESIAN_POINT('Ctrl Pts',(-26.5156120052801,24.8123024143983,8.23108470671077));
#45738=CARTESIAN_POINT('Ctrl Pts',(-26.5180711408746,24.8065092521113,8.23147125544782));
#45739=CARTESIAN_POINT('Ctrl Pts',(-26.5193436416291,24.8034988065232,8.23167215450587));
#45740=CARTESIAN_POINT('Ctrl Pts',(-26.522818333991,24.7952434842538,8.23222314225965));
#45741=CARTESIAN_POINT('Ctrl Pts',(-26.5250112142424,24.7899947229905,8.23257354731746));
#45742=CARTESIAN_POINT('Ctrl Pts',(-26.5333635743977,24.7698532053452,8.23391853345596));
#45743=CARTESIAN_POINT('Ctrl Pts',(-26.5394251243895,24.7549203249751,8.23491643093377));
#45744=CARTESIAN_POINT('Ctrl Pts',(-26.6365719424712,24.51034696466,8.25127378739768));
#45745=CARTESIAN_POINT('Ctrl Pts',(-26.7010479566851,24.271077003911,8.26756978276075));
#45746=CARTESIAN_POINT('Ctrl Pts',(-26.7612397577237,23.8685326980362,8.29505539645285));
#45747=CARTESIAN_POINT('Ctrl Pts',(-26.7730847377883,23.7086716858235,8.30596155425315));
#45748=CARTESIAN_POINT('Ctrl Pts',(-26.7729540622555,23.4555243342009,8.3227265290296));
#45749=CARTESIAN_POINT('Ctrl Pts',(-26.7688748168057,23.3624946551144,8.32877609515968));
#45750=CARTESIAN_POINT('Ctrl Pts',(-26.7602108055362,23.2633253687827,8.33501704747616));
#45751=CARTESIAN_POINT('Ctrl Pts',(-26.7596290471725,23.2568897865697,8.33542110954034));
#45752=CARTESIAN_POINT('Ctrl Pts',(-26.7587966907662,23.2479809305018,8.3359791092887));
#45753=CARTESIAN_POINT('Ctrl Pts',(-26.7585625864425,23.24550618749,8.33613396888424));
#45754=CARTESIAN_POINT('Ctrl Pts',(-26.7581557274082,23.2412576684563,8.33639957393928));
#45755=CARTESIAN_POINT('Ctrl Pts',(-26.7579843646992,23.2394837653393,8.33651039823266));
#45756=CARTESIAN_POINT('Ctrl Pts',(-26.7576461796473,23.2360130424883,8.33672708312222));
#45757=CARTESIAN_POINT('Ctrl Pts',(-26.757479482605,23.2343162171191,8.3368329503125));
#45758=CARTESIAN_POINT('Ctrl Pts',(-26.7570714723611,23.2301966425051,8.33708980901462));
#45759=CARTESIAN_POINT('Ctrl Pts',(-26.7568287594671,23.2277740269834,8.33724072078007));
#45760=CARTESIAN_POINT('Ctrl Pts',(-26.7560687811289,23.2202740715022,8.3377074870878));
#45761=CARTESIAN_POINT('Ctrl Pts',(-26.7555421968605,23.215197651776,8.33802281545169));
#45762=CARTESIAN_POINT('Ctrl Pts',(-26.7492600043566,23.156005993375,8.34169272290107));
#45763=CARTESIAN_POINT('Ctrl Pts',(-26.7421462091938,23.1020396755507,8.34497179279391));
#45764=CARTESIAN_POINT('Ctrl Pts',(-26.7234289304278,22.9833392392724,8.35208722548512));
#45765=CARTESIAN_POINT('Ctrl Pts',(-26.7112043225033,22.9187274426189,8.35589613942054));
#45766=CARTESIAN_POINT('Ctrl Pts',(-26.6235759694993,22.5223829931758,8.37910715031988));
#45767=CARTESIAN_POINT('Ctrl Pts',(-26.4980265589085,22.2039689530081,8.39734114433901));
#45768=CARTESIAN_POINT('Ctrl Pts',(-26.2979968701983,21.865368094769,8.42071761386771));
#45769=CARTESIAN_POINT('Ctrl Pts',(-26.2698779145882,21.8203473933895,8.42391019581193));
#45770=CARTESIAN_POINT('Ctrl Pts',(-26.2358499827951,21.7687474731935,8.42767691307078));
#45771=CARTESIAN_POINT('Ctrl Pts',(-26.2310089903571,21.7614711728383,8.42821061219945));
#45772=CARTESIAN_POINT('Ctrl Pts',(-26.2237478875708,21.7506529802548,8.42900793243711));
#45773=CARTESIAN_POINT('Ctrl Pts',(-26.221350177536,21.7470960411113,8.42927070613535));
#45774=CARTESIAN_POINT('Ctrl Pts',(-26.2170601085741,21.7407591718175,8.42973996471255));
#45775=CARTESIAN_POINT('Ctrl Pts',(-26.2151704830173,21.737977391402,8.42994634566487));
#45776=CARTESIAN_POINT('Ctrl Pts',(-26.211176526839,21.7321175098907,8.43038190532559));
#45777=CARTESIAN_POINT('Ctrl Pts',(-26.2090712026781,21.7290400948579,8.43061112163977));
#45778=CARTESIAN_POINT('Ctrl Pts',(-26.2034941193982,21.7209181883168,8.43121732921147));
#45779=CARTESIAN_POINT('Ctrl Pts',(-26.2000133271131,21.7158799444551,8.43159466476931));
#45780=CARTESIAN_POINT('Ctrl Pts',(-26.1841804382223,21.693101858592,8.43330648989124));
#45781=CARTESIAN_POINT('Ctrl Pts',(-26.1716646380853,21.6754769794784,8.4346472438909));
#45782=CARTESIAN_POINT('Ctrl Pts',(-26.0784938539611,21.5470301196691,8.44454003171268));
#45783=CARTESIAN_POINT('Ctrl Pts',(-25.9910301339395,21.441342860974,8.45336007573995));
#45784=CARTESIAN_POINT('Ctrl Pts',(-25.7904914470126,21.2282595232036,8.47266302867951));
#45785=CARTESIAN_POINT('Ctrl Pts',(-25.6758101730521,21.122842396553,8.48318726143137));
#45786=CARTESIAN_POINT('Ctrl Pts',(-25.4022050280378,20.9056468739201,8.50683113051343));
#45787=CARTESIAN_POINT('Ctrl Pts',(-25.2398577530878,20.7990854706112,8.51991124981041));
#45788=CARTESIAN_POINT('Ctrl Pts',(-25.0582822018522,20.7020760932013,8.53289124846135));
#45789=CARTESIAN_POINT('Ctrl Pts',(-25.0476313574047,20.6964622145755,8.53364685178423));
#45790=CARTESIAN_POINT('Ctrl Pts',(-25.033788490599,20.6892647108215,8.53462119685486));
#45791=CARTESIAN_POINT('Ctrl Pts',(-25.0306251358594,20.6876266033419,8.53484333365114));
#45792=CARTESIAN_POINT('Ctrl Pts',(-25.0257715123533,20.6851234062478,8.53518336127414));
#45793=CARTESIAN_POINT('Ctrl Pts',(-25.0240831974669,20.6842545665104,8.53530148992276));
#45794=CARTESIAN_POINT('Ctrl Pts',(-25.0207517340334,20.6825438527866,8.53553429237204));
#45795=CARTESIAN_POINT('Ctrl Pts',(-25.0191086385039,20.6817019031214,8.53564897039494));
#45796=CARTESIAN_POINT('Ctrl Pts',(-25.0154868842574,20.6798499833351,8.53590143583168));
#45797=CARTESIAN_POINT('Ctrl Pts',(-25.0135079094587,20.6788406495233,8.53603918238165));
#45798=CARTESIAN_POINT('Ctrl Pts',(-25.0078575332793,20.6759661542096,8.5364318996918));
#45799=CARTESIAN_POINT('Ctrl Pts',(-25.0041835813975,20.6741059736072,8.53668655527253));
#45800=CARTESIAN_POINT('Ctrl Pts',(-24.9959008938861,20.669932242565,8.53725911960972));
#45801=CARTESIAN_POINT('Ctrl Pts',(-24.9912901375239,20.6676226951524,8.53757677992103));
#45802=CARTESIAN_POINT('Ctrl Pts',(-24.8365450862406,20.5905743040348,8.54820280752068));
#45803=CARTESIAN_POINT('Ctrl Pts',(-24.6807853984301,20.5276449034363,8.55779448953633));
#45804=CARTESIAN_POINT('Ctrl Pts',(-24.265274285589,20.3964176513425,8.58231237733002));
#45805=CARTESIAN_POINT('Ctrl Pts',(-24.0006896542555,20.3479048898667,8.59698956182451));
#45806=CARTESIAN_POINT('Ctrl Pts',(-23.6607527554434,20.3285811978673,8.61704140567542));
#45807=CARTESIAN_POINT('Ctrl Pts',(-23.588237749468,20.326910732647,8.62137930249063));
#45808=CARTESIAN_POINT('Ctrl Pts',(-23.5061599636176,20.3277899570676,8.62637836573433));
#45809=CARTESIAN_POINT('Ctrl Pts',(-23.4965883816556,20.3279351427149,8.62696269641176));
#45810=CARTESIAN_POINT('Ctrl Pts',(-23.4826140401443,20.3282093916388,8.62781784007091));
#45811=CARTESIAN_POINT('Ctrl Pts',(-23.4782106103974,20.3283048407489,8.62808759734863));
#45812=CARTESIAN_POINT('Ctrl Pts',(-23.4704192602244,20.3284897072035,8.62856542719746));
#45813=CARTESIAN_POINT('Ctrl Pts',(-23.4670312523014,20.3285754425028,8.62877338383992));
#45814=CARTESIAN_POINT('Ctrl Pts',(-23.4600073482871,20.3287642731759,8.62920488015155));
#45815=CARTESIAN_POINT('Ctrl Pts',(-23.45637148044,20.3288681800618,8.62942844501741));
#45816=CARTESIAN_POINT('Ctrl Pts',(-23.4470234957408,20.3291511689531,8.63000376963261));
#45817=CARTESIAN_POINT('Ctrl Pts',(-23.4413116831125,20.3293392894981,8.63035581284039));
#45818=CARTESIAN_POINT('Ctrl Pts',(-23.4180849171385,20.3301661250665,8.63178946491573));
#45819=CARTESIAN_POINT('Ctrl Pts',(-23.4005750674499,20.3309325131727,8.63287507719618));
#45820=CARTESIAN_POINT('Ctrl Pts',(-23.2849027796125,20.3369410945609,8.64007962502133));
#45821=CARTESIAN_POINT('Ctrl Pts',(-23.1870273771757,20.3465289184664,8.64633458895748));
#45822=CARTESIAN_POINT('Ctrl Pts',(-22.9442757532686,20.3815755451505,8.66226263979204));
#45823=CARTESIAN_POINT('Ctrl Pts',(-22.8004224509638,20.4125035818414,8.67208178317791));
#45824=CARTESIAN_POINT('Ctrl Pts',(-22.4247137120696,20.5205970067321,8.69848196923771));
#45825=CARTESIAN_POINT('Ctrl Pts',(-22.1986323472732,20.6144741789378,8.71520291483597));
#45826=CARTESIAN_POINT('Ctrl Pts',(-21.9732195941979,20.7396875322024,8.73148739548046));
#45827=CARTESIAN_POINT('Ctrl Pts',(-21.9611830604198,20.7464753054924,8.73235550754247));
#45828=CARTESIAN_POINT('Ctrl Pts',(-21.9459696959232,20.7551840322618,8.73345054192751));
#45829=CARTESIAN_POINT('Ctrl Pts',(-21.9427522572708,20.7570332059469,8.73368200259418));
#45830=CARTESIAN_POINT('Ctrl Pts',(-21.9376632781504,20.7599697240406,8.73404789290686));
#45831=CARTESIAN_POINT('Ctrl Pts',(-21.9357896393625,20.761053396336,8.73418256014115));
#45832=CARTESIAN_POINT('Ctrl Pts',(-21.932303189376,20.7630745739325,8.73443306233311));
#45833=CARTESIAN_POINT('Ctrl Pts',(-21.9306901107767,20.7640115860252,8.73454892806822));
#45834=CARTESIAN_POINT('Ctrl Pts',(-21.9271278600629,20.7660849804494,8.73480472564117));
#45835=CARTESIAN_POINT('Ctrl Pts',(-21.9251790720987,20.7672220065192,8.73494461438896));
#45836=CARTESIAN_POINT('Ctrl Pts',(-21.9195385821656,20.7705209116245,8.73534936375295));
#45837=CARTESIAN_POINT('Ctrl Pts',(-21.915849970721,20.7726881068808,8.73561387819089));
#45838=CARTESIAN_POINT('Ctrl Pts',(-21.9075122120077,20.7776092075888,8.73621142320065));
#45839=CARTESIAN_POINT('Ctrl Pts',(-21.9028656393559,20.7803674819913,8.73654417314357));
#45840=CARTESIAN_POINT('Ctrl Pts',(-21.7851635559057,20.8506381287567,8.74496707679133));
#45841=CARTESIAN_POINT('Ctrl Pts',(-21.6763282589843,20.9250145735171,8.75261725830812));
#45842=CARTESIAN_POINT('Ctrl Pts',(-21.4161021337198,21.1273040292365,8.77135263853859));
#45843=CARTESIAN_POINT('Ctrl Pts',(-21.2713832610021,21.2628880171032,8.78221273123673));
#45844=CARTESIAN_POINT('Ctrl Pts',(-21.0239600428047,21.541639476319,8.80333313088229));
#45845=CARTESIAN_POINT('Ctrl Pts',(-20.9187560232081,21.6815918691193,8.81347876206296));
#45846=CARTESIAN_POINT('Ctrl Pts',(-20.8192870933154,21.8390899174721,8.82480664380453));
#45847=CARTESIAN_POINT('Ctrl Pts',(-20.8132006392869,21.8488423369251,8.82550763069144));
#45848=CARTESIAN_POINT('Ctrl Pts',(-20.8048345379281,21.8624085400167,8.82648220600942));
#45849=CARTESIAN_POINT('Ctrl Pts',(-20.8025103519581,21.8661948681583,8.82675415203712));
#45850=CARTESIAN_POINT('Ctrl Pts',(-20.798527471922,21.8727135679028,8.82722225106653));
#45851=CARTESIAN_POINT('Ctrl Pts',(-20.7968649952568,21.8754436310441,8.82741826478684));
#45852=CARTESIAN_POINT('Ctrl Pts',(-20.7934483524402,21.8810731633247,8.82782239894562));
#45853=CARTESIAN_POINT('Ctrl Pts',(-20.7916946933555,21.8839729336239,8.82803053761587));
#45854=CARTESIAN_POINT('Ctrl Pts',(-20.787633980049,21.8907115229573,8.82851414927054));
#45855=CARTESIAN_POINT('Ctrl Pts',(-20.7853303521335,21.8945523890889,8.82878974719933));
#45856=CARTESIAN_POINT('Ctrl Pts',(-20.7780573743829,21.906736218444,8.82966383295542));
#45857=CARTESIAN_POINT('Ctrl Pts',(-20.7731177580741,21.9150967874368,8.83026340426924));
#45858=CARTESIAN_POINT('Ctrl Pts',(-20.720347017574,22.0053430116168,8.83673316296633));
#45859=CARTESIAN_POINT('Ctrl Pts',(-20.6761192108494,22.0892716159403,8.84273293274057));
#45860=CARTESIAN_POINT('Ctrl Pts',(-20.6017547280566,22.2468758207101,8.85398636158182));
#45861=CARTESIAN_POINT('Ctrl Pts',(-20.5705215999902,22.3199549295507,8.85919905601402));
#45862=CARTESIAN_POINT('Ctrl Pts',(-20.4631811437182,22.5992496950615,8.87906949633699));
#45863=CARTESIAN_POINT('Ctrl Pts',(-20.4055360492379,22.8118997131531,8.89414297754651));
#45864=CARTESIAN_POINT('Ctrl Pts',(-20.3641774893267,23.0641170043646,8.91120121883877));
#45865=CARTESIAN_POINT('Ctrl Pts',(-20.3589683726862,23.0995780438729,8.91357979721791));
#45866=CARTESIAN_POINT('Ctrl Pts',(-20.3511411729773,23.1598357382444,8.91758088284595));
#45867=CARTESIAN_POINT('Ctrl Pts',(-20.3482174005271,23.1845889670626,8.91921288229018));
#45868=CARTESIAN_POINT('Ctrl Pts',(-20.3454023953977,23.2110534486138,8.92094368399854));
#45869=CARTESIAN_POINT('Ctrl Pts',(-20.3452251006871,23.212732783229,8.92105345381956));
#45870=CARTESIAN_POINT('Ctrl Pts',(-20.344802576429,23.2167652841061,8.92131689274395));
#45871=CARTESIAN_POINT('Ctrl Pts',(-20.3445586178114,23.2191185851347,8.9214705121963));
#45872=CARTESIAN_POINT('Ctrl Pts',(-20.3435525047375,23.2289291871993,8.92211042915794));
#45873=CARTESIAN_POINT('Ctrl Pts',(-20.3428137722328,23.2363889292139,8.92259579686318));
#45874=CARTESIAN_POINT('Ctrl Pts',(-20.3415001094199,23.2501435363502,8.92348843094332));
#45875=CARTESIAN_POINT('Ctrl Pts',(-20.340917659632,23.2564376294363,8.92389600906343));
#45876=CARTESIAN_POINT('Ctrl Pts',(-20.3369194552409,23.3010740801043,8.92677997508019));
#45877=CARTESIAN_POINT('Ctrl Pts',(-20.33417220573,23.3394753354339,8.92922713301581));
#45878=CARTESIAN_POINT('Ctrl Pts',(-20.3318598540093,23.3826558721342,8.93193391128876));
#45879=CARTESIAN_POINT('Ctrl Pts',(-20.3316166307622,23.3873936787359,8.93223029414352));
#45880=CARTESIAN_POINT('Ctrl Pts',(-20.3312659602958,23.39453229923,8.9326759322857));
#45881=CARTESIAN_POINT('Ctrl Pts',(-20.3311507367227,23.39693269819,8.93282562168555));
#45882=CARTESIAN_POINT('Ctrl Pts',(-20.3309557573381,23.4010917450178,8.93308470301539));
#45883=CARTESIAN_POINT('Ctrl Pts',(-20.3308747575987,23.4028503290115,8.93319416524176));
#45884=CARTESIAN_POINT('Ctrl Pts',(-20.3307089210712,23.4065161530836,8.93342216217588));
#45885=CARTESIAN_POINT('Ctrl Pts',(-20.3306243381385,23.4084234002739,8.93354068191174));
#45886=CARTESIAN_POINT('Ctrl Pts',(-20.3304295532102,23.412905555037,8.93381897341616));
#45887=CARTESIAN_POINT('Ctrl Pts',(-20.3303207448092,23.4154805290788,8.9339786662154));
#45888=CARTESIAN_POINT('Ctrl Pts',(-20.3299740024239,23.4239264424841,8.93450186251004));
#45889=CARTESIAN_POINT('Ctrl Pts',(-20.3297490336311,23.4297979462816,8.93486463823999));
#45890=CARTESIAN_POINT('Ctrl Pts',(-20.3292552953519,23.443676067056,8.9357199466054));
#45891=CARTESIAN_POINT('Ctrl Pts',(-20.3290003178443,23.451683179193,8.9362117239065));
#45892=CARTESIAN_POINT('Ctrl Pts',(-20.3282114851183,23.4797438127093,8.9379294396505));
#45893=CARTESIAN_POINT('Ctrl Pts',(-20.3278349996217,23.4998017646356,8.93914707761374));
#45894=CARTESIAN_POINT('Ctrl Pts',(-20.3269513763952,23.5935025225187,8.94479307487094));
#45895=CARTESIAN_POINT('Ctrl Pts',(-20.328781217753,23.6671505896015,8.94910922140287));
#45896=CARTESIAN_POINT('Ctrl Pts',(-20.3431630548736,23.9101244776603,8.96313349192628));
#45897=CARTESIAN_POINT('Ctrl Pts',(-20.3665650246052,24.0785245548232,8.9725183703753));
#45898=CARTESIAN_POINT('Ctrl Pts',(-20.4528670545767,24.4698542624448,8.99495730131921));
#45899=CARTESIAN_POINT('Ctrl Pts',(-20.5267008692826,24.6893645924753,9.00808771556767));
#45900=CARTESIAN_POINT('Ctrl Pts',(-20.62966139205,24.9127841752777,9.02301244191091));
#45901=CARTESIAN_POINT('Ctrl Pts',(-20.6360705147369,24.9264386545291,9.02393082670351));
#45902=CARTESIAN_POINT('Ctrl Pts',(-20.6449621336223,24.9450413695093,9.02519076542979));
#45903=CARTESIAN_POINT('Ctrl Pts',(-20.6473619439125,24.9500290974311,9.02552944187062));
#45904=CARTESIAN_POINT('Ctrl Pts',(-20.6511859265764,24.957924675826,9.02606694694528));
#45905=CARTESIAN_POINT('Ctrl Pts',(-20.6526016600799,24.9608366207804,9.02626548090226));
#45906=CARTESIAN_POINT('Ctrl Pts',(-20.6553524068347,24.9664728654275,9.0266503356672));
#45907=CARTESIAN_POINT('Ctrl Pts',(-20.6566868839321,24.9691974244169,9.02683663758455));
#45908=CARTESIAN_POINT('Ctrl Pts',(-20.6598688605097,24.9756708081405,9.02727990780957));
#45909=CARTESIAN_POINT('Ctrl Pts',(-20.6617198056478,24.979417924423,9.02753699657255));
#45910=CARTESIAN_POINT('Ctrl Pts',(-20.667223064191,24.9905045443085,9.02829914137707));
#45911=CARTESIAN_POINT('Ctrl Pts',(-20.6708960794395,24.9978336828562,9.02880492336293));
#45912=CARTESIAN_POINT('Ctrl Pts',(-20.6960228492536,25.047497664181,9.03224554843079));
#45913=CARTESIAN_POINT('Ctrl Pts',(-20.7183805930161,25.0893662381444,9.03521216815063));
#45914=CARTESIAN_POINT('Ctrl Pts',(-20.7714507153635,25.1836752280068,9.04205152337455));
#45915=CARTESIAN_POINT('Ctrl Pts',(-20.8027374357924,25.2357700344135,9.04594390233056));
#45916=CARTESIAN_POINT('Ctrl Pts',(-20.9074073886994,25.3993886460025,9.05854229728576));
#45917=CARTESIAN_POINT('Ctrl Pts',(-20.9862477809929,25.5072420912258,9.06742710590673));
#45918=CARTESIAN_POINT('Ctrl Pts',(-21.1592741939436,25.7154744482687,9.08566943292162));
#45919=CARTESIAN_POINT('Ctrl Pts',(-21.2536650885101,25.8153462457989,9.09501476061617));
#45920=CARTESIAN_POINT('Ctrl Pts',(-21.4297181053238,25.9792680245846,9.11114700274104));
#45921=CARTESIAN_POINT('Ctrl Pts',(-21.5086460282935,26.0459747613417,9.11798293101955));
#45922=CARTESIAN_POINT('Ctrl Pts',(-21.5947116745465,26.1118933566586,9.12492645203125));
#45923=CARTESIAN_POINT('Ctrl Pts',(-21.5987825567572,26.1149959297272,9.12525372475191));
#45924=CARTESIAN_POINT('Ctrl Pts',(-21.6068881186365,26.1211430131538,9.12590304209541));
#45925=CARTESIAN_POINT('Ctrl Pts',(-21.6109226050256,26.1241877573518,9.12622510016796));
#45926=CARTESIAN_POINT('Ctrl Pts',(-21.622236967678,26.1326847709488,9.1271250732373));
#45927=CARTESIAN_POINT('Ctrl Pts',(-21.6295328542827,26.1381157836098,9.12770169975395));
#45928=CARTESIAN_POINT('Ctrl Pts',(-21.6483735634865,26.1520171205858,9.12918104452008));
#45929=CARTESIAN_POINT('Ctrl Pts',(-21.6599521811021,26.1604416414096,9.13008085183502));
#45930=CARTESIAN_POINT('Ctrl Pts',(-21.6746424553593,26.1709811607204,9.13121034954066));
#45931=CARTESIAN_POINT('Ctrl Pts',(-21.677701947236,26.173168087795,9.13144492684119));
#45932=CARTESIAN_POINT('Ctrl Pts',(-21.6825377587891,26.1766119558075,9.13181464950696));
#45933=CARTESIAN_POINT('Ctrl Pts',(-21.6843115231953,26.1778724529207,9.13195004081434));
#45934=CARTESIAN_POINT('Ctrl Pts',(-21.6876076399254,26.1802097645628,9.1322012189221));
#45935=CARTESIAN_POINT('Ctrl Pts',(-21.689129640812,26.1812870477386,9.13231703793973));
#45936=CARTESIAN_POINT('Ctrl Pts',(-21.6921150151896,26.1833962304841,9.13254389405364));
#45937=CARTESIAN_POINT('Ctrl Pts',(-21.6935783069382,26.1844282266476,9.13265493782859));
#45938=CARTESIAN_POINT('Ctrl Pts',(-21.6980164630672,26.1875527301812,9.13299127944001));
#45939=CARTESIAN_POINT('Ctrl Pts',(-21.7009940234705,26.1896414308401,9.13321631414353));
#45940=CARTESIAN_POINT('Ctrl Pts',(-21.7158933737338,26.200055445365,9.13433931497765));
#45941=CARTESIAN_POINT('Ctrl Pts',(-21.7278681252211,26.2083052203341,9.13523215373943));
#45942=CARTESIAN_POINT('Ctrl Pts',(-21.7611327274915,26.2308917566385,9.13768681693809));
#45943=CARTESIAN_POINT('Ctrl Pts',(-21.7825391144246,26.2450559929775,9.13923778613895));
#45944=CARTESIAN_POINT('Ctrl Pts',(-21.8573049716843,26.2932529430453,9.14456475083909));
#45945=CARTESIAN_POINT('Ctrl Pts',(-21.9114987972983,26.3259704455679,9.14826928343459));
#45946=CARTESIAN_POINT('Ctrl Pts',(-22.0023926632846,26.3772534202516,9.15428783567698));
#45947=CARTESIAN_POINT('Ctrl Pts',(-22.0385366392128,26.396744753782,9.15663222934342));
#45948=CARTESIAN_POINT('Ctrl Pts',(-22.0750360476606,26.4155367911937,9.15896072794325));
#45949=CARTESIAN_POINT('Origin',(-23.5502525316942,23.5502525316942,-77.3107734492734));
#45950=CARTESIAN_POINT('',(-22.0750358939633,26.4155367120613,10.654266819213));
#45951=CARTESIAN_POINT('',(-22.0750360597002,26.4155367973924,10.4044010236784));
#45952=CARTESIAN_POINT('',(-22.0750360153461,26.4155367745563,-77.3107734492734));
#45953=CARTESIAN_POINT('Ctrl Pts',(-22.0750358939633,26.4155367120613,10.654266819213));
#45954=CARTESIAN_POINT('Ctrl Pts',(-22.0114257619618,26.3827864788733,10.6502545497521));
#45955=CARTESIAN_POINT('Ctrl Pts',(-21.9489028433,26.3479162601968,10.6462204514863));
#45956=CARTESIAN_POINT('Ctrl Pts',(-21.7940114567944,26.254631177202,10.6359072392353));
#45957=CARTESIAN_POINT('Ctrl Pts',(-21.7033824925041,26.1935675377572,10.6295707120918));
#45958=CARTESIAN_POINT('Ctrl Pts',(-21.5902202490526,26.1086568165435,10.6211405043412));
#45959=CARTESIAN_POINT('Ctrl Pts',(-21.5647001786132,26.0889019312882,10.6192033802087));
#45960=CARTESIAN_POINT('Ctrl Pts',(-21.523722684736,26.0561856903716,10.6160313122216));
#45961=CARTESIAN_POINT('Ctrl Pts',(-21.5080823489127,26.0434563204302,10.6148056110686));
#45962=CARTESIAN_POINT('Ctrl Pts',(-21.489154345466,26.0277535795707,10.6133034700161));
#45963=CARTESIAN_POINT('Ctrl Pts',(-21.4857517589214,26.0249189202029,10.6130326893305));
#45964=CARTESIAN_POINT('Ctrl Pts',(-21.4791743948838,26.0194163801552,10.6125077990431));
#45965=CARTESIAN_POINT('Ctrl Pts',(-21.4759989010499,26.0167493662398,10.612253725194));
#45966=CARTESIAN_POINT('Ctrl Pts',(-21.4705125267413,26.0121234161849,10.6118136054193));
#45967=CARTESIAN_POINT('Ctrl Pts',(-21.4681992390471,26.0101673323693,10.6116276769055));
#45968=CARTESIAN_POINT('Ctrl Pts',(-21.4634088909582,26.006105082929,10.6112419172777));
#45969=CARTESIAN_POINT('Ctrl Pts',(-21.4609322537915,26.003998425323,10.6110420659906));
#45970=CARTESIAN_POINT('Ctrl Pts',(-21.4549243359952,25.9988723269709,10.6105562563182));
#45971=CARTESIAN_POINT('Ctrl Pts',(-21.4513963959832,25.9958489969248,10.6102701372146));
#45972=CARTESIAN_POINT('Ctrl Pts',(-21.4381941979904,25.9844855334559,10.6091962446419));
#45973=CARTESIAN_POINT('Ctrl Pts',(-21.4285631125958,25.9760956249652,10.6084064053043));
#45974=CARTESIAN_POINT('Ctrl Pts',(-21.2720213498002,25.8380823371557,10.5954620358419));
#45975=CARTESIAN_POINT('Ctrl Pts',(-21.1372096571707,25.6954101369374,10.582734209057));
#45976=CARTESIAN_POINT('Ctrl Pts',(-20.9375838045897,25.4413556448599,10.5611284261831));
#45977=CARTESIAN_POINT('Ctrl Pts',(-20.8649630958745,25.3367371920506,10.5524922414885));
#45978=CARTESIAN_POINT('Ctrl Pts',(-20.7425704366555,25.1360237728624,10.5365987895456));
#45979=CARTESIAN_POINT('Ctrl Pts',(-20.6910749559801,25.0411769222699,10.5293431070927));
#45980=CARTESIAN_POINT('Ctrl Pts',(-20.6219162681521,24.8969799213987,10.5188410400439));
#45981=CARTESIAN_POINT('Ctrl Pts',(-20.6005418495196,24.8494967375762,10.5154642906458));
#45982=CARTESIAN_POINT('Ctrl Pts',(-20.5707495865267,24.7787834168032,10.5105757266236));
#45983=CARTESIAN_POINT('Ctrl Pts',(-20.5614339986934,24.755943123412,10.5090178694784));
#45984=CARTESIAN_POINT('Ctrl Pts',(-20.5507650317147,24.7289007801116,10.5072001162085));
#45985=CARTESIAN_POINT('Ctrl Pts',(-20.5491572269697,24.724800925138,10.5069252481421));
#45986=CARTESIAN_POINT('Ctrl Pts',(-20.5467183196721,24.7185440804105,10.5065068782936));
#45987=CARTESIAN_POINT('Ctrl Pts',(-20.5458811338398,24.7163894916712,10.5063630100716));
#45988=CARTESIAN_POINT('Ctrl Pts',(-20.5444368746334,24.712660654956,10.5061143735594));
#45989=CARTESIAN_POINT('Ctrl Pts',(-20.5438287204809,24.7110868336834,10.5060095396303));
#45990=CARTESIAN_POINT('Ctrl Pts',(-20.5425633519946,24.7078045657263,10.5057911286985));
#45991=CARTESIAN_POINT('Ctrl Pts',(-20.5419063590794,24.7060960413995,10.5056775653676));
#45992=CARTESIAN_POINT('Ctrl Pts',(-20.5400962701562,24.7013768678209,10.5053642348629));
#45993=CARTESIAN_POINT('Ctrl Pts',(-20.5389462314829,24.6983650360352,10.5051646529751));
#45994=CARTESIAN_POINT('Ctrl Pts',(-20.5344698902678,24.6865889686323,10.5043858022915));
#45995=CARTESIAN_POINT('Ctrl Pts',(-20.5311772714137,24.6778118499348,10.5038085443272));
#45996=CARTESIAN_POINT('Ctrl Pts',(-20.4727357912453,24.5199333252625,10.4934811947188));
#45997=CARTESIAN_POINT('Ctrl Pts',(-20.4286469599481,24.3669434021449,10.4843658988429));
#45998=CARTESIAN_POINT('Ctrl Pts',(-20.3562213934687,24.0213626631628,10.4644697182507));
#45999=CARTESIAN_POINT('Ctrl Pts',(-20.333652696768,23.8282186381666,10.4537889030883));
#46000=CARTESIAN_POINT('Ctrl Pts',(-20.3268080151372,23.5655940228441,10.4387890688568));
#46001=CARTESIAN_POINT('Ctrl Pts',(-20.3272126179922,23.4969344207244,10.4348267912876));
#46002=CARTESIAN_POINT('Ctrl Pts',(-20.3329812388142,23.3445468624452,10.4258897661041));
#46003=CARTESIAN_POINT('Ctrl Pts',(-20.3394223980521,23.2609130363562,10.4208883753321));
#46004=CARTESIAN_POINT('Ctrl Pts',(-20.3502098835418,23.1682394387018,10.4152060518849));
#46005=CARTESIAN_POINT('Ctrl Pts',(-20.3513443664597,23.1588531185484,10.4146289309233));
#46006=CARTESIAN_POINT('Ctrl Pts',(-20.3530771800223,23.1450274116994,10.4137764576133));
#46007=CARTESIAN_POINT('Ctrl Pts',(-20.353643496555,23.1405840030539,10.4135021184168));
#46008=CARTESIAN_POINT('Ctrl Pts',(-20.3546545144712,23.1327811452749,10.4130197179599));
#46009=CARTESIAN_POINT('Ctrl Pts',(-20.3550952552011,23.1294211824709,10.4128117823883));
#46010=CARTESIAN_POINT('Ctrl Pts',(-20.3559619597076,23.1228937614821,10.4124074127174));
#46011=CARTESIAN_POINT('Ctrl Pts',(-20.3563873375099,23.1197262281837,10.4122109974007));
#46012=CARTESIAN_POINT('Ctrl Pts',(-20.3574151312657,23.1121582221753,10.4117412603311));
#46013=CARTESIAN_POINT('Ctrl Pts',(-20.3580219326808,23.1077583599547,10.4114677998048));
#46014=CARTESIAN_POINT('Ctrl Pts',(-20.3602310104389,23.0919815878221,10.4104859171206));
#46015=CARTESIAN_POINT('Ctrl Pts',(-20.3618850126717,23.0806121137342,10.4097758562915));
#46016=CARTESIAN_POINT('Ctrl Pts',(-20.3895962383634,22.8970239055613,10.3982695513132));
#46017=CARTESIAN_POINT('Ctrl Pts',(-20.4295073432051,22.7272172173318,10.38702438803));
#46018=CARTESIAN_POINT('Ctrl Pts',(-20.5412161608102,22.3806766398056,10.3628257654625));
#46019=CARTESIAN_POINT('Ctrl Pts',(-20.6153739913148,22.2053776362976,10.3498535004855));
#46020=CARTESIAN_POINT('Ctrl Pts',(-20.7365298597034,21.97744274913,10.3325035214382));
#46021=CARTESIAN_POINT('Ctrl Pts',(-20.7704337078204,21.9182678161164,10.3279549295725));
#46022=CARTESIAN_POINT('Ctrl Pts',(-20.8336434631589,21.8156363734818,10.3200375580268));
#46023=CARTESIAN_POINT('Ctrl Pts',(-20.8621799214616,21.7717350648642,10.3166413105595));
#46024=CARTESIAN_POINT('Ctrl Pts',(-20.9058419357566,21.7080176253605,10.3117195270083));
#46025=CARTESIAN_POINT('Ctrl Pts',(-20.9201466564327,21.6876521914295,10.3101476002546));
#46026=CARTESIAN_POINT('Ctrl Pts',(-20.9372645344425,21.6638721980407,10.3083154756052));
#46027=CARTESIAN_POINT('Ctrl Pts',(-20.9398500684273,21.6602959138588,10.3080400320711));
#46028=CARTESIAN_POINT('Ctrl Pts',(-20.9438022321421,21.6548529034997,10.3076209668129));
#46029=CARTESIAN_POINT('Ctrl Pts',(-20.9451635263834,21.6529823376826,10.3074769767847));
#46030=CARTESIAN_POINT('Ctrl Pts',(-20.9475212474141,21.6497498950566,10.3072282039678));
#46031=CARTESIAN_POINT('Ctrl Pts',(-20.9485167279467,21.648387337317,10.3071233553186));
#46032=CARTESIAN_POINT('Ctrl Pts',(-20.950593751073,21.6455491075006,10.3069049866252));
#46033=CARTESIAN_POINT('Ctrl Pts',(-20.9516754771229,21.6440735785812,10.3067914801412));
#46034=CARTESIAN_POINT('Ctrl Pts',(-20.9546640801672,21.6400042450146,10.3064784907316));
#46035=CARTESIAN_POINT('Ctrl Pts',(-20.9565735948042,21.6374123661259,10.3062791924051));
#46036=CARTESIAN_POINT('Ctrl Pts',(-20.9640392731625,21.6273105633977,10.3055026223818));
#46037=CARTESIAN_POINT('Ctrl Pts',(-20.9696242672262,21.6198218549372,10.3049273466287));
#46038=CARTESIAN_POINT('Ctrl Pts',(-20.9806359710058,21.6051898683726,10.3038039150716));
#46039=CARTESIAN_POINT('Ctrl Pts',(-20.9860600902259,21.598044765948,10.303255595879));
#46040=CARTESIAN_POINT('Ctrl Pts',(-20.9958737552024,21.585228854682,10.3022724061693));
#46041=CARTESIAN_POINT('Ctrl Pts',(-21.0002525002768,21.579549909055,10.3018368489219));
#46042=CARTESIAN_POINT('Ctrl Pts',(-21.0068949163627,21.5709943370716,10.3011807508338));
#46043=CARTESIAN_POINT('Ctrl Pts',(-21.0091445597129,21.5681069176129,10.3009593394347));
#46044=CARTESIAN_POINT('Ctrl Pts',(-21.0150167204617,21.5605964209167,10.3003834449727));
#46045=CARTESIAN_POINT('Ctrl Pts',(-21.0186469832641,21.5559793794029,10.3000294374425));
#46046=CARTESIAN_POINT('Ctrl Pts',(-21.0862149276822,21.4705269178776,10.2934772930075));
#46047=CARTESIAN_POINT('Ctrl Pts',(-21.1539878458718,21.3927865160274,10.2875131148611));
#46048=CARTESIAN_POINT('Ctrl Pts',(-21.4006912620173,21.1357980347168,10.2672566247874));
#46049=CARTESIAN_POINT('Ctrl Pts',(-21.5969093008709,20.9744691217061,10.2534829997442));
#46050=CARTESIAN_POINT('Ctrl Pts',(-21.9035343671022,20.7777465943858,10.2324731251937));
#46051=CARTESIAN_POINT('Ctrl Pts',(-22.0001110944063,20.7226161775626,10.2259314646765));
#46052=CARTESIAN_POINT('Ctrl Pts',(-22.1162429256501,20.6640625582583,10.2180580565959));
#46053=CARTESIAN_POINT('Ctrl Pts',(-22.1332253066132,20.6556869455438,10.2169066355041));
#46054=CARTESIAN_POINT('Ctrl Pts',(-22.1555765708045,20.6449072677921,10.2153907782825));
#46055=CARTESIAN_POINT('Ctrl Pts',(-22.1608798611912,20.6423674376616,10.2150310798906));
#46056=CARTESIAN_POINT('Ctrl Pts',(-22.1695079920747,20.6382642801293,10.2144458116799));
#46057=CARTESIAN_POINT('Ctrl Pts',(-22.1728286237614,20.6366920915078,10.2142205501462));
#46058=CARTESIAN_POINT('Ctrl Pts',(-22.1792061605115,20.6336859180934,10.2137878864309));
#46059=CARTESIAN_POINT('Ctrl Pts',(-22.1822626466146,20.632251051625,10.2135805151857));
#46060=CARTESIAN_POINT('Ctrl Pts',(-22.1892377034797,20.6289899809911,10.2131072495706));
#46061=CARTESIAN_POINT('Ctrl Pts',(-22.1931576992186,20.6271668558822,10.212841249019));
#46062=CARTESIAN_POINT('Ctrl Pts',(-22.2034922323319,20.6223857049983,10.2121399044396));
#46063=CARTESIAN_POINT('Ctrl Pts',(-22.2099128208876,20.6194408835042,10.2117041050797));
#46064=CARTESIAN_POINT('Ctrl Pts',(-22.2421092348739,20.6048018316161,10.2095183568531));
#46065=CARTESIAN_POINT('Ctrl Pts',(-22.2680280021833,20.5934267192576,10.2077574657655));
#46066=CARTESIAN_POINT('Ctrl Pts',(-22.3004193763429,20.5797169157814,10.2055545629359));
#46067=CARTESIAN_POINT('Ctrl Pts',(-22.3067546731726,20.5770593263517,10.2051236000609));
#46068=CARTESIAN_POINT('Ctrl Pts',(-22.3223284931955,20.5705847586318,10.2040639066434));
#46069=CARTESIAN_POINT('Ctrl Pts',(-22.3315763245823,20.5667904855561,10.2034344182222));
#46070=CARTESIAN_POINT('Ctrl Pts',(-22.3424212431676,20.5623997834269,10.2026959256665));
#46071=CARTESIAN_POINT('Ctrl Pts',(-22.344001415514,20.5617614891163,10.2025883154505));
#46072=CARTESIAN_POINT('Ctrl Pts',(-22.3520531968881,20.5585164816259,10.202039949513));
#46073=CARTESIAN_POINT('Ctrl Pts',(-22.3585327135207,20.5559295509595,10.2015985401792));
#46074=CARTESIAN_POINT('Ctrl Pts',(-22.369381088894,20.551639154394,10.2008592968982));
#46075=CARTESIAN_POINT('Ctrl Pts',(-22.3737453790911,20.5499241379266,10.200561843267));
#46076=CARTESIAN_POINT('Ctrl Pts',(-22.3818541167625,20.5467580947328,10.2000090749873));
#46077=CARTESIAN_POINT('Ctrl Pts',(-22.3855975682215,20.5453045280342,10.1997538436161));
#46078=CARTESIAN_POINT('Ctrl Pts',(-22.3934838613298,20.5422592633436,10.1992160600866));
#46079=CARTESIAN_POINT('Ctrl Pts',(-22.3976272908432,20.5406691198213,10.1989334583733));
#46080=CARTESIAN_POINT('Ctrl Pts',(-22.4194085767439,20.5323615910385,10.1974475934335));
#46081=CARTESIAN_POINT('Ctrl Pts',(-22.4371016226992,20.5257907927492,10.1962396616554));
#46082=CARTESIAN_POINT('Ctrl Pts',(-22.6876737035053,20.4352305177069,10.1791189968194));
#46083=CARTESIAN_POINT('Ctrl Pts',(-22.9293859952176,20.3782040254862,10.1623413343034));
#46084=CARTESIAN_POINT('Ctrl Pts',(-23.3477256878194,20.329184764327,10.1338716710516));
#46085=CARTESIAN_POINT('Ctrl Pts',(-23.5216374532977,20.3229484006228,10.1222281043836));
#46086=CARTESIAN_POINT('Ctrl Pts',(-23.7057518442876,20.3312389254891,10.1106262390037));
#46087=CARTESIAN_POINT('Ctrl Pts',(-23.7162779684177,20.3317646577276,10.1099655106216));
#46088=CARTESIAN_POINT('Ctrl Pts',(-23.7300364661536,20.3325195104608,10.1091054121356));
#46089=CARTESIAN_POINT('Ctrl Pts',(-23.7332711827749,20.3327018743458,10.1089034521207));
#46090=CARTESIAN_POINT('Ctrl Pts',(-23.7385541177961,20.3330077033492,10.1085740339224));
#46091=CARTESIAN_POINT('Ctrl Pts',(-23.7406024929208,20.3331282466908,10.108446410986));
#46092=CARTESIAN_POINT('Ctrl Pts',(-23.7445334602574,20.3333633448335,10.1082016951737));
#46093=CARTESIAN_POINT('Ctrl Pts',(-23.74641606143,20.3334775956192,10.108084585721));
#46094=CARTESIAN_POINT('Ctrl Pts',(-23.7507429565837,20.333743997628,10.1078156283359));
#46095=CARTESIAN_POINT('Ctrl Pts',(-23.7531871840994,20.3338972827919,10.1076638448003));
#46096=CARTESIAN_POINT('Ctrl Pts',(-23.7609361739919,20.3343921145731,10.1071831054818));
#46097=CARTESIAN_POINT('Ctrl Pts',(-23.7662403024047,20.3347440021768,10.1068547315709));
#46098=CARTESIAN_POINT('Ctrl Pts',(-23.8111664751135,20.33783616893,10.1040790441649));
#46099=CARTESIAN_POINT('Ctrl Pts',(-23.8507377936744,20.3412957022526,10.1016714458111));
#46100=CARTESIAN_POINT('Ctrl Pts',(-23.8975977524443,20.3462669438034,10.0988539573671));
#46101=CARTESIAN_POINT('Ctrl Pts',(-23.9049556469169,20.3470731655292,10.0984125431298));
#46102=CARTESIAN_POINT('Ctrl Pts',(-23.9222045231954,20.3490233277439,10.0973799233608));
#46103=CARTESIAN_POINT('Ctrl Pts',(-23.9320931583028,20.350187776004,10.0967896087591));
#46104=CARTESIAN_POINT('Ctrl Pts',(-23.9462925932158,20.3519266037289,10.0959441649481));
#46105=CARTESIAN_POINT('Ctrl Pts',(-23.950607782581,20.352463898078,10.0956875291792));
#46106=CARTESIAN_POINT('Ctrl Pts',(-23.9636768159073,20.3541180225896,10.0949111329689));
#46107=CARTESIAN_POINT('Ctrl Pts',(-23.9724272322403,20.3552620834845,10.0943924553257));
#46108=CARTESIAN_POINT('Ctrl Pts',(-24.2645182163729,20.3946720490982,10.0771144231299));
#46109=CARTESIAN_POINT('Ctrl Pts',(-24.5415387855318,20.4704392189449,10.0617399871382));
#46110=CARTESIAN_POINT('Ctrl Pts',(-24.9053432699292,20.624209768643,10.0392098355348));
#46111=CARTESIAN_POINT('Ctrl Pts',(-25.0035114582854,20.6717056306109,10.0328859065209));
#46112=CARTESIAN_POINT('Ctrl Pts',(-25.1420110045653,20.7476074887997,10.0234747490309));
#46113=CARTESIAN_POINT('Ctrl Pts',(-25.1843992732781,20.7721095727227,10.0205250264729));
#46114=CARTESIAN_POINT('Ctrl Pts',(-25.232928210657,20.8016561694468,10.0170604589054));
#46115=CARTESIAN_POINT('Ctrl Pts',(-25.2396300431923,20.8057702444406,10.0165800338997));
#46116=CARTESIAN_POINT('Ctrl Pts',(-25.2498396087567,20.8120891883154,10.0158451156775));
#46117=CARTESIAN_POINT('Ctrl Pts',(-25.2533582920892,20.8142763811775,10.0155912754888));
#46118=CARTESIAN_POINT('Ctrl Pts',(-25.2596869733633,20.8182271916611,10.0151337175826));
#46119=CARTESIAN_POINT('Ctrl Pts',(-25.2624984887638,20.8199883775664,10.0149300901455));
#46120=CARTESIAN_POINT('Ctrl Pts',(-25.2685326437524,20.8237812715702,10.0144922880063));
#46121=CARTESIAN_POINT('Ctrl Pts',(-25.2717544076802,20.8258143572158,10.0142580623582));
#46122=CARTESIAN_POINT('Ctrl Pts',(-25.2804517642747,20.8313243882109,10.0136244689582));
#46123=CARTESIAN_POINT('Ctrl Pts',(-25.2859204560128,20.8348121457983,10.0132246990771));
#46124=CARTESIAN_POINT('Ctrl Pts',(-25.3102268868345,20.8504174390503,10.011441662621));
#46125=CARTESIAN_POINT('Ctrl Pts',(-25.3289481597964,20.8627144240605,10.0100516972492));
#46126=CARTESIAN_POINT('Ctrl Pts',(-25.6287686291538,21.0641551222702,9.98751693373543));
#46127=CARTESIAN_POINT('Ctrl Pts',(-25.8783873431475,21.2962386195797,9.96449421718862));
#46128=CARTESIAN_POINT('Ctrl Pts',(-26.1829230411643,21.6849785310592,9.93122724731233));
#46129=CARTESIAN_POINT('Ctrl Pts',(-26.2696916598121,21.8139157066536,9.92091675488752));
#46130=CARTESIAN_POINT('Ctrl Pts',(-26.3496913552182,21.9536020425832,9.91083481968869));
#46131=CARTESIAN_POINT('Ctrl Pts',(-26.3525307550793,21.958590736279,9.91047614260217));
#46132=CARTESIAN_POINT('Ctrl Pts',(-26.3566146895984,21.9658108228871,9.90995906050701));
#46133=CARTESIAN_POINT('Ctrl Pts',(-26.3578699024113,21.9680361148658,9.90979996896176));
#46134=CARTESIAN_POINT('Ctrl Pts',(-26.3600520174968,21.9719154298777,9.90952311366748));
#46135=CARTESIAN_POINT('Ctrl Pts',(-26.3609801074187,21.9735687801054,9.90940527262999));
#46136=CARTESIAN_POINT('Ctrl Pts',(-26.3627764302843,21.9767754746579,9.90917701736984));
#46137=CARTESIAN_POINT('Ctrl Pts',(-26.3636448334625,21.9783287149812,9.90906659200037));
#46138=CARTESIAN_POINT('Ctrl Pts',(-26.3657185015278,21.9820449350017,9.90880271492932));
#46139=CARTESIAN_POINT('Ctrl Pts',(-26.3669225631973,21.9842085899916,9.90864934134456));
#46140=CARTESIAN_POINT('Ctrl Pts',(-26.3712315014598,21.9919726405366,9.90809990281217));
#46141=CARTESIAN_POINT('Ctrl Pts',(-26.3743222052459,21.9975809477329,9.90770474670204));
#46142=CARTESIAN_POINT('Ctrl Pts',(-26.4203057292261,22.0816129369644,9.90180915660264));
#46143=CARTESIAN_POINT('Ctrl Pts',(-26.4599389953425,22.1617872908641,9.89651202471771));
#46144=CARTESIAN_POINT('Ctrl Pts',(-26.6172348139953,22.5163982764757,9.87403292326879));
#46145=CARTESIAN_POINT('Ctrl Pts',(-26.6997830209683,22.8047857037683,9.85801234086306));
#46146=CARTESIAN_POINT('Ctrl Pts',(-26.7529737118501,23.1821444172696,9.83601893386724));
#46147=CARTESIAN_POINT('Ctrl Pts',(-26.7613478469282,23.2642598824024,9.83118364245458));
#46148=CARTESIAN_POINT('Ctrl Pts',(-26.7692477265032,23.389024671387,9.82370999942974));
#46149=CARTESIAN_POINT('Ctrl Pts',(-26.771094172069,23.4314949987661,9.8211439883325));
#46150=CARTESIAN_POINT('Ctrl Pts',(-26.7722797778683,23.4815816879287,9.81808809973317));
#46151=CARTESIAN_POINT('Ctrl Pts',(-26.7724326811429,23.4891759992756,9.81762395390833));
#46152=CARTESIAN_POINT('Ctrl Pts',(-26.7726259866295,23.5008227546305,9.81691087981366));
#46153=CARTESIAN_POINT('Ctrl Pts',(-26.7726855961948,23.5048748884383,9.81666255489299));
#46154=CARTESIAN_POINT('Ctrl Pts',(-26.7727804280571,23.5122697131915,9.81620895321523));
#46155=CARTESIAN_POINT('Ctrl Pts',(-26.7728180929389,23.5156123717067,9.81600375344587));
#46156=CARTESIAN_POINT('Ctrl Pts',(-26.7728883382005,23.5228452988839,9.81555938903561));
#46157=CARTESIAN_POINT('Ctrl Pts',(-26.7729190751632,23.526735576521,9.81532016682901));
#46158=CARTESIAN_POINT('Ctrl Pts',(-26.7729833958779,23.5372970219284,9.81467012266586));
#46159=CARTESIAN_POINT('Ctrl Pts',(-26.7730033093116,23.543968226646,9.81425887212319));
#46160=CARTESIAN_POINT('Ctrl Pts',(-26.772999057819,23.5793841912314,9.81207215828765));
#46161=CARTESIAN_POINT('Ctrl Pts',(-26.7726110314294,23.6081268620325,9.8102853094006));
#46162=CARTESIAN_POINT('Ctrl Pts',(-26.7636347353523,23.9420240309938,9.78938006149644));
#46163=CARTESIAN_POINT('Ctrl Pts',(-26.7121133467723,24.2444138632098,9.76878854226643));
#46164=CARTESIAN_POINT('Ctrl Pts',(-26.5724002238423,24.67980205695,9.73787743807381));
#46165=CARTESIAN_POINT('Ctrl Pts',(-26.5157169699548,24.8211928189896,9.72766593036809));
#46166=CARTESIAN_POINT('Ctrl Pts',(-26.4473820904776,24.9619097768698,9.71765261287181));
#46167=CARTESIAN_POINT('Ctrl Pts',(-26.4455059250084,24.9657537316819,9.71737920548148));
#46168=CARTESIAN_POINT('Ctrl Pts',(-26.4414195537452,24.9740839206039,9.71678699842042));
#46169=CARTESIAN_POINT('Ctrl Pts',(-26.4392065418069,24.9785687787576,9.71646834582569));
#46170=CARTESIAN_POINT('Ctrl Pts',(-26.4328808213499,24.9913135455803,9.71556338090899));
#46171=CARTESIAN_POINT('Ctrl Pts',(-26.4287430269699,24.9995610479356,9.71497842362775));
#46172=CARTESIAN_POINT('Ctrl Pts',(-26.4181478909131,25.0204550332429,9.7134984320716));
#46173=CARTESIAN_POINT('Ctrl Pts',(-26.4116421991446,25.033076990542,9.712606172948));
#46174=CARTESIAN_POINT('Ctrl Pts',(-26.4033136245163,25.0489766614569,9.7114848811479));
#46175=CARTESIAN_POINT('Ctrl Pts',(-26.4015682912596,25.0522944938585,9.71125104567565));
#46176=CARTESIAN_POINT('Ctrl Pts',(-26.3988020566558,25.0575308368223,9.71088223961336));
#46177=CARTESIAN_POINT('Ctrl Pts',(-26.3977850042356,25.0594513599331,9.71074702507237));
#46178=CARTESIAN_POINT('Ctrl Pts',(-26.3958916423835,25.0630179105632,9.7104960201257));
#46179=CARTESIAN_POINT('Ctrl Pts',(-26.3950158523741,25.0646641960494,9.71038019784211));
#46180=CARTESIAN_POINT('Ctrl Pts',(-26.3930607440312,25.0683316733856,9.71012226394974));
#46181=CARTESIAN_POINT('Ctrl Pts',(-26.3919807013475,25.0703524700029,9.70998019972637));
#46182=CARTESIAN_POINT('Ctrl Pts',(-26.3888215657474,25.0762481866551,9.70956589023506));
#46183=CARTESIAN_POINT('Ctrl Pts',(-26.3867366852842,25.0801200249835,9.70929401407809));
#46184=CARTESIAN_POINT('Ctrl Pts',(-26.3716782458132,25.1079485013646,9.70734134985502));
#46185=CARTESIAN_POINT('Ctrl Pts',(-26.3584087865055,25.1317449792265,9.70567918642833));
#46186=CARTESIAN_POINT('Ctrl Pts',(-26.316712698874,25.2043398000426,9.70062301898617));
#46187=CARTESIAN_POINT('Ctrl Pts',(-26.2873027030324,25.2525638215775,9.69728465467246));
#46188=CARTESIAN_POINT('Ctrl Pts',(-26.2122338981055,25.368675428995,9.6892346597337));
#46189=CARTESIAN_POINT('Ctrl Pts',(-26.1652281688687,25.4356465209913,9.68458071872071));
#46190=CARTESIAN_POINT('Ctrl Pts',(-25.914883504586,25.7649207650677,9.66126896494603));
#46191=CARTESIAN_POINT('Ctrl Pts',(-25.6744804934729,25.9964494213852,9.64318862987));
#46192=CARTESIAN_POINT('Ctrl Pts',(-25.38558494636,26.1994267563148,9.6218472952312));
#46193=CARTESIAN_POINT('Ctrl Pts',(-25.3680770605265,26.2114708792732,9.62055640143095));
#46194=CARTESIAN_POINT('Ctrl Pts',(-25.3451800488028,26.2268909392013,9.61887083718964));
#46195=CARTESIAN_POINT('Ctrl Pts',(-25.3398979747377,26.2304255006451,9.61848218098158));
#46196=CARTESIAN_POINT('Ctrl Pts',(-25.331457406695,26.2360375282145,9.61786140065487));
#46197=CARTESIAN_POINT('Ctrl Pts',(-25.3283056340829,26.2381251140822,9.61762965823046));
#46198=CARTESIAN_POINT('Ctrl Pts',(-25.3226311205042,26.2418692965731,9.61721253224171));
#46199=CARTESIAN_POINT('Ctrl Pts',(-25.3201097080586,26.2435279068128,9.61702722465354));
#46200=CARTESIAN_POINT('Ctrl Pts',(-25.3142032316264,26.2474013698149,9.61659322371564));
#46201=CARTESIAN_POINT('Ctrl Pts',(-25.3108163253293,26.2496133921706,9.61634442460059));
#46202=CARTESIAN_POINT('Ctrl Pts',(-25.3010864423463,26.2559419742088,9.61562986164836));
#46203=CARTESIAN_POINT('Ctrl Pts',(-25.2947331618613,26.260042573641,9.61516350215529));
#46204=CARTESIAN_POINT('Ctrl Pts',(-25.2538125784584,26.2862504043605,9.61216111373683));
#46205=CARTESIAN_POINT('Ctrl Pts',(-25.2188414917677,26.3077172773216,9.60960142432445));
#46206=CARTESIAN_POINT('Ctrl Pts',(-25.1135637650723,26.369605556149,9.60190955620714));
#46207=CARTESIAN_POINT('Ctrl Pts',(-25.0421354715868,26.4080448479951,9.5967079626743));
#46208=CARTESIAN_POINT('Ctrl Pts',(-24.7227494426512,26.5646845734089,9.57352002744865));
#46209=CARTESIAN_POINT('Ctrl Pts',(-24.4617236595673,26.6535948366625,9.55462346320315));
#46210=CARTESIAN_POINT('Ctrl Pts',(-24.1559165144712,26.7158005101852,9.53378972004817));
#46211=CARTESIAN_POINT('Ctrl Pts',(-24.1190527170591,26.7226316682266,9.53130149402064));
#46212=CARTESIAN_POINT('Ctrl Pts',(-24.0042287886528,26.7418435345227,9.52363828318648));
#46213=CARTESIAN_POINT('Ctrl Pts',(-23.9259202170361,26.7520057764936,9.51853574023417));
#46214=CARTESIAN_POINT('Ctrl Pts',(-23.841112123262,26.7598564022402,9.51319755999968));
#46215=CARTESIAN_POINT('Ctrl Pts',(-23.8349123370484,26.7604122013341,9.51280840040594));
#46216=CARTESIAN_POINT('Ctrl Pts',(-23.8262741035326,26.7611613807758,9.51226772227356));
#46217=CARTESIAN_POINT('Ctrl Pts',(-23.8238370391775,26.7613699482009,9.51211535421511));
#46218=CARTESIAN_POINT('Ctrl Pts',(-23.8196344810058,26.7617247900526,9.51185290293051));
#46219=CARTESIAN_POINT('Ctrl Pts',(-23.8178691044347,26.7618723832411,9.51174274501014));
#46220=CARTESIAN_POINT('Ctrl Pts',(-23.8142090889729,26.7621753377624,9.51151455216016));
#46221=CARTESIAN_POINT('Ctrl Pts',(-23.812314437244,26.7623304781249,9.51139653042299));
#46222=CARTESIAN_POINT('Ctrl Pts',(-23.8078956102732,26.762688370603,9.51112151564151));
#46223=CARTESIAN_POINT('Ctrl Pts',(-23.8053713244894,26.762889824747,9.51096459634618));
#46224=CARTESIAN_POINT('Ctrl Pts',(-23.7972069141976,26.7635317135134,9.5104576553628));
#46225=CARTESIAN_POINT('Ctrl Pts',(-23.7915658263767,26.7639602754556,9.51010830199799));
#46226=CARTESIAN_POINT('Ctrl Pts',(-23.7783149303232,26.7649318792744,9.50928974904194));
#46227=CARTESIAN_POINT('Ctrl Pts',(-23.7707042259364,26.7654627610039,9.5088212177828));
#46228=CARTESIAN_POINT('Ctrl Pts',(-23.6893193113883,26.7708494000177,9.5038274898316));
#46229=CARTESIAN_POINT('Ctrl Pts',(-23.615394105057,26.7731925380821,9.49943629577195));
#46230=CARTESIAN_POINT('Ctrl Pts',(-23.4108415405854,26.772633665587,9.48752610757906));
#46231=CARTESIAN_POINT('Ctrl Pts',(-23.2803685149324,26.7643376284446,9.48019701891813));
#46232=CARTESIAN_POINT('Ctrl Pts',(-23.0477836495362,26.7352816342032,9.46708939423936));
#46233=CARTESIAN_POINT('Ctrl Pts',(-22.9454983155951,26.7174527512905,9.46131017670366));
#46234=CARTESIAN_POINT('Ctrl Pts',(-22.6587915114503,26.6530810303466,9.44472931339738));
#46235=CARTESIAN_POINT('Ctrl Pts',(-22.4774063646374,26.5951223488322,9.43375869578466));
#46236=CARTESIAN_POINT('Ctrl Pts',(-22.2905968592045,26.5166549856943,9.42144609262112));
#46237=CARTESIAN_POINT('Ctrl Pts',(-22.2790231085889,26.5117136033821,9.42067909180608));
#46238=CARTESIAN_POINT('Ctrl Pts',(-22.2632430637916,26.5048668060765,9.41962751612401));
#46239=CARTESIAN_POINT('Ctrl Pts',(-22.259011375932,26.5030199045429,9.41934494356333));
#46240=CARTESIAN_POINT('Ctrl Pts',(-22.2518138150707,26.499860129613,9.41886333887613));
#46241=CARTESIAN_POINT('Ctrl Pts',(-22.2488459192774,26.4985518569952,9.41866446468593));
#46242=CARTESIAN_POINT('Ctrl Pts',(-22.2431076115636,26.4960120113952,9.41827939407669));
#46243=CARTESIAN_POINT('Ctrl Pts',(-22.2403369520721,26.49478100475,9.41809321730081));
#46244=CARTESIAN_POINT('Ctrl Pts',(-22.2337638973252,26.4918494769087,9.41765093720547));
#46245=CARTESIAN_POINT('Ctrl Pts',(-22.2299630606637,26.4901454931716,9.41739471496134));
#46246=CARTESIAN_POINT('Ctrl Pts',(-22.2187524443579,26.4850934463618,9.41663757146618));
#46247=CARTESIAN_POINT('Ctrl Pts',(-22.211352061066,26.4817247223849,9.41613593852285));
#46248=CARTESIAN_POINT('Ctrl Pts',(-22.1605252907426,26.458355287734,9.41267797581846));
#46249=CARTESIAN_POINT('Ctrl Pts',(-22.1175386100646,26.4374196051673,9.40968941864562));
#46250=CARTESIAN_POINT('Ctrl Pts',(-22.0750360149249,26.4155367743394,9.40666775021339));
#46251=CARTESIAN_POINT('',(-26.7730012638346,23.5531112005712,9.56507739177766));
#46252=CARTESIAN_POINT('Ctrl Pts',(-22.0750360476606,26.4155367911937,9.15896072794325));
#46253=CARTESIAN_POINT('Ctrl Pts',(-22.1583267955234,26.4584197560539,9.16427430419078));
#46254=CARTESIAN_POINT('Ctrl Pts',(-22.2434683747133,26.4976611756449,9.1695061070461));
#46255=CARTESIAN_POINT('Ctrl Pts',(-22.57608362442,26.6337040788026,9.18958538803959));
#46256=CARTESIAN_POINT('Ctrl Pts',(-22.8333933469615,26.7034675760865,9.2044842187267));
#46257=CARTESIAN_POINT('Ctrl Pts',(-23.1129501123843,26.7432395341934,9.22159733060522));
#46258=CARTESIAN_POINT('Ctrl Pts',(-23.1295888604008,26.7454741927175,9.22261880629557));
#46259=CARTESIAN_POINT('Ctrl Pts',(-23.1519838047304,26.7483039781564,9.22399783954222));
#46260=CARTESIAN_POINT('Ctrl Pts',(-23.1577254552396,26.7490137804679,9.22435176654865));
#46261=CARTESIAN_POINT('Ctrl Pts',(-23.1667329274327,26.7501026976941,9.22490759319267));
#46262=CARTESIAN_POINT('Ctrl Pts',(-23.1699974906551,26.7504922844842,9.22510916151078));
#46263=CARTESIAN_POINT('Ctrl Pts',(-23.1762626754245,26.7512302378049,9.22549623556743));
#46264=CARTESIAN_POINT('Ctrl Pts',(-23.1792632034328,26.7515793825214,9.22568171650463));
#46265=CARTESIAN_POINT('Ctrl Pts',(-23.1863085179171,26.7523891449319,9.22611747435042));
#46266=CARTESIAN_POINT('Ctrl Pts',(-23.1903536882655,26.7528463175589,9.22636785981343));
#46267=CARTESIAN_POINT('Ctrl Pts',(-23.2020340293893,26.7541439842134,9.22709139299253));
#46268=CARTESIAN_POINT('Ctrl Pts',(-23.2096713138245,26.7549648428495,9.22756515993356));
#46269=CARTESIAN_POINT('Ctrl Pts',(-23.2605051331313,26.7602447174578,9.2307231579031));
#46270=CARTESIAN_POINT('Ctrl Pts',(-23.303783312234,26.7638573633208,9.23343395980405));
#46271=CARTESIAN_POINT('Ctrl Pts',(-23.4523087600109,26.7732377112293,9.24281871401772));
#46272=CARTESIAN_POINT('Ctrl Pts',(-23.55774979958,26.7747162467735,9.24962397153464));
#46273=CARTESIAN_POINT('Ctrl Pts',(-23.6889733090509,26.7701199471366,9.25826571057158));
#46274=CARTESIAN_POINT('Ctrl Pts',(-23.7148692590524,26.7688999047676,9.25997929072323));
#46275=CARTESIAN_POINT('Ctrl Pts',(-23.90126398205,26.7578629343217,9.2723693790412));
#46276=CARTESIAN_POINT('Ctrl Pts',(-24.0608367894398,26.7363585528252,9.28329211165587));
#46277=CARTESIAN_POINT('Ctrl Pts',(-24.3627835287042,26.6723953187608,9.30414990529683));
#46278=CARTESIAN_POINT('Ctrl Pts',(-24.5051758802602,26.6318288746371,9.31406585226229));
#46279=CARTESIAN_POINT('Ctrl Pts',(-24.6486747983109,26.5800392911524,9.3238353675773));
#46280=CARTESIAN_POINT('Ctrl Pts',(-24.6530552117312,26.5784476266389,9.32413336148684));
#46281=CARTESIAN_POINT('Ctrl Pts',(-24.6623287805766,26.5750551970638,9.32476372439559));
#46282=CARTESIAN_POINT('Ctrl Pts',(-24.66722105931,26.5732520449089,9.32509597367348));
#46283=CARTESIAN_POINT('Ctrl Pts',(-24.680070230751,26.5684807620328,9.32596777243583));
#46284=CARTESIAN_POINT('Ctrl Pts',(-24.6880198674389,26.5654930157655,9.32650630925608));
#46285=CARTESIAN_POINT('Ctrl Pts',(-24.6989570556881,26.5613330315561,9.327245990374));
#46286=CARTESIAN_POINT('Ctrl Pts',(-24.7019547213058,26.5601877347735,9.32744859323432));
#46287=CARTESIAN_POINT('Ctrl Pts',(-24.7163079456354,26.5546793188199,9.32841804731137));
#46288=CARTESIAN_POINT('Ctrl Pts',(-24.7276406526046,26.550256326952,9.3291815805187));
#46289=CARTESIAN_POINT('Ctrl Pts',(-24.7422727423089,26.5444499487968,9.330164680193));
#46290=CARTESIAN_POINT('Ctrl Pts',(-24.7455950489978,26.5431251687639,9.33038771647948));
#46291=CARTESIAN_POINT('Ctrl Pts',(-24.7506803798343,26.5410875589344,9.33072882225837));
#46292=CARTESIAN_POINT('Ctrl Pts',(-24.7524449760967,26.5403787005075,9.33084713195368));
#46293=CARTESIAN_POINT('Ctrl Pts',(-24.7559213653692,26.5389786205154,9.33108010490143));
#46294=CARTESIAN_POINT('Ctrl Pts',(-24.7576331830736,26.538287493539,9.33119477269725));
#46295=CARTESIAN_POINT('Ctrl Pts',(-24.7609983131798,26.536925496477,9.33142008934035));
#46296=CARTESIAN_POINT('Ctrl Pts',(-24.7626516547375,26.5362547273449,9.33153074365644));
#46297=CARTESIAN_POINT('Ctrl Pts',(-24.7663583404249,26.534747319867,9.33177871923271));
#46298=CARTESIAN_POINT('Ctrl Pts',(-24.7684113824629,26.5339099337806,9.33191599496229));
#46299=CARTESIAN_POINT('Ctrl Pts',(-24.7777522452705,26.5300887739676,9.33254024753811));
#46300=CARTESIAN_POINT('Ctrl Pts',(-24.7850300614542,26.5270803790291,9.33302573889215));
#46301=CARTESIAN_POINT('Ctrl Pts',(-24.8029615585778,26.519591049354,9.3342199010479));
#46302=CARTESIAN_POINT('Ctrl Pts',(-24.8136023957874,26.51507938475,9.33492677101193));
#46303=CARTESIAN_POINT('Ctrl Pts',(-24.8545740916084,26.4974469473966,9.33764254872906));
#46304=CARTESIAN_POINT('Ctrl Pts',(-24.8847278604639,26.4839166981611,9.3396285984888));
#46305=CARTESIAN_POINT('Ctrl Pts',(-24.9964736060865,26.431695835367,9.34696035299412));
#46306=CARTESIAN_POINT('Ctrl Pts',(-25.0766415908517,26.3900429972723,9.35216382884057));
#46307=CARTESIAN_POINT('Ctrl Pts',(-25.2187517019879,26.3084474212308,9.36146854096072));
#46308=CARTESIAN_POINT('Ctrl Pts',(-25.2812724451053,26.2696456868055,9.36559234386658));
#46309=CARTESIAN_POINT('Ctrl Pts',(-25.4288687659926,26.1708898120042,9.37552378619351));
#46310=CARTESIAN_POINT('Ctrl Pts',(-25.5124732861423,26.1088904428256,9.3813168945732));
#46311=CARTESIAN_POINT('Ctrl Pts',(-25.7401940315848,25.9222817598008,9.39792859240034));
#46312=CARTESIAN_POINT('Ctrl Pts',(-25.8764503586455,25.7888131638589,9.40891602758545));
#46313=CARTESIAN_POINT('Ctrl Pts',(-26.0083110400416,25.6345329333341,9.4212486538743));
#46314=CARTESIAN_POINT('Ctrl Pts',(-26.0164436429954,25.6249037839733,9.42201683573491));
#46315=CARTESIAN_POINT('Ctrl Pts',(-26.0274799458272,25.6116800101105,9.42306979212775));
#46316=CARTESIAN_POINT('Ctrl Pts',(-26.0304327854314,25.6081263904894,9.42335255760914));
#46317=CARTESIAN_POINT('Ctrl Pts',(-26.0354461010337,25.6020666099687,9.42383441530304));
#46318=CARTESIAN_POINT('Ctrl Pts',(-26.0375104593923,25.5995636573848,9.42403334924495));
#46319=CARTESIAN_POINT('Ctrl Pts',(-26.041496530981,25.5947158084627,9.42441847498305));
#46320=CARTESIAN_POINT('Ctrl Pts',(-26.0434187222781,25.5923713088639,9.42460464703693));
#46321=CARTESIAN_POINT('Ctrl Pts',(-26.0479729248483,25.5868005268418,9.42504682160047));
#46322=CARTESIAN_POINT('Ctrl Pts',(-26.050601992821,25.5835718550916,9.42530294284314));
#46323=CARTESIAN_POINT('Ctrl Pts',(-26.0583413639303,25.5740296804317,9.42605945786255));
#46324=CARTESIAN_POINT('Ctrl Pts',(-26.0634340354701,25.5677019772274,9.42656056150282));
#46325=CARTESIAN_POINT('Ctrl Pts',(-26.0997930884796,25.5221741205263,9.43016207894104));
#46326=CARTESIAN_POINT('Ctrl Pts',(-26.1301632802207,25.4822700975826,9.43329808889174));
#46327=CARTESIAN_POINT('Ctrl Pts',(-26.254705628078,25.310456140014,9.44672522327764));
#46328=CARTESIAN_POINT('Ctrl Pts',(-26.3397749346718,25.172268107692,9.45735779162834));
#46329=CARTESIAN_POINT('Ctrl Pts',(-26.4394053947308,24.9792247632555,9.47191472380165));
#46330=CARTESIAN_POINT('Ctrl Pts',(-26.463461411714,24.9295203382765,9.47563630302654));
#46331=CARTESIAN_POINT('Ctrl Pts',(-26.4974362825707,24.8544627212158,9.4812049326555));
#46332=CARTESIAN_POINT('Ctrl Pts',(-26.5083305596401,24.8295611928029,9.48304414395847));
#46333=CARTESIAN_POINT('Ctrl Pts',(-26.5307461980921,24.7765070723564,9.48694268576868));
#46334=CARTESIAN_POINT('Ctrl Pts',(-26.5421866702694,24.748322984817,9.4890019646958));
#46335=CARTESIAN_POINT('Ctrl Pts',(-26.59855619592,24.6036088894269,9.49950600975966));
#46336=CARTESIAN_POINT('Ctrl Pts',(-26.6370863484994,24.484691521539,9.50791366539804));
#46337=CARTESIAN_POINT('Ctrl Pts',(-26.6695689435786,24.3601888560918,9.51631432739777));
#46338=CARTESIAN_POINT('Ctrl Pts',(-26.6705126771592,24.3565455007143,9.5165598057875));
#46339=CARTESIAN_POINT('Ctrl Pts',(-26.6724175917225,24.3491380008965,9.51705817405828));
#46340=CARTESIAN_POINT('Ctrl Pts',(-26.6733783534086,24.3453737532531,9.51731104746704));
#46341=CARTESIAN_POINT('Ctrl Pts',(-26.6761267323784,24.3345238152638,9.51803880690306));
#46342=CARTESIAN_POINT('Ctrl Pts',(-26.6778970703135,24.3274337246252,9.51851300693196));
#46343=CARTESIAN_POINT('Ctrl Pts',(-26.6800240843095,24.3187901888501,9.51908939132572));
#46344=CARTESIAN_POINT('Ctrl Pts',(-26.6804037292492,24.3172424810962,9.51919253163381));
#46345=CARTESIAN_POINT('Ctrl Pts',(-26.6824302249699,24.3089544522432,9.51974449158068));
#46346=CARTESIAN_POINT('Ctrl Pts',(-26.6840564663185,24.3022090513894,9.52019244234582));
#46347=CARTESIAN_POINT('Ctrl Pts',(-26.6949285582426,24.256465385041,9.52322133855341));
#46348=CARTESIAN_POINT('Ctrl Pts',(-26.7034685326044,24.2173006010444,9.52577103316768));
#46349=CARTESIAN_POINT('Ctrl Pts',(-26.7123142449377,24.1727569010233,9.52861392726454));
#46350=CARTESIAN_POINT('Ctrl Pts',(-26.7133394109521,24.1675266713047,9.52894684792257));
#46351=CARTESIAN_POINT('Ctrl Pts',(-26.7148172212889,24.1598867653613,9.5294318347485));
#46352=CARTESIAN_POINT('Ctrl Pts',(-26.7152800912984,24.1574791125772,9.52958448347532));
#46353=CARTESIAN_POINT('Ctrl Pts',(-26.7160942688041,24.1532178849128,9.52985431110272));
#46354=CARTESIAN_POINT('Ctrl Pts',(-26.7164466964422,24.1513645285788,9.52997155456625));
#46355=CARTESIAN_POINT('Ctrl Pts',(-26.7171788421087,24.1474957926748,9.53021605219894));
#46356=CARTESIAN_POINT('Ctrl Pts',(-26.7175582630661,24.145480364089,9.53034328894474));
#46357=CARTESIAN_POINT('Ctrl Pts',(-26.7183240207792,24.141391307028,9.53060116545819));
#46358=CARTESIAN_POINT('Ctrl Pts',(-26.7187102461443,24.139317658365,9.53073179876874));
#46359=CARTESIAN_POINT('Ctrl Pts',(-26.7196565662239,24.1342089969917,9.531053283364));
#46360=CARTESIAN_POINT('Ctrl Pts',(-26.7202143390603,24.1311735482563,9.53124400236555));
#46361=CARTESIAN_POINT('Ctrl Pts',(-26.7217446684244,24.1227775272685,9.531770712314));
#46362=CARTESIAN_POINT('Ctrl Pts',(-26.722707999196,24.1174152522839,9.53210618510366));
#46363=CARTESIAN_POINT('Ctrl Pts',(-26.7563202363051,23.9275511883541,9.543952662313));
#46364=CARTESIAN_POINT('Ctrl Pts',(-26.7728350193474,23.7405285732528,9.55457143638722));
#46365=CARTESIAN_POINT('Ctrl Pts',(-26.7730012638346,23.5531112005712,9.56507739177766));
#46366=CARTESIAN_POINT('Ctrl Pts',(-26.7730012617393,23.5531135616897,9.5650772594217));
#46367=CARTESIAN_POINT('Ctrl Pts',(-26.7732594660026,23.2622646496,9.5813812232073));
#46368=CARTESIAN_POINT('Ctrl Pts',(-26.7341483716483,22.9727404047934,9.59741081275145));
#46369=CARTESIAN_POINT('Ctrl Pts',(-26.6508830654244,22.6712248915581,9.61619688286547));
#46370=CARTESIAN_POINT('Ctrl Pts',(-26.6448246833606,22.6501289509257,9.61752178419563));
#46371=CARTESIAN_POINT('Ctrl Pts',(-26.6356848506449,22.6194864243494,9.61946225669596));
#46372=CARTESIAN_POINT('Ctrl Pts',(-26.6327734793119,22.6098894393948,9.62007229715068));
#46373=CARTESIAN_POINT('Ctrl Pts',(-26.6274589248023,22.592660553741,9.62117167590116));
#46374=CARTESIAN_POINT('Ctrl Pts',(-26.6250720158306,22.5850236882684,9.6216604785591));
#46375=CARTESIAN_POINT('Ctrl Pts',(-26.6214074382732,22.5734504899288,9.62240352323699));
#46376=CARTESIAN_POINT('Ctrl Pts',(-26.6201505738228,22.5695075599087,9.6226570798158));
#46377=CARTESIAN_POINT('Ctrl Pts',(-26.6178631321862,22.5623790700897,9.62311622640468));
#46378=CARTESIAN_POINT('Ctrl Pts',(-26.6168351772588,22.5591926696378,9.62332172966447));
#46379=CARTESIAN_POINT('Ctrl Pts',(-26.6147739508377,22.5528373001323,9.62373214732872));
#46380=CARTESIAN_POINT('Ctrl Pts',(-26.6137407247162,22.5496683205337,9.62393706002642));
#46381=CARTESIAN_POINT('Ctrl Pts',(-26.6108302863364,22.5407885614183,9.62451199276973));
#46382=CARTESIAN_POINT('Ctrl Pts',(-26.6089420163196,22.5350814449536,9.62488237811046));
#46383=CARTESIAN_POINT('Ctrl Pts',(-26.601191332594,22.5118736814275,9.6263921052055));
#46384=CARTESIAN_POINT('Ctrl Pts',(-26.5951946906331,22.4944185346002,9.62753588708407));
#46385=CARTESIAN_POINT('Ctrl Pts',(-26.4878053690423,22.1903529559902,9.64760819452844));
#46386=CARTESIAN_POINT('Ctrl Pts',(-26.3465300324249,21.9195203719462,9.6680115792069));
#46387=CARTESIAN_POINT('Ctrl Pts',(-26.1274408433168,21.61390938295,9.69345473667857));
#46388=CARTESIAN_POINT('Ctrl Pts',(-26.0834397793119,21.5566910754048,9.69832756584687));
#46389=CARTESIAN_POINT('Ctrl Pts',(-25.9645341693013,21.412368380956,9.71083040500302));
#46390=CARTESIAN_POINT('Ctrl Pts',(-25.8868201136967,21.3276948303605,9.71837987664804));
#46391=CARTESIAN_POINT('Ctrl Pts',(-25.7965119205114,21.2392854226906,9.72634292847421));
#46392=CARTESIAN_POINT('Ctrl Pts',(-25.7882383030415,21.2312721700771,9.72706543536277));
#46393=CARTESIAN_POINT('Ctrl Pts',(-25.7781238406935,21.2215805510566,9.72793998751222));
#46394=CARTESIAN_POINT('Ctrl Pts',(-25.7763239228131,21.2198598770948,9.72809528536088));
#46395=CARTESIAN_POINT('Ctrl Pts',(-25.7731666630712,21.2168486157447,9.7283671096234));
#46396=CARTESIAN_POINT('Ctrl Pts',(-25.7718101901205,21.2155571252709,9.7284837062347));
#46397=CARTESIAN_POINT('Ctrl Pts',(-25.7690761900943,21.2129586389162,9.72871832758051));
#46398=CARTESIAN_POINT('Ctrl Pts',(-25.7676986305437,21.2116516749712,9.72883634978317));
#46399=CARTESIAN_POINT('Ctrl Pts',(-25.7650311139017,21.2091253362788,9.72906451135851));
#46400=CARTESIAN_POINT('Ctrl Pts',(-25.7637413077141,21.207905812741,9.7291746626015));
#46401=CARTESIAN_POINT('Ctrl Pts',(-25.7606622634242,21.2049993625376,9.72943721358092));
#46402=CARTESIAN_POINT('Ctrl Pts',(-25.7588720975974,21.2033134138709,9.72958953698752));
#46403=CARTESIAN_POINT('Ctrl Pts',(-25.7534613572047,21.1982293410369,9.73004895908232));
#46404=CARTESIAN_POINT('Ctrl Pts',(-25.749834835602,21.1948375136324,9.73035557275996));
#46405=CARTESIAN_POINT('Ctrl Pts',(-25.7130621182603,21.1606035706839,9.73345155269726));
#46406=CARTESIAN_POINT('Ctrl Pts',(-25.6792752501237,21.1304529032963,9.73618903330854));
#46407=CARTESIAN_POINT('Ctrl Pts',(-25.6419481672626,21.0985303548686,9.73911383187181));
#46408=CARTESIAN_POINT('Ctrl Pts',(-25.63902972821,21.0960434762595,9.73934186295353));
#46409=CARTESIAN_POINT('Ctrl Pts',(-25.6235770060692,21.0829233359351,9.74054588799739));
#46410=CARTESIAN_POINT('Ctrl Pts',(-25.6109657323873,21.0723806906732,9.74151683038013));
#46411=CARTESIAN_POINT('Ctrl Pts',(-25.5903853040761,21.055441872506,9.74308351228039));
#46412=CARTESIAN_POINT('Ctrl Pts',(-25.5824655700994,21.0489864273123,9.74368218509627));
#46413=CARTESIAN_POINT('Ctrl Pts',(-25.4988687441232,20.9815050604936,9.7499589079307));
#46414=CARTESIAN_POINT('Ctrl Pts',(-25.4204929068524,20.9238915367616,9.75547944982786));
#46415=CARTESIAN_POINT('Ctrl Pts',(-25.2669435169188,20.8213833328133,9.76586236129896));
#46416=CARTESIAN_POINT('Ctrl Pts',(-25.1923150816533,20.7758362065554,9.7707304264875));
#46417=CARTESIAN_POINT('Ctrl Pts',(-25.0372450068812,20.6896451844314,9.78065349991479));
#46418=CARTESIAN_POINT('Ctrl Pts',(-24.9567672916642,20.6492291977996,9.78570546873646));
#46419=CARTESIAN_POINT('Ctrl Pts',(-24.7716774881621,20.5657910055625,9.79726829109988));
#46420=CARTESIAN_POINT('Ctrl Pts',(-24.6662865639314,20.52480151575,9.80381544761824));
#46421=CARTESIAN_POINT('Ctrl Pts',(-24.511494706669,20.4737887367934,9.81352245850843));
#46422=CARTESIAN_POINT('Ctrl Pts',(-24.4636664800881,20.4592509892938,9.81653325743071));
#46423=CARTESIAN_POINT('Ctrl Pts',(-24.4078464421007,20.4436927416017,9.82006672093656));
#46424=CARTESIAN_POINT('Ctrl Pts',(-24.4001635701171,20.4415820329833,9.82055347659638));
#46425=CARTESIAN_POINT('Ctrl Pts',(-24.3884852046702,20.4384201749147,9.82129403789738));
#46426=CARTESIAN_POINT('Ctrl Pts',(-24.3844953477585,20.4373481717215,9.82154716509809));
#46427=CARTESIAN_POINT('Ctrl Pts',(-24.3772985949219,20.4354293628653,9.82200396321513));
#46428=CARTESIAN_POINT('Ctrl Pts',(-24.3740924269704,20.4345798289553,9.82220754519021));
#46429=CARTESIAN_POINT('Ctrl Pts',(-24.3676657890163,20.4328875850017,9.82261577479757));
#46430=CARTESIAN_POINT('Ctrl Pts',(-24.3644453134005,20.4320449122116,9.82282042336128));
#46431=CARTESIAN_POINT('Ctrl Pts',(-24.3554260847859,20.4296998571416,9.82339378456594));
#46432=CARTESIAN_POINT('Ctrl Pts',(-24.3496244622933,20.4282086561136,9.82376285920426));
#46433=CARTESIAN_POINT('Ctrl Pts',(-24.3260869767082,20.4222286847907,9.825261292322));
#46434=CARTESIAN_POINT('Ctrl Pts',(-24.3083174689608,20.4178748722262,9.82639500824015));
#46435=CARTESIAN_POINT('Ctrl Pts',(-24.0151418947004,20.348682935108,9.84514328749083));
#46436=CARTESIAN_POINT('Ctrl Pts',(-23.7324734711579,20.3202535138427,9.86401511527225));
#46437=CARTESIAN_POINT('Ctrl Pts',(-23.3181573708364,20.3331736238322,9.89207423456088));
#46438=CARTESIAN_POINT('Ctrl Pts',(-23.1868811615217,20.3453454307033,9.90099415660954));
#46439=CARTESIAN_POINT('Ctrl Pts',(-22.9772544214802,20.3778313754213,9.91498364404609));
#46440=CARTESIAN_POINT('Ctrl Pts',(-22.8982764789008,20.3931157567231,9.92019330915995));
#46441=CARTESIAN_POINT('Ctrl Pts',(-22.811789685451,20.4132379778774,9.9257711836903));
#46442=CARTESIAN_POINT('Ctrl Pts',(-22.8036408620733,20.4151674124913,9.92629546974006));
#46443=CARTESIAN_POINT('Ctrl Pts',(-22.7933033541201,20.4176576635031,9.92695888572668));
#46444=CARTESIAN_POINT('Ctrl Pts',(-22.7911077128188,20.4181890250432,9.92709969556467));
#46445=CARTESIAN_POINT('Ctrl Pts',(-22.7871674727165,20.4191469792042,9.92735221311207));
#46446=CARTESIAN_POINT('Ctrl Pts',(-22.7854226712723,20.4195727216987,9.92746396990977));
#46447=CARTESIAN_POINT('Ctrl Pts',(-22.7820396407255,20.4204011993433,9.9276805358768));
#46448=CARTESIAN_POINT('Ctrl Pts',(-22.7804013733479,20.420803761941,9.92778535477929));
#46449=CARTESIAN_POINT('Ctrl Pts',(-22.7769847458104,20.4216461566792,9.92800383995364));
#46450=CARTESIAN_POINT('Ctrl Pts',(-22.7752064494867,20.4220862175471,9.92811749239075));
#46451=CARTESIAN_POINT('Ctrl Pts',(-22.7702930072805,20.4233065550729,9.92843133643765));
#46452=CARTESIAN_POINT('Ctrl Pts',(-22.7671586469503,20.4240900329865,9.92863134174013));
#46453=CARTESIAN_POINT('Ctrl Pts',(-22.7548918589547,20.4271758972516,9.92941332558684));
#46454=CARTESIAN_POINT('Ctrl Pts',(-22.7457682457995,20.4295136282758,9.92999327312652));
#46455=CARTESIAN_POINT('Ctrl Pts',(-22.5919497870095,20.4696457137232,9.93974472504502));
#46456=CARTESIAN_POINT('Ctrl Pts',(-22.4500259417727,20.5174325613287,9.94835500180697));
#46457=CARTESIAN_POINT('Ctrl Pts',(-22.1607185321659,20.6378421865267,9.96605601923618));
#46458=CARTESIAN_POINT('Ctrl Pts',(-22.0145357699813,20.7122049266954,9.97509555538223));
#46459=CARTESIAN_POINT('Ctrl Pts',(-21.7569343781771,20.8690001841141,9.99212257320224));
#46460=CARTESIAN_POINT('Ctrl Pts',(-21.6439591265324,20.9481104005739,10.0000297559278));
#46461=CARTESIAN_POINT('Ctrl Pts',(-21.5072763004697,21.0575116246166,10.0104244143713));
#46462=CARTESIAN_POINT('Ctrl Pts',(-21.478560776641,21.0813251915461,10.0126578070469));
#46463=CARTESIAN_POINT('Ctrl Pts',(-21.4331613503375,21.1203243537113,10.0162735037541));
#46464=CARTESIAN_POINT('Ctrl Pts',(-21.4162117970594,21.1351963991918,10.0176429619218));
#46465=CARTESIAN_POINT('Ctrl Pts',(-21.3947564967531,21.1544241527385,10.0194022568126));
#46466=CARTESIAN_POINT('Ctrl Pts',(-21.3901051797319,21.1586170672071,10.0197852271972));
#46467=CARTESIAN_POINT('Ctrl Pts',(-21.3826809460276,21.1653489448089,10.0203990423436));
#46468=CARTESIAN_POINT('Ctrl Pts',(-21.3799001841313,21.167879264348,10.020629520337));
#46469=CARTESIAN_POINT('Ctrl Pts',(-21.3746449424871,21.1726780430055,10.0210661789662));
#46470=CARTESIAN_POINT('Ctrl Pts',(-21.3721695650827,21.1749455153488,10.0212723174305));
#46471=CARTESIAN_POINT('Ctrl Pts',(-21.366578574031,21.1800830117546,10.0217389529322));
#46472=CARTESIAN_POINT('Ctrl Pts',(-21.3634650716837,21.1829553152268,10.0219995471816));
#46473=CARTESIAN_POINT('Ctrl Pts',(-21.3554962380755,21.1903359497997,10.0226684173856));
#46474=CARTESIAN_POINT('Ctrl Pts',(-21.3506491480087,21.1948531143324,10.0230770720028));
#46475=CARTESIAN_POINT('Ctrl Pts',(-21.3259242485419,21.2180379486562,10.0251709403466));
#46476=CARTESIAN_POINT('Ctrl Pts',(-21.3062705046678,21.2369419686161,10.0268663471001));
#46477=CARTESIAN_POINT('Ctrl Pts',(-21.2802022522148,21.262660621387,10.0291578508912));
#46478=CARTESIAN_POINT('Ctrl Pts',(-21.2735736888501,21.2692574718488,10.0297443183353));
#46479=CARTESIAN_POINT('Ctrl Pts',(-21.2646534430799,21.2782126595186,10.0305387081105));
#46480=CARTESIAN_POINT('Ctrl Pts',(-21.2623364715423,21.2805458378238,10.0307455196922));
#46481=CARTESIAN_POINT('Ctrl Pts',(-21.2589751504957,21.2839410474797,10.0310462404424));
#46482=CARTESIAN_POINT('Ctrl Pts',(-21.2579279546272,21.2850002688243,10.0311400256239));
#46483=CARTESIAN_POINT('Ctrl Pts',(-21.254072397586,21.2889055125535,10.0314856837092));
#46484=CARTESIAN_POINT('Ctrl Pts',(-21.2512686080507,21.2917560256427,10.0317377545512));
#46485=CARTESIAN_POINT('Ctrl Pts',(-21.2435991667335,21.2995823537661,10.0324292052521));
#46486=CARTESIAN_POINT('Ctrl Pts',(-21.2387443373613,21.3045687021639,10.0328690490053));
#46487=CARTESIAN_POINT('Ctrl Pts',(-21.2295896692366,21.3140325117979,10.0337025414262));
#46488=CARTESIAN_POINT('Ctrl Pts',(-21.225286535791,21.3185067541449,10.034096047231));
#46489=CARTESIAN_POINT('Ctrl Pts',(-21.2149702038642,21.3292955209327,10.0350436024534));
#46490=CARTESIAN_POINT('Ctrl Pts',(-21.2089696767702,21.3356220466723,10.0355981783216));
#46491=CARTESIAN_POINT('Ctrl Pts',(-21.1841843416621,21.3619672442333,10.037903166935));
#46492=CARTESIAN_POINT('Ctrl Pts',(-21.1656304494669,21.3822007260568,10.0396629692902));
#46493=CARTESIAN_POINT('Ctrl Pts',(-21.0319835248743,21.5317371987251,10.0525935905876));
#46494=CARTESIAN_POINT('Ctrl Pts',(-20.9272300063733,21.6698743882735,10.0641562772667));
#46495=CARTESIAN_POINT('Ctrl Pts',(-20.7420943473768,21.959787700169,10.0874041577501));
#46496=CARTESIAN_POINT('Ctrl Pts',(-20.6617059540806,22.1109351431346,10.099046593302));
#46497=CARTESIAN_POINT('Ctrl Pts',(-20.5728105365335,22.3158670378401,10.1137209585626));
#46498=CARTESIAN_POINT('Ctrl Pts',(-20.5531149675324,22.3644888550931,10.1171239425134));
#46499=CARTESIAN_POINT('Ctrl Pts',(-20.5287398994178,22.4291564902782,10.12152786615));
#46500=CARTESIAN_POINT('Ctrl Pts',(-20.5229866617987,22.4447859780416,10.1225829862264));
#46501=CARTESIAN_POINT('Ctrl Pts',(-20.5138140375137,22.470313429217,10.1242904492873));
#46502=CARTESIAN_POINT('Ctrl Pts',(-20.510321354729,22.4801844775349,10.1249468613048));
#46503=CARTESIAN_POINT('Ctrl Pts',(-20.5058119972764,22.4931291370565,10.1258024872598));
#46504=CARTESIAN_POINT('Ctrl Pts',(-20.5047518092512,22.496187358702,10.1260042546633));
#46505=CARTESIAN_POINT('Ctrl Pts',(-20.5030272562966,22.5011863320313,10.1263334418329));
#46506=CARTESIAN_POINT('Ctrl Pts',(-20.5023601370619,22.5031261204637,10.1264610258994));
#46507=CARTESIAN_POINT('Ctrl Pts',(-20.5010830756246,22.5068510034069,10.126705724329));
#46508=CARTESIAN_POINT('Ctrl Pts',(-20.5004728505192,22.5086359912308,10.1268228551687));
#46509=CARTESIAN_POINT('Ctrl Pts',(-20.4990734541007,22.5127411799256,10.1270919399047));
#46510=CARTESIAN_POINT('Ctrl Pts',(-20.4982853599476,22.5150617515623,10.1272438292192));
#46511=CARTESIAN_POINT('Ctrl Pts',(-20.4957934779308,22.5224267679684,10.1277252090735));
#46512=CARTESIAN_POINT('Ctrl Pts',(-20.4940995323904,22.5274745706955,10.1280541155636));
#46513=CARTESIAN_POINT('Ctrl Pts',(-20.4798055621644,22.570421883641,10.1308440163167));
#46514=CARTESIAN_POINT('Ctrl Pts',(-20.4678978592618,22.6085504966277,10.1332648448311));
#46515=CARTESIAN_POINT('Ctrl Pts',(-20.4546015545916,22.6540836252423,10.136100511888));
#46516=CARTESIAN_POINT('Ctrl Pts',(-20.4525267711698,22.6612818935096,10.1365471700814));
#46517=CARTESIAN_POINT('Ctrl Pts',(-20.4435889773841,22.6927019991411,10.1384899805712));
#46518=CARTESIAN_POINT('Ctrl Pts',(-20.4369846504172,22.7169971539186,10.1399745578865));
#46519=CARTESIAN_POINT('Ctrl Pts',(-20.4176113813649,22.7917131184576,10.144493079108));
#46520=CARTESIAN_POINT('Ctrl Pts',(-20.4057773329277,22.8423692064602,10.1474913007309));
#46521=CARTESIAN_POINT('Ctrl Pts',(-20.3532243485018,23.0947567857408,10.162204494736));
#46522=CARTESIAN_POINT('Ctrl Pts',(-20.330666237766,23.2997810632507,10.1734794439604));
#46523=CARTESIAN_POINT('Ctrl Pts',(-20.3260243255975,23.6344957344806,10.1924330484611));
#46524=CARTESIAN_POINT('Ctrl Pts',(-20.3319759177558,23.7634073428135,10.1998575871149));
#46525=CARTESIAN_POINT('Ctrl Pts',(-20.3513725425805,23.9455017129285,10.2107420226139));
#46526=CARTESIAN_POINT('Ctrl Pts',(-20.3584716824424,23.9992398060966,10.2140028231158));
#46527=CARTESIAN_POINT('Ctrl Pts',(-20.3681891681188,24.0607976770839,10.2178024312092));
#46528=CARTESIAN_POINT('Ctrl Pts',(-20.3694865962945,24.068819458507,10.2182988261917));
#46529=CARTESIAN_POINT('Ctrl Pts',(-20.3714947908558,24.0809446553052,10.2190510751543));
#46530=CARTESIAN_POINT('Ctrl Pts',(-20.3721832017651,24.0850517827297,10.2193062174361));
#46531=CARTESIAN_POINT('Ctrl Pts',(-20.3733865518856,24.0921467104341,10.2197475514024));
#46532=CARTESIAN_POINT('Ctrl Pts',(-20.3738977513965,24.0951351467547,10.2199336237567));
#46533=CARTESIAN_POINT('Ctrl Pts',(-20.3749646707315,24.1013197570857,10.2203190759497));
#46534=CARTESIAN_POINT('Ctrl Pts',(-20.3755210009019,24.1045158212427,10.2205184750589));
#46535=CARTESIAN_POINT('Ctrl Pts',(-20.3768811670764,24.112260611558,10.2210021671578));
#46536=CARTESIAN_POINT('Ctrl Pts',(-20.3776899570954,24.1168084508386,10.221286617908));
#46537=CARTESIAN_POINT('Ctrl Pts',(-20.3807407659188,24.1337518074821,10.2223479420846));
#46538=CARTESIAN_POINT('Ctrl Pts',(-20.3830456534096,24.1461357594668,10.2231268197785));
#46539=CARTESIAN_POINT('Ctrl Pts',(-20.4236401278124,24.3573546845948,10.2364660490928));
#46540=CARTESIAN_POINT('Ctrl Pts',(-20.4805045395809,24.5521199163188,10.2496409639259));
#46541=CARTESIAN_POINT('Ctrl Pts',(-20.6644750750044,25.0151461744725,10.283006592554));
#46542=CARTESIAN_POINT('Ctrl Pts',(-20.8110326273105,25.2737115605248,10.30354247522));
#46543=CARTESIAN_POINT('Ctrl Pts',(-20.995608096444,25.5149336235747,10.322687537788));
#46544=CARTESIAN_POINT('Ctrl Pts',(-21.0004323161356,25.5211905963562,10.3231840236561));
#46545=CARTESIAN_POINT('Ctrl Pts',(-21.008836773015,25.5320086021746,10.3240421378804));
#46546=CARTESIAN_POINT('Ctrl Pts',(-21.0124063738628,25.5365777975498,10.3244044900252));
#46547=CARTESIAN_POINT('Ctrl Pts',(-21.0175760982318,25.5431585134001,10.324926202691));
#46548=CARTESIAN_POINT('Ctrl Pts',(-21.0191663008336,25.5451777585119,10.3250862646727));
#46549=CARTESIAN_POINT('Ctrl Pts',(-21.0219410934185,25.5486925416565,10.325364834075));
#46550=CARTESIAN_POINT('Ctrl Pts',(-21.023124597488,25.5501889323233,10.3254834196823));
#46551=CARTESIAN_POINT('Ctrl Pts',(-21.0254037608313,25.5530653915963,10.3257113461496));
#46552=CARTESIAN_POINT('Ctrl Pts',(-21.0264992210538,25.5544456098645,10.3258207010403));
#46553=CARTESIAN_POINT('Ctrl Pts',(-21.029095346845,25.5577110786939,10.3260793989734));
#46554=CARTESIAN_POINT('Ctrl Pts',(-21.0305969984067,25.5595955492751,10.3262286708006));
#46555=CARTESIAN_POINT('Ctrl Pts',(-21.0350771456954,25.5652049098675,10.3266729425233));
#46556=CARTESIAN_POINT('Ctrl Pts',(-21.0380618148502,25.5689248952871,10.3269675006466));
#46557=CARTESIAN_POINT('Ctrl Pts',(-21.0656660204678,25.6031737579567,10.3296788973547));
#46558=CARTESIAN_POINT('Ctrl Pts',(-21.0908340015717,25.6332591390837,10.3320568848884));
#46559=CARTESIAN_POINT('Ctrl Pts',(-21.1183446272352,25.6649508630178,10.3345670048003));
#46560=CARTESIAN_POINT('Ctrl Pts',(-21.1201456173546,25.6670202263773,10.3347309311805));
#46561=CARTESIAN_POINT('Ctrl Pts',(-21.1230447815097,25.6703428308316,10.3349941774349));
#46562=CARTESIAN_POINT('Ctrl Pts',(-21.124141285135,25.6715975197637,10.3350935949948));
#46563=CARTESIAN_POINT('Ctrl Pts',(-21.1324227555589,25.6810588835894,10.3358433635224));
#46564=CARTESIAN_POINT('Ctrl Pts',(-21.1396484600537,25.6892299863481,10.3364913404259));
#46565=CARTESIAN_POINT('Ctrl Pts',(-21.1524203672679,25.7035260262691,10.337626160937));
#46566=CARTESIAN_POINT('Ctrl Pts',(-21.1579488588396,25.7096665657605,10.3381139678288));
#46567=CARTESIAN_POINT('Ctrl Pts',(-21.1869951468207,25.7416800534615,10.3406594965129));
#46568=CARTESIAN_POINT('Ctrl Pts',(-21.2109099658353,25.7671910899603,10.3426961197103));
#46569=CARTESIAN_POINT('Ctrl Pts',(-21.4324401971319,25.9959302983987,10.3610868640007));
#46570=CARTESIAN_POINT('Ctrl Pts',(-21.6556512693953,26.1726516140465,10.3763583019341));
#46571=CARTESIAN_POINT('Ctrl Pts',(-21.9567406782508,26.3522767329498,10.3965290944547));
#46572=CARTESIAN_POINT('Ctrl Pts',(-22.0154087963457,26.3848371833493,10.4004350448422));
#46573=CARTESIAN_POINT('Ctrl Pts',(-22.0750360597002,26.4155367973924,10.4044010236784));
#46574=CARTESIAN_POINT('Origin',(-23.5502525316942,23.5502525316942,-77.3107734492734));
#46575=CARTESIAN_POINT('',(-22.075036015346,26.4155367745563,11.9036974267447));
#46576=CARTESIAN_POINT('',(-22.0750360887345,26.4155368123409,11.6559056162233));
#46577=CARTESIAN_POINT('',(-22.0750360153461,26.4155367745563,-77.3107734492734));
#46578=CARTESIAN_POINT('',(-26.7730011657502,23.5472853461167,11.0607734492729));
#46579=CARTESIAN_POINT('Ctrl Pts',(-26.7730011657502,23.5472853461167,11.0607734492729));
#46580=CARTESIAN_POINT('Ctrl Pts',(-26.7728766101578,23.412001807288,11.0691292856908));
#46581=CARTESIAN_POINT('Ctrl Pts',(-26.7642301502994,23.2770954679651,11.0774851221087));
#46582=CARTESIAN_POINT('Ctrl Pts',(-26.7472248682243,23.143453512569,11.0858409585267));
#46583=CARTESIAN_POINT('Ctrl Pts',(-26.7337234486191,23.0373478855828,11.0924751121462));
#46584=CARTESIAN_POINT('Ctrl Pts',(-26.7149538773761,22.9320384752182,11.0991092657658));
#46585=CARTESIAN_POINT('Ctrl Pts',(-26.6910180747066,22.8279580167446,11.1057434193854));
#46586=CARTESIAN_POINT('Ctrl Pts',(-26.6687493772687,22.7311266603478,11.1119155106977));
#46587=CARTESIAN_POINT('Ctrl Pts',(-26.6419592261036,22.6351555609155,11.1180876020101));
#46588=CARTESIAN_POINT('Ctrl Pts',(-26.6107288815254,22.5404990594922,11.1242596933224));
#46589=CARTESIAN_POINT('Ctrl Pts',(-26.5795408509766,22.4459708082704,11.1304234220612));
#46590=CARTESIAN_POINT('Ctrl Pts',(-26.5439247194081,22.352754023724,11.1365871508));
#46591=CARTESIAN_POINT('Ctrl Pts',(-26.5040125621126,22.2612920027397,11.1427508795388));
#46592=CARTESIAN_POINT('Ctrl Pts',(-26.4641426880019,22.1699268771826,11.1489080783854));
#46593=CARTESIAN_POINT('Ctrl Pts',(-26.4199860092171,22.0803132152584,11.1550652772321));
#46594=CARTESIAN_POINT('Ctrl Pts',(-26.3717238173773,21.992877385313,11.1612224760788));
#46595=CARTESIAN_POINT('Ctrl Pts',(-26.3234969022729,21.9055054656569,11.1673751743865));
#46596=CARTESIAN_POINT('Ctrl Pts',(-26.2711706496585,21.8203085922524,11.1735278726942));
#46597=CARTESIAN_POINT('Ctrl Pts',(-26.2149733013765,21.7376905928564,11.1796805710019));
#46598=CARTESIAN_POINT('Ctrl Pts',(-26.158797263209,21.6551039223233,11.1858309361976));
#46599=CARTESIAN_POINT('Ctrl Pts',(-26.0987532901732,21.5750945414807,11.1919813013934));
#46600=CARTESIAN_POINT('Ctrl Pts',(-26.0351136844878,21.4980384556687,11.1981316665891));
#46601=CARTESIAN_POINT('Ctrl Pts',(-25.971481185564,21.4209909748634,11.2042813449613));
#46602=CARTESIAN_POINT('Ctrl Pts',(-25.9042541289125,21.3468964683414,11.2104310233336));
#46603=CARTESIAN_POINT('Ctrl Pts',(-25.8337453125777,21.2760981213357,11.2165807017058));
#46604=CARTESIAN_POINT('Ctrl Pts',(-25.7632255070671,21.2052887400292,11.2227313385382));
#46605=CARTESIAN_POINT('Ctrl Pts',(-25.6894232325111,21.1377768464531,11.2288819753707));
#46606=CARTESIAN_POINT('Ctrl Pts',(-25.6126876401643,21.0738682751924,11.2350326122031));
#46607=CARTESIAN_POINT('Ctrl Pts',(-25.5358699568532,21.0098913351855,11.2411898289249));
#46608=CARTESIAN_POINT('Ctrl Pts',(-25.4561130238567,20.949525693689,11.2473470456467));
#46609=CARTESIAN_POINT('Ctrl Pts',(-25.373798434421,20.8930363374133,11.2535042623686));
#46610=CARTESIAN_POINT('Ctrl Pts',(-25.2914379220129,20.8365154659572,11.2596649141764));
#46611=CARTESIAN_POINT('Ctrl Pts',(-25.2065172807383,20.7838754153129,11.2658255659842));
#46612=CARTESIAN_POINT('Ctrl Pts',(-25.1194445925097,20.735336220545,11.271986217792));
#46613=CARTESIAN_POINT('Ctrl Pts',(-25.0322262007103,20.6867158024436,11.278157178561));
#46614=CARTESIAN_POINT('Ctrl Pts',(-24.9428489578115,20.6422101410048,11.2843281393301));
#46615=CARTESIAN_POINT('Ctrl Pts',(-24.8517430197356,20.6019920153833,11.2904991000991));
#46616=CARTESIAN_POINT('Ctrl Pts',(-24.7822001466058,20.5712927649647,11.2952095103195));
#46617=CARTESIAN_POINT('Ctrl Pts',(-24.7116504972118,20.5430906941663,11.2999199205399));
#46618=CARTESIAN_POINT('Ctrl Pts',(-24.6402909599315,20.5174429782494,11.3046303307602));
#46619=CARTESIAN_POINT('Ctrl Pts',(-24.5467879401322,20.4838365539285,11.3108024220726));
#46620=CARTESIAN_POINT('Ctrl Pts',(-24.4515646315331,20.4544991098487,11.3169745133849));
#46621=CARTESIAN_POINT('Ctrl Pts',(-24.3550472035227,20.4296078709396,11.3231466046972));
#46622=CARTESIAN_POINT('Ctrl Pts',(-24.2586605470852,20.4047503571983,11.329310333436));
#46623=CARTESIAN_POINT('Ctrl Pts',(-24.1609836732443,20.3843271824758,11.3354740621748));
#46624=CARTESIAN_POINT('Ctrl Pts',(-24.062460927403,20.3684668503722,11.3416377909136));
#46625=CARTESIAN_POINT('Ctrl Pts',(-23.9640425571641,20.352623320802,11.3477949897603));
#46626=CARTESIAN_POINT('Ctrl Pts',(-23.8647805230092,20.3413330922724,11.353952188607));
#46627=CARTESIAN_POINT('Ctrl Pts',(-23.765131531587,20.3346741112689,11.3601093874537));
#46628=CARTESIAN_POINT('Ctrl Pts',(-23.6655553775348,20.3280199975766,11.3662620857614));
#46629=CARTESIAN_POINT('Ctrl Pts',(-23.56559326068,20.3259904300169,11.3724147840691));
#46630=CARTESIAN_POINT('Ctrl Pts',(-23.4657083024818,20.3286116709205,11.3785674823768));
#46631=CARTESIAN_POINT('Ctrl Pts',(-23.3658612208019,20.3312319178457,11.3847178475726));
#46632=CARTESIAN_POINT('Ctrl Pts',(-23.2660916734112,20.3384994576095,11.3908682127683));
#46633=CARTESIAN_POINT('Ctrl Pts',(-23.1668631908042,20.350388444613,11.3970185779641));
#46634=CARTESIAN_POINT('Ctrl Pts',(-23.0676457892397,20.3622761039496,11.4031682563363));
#46635=CARTESIAN_POINT('Ctrl Pts',(-22.9689697636495,20.3787841327985,11.4093179347085));
#46636=CARTESIAN_POINT('Ctrl Pts',(-22.8712929221316,20.3998348750838,11.4154676130807));
#46637=CARTESIAN_POINT('Ctrl Pts',(-22.7736008571558,20.4208888982398,11.4216182499132));
#46638=CARTESIAN_POINT('Ctrl Pts',(-22.6769087102609,20.4464869495863,11.4277688867456));
#46639=CARTESIAN_POINT('Ctrl Pts',(-22.5816625162692,20.4765005988735,11.4339195235781));
#46640=CARTESIAN_POINT('Ctrl Pts',(-22.4863144288581,20.5065463564606,11.4400767402999));
#46641=CARTESIAN_POINT('Ctrl Pts',(-22.3924157984164,20.541017014062,11.4462339570217));
#46642=CARTESIAN_POINT('Ctrl Pts',(-22.3003958300361,20.5797347674281,11.4523911737436));
#46643=CARTESIAN_POINT('Ctrl Pts',(-22.2083245240924,20.6184741212702,11.4585518255514));
#46644=CARTESIAN_POINT('Ctrl Pts',(-22.1181343596272,20.6614651026508,11.4647124773592));
#46645=CARTESIAN_POINT('Ctrl Pts',(-22.0302310414056,20.70848332369,11.470873129167));
#46646=CARTESIAN_POINT('Ctrl Pts',(-21.9421806296738,20.755580222933,11.477044089936));
#46647=CARTESIAN_POINT('Ctrl Pts',(-21.8564250812213,20.8067176002407,11.4832150507051));
#46648=CARTESIAN_POINT('Ctrl Pts',(-21.7733422755615,20.8616269526761,11.4893860114741));
#46649=CARTESIAN_POINT('Ctrl Pts',(-21.7099236100468,20.9035402923627,11.4940964216945));
#46650=CARTESIAN_POINT('Ctrl Pts',(-21.6480616583938,20.9476504812598,11.4988068319148));
#46651=CARTESIAN_POINT('Ctrl Pts',(-21.587910949624,20.9938227795245,11.5035172421352));
#46652=CARTESIAN_POINT('Ctrl Pts',(-21.5090949549101,21.0543227418755,11.5096893334475));
#46653=CARTESIAN_POINT('Ctrl Pts',(-21.4329406358746,21.1185775768524,11.5158614247599));
#46654=CARTESIAN_POINT('Ctrl Pts',(-21.3598274574452,21.1863245385859,11.5220335160722));
#46655=CARTESIAN_POINT('Ctrl Pts',(-21.2868133401444,21.2539797098838,11.528197244811));
#46656=CARTESIAN_POINT('Ctrl Pts',(-21.2168324894578,21.3251173109555,11.5343609735497));
#46657=CARTESIAN_POINT('Ctrl Pts',(-21.1502332051477,21.3994329682014,11.5405247022885));
#46658=CARTESIAN_POINT('Ctrl Pts',(-21.0837044765288,21.4736698949833,11.5466819011352));
#46659=CARTESIAN_POINT('Ctrl Pts',(-21.0205504803597,21.5510778626136,11.5528390999819));
#46660=CARTESIAN_POINT('Ctrl Pts',(-20.9610836636312,21.6313147695056,11.5589962988285));
#46661=CARTESIAN_POINT('Ctrl Pts',(-20.9016603135395,21.7114930280845,11.5651489971362));
#46662=CARTESIAN_POINT('Ctrl Pts',(-20.845919042444,21.794495766878,11.5713016954439));
#46663=CARTESIAN_POINT('Ctrl Pts',(-20.7941322820659,21.8799475499352,11.5774543937516));
#46664=CARTESIAN_POINT('Ctrl Pts',(-20.742365159301,21.9653669295547,11.5836047589474));
#46665=CARTESIAN_POINT('Ctrl Pts',(-20.6945497925449,22.0532331370677,11.5897551241432));
#46666=CARTESIAN_POINT('Ctrl Pts',(-20.6509149953443,22.1431422258502,11.5959054893389));
#46667=CARTESIAN_POINT('Ctrl Pts',(-20.6072850709284,22.2330412743055,11.6020551677111));
#46668=CARTESIAN_POINT('Ctrl Pts',(-20.5678349775696,22.3249823596631,11.6082048460833));
#46669=CARTESIAN_POINT('Ctrl Pts',(-20.5327468465931,22.4185383438878,11.6143545244555));
#46670=CARTESIAN_POINT('Ctrl Pts',(-20.4976532469438,22.5121089093126,11.620505161288));
#46671=CARTESIAN_POINT('Ctrl Pts',(-20.4669231125643,22.6072944667511,11.6266557981204));
#46672=CARTESIAN_POINT('Ctrl Pts',(-20.4406894936607,22.703650337629,11.6328064349529));
#46673=CARTESIAN_POINT('Ctrl Pts',(-20.4144278102958,22.8001092890476,11.6389636516747));
#46674=CARTESIAN_POINT('Ctrl Pts',(-20.3926723624938,22.897740634041,11.6451208683965));
#46675=CARTESIAN_POINT('Ctrl Pts',(-20.3755055641038,22.9960871644295,11.6512780851183));
#46676=CARTESIAN_POINT('Ctrl Pts',(-20.3583291884273,23.0944885619444,11.6574387369261));
#46677=CARTESIAN_POINT('Ctrl Pts',(-20.3457466150501,23.1936055084951,11.6635993887339));
#46678=CARTESIAN_POINT('Ctrl Pts',(-20.3377883633087,23.2929753866941,11.6697600405417));
#46679=CARTESIAN_POINT('Ctrl Pts',(-20.3298167945822,23.3925115460356,11.6759310013108));
#46680=CARTESIAN_POINT('Ctrl Pts',(-20.3264850187324,23.4923010480786,11.6821019620798));
#46681=CARTESIAN_POINT('Ctrl Pts',(-20.3277713996297,23.591880839228,11.6882729228488));
#46682=CARTESIAN_POINT('Ctrl Pts',(-20.3287533183215,23.6678919635137,11.6929833330692));
#46683=CARTESIAN_POINT('Ctrl Pts',(-20.3324249529497,23.743780888438,11.6976937432897));
#46684=CARTESIAN_POINT('Ctrl Pts',(-20.3387564741105,23.8193447735452,11.7024041535101));
#46685=CARTESIAN_POINT('Ctrl Pts',(-20.3470527211297,23.9183567867183,11.7085762448224));
#46686=CARTESIAN_POINT('Ctrl Pts',(-20.3599467540298,24.0171591553197,11.7147483361347));
#46687=CARTESIAN_POINT('Ctrl Pts',(-20.3774226371827,24.1152906038577,11.720920427447));
#46688=CARTESIAN_POINT('Ctrl Pts',(-20.3948748422417,24.2132890939845,11.7270841561858));
#46689=CARTESIAN_POINT('Ctrl Pts',(-20.4168964830926,24.3106180469394,11.7332478849246));
#46690=CARTESIAN_POINT('Ctrl Pts',(-20.4434197559064,24.4068199054544,11.7394116136634));
#46691=CARTESIAN_POINT('Ctrl Pts',(-20.4699149298019,24.5029198471293,11.7455688125101));
#46692=CARTESIAN_POINT('Ctrl Pts',(-20.500902139522,24.5978946517805,11.7517260113567));
#46693=CARTESIAN_POINT('Ctrl Pts',(-20.5362624601059,24.6912965321022,11.7578832102034));
#46694=CARTESIAN_POINT('Ctrl Pts',(-20.5715969344397,24.7846301413135,11.7640359085111));
#46695=CARTESIAN_POINT('Ctrl Pts',(-20.6112980111599,24.8763927069807,11.7701886068188));
#46696=CARTESIAN_POINT('Ctrl Pts',(-20.6551970905961,24.9661520886785,11.7763413051265));
#46697=CARTESIAN_POINT('Ctrl Pts',(-20.699079523439,25.0558774334911,11.7824916703223));
#46698=CARTESIAN_POINT('Ctrl Pts',(-20.7471566052917,25.1436007138747,11.788642035518));
#46699=CARTESIAN_POINT('Ctrl Pts',(-20.799212172504,25.2289110748788,11.7947924007138));
#46700=CARTESIAN_POINT('Ctrl Pts',(-20.8512619265674,25.3142119091048,11.800942079086));
#46701=CARTESIAN_POINT('Ctrl Pts',(-20.9072890564203,25.397099988846,11.8070917574582));
#46702=CARTESIAN_POINT('Ctrl Pts',(-20.9670326533697,25.477191197747,11.8132414358304));
#46703=CARTESIAN_POINT('Ctrl Pts',(-21.026785561678,25.5572948892909,11.8193920726629));
#46704=CARTESIAN_POINT('Ctrl Pts',(-21.0902558278228,25.6346004959399,11.8255427094953));
#46705=CARTESIAN_POINT('Ctrl Pts',(-21.1571412555356,25.7087557127024,11.8316933463278));
#46706=CARTESIAN_POINT('Ctrl Pts',(-21.2240982366056,25.7829902599693,11.8378505630496));
#46707=CARTESIAN_POINT('Ctrl Pts',(-21.2944773834156,25.8540673640787,11.8440077797714));
#46708=CARTESIAN_POINT('Ctrl Pts',(-21.3679385872317,25.9216705484733,11.8501649964932));
#46709=CARTESIAN_POINT('Ctrl Pts',(-21.4414407747526,25.9893114484076,11.8563256483011));
#46710=CARTESIAN_POINT('Ctrl Pts',(-21.5180281105708,26.0534742899796,11.8624863001088));
#46711=CARTESIAN_POINT('Ctrl Pts',(-21.5973278839115,26.1138833324498,11.8686469519166));
#46712=CARTESIAN_POINT('Ctrl Pts',(-21.6767603539723,26.1743934607297,11.8748179126857));
#46713=CARTESIAN_POINT('Ctrl Pts',(-21.7589139702431,26.231136995885,11.8809888734547));
#46714=CARTESIAN_POINT('Ctrl Pts',(-21.84338746272,26.2838818406561,11.8871598342238));
#46715=CARTESIAN_POINT('Ctrl Pts',(-21.9078676655937,26.3241429710021,11.8918702444441));
#46716=CARTESIAN_POINT('Ctrl Pts',(-21.9736989655831,26.3620751442669,11.8965806546645));
#46717=CARTESIAN_POINT('Ctrl Pts',(-22.0406945855522,26.397593812563,11.9012910648848));
#46718=CARTESIAN_POINT('Ctrl Pts',(-22.0521030543927,26.4036421724513,11.9020931855048));
#46719=CARTESIAN_POINT('Ctrl Pts',(-22.0635504782946,26.4096233458974,11.9028953061248));
#46720=CARTESIAN_POINT('Ctrl Pts',(-22.075036015346,26.4155367745563,11.9036974267448));
#46721=CARTESIAN_POINT('Ctrl Pts',(-26.7730011593802,23.5472784355037,11.0606497612747));
#46722=CARTESIAN_POINT('Ctrl Pts',(-26.7732128984034,23.7767201223076,11.0478295799405));
#46723=CARTESIAN_POINT('Ctrl Pts',(-26.7489235004643,24.0055091845135,11.034997470879));
#46724=CARTESIAN_POINT('Ctrl Pts',(-26.690296845201,24.2773033895601,11.0184510144448));
#46725=CARTESIAN_POINT('Ctrl Pts',(-26.6789720184836,24.324587875792,11.0155259372985));
#46726=CARTESIAN_POINT('Ctrl Pts',(-26.6648259122225,24.3782608176138,11.0121464884727));
#46727=CARTESIAN_POINT('Ctrl Pts',(-26.6630480283088,24.3849196865192,11.0117261762637));
#46728=CARTESIAN_POINT('Ctrl Pts',(-26.6601112650086,24.3957791183713,11.0110389954556));
#46729=CARTESIAN_POINT('Ctrl Pts',(-26.6589651959815,24.3999831481575,11.0107725428983));
#46730=CARTESIAN_POINT('Ctrl Pts',(-26.6567254242061,24.4081339359079,11.0102551170065));
#46731=CARTESIAN_POINT('Ctrl Pts',(-26.6556327168615,24.4120809606345,11.0100041764616));
#46732=CARTESIAN_POINT('Ctrl Pts',(-26.6537202984865,24.4189380463477,11.0095675635285));
#46733=CARTESIAN_POINT('Ctrl Pts',(-26.6529040089133,24.4218490631799,11.0093820029019));
#46734=CARTESIAN_POINT('Ctrl Pts',(-26.6511948878978,24.4279112312635,11.008995141789));
#46735=CARTESIAN_POINT('Ctrl Pts',(-26.6503013470046,24.4310621774152,11.0087938183256));
#46736=CARTESIAN_POINT('Ctrl Pts',(-26.647833162831,24.439715601717,11.0082402517437));
#46737=CARTESIAN_POINT('Ctrl Pts',(-26.6462486680147,24.4452152362473,11.0078876870998));
#46738=CARTESIAN_POINT('Ctrl Pts',(-26.6400779124813,24.4664208517994,11.0065253484169));
#46739=CARTESIAN_POINT('Ctrl Pts',(-26.6353867795628,24.4820958292839,11.005512147522));
#46740=CARTESIAN_POINT('Ctrl Pts',(-26.5530367622513,24.7498210546617,10.9880990312428));
#46741=CARTESIAN_POINT('Ctrl Pts',(-26.4448630840975,24.9913800011566,10.9706198347406));
#46742=CARTESIAN_POINT('Ctrl Pts',(-26.2859366488993,25.2543816848082,10.9498369250046));
#46743=CARTESIAN_POINT('Ctrl Pts',(-26.2625992944151,25.2912863593656,10.9468798659495));
#46744=CARTESIAN_POINT('Ctrl Pts',(-26.2156247034077,25.3623319768872,10.9411172406081));
#46745=CARTESIAN_POINT('Ctrl Pts',(-26.1920628593873,25.3965133464821,10.9383118960035));
#46746=CARTESIAN_POINT('Ctrl Pts',(-26.1049184440959,25.5178492167718,10.9282535880205));
#46747=CARTESIAN_POINT('Ctrl Pts',(-26.0376245589581,25.6022610579256,10.9210639760687));
#46748=CARTESIAN_POINT('Ctrl Pts',(-25.9361708697199,25.717179493118,10.9111594728993));
#46749=CARTESIAN_POINT('Ctrl Pts',(-25.9054058935783,25.7505779493756,10.9082661362026));
#46750=CARTESIAN_POINT('Ctrl Pts',(-25.8715133164393,25.7858460172218,10.9052053112538));
#46751=CARTESIAN_POINT('Ctrl Pts',(-25.8690789771374,25.7883708885998,10.9049861532107));
#46752=CARTESIAN_POINT('Ctrl Pts',(-25.8650516983214,25.7925343165894,10.9046247255665));
#46753=CARTESIAN_POINT('Ctrl Pts',(-25.8634611368485,25.7941751537577,10.9044822731369));
#46754=CARTESIAN_POINT('Ctrl Pts',(-25.8603536307343,25.797374068994,10.9042045338914));
#46755=CARTESIAN_POINT('Ctrl Pts',(-25.8588368522113,25.7989323057644,10.9040692342311));
#46756=CARTESIAN_POINT('Ctrl Pts',(-25.8561476054347,25.8016894691796,10.9038298194651));
#46757=CARTESIAN_POINT('Ctrl Pts',(-25.8549757850054,25.8028890093015,10.9037256544237));
#46758=CARTESIAN_POINT('Ctrl Pts',(-25.8524642776507,25.8054559157993,10.9035027408083));
#46759=CARTESIAN_POINT('Ctrl Pts',(-25.851124312352,25.8068229994438,10.9033840151966));
#46760=CARTESIAN_POINT('Ctrl Pts',(-25.8472330178103,25.8107859768783,10.90303982583));
#46761=CARTESIAN_POINT('Ctrl Pts',(-25.8446784973827,25.8133787541306,10.9028146137892));
#46762=CARTESIAN_POINT('Ctrl Pts',(-25.8331698918202,25.8250201995503,10.9018032732035));
#46763=CARTESIAN_POINT('Ctrl Pts',(-25.8241664720607,25.8340202564006,10.9010209941633));
#46764=CARTESIAN_POINT('Ctrl Pts',(-25.6686950401911,25.9876026669407,10.8876595817541));
#46765=CARTESIAN_POINT('Ctrl Pts',(-25.5087362051239,26.11790594733,10.8761215485457));
#46766=CARTESIAN_POINT('Ctrl Pts',(-25.2618465006103,26.282433071645,10.8595336611637));
#46767=CARTESIAN_POINT('Ctrl Pts',(-25.1841826202237,26.3295755775236,10.8544722590818));
#46768=CARTESIAN_POINT('Ctrl Pts',(-25.0053737376604,26.4280257865806,10.8429795710441));
#46769=CARTESIAN_POINT('Ctrl Pts',(-24.9033078126986,26.4774004814728,10.8365261831315));
#46770=CARTESIAN_POINT('Ctrl Pts',(-24.7415250626844,26.5453911254332,10.8262745970161));
#46771=CARTESIAN_POINT('Ctrl Pts',(-24.6835077975662,26.5678206243763,10.8225947878011));
#46772=CARTESIAN_POINT('Ctrl Pts',(-24.5935901079937,26.5996239168669,10.8168658955509));
#46773=CARTESIAN_POINT('Ctrl Pts',(-24.5621314372683,26.6102067955271,10.814856922907));
#46774=CARTESIAN_POINT('Ctrl Pts',(-24.5256591787038,26.621852347267,10.8125207108932));
#46775=CARTESIAN_POINT('Ctrl Pts',(-24.5207988998445,26.6233915296662,10.8122092450651));
#46776=CARTESIAN_POINT('Ctrl Pts',(-24.5115171479648,26.6263067156798,10.8116141520718));
#46777=CARTESIAN_POINT('Ctrl Pts',(-24.5070963177831,26.6276847363053,10.8113305919417));
#46778=CARTESIAN_POINT('Ctrl Pts',(-24.4994114225286,26.6300620412473,10.8108374516701));
#46779=CARTESIAN_POINT('Ctrl Pts',(-24.4961487031162,26.6310656788889,10.8106280148865));
#46780=CARTESIAN_POINT('Ctrl Pts',(-24.489866913102,26.6329870862517,10.8102246483926));
#46781=CARTESIAN_POINT('Ctrl Pts',(-24.4868480754787,26.6339056099207,10.81003074369));
#46782=CARTESIAN_POINT('Ctrl Pts',(-24.4797253601243,26.6360613715805,10.80957309905));
#46783=CARTESIAN_POINT('Ctrl Pts',(-24.4756203604392,26.6372948566969,10.8093092363698));
#46784=CARTESIAN_POINT('Ctrl Pts',(-24.4613798131291,26.6415429510651,10.80839348592));
#46785=CARTESIAN_POINT('Ctrl Pts',(-24.4512319810967,26.6445158377725,10.8077402341967));
#46786=CARTESIAN_POINT('Ctrl Pts',(-24.3300943885958,26.6793576112831,10.7999336184134));
#46787=CARTESIAN_POINT('Ctrl Pts',(-24.2174967936964,26.7052852637205,10.7925871131172));
#46788=CARTESIAN_POINT('Ctrl Pts',(-23.9625125640323,26.7497395096324,10.7757259857807));
#46789=CARTESIAN_POINT('Ctrl Pts',(-23.8197909062603,26.7649091401567,10.7661317973485));
#46790=CARTESIAN_POINT('Ctrl Pts',(-23.525300221796,26.7764586014372,10.746220511709));
#46791=CARTESIAN_POINT('Ctrl Pts',(-23.3738203884374,26.7717277280065,10.7359171482124));
#46792=CARTESIAN_POINT('Ctrl Pts',(-23.131986108612,26.7470607773478,10.7197917188221));
#46793=CARTESIAN_POINT('Ctrl Pts',(-23.0411702309593,26.7338618894257,10.7138135731468));
#46794=CARTESIAN_POINT('Ctrl Pts',(-22.9403154489346,26.7147767114425,10.7073497356995));
#46795=CARTESIAN_POINT('Ctrl Pts',(-22.9296086440722,26.7126942627053,10.7066657726361));
#46796=CARTESIAN_POINT('Ctrl Pts',(-22.9165103107795,26.7100775838797,10.7058319572611));
#46797=CARTESIAN_POINT('Ctrl Pts',(-22.9141087236917,26.7095949662245,10.7056791971631));
#46798=CARTESIAN_POINT('Ctrl Pts',(-22.9094608704415,26.7086554293309,10.705383792935));
#46799=CARTESIAN_POINT('Ctrl Pts',(-22.9072145379669,26.7081988510025,10.7052411294067));
#46800=CARTESIAN_POINT('Ctrl Pts',(-22.9031416539365,26.7073664909693,10.7049826587916));
#46801=CARTESIAN_POINT('Ctrl Pts',(-22.9013149473845,26.7069915218049,10.7048668054145));
#46802=CARTESIAN_POINT('Ctrl Pts',(-22.8976392891047,26.7062336918469,10.7046338325853));
#46803=CARTESIAN_POINT('Ctrl Pts',(-22.8957903558574,26.7058507932106,10.7045167158806));
#46804=CARTESIAN_POINT('Ctrl Pts',(-22.890505250952,26.7047514473032,10.7041821497165));
#46805=CARTESIAN_POINT('Ctrl Pts',(-22.8870698982306,26.7040310080581,10.7039649303278));
#46806=CARTESIAN_POINT('Ctrl Pts',(-22.8722933418599,26.7009069556398,10.703031652652));
#46807=CARTESIAN_POINT('Ctrl Pts',(-22.8609637921499,26.6984477298026,10.7023187554815));
#46808=CARTESIAN_POINT('Ctrl Pts',(-22.6664534247087,26.6551263638781,10.6901215307164));
#46809=CARTESIAN_POINT('Ctrl Pts',(-22.4871424159341,26.5983932464084,10.6795096899166));
#46810=CARTESIAN_POINT('Ctrl Pts',(-22.2326864821954,26.4926743659886,10.6640744991824));
#46811=CARTESIAN_POINT('Ctrl Pts',(-22.1530436379315,26.4556996817807,10.6591872317164));
#46812=CARTESIAN_POINT('Ctrl Pts',(-22.0750358939633,26.4155367120613,10.654266819213));
#46813=CARTESIAN_POINT('Ctrl Pts',(-22.0750360597002,26.4155367973924,10.4044010236784));
#46814=CARTESIAN_POINT('Ctrl Pts',(-22.1193205426974,26.4383370478085,10.4073465105658));
#46815=CARTESIAN_POINT('Ctrl Pts',(-22.1641340840807,26.4601108885803,10.4103249860603));
#46816=CARTESIAN_POINT('Ctrl Pts',(-22.2272148220196,26.4889717770413,10.4145229535466));
#46817=CARTESIAN_POINT('Ctrl Pts',(-22.2450615811766,26.4969415449219,10.4157112079245));
#46818=CARTESIAN_POINT('Ctrl Pts',(-22.2684346000349,26.5071251634973,10.4172685149745));
#46819=CARTESIAN_POINT('Ctrl Pts',(-22.2738963127654,26.5094868536566,10.4176324983703));
#46820=CARTESIAN_POINT('Ctrl Pts',(-22.282755360233,26.5132884913216,10.4182230275066));
#46821=CARTESIAN_POINT('Ctrl Pts',(-22.2861486995844,26.5147377617422,10.4184492545082));
#46822=CARTESIAN_POINT('Ctrl Pts',(-22.2926480336091,26.5175003914179,10.41888261756));
#46823=CARTESIAN_POINT('Ctrl Pts',(-22.2957536172038,26.5188147102654,10.4190897205461));
#46824=CARTESIAN_POINT('Ctrl Pts',(-22.3028164643854,26.5217907262478,10.4195607905982));
#46825=CARTESIAN_POINT('Ctrl Pts',(-22.3067749900918,26.5234493948298,10.419824860338));
#46826=CARTESIAN_POINT('Ctrl Pts',(-22.3171607582342,26.5277767838768,10.4205178185527));
#46827=CARTESIAN_POINT('Ctrl Pts',(-22.3235933266464,26.5304325912819,10.4209471449073));
#46828=CARTESIAN_POINT('Ctrl Pts',(-22.3563854140118,26.5438472681685,10.4231364998463));
#46829=CARTESIAN_POINT('Ctrl Pts',(-22.3828774004522,26.5542770588902,10.4249076292453));
#46830=CARTESIAN_POINT('Ctrl Pts',(-22.4159562274997,26.5667964249225,10.4271227406175));
#46831=CARTESIAN_POINT('Ctrl Pts',(-22.4224168149728,26.5692178776985,10.4275555406217));
#46832=CARTESIAN_POINT('Ctrl Pts',(-22.435254856928,26.5739826636259,10.4284159179758));
#46833=CARTESIAN_POINT('Ctrl Pts',(-22.4416320463025,26.576326612697,10.4288434722868));
#46834=CARTESIAN_POINT('Ctrl Pts',(-22.4499557401983,26.579356160111,10.4294017549609));
#46835=CARTESIAN_POINT('Ctrl Pts',(-22.451895593106,26.5800600926604,10.4295318798039));
#46836=CARTESIAN_POINT('Ctrl Pts',(-22.4562297950958,26.5816281755203,10.4298226529442));
#46837=CARTESIAN_POINT('Ctrl Pts',(-22.458624492687,26.5824913525278,10.4299833330185));
#46838=CARTESIAN_POINT('Ctrl Pts',(-22.4675138354534,26.5856836515596,10.4305798841966));
#46839=CARTESIAN_POINT('Ctrl Pts',(-22.4740148972478,26.5879947394533,10.4310163426224));
#46840=CARTESIAN_POINT('Ctrl Pts',(-22.4854565980335,26.5920208550813,10.4317848231876));
#46841=CARTESIAN_POINT('Ctrl Pts',(-22.4903941007061,26.5937447724024,10.4321165560944));
#46842=CARTESIAN_POINT('Ctrl Pts',(-22.4991216841054,26.5967681737169,10.4327031203373));
#46843=CARTESIAN_POINT('Ctrl Pts',(-22.5029100424305,26.5980726257605,10.4329577916154));
#46844=CARTESIAN_POINT('Ctrl Pts',(-22.5109660506878,26.6008297715119,10.4334994891419));
#46845=CARTESIAN_POINT('Ctrl Pts',(-22.5152343324541,26.6022805808135,10.4337865747312));
#46846=CARTESIAN_POINT('Ctrl Pts',(-22.5368410822363,26.6095742798648,10.4352402580337));
#46847=CARTESIAN_POINT('Ctrl Pts',(-22.5542257713685,26.6152783058002,10.436411216724));
#46848=CARTESIAN_POINT('Ctrl Pts',(-22.6258978182909,26.6381201973344,10.4412442716266));
#46849=CARTESIAN_POINT('Ctrl Pts',(-22.6805836184896,26.6539654267989,10.4449451334664));
#46850=CARTESIAN_POINT('Ctrl Pts',(-22.9574715594903,26.7263015817659,10.4637409459603));
#46851=CARTESIAN_POINT('Ctrl Pts',(-23.1848233839031,26.7604113079534,10.4794217523819));
#46852=CARTESIAN_POINT('Ctrl Pts',(-23.4933401491112,26.7734824375079,10.5001691331206));
#46853=CARTESIAN_POINT('Ctrl Pts',(-23.5729483528909,26.7739051974754,10.5054683205015));
#46854=CARTESIAN_POINT('Ctrl Pts',(-23.7091539135128,26.7695818683568,10.5143616640604));
#46855=CARTESIAN_POINT('Ctrl Pts',(-23.7657598625508,26.7662886911308,10.5180060663949));
#46856=CARTESIAN_POINT('Ctrl Pts',(-23.8319812801346,26.7606795724336,10.5221865443536));
#46857=CARTESIAN_POINT('Ctrl Pts',(-23.8417054408293,26.7598113922279,10.5227983121976));
#46858=CARTESIAN_POINT('Ctrl Pts',(-23.8543124063815,26.7586280648666,10.5235885783629));
#46859=CARTESIAN_POINT('Ctrl Pts',(-23.8571988046419,26.7583532088762,10.5237693169769));
#46860=CARTESIAN_POINT('Ctrl Pts',(-23.862163819886,26.7578736554042,10.5240798730951));
#46861=CARTESIAN_POINT('Ctrl Pts',(-23.8642426096241,26.7576708324453,10.5242097964911));
#46862=CARTESIAN_POINT('Ctrl Pts',(-23.8681884490219,26.7572819726916,10.524456213007));
#46863=CARTESIAN_POINT('Ctrl Pts',(-23.8700555195376,26.7570963276929,10.5245727271784));
#46864=CARTESIAN_POINT('Ctrl Pts',(-23.8743284972309,26.7566676917167,10.5248391909866));
#46865=CARTESIAN_POINT('Ctrl Pts',(-23.8767342904402,26.7564236236914,10.5249890786598));
#46866=CARTESIAN_POINT('Ctrl Pts',(-23.8841326964325,26.7556646408158,10.5254496015725));
#46867=CARTESIAN_POINT('Ctrl Pts',(-23.8891244133734,26.7551407672375,10.5257597308031));
#46868=CARTESIAN_POINT('Ctrl Pts',(-23.9265426620332,26.7511253763653,10.5280802195263));
#46869=CARTESIAN_POINT('Ctrl Pts',(-23.9589172322387,26.7471533108994,10.5300639254062));
#46870=CARTESIAN_POINT('Ctrl Pts',(-23.9997695085673,26.7415103416319,10.5325430043859));
#46871=CARTESIAN_POINT('Ctrl Pts',(-24.0083069195981,26.7402961212035,10.5330597542648));
#46872=CARTESIAN_POINT('Ctrl Pts',(-24.0202422753242,26.7385497309103,10.5337804350534));
#46873=CARTESIAN_POINT('Ctrl Pts',(-24.0236443184346,26.7380463779289,10.5339856594312));
#46874=CARTESIAN_POINT('Ctrl Pts',(-24.036553864194,26.7361152103764,10.5347636841201));
#46875=CARTESIAN_POINT('Ctrl Pts',(-24.0460558600688,26.7346502859263,10.5353348434018));
#46876=CARTESIAN_POINT('Ctrl Pts',(-24.0597309324058,26.7324793041945,10.5361548628734));
#46877=CARTESIAN_POINT('Ctrl Pts',(-24.0639093088402,26.7318075269824,10.5364051506095));
#46878=CARTESIAN_POINT('Ctrl Pts',(-24.0755404240493,26.7299140275347,10.5371011498845));
#46879=CARTESIAN_POINT('Ctrl Pts',(-24.082990250518,26.7286743291875,10.5375461277499));
#46880=CARTESIAN_POINT('Ctrl Pts',(-24.3552167058685,26.6823901190218,10.553778604314));
#46881=CARTESIAN_POINT('Ctrl Pts',(-24.6133561284165,26.6044456608113,10.5682945159859));
#46882=CARTESIAN_POINT('Ctrl Pts',(-24.9741050930122,26.4441542242742,10.5906675811731));
#46883=CARTESIAN_POINT('Ctrl Pts',(-25.086241183986,26.386228049148,10.597937183782));
#46884=CARTESIAN_POINT('Ctrl Pts',(-25.2407077058277,26.2945816238037,10.608616431837));
#46885=CARTESIAN_POINT('Ctrl Pts',(-25.2860378547698,26.2661372228601,10.6118364751075));
#46886=CARTESIAN_POINT('Ctrl Pts',(-25.3373605461971,26.2321226945501,10.6155905935662));
#46887=CARTESIAN_POINT('Ctrl Pts',(-25.3440673240266,26.2276413930406,10.6160833476486));
#46888=CARTESIAN_POINT('Ctrl Pts',(-25.3542007261504,26.2208153400088,10.6168311839908));
#46889=CARTESIAN_POINT('Ctrl Pts',(-25.3576397937218,26.2184890441195,10.6170855672015));
#46890=CARTESIAN_POINT('Ctrl Pts',(-25.3638194686595,26.2142914841526,10.6175437240084));
#46891=CARTESIAN_POINT('Ctrl Pts',(-25.3665617039221,26.2124226175113,10.6177474063336));
#46892=CARTESIAN_POINT('Ctrl Pts',(-25.3724409983222,26.2084024942934,10.6181849049041));
#46893=CARTESIAN_POINT('Ctrl Pts',(-25.3755771425727,26.2062499142798,10.6184187713607));
#46894=CARTESIAN_POINT('Ctrl Pts',(-25.3840287715977,26.2004268639372,10.6190503627662));
#46895=CARTESIAN_POINT('Ctrl Pts',(-25.3893370231811,26.1967459704757,10.6194484854597));
#46896=CARTESIAN_POINT('Ctrl Pts',(-25.4128051485247,26.1803677980986,10.6212150229026));
#46897=CARTESIAN_POINT('Ctrl Pts',(-25.4308445053855,26.1674996262599,10.6225899858126));
#46898=CARTESIAN_POINT('Ctrl Pts',(-25.4590045418694,26.1469705348221,10.6247638075597));
#46899=CARTESIAN_POINT('Ctrl Pts',(-25.4692153385196,26.1394339395328,10.6255578019092));
#46900=CARTESIAN_POINT('Ctrl Pts',(-25.48384435046,26.1285021866681,10.6267037509748));
#46901=CARTESIAN_POINT('Ctrl Pts',(-25.4882987847766,26.1251555056441,10.6270538136856));
#46902=CARTESIAN_POINT('Ctrl Pts',(-25.4942910263318,26.1206290897798,10.6275262572224));
#46903=CARTESIAN_POINT('Ctrl Pts',(-25.4958365000501,26.119459479575,10.6276482437869));
#46904=CARTESIAN_POINT('Ctrl Pts',(-25.5011850377363,26.1154041276422,10.6280708887614));
#46905=CARTESIAN_POINT('Ctrl Pts',(-25.5049827301577,26.1125113406648,10.628371820904));
#46906=CARTESIAN_POINT('Ctrl Pts',(-25.512193752647,26.1069931817093,10.6289448235678));
#46907=CARTESIAN_POINT('Ctrl Pts',(-25.5156082787859,26.1043693835626,10.6292168325383));
#46908=CARTESIAN_POINT('Ctrl Pts',(-25.7693656019002,25.9085664321569,10.6494827619479));
#46909=CARTESIAN_POINT('Ctrl Pts',(-25.9898799248703,25.6796275058191,10.6710531817898));
#46910=CARTESIAN_POINT('Ctrl Pts',(-26.2159666206192,25.3628290157788,10.6972403813263));
#46911=CARTESIAN_POINT('Ctrl Pts',(-26.2564101777454,25.3018737823719,10.7021247957741));
#46912=CARTESIAN_POINT('Ctrl Pts',(-26.330673999434,25.1812251084219,10.711431704681));
#46913=CARTESIAN_POINT('Ctrl Pts',(-26.3647334297483,25.1217212647439,10.7158616098211));
#46914=CARTESIAN_POINT('Ctrl Pts',(-26.4020327215134,25.0514482184307,10.720871905912));
#46915=CARTESIAN_POINT('Ctrl Pts',(-26.407143879593,25.0416983321162,10.721562209142));
#46916=CARTESIAN_POINT('Ctrl Pts',(-26.4137228852048,25.0289905058272,10.7224554743431));
#46917=CARTESIAN_POINT('Ctrl Pts',(-26.4152362053574,25.0260563843297,10.7226612751403));
#46918=CARTESIAN_POINT('Ctrl Pts',(-26.4176823371621,25.0212957259895,10.7229944612503));
#46919=CARTESIAN_POINT('Ctrl Pts',(-26.4186179136438,25.0194706245782,10.7231220219795));
#46920=CARTESIAN_POINT('Ctrl Pts',(-26.4204107340502,25.0159649915479,10.7233667045886));
#46921=CARTESIAN_POINT('Ctrl Pts',(-26.4212682420495,25.0142846052599,10.7234838428938));
#46922=CARTESIAN_POINT('Ctrl Pts',(-26.4232366796763,25.0104188434356,10.723752984353));
#46923=CARTESIAN_POINT('Ctrl Pts',(-26.4243465942659,25.0082329472304,10.7239049228347));
#46924=CARTESIAN_POINT('Ctrl Pts',(-26.427861087235,25.0012917998977,10.7243866132169));
#46925=CARTESIAN_POINT('Ctrl Pts',(-26.4302563826072,24.9965318188587,10.7247157799964));
#46926=CARTESIAN_POINT('Ctrl Pts',(-26.4505543853361,24.9559448160244,10.7275128223617));
#46927=CARTESIAN_POINT('Ctrl Pts',(-26.4678005921399,24.9197908905198,10.7299403045388));
#46928=CARTESIAN_POINT('Ctrl Pts',(-26.4874246138234,24.8765979924787,10.7327761600183));
#46929=CARTESIAN_POINT('Ctrl Pts',(-26.4904568500345,24.8698625838511,10.733216548521));
#46930=CARTESIAN_POINT('Ctrl Pts',(-26.4953538726103,24.8588843103488,10.7339314750054));
#46931=CARTESIAN_POINT('Ctrl Pts',(-26.4972326937314,24.8546477806102,10.7342066710095));
#46932=CARTESIAN_POINT('Ctrl Pts',(-26.5005965272106,24.8470183499256,10.7347010389309));
#46933=CARTESIAN_POINT('Ctrl Pts',(-26.5020848380141,24.8436269225083,10.7349203609288));
#46934=CARTESIAN_POINT('Ctrl Pts',(-26.5068051507016,24.8328201154468,10.7356178742657));
#46935=CARTESIAN_POINT('Ctrl Pts',(-26.5100151038521,24.8253950784762,10.7360950824805));
#46936=CARTESIAN_POINT('Ctrl Pts',(-26.5154403691719,24.8127148769824,10.7369067091626));
#46937=CARTESIAN_POINT('Ctrl Pts',(-26.517669735719,24.8074658082807,10.7372417187417));
#46938=CARTESIAN_POINT('Ctrl Pts',(-26.6423305341338,24.5117716309108,10.7560606869111));
#46939=CARTESIAN_POINT('Ctrl Pts',(-26.7215171657011,24.2049209831682,10.7728769383046));
#46940=CARTESIAN_POINT('Ctrl Pts',(-26.7669477794599,23.7781923874672,10.7975975107917));
#46941=CARTESIAN_POINT('Ctrl Pts',(-26.7729918350825,23.664410071898,10.8042939311957));
#46942=CARTESIAN_POINT('Ctrl Pts',(-26.7730042922185,23.5316397438179,10.8123301618297));
#46943=CARTESIAN_POINT('Ctrl Pts',(-26.7728395399343,23.5127252562369,10.8134801487195));
#46944=CARTESIAN_POINT('Ctrl Pts',(-26.7724019798592,23.4877437228323,10.8150061420369));
#46945=CARTESIAN_POINT('Ctrl Pts',(-26.7722785130801,23.4816741679591,10.8153774560738));
#46946=CARTESIAN_POINT('Ctrl Pts',(-26.7720604153553,23.4722607802433,10.8159542085373));
#46947=CARTESIAN_POINT('Ctrl Pts',(-26.7719777261741,23.4689166624007,10.8161592717701));
#46948=CARTESIAN_POINT('Ctrl Pts',(-26.7718018979418,23.4622272924601,10.8165698126992));
#46949=CARTESIAN_POINT('Ctrl Pts',(-26.7717087545637,23.4588820445849,10.8167752902833));
#46950=CARTESIAN_POINT('Ctrl Pts',(-26.7714894222586,23.4514223648541,10.8172338790897));
#46951=CARTESIAN_POINT('Ctrl Pts',(-26.7713605607507,23.4473080228201,10.8174870739362));
#46952=CARTESIAN_POINT('Ctrl Pts',(-26.7709615119465,23.4353022146965,10.8182266796868));
#46953=CARTESIAN_POINT('Ctrl Pts',(-26.7706702057895,23.4274115228575,10.8187137532332));
#46954=CARTESIAN_POINT('Ctrl Pts',(-26.7683558721294,23.3704058504887,10.8222397268425));
#46955=CARTESIAN_POINT('Ctrl Pts',(-26.7652384447557,23.3213440657745,10.8253128546951));
#46956=CARTESIAN_POINT('Ctrl Pts',(-26.7515547946116,23.1632358242845,10.8353482890459));
#46957=CARTESIAN_POINT('Ctrl Pts',(-26.7365517066242,23.0546606992704,10.8424460772234));
#46958=CARTESIAN_POINT('Ctrl Pts',(-26.6517514213579,22.6095874427737,10.8723660718261));
#46959=CARTESIAN_POINT('Ctrl Pts',(-26.5339142093063,22.2845969694627,10.8964658368068));
#46960=CARTESIAN_POINT('Ctrl Pts',(-26.366111136449,21.9827509351699,10.9182929659547));
#46961=CARTESIAN_POINT('Ctrl Pts',(-26.3652171858749,21.9811461194928,10.918408988645));
#46962=CARTESIAN_POINT('Ctrl Pts',(-26.3579201043826,21.9680727405011,10.9193539403912));
#46963=CARTESIAN_POINT('Ctrl Pts',(-26.3514481573238,21.9566424252233,10.9201788198388));
#46964=CARTESIAN_POINT('Ctrl Pts',(-26.3430933292041,21.9420948604869,10.9212266639652));
#46965=CARTESIAN_POINT('Ctrl Pts',(-26.3412749239718,21.9389410094193,10.9214537117862));
#46966=CARTESIAN_POINT('Ctrl Pts',(-26.3383751043843,21.9339311848979,10.9218141723359));
#46967=CARTESIAN_POINT('Ctrl Pts',(-26.3372971787775,21.9320732116921,10.9219478110332));
#46968=CARTESIAN_POINT('Ctrl Pts',(-26.3352788946983,21.9286023827981,10.9221973738033));
#46969=CARTESIAN_POINT('Ctrl Pts',(-26.3343389986212,21.9269892773994,10.9223133265918));
#46970=CARTESIAN_POINT('Ctrl Pts',(-26.3322257255409,21.92336958743,10.9225734401239));
#46971=CARTESIAN_POINT('Ctrl Pts',(-26.3310515815791,21.9213634593935,10.9227175496632));
#46972=CARTESIAN_POINT('Ctrl Pts',(-26.3275697259718,21.9154291403167,10.9231436900396));
#46973=CARTESIAN_POINT('Ctrl Pts',(-26.3252558415842,21.9115045494437,10.9234253187858));
#46974=CARTESIAN_POINT('Ctrl Pts',(-26.30694306519,21.8805941654071,10.9256420236892));
#46975=CARTESIAN_POINT('Ctrl Pts',(-26.2905585161613,21.8538371792182,10.9275522935291));
#46976=CARTESIAN_POINT('Ctrl Pts',(-26.2303257019679,21.7586237747518,10.9343347808559));
#46977=CARTESIAN_POINT('Ctrl Pts',(-26.1842788308701,21.6915881067284,10.939081791127));
#46978=CARTESIAN_POINT('Ctrl Pts',(-25.933327282883,21.3543380577292,10.9632052931394));
#46979=CARTESIAN_POINT('Ctrl Pts',(-25.6892621821821,21.1159666817246,10.9813393152816));
#46980=CARTESIAN_POINT('Ctrl Pts',(-25.3619883516068,20.8842514604203,11.0050733469101));
#46981=CARTESIAN_POINT('Ctrl Pts',(-25.3104570614142,20.8499511381906,11.0087869537192));
#46982=CARTESIAN_POINT('Ctrl Pts',(-25.2502143429537,20.8123096734548,11.0131145769786));
#46983=CARTESIAN_POINT('Ctrl Pts',(-25.2424354267687,20.8074951050111,11.013673121141));
#46984=CARTESIAN_POINT('Ctrl Pts',(-25.2309500962642,20.8004540022255,11.0144974441474));
#46985=CARTESIAN_POINT('Ctrl Pts',(-25.2272594841021,20.7982016714254,11.0147622730543));
#46986=CARTESIAN_POINT('Ctrl Pts',(-25.2206784524905,20.7942035103438,11.0152344215391));
#46987=CARTESIAN_POINT('Ctrl Pts',(-25.217789795141,20.7924547798942,11.0154416342804));
#46988=CARTESIAN_POINT('Ctrl Pts',(-25.2117523350789,20.7888127866905,11.0158746595001));
#46989=CARTESIAN_POINT('Ctrl Pts',(-25.208603034014,20.7869203632405,11.0161005023257));
#46990=CARTESIAN_POINT('Ctrl Pts',(-25.2005060204981,20.7820736731648,11.01668107053));
#46991=CARTESIAN_POINT('Ctrl Pts',(-25.1955536235319,20.7791272933432,11.0170360834278));
#46992=CARTESIAN_POINT('Ctrl Pts',(-25.17472592127,20.7668115714036,11.0185288004902));
#46993=CARTESIAN_POINT('Ctrl Pts',(-25.1587785284803,20.7575653906418,11.0196709754918));
#46994=CARTESIAN_POINT('Ctrl Pts',(-25.0501767987787,20.6958377310961,11.0274450676712));
#46995=CARTESIAN_POINT('Ctrl Pts',(-24.9550595855672,20.6478449917616,11.0342370429734));
#46996=CARTESIAN_POINT('Ctrl Pts',(-24.6216720757171,20.4998604764889,11.0580095661414));
#46997=CARTESIAN_POINT('Ctrl Pts',(-24.3738676499993,20.4238395764081,11.075713600696));
#46998=CARTESIAN_POINT('Ctrl Pts',(-24.0182666590555,20.3600016010271,11.099944426748));
#46999=CARTESIAN_POINT('Ctrl Pts',(-23.9160064393972,20.3466660557287,11.1067671732972));
#47000=CARTESIAN_POINT('Ctrl Pts',(-23.8068900658058,20.3377308165948,11.1137817078811));
#47001=CARTESIAN_POINT('Ctrl Pts',(-23.8005042582184,20.3372270620292,11.1141912508643));
#47002=CARTESIAN_POINT('Ctrl Pts',(-23.7680106938155,20.334761215262,11.1162701057945));
#47003=CARTESIAN_POINT('Ctrl Pts',(-23.7418802450931,20.3330982068341,11.1179252409949));
#47004=CARTESIAN_POINT('Ctrl Pts',(-23.7111052525198,20.3315159126458,11.1198527378459));
#47005=CARTESIAN_POINT('Ctrl Pts',(-23.7064785322951,20.3312880308064,11.1201419379402));
#47006=CARTESIAN_POINT('Ctrl Pts',(-23.699482134913,20.3309585542162,11.120578364503));
#47007=CARTESIAN_POINT('Ctrl Pts',(-23.6971128357321,20.3308495996138,11.1207260034949));
#47008=CARTESIAN_POINT('Ctrl Pts',(-23.6928741737281,20.3306593693827,11.1209898489777));
#47009=CARTESIAN_POINT('Ctrl Pts',(-23.6910048629802,20.3305771063009,11.1211061111608));
#47010=CARTESIAN_POINT('Ctrl Pts',(-23.6870214550233,20.330405283536,11.1213536518209));
#47011=CARTESIAN_POINT('Ctrl Pts',(-23.6849073466448,20.3303161781721,11.1214849040573));
#47012=CARTESIAN_POINT('Ctrl Pts',(-23.6792762860326,20.3300843959338,11.121834174255));
#47013=CARTESIAN_POINT('Ctrl Pts',(-23.6757591726004,20.3299453980314,11.1220519843567));
#47014=CARTESIAN_POINT('Ctrl Pts',(-23.6598828113058,20.3293440063675,11.1230336746236));
#47015=CARTESIAN_POINT('Ctrl Pts',(-23.6475209755071,20.3289469907293,11.1237939157647));
#47016=CARTESIAN_POINT('Ctrl Pts',(-23.3398233638043,20.3208377826917,11.1426209465618));
#47017=CARTESIAN_POINT('Ctrl Pts',(-23.044764394644,20.3536996662269,11.1585619801404));
#47018=CARTESIAN_POINT('Ctrl Pts',(-22.562375509171,20.4759948893336,11.1865701098311));
#47019=CARTESIAN_POINT('Ctrl Pts',(-22.3716127846577,20.5439673165184,11.198189196753));
#47020=CARTESIAN_POINT('Ctrl Pts',(-22.1770695567283,20.6346660176577,11.2112325393831));
#47021=CARTESIAN_POINT('Ctrl Pts',(-22.1656853732181,20.6400549473063,11.212000193099));
#47022=CARTESIAN_POINT('Ctrl Pts',(-22.1501699822298,20.6475111115298,11.2130525362298));
#47023=CARTESIAN_POINT('Ctrl Pts',(-22.1460110904959,20.6495207495204,11.2133352196204));
#47024=CARTESIAN_POINT('Ctrl Pts',(-22.1389386603159,20.6529570267536,11.2138169725945));
#47025=CARTESIAN_POINT('Ctrl Pts',(-22.1360229204009,20.6543791413472,11.2140158840542));
#47026=CARTESIAN_POINT('Ctrl Pts',(-22.1303863302755,20.6571388587126,11.2144009943718));
#47027=CARTESIAN_POINT('Ctrl Pts',(-22.1276652100543,20.6584759035752,11.2145871735325));
#47028=CARTESIAN_POINT('Ctrl Pts',(-22.1212108481018,20.6616586224197,11.2150294087414));
#47029=CARTESIAN_POINT('Ctrl Pts',(-22.117479296067,20.6635076934459,11.2152855836179));
#47030=CARTESIAN_POINT('Ctrl Pts',(-22.106622030793,20.668913959275,11.2160324074876));
#47031=CARTESIAN_POINT('Ctrl Pts',(-22.0995059448409,20.672490322798,11.2165237290734));
#47032=CARTESIAN_POINT('Ctrl Pts',(-22.0492942806905,20.6979589992145,11.2200036452253));
#47033=CARTESIAN_POINT('Ctrl Pts',(-22.0066847483304,20.7207910715358,11.2230252918054));
#47034=CARTESIAN_POINT('Ctrl Pts',(-21.8712287535633,20.7973447738146,11.232861540725));
#47035=CARTESIAN_POINT('Ctrl Pts',(-21.7805531745613,20.8547410774885,11.2398057705441));
#47036=CARTESIAN_POINT('Ctrl Pts',(-21.5112825753855,21.044635552459,11.2615442665771));
#47037=CARTESIAN_POINT('Ctrl Pts',(-21.3433958056176,21.1911672127142,11.2767580163808));
#47038=CARTESIAN_POINT('Ctrl Pts',(-21.123220882442,21.427565283442,11.298431053134));
#47039=CARTESIAN_POINT('Ctrl Pts',(-21.0579955317232,21.5045393291019,11.3051116739332));
#47040=CARTESIAN_POINT('Ctrl Pts',(-20.9749119951168,21.612473094337,11.3138584273169));
#47041=CARTESIAN_POINT('Ctrl Pts',(-20.9538036052451,21.6408491545473,11.316103349588));
#47042=CARTESIAN_POINT('Ctrl Pts',(-20.9304642500541,21.6733272938328,11.3186064207481));
#47043=CARTESIAN_POINT('Ctrl Pts',(-20.9277710722804,21.6770921048202,11.3188955787177));
#47044=CARTESIAN_POINT('Ctrl Pts',(-20.9237091294605,21.6827962529714,11.3193321707757));
#47045=CARTESIAN_POINT('Ctrl Pts',(-20.922334394684,21.6847313010402,11.3194800148158));
#47046=CARTESIAN_POINT('Ctrl Pts',(-20.9199481615072,21.6880979851151,11.3197367804938));
#47047=CARTESIAN_POINT('Ctrl Pts',(-20.9189356934341,21.6895289273153,11.3198457694407));
#47048=CARTESIAN_POINT('Ctrl Pts',(-20.9168193779014,21.6925251416988,11.320073675853));
#47049=CARTESIAN_POINT('Ctrl Pts',(-20.9157157590044,21.6940905709804,11.3201925770772));
#47050=CARTESIAN_POINT('Ctrl Pts',(-20.9130804753147,21.6978356767414,11.3204766236543));
#47051=CARTESIAN_POINT('Ctrl Pts',(-20.9115501118055,21.7000162768179,11.3206416786789));
#47052=CARTESIAN_POINT('Ctrl Pts',(-20.9064956385073,21.7072373722328,11.3211871726917));
#47053=CARTESIAN_POINT('Ctrl Pts',(-20.9029832259414,21.7122860976772,11.3215668100693));
#47054=CARTESIAN_POINT('Ctrl Pts',(-20.8572168639281,21.7784738163158,11.3265213354453));
#47055=CARTESIAN_POINT('Ctrl Pts',(-20.8170716272202,21.8410523870443,11.3309558503844));
#47056=CARTESIAN_POINT('Ctrl Pts',(-20.7428373173508,21.9660842622704,11.3394532427876));
#47057=CARTESIAN_POINT('Ctrl Pts',(-20.708581479622,22.0283865777841,11.3435215609221));
#47058=CARTESIAN_POINT('Ctrl Pts',(-20.5865759381276,22.268790780818,11.3587887783013));
#47059=CARTESIAN_POINT('Ctrl Pts',(-20.5132867138653,22.4537287950224,11.3696886034136));
#47060=CARTESIAN_POINT('Ctrl Pts',(-20.4365050382738,22.715830816055,11.3852170045572));
#47061=CARTESIAN_POINT('Ctrl Pts',(-20.4180253173361,22.7881273754,11.389504704196));
#47062=CARTESIAN_POINT('Ctrl Pts',(-20.3960161591698,22.8886544166408,11.3955162303357));
#47063=CARTESIAN_POINT('Ctrl Pts',(-20.3903257736931,22.9163897894362,11.3971798505208));
#47064=CARTESIAN_POINT('Ctrl Pts',(-20.3829315106859,22.9550077974361,11.3995051305546));
#47065=CARTESIAN_POINT('Ctrl Pts',(-20.3809167770313,22.9658300699515,11.4001577289162));
#47066=CARTESIAN_POINT('Ctrl Pts',(-20.3694607810698,23.0291685723939,11.4039831900359));
#47067=CARTESIAN_POINT('Ctrl Pts',(-20.3612699311525,23.0818999783438,11.407192541446));
#47068=CARTESIAN_POINT('Ctrl Pts',(-20.3532637072807,23.1434889050007,11.4109773372298));
#47069=CARTESIAN_POINT('Ctrl Pts',(-20.352170638663,23.1521741543488,11.4115119002514));
#47070=CARTESIAN_POINT('Ctrl Pts',(-20.3505943388137,23.1651247131689,11.4123102612106));
#47071=CARTESIAN_POINT('Ctrl Pts',(-20.3500842156329,23.1693867594534,11.4125732084622));
#47072=CARTESIAN_POINT('Ctrl Pts',(-20.3491895922107,23.1769899816446,11.4130426610465));
#47073=CARTESIAN_POINT('Ctrl Pts',(-20.348801803629,23.1803307704538,11.4132490621287));
#47074=CARTESIAN_POINT('Ctrl Pts',(-20.3479952982837,23.1873750526616,11.413684544795));
#47075=CARTESIAN_POINT('Ctrl Pts',(-20.3475777754212,23.1910786753729,11.4139136637805));
#47076=CARTESIAN_POINT('Ctrl Pts',(-20.3465054919453,23.2007408706978,11.4145118178363));
#47077=CARTESIAN_POINT('Ctrl Pts',(-20.3458609319735,23.206700540382,11.4148811745026));
#47078=CARTESIAN_POINT('Ctrl Pts',(-20.3430901333203,23.2330059648974,11.4165133322204));
#47079=CARTESIAN_POINT('Ctrl Pts',(-20.3411410514901,23.2533695408764,11.4177817100035));
#47080=CARTESIAN_POINT('Ctrl Pts',(-20.3365640804233,23.3065192858193,11.4211055253391));
#47081=CARTESIAN_POINT('Ctrl Pts',(-20.3342440660622,23.3393289039834,11.4231705260076));
#47082=CARTESIAN_POINT('Ctrl Pts',(-20.3261923031749,23.4848164055113,11.4323883093344));
#47083=CARTESIAN_POINT('Ctrl Pts',(-20.3258781914935,23.5977031345775,11.4397063093796));
#47084=CARTESIAN_POINT('Ctrl Pts',(-20.3402581377045,23.8867875778558,11.4588454321717));
#47085=CARTESIAN_POINT('Ctrl Pts',(-20.3635237126299,24.0621813067796,11.4708531778101));
#47086=CARTESIAN_POINT('Ctrl Pts',(-20.4261041984751,24.350091362431,11.4907547148228));
#47087=CARTESIAN_POINT('Ctrl Pts',(-20.4574882496792,24.4639583600217,11.4986707084414));
#47088=CARTESIAN_POINT('Ctrl Pts',(-20.4960111090153,24.5787154634658,11.5065434744349));
#47089=CARTESIAN_POINT('Ctrl Pts',(-20.4969755317072,24.5815750959363,11.5067395855296));
#47090=CARTESIAN_POINT('Ctrl Pts',(-20.5148614195832,24.6343639759012,11.5103584485964));
#47091=CARTESIAN_POINT('Ctrl Pts',(-20.5330027549045,24.6838756695719,11.5137303842427));
#47092=CARTESIAN_POINT('Ctrl Pts',(-20.5544602875104,24.7382674288478,11.5173925380823));
#47093=CARTESIAN_POINT('Ctrl Pts',(-20.5565828246385,24.743605896143,11.5177515165796));
#47094=CARTESIAN_POINT('Ctrl Pts',(-20.5595753913272,24.7510743744164,11.5182530562658));
#47095=CARTESIAN_POINT('Ctrl Pts',(-20.560433427811,24.7532091319125,11.5183963375356));
#47096=CARTESIAN_POINT('Ctrl Pts',(-20.5620072922888,24.7571127526465,11.5186581991264));
#47097=CARTESIAN_POINT('Ctrl Pts',(-20.5627224062121,24.7588819013278,11.5187768229576));
#47098=CARTESIAN_POINT('Ctrl Pts',(-20.5641778123513,24.7624733043297,11.5190175208003));
#47099=CARTESIAN_POINT('Ctrl Pts',(-20.5649182017018,24.7642955166523,11.51913958868));
#47100=CARTESIAN_POINT('Ctrl Pts',(-20.5667616070543,24.7688205383609,11.5194425736629));
#47101=CARTESIAN_POINT('Ctrl Pts',(-20.567866630913,24.7715225359368,11.5196233681407));
#47102=CARTESIAN_POINT('Ctrl Pts',(-20.571927881771,24.7814146979628,11.520284821565));
#47103=CARTESIAN_POINT('Ctrl Pts',(-20.5749064825798,24.7885957357251,11.5207641295584));
#47104=CARTESIAN_POINT('Ctrl Pts',(-20.6532720103714,24.9756102566819,11.5332259062039));
#47105=CARTESIAN_POINT('Ctrl Pts',(-20.7448136597775,25.1482760674421,11.5442416706843));
#47106=CARTESIAN_POINT('Ctrl Pts',(-20.9218719331134,25.4195700115963,11.5623837291471));
#47107=CARTESIAN_POINT('Ctrl Pts',(-20.998732905295,25.5231892641634,11.5695433776873));
#47108=CARTESIAN_POINT('Ctrl Pts',(-21.1975683583782,25.7601270344267,11.5870433995674));
#47109=CARTESIAN_POINT('Ctrl Pts',(-21.3249280914906,25.8883253830876,11.5974939427606));
#47110=CARTESIAN_POINT('Ctrl Pts',(-21.4712720927064,26.0127909935341,11.6091748308002));
#47111=CARTESIAN_POINT('Ctrl Pts',(-21.4802548692204,26.0203466621702,11.6098904997992));
#47112=CARTESIAN_POINT('Ctrl Pts',(-21.4927247472399,26.0307196393112,11.6108822580019));
#47113=CARTESIAN_POINT('Ctrl Pts',(-21.4961768271812,26.0335790618892,11.6111566278147));
#47114=CARTESIAN_POINT('Ctrl Pts',(-21.5021089114825,26.0384718867002,11.6116278006898));
#47115=CARTESIAN_POINT('Ctrl Pts',(-21.5045860130364,26.040508812074,11.6118244602784));
#47116=CARTESIAN_POINT('Ctrl Pts',(-21.5094211609765,26.0444726808201,11.6122081517916));
#47117=CARTESIAN_POINT('Ctrl Pts',(-21.5117789065443,26.0463999863699,11.6123951686996));
#47118=CARTESIAN_POINT('Ctrl Pts',(-21.5174409920382,26.0510150052697,11.6128440942085));
#47119=CARTESIAN_POINT('Ctrl Pts',(-21.5207479289139,26.0536995097655,11.6131061320981));
#47120=CARTESIAN_POINT('Ctrl Pts',(-21.5306060667776,26.0616697763789,11.6138868209155));
#47121=CARTESIAN_POINT('Ctrl Pts',(-21.5371726278454,26.0669364051107,11.6144062412082));
#47122=CARTESIAN_POINT('Ctrl Pts',(-21.5948479100937,26.1128239931345,11.6189633055014));
#47123=CARTESIAN_POINT('Ctrl Pts',(-21.6471561227556,26.1519063863036,11.6230618724274));
#47124=CARTESIAN_POINT('Ctrl Pts',(-21.7846427491397,26.2482646213656,11.6337598546252));
#47125=CARTESIAN_POINT('Ctrl Pts',(-21.8714303682177,26.3031055551097,11.6404444481765));
#47126=CARTESIAN_POINT('Ctrl Pts',(-21.9983872080542,26.3750906952972,11.6501127898601));
#47127=CARTESIAN_POINT('Ctrl Pts',(-22.036514291001,26.395703530941,11.6530024603944));
#47128=CARTESIAN_POINT('Ctrl Pts',(-22.0750360887345,26.4155368123409,11.6559056162233));
#47129=CARTESIAN_POINT('Origin',(-23.5502525316942,23.5502525316942,-77.3107734492734));
#47130=CARTESIAN_POINT('',(-22.0759547750155,26.4137025163195,13.1538544762661));
#47131=CARTESIAN_POINT('',(-22.0750360153462,26.4155367745564,12.9101997884793));
#47132=CARTESIAN_POINT('',(-22.0750360153461,26.4155367745563,-77.3107734492734));
#47133=CARTESIAN_POINT('',(-26.7732842589511,23.5513999092453,12.3107735328638));
#47134=CARTESIAN_POINT('Ctrl Pts',(-26.777835819343,23.5513797621693,12.3107748823706));
#47135=CARTESIAN_POINT('Ctrl Pts',(-26.7732053868241,22.5449087652806,12.3731671879169));
#47136=CARTESIAN_POINT('Ctrl Pts',(-25.7246919797972,20.4607039664501,12.5018551305882));
#47137=CARTESIAN_POINT('Ctrl Pts',(-22.1726033898576,19.9960316527802,12.6968387103845));
#47138=CARTESIAN_POINT('Ctrl Pts',(-19.8153491088126,22.7880848100881,12.8957256217594));
#47139=CARTESIAN_POINT('Ctrl Pts',(-20.6386024886415,25.4631247734142,13.0480642103866));
#47140=CARTESIAN_POINT('Ctrl Pts',(-21.7898377407983,26.26967571401,13.1341071618889));
#47141=CARTESIAN_POINT('Ctrl Pts',(-22.075954775016,26.4137025163198,13.1538544762662));
#47142=CARTESIAN_POINT('Ctrl Pts',(-22.075036015346,26.4155367745563,11.9036974267448));
#47143=CARTESIAN_POINT('Ctrl Pts',(-22.1633969361913,26.4610301632682,11.9098683281394));
#47144=CARTESIAN_POINT('Ctrl Pts',(-22.2540160014955,26.5025104832484,11.9160392295341));
#47145=CARTESIAN_POINT('Ctrl Pts',(-22.3464929848755,26.5397475586081,11.9222101309288));
#47146=CARTESIAN_POINT('Ctrl Pts',(-22.4388482208512,26.5769356107719,11.9283729082346));
#47147=CARTESIAN_POINT('Ctrl Pts',(-22.5330561135148,26.6098913611028,11.9345356855405));
#47148=CARTESIAN_POINT('Ctrl Pts',(-22.6286922229561,26.6384306612487,11.9406984628463));
#47149=CARTESIAN_POINT('Ctrl Pts',(-22.724230684154,26.6669408216423,11.9468549477133));
#47150=CARTESIAN_POINT('Ctrl Pts',(-22.8211940487476,26.6910433736225,11.9530114325802));
#47151=CARTESIAN_POINT('Ctrl Pts',(-22.9191391990101,26.7106027533957,11.9591679174471));
#47152=CARTESIAN_POINT('Ctrl Pts',(-23.0170178062356,26.7301488447055,11.9653202196547));
#47153=CARTESIAN_POINT('Ctrl Pts',(-23.115876448277,26.7451578151042,11.9714725218622));
#47154=CARTESIAN_POINT('Ctrl Pts',(-23.2152590673981,26.755544552927,11.9776248240697));
#47155=CARTESIAN_POINT('Ctrl Pts',(-23.3146074535599,26.7659277129736,11.9837750070787));
#47156=CARTESIAN_POINT('Ctrl Pts',(-23.414479026507,26.7716917590445,11.9899251900876));
#47157=CARTESIAN_POINT('Ctrl Pts',(-23.5144107150789,26.7728032181353,11.9960753730965));
#47158=CARTESIAN_POINT('Ctrl Pts',(-23.6143347162029,26.7739145917248,12.0022250829901));
#47159=CARTESIAN_POINT('Ctrl Pts',(-23.7143183893491,26.7703740852893,12.0083747928837));
#47160=CARTESIAN_POINT('Ctrl Pts',(-23.8138977699165,26.7622003442937,12.0145245027773));
#47161=CARTESIAN_POINT('Ctrl Pts',(-23.9134961303172,26.7540250453827,12.0206753848058));
#47162=CARTESIAN_POINT('Ctrl Pts',(-24.0126896121068,26.741214793225,12.0268262668344));
#47163=CARTESIAN_POINT('Ctrl Pts',(-24.1110194905167,26.7238400884496,12.0329771488629));
#47164=CARTESIAN_POINT('Ctrl Pts',(-24.2094564287027,26.706446466413,12.0391347278595));
#47165=CARTESIAN_POINT('Ctrl Pts',(-24.3070274576873,26.6844785452428,12.045292306856));
#47166=CARTESIAN_POINT('Ctrl Pts',(-24.4032843061283,26.6580579236558,12.0514498858525));
#47167=CARTESIAN_POINT('Ctrl Pts',(-24.4995978549259,26.6316217389303,12.0576110919876));
#47168=CARTESIAN_POINT('Ctrl Pts',(-24.5945952688175,26.6007277653805,12.0637722981227));
#47169=CARTESIAN_POINT('Ctrl Pts',(-24.6878456816555,26.5655467773129,12.0699335042578));
#47170=CARTESIAN_POINT('Ctrl Pts',(-24.7812484867023,26.5303082955751,12.0761047791935));
#47171=CARTESIAN_POINT('Ctrl Pts',(-24.8728981906794,26.4907689806387,12.0822760541292));
#47172=CARTESIAN_POINT('Ctrl Pts',(-24.9623860181702,26.4471468305724,12.0884473290649));
#47173=CARTESIAN_POINT('Ctrl Pts',(-25.0190868967554,26.4195071581847,12.0923575447965));
#47174=CARTESIAN_POINT('Ctrl Pts',(-25.0749203560244,26.3902292782621,12.0962677605281));
#47175=CARTESIAN_POINT('Ctrl Pts',(-25.1297884600919,26.3593776291935,12.1001779762598));
#47176=CARTESIAN_POINT('Ctrl Pts',(-25.2163951773887,26.3106797546373,12.1063500675721));
#47177=CARTESIAN_POINT('Ctrl Pts',(-25.3009002478314,26.2578871680822,12.1125221588844));
#47178=CARTESIAN_POINT('Ctrl Pts',(-25.3828907486128,26.2012060824735,12.1186942501967));
#47179=CARTESIAN_POINT('Ctrl Pts',(-25.4647701603715,26.1446017941322,12.1248579789355));
#47180=CARTESIAN_POINT('Ctrl Pts',(-25.5441414200523,26.084119723353,12.1310217076743));
#47181=CARTESIAN_POINT('Ctrl Pts',(-25.6206165445705,26.0200117136159,12.1371854364131));
#47182=CARTESIAN_POINT('Ctrl Pts',(-25.6970106508718,25.9559716202984,12.1433426352598));
#47183=CARTESIAN_POINT('Ctrl Pts',(-25.7705143907708,25.888313502488,12.1494998341065));
#47184=CARTESIAN_POINT('Ctrl Pts',(-25.8407699146686,25.8173316394433,12.1556570329531));
#47185=CARTESIAN_POINT('Ctrl Pts',(-25.9109740860388,25.746401659836,12.1618097312609));
#47186=CARTESIAN_POINT('Ctrl Pts',(-25.9779344571518,25.6721530729742,12.1679624295686));
#47187=CARTESIAN_POINT('Ctrl Pts',(-26.041328055983,25.5949188357128,12.1741151278763));
#47188=CARTESIAN_POINT('Ctrl Pts',(-26.1046976158714,25.517713885784,12.180265493072));
#47189=CARTESIAN_POINT('Ctrl Pts',(-26.1645028156326,25.4375258704559,12.1864158582678));
#47190=CARTESIAN_POINT('Ctrl Pts',(-26.2204598120355,25.3547221608408,12.1925662234635));
#47191=CARTESIAN_POINT('Ctrl Pts',(-26.276410559609,25.271927698081,12.1987159018358));
#47192=CARTESIAN_POINT('Ctrl Pts',(-26.32851371497,25.1865184816921,12.204865580208));
#47193=CARTESIAN_POINT('Ctrl Pts',(-26.3765283518551,25.0988914666541,12.2110152585802));
#47194=CARTESIAN_POINT('Ctrl Pts',(-26.4245504720781,25.0112507944774,12.2171658954127));
#47195=CARTESIAN_POINT('Ctrl Pts',(-26.4684825993837,24.9213920180873,12.2233165322451));
#47196=CARTESIAN_POINT('Ctrl Pts',(-26.508129901316,24.8297364232611,12.2294671690776));
#47197=CARTESIAN_POINT('Ctrl Pts',(-26.5478196175327,24.7379827762025,12.2356243857994));
#47198=CARTESIAN_POINT('Ctrl Pts',(-26.5832151820521,24.6444288717054,12.2417816025212));
#47199=CARTESIAN_POINT('Ctrl Pts',(-26.6141701071009,24.5495155869575,12.247938819243));
#47200=CARTESIAN_POINT('Ctrl Pts',(-26.6451423017755,24.4545493504767,12.2540994710509));
#47201=CARTESIAN_POINT('Ctrl Pts',(-26.6716688079092,24.3582226422454,12.2602601228587));
#47202=CARTESIAN_POINT('Ctrl Pts',(-26.6936537386872,24.2609890612009,12.2664207746665));
#47203=CARTESIAN_POINT('Ctrl Pts',(-26.7156754580723,24.1635927737985,12.2725917354355));
#47204=CARTESIAN_POINT('Ctrl Pts',(-26.7331403459201,24.0652870102811,12.2787626962046));
#47205=CARTESIAN_POINT('Ctrl Pts',(-26.7460040806895,23.9665332057521,12.2849336569736));
#47206=CARTESIAN_POINT('Ctrl Pts',(-26.7558232109672,23.8911525725633,12.289644067194));
#47207=CARTESIAN_POINT('Ctrl Pts',(-26.7629625202242,23.8155110489789,12.2943544774143));
#47208=CARTESIAN_POINT('Ctrl Pts',(-26.7674227389952,23.7398136557539,12.2990648876347));
#47209=CARTESIAN_POINT('Ctrl Pts',(-26.7711182944392,23.6770938816813,12.3029677415141));
#47210=CARTESIAN_POINT('Ctrl Pts',(-26.772979921602,23.6142649885854,12.3068705953935));
#47211=CARTESIAN_POINT('Ctrl Pts',(-26.7730023270025,23.551401157192,12.3107734492729));
#47212=CARTESIAN_POINT('',(-26.7730010877972,23.5472596439823,12.0640407997644));
#47213=CARTESIAN_POINT('Ctrl Pts',(-22.0750360887345,26.4155368123409,11.6559056162233));
#47214=CARTESIAN_POINT('Ctrl Pts',(-22.1583819015529,26.4584481263603,11.6621868880363));
#47215=CARTESIAN_POINT('Ctrl Pts',(-22.2435753494475,26.4977101766977,11.6685327647814));
#47216=CARTESIAN_POINT('Ctrl Pts',(-22.4944958418206,26.6003239394625,11.6868829776968));
#47217=CARTESIAN_POINT('Ctrl Pts',(-22.6638924415869,26.653788603226,11.6988702860808));
#47218=CARTESIAN_POINT('Ctrl Pts',(-22.8411604157104,26.6940282146079,11.7105090997077));
#47219=CARTESIAN_POINT('Ctrl Pts',(-22.8454810142825,26.6949996252062,11.710792225488));
#47220=CARTESIAN_POINT('Ctrl Pts',(-22.8548833172774,26.6970932173249,11.711407135838));
#47221=CARTESIAN_POINT('Ctrl Pts',(-22.8599657777958,26.6982120046405,11.7117387569925));
#47222=CARTESIAN_POINT('Ctrl Pts',(-22.8732665170419,26.7011060968989,11.7126045491575));
#47223=CARTESIAN_POINT('Ctrl Pts',(-22.8814891356707,26.7028615745325,11.7131377374304));
#47224=CARTESIAN_POINT('Ctrl Pts',(-22.8930838902174,26.7052895775527,11.7138866114003));
#47225=CARTESIAN_POINT('Ctrl Pts',(-22.8964502929972,26.7059888985347,11.714103685199));
#47226=CARTESIAN_POINT('Ctrl Pts',(-22.9116191278717,26.7091146880194,11.7150801986262));
#47227=CARTESIAN_POINT('Ctrl Pts',(-22.9234341987885,26.711480384223,11.715836421878));
#47228=CARTESIAN_POINT('Ctrl Pts',(-22.9387604333931,26.714459805925,11.7168114516609));
#47229=CARTESIAN_POINT('Ctrl Pts',(-22.9422595321867,26.7151340102685,11.7170336590572));
#47230=CARTESIAN_POINT('Ctrl Pts',(-22.947625038379,26.7161586062532,11.7173737713073));
#47231=CARTESIAN_POINT('Ctrl Pts',(-22.9494906346947,26.716513151382,11.7174919141692));
#47232=CARTESIAN_POINT('Ctrl Pts',(-22.9531706313834,26.7172091426108,11.7177247299621));
#47233=CARTESIAN_POINT('Ctrl Pts',(-22.954985002299,26.7175506767369,11.7178394071403));
#47234=CARTESIAN_POINT('Ctrl Pts',(-22.9590278497894,26.7183080989157,11.7180946918475));
#47235=CARTESIAN_POINT('Ctrl Pts',(-22.9612564668359,26.7187231938835,11.7182352531147));
#47236=CARTESIAN_POINT('Ctrl Pts',(-22.9658594701741,26.7195755100242,11.7185252337981));
#47237=CARTESIAN_POINT('Ctrl Pts',(-22.9682339145395,26.720012415455,11.7186746350598));
#47238=CARTESIAN_POINT('Ctrl Pts',(-22.980835024686,26.7223164238251,11.7194665362847));
#47239=CARTESIAN_POINT('Ctrl Pts',(-22.9910703451991,26.7241367328508,11.7201063836719));
#47240=CARTESIAN_POINT('Ctrl Pts',(-23.097719087717,26.7425718448006,11.7267399263721));
#47241=CARTESIAN_POINT('Ctrl Pts',(-23.1948435507788,26.7548395265761,11.7324970744747));
#47242=CARTESIAN_POINT('Ctrl Pts',(-23.453293512803,26.7755857935668,11.7474218260412));
#47243=CARTESIAN_POINT('Ctrl Pts',(-23.6149530678943,26.7763950254761,11.7563617826249));
#47244=CARTESIAN_POINT('Ctrl Pts',(-24.0131954265344,26.7484302245771,11.7787016166142));
#47245=CARTESIAN_POINT('Ctrl Pts',(-24.2477784870213,26.7055797608932,11.7921904611814));
#47246=CARTESIAN_POINT('Ctrl Pts',(-24.4860359704883,26.63417015758,11.807284655181));
#47247=CARTESIAN_POINT('Ctrl Pts',(-24.4965567610809,26.6309581113191,11.8079539458553));
#47248=CARTESIAN_POINT('Ctrl Pts',(-24.5134210731075,26.6257148200039,11.8090313248342));
#47249=CARTESIAN_POINT('Ctrl Pts',(-24.51977516248,26.6237176434739,11.809438294802));
#47250=CARTESIAN_POINT('Ctrl Pts',(-24.5301704416099,26.6204148218703,11.8101058153326));
#47251=CARTESIAN_POINT('Ctrl Pts',(-24.5342153443628,26.6191208542529,11.8103659809809));
#47252=CARTESIAN_POINT('Ctrl Pts',(-24.5414540350917,26.6167894088267,11.8108323387636));
#47253=CARTESIAN_POINT('Ctrl Pts',(-24.5446487871529,26.6157549254537,11.8110384318356));
#47254=CARTESIAN_POINT('Ctrl Pts',(-24.5514107768075,26.6135536623918,11.8114752192641));
#47255=CARTESIAN_POINT('Ctrl Pts',(-24.5549776023186,26.6123856413679,11.8117059543817));
#47256=CARTESIAN_POINT('Ctrl Pts',(-24.5622262301198,26.6099979197232,11.812175552864));
#47257=CARTESIAN_POINT('Ctrl Pts',(-24.5659078863463,26.6087777982608,11.8124144298487));
#47258=CARTESIAN_POINT('Ctrl Pts',(-24.5750467197972,26.6057308171349,11.8130082910244));
#47259=CARTESIAN_POINT('Ctrl Pts',(-24.5805012074329,26.6038959860318,11.8133635390273));
#47260=CARTESIAN_POINT('Ctrl Pts',(-24.6383269017339,26.5842714745622,11.8171382881326));
#47261=CARTESIAN_POINT('Ctrl Pts',(-24.6902339669244,26.565151948513,11.8206017839665));
#47262=CARTESIAN_POINT('Ctrl Pts',(-24.8654369191102,26.4954460164466,11.83256101336));
#47263=CARTESIAN_POINT('Ctrl Pts',(-24.986063359095,26.438559000576,11.8412641988081));
#47264=CARTESIAN_POINT('Ctrl Pts',(-25.1832705150222,26.3301446170131,11.8562583103202));
#47265=CARTESIAN_POINT('Ctrl Pts',(-25.2617996061271,26.2824957697177,11.8624493163574));
#47266=CARTESIAN_POINT('Ctrl Pts',(-25.52348486242,26.10800061983,11.8837283106694));
#47267=CARTESIAN_POINT('Ctrl Pts',(-25.6954977158155,25.965550801648,11.8988979644344));
#47268=CARTESIAN_POINT('Ctrl Pts',(-25.8606563609484,25.7971001946111,11.9137873562586));
#47269=CARTESIAN_POINT('Ctrl Pts',(-25.8697997123429,25.7876597734501,11.9146126792152));
#47270=CARTESIAN_POINT('Ctrl Pts',(-25.8814024553184,25.7755324814229,11.915661008562));
#47271=CARTESIAN_POINT('Ctrl Pts',(-25.8839152207294,25.7728971895725,11.9158881026453));
#47272=CARTESIAN_POINT('Ctrl Pts',(-25.8879033149234,25.7687004109248,11.9162486201375));
#47273=CARTESIAN_POINT('Ctrl Pts',(-25.8893815485406,25.7671417079516,11.9163822696364));
#47274=CARTESIAN_POINT('Ctrl Pts',(-25.8921415706526,25.7642256067751,11.9166318421381));
#47275=CARTESIAN_POINT('Ctrl Pts',(-25.8934237295114,25.7628685819216,11.9167477938787));
#47276=CARTESIAN_POINT('Ctrl Pts',(-25.8962994620486,25.7598196307186,11.9170078916945));
#47277=CARTESIAN_POINT('Ctrl Pts',(-25.8978923816025,25.7581270978144,11.9171519865928));
#47278=CARTESIAN_POINT('Ctrl Pts',(-25.9011907888867,25.7546148189507,11.9174504088359));
#47279=CARTESIAN_POINT('Ctrl Pts',(-25.9028959988638,25.7527948125811,11.9176047146762));
#47280=CARTESIAN_POINT('Ctrl Pts',(-25.9073338930857,25.7480471210699,11.9180063810837));
#47281=CARTESIAN_POINT('Ctrl Pts',(-25.9100632463183,25.7451163071618,11.9182534873194));
#47282=CARTESIAN_POINT('Ctrl Pts',(-25.9442779216337,25.7082385630836,11.9213522518531));
#47283=CARTESIAN_POINT('Ctrl Pts',(-25.9750356074631,25.6736198715369,11.9241495062405));
#47284=CARTESIAN_POINT('Ctrl Pts',(-26.0799581081083,25.5502719416452,11.9337830736277));
#47285=CARTESIAN_POINT('Ctrl Pts',(-26.1500904763527,25.4582188643049,11.9403909800539));
#47286=CARTESIAN_POINT('Ctrl Pts',(-26.2403333792828,25.3255247721238,11.9494380567717));
#47287=CARTESIAN_POINT('Ctrl Pts',(-26.2647632193281,25.2879401675862,11.9519505237983));
#47288=CARTESIAN_POINT('Ctrl Pts',(-26.3130386008662,25.2101661195729,11.9570717531765));
#47289=CARTESIAN_POINT('Ctrl Pts',(-26.3368098353016,25.1699433630333,11.9596794795737));
#47290=CARTESIAN_POINT('Ctrl Pts',(-26.4810979108476,24.913212282793,11.9761439799149));
#47291=CARTESIAN_POINT('Ctrl Pts',(-26.5771627767355,24.6839646348247,11.9901384764632));
#47292=CARTESIAN_POINT('Ctrl Pts',(-26.6504932628538,24.4305276022776,12.0061348066016));
#47293=CARTESIAN_POINT('Ctrl Pts',(-26.6548522781249,24.4150283354731,12.0071147061851));
#47294=CARTESIAN_POINT('Ctrl Pts',(-26.6605933062523,24.3940120716357,12.0084458061184));
#47295=CARTESIAN_POINT('Ctrl Pts',(-26.6620771752929,24.3885229426941,12.0087936900645));
#47296=CARTESIAN_POINT('Ctrl Pts',(-26.6643909449012,24.3798730383238,12.0093422514946));
#47297=CARTESIAN_POINT('Ctrl Pts',(-26.6652305831348,24.3767148602656,12.009542612382));
#47298=CARTESIAN_POINT('Ctrl Pts',(-26.6668382690031,24.370630527986,12.0099287604746));
#47299=CARTESIAN_POINT('Ctrl Pts',(-26.6676070031501,24.3677045571932,12.0101145251773));
#47300=CARTESIAN_POINT('Ctrl Pts',(-26.6694107353925,24.360799610099,12.0105530636269));
#47301=CARTESIAN_POINT('Ctrl Pts',(-26.6704422396957,24.356819734004,12.0108059503631));
#47302=CARTESIAN_POINT('Ctrl Pts',(-26.6725567560446,24.3485964877967,12.0113287223218));
#47303=CARTESIAN_POINT('Ctrl Pts',(-26.6736387395095,24.3443528642511,12.0115986403203));
#47304=CARTESIAN_POINT('Ctrl Pts',(-26.6764139638471,24.3333747970601,12.012297275495));
#47305=CARTESIAN_POINT('Ctrl Pts',(-26.6780940879305,24.3266370886384,12.0127264165809));
#47306=CARTESIAN_POINT('Ctrl Pts',(-26.6913132929716,24.2728854394685,12.0161529211494));
#47307=CARTESIAN_POINT('Ctrl Pts',(-26.7018129830375,24.225624529109,12.019183659344));
#47308=CARTESIAN_POINT('Ctrl Pts',(-26.7525202735369,23.970350280686,12.035661289225));
#47309=CARTESIAN_POINT('Ctrl Pts',(-26.7731978449979,23.7590327634544,12.0497328038615));
#47310=CARTESIAN_POINT('Ctrl Pts',(-26.7730011414961,23.5472591188997,12.0640407412713));
#47311=CARTESIAN_POINT('Ctrl Pts',(-26.7730011419778,23.5472596376123,12.0640407062258));
#47312=CARTESIAN_POINT('Ctrl Pts',(-26.7727976210084,23.328108239907,12.078847102146));
#47313=CARTESIAN_POINT('Ctrl Pts',(-26.7502410738742,23.109526304479,12.0938263018387));
#47314=CARTESIAN_POINT('Ctrl Pts',(-26.6994140844638,22.8648004766997,12.1098371960409));
#47315=CARTESIAN_POINT('Ctrl Pts',(-26.6927306461825,22.8347845201557,12.1117867810493));
#47316=CARTESIAN_POINT('Ctrl Pts',(-26.6847124201125,22.8010568884623,12.1139578945829));
#47317=CARTESIAN_POINT('Ctrl Pts',(-26.6837995539451,22.7972479077596,12.1142028036925));
#47318=CARTESIAN_POINT('Ctrl Pts',(-26.6823027138725,22.7910521256905,12.1146007084122));
#47319=CARTESIAN_POINT('Ctrl Pts',(-26.6817229537988,22.7886643255492,12.114753943577));
#47320=CARTESIAN_POINT('Ctrl Pts',(-26.6805957685026,22.7840449476642,12.1150501649778));
#47321=CARTESIAN_POINT('Ctrl Pts',(-26.6800486867298,22.7818132887731,12.115193170924));
#47322=CARTESIAN_POINT('Ctrl Pts',(-26.6790531842497,22.7777711286668,12.1154520093233));
#47323=CARTESIAN_POINT('Ctrl Pts',(-26.6786055798535,22.7759604372089,12.1155678887156));
#47324=CARTESIAN_POINT('Ctrl Pts',(-26.6776342334082,22.772045646765,12.1158182782911));
#47325=CARTESIAN_POINT('Ctrl Pts',(-26.6771099412237,22.7699416933075,12.1159527556708));
#47326=CARTESIAN_POINT('Ctrl Pts',(-26.6756785804037,22.764222334813,12.1163180729448));
#47327=CARTESIAN_POINT('Ctrl Pts',(-26.6747673585438,22.7606079575401,12.1165486715475));
#47328=CARTESIAN_POINT('Ctrl Pts',(-26.6704082102087,22.7434430065688,12.1176425752836));
#47329=CARTESIAN_POINT('Ctrl Pts',(-26.6668783238818,22.729913116428,12.1185011866327));
#47330=CARTESIAN_POINT('Ctrl Pts',(-26.6023500718809,22.4890090273683,12.1337311398228));
#47331=CARTESIAN_POINT('Ctrl Pts',(-26.5166957068614,22.2689287919727,12.1467538621821));
#47332=CARTESIAN_POINT('Ctrl Pts',(-26.3872188411653,22.0206374073645,12.1624033714415));
#47333=CARTESIAN_POINT('Ctrl Pts',(-26.365814291604,21.9815867958034,12.1648936692625));
#47334=CARTESIAN_POINT('Ctrl Pts',(-26.3218448765043,21.9051696694215,12.169843502498));
#47335=CARTESIAN_POINT('Ctrl Pts',(-26.2993164889924,21.8677933218009,12.1723021272307));
#47336=CARTESIAN_POINT('Ctrl Pts',(-26.2074364487072,21.7221319934775,12.1820652117813));
#47337=CARTESIAN_POINT('Ctrl Pts',(-26.1323960706743,21.6175909896871,12.1894823789752));
#47338=CARTESIAN_POINT('Ctrl Pts',(-26.0196937486545,21.4789022087681,12.2001246831744));
#47339=CARTESIAN_POINT('Ctrl Pts',(-25.9871671719643,21.4407315689241,12.2031448655017));
#47340=CARTESIAN_POINT('Ctrl Pts',(-25.949984013577,21.3991043302083,12.2065481457253));
#47341=CARTESIAN_POINT('Ctrl Pts',(-25.9461922119889,21.3948818402269,12.2068946453915));
#47342=CARTESIAN_POINT('Ctrl Pts',(-25.9398125734151,21.3878152134252,12.2074767085759));
#47343=CARTESIAN_POINT('Ctrl Pts',(-25.9372307535791,21.3849656415856,12.2077120176891));
#47344=CARTESIAN_POINT('Ctrl Pts',(-25.9321345786174,21.3793611505714,12.2081759993136));
#47345=CARTESIAN_POINT('Ctrl Pts',(-25.9296205280847,21.3766059616061,12.2084046587037));
#47346=CARTESIAN_POINT('Ctrl Pts',(-25.9248308360907,21.3713751266576,12.2088398554652));
#47347=CARTESIAN_POINT('Ctrl Pts',(-25.9225560903345,21.3688986641579,12.2090463544947));
#47348=CARTESIAN_POINT('Ctrl Pts',(-25.9173721197974,21.3632726961371,12.2095165281168));
#47349=CARTESIAN_POINT('Ctrl Pts',(-25.9144604817994,21.3601254317544,12.2097803057697));
#47350=CARTESIAN_POINT('Ctrl Pts',(-25.9056018801081,21.3505881919075,12.2105819398645));
#47351=CARTESIAN_POINT('Ctrl Pts',(-25.8996352635171,21.3442165986662,12.2111206400982));
#47352=CARTESIAN_POINT('Ctrl Pts',(-25.8573492692387,21.2994266215793,12.2149299389543));
#47353=CARTESIAN_POINT('Ctrl Pts',(-25.8201170672009,21.2618847535737,12.2182400626652));
#47354=CARTESIAN_POINT('Ctrl Pts',(-25.7791231222399,21.2225349509252,12.2218415425201));
#47355=CARTESIAN_POINT('Ctrl Pts',(-25.7762611316239,21.2197978640303,12.2220927589447));
#47356=CARTESIAN_POINT('Ctrl Pts',(-25.7704725834773,21.214282333108,12.222600415537));
#47357=CARTESIAN_POINT('Ctrl Pts',(-25.7675458381388,21.2115040971712,12.2228568637536));
#47358=CARTESIAN_POINT('Ctrl Pts',(-25.7612489424562,21.20554916379,12.223408125095));
#47359=CARTESIAN_POINT('Ctrl Pts',(-25.757877150235,21.2023742224283,12.2237030101263));
#47360=CARTESIAN_POINT('Ctrl Pts',(-25.739702778606,21.185334663516,12.2252908785694));
#47361=CARTESIAN_POINT('Ctrl Pts',(-25.7247766684107,21.1716029869927,12.2265892702901));
#47362=CARTESIAN_POINT('Ctrl Pts',(-25.5921579310663,21.0518883099257,12.2380760900638));
#47363=CARTESIAN_POINT('Ctrl Pts',(-25.4669449838263,20.9545868539293,12.2485985469542));
#47364=CARTESIAN_POINT('Ctrl Pts',(-25.2648736593938,20.8201781199876,12.2649589977585));
#47365=CARTESIAN_POINT('Ctrl Pts',(-25.1928377896861,20.7762400367263,12.2706786860824));
#47366=CARTESIAN_POINT('Ctrl Pts',(-25.041142966112,20.6916967788872,12.2824202997753));
#47367=CARTESIAN_POINT('Ctrl Pts',(-24.961346124519,20.6514749368908,12.2884353794428));
#47368=CARTESIAN_POINT('Ctrl Pts',(-24.8186968933982,20.5868604905487,12.2988054439178));
#47369=CARTESIAN_POINT('Ctrl Pts',(-24.7565565401166,20.5610259632413,12.3032009527136));
#47370=CARTESIAN_POINT('Ctrl Pts',(-24.6758411530252,20.5303964774462,12.3087166962151));
#47371=CARTESIAN_POINT('Ctrl Pts',(-24.6579736138941,20.5237967865959,12.3099257187946));
#47372=CARTESIAN_POINT('Ctrl Pts',(-24.629123999839,20.5134303995344,12.3118574602161));
#47373=CARTESIAN_POINT('Ctrl Pts',(-24.6181785439863,20.5095640653729,12.3125856660564));
#47374=CARTESIAN_POINT('Ctrl Pts',(-24.604853644943,20.5049380507426,12.3134662809272));
#47375=CARTESIAN_POINT('Ctrl Pts',(-24.6024940900343,20.5041219535735,12.3136219949516));
#47376=CARTESIAN_POINT('Ctrl Pts',(-24.5979343269672,20.502550802634,12.3139224713079));
#47377=CARTESIAN_POINT('Ctrl Pts',(-24.5957342461335,20.501795387774,12.3140672550178));
#47378=CARTESIAN_POINT('Ctrl Pts',(-24.5917667988417,20.5004379340799,12.3143279908685));
#47379=CARTESIAN_POINT('Ctrl Pts',(-24.5899997313038,20.4998350505195,12.3144439933168));
#47380=CARTESIAN_POINT('Ctrl Pts',(-24.5861997338368,20.4985422627508,12.3146931777323));
#47381=CARTESIAN_POINT('Ctrl Pts',(-24.5841666438308,20.4978528560306,12.3148263295532));
#47382=CARTESIAN_POINT('Ctrl Pts',(-24.5786889771401,20.4960015178925,12.3151846267146));
#47383=CARTESIAN_POINT('Ctrl Pts',(-24.5752431078255,20.4948433779504,12.3154095460663));
#47384=CARTESIAN_POINT('Ctrl Pts',(-24.5593846199082,20.489543264315,12.3164425037078));
#47385=CARTESIAN_POINT('Ctrl Pts',(-24.5469485767194,20.4854710062822,12.3172464554461));
#47386=CARTESIAN_POINT('Ctrl Pts',(-24.3219204603616,20.4132987560228,12.3316900410853));
#47387=CARTESIAN_POINT('Ctrl Pts',(-24.1028062393352,20.367381367461,12.3441087266092));
#47388=CARTESIAN_POINT('Ctrl Pts',(-23.7215469805187,20.3280845937371,12.3655245211381));
#47389=CARTESIAN_POINT('Ctrl Pts',(-23.5614261096603,20.3235547241923,12.3744600407154));
#47390=CARTESIAN_POINT('Ctrl Pts',(-23.2985467387886,20.3356899466087,12.3896711794525));
#47391=CARTESIAN_POINT('Ctrl Pts',(-23.1957509916258,20.3453978096635,12.3957532966788));
#47392=CARTESIAN_POINT('Ctrl Pts',(-23.0732888433141,20.3629269431133,12.4032355469154));
#47393=CARTESIAN_POINT('Ctrl Pts',(-23.0530012514773,20.366028936896,12.4044828325208));
#47394=CARTESIAN_POINT('Ctrl Pts',(-23.0283513415207,20.3700392486509,12.40600815405));
#47395=CARTESIAN_POINT('Ctrl Pts',(-23.0239591568385,20.3707631605499,12.4062803205849));
#47396=CARTESIAN_POINT('Ctrl Pts',(-23.0154619082103,20.3721817512233,12.4068076049703));
#47397=CARTESIAN_POINT('Ctrl Pts',(-23.0113566608171,20.3728752898889,12.407062686113));
#47398=CARTESIAN_POINT('Ctrl Pts',(-23.004264407641,20.3740875923032,12.4075039509772));
#47399=CARTESIAN_POINT('Ctrl Pts',(-23.0012767615913,20.3746026206426,12.4076900154793));
#47400=CARTESIAN_POINT('Ctrl Pts',(-22.9950932391181,20.3756775602188,12.4080754862494));
#47401=CARTESIAN_POINT('Ctrl Pts',(-22.9918974736278,20.376238083294,12.4082749118398));
#47402=CARTESIAN_POINT('Ctrl Pts',(-22.9841524875955,20.3776085784464,12.4087587266489));
#47403=CARTESIAN_POINT('Ctrl Pts',(-22.979604161271,20.3784235087177,12.4090432737982));
#47404=CARTESIAN_POINT('Ctrl Pts',(-22.9626533053871,20.381498258876,12.4101053173987));
#47405=CARTESIAN_POINT('Ctrl Pts',(-22.9502624427238,20.3838210421242,12.4108848216122));
#47406=CARTESIAN_POINT('Ctrl Pts',(-22.7364428133157,20.4252036471991,12.4243917703911));
#47407=CARTESIAN_POINT('Ctrl Pts',(-22.5392238224086,20.4833308445629,12.4377511318064));
#47408=CARTESIAN_POINT('Ctrl Pts',(-22.2406549010072,20.6032745929559,12.4593115707154));
#47409=CARTESIAN_POINT('Ctrl Pts',(-22.1348554122537,20.6526027074621,12.4672263787619));
#47410=CARTESIAN_POINT('Ctrl Pts',(-21.9341842687456,20.7597812776515,12.4826089448638));
#47411=CARTESIAN_POINT('Ctrl Pts',(-21.839155552902,20.8170206399463,12.490068812216));
#47412=CARTESIAN_POINT('Ctrl Pts',(-21.7063826128123,20.9066387868157,12.5005810887377));
#47413=CARTESIAN_POINT('Ctrl Pts',(-21.666140502092,20.9351669979323,12.5037794508485));
#47414=CARTESIAN_POINT('Ctrl Pts',(-21.6127181364398,20.9749125594687,12.5080254340408));
#47415=CARTESIAN_POINT('Ctrl Pts',(-21.5989520999209,20.9853271603682,12.509119551023));
#47416=CARTESIAN_POINT('Ctrl Pts',(-21.5767375633319,21.0024157792196,12.5108842518007));
#47417=CARTESIAN_POINT('Ctrl Pts',(-21.5682378613114,21.0090222584145,12.5115592429886));
#47418=CARTESIAN_POINT('Ctrl Pts',(-21.5578518357827,21.0171787100422,12.5123836001375));
#47419=CARTESIAN_POINT('Ctrl Pts',(-21.5559340971832,21.0186882917684,12.5125357961856));
#47420=CARTESIAN_POINT('Ctrl Pts',(-21.5522235596711,21.0216159396864,12.5128302343398));
#47421=CARTESIAN_POINT('Ctrl Pts',(-21.5504305518047,21.0230337369886,12.5129724954674));
#47422=CARTESIAN_POINT('Ctrl Pts',(-21.5471777093889,21.025611508625,12.5132305489739));
#47423=CARTESIAN_POINT('Ctrl Pts',(-21.5457173781071,21.0267708382392,12.5133463868667));
#47424=CARTESIAN_POINT('Ctrl Pts',(-21.5427770551997,21.0291092683387,12.5135795965207));
#47425=CARTESIAN_POINT('Ctrl Pts',(-21.5412971018857,21.0302884001681,12.5136969650987));
#47426=CARTESIAN_POINT('Ctrl Pts',(-21.5370592654813,21.0336709422632,12.5140330150882));
#47427=CARTESIAN_POINT('Ctrl Pts',(-21.5343039519525,21.0358775899822,12.5142514631643));
#47428=CARTESIAN_POINT('Ctrl Pts',(-21.5223843282463,21.0454558460183,12.5151963278757));
#47429=CARTESIAN_POINT('Ctrl Pts',(-21.5132566327153,21.0528731843108,12.5159194858819));
#47430=CARTESIAN_POINT('Ctrl Pts',(-21.3563303303913,21.1818272285785,12.5283495115638));
#47431=CARTESIAN_POINT('Ctrl Pts',(-21.2195794964766,21.3162606172501,12.5391504471633));
#47432=CARTESIAN_POINT('Ctrl Pts',(-20.9903022205163,21.5857788536466,12.5589624169127));
#47433=CARTESIAN_POINT('Ctrl Pts',(-20.8945581547298,21.7172801882064,12.5679706498143));
#47434=CARTESIAN_POINT('Ctrl Pts',(-20.7617980318484,21.9319995698742,12.5824019411968));
#47435=CARTESIAN_POINT('Ctrl Pts',(-20.717689296962,22.0105107508227,12.587623528924));
#47436=CARTESIAN_POINT('Ctrl Pts',(-20.6494720373039,22.1448112179258,12.5965492698235));
#47437=CARTESIAN_POINT('Ctrl Pts',(-20.6235495138283,22.1996225076053,12.6001900340611));
#47438=CARTESIAN_POINT('Ctrl Pts',(-20.5958701184,22.2626926937489,12.6043886788086));
#47439=CARTESIAN_POINT('Ctrl Pts',(-20.5925800320215,22.270268483766,12.604893150223));
#47440=CARTESIAN_POINT('Ctrl Pts',(-20.5876460778569,22.2817500607094,12.6056579544832));
#47441=CARTESIAN_POINT('Ctrl Pts',(-20.585980714297,22.2856466201438,12.6059175527084));
#47442=CARTESIAN_POINT('Ctrl Pts',(-20.5831330501037,22.2923460175987,12.606363960622));
#47443=CARTESIAN_POINT('Ctrl Pts',(-20.5819470209457,22.2951472727647,12.6065506428963));
#47444=CARTESIAN_POINT('Ctrl Pts',(-20.5795156630539,22.3009125634801,12.6069349053137));
#47445=CARTESIAN_POINT('Ctrl Pts',(-20.5782708002299,22.3038767911598,12.6071325010944));
#47446=CARTESIAN_POINT('Ctrl Pts',(-20.5752894628311,22.3110057195054,12.6076077837204));
#47447=CARTESIAN_POINT('Ctrl Pts',(-20.5735572985081,22.3151722059563,12.6078856168021));
#47448=CARTESIAN_POINT('Ctrl Pts',(-20.5672799860644,22.3303613431314,12.6088986821734));
#47449=CARTESIAN_POINT('Ctrl Pts',(-20.5627873098702,22.3414054519858,12.6096356920489));
#47450=CARTESIAN_POINT('Ctrl Pts',(-20.490634976463,22.5216327031507,12.6216701657291));
#47451=CARTESIAN_POINT('Ctrl Pts',(-20.4373937635843,22.6961987116296,12.6334605310436));
#47452=CARTESIAN_POINT('Ctrl Pts',(-20.3609520345424,23.0525449577599,12.6577402115178));
#47453=CARTESIAN_POINT('Ctrl Pts',(-20.3379099518835,23.233708399093,12.6701849705025));
#47454=CARTESIAN_POINT('Ctrl Pts',(-20.3274463490543,23.4843597546447,12.6870431640661));
#47455=CARTESIAN_POINT('Ctrl Pts',(-20.3267737977663,23.5529631390126,12.691617217088));
#47456=CARTESIAN_POINT('Ctrl Pts',(-20.3294308078937,23.6730532495847,12.6995021584923));
#47457=CARTESIAN_POINT('Ctrl Pts',(-20.3318059406975,23.7245361972825,12.702843025759));
#47458=CARTESIAN_POINT('Ctrl Pts',(-20.3371353598512,23.8004508379356,12.7076902575868));
#47459=CARTESIAN_POINT('Ctrl Pts',(-20.3391361261755,23.8249390292553,12.7092416503787));
#47460=CARTESIAN_POINT('Ctrl Pts',(-20.3418129815249,23.8536523182508,12.7110444950601));
#47461=CARTESIAN_POINT('Ctrl Pts',(-20.3422175922927,23.8579010416103,12.7113108456383));
#47462=CARTESIAN_POINT('Ctrl Pts',(-20.3428515430429,23.8644207513634,12.7117189093962));
#47463=CARTESIAN_POINT('Ctrl Pts',(-20.3430748555175,23.8666922980998,12.7118609619231));
#47464=CARTESIAN_POINT('Ctrl Pts',(-20.3434671296774,23.8706394604394,12.7121075859598));
#47465=CARTESIAN_POINT('Ctrl Pts',(-20.3436349911408,23.872315176779,12.7122122197958));
#47466=CARTESIAN_POINT('Ctrl Pts',(-20.3439895206481,23.8758265956148,12.7124313361009));
#47467=CARTESIAN_POINT('Ctrl Pts',(-20.344176451152,23.8776622641649,12.7125458031708));
#47468=CARTESIAN_POINT('Ctrl Pts',(-20.3447017422782,23.8827770663358,12.7128645255361));
#47469=CARTESIAN_POINT('Ctrl Pts',(-20.3450435590845,23.8860558547835,12.7130685845681));
#47470=CARTESIAN_POINT('Ctrl Pts',(-20.3464322409015,23.8991811136403,12.7138844511981));
#47471=CARTESIAN_POINT('Ctrl Pts',(-20.3475194668355,23.9090233949306,12.7144939975841));
#47472=CARTESIAN_POINT('Ctrl Pts',(-20.3672564239271,24.0804516579629,12.7250739949944));
#47473=CARTESIAN_POINT('Ctrl Pts',(-20.3980709234063,24.2404282105695,12.7343821353934));
#47474=CARTESIAN_POINT('Ctrl Pts',(-20.4970029778575,24.6035472928319,12.7555675281017));
#47475=CARTESIAN_POINT('Ctrl Pts',(-20.57351985322,24.8035775947017,12.767311198549));
#47476=CARTESIAN_POINT('Ctrl Pts',(-20.6899952423621,25.0359123478748,12.7822730444915));
#47477=CARTESIAN_POINT('Ctrl Pts',(-20.7116108294858,25.076807435002,12.7849579853745));
#47478=CARTESIAN_POINT('Ctrl Pts',(-20.7735420016451,25.188110006927,12.7924274003587));
#47479=CARTESIAN_POINT('Ctrl Pts',(-20.8156452075056,25.2574782148758,12.7972664319348));
#47480=CARTESIAN_POINT('Ctrl Pts',(-20.8659756517482,25.3337549097732,12.8028289148867));
#47481=CARTESIAN_POINT('Ctrl Pts',(-20.8716745181362,25.3423024535066,12.8034557509153));
#47482=CARTESIAN_POINT('Ctrl Pts',(-20.8800047573507,25.3546681952177,12.8043677556763));
#47483=CARTESIAN_POINT('Ctrl Pts',(-20.8826036961857,25.3585082528822,12.8046516963061));
#47484=CARTESIAN_POINT('Ctrl Pts',(-20.8871309996156,25.3651665596831,12.805145292631));
#47485=CARTESIAN_POINT('Ctrl Pts',(-20.889055577722,25.3679873846459,12.8053548042458));
#47486=CARTESIAN_POINT('Ctrl Pts',(-20.8927664866768,25.3734078822708,12.8057581688946));
#47487=CARTESIAN_POINT('Ctrl Pts',(-20.8945521588681,25.3760080031228,12.8059519966835));
#47488=CARTESIAN_POINT('Ctrl Pts',(-20.8987703739668,25.3821308728561,12.8064092361674));
#47489=CARTESIAN_POINT('Ctrl Pts',(-20.9012061204963,25.3856513985918,12.8066727700542));
#47490=CARTESIAN_POINT('Ctrl Pts',(-20.9084278456946,25.396045054318,12.8074526750924));
#47491=CARTESIAN_POINT('Ctrl Pts',(-20.9132335830471,25.4029043528635,12.8079698026508));
#47492=CARTESIAN_POINT('Ctrl Pts',(-20.9559430687199,25.4633613587537,12.8125493692115));
#47493=CARTESIAN_POINT('Ctrl Pts',(-20.99544707207,25.5158046202051,12.8166734275706));
#47494=CARTESIAN_POINT('Ctrl Pts',(-21.0470671302845,25.5801452224494,12.8219333810961));
#47495=CARTESIAN_POINT('Ctrl Pts',(-21.0577144579651,25.5932051557233,12.823011781879));
#47496=CARTESIAN_POINT('Ctrl Pts',(-21.1120645111481,25.6588131658551,12.8284839033188));
#47497=CARTESIAN_POINT('Ctrl Pts',(-21.157326104986,25.7100420716934,12.8329362703006));
#47498=CARTESIAN_POINT('Ctrl Pts',(-21.3691530469982,25.9349585076166,12.8533021167513));
#47499=CARTESIAN_POINT('Ctrl Pts',(-21.5532223144827,26.0910929051231,12.8698242664419));
#47500=CARTESIAN_POINT('Ctrl Pts',(-21.8257229957743,26.2741851064674,12.8917570024975));
#47501=CARTESIAN_POINT('Ctrl Pts',(-21.9005000118894,26.3201135486168,12.8975393880501));
#47502=CARTESIAN_POINT('Ctrl Pts',(-22.0064189117119,26.3793560330567,12.9053200910249));
#47503=CARTESIAN_POINT('Ctrl Pts',(-22.0360307734183,26.3953151948964,12.9074527034947));
#47504=CARTESIAN_POINT('Ctrl Pts',(-22.0689351273279,26.4123895115327,12.9097713274644));
#47505=CARTESIAN_POINT('Ctrl Pts',(-22.0719843072135,26.4139655760787,12.909985710627));
#47506=CARTESIAN_POINT('Ctrl Pts',(-22.0750360153462,26.4155367745564,12.9101997884793));
#47507=CARTESIAN_POINT('Origin',(-23.5502525316942,23.5502525316942,-77.3107734492734));
#47508=CARTESIAN_POINT('',(-22.0750358569346,26.4155366929967,14.4063516850465));
#47509=CARTESIAN_POINT('',(-22.0750361586249,26.4155368483246,14.1564144975666));
#47510=CARTESIAN_POINT('',(-22.0750360153461,26.4155367745563,-77.3107734492734));
#47511=CARTESIAN_POINT('',(-26.7696996717685,23.55268397525,13.5607719477124));
#47512=CARTESIAN_POINT('Ctrl Pts',(-22.0750358569346,26.4155366929967,14.4063516850465));
#47513=CARTESIAN_POINT('Ctrl Pts',(-22.0142029387246,26.3842163316414,14.4023201504987));
#47514=CARTESIAN_POINT('Ctrl Pts',(-21.9543647139263,26.3509572618314,14.398227214807));
#47515=CARTESIAN_POINT('Ctrl Pts',(-21.8858777544244,26.309981299096,14.393373398924));
#47516=CARTESIAN_POINT('Ctrl Pts',(-21.876173242285,26.3041052504215,14.3926815727776));
#47517=CARTESIAN_POINT('Ctrl Pts',(-21.8627333518613,26.2958701480209,14.391717741403));
#47518=CARTESIAN_POINT('Ctrl Pts',(-21.8589714132938,26.2935544209534,14.3914473313953));
#47519=CARTESIAN_POINT('Ctrl Pts',(-21.8525014599586,26.289553361214,14.3909811845128));
#47520=CARTESIAN_POINT('Ctrl Pts',(-21.8497911566245,26.2878717250761,14.3907855842914));
#47521=CARTESIAN_POINT('Ctrl Pts',(-21.8443523023718,26.2844859378319,14.3903924045676));
#47522=CARTESIAN_POINT('Ctrl Pts',(-21.8416237983045,26.282781719637,14.3901948227564));
#47523=CARTESIAN_POINT('Ctrl Pts',(-21.8352447242594,26.2787840725517,14.3897320997684));
#47524=CARTESIAN_POINT('Ctrl Pts',(-21.8315962020672,26.2764874022365,14.3894668385383));
#47525=CARTESIAN_POINT('Ctrl Pts',(-21.8203912081306,26.2694026544044,14.3886503201982));
#47526=CARTESIAN_POINT('Ctrl Pts',(-21.8128501033255,26.2645904597913,14.3880981663744));
#47527=CARTESIAN_POINT('Ctrl Pts',(-21.795561470701,26.2534565234525,14.3868262066001));
#47528=CARTESIAN_POINT('Ctrl Pts',(-21.7858279406812,26.2471133730282,14.386105603215));
#47529=CARTESIAN_POINT('Ctrl Pts',(-21.6948388319251,26.1871141160455,14.3793267854803));
#47530=CARTESIAN_POINT('Ctrl Pts',(-21.6160277185812,26.1298591097764,14.3731326656458));
#47531=CARTESIAN_POINT('Ctrl Pts',(-21.3777677906952,25.9397037040801,14.3533442272863));
#47532=CARTESIAN_POINT('Ctrl Pts',(-21.228496030504,25.7949336836897,14.3393137962258));
#47533=CARTESIAN_POINT('Ctrl Pts',(-20.9729332779317,25.4941192319451,14.312605572933));
#47534=CARTESIAN_POINT('Ctrl Pts',(-20.8643316980723,25.3410734617185,14.2999919058949));
#47535=CARTESIAN_POINT('Ctrl Pts',(-20.7638035359656,25.1694969332139,14.2874597656363));
#47536=CARTESIAN_POINT('Ctrl Pts',(-20.7580295377401,25.1595198181541,14.2867365329266));
#47537=CARTESIAN_POINT('Ctrl Pts',(-20.7505711484559,25.1464711822578,14.2857980237518));
#47538=CARTESIAN_POINT('Ctrl Pts',(-20.7488381516001,25.1434277572542,14.2855796492051));
#47539=CARTESIAN_POINT('Ctrl Pts',(-20.7461792578408,25.1387405538515,14.2852441362653));
#47540=CARTESIAN_POINT('Ctrl Pts',(-20.74524984442,25.1370987895604,14.2851267698875));
#47541=CARTESIAN_POINT('Ctrl Pts',(-20.7434045438485,25.1338324676737,14.2848935710443));
#47542=CARTESIAN_POINT('Ctrl Pts',(-20.7424886304771,25.1322079405363,14.2847777375001));
#47543=CARTESIAN_POINT('Ctrl Pts',(-20.7404487755772,25.1285825609308,14.2845195698734));
#47544=CARTESIAN_POINT('Ctrl Pts',(-20.7393255634705,25.1265813071948,14.2843772835931));
#47545=CARTESIAN_POINT('Ctrl Pts',(-20.7360479501751,25.1207268626825,14.2839616944584));
#47546=CARTESIAN_POINT('Ctrl Pts',(-20.7338993163644,25.1168704232009,14.283688764218));
#47547=CARTESIAN_POINT('Ctrl Pts',(-20.7183477544624,25.0888225678663,14.2817096529921));
#47548=CARTESIAN_POINT('Ctrl Pts',(-20.7052482630322,25.0644629724648,14.2800226743612));
#47549=CARTESIAN_POINT('Ctrl Pts',(-20.664292738755,24.9858944774439,14.2746732289151));
#47550=CARTESIAN_POINT('Ctrl Pts',(-20.6376586840455,24.9310601991972,14.2710776878622));
#47551=CARTESIAN_POINT('Ctrl Pts',(-20.5781852625296,24.7992262530383,14.2626795273687));
#47552=CARTESIAN_POINT('Ctrl Pts',(-20.5467581430206,24.7216372389472,14.2579295961377));
#47553=CARTESIAN_POINT('Ctrl Pts',(-20.4197022219535,24.3690867322549,14.236843177525));
#47554=CARTESIAN_POINT('Ctrl Pts',(-20.3585748744525,24.083186927155,14.220921035406));
#47555=CARTESIAN_POINT('Ctrl Pts',(-20.3361369641207,23.7861042929074,14.2031944560384));
#47556=CARTESIAN_POINT('Ctrl Pts',(-20.3356405929824,23.7792394689123,14.2027842941276));
#47557=CARTESIAN_POINT('Ctrl Pts',(-20.3320804218505,23.7277077480629,14.199701138409));
#47558=CARTESIAN_POINT('Ctrl Pts',(-20.329925849144,23.6829847202599,14.197001456098));
#47559=CARTESIAN_POINT('Ctrl Pts',(-20.3285001242239,23.6307794450926,14.1938177493432));
#47560=CARTESIAN_POINT('Ctrl Pts',(-20.3283224380257,23.6233252958665,14.1933623963767));
#47561=CARTESIAN_POINT('Ctrl Pts',(-20.3280802255348,23.6114318043876,14.1926346109333));
#47562=CARTESIAN_POINT('Ctrl Pts',(-20.3279990010389,23.6069927983005,14.1923627029124));
#47563=CARTESIAN_POINT('Ctrl Pts',(-20.3278718584805,23.5991594156847,14.1918823813876));
#47564=CARTESIAN_POINT('Ctrl Pts',(-20.3278221302239,23.5957651007533,14.1916740878192));
#47565=CARTESIAN_POINT('Ctrl Pts',(-20.3277313807123,23.5888218300205,14.1912476741062));
#47566=CARTESIAN_POINT('Ctrl Pts',(-20.3276908589237,23.5852728733397,14.1910295385679));
#47567=CARTESIAN_POINT('Ctrl Pts',(-20.3276055013191,23.5765324405043,14.1904918636632));
#47568=CARTESIAN_POINT('Ctrl Pts',(-20.3275673476793,23.5713409223144,14.1901721148989));
#47569=CARTESIAN_POINT('Ctrl Pts',(-20.3274671817358,23.551034614295,14.1889199023045));
#47570=CARTESIAN_POINT('Ctrl Pts',(-20.3274989602527,23.5359197440218,14.1879844988325));
#47571=CARTESIAN_POINT('Ctrl Pts',(-20.3278410569835,23.4984810054802,14.1856590880073));
#47572=CARTESIAN_POINT('Ctrl Pts',(-20.3282770255972,23.4761593411435,14.1842651746593));
#47573=CARTESIAN_POINT('Ctrl Pts',(-20.3308692773963,23.3895437727808,14.1788264848373));
#47574=CARTESIAN_POINT('Ctrl Pts',(-20.3347183828118,23.3253191327741,14.1747294990411));
#47575=CARTESIAN_POINT('Ctrl Pts',(-20.3559535923923,23.0894682226301,14.159441181367));
#47576=CARTESIAN_POINT('Ctrl Pts',(-20.3851850358819,22.919219894207,14.1479097030004));
#47577=CARTESIAN_POINT('Ctrl Pts',(-20.4748604529884,22.5683899019768,14.1234310472453));
#47578=CARTESIAN_POINT('Ctrl Pts',(-20.5379632463702,22.3891269208478,14.1105036297968));
#47579=CARTESIAN_POINT('Ctrl Pts',(-20.6206722335937,22.2072037891786,14.0975185927279));
#47580=CARTESIAN_POINT('Ctrl Pts',(-20.6249180211257,22.1979808673657,14.0968607419501));
#47581=CARTESIAN_POINT('Ctrl Pts',(-20.6312920980296,22.1843052775927,14.0958861210028));
#47582=CARTESIAN_POINT('Ctrl Pts',(-20.6333871039772,22.1798372692728,14.095567830644));
#47583=CARTESIAN_POINT('Ctrl Pts',(-20.6388460096187,22.1682643186375,14.0947437762109));
#47584=CARTESIAN_POINT('Ctrl Pts',(-20.6422256790694,22.1611667946765,14.0942387630755));
#47585=CARTESIAN_POINT('Ctrl Pts',(-20.6485904205377,22.1479254621691,14.0932973803523));
#47586=CARTESIAN_POINT('Ctrl Pts',(-20.65156911397,22.1417786544757,14.0928606946515));
#47587=CARTESIAN_POINT('Ctrl Pts',(-20.6659446374602,22.1123522018075,14.0907718448422));
#47588=CARTESIAN_POINT('Ctrl Pts',(-20.6776029134701,22.0892002867249,14.0891334579532));
#47589=CARTESIAN_POINT('Ctrl Pts',(-20.6916659282011,22.0620920860076,14.0872233110144));
#47590=CARTESIAN_POINT('Ctrl Pts',(-20.6938009864599,22.0579980453084,14.0869350520328));
#47591=CARTESIAN_POINT('Ctrl Pts',(-20.6970445483644,22.0518108825075,14.0864997711836));
#47592=CARTESIAN_POINT('Ctrl Pts',(-20.6981465613434,22.0497143928483,14.0863523399783));
#47593=CARTESIAN_POINT('Ctrl Pts',(-20.7001231142995,22.0459642062422,14.0860887289006));
#47594=CARTESIAN_POINT('Ctrl Pts',(-20.7009967817137,22.0443100582717,14.0859724937168));
#47595=CARTESIAN_POINT('Ctrl Pts',(-20.7028626321134,22.0407848084066,14.0857248630409));
#47596=CARTESIAN_POINT('Ctrl Pts',(-20.7038552166992,22.0389139286229,14.085593494046));
#47597=CARTESIAN_POINT('Ctrl Pts',(-20.7065403114797,22.0338649374345,14.0852390984224));
#47598=CARTESIAN_POINT('Ctrl Pts',(-20.7082363111876,22.0306886698904,14.0850162945565));
#47599=CARTESIAN_POINT('Ctrl Pts',(-20.7165772309169,22.0151306097217,14.083925619333));
#47600=CARTESIAN_POINT('Ctrl Pts',(-20.7232978947413,22.0027892774572,14.0830625231316));
#47601=CARTESIAN_POINT('Ctrl Pts',(-20.7808326367159,21.8987625413934,14.0758016036561));
#47602=CARTESIAN_POINT('Ctrl Pts',(-20.8360172527908,21.8095522273518,14.0696681703263));
#47603=CARTESIAN_POINT('Ctrl Pts',(-21.0534455835168,21.4936217155273,14.0477028509342));
#47604=CARTESIAN_POINT('Ctrl Pts',(-21.2405378733918,21.2855213774076,14.0326427488444));
#47605=CARTESIAN_POINT('Ctrl Pts',(-21.4935371483055,21.0685146515761,14.0133691735308));
#47606=CARTESIAN_POINT('Ctrl Pts',(-21.5358923678211,21.0340145179315,14.0101780259796));
#47607=CARTESIAN_POINT('Ctrl Pts',(-21.5877667381218,20.9939100239729,14.0062987698934));
#47608=CARTESIAN_POINT('Ctrl Pts',(-21.5964652349386,20.9872557112353,14.0056492446608));
#47609=CARTESIAN_POINT('Ctrl Pts',(-21.6107810217605,20.9764194243055,14.004581726848));
#47610=CARTESIAN_POINT('Ctrl Pts',(-21.6163783650655,20.9722111609891,14.0041646988256));
#47611=CARTESIAN_POINT('Ctrl Pts',(-21.6232806609528,20.9670569198226,14.0036508678575));
#47612=CARTESIAN_POINT('Ctrl Pts',(-21.6245726948971,20.9660936112792,14.003554702478));
#47613=CARTESIAN_POINT('Ctrl Pts',(-21.6359532425114,20.9576218311829,14.0027078122126));
#47614=CARTESIAN_POINT('Ctrl Pts',(-21.646084797578,20.9501715807355,14.0019549558013));
#47615=CARTESIAN_POINT('Ctrl Pts',(-21.6663118637146,20.9354792174883,14.0004538864889));
#47616=CARTESIAN_POINT('Ctrl Pts',(-21.6764061639986,20.9282358061763,13.9997057398887));
#47617=CARTESIAN_POINT('Ctrl Pts',(-21.7050352449431,20.9079420707142,13.9975863359687));
#47618=CARTESIAN_POINT('Ctrl Pts',(-21.7236659136074,20.8950288700357,13.9962099967602));
#47619=CARTESIAN_POINT('Ctrl Pts',(-21.7478252255627,20.8786582832595,13.9944283321966));
#47620=CARTESIAN_POINT('Ctrl Pts',(-21.7532305976075,20.8750194223027,13.9940299032102));
#47621=CARTESIAN_POINT('Ctrl Pts',(-21.7618191635952,20.8692754309997,13.9933971402388));
#47622=CARTESIAN_POINT('Ctrl Pts',(-21.7649951450718,20.867159505001,13.9931632141525));
#47623=CARTESIAN_POINT('Ctrl Pts',(-21.7709384547064,20.8632151335043,13.9927255782272));
#47624=CARTESIAN_POINT('Ctrl Pts',(-21.7737048643314,20.8613853075095,13.9925219207325));
#47625=CARTESIAN_POINT('Ctrl Pts',(-21.7798559893114,20.8573303172754,13.9920691895597));
#47626=CARTESIAN_POINT('Ctrl Pts',(-21.7832420808177,20.8551072598312,13.9918200371894));
#47627=CARTESIAN_POINT('Ctrl Pts',(-21.7930556697901,20.8486908262629,13.9910981348271));
#47628=CARTESIAN_POINT('Ctrl Pts',(-21.7994939335048,20.8445140393466,13.9906247647078));
#47629=CARTESIAN_POINT('Ctrl Pts',(-21.8140502001286,20.8351444503609,13.9895550295402));
#47630=CARTESIAN_POINT('Ctrl Pts',(-21.8221766720946,20.829965000995,13.988958171381));
#47631=CARTESIAN_POINT('Ctrl Pts',(-21.8479172651009,20.8137209890315,13.9870686642779));
#47632=CARTESIAN_POINT('Ctrl Pts',(-21.865615069884,20.8027906423523,13.9857710707288));
#47633=CARTESIAN_POINT('Ctrl Pts',(-21.9335037294335,20.7617644644939,13.9807985796295));
#47634=CARTESIAN_POINT('Ctrl Pts',(-21.9844026697482,20.7328679495321,13.9770806831924));
#47635=CARTESIAN_POINT('Ctrl Pts',(-22.1560416723955,20.6415125656399,13.9645712027929));
#47636=CARTESIAN_POINT('Ctrl Pts',(-22.2799326049921,20.5853120393978,13.955578953587));
#47637=CARTESIAN_POINT('Ctrl Pts',(-22.6424802050175,20.4477524270943,13.9295302587125));
#47638=CARTESIAN_POINT('Ctrl Pts',(-22.8876373274337,20.3863139622003,13.9121720158848));
#47639=CARTESIAN_POINT('Ctrl Pts',(-23.1748392305863,20.3492209013376,13.8935462908562));
#47640=CARTESIAN_POINT('Ctrl Pts',(-23.2123098729675,20.3450483706583,13.8911506329103));
#47641=CARTESIAN_POINT('Ctrl Pts',(-23.2550616990382,20.3410458749905,13.8884629654269));
#47642=CARTESIAN_POINT('Ctrl Pts',(-23.2602775465681,20.3405703820042,13.8881358344852));
#47643=CARTESIAN_POINT('Ctrl Pts',(-23.267919245985,20.3398925201727,13.8876577114698));
#47644=CARTESIAN_POINT('Ctrl Pts',(-23.2703441707893,20.3396801843727,13.8875061598264));
#47645=CARTESIAN_POINT('Ctrl Pts',(-23.2746461757725,20.3393083951692,13.887237600054));
#47646=CARTESIAN_POINT('Ctrl Pts',(-23.2765231559845,20.3391478401191,13.8871205293738));
#47647=CARTESIAN_POINT('Ctrl Pts',(-23.2804519716744,20.3388152428964,13.8868756983626));
#47648=CARTESIAN_POINT('Ctrl Pts',(-23.2825038269735,20.3386435216736,13.886747956634));
#47649=CARTESIAN_POINT('Ctrl Pts',(-23.2878823905409,20.3381985761827,13.8864134246947));
#47650=CARTESIAN_POINT('Ctrl Pts',(-23.2912093721805,20.3379285527289,13.8862068159993));
#47651=CARTESIAN_POINT('Ctrl Pts',(-23.3058454254889,20.3367635517003,13.8852992891703));
#47652=CARTESIAN_POINT('Ctrl Pts',(-23.3171589388607,20.3359231079811,13.8846014193999));
#47653=CARTESIAN_POINT('Ctrl Pts',(-23.4003215549433,20.3301866184262,13.8794967475945));
#47654=CARTESIAN_POINT('Ctrl Pts',(-23.4723185991867,20.3276399420705,13.8752153897253));
#47655=CARTESIAN_POINT('Ctrl Pts',(-23.6262441031167,20.3273578574963,13.8662424030426));
#47656=CARTESIAN_POINT('Ctrl Pts',(-23.708122373949,20.3303296445114,13.8615780794641));
#47657=CARTESIAN_POINT('Ctrl Pts',(-23.813873754763,20.3382120504177,13.8555983608753));
#47658=CARTESIAN_POINT('Ctrl Pts',(-23.8379242001918,20.3402766388643,13.8542414652921));
#47659=CARTESIAN_POINT('Ctrl Pts',(-23.882403491687,20.3445988348472,13.8517343230038));
#47660=CARTESIAN_POINT('Ctrl Pts',(-23.9028382276226,20.3467820357256,13.8505833995107));
#47661=CARTESIAN_POINT('Ctrl Pts',(-23.9409629459315,20.3512244112206,13.8484358561341));
#47662=CARTESIAN_POINT('Ctrl Pts',(-23.9586577249909,20.3534352482392,13.847439004415));
#47663=CARTESIAN_POINT('Ctrl Pts',(-24.1283313643118,20.3760665151404,13.8378727126086));
#47664=CARTESIAN_POINT('Ctrl Pts',(-24.2786838517404,20.4071622407372,13.8293258207096));
#47665=CARTESIAN_POINT('Ctrl Pts',(-24.4793288046129,20.4638342830492,13.8173441072551));
#47666=CARTESIAN_POINT('Ctrl Pts',(-24.532017389905,20.4801877695452,13.8141432478161));
#47667=CARTESIAN_POINT('Ctrl Pts',(-24.5921841713001,20.5005695899272,13.8104114546292));
#47668=CARTESIAN_POINT('Ctrl Pts',(-24.6000992854876,20.5032852888936,13.8099189870317));
#47669=CARTESIAN_POINT('Ctrl Pts',(-24.6741445200517,20.5290131970191,13.8052972259453));
#47670=CARTESIAN_POINT('Ctrl Pts',(-24.7395145871519,20.5541425619747,13.8011058131571));
#47671=CARTESIAN_POINT('Ctrl Pts',(-24.8126316594597,20.5850199824749,13.7962716496089));
#47672=CARTESIAN_POINT('Ctrl Pts',(-24.8212364254666,20.5886980290668,13.795700420637));
#47673=CARTESIAN_POINT('Ctrl Pts',(-24.8338915575807,20.5941726874369,13.7948568376666));
#47674=CARTESIAN_POINT('Ctrl Pts',(-24.8379544872731,20.5959402821696,13.7945854765096));
#47675=CARTESIAN_POINT('Ctrl Pts',(-24.8451224463395,20.599076328802,13.794105792078));
#47676=CARTESIAN_POINT('Ctrl Pts',(-24.8482289903587,20.6004413192632,13.7938975877226));
#47677=CARTESIAN_POINT('Ctrl Pts',(-24.8541990411662,20.6030757683909,13.7934968640113));
#47678=CARTESIAN_POINT('Ctrl Pts',(-24.8570628657015,20.6043445011304,13.7933043697752));
#47679=CARTESIAN_POINT('Ctrl Pts',(-24.8631730047553,20.6070620805576,13.7928930980925));
#47680=CARTESIAN_POINT('Ctrl Pts',(-24.8664187784382,20.6085121265914,13.7926742795595));
#47681=CARTESIAN_POINT('Ctrl Pts',(-24.8787750519438,20.6140568224138,13.7918399375391));
#47682=CARTESIAN_POINT('Ctrl Pts',(-24.8878688241608,20.6181884156609,13.7912231419522));
#47683=CARTESIAN_POINT('Ctrl Pts',(-24.9089483486993,20.6278839966976,13.789786933533));
#47684=CARTESIAN_POINT('Ctrl Pts',(-24.9209193141783,20.6334795305002,13.7889664351532));
#47685=CARTESIAN_POINT('Ctrl Pts',(-24.961578138116,20.6527900754657,13.7861627847028));
#47686=CARTESIAN_POINT('Ctrl Pts',(-24.9900965539964,20.6668556240136,13.7841675045569));
#47687=CARTESIAN_POINT('Ctrl Pts',(-25.1130481097952,20.7297753579528,13.7754370093258));
#47688=CARTESIAN_POINT('Ctrl Pts',(-25.205230498133,20.7828592847096,13.768555680825));
#47689=CARTESIAN_POINT('Ctrl Pts',(-25.3395228773174,20.8693046200107,13.7580228292325));
#47690=CARTESIAN_POINT('Ctrl Pts',(-25.3837047379595,20.8993238824793,13.7544701571006));
#47691=CARTESIAN_POINT('Ctrl Pts',(-25.6649041785372,21.1007775946131,13.7313137978281));
#47692=CARTESIAN_POINT('Ctrl Pts',(-25.8783906368783,21.3027068378809,13.7110146864788));
#47693=CARTESIAN_POINT('Ctrl Pts',(-26.0706194607177,21.541752987898,13.6916071686117));
#47694=CARTESIAN_POINT('Ctrl Pts',(-26.0794596300327,21.5528964428244,13.6907120177312));
#47695=CARTESIAN_POINT('Ctrl Pts',(-26.0912801569453,21.5680011020296,13.6895119044692));
#47696=CARTESIAN_POINT('Ctrl Pts',(-26.0943254086276,21.5719109736385,13.6892024384589));
#47697=CARTESIAN_POINT('Ctrl Pts',(-26.0988354045288,21.5777290998046,13.6887437122166));
#47698=CARTESIAN_POINT('Ctrl Pts',(-26.1003070323245,21.5796319713211,13.6885939630911));
#47699=CARTESIAN_POINT('Ctrl Pts',(-26.1029217449372,21.583020729207,13.6883277832372));
#47700=CARTESIAN_POINT('Ctrl Pts',(-26.1040656629729,21.5845059642209,13.6882112928368));
#47701=CARTESIAN_POINT('Ctrl Pts',(-26.1064855165773,21.5876535199874,13.687964786936));
#47702=CARTESIAN_POINT('Ctrl Pts',(-26.1077611236758,21.5893160830153,13.6878347950183));
#47703=CARTESIAN_POINT('Ctrl Pts',(-26.1111634413813,21.5937594622139,13.6874879461592));
#47704=CARTESIAN_POINT('Ctrl Pts',(-26.113287251615,21.5965425114927,13.6872712959045));
#47705=CARTESIAN_POINT('Ctrl Pts',(-26.1232505719789,21.6096426925679,13.6862542533915));
#47706=CARTESIAN_POINT('Ctrl Pts',(-26.1310324927651,21.6200037733788,13.6854578923549));
#47707=CARTESIAN_POINT('Ctrl Pts',(-26.3141792691389,21.8669384693518,13.6666605042191));
#47708=CARTESIAN_POINT('Ctrl Pts',(-26.4563944933373,22.1264394265528,13.6507663448529));
#47709=CARTESIAN_POINT('Ctrl Pts',(-26.5793638075808,22.4488230248718,13.6313490032783));
#47710=CARTESIAN_POINT('Ctrl Pts',(-26.5962319125702,22.4963685335879,13.6284962472395));
#47711=CARTESIAN_POINT('Ctrl Pts',(-26.618021047271,22.5626853976568,13.6245160554373));
#47712=CARTESIAN_POINT('Ctrl Pts',(-26.6238992846075,22.5811353396411,13.6234086281098));
#47713=CARTESIAN_POINT('Ctrl Pts',(-26.6431807950287,22.6435945291476,13.6196572815646));
#47714=CARTESIAN_POINT('Ctrl Pts',(-26.6558075343745,22.6878362453225,13.6169961035464));
#47715=CARTESIAN_POINT('Ctrl Pts',(-26.674571957731,22.7593505421771,13.6126768553445));
#47716=CARTESIAN_POINT('Ctrl Pts',(-26.6813095879346,22.786459707332,13.6110355537942));
#47717=CARTESIAN_POINT('Ctrl Pts',(-26.6902151184922,22.824391525728,13.6087316088405));
#47718=CARTESIAN_POINT('Ctrl Pts',(-26.6926812263959,22.8351433505509,13.608077730291));
#47719=CARTESIAN_POINT('Ctrl Pts',(-26.7068008428178,22.89818621722,13.6042384998317));
#47720=CARTESIAN_POINT('Ctrl Pts',(-26.7172036412301,22.9507461764746,13.6010163749191));
#47721=CARTESIAN_POINT('Ctrl Pts',(-26.7277779746316,23.0121759259912,13.5972178307639));
#47722=CARTESIAN_POINT('Ctrl Pts',(-26.7292295042233,23.0208190799182,13.5966826337563));
#47723=CARTESIAN_POINT('Ctrl Pts',(-26.7313397112716,23.0337059602368,13.5958835179731));
#47724=CARTESIAN_POINT('Ctrl Pts',(-26.7320251997566,23.0379453064432,13.5956204523088));
#47725=CARTESIAN_POINT('Ctrl Pts',(-26.7332324337978,23.0455072324914,13.595150877286));
#47726=CARTESIAN_POINT('Ctrl Pts',(-26.733757456428,23.0488292889921,13.5949444724148));
#47727=CARTESIAN_POINT('Ctrl Pts',(-26.734762120129,23.0552514364337,13.5945452307467));
#47728=CARTESIAN_POINT('Ctrl Pts',(-26.7352424372382,23.0583514190571,13.5943524156855));
#47729=CARTESIAN_POINT('Ctrl Pts',(-26.7362724017622,23.06506359927,13.5939347071687));
#47730=CARTESIAN_POINT('Ctrl Pts',(-26.7368204334175,23.0686760370997,13.5937097626457));
#47731=CARTESIAN_POINT('Ctrl Pts',(-26.7381354263979,23.0774445520917,13.5931634152084));
#47732=CARTESIAN_POINT('Ctrl Pts',(-26.7388960214375,23.0826015606422,13.5928418105684));
#47733=CARTESIAN_POINT('Ctrl Pts',(-26.7409282409558,23.096615946823,13.5919670585872));
#47734=CARTESIAN_POINT('Ctrl Pts',(-26.7421754859368,23.1054767630348,13.5914131392337));
#47735=CARTESIAN_POINT('Ctrl Pts',(-26.7632251569263,23.259670090473,13.5817590082109));
#47736=CARTESIAN_POINT('Ctrl Pts',(-26.7731168665485,23.4061570475411,13.5723436394165));
#47737=CARTESIAN_POINT('Ctrl Pts',(-26.7730015348059,23.552787377377,13.5626736252116));
#47738=CARTESIAN_POINT('Ctrl Pts',(-22.075954775016,26.4137025163198,13.1538544762662));
#47739=CARTESIAN_POINT('Ctrl Pts',(-22.7503891714052,26.7532021541,13.2004027990139));
#47740=CARTESIAN_POINT('Ctrl Pts',(-24.6803998219367,27.0228698900686,13.3132467588865));
#47741=CARTESIAN_POINT('Ctrl Pts',(-26.5420719176933,25.3662309742614,13.4488859160352));
#47742=CARTESIAN_POINT('Ctrl Pts',(-26.7722508965562,23.9227962910001,13.5379767504363));
#47743=CARTESIAN_POINT('Ctrl Pts',(-26.7696996717685,23.55268397525,13.5607719477124));
#47744=CARTESIAN_POINT('Ctrl Pts',(-22.0750360153462,26.4155367745564,12.9101997884793));
#47745=CARTESIAN_POINT('Ctrl Pts',(-22.0760890146292,26.4160789203968,12.9102736565607));
#47746=CARTESIAN_POINT('Ctrl Pts',(-22.0771423149283,26.4166204868775,12.9103474882914));
#47747=CARTESIAN_POINT('Ctrl Pts',(-22.080292118416,26.4182377998639,12.9105681034007));
#47748=CARTESIAN_POINT('Ctrl Pts',(-22.0823895089747,26.4193118307784,12.9107147784804));
#47749=CARTESIAN_POINT('Ctrl Pts',(-22.0859959120397,26.4211536064108,12.9109665878938));
#47750=CARTESIAN_POINT('Ctrl Pts',(-22.0875043503513,26.4219224617247,12.9110717929643));
#47751=CARTESIAN_POINT('Ctrl Pts',(-22.0906273645983,26.4235111718192,12.911289360033));
#47752=CARTESIAN_POINT('Ctrl Pts',(-22.0922420215443,26.4243308524444,12.9114017108153));
#47753=CARTESIAN_POINT('Ctrl Pts',(-22.0961688624288,26.4263201525001,12.9116746204702));
#47754=CARTESIAN_POINT('Ctrl Pts',(-22.0984817724824,26.4274883474522,12.9118350888975));
#47755=CARTESIAN_POINT('Ctrl Pts',(-22.1071737908921,26.4318653265521,12.9124371119949));
#47756=CARTESIAN_POINT('Ctrl Pts',(-22.1135622114161,26.4350557273318,12.9128775142274));
#47757=CARTESIAN_POINT('Ctrl Pts',(-22.2186652618329,26.4871088486118,12.9200899813498));
#47758=CARTESIAN_POINT('Ctrl Pts',(-22.3198230877258,26.5309066618636,12.9265539691476));
#47759=CARTESIAN_POINT('Ctrl Pts',(-22.646552758391,26.6528913009366,12.9465547385214));
#47760=CARTESIAN_POINT('Ctrl Pts',(-22.8786490089429,26.7112650881736,12.95954054459));
#47761=CARTESIAN_POINT('Ctrl Pts',(-23.2571233585094,26.7628443401656,12.981298976024));
#47762=CARTESIAN_POINT('Ctrl Pts',(-23.4002906374693,26.7727010411547,12.989646639936));
#47763=CARTESIAN_POINT('Ctrl Pts',(-23.5582327225904,26.7730257484614,12.9991906553933));
#47764=CARTESIAN_POINT('Ctrl Pts',(-23.572838277788,26.772956483871,13.0000762728136));
#47765=CARTESIAN_POINT('Ctrl Pts',(-23.5982051001567,26.7726637343368,13.0016199073607));
#47766=CARTESIAN_POINT('Ctrl Pts',(-23.6089667321288,26.7724856154407,13.0022764992294));
#47767=CARTESIAN_POINT('Ctrl Pts',(-23.6243836749394,26.7721531864686,13.0032196501878));
#47768=CARTESIAN_POINT('Ctrl Pts',(-23.6290399388523,26.7720426862119,13.0035048334076));
#47769=CARTESIAN_POINT('Ctrl Pts',(-23.6371305274474,26.7718331345573,13.0040009394578));
#47770=CARTESIAN_POINT('Ctrl Pts',(-23.6405649722276,26.7717386840511,13.0042117174934));
#47771=CARTESIAN_POINT('Ctrl Pts',(-23.6471269694284,26.7715477210139,13.0046147885852));
#47772=CARTESIAN_POINT('Ctrl Pts',(-23.6502545471095,26.7714521452262,13.0048070519888));
#47773=CARTESIAN_POINT('Ctrl Pts',(-23.6575601431357,26.7712182430976,13.0052565098583));
#47774=CARTESIAN_POINT('Ctrl Pts',(-23.661738034727,26.77107634244,13.0055138163829));
#47775=CARTESIAN_POINT('Ctrl Pts',(-23.6760973293548,26.7705606613993,13.0063991160263));
#47776=CARTESIAN_POINT('Ctrl Pts',(-23.6862771491114,26.770146732281,13.0070283692233));
#47777=CARTESIAN_POINT('Ctrl Pts',(-23.7927449871843,26.7653117697163,13.0136269347085));
#47778=CARTESIAN_POINT('Ctrl Pts',(-23.88878116157,26.7566217633932,13.01973004565));
#47779=CARTESIAN_POINT('Ctrl Pts',(-24.2839818400787,26.7029088247568,13.0455108545032));
#47780=CARTESIAN_POINT('Ctrl Pts',(-24.5764414252619,26.6201841589304,13.0663676788769));
#47781=CARTESIAN_POINT('Ctrl Pts',(-24.884913959955,26.4838533225825,13.088838012318));
#47782=CARTESIAN_POINT('Ctrl Pts',(-24.9165942187286,26.4692327078018,13.0911490913798));
#47783=CARTESIAN_POINT('Ctrl Pts',(-25.0103204564478,26.4241171910422,13.0979845306184));
#47784=CARTESIAN_POINT('Ctrl Pts',(-25.0716339465085,26.3921351250051,13.1024537884725));
#47785=CARTESIAN_POINT('Ctrl Pts',(-25.141478640888,26.3527939668892,13.1075023968045));
#47786=CARTESIAN_POINT('Ctrl Pts',(-25.1510535519037,26.3473358569926,13.1081935486535));
#47787=CARTESIAN_POINT('Ctrl Pts',(-25.1634851680768,26.3401645579504,13.109089471001));
#47788=CARTESIAN_POINT('Ctrl Pts',(-25.1663673317343,26.3384959942831,13.109297081865));
#47789=CARTESIAN_POINT('Ctrl Pts',(-25.171025855392,26.3357893971026,13.1096324790693));
#47790=CARTESIAN_POINT('Ctrl Pts',(-25.1728038073268,26.3347541304295,13.1097604451286));
#47791=CARTESIAN_POINT('Ctrl Pts',(-25.1762083808187,26.3327673457519,13.1100054065509));
#47792=CARTESIAN_POINT('Ctrl Pts',(-25.1778351541235,26.3318161065444,13.1101224192288));
#47793=CARTESIAN_POINT('Ctrl Pts',(-25.181564554116,26.3296309858585,13.1103905941957));
#47794=CARTESIAN_POINT('Ctrl Pts',(-25.1836666204961,26.3283961421954,13.1105416933428));
#47795=CARTESIAN_POINT('Ctrl Pts',(-25.1902967095267,26.3244912181555,13.1110180990837));
#47796=CARTESIAN_POINT('Ctrl Pts',(-25.1948196313349,26.3218124264839,13.1113428386469));
#47797=CARTESIAN_POINT('Ctrl Pts',(-25.2321372554418,26.2995867976096,13.1140202517666));
#47798=CARTESIAN_POINT('Ctrl Pts',(-25.2645905381461,26.2794686542824,13.1163362588766));
#47799=CARTESIAN_POINT('Ctrl Pts',(-25.3059258847923,26.2528160661589,13.1192802894086));
#47800=CARTESIAN_POINT('Ctrl Pts',(-25.3151409452556,26.2468072733507,13.1199362335319));
#47801=CARTESIAN_POINT('Ctrl Pts',(-25.5777990613099,26.0736146373945,13.1386272168853));
#47802=CARTESIAN_POINT('Ctrl Pts',(-25.8064128810081,25.8714792483265,13.1548754515252));
#47803=CARTESIAN_POINT('Ctrl Pts',(-26.0665089258595,25.5662011070761,13.177727505221));
#47804=CARTESIAN_POINT('Ctrl Pts',(-26.1262497525851,25.4892808652838,13.1833574408407));
#47805=CARTESIAN_POINT('Ctrl Pts',(-26.2189731775053,25.3580307571731,13.1928676325672));
#47806=CARTESIAN_POINT('Ctrl Pts',(-26.2539955130713,25.3052183546097,13.1966699218102));
#47807=CARTESIAN_POINT('Ctrl Pts',(-26.2918666083502,25.2442832987771,13.2010432347214));
#47808=CARTESIAN_POINT('Ctrl Pts',(-26.2962684182788,25.2371386374133,13.2015557908225));
#47809=CARTESIAN_POINT('Ctrl Pts',(-26.302841328439,25.2263761191056,13.2023275972631));
#47810=CARTESIAN_POINT('Ctrl Pts',(-26.3050333350008,25.2227710187991,13.2025860784789));
#47811=CARTESIAN_POINT('Ctrl Pts',(-26.308792179942,25.2165615694073,13.2030312078137));
#47812=CARTESIAN_POINT('Ctrl Pts',(-26.3103624291416,25.2139592829061,13.2032177305503));
#47813=CARTESIAN_POINT('Ctrl Pts',(-26.3135896837366,25.2085937895922,13.2036022621594));
#47814=CARTESIAN_POINT('Ctrl Pts',(-26.315246230912,25.2058303120063,13.2038002875527));
#47815=CARTESIAN_POINT('Ctrl Pts',(-26.3192259095221,25.1991687174601,13.2042775838279));
#47816=CARTESIAN_POINT('Ctrl Pts',(-26.3215449527221,25.195268176491,13.2045570036859));
#47817=CARTESIAN_POINT('Ctrl Pts',(-26.3286420848976,25.1832734742668,13.2054161140473));
#47818=CARTESIAN_POINT('Ctrl Pts',(-26.3333929758748,25.1751633517673,13.205996793527));
#47819=CARTESIAN_POINT('Ctrl Pts',(-26.3887460526593,25.0797166095454,13.2128286304378));
#47820=CARTESIAN_POINT('Ctrl Pts',(-26.4352486133737,24.9900788273038,13.2192269687596));
#47821=CARTESIAN_POINT('Ctrl Pts',(-26.4918457529391,24.867191615932,13.2279890482217));
#47822=CARTESIAN_POINT('Ctrl Pts',(-26.5057250071247,24.8357413679618,13.2302304104488));
#47823=CARTESIAN_POINT('Ctrl Pts',(-26.6176680867532,24.5706787501887,13.2491074577465));
#47824=CARTESIAN_POINT('Ctrl Pts',(-26.6883655152247,24.3264806809558,13.2665125650853));
#47825=CARTESIAN_POINT('Ctrl Pts',(-26.7493352292583,23.9581643472272,13.2914621421967));
#47826=CARTESIAN_POINT('Ctrl Pts',(-26.7623088510815,23.838737874378,13.2993398647134));
#47827=CARTESIAN_POINT('Ctrl Pts',(-26.7689189370707,23.7125603529907,13.3072585501932));
#47828=CARTESIAN_POINT('Ctrl Pts',(-26.7692300990929,23.7062675314069,13.3076524153361));
#47829=CARTESIAN_POINT('Ctrl Pts',(-26.7696461141904,23.6973224745093,13.3082107353359));
#47830=CARTESIAN_POINT('Ctrl Pts',(-26.769766145568,23.6946710114692,13.3083760374412));
#47831=CARTESIAN_POINT('Ctrl Pts',(-26.7699670758576,23.6901077358023,13.3086601930956));
#47832=CARTESIAN_POINT('Ctrl Pts',(-26.7700495477356,23.688195996838,13.308779135795));
#47833=CARTESIAN_POINT('Ctrl Pts',(-26.7702043966908,23.6845307120772,13.3090069829559));
#47834=CARTESIAN_POINT('Ctrl Pts',(-26.7702770439217,23.6827771834125,13.3091159027087));
#47835=CARTESIAN_POINT('Ctrl Pts',(-26.7704449153017,23.6786435324645,13.309372462334));
#47836=CARTESIAN_POINT('Ctrl Pts',(-26.7705389332734,23.6762633582622,13.3095200338033));
#47837=CARTESIAN_POINT('Ctrl Pts',(-26.7708091326994,23.6692250955594,13.3099559505528));
#47838=CARTESIAN_POINT('Ctrl Pts',(-26.7709778479184,23.6645667010217,13.3102438770115));
#47839=CARTESIAN_POINT('Ctrl Pts',(-26.7723687797822,23.6237111620692,13.3127640120366));
#47840=CARTESIAN_POINT('Ctrl Pts',(-26.7729909022866,23.5874943287455,13.3149631334267));
#47841=CARTESIAN_POINT('Ctrl Pts',(-26.7730347348718,23.4490485647083,13.3232625536465));
#47842=CARTESIAN_POINT('Ctrl Pts',(-26.768203290968,23.3468706993055,13.3291653882643));
#47843=CARTESIAN_POINT('Ctrl Pts',(-26.7245388259226,22.8878173385831,13.3553517595979));
#47844=CARTESIAN_POINT('Ctrl Pts',(-26.6311313745349,22.5387659216273,13.3746802204848));
#47845=CARTESIAN_POINT('Ctrl Pts',(-26.4736680397546,22.1937220673131,13.3976168869846));
#47846=CARTESIAN_POINT('Ctrl Pts',(-26.4650289741884,22.175257479284,13.3988556169586));
#47847=CARTESIAN_POINT('Ctrl Pts',(-26.453511735187,22.1512376404951,13.4004822896714));
#47848=CARTESIAN_POINT('Ctrl Pts',(-26.4507916142844,22.1456067763672,13.4008647268163));
#47849=CARTESIAN_POINT('Ctrl Pts',(-26.4465751959254,22.1369429319076,13.4014548734712));
#47850=CARTESIAN_POINT('Ctrl Pts',(-26.4450904736969,22.1339043084132,13.401662178525));
#47851=CARTESIAN_POINT('Ctrl Pts',(-26.4421285801691,22.1278666279533,13.4020747407217));
#47852=CARTESIAN_POINT('Ctrl Pts',(-26.4406515197578,22.1248675210497,13.4022799937911));
#47853=CARTESIAN_POINT('Ctrl Pts',(-26.4373730587202,22.1182367990171,13.4027344995731));
#47854=CARTESIAN_POINT('Ctrl Pts',(-26.4355694692152,22.1146062779029,13.4029838287909));
#47855=CARTESIAN_POINT('Ctrl Pts',(-26.4303643763494,22.1041781551492,13.4037013577848));
#47856=CARTESIAN_POINT('Ctrl Pts',(-26.4269456845719,22.0973892061115,13.4041701609419));
#47857=CARTESIAN_POINT('Ctrl Pts',(-26.404204648655,22.052624271167,13.4072725205479));
#47858=CARTESIAN_POINT('Ctrl Pts',(-26.3841555797846,22.0150241039054,13.4099316447025));
#47859=CARTESIAN_POINT('Ctrl Pts',(-26.3231253757619,21.9058388102278,13.4178160986461));
#47860=CARTESIAN_POINT('Ctrl Pts',(-26.2801372682049,21.835420857111,13.4231120440113));
#47861=CARTESIAN_POINT('Ctrl Pts',(-26.0690549651572,21.5177360086348,13.4480027342875));
#47862=CARTESIAN_POINT('Ctrl Pts',(-25.869805189754,21.293014867854,13.4686949538292));
#47863=CARTESIAN_POINT('Ctrl Pts',(-25.5748066288183,21.0412262900228,13.4943371255897));
#47864=CARTESIAN_POINT('Ctrl Pts',(-25.5047699577869,20.9862913336202,13.50011089492));
#47865=CARTESIAN_POINT('Ctrl Pts',(-25.4273499192802,20.9305838730474,13.5060901028499));
#47866=CARTESIAN_POINT('Ctrl Pts',(-25.4221462904076,20.9268630750309,13.5064900938947));
#47867=CARTESIAN_POINT('Ctrl Pts',(-25.4149139261054,20.9217241272722,13.50704337492));
#47868=CARTESIAN_POINT('Ctrl Pts',(-25.4128946285229,20.920292815675,13.5071975667357));
#47869=CARTESIAN_POINT('Ctrl Pts',(-25.4094208628145,20.9178365605755,13.507462326605));
#47870=CARTESIAN_POINT('Ctrl Pts',(-25.4079671951702,20.9168104955782,13.5075729723746));
#47871=CARTESIAN_POINT('Ctrl Pts',(-25.4049625146326,20.9146933808315,13.5078013657549));
#47872=CARTESIAN_POINT('Ctrl Pts',(-25.4034113914225,20.9136024981986,13.50791910133));
#47873=CARTESIAN_POINT('Ctrl Pts',(-25.3997671861678,20.9110443854657,13.5081953138826));
#47874=CARTESIAN_POINT('Ctrl Pts',(-25.3976733142084,20.9095782714579,13.5083537134177));
#47875=CARTESIAN_POINT('Ctrl Pts',(-25.3908665849309,20.90482430731,13.5088676527205));
#47876=CARTESIAN_POINT('Ctrl Pts',(-25.3861466434397,20.9015465466883,13.5092225007244));
#47877=CARTESIAN_POINT('Ctrl Pts',(-25.2511836191136,20.8083556309474,13.5193263145242));
#47878=CARTESIAN_POINT('Ctrl Pts',(-25.1144805777191,20.728130748235,13.5284293807049));
#47879=CARTESIAN_POINT('Ctrl Pts',(-24.6685525390206,20.5088410142806,13.5564727088257));
#47880=CARTESIAN_POINT('Ctrl Pts',(-24.3430778271196,20.4082470927213,13.5748796902867));
#47881=CARTESIAN_POINT('Ctrl Pts',(-23.9881273839712,20.3573255984267,13.5965702006371));
#47882=CARTESIAN_POINT('Ctrl Pts',(-23.9683236576181,20.3546722568234,13.5977844985711));
#47883=CARTESIAN_POINT('Ctrl Pts',(-23.9423401133947,20.3514365969539,13.5993835152735));
#47884=CARTESIAN_POINT('Ctrl Pts',(-23.9361811806791,20.3506876967339,13.5997629588706));
#47885=CARTESIAN_POINT('Ctrl Pts',(-23.9266715942994,20.3495592282707,13.6003495006943));
#47886=CARTESIAN_POINT('Ctrl Pts',(-23.9233224195391,20.3491671232868,13.6005562024325));
#47887=CARTESIAN_POINT('Ctrl Pts',(-23.9166508749906,20.3483966639437,13.6009682088982));
#47888=CARTESIAN_POINT('Ctrl Pts',(-23.913328519315,20.3480182225128,13.6011735106033));
#47889=CARTESIAN_POINT('Ctrl Pts',(-23.9060424069379,20.3471997640689,13.6016240298211));
#47890=CARTESIAN_POINT('Ctrl Pts',(-23.9020784146447,20.3467619330852,13.6018693160478));
#47891=CARTESIAN_POINT('Ctrl Pts',(-23.8907590929466,20.3455329540814,13.6025702655101));
#47892=CARTESIAN_POINT('Ctrl Pts',(-23.8834018738874,20.3447597764809,13.6030264953344));
#47893=CARTESIAN_POINT('Ctrl Pts',(-23.8668828130589,20.3430812568386,13.6040523096185));
#47894=CARTESIAN_POINT('Ctrl Pts',(-23.8577196509148,20.3421898313867,13.60462233003));
#47895=CARTESIAN_POINT('Ctrl Pts',(-23.6527883668902,20.3231394437953,13.6173934318721));
#47896=CARTESIAN_POINT('Ctrl Pts',(-23.4558072222142,20.3228965132843,13.6301731140655));
#47897=CARTESIAN_POINT('Ctrl Pts',(-23.0307682693458,20.3613249300302,13.658721940921));
#47898=CARTESIAN_POINT('Ctrl Pts',(-22.8043635805349,20.4065650467632,13.6745575817468));
#47899=CARTESIAN_POINT('Ctrl Pts',(-22.5201407739078,20.4958183519919,13.6941524000776));
#47900=CARTESIAN_POINT('Ctrl Pts',(-22.4562171518796,20.5181267906043,13.6985349497666));
#47901=CARTESIAN_POINT('Ctrl Pts',(-22.3802338547722,20.5473602443118,13.7036760110389));
#47902=CARTESIAN_POINT('Ctrl Pts',(-22.3674604181117,20.5523685069095,13.7045378970302));
#47903=CARTESIAN_POINT('Ctrl Pts',(-22.3512821714888,20.558831241537,13.7056261486081));
#47904=CARTESIAN_POINT('Ctrl Pts',(-22.3478476047982,20.5602101152792,13.7058569855419));
#47905=CARTESIAN_POINT('Ctrl Pts',(-22.3424103242237,20.5624039011325,13.7062221086276));
#47906=CARTESIAN_POINT('Ctrl Pts',(-22.340406055446,20.5632149120328,13.70635663071));
#47907=CARTESIAN_POINT('Ctrl Pts',(-22.3368467890316,20.5646593100148,13.7065953977134));
#47908=CARTESIAN_POINT('Ctrl Pts',(-22.3352914789837,20.565291891738,13.706699690941));
#47909=CARTESIAN_POINT('Ctrl Pts',(-22.3316789953829,20.5667644662592,13.7069418333288));
#47910=CARTESIAN_POINT('Ctrl Pts',(-22.3296221991345,20.5676053699772,13.7070796260104));
#47911=CARTESIAN_POINT('Ctrl Pts',(-22.3237978543273,20.5699936376472,13.7074696187913));
#47912=CARTESIAN_POINT('Ctrl Pts',(-22.3200323499259,20.5715460245026,13.7077215133138));
#47913=CARTESIAN_POINT('Ctrl Pts',(-22.2971763626606,20.5810194883337,13.7092490701682));
#47914=CARTESIAN_POINT('Ctrl Pts',(-22.2781589322225,20.5891171618776,13.7105141367341));
#47915=CARTESIAN_POINT('Ctrl Pts',(-22.2214289227027,20.613920370587,13.7142738294222));
#47916=CARTESIAN_POINT('Ctrl Pts',(-22.1839564161904,20.6311680827679,13.7167384920901));
#47917=CARTESIAN_POINT('Ctrl Pts',(-22.0764232280724,20.6831876948469,13.7237854978818));
#47918=CARTESIAN_POINT('Ctrl Pts',(-22.0072812818265,20.7197976411985,13.728284664035));
#47919=CARTESIAN_POINT('Ctrl Pts',(-21.6375772939359,20.9331301008273,13.7525249196615));
#47920=CARTESIAN_POINT('Ctrl Pts',(-21.3659135028519,21.1551898971024,13.7713129099303));
#47921=CARTESIAN_POINT('Ctrl Pts',(-21.1158498725972,21.4382286045062,13.7940422155562));
#47922=CARTESIAN_POINT('Ctrl Pts',(-21.096912505344,21.4602563581055,13.7958022358817));
#47923=CARTESIAN_POINT('Ctrl Pts',(-21.0741486228984,21.4874708231131,13.7979671272959));
#47924=CARTESIAN_POINT('Ctrl Pts',(-21.0700360965401,21.4924174123866,13.7983602450613));
#47925=CARTESIAN_POINT('Ctrl Pts',(-21.0632782032856,21.5005955620775,13.7990095732424));
#47926=CARTESIAN_POINT('Ctrl Pts',(-21.0606242452798,21.5038200264582,13.7992654335999));
#47927=CARTESIAN_POINT('Ctrl Pts',(-21.0558519428783,21.5096412273421,13.7997270688794));
#47928=CARTESIAN_POINT('Ctrl Pts',(-21.0537313636026,21.5122361308597,13.799932752758));
#47929=CARTESIAN_POINT('Ctrl Pts',(-21.0492648360855,21.5177191485434,13.8003671572195));
#47930=CARTESIAN_POINT('Ctrl Pts',(-21.0469198359111,21.5206080255684,13.8005959157108));
#47931=CARTESIAN_POINT('Ctrl Pts',(-21.040769208546,21.5282120452587,13.8011977382662));
#47932=CARTESIAN_POINT('Ctrl Pts',(-21.0369718804037,21.532933854591,13.8015711360437));
#47933=CARTESIAN_POINT('Ctrl Pts',(-21.0286167171303,21.5433833378178,13.8023968032338));
#47934=CARTESIAN_POINT('Ctrl Pts',(-21.0240650439164,21.5491158752423,13.8028493175737));
#47935=CARTESIAN_POINT('Ctrl Pts',(-21.0106587592742,21.566118851554,13.8041902215362));
#47936=CARTESIAN_POINT('Ctrl Pts',(-21.0018598479592,21.5774327962996,13.8050808247874));
#47937=CARTESIAN_POINT('Ctrl Pts',(-20.9087485621644,21.698820862043,13.8146194174393));
#47938=CARTESIAN_POINT('Ctrl Pts',(-20.8315597064804,21.8141527200699,13.8235457822466));
#47939=CARTESIAN_POINT('Ctrl Pts',(-20.6746932833012,22.0847779560447,13.8441926274079));
#47940=CARTESIAN_POINT('Ctrl Pts',(-20.599709757958,22.2422978238224,13.8560167135887));
#47941=CARTESIAN_POINT('Ctrl Pts',(-20.4837734195369,22.5472758794155,13.8780734134664));
#47942=CARTESIAN_POINT('Ctrl Pts',(-20.4398502988963,22.6931271115699,13.8882849208496));
#47943=CARTESIAN_POINT('Ctrl Pts',(-20.4054318759038,22.8458097148962,13.8983046391235));
#47944=CARTESIAN_POINT('Ctrl Pts',(-20.4044800493325,22.8500724627846,13.8985838450503));
#47945=CARTESIAN_POINT('Ctrl Pts',(-20.4024435578289,22.859280852079,13.8991858126033));
#47946=CARTESIAN_POINT('Ctrl Pts',(-20.4013618734185,22.8642271524552,13.8995084306072));
#47947=CARTESIAN_POINT('Ctrl Pts',(-20.3984111900931,22.8778739840161,13.9003964833664));
#47948=CARTESIAN_POINT('Ctrl Pts',(-20.3965665477139,22.8865798167594,13.9009607112578));
#47949=CARTESIAN_POINT('Ctrl Pts',(-20.3918123744017,22.9094847047598,13.902438958579));
#47950=CARTESIAN_POINT('Ctrl Pts',(-20.3889624859441,22.9236961489612,13.9033498670902));
#47951=CARTESIAN_POINT('Ctrl Pts',(-20.3854907058621,22.9416357222806,13.9044914169664));
#47952=CARTESIAN_POINT('Ctrl Pts',(-20.384779421142,22.9453460747408,13.9047270702611));
#47953=CARTESIAN_POINT('Ctrl Pts',(-20.3836679842414,22.9511994299092,13.9050981154988));
#47954=CARTESIAN_POINT('Ctrl Pts',(-20.3832634821689,22.9533415875995,13.9052337562961));
#47955=CARTESIAN_POINT('Ctrl Pts',(-20.3825170624198,22.9573165862676,13.9054851699103));
#47956=CARTESIAN_POINT('Ctrl Pts',(-20.3821745637353,22.9591493024321,13.9056009754381));
#47957=CARTESIAN_POINT('Ctrl Pts',(-20.3814161645905,22.96322710267,13.9058583958888));
#47958=CARTESIAN_POINT('Ctrl Pts',(-20.3810010605094,22.9654723265994,13.9059999643676));
#47959=CARTESIAN_POINT('Ctrl Pts',(-20.379800430283,22.9720051489733,13.9064114004878));
#47960=CARTESIAN_POINT('Ctrl Pts',(-20.3790212124724,22.9762939238804,13.9066809068463));
#47961=CARTESIAN_POINT('Ctrl Pts',(-20.3735946130188,23.0065100784415,13.9085755479458));
#47962=CARTESIAN_POINT('Ctrl Pts',(-20.3692563764936,23.0324929774112,13.9101832935549));
#47963=CARTESIAN_POINT('Ctrl Pts',(-20.3585719392816,23.1016984708984,13.9144155976454));
#47964=CARTESIAN_POINT('Ctrl Pts',(-20.3527849295169,23.1450031264455,13.9170123869929));
#47965=CARTESIAN_POINT('Ctrl Pts',(-20.3379678712164,23.2761383443914,13.924756717945));
#47966=CARTESIAN_POINT('Ctrl Pts',(-20.3316639958613,23.3642386013023,13.9297992730091));
#47967=CARTESIAN_POINT('Ctrl Pts',(-20.3210667793382,23.7134220287852,13.9495249199212));
#47968=CARTESIAN_POINT('Ctrl Pts',(-20.3448790640442,23.9743333519304,13.9637765785128));
#47969=CARTESIAN_POINT('Ctrl Pts',(-20.4194232271444,24.3200607830885,13.9844181801597));
#47970=CARTESIAN_POINT('Ctrl Pts',(-20.4428385409979,24.4097132036604,13.9899271140004));
#47971=CARTESIAN_POINT('Ctrl Pts',(-20.4730863232288,24.5079947382254,13.9961869154009));
#47972=CARTESIAN_POINT('Ctrl Pts',(-20.4761389306971,24.5177480474846,13.9968105566313));
#47973=CARTESIAN_POINT('Ctrl Pts',(-20.4804860031172,24.5314089746514,13.997687521106));
#47974=CARTESIAN_POINT('Ctrl Pts',(-20.4817416640941,24.5353289554771,13.9979395658332));
#47975=CARTESIAN_POINT('Ctrl Pts',(-20.4840558789441,24.5425062188146,13.9984017852077));
#47976=CARTESIAN_POINT('Ctrl Pts',(-20.4851121235143,24.5457642448076,13.9986118834421));
#47977=CARTESIAN_POINT('Ctrl Pts',(-20.4871489451164,24.5520129251808,13.9990153776024));
#47978=CARTESIAN_POINT('Ctrl Pts',(-20.4881287137721,24.5550038400616,13.9992087465906));
#47979=CARTESIAN_POINT('Ctrl Pts',(-20.4905962669691,24.5624993440383,13.9996939451103));
#47980=CARTESIAN_POINT('Ctrl Pts',(-20.4920896157727,24.5670020813231,13.9999859584437));
#47981=CARTESIAN_POINT('Ctrl Pts',(-20.4971596543363,24.5821770121503,14.0009719305907));
#47982=CARTESIAN_POINT('Ctrl Pts',(-20.500782279691,24.5928336691238,14.0016674097824));
#47983=CARTESIAN_POINT('Ctrl Pts',(-20.5095058313893,24.6180612201338,14.0033212212832));
#47984=CARTESIAN_POINT('Ctrl Pts',(-20.5146557424052,24.6326147677317,14.0042811721772));
#47985=CARTESIAN_POINT('Ctrl Pts',(-20.5332473982988,24.6839778961395,14.0076902441949));
#47986=CARTESIAN_POINT('Ctrl Pts',(-20.5472553029542,24.7205775306143,14.0101581279805));
#47987=CARTESIAN_POINT('Ctrl Pts',(-20.5940462911039,24.8364567802455,14.0180987416822));
#47988=CARTESIAN_POINT('Ctrl Pts',(-20.6293266849482,24.9146816368908,14.0236524448172));
#47989=CARTESIAN_POINT('Ctrl Pts',(-20.7276360862386,25.1113190746447,14.0381075927319));
#47990=CARTESIAN_POINT('Ctrl Pts',(-20.795009764753,25.2273704780872,14.0471241513402));
#47991=CARTESIAN_POINT('Ctrl Pts',(-20.9781336513916,25.5018414550085,14.0694452821793));
#47992=CARTESIAN_POINT('Ctrl Pts',(-21.1014997962609,25.6545617503964,14.0827769227213));
#47993=CARTESIAN_POINT('Ctrl Pts',(-21.2647199450713,25.8226811401634,14.0978547713474));
#47994=CARTESIAN_POINT('Ctrl Pts',(-21.2919495345811,25.8497435371589,14.1002948863727));
#47995=CARTESIAN_POINT('Ctrl Pts',(-21.3234573829001,25.8799582306063,14.1030274144155));
#47996=CARTESIAN_POINT('Ctrl Pts',(-21.3272661127705,25.8835927684478,14.1033562487614));
#47997=CARTESIAN_POINT('Ctrl Pts',(-21.332852707056,25.8888977658009,14.1038363959952));
#47998=CARTESIAN_POINT('Ctrl Pts',(-21.334623564088,25.8905755417324,14.1039882751632));
#47999=CARTESIAN_POINT('Ctrl Pts',(-21.337765953823,25.8935459954563,14.1042572165494));
#48000=CARTESIAN_POINT('Ctrl Pts',(-21.3391367161578,25.8948394814423,14.1043743419131));
#48001=CARTESIAN_POINT('Ctrl Pts',(-21.3420056925938,25.8975419663331,14.1046190820237));
#48002=CARTESIAN_POINT('Ctrl Pts',(-21.343504117705,25.8989507306498,14.1047466785157));
#48003=CARTESIAN_POINT('Ctrl Pts',(-21.3474300513924,25.9026346758131,14.1050803940657));
#48004=CARTESIAN_POINT('Ctrl Pts',(-21.3498597443817,25.9049075411327,14.1052863332482));
#48005=CARTESIAN_POINT('Ctrl Pts',(-21.3605151682964,25.9148443018117,14.1061869160111));
#48006=CARTESIAN_POINT('Ctrl Pts',(-21.3687775812838,25.9224690078034,14.106878568695));
#48007=CARTESIAN_POINT('Ctrl Pts',(-21.4294746039489,25.9778960292262,14.1119124846623));
#48008=CARTESIAN_POINT('Ctrl Pts',(-21.483439762614,26.0240024568831,14.1161329555529));
#48009=CARTESIAN_POINT('Ctrl Pts',(-21.6538441684543,26.1601183743674,14.1288550348207));
#48010=CARTESIAN_POINT('Ctrl Pts',(-21.774962994599,26.2439707978081,14.1370797444969));
#48011=CARTESIAN_POINT('Ctrl Pts',(-21.9582948740137,26.353139221211,14.1490036783203));
#48012=CARTESIAN_POINT('Ctrl Pts',(-22.0162031362245,26.3852461586997,14.1526987592031));
#48013=CARTESIAN_POINT('Ctrl Pts',(-22.0750361586249,26.4155368483246,14.1564144975666));
#48014=CARTESIAN_POINT('Origin',(-23.5502525316942,23.5502525316942,-77.3107734492734));
#48015=CARTESIAN_POINT('',(-22.0750357147148,26.4155366197736,15.6517373095585));
#48016=CARTESIAN_POINT('',(-22.0750360153461,26.4155367745563,15.4070961373485));
#48017=CARTESIAN_POINT('',(-22.0750360153461,26.4155367745563,-77.3107734492734));
#48018=CARTESIAN_POINT('Ctrl Pts',(-22.0750357147148,26.4155366197736,15.6517373095584));
#48019=CARTESIAN_POINT('Ctrl Pts',(-21.9384970982726,26.3452385072826,15.6430022732087));
#48020=CARTESIAN_POINT('Ctrl Pts',(-21.8070317499559,26.265205804068,15.6345020377301));
#48021=CARTESIAN_POINT('Ctrl Pts',(-21.5085125180744,26.0527684592155,15.6139443619397));
#48022=CARTESIAN_POINT('Ctrl Pts',(-21.3479916439476,25.9127333323856,15.601804203723));
#48023=CARTESIAN_POINT('Ctrl Pts',(-21.1900717776686,25.7447889048543,15.5878405393531));
#48024=CARTESIAN_POINT('Ctrl Pts',(-21.1778231020358,25.7315415234239,15.5867430333099));
#48025=CARTESIAN_POINT('Ctrl Pts',(-21.1618319742737,25.7139525191278,15.5852906974511));
#48026=CARTESIAN_POINT('Ctrl Pts',(-21.1579887839497,25.7097025902243,15.5849401474905));
#48027=CARTESIAN_POINT('Ctrl Pts',(-21.1517223696583,25.7027357204763,15.5843660865009));
#48028=CARTESIAN_POINT('Ctrl Pts',(-21.1492923678544,25.700024870261,15.5841428618572));
#48029=CARTESIAN_POINT('Ctrl Pts',(-21.1446100582099,25.6947835593118,15.583711544893));
#48030=CARTESIAN_POINT('Ctrl Pts',(-21.1423571356176,25.6922536521561,15.5835034788338));
#48031=CARTESIAN_POINT('Ctrl Pts',(-21.137189668407,25.6864324182602,15.5830250086592));
#48032=CARTESIAN_POINT('Ctrl Pts',(-21.1342778660054,25.6831386759572,15.5827544901546));
#48033=CARTESIAN_POINT('Ctrl Pts',(-21.125075366183,25.6726860644171,15.5818966531688));
#48034=CARTESIAN_POINT('Ctrl Pts',(-21.1188097227842,25.6655052940877,15.5813082912353));
#48035=CARTESIAN_POINT('Ctrl Pts',(-21.0953017183096,25.6383213742806,15.5790844626406));
#48036=CARTESIAN_POINT('Ctrl Pts',(-21.0782739784902,25.6181347703707,15.5774401640783));
#48037=CARTESIAN_POINT('Ctrl Pts',(-21.0565590098194,25.5917398774904,15.5752987359473));
#48038=CARTESIAN_POINT('Ctrl Pts',(-21.0516431347031,25.5857203019246,15.5748109338653));
#48039=CARTESIAN_POINT('Ctrl Pts',(-21.0451056786475,25.5776557027918,15.5741581579396));
#48040=CARTESIAN_POINT('Ctrl Pts',(-21.0434647082,25.5756263691432,15.573993959663));
#48041=CARTESIAN_POINT('Ctrl Pts',(-21.038503961822,25.5694763146224,15.5734965332191));
#48042=CARTESIAN_POINT('Ctrl Pts',(-21.0351918804705,25.5653494236394,15.5731630003144));
#48043=CARTESIAN_POINT('Ctrl Pts',(-21.0306543579807,25.559667005313,15.5727040999479));
#48044=CARTESIAN_POINT('Ctrl Pts',(-21.0294201506534,25.5581184610922,15.5725790782482));
#48045=CARTESIAN_POINT('Ctrl Pts',(-21.0238710278884,25.5511428663055,15.5720160630685));
#48046=CARTESIAN_POINT('Ctrl Pts',(-21.0195722305097,25.5457030687679,15.5715774390762));
#48047=CARTESIAN_POINT('Ctrl Pts',(-21.0122285812516,25.5363483468505,15.5708238809107));
#48048=CARTESIAN_POINT('Ctrl Pts',(-21.0091751382871,25.532440171722,15.5705092815528));
#48049=CARTESIAN_POINT('Ctrl Pts',(-21.0036687341064,25.5253587594217,15.5699396368534));
#48050=CARTESIAN_POINT('Ctrl Pts',(-21.0012126474484,25.5221879559001,15.569684712209));
#48051=CARTESIAN_POINT('Ctrl Pts',(-20.9960801319971,25.5155362758231,15.5691502295933));
#48052=CARTESIAN_POINT('Ctrl Pts',(-20.9934048867823,25.5120544999665,15.5688706273495));
#48053=CARTESIAN_POINT('Ctrl Pts',(-20.9783132691954,25.4923297682804,15.5672875939356));
#48054=CARTESIAN_POINT('Ctrl Pts',(-20.9660447883879,25.4759747007311,15.5659786329155));
#48055=CARTESIAN_POINT('Ctrl Pts',(-20.7751907261955,25.2164394501035,15.5452635295142));
#48056=CARTESIAN_POINT('Ctrl Pts',(-20.6314863601676,24.9494983346909,15.5245266860199));
#48057=CARTESIAN_POINT('Ctrl Pts',(-20.4966844908557,24.5844220973162,15.4984908085983));
#48058=CARTESIAN_POINT('Ctrl Pts',(-20.469712358939,24.5010728270338,15.4927055812756));
#48059=CARTESIAN_POINT('Ctrl Pts',(-20.4392428266385,24.3919171950279,15.4854163446113));
#48060=CARTESIAN_POINT('Ctrl Pts',(-20.4326161323492,24.367029225528,15.4837734019697));
#48061=CARTESIAN_POINT('Ctrl Pts',(-20.4239229468351,24.3327316494013,15.4815378631532));
#48062=CARTESIAN_POINT('Ctrl Pts',(-20.421599425109,24.3233889924433,15.4809317992994));
#48063=CARTESIAN_POINT('Ctrl Pts',(-20.4182130136489,24.309507264424,15.4800357214841));
#48064=CARTESIAN_POINT('Ctrl Pts',(-20.4171180768358,24.304976176608,15.4797439360673));
#48065=CARTESIAN_POINT('Ctrl Pts',(-20.4153889809418,24.2977521866913,15.479279870633));
#48066=CARTESIAN_POINT('Ctrl Pts',(-20.4147484567957,24.2950608375608,15.4791072300335));
#48067=CARTESIAN_POINT('Ctrl Pts',(-20.4135590291707,24.2900343830949,15.4787852721389));
#48068=CARTESIAN_POINT('Ctrl Pts',(-20.4130092663402,24.2876994860683,15.4786359055207));
#48069=CARTESIAN_POINT('Ctrl Pts',(-20.412035780863,24.2835442066709,15.4783704268037));
#48070=CARTESIAN_POINT('Ctrl Pts',(-20.4116110342726,24.2817240666976,15.4782542550879));
#48071=CARTESIAN_POINT('Ctrl Pts',(-20.4107888606498,24.2781869563423,15.478028723327));
#48072=CARTESIAN_POINT('Ctrl Pts',(-20.4103912593126,24.276470032606,15.4779193531646));
#48073=CARTESIAN_POINT('Ctrl Pts',(-20.4094530964339,24.2724036806654,15.4776605649694));
#48074=CARTESIAN_POINT('Ctrl Pts',(-20.4089137614743,24.2700539663231,15.4775112182819));
#48075=CARTESIAN_POINT('Ctrl Pts',(-20.407314195797,24.26304911804,15.4770665606779));
#48076=CARTESIAN_POINT('Ctrl Pts',(-20.4062616663822,24.25839220456,15.4767716926295));
#48077=CARTESIAN_POINT('Ctrl Pts',(-20.3966254484465,24.2153117949452,15.4740506624236));
#48078=CARTESIAN_POINT('Ctrl Pts',(-20.3887357134796,24.1767342596741,15.4716636547151));
#48079=CARTESIAN_POINT('Ctrl Pts',(-20.381075756434,24.1354388437405,15.4691518318476));
#48080=CARTESIAN_POINT('Ctrl Pts',(-20.3806001753773,24.1328573658998,15.4689949916503));
#48081=CARTESIAN_POINT('Ctrl Pts',(-20.3798508359552,24.1287618379348,15.4687464452301));
#48082=CARTESIAN_POINT('Ctrl Pts',(-20.3795750080064,24.1272481734025,15.4686546459898));
#48083=CARTESIAN_POINT('Ctrl Pts',(-20.378758431994,24.1227487719266,15.4683819502308));
#48084=CARTESIAN_POINT('Ctrl Pts',(-20.3782208150995,24.119762460111,15.4682011933681));
#48085=CARTESIAN_POINT('Ctrl Pts',(-20.3774773245037,24.115598864017,15.4679494990604));
#48086=CARTESIAN_POINT('Ctrl Pts',(-20.3772678885358,24.114422227019,15.4678784057643));
#48087=CARTESIAN_POINT('Ctrl Pts',(-20.3297356349389,23.8465164972107,15.4516994338179));
#48088=CARTESIAN_POINT('Ctrl Pts',(-20.3162247375172,23.5748522487775,15.4370448082681));
#48089=CARTESIAN_POINT('Ctrl Pts',(-20.3474176136987,23.1666976550411,15.4139365461235));
#48090=CARTESIAN_POINT('Ctrl Pts',(-20.3668364614817,23.0295587740683,15.4059975116656));
#48091=CARTESIAN_POINT('Ctrl Pts',(-20.4065382737658,22.8386439934997,15.3944206003304));
#48092=CARTESIAN_POINT('Ctrl Pts',(-20.4195303497392,22.7835035150612,15.3910149770569));
#48093=CARTESIAN_POINT('Ctrl Pts',(-20.4360526038835,22.7208290905679,15.3870633792164));
#48094=CARTESIAN_POINT('Ctrl Pts',(-20.4381672332837,22.712929697573,15.3865638517416));
#48095=CARTESIAN_POINT('Ctrl Pts',(-20.441406838606,22.70100966333,15.3858078168937));
#48096=CARTESIAN_POINT('Ctrl Pts',(-20.4425096109953,22.6969829778683,15.3855520322035));
#48097=CARTESIAN_POINT('Ctrl Pts',(-20.4444270450495,22.6900346472625,15.3851099799567));
#48098=CARTESIAN_POINT('Ctrl Pts',(-20.445238014418,22.6871119813837,15.384923832905));
#48099=CARTESIAN_POINT('Ctrl Pts',(-20.4469236432282,22.6810702342247,15.3845385982831));
#48100=CARTESIAN_POINT('Ctrl Pts',(-20.4477988816613,22.6779513190964,15.3843394920006));
#48101=CARTESIAN_POINT('Ctrl Pts',(-20.4501846206382,22.6694987414862,15.3837992463022));
#48102=CARTESIAN_POINT('Ctrl Pts',(-20.4517041776177,22.6641676661421,15.3834578115614));
#48103=CARTESIAN_POINT('Ctrl Pts',(-20.4574252399326,22.6442910919145,15.3821821631118));
#48104=CARTESIAN_POINT('Ctrl Pts',(-20.4617154229795,22.6297715147562,15.3812450539191));
#48105=CARTESIAN_POINT('Ctrl Pts',(-20.5370512472136,22.3812644125251,15.3651140999572));
#48106=CARTESIAN_POINT('Ctrl Pts',(-20.6343829522037,22.1561320254541,15.3490034052628));
#48107=CARTESIAN_POINT('Ctrl Pts',(-20.8482050969422,21.7841426536676,15.3200419270049));
#48108=CARTESIAN_POINT('Ctrl Pts',(-20.9538001837811,21.6322731764394,15.3074377923054));
#48109=CARTESIAN_POINT('Ctrl Pts',(-21.1145341836154,21.4388883218212,15.2909334923109));
#48110=CARTESIAN_POINT('Ctrl Pts',(-21.1588381554949,21.3888359843137,15.2866178325179));
#48111=CARTESIAN_POINT('Ctrl Pts',(-21.2095996763094,21.3349617050405,15.281956982503));
#48112=CARTESIAN_POINT('Ctrl Pts',(-21.2145468206594,21.3297462673864,15.2815056114234));
#48113=CARTESIAN_POINT('Ctrl Pts',(-21.2221121193208,21.3218239455839,15.2808197809941));
#48114=CARTESIAN_POINT('Ctrl Pts',(-21.2247175965876,21.3191050670341,15.280584374788));
#48115=CARTESIAN_POINT('Ctrl Pts',(-21.2295406169146,21.3140897554197,15.280150085343));
#48116=CARTESIAN_POINT('Ctrl Pts',(-21.2317568139424,21.3117920427927,15.2799510994259));
#48117=CARTESIAN_POINT('Ctrl Pts',(-21.235373233458,21.3080537374451,15.2796273276305));
#48118=CARTESIAN_POINT('Ctrl Pts',(-21.2367713884605,21.3066111614458,15.279502380391));
#48119=CARTESIAN_POINT('Ctrl Pts',(-21.2394851735825,21.3038163900534,15.2792603026163));
#48120=CARTESIAN_POINT('Ctrl Pts',(-21.2408006384053,21.3024640464529,15.2791431601776));
#48121=CARTESIAN_POINT('Ctrl Pts',(-21.243828909392,21.299356343073,15.2788739520684));
#48122=CARTESIAN_POINT('Ctrl Pts',(-21.245542536554,21.2976017785014,15.2787219511919));
#48123=CARTESIAN_POINT('Ctrl Pts',(-21.2509897641034,21.2920371424173,15.2782398393461));
#48124=CARTESIAN_POINT('Ctrl Pts',(-21.2547308471595,21.2882343585588,15.2779103149811));
#48125=CARTESIAN_POINT('Ctrl Pts',(-21.286752279709,21.2558460556432,15.2751030837406));
#48126=CARTESIAN_POINT('Ctrl Pts',(-21.3155574730846,21.2277812556397,15.2726660967448));
#48127=CARTESIAN_POINT('Ctrl Pts',(-21.3479003953225,21.1974287464245,15.2700150887176));
#48128=CARTESIAN_POINT('Ctrl Pts',(-21.3509242650302,21.1946019054524,15.2697680400688));
#48129=CARTESIAN_POINT('Ctrl Pts',(-21.3597166360948,21.1864141134559,15.2690520098054));
#48130=CARTESIAN_POINT('Ctrl Pts',(-21.3654993893466,21.1810684344248,15.2685839412356));
#48131=CARTESIAN_POINT('Ctrl Pts',(-21.3748115487557,21.1725231979923,15.2678346662354));
#48132=CARTESIAN_POINT('Ctrl Pts',(-21.3783285209827,21.1693102084157,15.2675526995875));
#48133=CARTESIAN_POINT('Ctrl Pts',(-21.4571777339989,21.0975962625136,15.2612534538216));
#48134=CARTESIAN_POINT('Ctrl Pts',(-21.535713426737,21.03269015361,15.2554335131454));
#48135=CARTESIAN_POINT('Ctrl Pts',(-21.8046641279156,20.8310738832475,15.2364644558426));
#48136=CARTESIAN_POINT('Ctrl Pts',(-22.0068898575021,20.7114072452864,15.2236349585423));
#48137=CARTESIAN_POINT('Ctrl Pts',(-22.3170757046627,20.5708767963287,15.2039547327801));
#48138=CARTESIAN_POINT('Ctrl Pts',(-22.415948620411,20.5318496587097,15.1976912195881));
#48139=CARTESIAN_POINT('Ctrl Pts',(-22.5340659137831,20.491850353538,15.190139466232));
#48140=CARTESIAN_POINT('Ctrl Pts',(-22.5516212438534,20.4860732525825,15.1890154211229));
#48141=CARTESIAN_POINT('Ctrl Pts',(-22.5747324976437,20.4786875143426,15.1875331560615));
#48142=CARTESIAN_POINT('Ctrl Pts',(-22.5802446808093,20.4769423030995,15.1871794420625));
#48143=CARTESIAN_POINT('Ctrl Pts',(-22.589246227679,20.4741189546077,15.1866015063355));
#48144=CARTESIAN_POINT('Ctrl Pts',(-22.592732796947,20.4730318932233,15.1863775784982));
#48145=CARTESIAN_POINT('Ctrl Pts',(-22.5994530946534,20.4709491297104,15.1859458123878));
#48146=CARTESIAN_POINT('Ctrl Pts',(-22.6026865597278,20.4699525885753,15.1857380020118));
#48147=CARTESIAN_POINT('Ctrl Pts',(-22.6100998746796,20.4676806117007,15.185261403286));
#48148=CARTESIAN_POINT('Ctrl Pts',(-22.6142807547415,20.4664085841392,15.1849925034942));
#48149=CARTESIAN_POINT('Ctrl Pts',(-22.6274548874138,20.4624296293219,15.1841448255665));
#48150=CARTESIAN_POINT('Ctrl Pts',(-22.6364573317819,20.4597535269498,15.1835650388066));
#48151=CARTESIAN_POINT('Ctrl Pts',(-22.6709944866181,20.4496509728991,15.1813386074721));
#48152=CARTESIAN_POINT('Ctrl Pts',(-22.696608492334,20.4425014924525,15.1796829506453));
#48153=CARTESIAN_POINT('Ctrl Pts',(-22.7282753936962,20.4340835246519,15.1776300585123));
#48154=CARTESIAN_POINT('Ctrl Pts',(-22.7342478640688,20.4325142364873,15.1772426167023));
#48155=CARTESIAN_POINT('Ctrl Pts',(-22.7464339164629,20.4293497216696,15.1764515533295));
#48156=CARTESIAN_POINT('Ctrl Pts',(-22.7526478224724,20.4277558635325,15.1760478898224));
#48157=CARTESIAN_POINT('Ctrl Pts',(-22.7613901763673,20.4255412610371,15.1754795693248));
#48158=CARTESIAN_POINT('Ctrl Pts',(-22.7639147105546,20.4249050035615,15.1753154076237));
#48159=CARTESIAN_POINT('Ctrl Pts',(-22.7687362413967,20.4236960465668,15.1750017891014));
#48160=CARTESIAN_POINT('Ctrl Pts',(-22.7710331045438,20.4231228172442,15.1748523492251));
#48161=CARTESIAN_POINT('Ctrl Pts',(-22.7800332404975,20.4208871801433,15.174266621919));
#48162=CARTESIAN_POINT('Ctrl Pts',(-22.7867411811505,20.4192438002433,15.1738297333345));
#48163=CARTESIAN_POINT('Ctrl Pts',(-22.796355025571,20.4169212344985,15.1732030956015));
#48164=CARTESIAN_POINT('Ctrl Pts',(-22.7992567043272,20.4162244949806,15.1730138984676));
#48165=CARTESIAN_POINT('Ctrl Pts',(-22.8152918662345,20.4123977440666,15.1719680114225));
#48166=CARTESIAN_POINT('Ctrl Pts',(-22.8284437973141,20.4093462946019,15.1711088770574));
#48167=CARTESIAN_POINT('Ctrl Pts',(-22.8482596462374,20.4048797469945,15.1698124439125));
#48168=CARTESIAN_POINT('Ctrl Pts',(-22.8549096267377,20.4034029627802,15.1693770398057));
#48169=CARTESIAN_POINT('Ctrl Pts',(-22.9014346059578,20.3932256744313,15.1663284886484));
#48170=CARTESIAN_POINT('Ctrl Pts',(-22.9414656349688,20.3852625534951,15.1636933154414));
#48171=CARTESIAN_POINT('Ctrl Pts',(-23.2280657283857,20.3338893385865,15.1447425769996));
#48172=CARTESIAN_POINT('Ctrl Pts',(-23.4787839086086,20.3185875864077,15.1276255812372));
#48173=CARTESIAN_POINT('Ctrl Pts',(-23.8095791909902,20.33693192408,15.1053478194706));
#48174=CARTESIAN_POINT('Ctrl Pts',(-23.8902688800614,20.3444655574046,15.099947095778));
#48175=CARTESIAN_POINT('Ctrl Pts',(-24.0288655956852,20.3626983723381,15.0908130985448));
#48176=CARTESIAN_POINT('Ctrl Pts',(-24.0869218621184,20.3719575365073,15.0870309107458));
#48177=CARTESIAN_POINT('Ctrl Pts',(-24.1512493766936,20.3840300495933,15.0829129643838));
#48178=CARTESIAN_POINT('Ctrl Pts',(-24.15779839923,20.3852801724858,15.0824945734581));
#48179=CARTESIAN_POINT('Ctrl Pts',(-24.1678442907904,20.3872301324019,15.0818541316317));
#48180=CARTESIAN_POINT('Ctrl Pts',(-24.1713439083479,20.3879154558174,15.0816312771457));
#48181=CARTESIAN_POINT('Ctrl Pts',(-24.1771085166777,20.389054266434,15.0812646119984));
#48182=CARTESIAN_POINT('Ctrl Pts',(-24.1793741589154,20.3895043803166,15.081120610776));
#48183=CARTESIAN_POINT('Ctrl Pts',(-24.1836712371576,20.3903628817954,15.0808477012696));
#48184=CARTESIAN_POINT('Ctrl Pts',(-24.1857027653732,20.3907707930948,15.080718765799));
#48185=CARTESIAN_POINT('Ctrl Pts',(-24.1895245948165,20.3915420148926,15.0804763720654));
#48186=CARTESIAN_POINT('Ctrl Pts',(-24.1913149733679,20.3919048868709,15.0803628892832));
#48187=CARTESIAN_POINT('Ctrl Pts',(-24.1952621540202,20.3927083917828,15.0801128506953));
#48188=CARTESIAN_POINT('Ctrl Pts',(-24.1974188080795,20.3931497112017,15.0799763352771));
#48189=CARTESIAN_POINT('Ctrl Pts',(-24.2033660651773,20.3943730575938,15.0796001484074));
#48190=CARTESIAN_POINT('Ctrl Pts',(-24.2071557300403,20.395159707221,15.0793607428334));
#48191=CARTESIAN_POINT('Ctrl Pts',(-24.2266051021672,20.3992335228834,15.0781335872822));
#48192=CARTESIAN_POINT('Ctrl Pts',(-24.2422419464662,20.402630529567,15.0771520616261));
#48193=CARTESIAN_POINT('Ctrl Pts',(-24.5721978193018,20.4768890979609,15.0565357612891));
#48194=CARTESIAN_POINT('Ctrl Pts',(-24.8742152495325,20.5943871070597,15.0393528562809));
#48195=CARTESIAN_POINT('Ctrl Pts',(-25.2067127340257,20.7851167331773,15.0176191495377));
#48196=CARTESIAN_POINT('Ctrl Pts',(-25.258736136087,20.8169542181277,15.0141329978844));
#48197=CARTESIAN_POINT('Ctrl Pts',(-25.3754724415382,20.8930302925773,15.0060696039607));
#48198=CARTESIAN_POINT('Ctrl Pts',(-25.4395350599354,20.9381905379804,15.0014669953377));
#48199=CARTESIAN_POINT('Ctrl Pts',(-25.5335331491884,21.0097216449567,14.9943957490371));
#48200=CARTESIAN_POINT('Ctrl Pts',(-25.5647316292989,21.0343882779344,14.9919931208424));
#48201=CARTESIAN_POINT('Ctrl Pts',(-25.6012263442089,21.0643564024758,14.9891124669186));
#48202=CARTESIAN_POINT('Ctrl Pts',(-25.6069715717371,21.0691076480295,14.9886568704943));
#48203=CARTESIAN_POINT('Ctrl Pts',(-25.6157910922121,21.0764529849152,14.9879542094789));
#48204=CARTESIAN_POINT('Ctrl Pts',(-25.6188771277236,21.079032990031,14.9877077208925));
#48205=CARTESIAN_POINT('Ctrl Pts',(-25.6242685097912,21.0835574997075,14.9872760075908));
#48206=CARTESIAN_POINT('Ctrl Pts',(-25.6265759769405,21.0854994793879,14.987090886624));
#48207=CARTESIAN_POINT('Ctrl Pts',(-25.6317826722372,21.0898939690308,14.9866723731695));
#48208=CARTESIAN_POINT('Ctrl Pts',(-25.6346802946091,21.0923483667901,14.9864389031429));
#48209=CARTESIAN_POINT('Ctrl Pts',(-25.6424738086489,21.0989734665222,14.985809442644));
#48210=CARTESIAN_POINT('Ctrl Pts',(-25.6473615455672,21.103153696325,14.9854130590041));
#48211=CARTESIAN_POINT('Ctrl Pts',(-25.668846112426,21.1216399811268,14.983663544704));
#48212=CARTESIAN_POINT('Ctrl Pts',(-25.6853089910335,21.1361001839078,14.9823040190447));
#48213=CARTESIAN_POINT('Ctrl Pts',(-25.7111635530089,21.1592809053668,14.9801382370392));
#48214=CARTESIAN_POINT('Ctrl Pts',(-25.7206530754617,21.1678916791159,14.9793366398407));
#48215=CARTESIAN_POINT('Ctrl Pts',(-25.7397729568686,21.1854500729292,14.977707862806));
#48216=CARTESIAN_POINT('Ctrl Pts',(-25.7494004213254,21.1944004751071,14.9768805733507));
#48217=CARTESIAN_POINT('Ctrl Pts',(-25.7639915476151,21.2081328441055,14.9756157463722));
#48218=CARTESIAN_POINT('Ctrl Pts',(-25.7689951542247,21.212872323986,14.9751800136716));
#48219=CARTESIAN_POINT('Ctrl Pts',(-25.7781859878633,21.221634102467,14.9743759447204));
#48220=CARTESIAN_POINT('Ctrl Pts',(-25.7823776306145,21.2256517452964,14.9740078063447));
#48221=CARTESIAN_POINT('Ctrl Pts',(-25.7894741752755,21.2324905959042,14.9733821057411));
#48222=CARTESIAN_POINT('Ctrl Pts',(-25.7923846697175,21.2353060019694,14.9731247888244));
#48223=CARTESIAN_POINT('Ctrl Pts',(-25.8006006557055,21.2432835939391,14.9723964303817));
#48224=CARTESIAN_POINT('Ctrl Pts',(-25.8058936536369,21.2484585603392,14.9719248514698));
#48225=CARTESIAN_POINT('Ctrl Pts',(-25.821346241917,21.2636710459271,14.9705411987586));
#48226=CARTESIAN_POINT('Ctrl Pts',(-25.8314568986725,21.2737578232613,14.9696270653708));
#48227=CARTESIAN_POINT('Ctrl Pts',(-26.021187952798,21.4655739584263,14.9523053259293));
#48228=CARTESIAN_POINT('Ctrl Pts',(-26.1786091851035,21.6679383275251,14.9349653653267));
#48229=CARTESIAN_POINT('Ctrl Pts',(-26.4003916535136,22.035928612022,14.9059419247136));
#48230=CARTESIAN_POINT('Ctrl Pts',(-26.4780870094096,22.1922125929812,14.8942909339694));
#48231=CARTESIAN_POINT('Ctrl Pts',(-26.5449144499306,22.3593911336872,14.8830143385004));
#48232=CARTESIAN_POINT('Ctrl Pts',(-26.5470423699649,22.3647562051429,14.8826536831015));
#48233=CARTESIAN_POINT('Ctrl Pts',(-26.5500935487412,22.3725097789139,14.8821342722929));
#48234=CARTESIAN_POINT('Ctrl Pts',(-26.5510283760272,22.3748936709793,14.8819748217399));
#48235=CARTESIAN_POINT('Ctrl Pts',(-26.5526507982834,22.3790455432546,14.8816975482373));
#48236=CARTESIAN_POINT('Ctrl Pts',(-26.5533396742809,22.3808130184685,14.8815796473175));
#48237=CARTESIAN_POINT('Ctrl Pts',(-26.554671169337,22.3842382207799,14.8813514307984));
#48238=CARTESIAN_POINT('Ctrl Pts',(-26.555313975532,22.3858958671492,14.8812411038011));
#48239=CARTESIAN_POINT('Ctrl Pts',(-26.5568465695567,22.3898577905069,14.8809776963718));
#48240=CARTESIAN_POINT('Ctrl Pts',(-26.5577350821936,22.3921625643677,14.8808246934279));
#48241=CARTESIAN_POINT('Ctrl Pts',(-26.5609044796981,22.4004121282887,14.8802778566236));
#48242=CARTESIAN_POINT('Ctrl Pts',(-26.5631704147708,22.4063627044817,14.8798849204014));
#48243=CARTESIAN_POINT('Ctrl Pts',(-26.59619239229,22.4938606438487,14.8741287226286));
#48244=CARTESIAN_POINT('Ctrl Pts',(-26.6236489896969,22.5766248486479,14.8689586974522));
#48245=CARTESIAN_POINT('Ctrl Pts',(-26.7306457119797,22.9490708094409,14.8464773058849));
#48246=CARTESIAN_POINT('Ctrl Pts',(-26.7728204513682,23.2479183136171,14.8303697289785));
#48247=CARTESIAN_POINT('Ctrl Pts',(-26.7730746935473,23.6687138283204,14.8060891589639));
#48248=CARTESIAN_POINT('Ctrl Pts',(-26.7663994938228,23.7890186458402,14.7989850392452));
#48249=CARTESIAN_POINT('Ctrl Pts',(-26.7518235465049,23.9192710030495,14.7910102352784));
#48250=CARTESIAN_POINT('Ctrl Pts',(-26.7505832380056,23.9298772951235,14.7903588398648));
#48251=CARTESIAN_POINT('Ctrl Pts',(-26.7487690530033,23.9447498744277,14.7894425339449));
#48252=CARTESIAN_POINT('Ctrl Pts',(-26.7482392976755,23.9490215561017,14.7891790187043));
#48253=CARTESIAN_POINT('Ctrl Pts',(-26.7473057811145,23.9564274561047,14.7887215711402));
#48254=CARTESIAN_POINT('Ctrl Pts',(-26.7469059639392,23.9595621734787,14.7885277637925));
#48255=CARTESIAN_POINT('Ctrl Pts',(-26.7460650919268,23.9660785439754,14.7881245011069));
#48256=CARTESIAN_POINT('Ctrl Pts',(-26.7456232790022,23.9694600933374,14.7879150220258));
#48257=CARTESIAN_POINT('Ctrl Pts',(-26.7445714125592,23.9774125902452,14.7874218784325));
#48258=CARTESIAN_POINT('Ctrl Pts',(-26.743956915046,23.9819829333084,14.7871380734877));
#48259=CARTESIAN_POINT('Ctrl Pts',(-26.7419206902413,23.9968851518233,14.7862113986722));
#48260=CARTESIAN_POINT('Ctrl Pts',(-26.7404586300804,24.007211367217,14.7855672518012));
#48261=CARTESIAN_POINT('Ctrl Pts',(-26.7148741631729,24.1817992818398,14.7746416895627));
#48262=CARTESIAN_POINT('Ctrl Pts',(-26.6781486131203,24.3439348442341,14.7639534537309));
#48263=CARTESIAN_POINT('Ctrl Pts',(-26.5363159612377,24.8025153798054,14.7321443059383));
#48264=CARTESIAN_POINT('Ctrl Pts',(-26.4001845830794,25.0873305771487,14.7102438007793));
#48265=CARTESIAN_POINT('Ctrl Pts',(-26.22258375519,25.3515805210341,14.6898606971357));
#48266=CARTESIAN_POINT('Ctrl Pts',(-26.2201365424214,25.3552057341273,14.6895810883095));
#48267=CARTESIAN_POINT('Ctrl Pts',(-26.2148344300244,25.3630257154467,14.6889780136434));
#48268=CARTESIAN_POINT('Ctrl Pts',(-26.2119769821574,25.3672187557089,14.688654692631));
#48269=CARTESIAN_POINT('Ctrl Pts',(-26.2044127535385,25.3782624231628,14.6878032824879));
#48270=CARTESIAN_POINT('Ctrl Pts',(-26.1996893164462,25.385101673575,14.6872761699066));
#48271=CARTESIAN_POINT('Ctrl Pts',(-26.1929507757418,25.3947783957977,14.686530681577));
#48272=CARTESIAN_POINT('Ctrl Pts',(-26.1909575010093,25.3976309276183,14.6863109631802));
#48273=CARTESIAN_POINT('Ctrl Pts',(-26.1820148240199,25.4103845497096,14.6853288000661));
#48274=CARTESIAN_POINT('Ctrl Pts',(-26.1750142084187,25.420249868379,14.6845695912735));
#48275=CARTESIAN_POINT('Ctrl Pts',(-26.1658764468832,25.4329744529136,14.6835912724674));
#48276=CARTESIAN_POINT('Ctrl Pts',(-26.1637899875912,25.4358697423885,14.6833687334791));
#48277=CARTESIAN_POINT('Ctrl Pts',(-26.1605853363612,25.4403011610429,14.6830282279546));
#48278=CARTESIAN_POINT('Ctrl Pts',(-26.1594705967788,25.4418397650258,14.682910022527));
#48279=CARTESIAN_POINT('Ctrl Pts',(-26.1572700682458,25.4448713679166,14.6826771548605));
#48280=CARTESIAN_POINT('Ctrl Pts',(-26.1561843627513,25.4463644119311,14.6825624882517));
#48281=CARTESIAN_POINT('Ctrl Pts',(-26.1537636492315,25.4496873302519,14.6823073284527));
#48282=CARTESIAN_POINT('Ctrl Pts',(-26.1524279978497,25.4515167259942,14.6821668813201));
#48283=CARTESIAN_POINT('Ctrl Pts',(-26.1485667810561,25.4567936111478,14.6817618388978));
#48284=CARTESIAN_POINT('Ctrl Pts',(-26.1460362731586,25.4602375039206,14.6814975878347));
#48285=CARTESIAN_POINT('Ctrl Pts',(-26.1289663780756,25.4833721813923,14.6797230191025));
#48286=CARTESIAN_POINT('Ctrl Pts',(-26.114209409169,25.5029025000609,14.6782276751155));
#48287=CARTESIAN_POINT('Ctrl Pts',(-26.0678641562336,25.5628073616852,14.6736430843277));
#48288=CARTESIAN_POINT('Ctrl Pts',(-26.0355326940446,25.6025995750588,14.6706006282148));
#48289=CARTESIAN_POINT('Ctrl Pts',(-25.9738659284887,25.674900894138,14.6650423979662));
#48290=CARTESIAN_POINT('Ctrl Pts',(-25.9447918384842,25.7076153544093,14.6625153370804));
#48291=CARTESIAN_POINT('Ctrl Pts',(-25.7266577909439,25.9432173336073,14.6441403618332));
#48292=CARTESIAN_POINT('Ctrl Pts',(-25.5127817460327,26.1215386636725,14.6291461523431));
#48293=CARTESIAN_POINT('Ctrl Pts',(-25.2394437272199,26.2952324533477,14.6104162374911));
#48294=CARTESIAN_POINT('Ctrl Pts',(-25.199646256108,26.3193285011329,14.6077019971461));
#48295=CARTESIAN_POINT('Ctrl Pts',(-25.0987396996147,26.3774768511741,14.600835127832));
#48296=CARTESIAN_POINT('Ctrl Pts',(-25.0370200002191,26.4104153292194,14.5966480978013));
#48297=CARTESIAN_POINT('Ctrl Pts',(-24.9657798505873,26.4455055041975,14.5918112549094));
#48298=CARTESIAN_POINT('Ctrl Pts',(-24.9572603716994,26.4496552806181,14.5912327740642));
#48299=CARTESIAN_POINT('Ctrl Pts',(-24.9447710975515,26.4556707064909,14.590384620798));
#48300=CARTESIAN_POINT('Ctrl Pts',(-24.9408155442015,26.4575659494228,14.5901159796346));
#48301=CARTESIAN_POINT('Ctrl Pts',(-24.933799537708,26.4609099677348,14.5896394521692));
#48302=CARTESIAN_POINT('Ctrl Pts',(-24.9307406410762,26.4623620089536,14.589431679746));
#48303=CARTESIAN_POINT('Ctrl Pts',(-24.9244505869723,26.4653357248933,14.5890044070043));
#48304=CARTESIAN_POINT('Ctrl Pts',(-24.9212191780416,26.4668568539912,14.5887848881121));
#48305=CARTESIAN_POINT('Ctrl Pts',(-24.9129531422857,26.4707311728466,14.5882233112979));
#48306=CARTESIAN_POINT('Ctrl Pts',(-24.9079149600735,26.473076710033,14.5878809888923));
#48307=CARTESIAN_POINT('Ctrl Pts',(-24.8969792678059,26.4781334705525,14.5871378609764));
#48308=CARTESIAN_POINT('Ctrl Pts',(-24.8910795924051,26.4808399277914,14.5867368922793));
#48309=CARTESIAN_POINT('Ctrl Pts',(-24.8741073791122,26.4885638974564,14.5855831897731));
#48310=CARTESIAN_POINT('Ctrl Pts',(-24.8630146653146,26.4935365671223,14.5848289150427));
#48311=CARTESIAN_POINT('Ctrl Pts',(-24.7558195960524,26.5408637036697,14.5775372361526));
#48312=CARTESIAN_POINT('Ctrl Pts',(-24.6577391949683,26.578555078469,14.5708414810364));
#48313=CARTESIAN_POINT('Ctrl Pts',(-24.4138606428955,26.6588418025909,14.5541183607413));
#48314=CARTESIAN_POINT('Ctrl Pts',(-24.266560986747,26.6960497299008,14.5439486847148));
#48315=CARTESIAN_POINT('Ctrl Pts',(-24.0204731939521,26.7400276904012,14.5270472441828));
#48316=CARTESIAN_POINT('Ctrl Pts',(-23.9230026808738,26.7528812531071,14.520378739078));
#48317=CARTESIAN_POINT('Ctrl Pts',(-23.6862757574035,26.773143725189,14.5044083485026));
#48318=CARTESIAN_POINT('Ctrl Pts',(-23.546810865969,26.7760126658359,14.4951842719377));
#48319=CARTESIAN_POINT('Ctrl Pts',(-23.3987828236384,26.769453064222,14.4858712199841));
#48320=CARTESIAN_POINT('Ctrl Pts',(-23.3899851006605,26.7690270649527,14.4853195366102));
#48321=CARTESIAN_POINT('Ctrl Pts',(-23.3780509692405,26.7684001447648,14.4845737445212));
#48322=CARTESIAN_POINT('Ctrl Pts',(-23.3749130521061,26.7682307020245,14.4843778895986));
#48323=CARTESIAN_POINT('Ctrl Pts',(-23.3699639664627,26.7679561984464,14.4840693749785));
#48324=CARTESIAN_POINT('Ctrl Pts',(-23.3681526407713,26.7678541980832,14.4839565425485));
#48325=CARTESIAN_POINT('Ctrl Pts',(-23.3646523099774,26.7676541203267,14.4837386560546));
#48326=CARTESIAN_POINT('Ctrl Pts',(-23.3629633073733,26.7675562430807,14.4836335916236));
#48327=CARTESIAN_POINT('Ctrl Pts',(-23.3589305565579,26.7673193598391,14.4833829042141));
#48328=CARTESIAN_POINT('Ctrl Pts',(-23.3565868843069,26.7671791227166,14.4832373516964));
#48329=CARTESIAN_POINT('Ctrl Pts',(-23.3495821336134,26.7667523003123,14.4828027290414));
#48330=CARTESIAN_POINT('Ctrl Pts',(-23.3449214968207,26.7664581434292,14.482514085542));
#48331=CARTESIAN_POINT('Ctrl Pts',(-23.3054715549848,26.7638821518488,14.480075263434));
#48332=CARTESIAN_POINT('Ctrl Pts',(-23.2707190373552,26.7610459430922,14.4779558080514));
#48333=CARTESIAN_POINT('Ctrl Pts',(-23.1436171339345,26.7485935121687,14.4702881311803));
#48334=CARTESIAN_POINT('Ctrl Pts',(-23.0516424465499,26.7355513264308,14.4649017173756));
#48335=CARTESIAN_POINT('Ctrl Pts',(-22.7437021425551,26.6782164514784,14.4470392497461));
#48336=CARTESIAN_POINT('Ctrl Pts',(-22.5317583046197,26.6157635702548,14.4349958628012));
#48337=CARTESIAN_POINT('Ctrl Pts',(-22.2418952315318,26.4969365178865,14.4171747671787));
#48338=CARTESIAN_POINT('Ctrl Pts',(-22.1575504760193,26.4580200681639,14.4118201147606));
#48339=CARTESIAN_POINT('Ctrl Pts',(-22.0750358569346,26.4155366929967,14.4063516850465));
#48340=CARTESIAN_POINT('',(-26.773001504593,23.5528255026527,14.5642265507266));
#48341=CARTESIAN_POINT('Ctrl Pts',(-22.0750361586249,26.4155368483246,14.1564144975666));
#48342=CARTESIAN_POINT('Ctrl Pts',(-22.1641783660915,26.4614324836105,14.1620444840364));
#48343=CARTESIAN_POINT('Ctrl Pts',(-22.2554435166684,26.5031584476492,14.1677232490408));
#48344=CARTESIAN_POINT('Ctrl Pts',(-22.4570048561852,26.584159622923,14.180274845889));
#48345=CARTESIAN_POINT('Ctrl Pts',(-22.5677517397116,26.6218107828571,14.1871789315501));
#48346=CARTESIAN_POINT('Ctrl Pts',(-22.6905015721636,26.6562239284404,14.1949361318805));
#48347=CARTESIAN_POINT('Ctrl Pts',(-22.7007269020646,26.6590362536987,14.1955830634446));
#48348=CARTESIAN_POINT('Ctrl Pts',(-22.7151095437004,26.6629157276887,14.1964941156984));
#48349=CARTESIAN_POINT('Ctrl Pts',(-22.7192554682639,26.6640251409857,14.1967568624061));
#48350=CARTESIAN_POINT('Ctrl Pts',(-22.7264549100795,26.6659362460338,14.197213351087));
#48351=CARTESIAN_POINT('Ctrl Pts',(-22.7295074197282,26.6667417407651,14.1974069693806));
#48352=CARTESIAN_POINT('Ctrl Pts',(-22.7356519942143,26.668353514313,14.1977968587649));
#48353=CARTESIAN_POINT('Ctrl Pts',(-22.73874408382,26.6691596820251,14.1979931331792));
#48354=CARTESIAN_POINT('Ctrl Pts',(-22.7450506789853,26.6707939202462,14.1983936038051));
#48355=CARTESIAN_POINT('Ctrl Pts',(-22.748265274243,26.6716216255416,14.1985978115815));
#48356=CARTESIAN_POINT('Ctrl Pts',(-22.7588562884303,26.6743311961511,14.1992708749277));
#48357=CARTESIAN_POINT('Ctrl Pts',(-22.7662380549854,26.6761918807994,14.1997404158028));
#48358=CARTESIAN_POINT('Ctrl Pts',(-22.815689199483,26.6884705998276,14.2028888506412));
#48359=CARTESIAN_POINT('Ctrl Pts',(-22.8579567457468,26.69806481661,14.2055942225938));
#48360=CARTESIAN_POINT('Ctrl Pts',(-22.9788744967297,26.7229585406235,14.2133789343628));
#48361=CARTESIAN_POINT('Ctrl Pts',(-23.0579147690575,26.7361806566581,14.2185224199575));
#48362=CARTESIAN_POINT('Ctrl Pts',(-23.238766482207,26.7595435463649,14.2304158806061));
#48363=CARTESIAN_POINT('Ctrl Pts',(-23.3407311575276,26.7678091130739,14.2372112876052));
#48364=CARTESIAN_POINT('Ctrl Pts',(-23.696661026257,26.779670976963,14.2611378849326));
#48365=CARTESIAN_POINT('Ctrl Pts',(-23.9505269205996,26.7581130096931,14.2786384522413));
#48366=CARTESIAN_POINT('Ctrl Pts',(-24.2336370473986,26.6999091137219,14.2971958614323));
#48367=CARTESIAN_POINT('Ctrl Pts',(-24.2679215223982,26.6922745642199,14.2994251894649));
#48368=CARTESIAN_POINT('Ctrl Pts',(-24.3065681413952,26.6830030167128,14.301912505102));
#48369=CARTESIAN_POINT('Ctrl Pts',(-24.3110579527206,26.6819156704801,14.3022010775983));
#48370=CARTESIAN_POINT('Ctrl Pts',(-24.3178488723063,26.6802555737431,14.3026369357577));
#48371=CARTESIAN_POINT('Ctrl Pts',(-24.3201516878883,26.6796899371613,14.3027846294433));
#48372=CARTESIAN_POINT('Ctrl Pts',(-24.3241551349439,26.6787018909967,14.3030412068006));
#48373=CARTESIAN_POINT('Ctrl Pts',(-24.3258560459269,26.6782806360725,14.3031501575395));
#48374=CARTESIAN_POINT('Ctrl Pts',(-24.329415931752,26.6773958973065,14.3033780586469));
#48375=CARTESIAN_POINT('Ctrl Pts',(-24.3312748358626,26.6769321432784,14.3034969926689));
#48376=CARTESIAN_POINT('Ctrl Pts',(-24.3357203219702,26.6758188844018,14.3037812491499));
#48377=CARTESIAN_POINT('Ctrl Pts',(-24.3383065211397,26.6751678240791,14.3039464809324));
#48378=CARTESIAN_POINT('Ctrl Pts',(-24.3470718451704,26.6729496321965,14.3045060410579));
#48379=CARTESIAN_POINT('Ctrl Pts',(-24.3532471785621,26.6713673643394,14.3048994948597));
#48380=CARTESIAN_POINT('Ctrl Pts',(-24.3679138507566,26.6675630020536,14.3058322288875));
#48381=CARTESIAN_POINT('Ctrl Pts',(-24.3764009378211,26.6653245078243,14.306370584403));
#48382=CARTESIAN_POINT('Ctrl Pts',(-24.4761887867704,26.6385686608135,14.3126851866119));
#48383=CARTESIAN_POINT('Ctrl Pts',(-24.5663871581839,26.6100774708763,14.3182436659957));
#48384=CARTESIAN_POINT('Ctrl Pts',(-24.7713446553043,26.5352710073156,14.330801792821));
#48385=CARTESIAN_POINT('Ctrl Pts',(-24.8849493767254,26.486234272644,14.337710505534));
#48386=CARTESIAN_POINT('Ctrl Pts',(-25.0496056072956,26.4036237934179,14.3480044251567));
#48387=CARTESIAN_POINT('Ctrl Pts',(-25.1029736045383,26.3749373604643,14.3513867446968));
#48388=CARTESIAN_POINT('Ctrl Pts',(-25.225170614364,26.3047438565162,14.3592958519203));
#48389=CARTESIAN_POINT('Ctrl Pts',(-25.2933169115535,26.2621335740474,14.3638334831546));
#48390=CARTESIAN_POINT('Ctrl Pts',(-25.4035077904985,26.1873632202491,14.3714638067219));
#48391=CARTESIAN_POINT('Ctrl Pts',(-25.4464805492464,26.1566344622288,14.3745176501839));
#48392=CARTESIAN_POINT('Ctrl Pts',(-25.5067964734806,26.1112226155249,14.3789327435448));
#48393=CARTESIAN_POINT('Ctrl Pts',(-25.5247707707015,26.0973900732245,14.3802653389994));
#48394=CARTESIAN_POINT('Ctrl Pts',(-25.5465191581981,26.0802845501943,14.3818993738021));
#48395=CARTESIAN_POINT('Ctrl Pts',(-25.5504338636023,26.0771908170175,14.3821943647709));
#48396=CARTESIAN_POINT('Ctrl Pts',(-25.6028032791899,26.0356061095346,14.3861523487597));
#48397=CARTESIAN_POINT('Ctrl Pts',(-25.6501440365499,25.9957385478484,14.3898652816964));
#48398=CARTESIAN_POINT('Ctrl Pts',(-25.7031301873842,25.9484433175447,14.3941921800626));
#48399=CARTESIAN_POINT('Ctrl Pts',(-25.7099287763556,25.9423227148695,14.3947506942733));
#48400=CARTESIAN_POINT('Ctrl Pts',(-25.7199020269315,25.9332668671974,14.3955749814105));
#48401=CARTESIAN_POINT('Ctrl Pts',(-25.7230970300878,25.9303540087134,14.3958398045199));
#48402=CARTESIAN_POINT('Ctrl Pts',(-25.728776917582,25.9251547328287,14.3963119463658));
#48403=CARTESIAN_POINT('Ctrl Pts',(-25.7312640929222,25.9228708184216,14.3965191582762));
#48404=CARTESIAN_POINT('Ctrl Pts',(-25.736052291107,25.9184600379189,14.3969189733547));
#48405=CARTESIAN_POINT('Ctrl Pts',(-25.7383538116413,25.9163337157137,14.3971115531361));
#48406=CARTESIAN_POINT('Ctrl Pts',(-25.7432952411801,25.9117550660842,14.3975258960409));
#48407=CARTESIAN_POINT('Ctrl Pts',(-25.7459341437246,25.9093016630144,14.3977477051942));
#48408=CARTESIAN_POINT('Ctrl Pts',(-25.7560329905152,25.8998810815878,14.398598608407));
#48409=CARTESIAN_POINT('Ctrl Pts',(-25.763463871326,25.8928829586436,14.3992290341238));
#48410=CARTESIAN_POINT('Ctrl Pts',(-25.8517051950243,25.8089860180301,14.4067673991941));
#48411=CARTESIAN_POINT('Ctrl Pts',(-25.9284946006083,25.7279855359648,14.4138554609292));
#48412=CARTESIAN_POINT('Ctrl Pts',(-26.0447763978912,25.5918273828638,14.425499015566));
#48413=CARTESIAN_POINT('Ctrl Pts',(-26.0870016270923,25.5391166091991,14.4299464752438));
#48414=CARTESIAN_POINT('Ctrl Pts',(-26.3180134503841,25.2314039962296,14.4555402933867));
#48415=CARTESIAN_POINT('Ctrl Pts',(-26.4699719113487,24.9509684018659,14.4776782685235));
#48416=CARTESIAN_POINT('Ctrl Pts',(-26.5841299806454,24.6374390849412,14.498798408725));
#48417=CARTESIAN_POINT('Ctrl Pts',(-26.5896279345108,24.6219727212992,14.4998310489897));
#48418=CARTESIAN_POINT('Ctrl Pts',(-26.5961883188077,24.6030610242234,14.5010819317832));
#48419=CARTESIAN_POINT('Ctrl Pts',(-26.5973633176643,24.599655409286,14.5013067259906));
#48420=CARTESIAN_POINT('Ctrl Pts',(-26.5992889638398,24.5940436163952,14.5016763702168));
#48421=CARTESIAN_POINT('Ctrl Pts',(-26.6000429289758,24.5918385942801,14.5018214169399));
#48422=CARTESIAN_POINT('Ctrl Pts',(-26.6013967674909,24.5878651289874,14.5020824361927));
#48423=CARTESIAN_POINT('Ctrl Pts',(-26.601997494122,24.5860969862593,14.5021984595274));
#48424=CARTESIAN_POINT('Ctrl Pts',(-26.603284553985,24.582297893637,14.5024474781995));
#48425=CARTESIAN_POINT('Ctrl Pts',(-26.6039703957749,24.5802667864014,14.5025804437681));
#48426=CARTESIAN_POINT('Ctrl Pts',(-26.6058397103479,24.5747125694664,14.5029435952363));
#48427=CARTESIAN_POINT('Ctrl Pts',(-26.6070191208747,24.5711880805637,14.5031735391021));
#48428=CARTESIAN_POINT('Ctrl Pts',(-26.6130654722392,24.5530150753995,14.5043566519487));
#48429=CARTESIAN_POINT('Ctrl Pts',(-26.617833330556,24.5383334457727,14.5053040162349));
#48430=CARTESIAN_POINT('Ctrl Pts',(-26.6621301977274,24.3985187724267,14.5142507940164));
#48431=CARTESIAN_POINT('Ctrl Pts',(-26.694092175547,24.2710988209974,14.5218366642828));
#48432=CARTESIAN_POINT('Ctrl Pts',(-26.7545046808052,23.9477161584249,14.5404829065207));
#48433=CARTESIAN_POINT('Ctrl Pts',(-26.7728495125508,23.75044052546,14.55133804464));
#48434=CARTESIAN_POINT('Ctrl Pts',(-26.7730015784458,23.5527312736527,14.5625675171146));
#48435=CARTESIAN_POINT('Ctrl Pts',(-26.773001504593,23.5528255026527,14.5642265507266));
#48436=CARTESIAN_POINT('Ctrl Pts',(-26.7730811417884,23.4530767321105,14.5703666451467));
#48437=CARTESIAN_POINT('Ctrl Pts',(-26.7685254240945,23.353267963731,14.5765067395667));
#48438=CARTESIAN_POINT('Ctrl Pts',(-26.7593443695323,23.25386235166,14.5826468339868));
#48439=CARTESIAN_POINT('Ctrl Pts',(-26.7501651566195,23.1544766795947,14.5887856967508));
#48440=CARTESIAN_POINT('Ctrl Pts',(-26.7363624905339,23.0554944367485,14.5949245595149));
#48441=CARTESIAN_POINT('Ctrl Pts',(-26.7179983712085,22.9573749231272,14.6010634222789));
#48442=CARTESIAN_POINT('Ctrl Pts',(-26.6996329917632,22.8592486766843,14.607202706283));
#48443=CARTESIAN_POINT('Ctrl Pts',(-26.676705617717,22.7619857052364,14.6133419902871));
#48444=CARTESIAN_POINT('Ctrl Pts',(-26.6493294175796,22.6660353536938,14.6194812742912));
#48445=CARTESIAN_POINT('Ctrl Pts',(-26.6219439689296,22.5700525872058,14.6256226323321));
#48446=CARTESIAN_POINT('Ctrl Pts',(-26.5901068274062,22.4753837404078,14.6317639903729));
#48447=CARTESIAN_POINT('Ctrl Pts',(-26.5539807836201,22.3824622461197,14.6379053484138));
#48448=CARTESIAN_POINT('Ctrl Pts',(-26.5178109255119,22.2894280549555,14.6440541548052));
#48449=CARTESIAN_POINT('Ctrl Pts',(-26.4773419433713,22.1981458514324,14.6502029611966));
#48450=CARTESIAN_POINT('Ctrl Pts',(-26.4327843892806,22.1090281728591,14.6563517675881));
#48451=CARTESIAN_POINT('Ctrl Pts',(-26.3881946596312,22.0198461413124,14.6625050141083));
#48452=CARTESIAN_POINT('Ctrl Pts',(-26.3395106942905,21.9328321246508,14.6686582606286));
#48453=CARTESIAN_POINT('Ctrl Pts',(-26.2869874634296,21.8483713737048,14.6748115071489));
#48454=CARTESIAN_POINT('Ctrl Pts',(-26.2343808308645,21.7637765074264,14.680974524417));
#48455=CARTESIAN_POINT('Ctrl Pts',(-26.1779230150736,21.6817433535447,14.6871375416852));
#48456=CARTESIAN_POINT('Ctrl Pts',(-26.1179103271923,21.6026255120321,14.6933005589533));
#48457=CARTESIAN_POINT('Ctrl Pts',(-26.1026662866333,21.5825285020907,14.6948660493274));
#48458=CARTESIAN_POINT('Ctrl Pts',(-26.0871930643724,21.562619414593,14.6964315397015));
#48459=CARTESIAN_POINT('Ctrl Pts',(-26.0714958924752,21.5429036636054,14.6979970300756));
#48460=CARTESIAN_POINT('Ctrl Pts',(-26.0096083332172,21.4651724827555,14.7041691213879));
#48461=CARTESIAN_POINT('Ctrl Pts',(-25.9440136725124,21.3901691187462,14.7103412127002));
#48462=CARTESIAN_POINT('Ctrl Pts',(-25.8749813413925,21.3182683194161,14.7165133040125));
#48463=CARTESIAN_POINT('Ctrl Pts',(-25.8060425422565,21.2464649385607,14.7226770327513));
#48464=CARTESIAN_POINT('Ctrl Pts',(-25.7336756285893,21.1777560777395,14.7288407614901));
#48465=CARTESIAN_POINT('Ctrl Pts',(-25.6581911001744,21.1124845866236,14.7350044902289));
#48466=CARTESIAN_POINT('Ctrl Pts',(-25.5827865405327,21.0472822445265,14.7411616890756));
#48467=CARTESIAN_POINT('Ctrl Pts',(-25.5042712592279,20.9855103149272,14.7473188879223));
#48468=CARTESIAN_POINT('Ctrl Pts',(-25.4229928425718,20.9274751315868,14.7534760867689));
#48469=CARTESIAN_POINT('Ctrl Pts',(-25.3417738355096,20.8694823684463,14.7596287850766));
#48470=CARTESIAN_POINT('Ctrl Pts',(-25.2577960610316,20.8152211728802,14.7657814833844));
#48471=CARTESIAN_POINT('Ctrl Pts',(-25.1714397252606,20.7649572787782,14.7719341816921));
#48472=CARTESIAN_POINT('Ctrl Pts',(-25.0851161359348,20.7147124448163,14.7780845468878));
#48473=CARTESIAN_POINT('Ctrl Pts',(-24.9964161525077,20.668462118755,14.7842349120836));
#48474=CARTESIAN_POINT('Ctrl Pts',(-24.905747714114,20.626427917779,14.7903852772793));
#48475=CARTESIAN_POINT('Ctrl Pts',(-24.8150894008456,20.5843984108459,14.7965349556515));
#48476=CARTESIAN_POINT('Ctrl Pts',(-24.7224634637546,20.5465842756483,14.8026846340238));
#48477=CARTESIAN_POINT('Ctrl Pts',(-24.6283002022478,20.51316004339,14.808834312396));
#48478=CARTESIAN_POINT('Ctrl Pts',(-24.5341222648933,20.4797306017863,14.8149849492284));
#48479=CARTESIAN_POINT('Ctrl Pts',(-24.4384069366313,20.4506925674244,14.8211355860609));
#48480=CARTESIAN_POINT('Ctrl Pts',(-24.3416011846338,20.4261710871748,14.8272862228933));
#48481=CARTESIAN_POINT('Ctrl Pts',(-24.2446918708176,20.4016233740925,14.8334434396151));
#48482=CARTESIAN_POINT('Ctrl Pts',(-24.1466902257566,20.381601970555,14.839600656337));
#48483=CARTESIAN_POINT('Ctrl Pts',(-24.0480548466727,20.3661811729301,14.8457578730588));
#48484=CARTESIAN_POINT('Ctrl Pts',(-23.9493644393148,20.3507517721053,14.8519185248666));
#48485=CARTESIAN_POINT('Ctrl Pts',(-23.8500400256912,20.3399281357169,14.8580791766744));
#48486=CARTESIAN_POINT('Ctrl Pts',(-23.7505446914926,20.3337325778896,14.8642398284822));
#48487=CARTESIAN_POINT('Ctrl Pts',(-23.6508828662191,20.3275266526909,14.8704107892512));
#48488=CARTESIAN_POINT('Ctrl Pts',(-23.5510499836273,20.3259642821496,14.8765817500203));
#48489=CARTESIAN_POINT('Ctrl Pts',(-23.4515086410323,20.3290156253868,14.8827527107893));
#48490=CARTESIAN_POINT('Ctrl Pts',(-23.3755268652506,20.3313447729715,14.8874631210097));
#48491=CARTESIAN_POINT('Ctrl Pts',(-23.2997149478882,20.3363610477618,14.8921735312301));
#48492=CARTESIAN_POINT('Ctrl Pts',(-23.2242751687707,20.3440310294643,14.8968839414505));
#48493=CARTESIAN_POINT('Ctrl Pts',(-23.1254257727498,20.3540810729248,14.9030560327628));
#48494=CARTESIAN_POINT('Ctrl Pts',(-23.0268674893177,20.3687244636739,14.9092281240752));
#48495=CARTESIAN_POINT('Ctrl Pts',(-22.9290612390132,20.3879370919575,14.9154002153875));
#48496=CARTESIAN_POINT('Ctrl Pts',(-22.8313875065087,20.407123689029,14.9215639441263));
#48497=CARTESIAN_POINT('Ctrl Pts',(-22.7344642043974,20.430867135638,14.927727672865));
#48498=CARTESIAN_POINT('Ctrl Pts',(-22.6387476161559,20.4590915278884,14.9338914016038));
#48499=CARTESIAN_POINT('Ctrl Pts',(-22.5431324306561,20.4872860190443,14.9400486004505));
#48500=CARTESIAN_POINT('Ctrl Pts',(-22.4487218318153,20.5199518959084,14.9462057992972));
#48501=CARTESIAN_POINT('Ctrl Pts',(-22.3559614285032,20.556962314669,14.9523629981439));
#48502=CARTESIAN_POINT('Ctrl Pts',(-22.2632688274209,20.5939456810578,14.9585156964516));
#48503=CARTESIAN_POINT('Ctrl Pts',(-22.1722244260074,20.6352671152272,14.9646683947593));
#48504=CARTESIAN_POINT('Ctrl Pts',(-22.0832573081701,20.6807503838195,14.970821093067));
#48505=CARTESIAN_POINT('Ctrl Pts',(-21.9943239267905,20.7262164050916,14.9769714582627));
#48506=CARTESIAN_POINT('Ctrl Pts',(-21.9074666501743,20.7758409274524,14.9831218234585));
#48507=CARTESIAN_POINT('Ctrl Pts',(-21.8230924369732,20.8294005383466,14.9892721886542));
#48508=CARTESIAN_POINT('Ctrl Pts',(-21.7387276460088,20.8829541681323,14.9954218670264));
#48509=CARTESIAN_POINT('Ctrl Pts',(-21.6568457339223,20.9404417799785,15.0015715453986));
#48510=CARTESIAN_POINT('Ctrl Pts',(-21.5778261318149,21.0015956972892,15.0077212237708));
#48511=CARTESIAN_POINT('Ctrl Pts',(-21.4987942140804,21.0627591457646,15.0138718606032));
#48512=CARTESIAN_POINT('Ctrl Pts',(-21.4226258359783,21.1275897687843,15.0200224974357));
#48513=CARTESIAN_POINT('Ctrl Pts',(-21.3496678903753,21.1957791725561,15.0261731342681));
#48514=CARTESIAN_POINT('Ctrl Pts',(-21.2766318950963,21.2640415246657,15.0323303509899));
#48515=CARTESIAN_POINT('Ctrl Pts',(-21.206813508636,21.3356695355718,15.0384875677118));
#48516=CARTESIAN_POINT('Ctrl Pts',(-21.1405231290148,21.4103175400735,15.0446447844336));
#48517=CARTESIAN_POINT('Ctrl Pts',(-21.0741957662625,21.4850071903911,15.0508054362414));
#48518=CARTESIAN_POINT('Ctrl Pts',(-21.011400603143,21.5627198517475,15.0569660880492));
#48519=CARTESIAN_POINT('Ctrl Pts',(-20.9524067303515,21.6430779841118,15.063126739857));
#48520=CARTESIAN_POINT('Ctrl Pts',(-20.8933141398322,21.7235705842074,15.069297700626));
#48521=CARTESIAN_POINT('Ctrl Pts',(-20.8380357860247,21.8067171358415,15.075468661395));
#48522=CARTESIAN_POINT('Ctrl Pts',(-20.7867966167566,21.8921123178713,15.0816396221641));
#48523=CARTESIAN_POINT('Ctrl Pts',(-20.7476847967922,21.9572960636871,15.0863500323845));
#48524=CARTESIAN_POINT('Ctrl Pts',(-20.7109255177076,22.0237894109348,15.0910604426049));
#48525=CARTESIAN_POINT('Ctrl Pts',(-20.6766000032702,22.0914041131179,15.0957708528253));
#48526=CARTESIAN_POINT('Ctrl Pts',(-20.6316229843831,22.1800002430518,15.1019429441377));
#48527=CARTESIAN_POINT('Ctrl Pts',(-20.5906677843335,22.2708343540157,15.10811503545));
#48528=CARTESIAN_POINT('Ctrl Pts',(-20.5539632662718,22.3635056334827,15.1142871267623));
#48529=CARTESIAN_POINT('Ctrl Pts',(-20.5173084792034,22.4560513525276,15.1204508555011));
#48530=CARTESIAN_POINT('Ctrl Pts',(-20.4848930855473,22.5504288922454,15.1266145842399));
#48531=CARTESIAN_POINT('Ctrl Pts',(-20.4568998666447,22.6462133444179,15.1327783129787));
#48532=CARTESIAN_POINT('Ctrl Pts',(-20.4289363039302,22.7418963219531,15.1389355118254));
#48533=CARTESIAN_POINT('Ctrl Pts',(-20.4053857231893,22.8389828340522,15.1450927106721));
#48534=CARTESIAN_POINT('Ctrl Pts',(-20.3863822790797,22.9370294180387,15.1512499095187));
#48535=CARTESIAN_POINT('Ctrl Pts',(-20.3673927253354,23.0350043359179,15.1574026078264));
#48536=CARTESIAN_POINT('Ctrl Pts',(-20.3529437825933,23.133937505301,15.1635553061342));
#48537=CARTESIAN_POINT('Ctrl Pts',(-20.3431191208146,23.2333726690966,15.1697080044419));
#48538=CARTESIAN_POINT('Ctrl Pts',(-20.3332981845617,23.3327701269367,15.1758583696376));
#48539=CARTESIAN_POINT('Ctrl Pts',(-20.3280980876839,23.4326687691357,15.1820087348334));
#48540=CARTESIAN_POINT('Ctrl Pts',(-20.3275508478537,23.5326054505947,15.1881591000291));
#48541=CARTESIAN_POINT('Ctrl Pts',(-20.3270036691347,23.6325309719251,15.1943087784013));
#48542=CARTESIAN_POINT('Ctrl Pts',(-20.331108316819,23.7324940896744,15.2004584567736));
#48543=CARTESIAN_POINT('Ctrl Pts',(-20.3398446886903,23.8320308915428,15.2066081351458));
#48544=CARTESIAN_POINT('Ctrl Pts',(-20.3485824221719,23.9315832067541,15.2127587719783));
#48545=CARTESIAN_POINT('Ctrl Pts',(-20.3619532756917,24.0307086413312,15.2189094088107));
#48546=CARTESIAN_POINT('Ctrl Pts',(-20.3798853026785,24.1289486485667,15.2250600456432));
#48547=CARTESIAN_POINT('Ctrl Pts',(-20.3978365131672,24.2272937519727,15.231217262365));
#48548=CARTESIAN_POINT('Ctrl Pts',(-20.4203585628417,24.3247511083536,15.2373744790869));
#48549=CARTESIAN_POINT('Ctrl Pts',(-20.4473284210579,24.420872727952,15.2435316958087));
#48550=CARTESIAN_POINT('Ctrl Pts',(-20.4743133256475,24.5170479734083,15.2496923476165));
#48551=CARTESIAN_POINT('Ctrl Pts',(-20.5057508437871,24.6118855856704,15.2558529994243));
#48552=CARTESIAN_POINT('Ctrl Pts',(-20.5414687996424,24.7049550978298,15.2620136512321));
#48553=CARTESIAN_POINT('Ctrl Pts',(-20.5772465243392,24.798180348379,15.2681846120012));
#48554=CARTESIAN_POINT('Ctrl Pts',(-20.6173188196338,24.8896311909018,15.2743555727702));
#48555=CARTESIAN_POINT('Ctrl Pts',(-20.6614662758851,24.9788992797562,15.2805265335392));
#48556=CARTESIAN_POINT('Ctrl Pts',(-20.6951648581499,25.0470392880676,15.2852369437596));
#48557=CARTESIAN_POINT('Ctrl Pts',(-20.731236878149,25.113907959357,15.2899473539799));
#48558=CARTESIAN_POINT('Ctrl Pts',(-20.769567865836,25.1793352034948,15.2946577642003));
#48559=CARTESIAN_POINT('Ctrl Pts',(-20.8197891319366,25.2650579890619,15.3008293444124));
#48560=CARTESIAN_POINT('Ctrl Pts',(-20.8740665401047,25.3486072349034,15.3070009246245));
#48561=CARTESIAN_POINT('Ctrl Pts',(-20.9321866452656,25.4295738391929,15.3131725048365));
#48562=CARTESIAN_POINT('Ctrl Pts',(-20.9902317578737,25.5104359720208,15.3193361218395));
#48563=CARTESIAN_POINT('Ctrl Pts',(-21.0521094643142,25.5887217351737,15.3254997388424));
#48564=CARTESIAN_POINT('Ctrl Pts',(-21.1175611014027,25.6640476891033,15.3316633558453));
#48565=CARTESIAN_POINT('Ctrl Pts',(-21.18431301884,25.7408700892947,15.3379494209706));
#48566=CARTESIAN_POINT('Ctrl Pts',(-21.2547821751005,25.8146134150258,15.3442354860958));
#48567=CARTESIAN_POINT('Ctrl Pts',(-21.3286482773805,25.8849028480618,15.3505215512211));
#48568=CARTESIAN_POINT('Ctrl Pts',(-21.4009429475736,25.9536969392964,15.3566738862031));
#48569=CARTESIAN_POINT('Ctrl Pts',(-21.4764911345749,26.0191823187827,15.3628262211852));
#48570=CARTESIAN_POINT('Ctrl Pts',(-21.5549535096008,26.081042798574,15.3689785561672));
#48571=CARTESIAN_POINT('Ctrl Pts',(-21.6359741291018,26.1449202225452,15.3753314863641));
#48572=CARTESIAN_POINT('Ctrl Pts',(-21.7201019028545,26.2049319602866,15.381684416561));
#48573=CARTESIAN_POINT('Ctrl Pts',(-21.8069251862289,26.2607741289247,15.3880373467579));
#48574=CARTESIAN_POINT('Ctrl Pts',(-21.8937484696032,26.3166162975627,15.3943902769548));
#48575=CARTESIAN_POINT('Ctrl Pts',(-21.9832668367093,26.3682886146734,15.4007432071517));
#48576=CARTESIAN_POINT('Ctrl Pts',(-22.0750360153461,26.4155367745563,15.4070961373485));
#48577=CARTESIAN_POINT('Origin',(-23.5502525316942,23.5502525316942,-77.3107734492734));
#48578=CARTESIAN_POINT('',(-22.0738786772418,26.4178312615861,16.9038400528878));
#48579=CARTESIAN_POINT('',(-22.075036069343,26.4155368023571,16.6585071611381));
#48580=CARTESIAN_POINT('',(-22.0750360153461,26.4155367745563,-77.3107734492734));
#48581=CARTESIAN_POINT('',(-26.7773237984114,23.5486249559515,16.0607734492729));
#48582=CARTESIAN_POINT('Ctrl Pts',(-26.7773237984114,23.5486249559515,16.0607734492729));
#48583=CARTESIAN_POINT('Ctrl Pts',(-26.7778921634797,23.4564077062131,16.0664877007678));
#48584=CARTESIAN_POINT('Ctrl Pts',(-26.7324159232951,22.2948726347971,16.1384975893877));
#48585=CARTESIAN_POINT('Ctrl Pts',(-25.3270871613455,20.1778258218927,16.2768031151326));
#48586=CARTESIAN_POINT('Ctrl Pts',(-21.6734278000226,20.2324321416343,16.4756900265074));
#48587=CARTESIAN_POINT('Ctrl Pts',(-19.7444112386102,23.3358340950614,16.6745769378823));
#48588=CARTESIAN_POINT('Ctrl Pts',(-20.8697362492241,25.7041498884009,16.8172936133424));
#48589=CARTESIAN_POINT('Ctrl Pts',(-21.9276889255433,26.3442939038094,16.8937146516776));
#48590=CARTESIAN_POINT('Ctrl Pts',(-22.0738786772418,26.4178312615861,16.9038400528878));
#48591=CARTESIAN_POINT('Ctrl Pts',(-26.7730020461525,23.5484834757995,16.0582900309385));
#48592=CARTESIAN_POINT('Ctrl Pts',(-26.7731762945756,23.8659177764973,16.0398136118881));
#48593=CARTESIAN_POINT('Ctrl Pts',(-26.7264540989983,24.1816697163335,16.0228649312083));
#48594=CARTESIAN_POINT('Ctrl Pts',(-26.6138474838689,24.552984430688,16.0003818521498));
#48595=CARTESIAN_POINT('Ctrl Pts',(-26.5911867086148,24.6197400683399,15.9962420906808));
#48596=CARTESIAN_POINT('Ctrl Pts',(-26.5508597316809,24.7268615417604,15.9894044471309));
#48597=CARTESIAN_POINT('Ctrl Pts',(-26.5345219966239,24.7677038862891,15.9867503428131));
#48598=CARTESIAN_POINT('Ctrl Pts',(-26.514361307108,24.8152566888191,15.9836001378943));
#48599=CARTESIAN_POINT('Ctrl Pts',(-26.5113433459068,24.8223050221252,15.9831316468539));
#48600=CARTESIAN_POINT('Ctrl Pts',(-26.5066857898116,24.8330761750402,15.9824132850001));
#48601=CARTESIAN_POINT('Ctrl Pts',(-26.5050642363678,24.8368068054476,15.982164031655));
#48602=CARTESIAN_POINT('Ctrl Pts',(-26.5020969778309,24.8435982347988,15.9817094610079));
#48603=CARTESIAN_POINT('Ctrl Pts',(-26.5007535624274,24.8466600329974,15.9815042224343));
#48604=CARTESIAN_POINT('Ctrl Pts',(-26.4980453310253,24.8528063892984,15.9810916076277));
#48605=CARTESIAN_POINT('Ctrl Pts',(-26.4966804324778,24.8558909062429,15.9808842287591));
#48606=CARTESIAN_POINT('Ctrl Pts',(-26.4927890198458,24.8646478826211,15.980294592518));
#48607=CARTESIAN_POINT('Ctrl Pts',(-26.4902509600939,24.8703151676267,15.9799119383634));
#48608=CARTESIAN_POINT('Ctrl Pts',(-26.4794584897939,24.8942283748715,15.978292821229));
#48609=CARTESIAN_POINT('Ctrl Pts',(-26.4710506222014,24.9124041742604,15.9770510736214));
#48610=CARTESIAN_POINT('Ctrl Pts',(-26.2965070283962,25.2806784020311,15.9516601379762));
#48611=CARTESIAN_POINT('Ctrl Pts',(-26.0687526282821,25.5979991208634,15.9249424712313));
#48612=CARTESIAN_POINT('Ctrl Pts',(-25.7370288425477,25.9187164459496,15.8942136619572));
#48613=CARTESIAN_POINT('Ctrl Pts',(-25.681972715479,25.9683887249353,15.8893389037841));
#48614=CARTESIAN_POINT('Ctrl Pts',(-25.6062658671256,26.0320950387839,15.882980536931));
#48615=CARTESIAN_POINT('Ctrl Pts',(-25.5870986560268,26.047849580302,15.8813988759047));
#48616=CARTESIAN_POINT('Ctrl Pts',(-25.5604465678583,26.0692454323661,15.8792401930912));
#48617=CARTESIAN_POINT('Ctrl Pts',(-25.553116734926,26.0750773345519,15.878650678345));
#48618=CARTESIAN_POINT('Ctrl Pts',(-25.5405320372317,26.085000922321,15.8776457849238));
#48619=CARTESIAN_POINT('Ctrl Pts',(-25.5352897739234,26.0891083887277,15.8772293234514));
#48620=CARTESIAN_POINT('Ctrl Pts',(-25.5278937547845,26.0948664744263,15.8766448047645));
#48621=CARTESIAN_POINT('Ctrl Pts',(-25.5257506353154,26.0965306326745,15.8764757888738));
#48622=CARTESIAN_POINT('Ctrl Pts',(-25.5222221823097,26.0992633830898,15.8761981115069));
#48623=CARTESIAN_POINT('Ctrl Pts',(-25.5208380812546,26.1003335530305,15.8760893369247));
#48624=CARTESIAN_POINT('Ctrl Pts',(-25.5179457126725,26.1025661358745,15.875862342959));
#48625=CARTESIAN_POINT('Ctrl Pts',(-25.5164372862144,26.1037283392309,15.875744138872));
#48626=CARTESIAN_POINT('Ctrl Pts',(-25.5131160264617,26.1062825955944,15.8754842651549));
#48627=CARTESIAN_POINT('Ctrl Pts',(-25.5113027372233,26.1076740609152,15.8753426376108));
#48628=CARTESIAN_POINT('Ctrl Pts',(-25.5051697836236,26.1123699527427,15.8748644739299));
#48629=CARTESIAN_POINT('Ctrl Pts',(-25.50084320459,26.1156653969009,15.8745285739121));
#48630=CARTESIAN_POINT('Ctrl Pts',(-25.4605395149139,26.1462027767031,15.8714125703997));
#48631=CARTESIAN_POINT('Ctrl Pts',(-25.4240000518611,26.1726988650413,15.8686838841043));
#48632=CARTESIAN_POINT('Ctrl Pts',(-25.3055356294849,26.2548609642573,15.8600978992325));
#48633=CARTESIAN_POINT('Ctrl Pts',(-25.2215918020301,26.3075254403933,15.8544002597142));
#48634=CARTESIAN_POINT('Ctrl Pts',(-25.0799124164264,26.3875597250451,15.8451785731714));
#48635=CARTESIAN_POINT('Ctrl Pts',(-25.0235587237739,26.4172266646204,15.841607374563));
#48636=CARTESIAN_POINT('Ctrl Pts',(-24.8551328753848,26.4996146975565,15.8311182625791));
#48637=CARTESIAN_POINT('Ctrl Pts',(-24.7408615150434,26.5475678767339,15.8242311485049));
#48638=CARTESIAN_POINT('Ctrl Pts',(-24.4600503345786,26.6468095801522,15.8073603647747));
#48639=CARTESIAN_POINT('Ctrl Pts',(-24.2915810314722,26.6914014188752,15.7972691325196));
#48640=CARTESIAN_POINT('Ctrl Pts',(-24.1072813554618,26.7245261174362,15.785893576524));
#48641=CARTESIAN_POINT('Ctrl Pts',(-24.0941970452484,26.7267944038485,15.785084314555));
#48642=CARTESIAN_POINT('Ctrl Pts',(-24.0760826730019,26.7298194979336,15.7839615367968));
#48643=CARTESIAN_POINT('Ctrl Pts',(-24.0710641514428,26.7306453826756,15.7836502202713));
#48644=CARTESIAN_POINT('Ctrl Pts',(-24.062587541198,26.7320197544366,15.7831239485304));
#48645=CARTESIAN_POINT('Ctrl Pts',(-24.0591304638352,26.7325744939895,15.7829091924718));
#48646=CARTESIAN_POINT('Ctrl Pts',(-24.0522868140439,26.7336612226664,15.7824838143815));
#48647=CARTESIAN_POINT('Ctrl Pts',(-24.0489002827755,26.7341934442429,15.7822732000442));
#48648=CARTESIAN_POINT('Ctrl Pts',(-24.0414332847372,26.7353547398381,15.7818085492307));
#48649=CARTESIAN_POINT('Ctrl Pts',(-24.0373524495981,26.7359813773768,15.7815544356708));
#48650=CARTESIAN_POINT('Ctrl Pts',(-24.0230901318942,26.7381433997283,15.780665704856));
#48651=CARTESIAN_POINT('Ctrl Pts',(-24.0129025863662,26.739637818175,15.7800297888816));
#48652=CARTESIAN_POINT('Ctrl Pts',(-23.9082339337787,26.7544796954288,15.7734847074987));
#48653=CARTESIAN_POINT('Ctrl Pts',(-23.813220522853,26.7636723797295,15.7674445014694));
#48654=CARTESIAN_POINT('Ctrl Pts',(-23.552372642849,26.7772638899716,15.750567214016));
#48655=CARTESIAN_POINT('Ctrl Pts',(-23.3863988929209,26.7731001577007,15.7394913032342));
#48656=CARTESIAN_POINT('Ctrl Pts',(-23.0657411463947,26.7402184403829,15.7177103454699));
#48657=CARTESIAN_POINT('Ctrl Pts',(-22.9113481791072,26.7129156773048,15.7070506753344));
#48658=CARTESIAN_POINT('Ctrl Pts',(-22.6961515304407,26.6584522597489,15.6923645106842));
#48659=CARTESIAN_POINT('Ctrl Pts',(-22.6332535893546,26.6404803974442,15.6880953643322));
#48660=CARTESIAN_POINT('Ctrl Pts',(-22.553046589218,26.6148978113509,15.6827180749298));
#48661=CARTESIAN_POINT('Ctrl Pts',(-22.5352010836062,26.6090334944509,15.6815259977277));
#48662=CARTESIAN_POINT('Ctrl Pts',(-22.5101782080147,26.6005674674096,15.6798615836035));
#48663=CARTESIAN_POINT('Ctrl Pts',(-22.5029576494625,26.598095906646,15.6793821402659));
#48664=CARTESIAN_POINT('Ctrl Pts',(-22.4920292778801,26.5943117585682,15.6786578424772));
#48665=CARTESIAN_POINT('Ctrl Pts',(-22.48831503777,26.593018015759,15.678411910174));
#48666=CARTESIAN_POINT('Ctrl Pts',(-22.4814818345048,26.5906238409219,15.6779599073608));
#48667=CARTESIAN_POINT('Ctrl Pts',(-22.4783621854736,26.5895254031322,15.6777537203965));
#48668=CARTESIAN_POINT('Ctrl Pts',(-22.4733254344228,26.5877432283603,15.6774211102004));
#48669=CARTESIAN_POINT('Ctrl Pts',(-22.4714072898055,26.5870624778844,15.6772945089123));
#48670=CARTESIAN_POINT('Ctrl Pts',(-22.4677197504036,26.5857498336116,15.6770512539575));
#48671=CARTESIAN_POINT('Ctrl Pts',(-22.4659502762978,26.5851182143027,15.6769345853124));
#48672=CARTESIAN_POINT('Ctrl Pts',(-22.4619228705945,26.5836766473545,15.6766691721931));
#48673=CARTESIAN_POINT('Ctrl Pts',(-22.459665293269,26.5828657269719,15.6765204869486));
#48674=CARTESIAN_POINT('Ctrl Pts',(-22.4526549359712,26.5803387703929,15.6760590641566));
#48675=CARTESIAN_POINT('Ctrl Pts',(-22.4479052555735,26.5786140655506,15.6757468439657));
#48676=CARTESIAN_POINT('Ctrl Pts',(-22.4118273264727,26.5654173162887,15.6733781982146));
#48677=CARTESIAN_POINT('Ctrl Pts',(-22.3806733919683,26.5534700521566,15.6713496813345));
#48678=CARTESIAN_POINT('Ctrl Pts',(-22.2561677256447,26.5034917679209,15.663289442689));
#48679=CARTESIAN_POINT('Ctrl Pts',(-22.1645124296855,26.4616044966735,15.6574615682194));
#48680=CARTESIAN_POINT('Ctrl Pts',(-22.0750357147148,26.4155366197736,15.6517373095584));
#48681=CARTESIAN_POINT('',(-26.7730019920283,23.5483874803723,15.8142265507266));
#48682=CARTESIAN_POINT('Ctrl Pts',(-22.0750360153461,26.4155367745563,15.4070961373485));
#48683=CARTESIAN_POINT('Ctrl Pts',(-22.163885353475,26.4612816291552,15.4132469349427));
#48684=CARTESIAN_POINT('Ctrl Pts',(-22.2548440136306,26.5028794401595,15.4193977325368));
#48685=CARTESIAN_POINT('Ctrl Pts',(-22.3474855442512,26.5401470342507,15.4255485301309));
#48686=CARTESIAN_POINT('Ctrl Pts',(-22.4402273622975,26.5774549717067,15.4317059861605));
#48687=CARTESIAN_POINT('Ctrl Pts',(-22.5346552845119,26.6104231702702,15.4378634421901));
#48688=CARTESIAN_POINT('Ctrl Pts',(-22.6303246422378,26.6389173307134,15.4440208982197));
#48689=CARTESIAN_POINT('Ctrl Pts',(-22.726049365229,26.6674279811466,15.4501819176597));
#48690=CARTESIAN_POINT('Ctrl Pts',(-22.8230165328247,26.6914593331419,15.4563429370998));
#48691=CARTESIAN_POINT('Ctrl Pts',(-22.9207701789003,26.7109280180453,15.4625039565398));
#48692=CARTESIAN_POINT('Ctrl Pts',(-23.0186848355554,26.7304287699291,15.4686751238296));
#48693=CARTESIAN_POINT('Ctrl Pts',(-23.1173881283593,26.7453517808918,15.4748462911193));
#48694=CARTESIAN_POINT('Ctrl Pts',(-23.2164177695234,26.7556654402079,15.4810174584091));
#48695=CARTESIAN_POINT('Ctrl Pts',(-23.2834264764393,26.7626442090515,15.4851931974644));
#48696=CARTESIAN_POINT('Ctrl Pts',(-23.3505845259072,26.7675136305882,15.4893689365198));
#48697=CARTESIAN_POINT('Ctrl Pts',(-23.4177491731461,26.7702774419198,15.4935446755752));
#48698=CARTESIAN_POINT('Ctrl Pts',(-23.5170241350681,26.7743625860541,15.4997167668875));
#48699=CARTESIAN_POINT('Ctrl Pts',(-23.6166630386624,26.7738595788928,15.5058888581998));
#48700=CARTESIAN_POINT('Ctrl Pts',(-23.7162062091023,26.7687268502891,15.5120609495121));
#48701=CARTESIAN_POINT('Ctrl Pts',(-23.8156145083873,26.7636010760252,15.5182246782509));
#48702=CARTESIAN_POINT('Ctrl Pts',(-23.9149269023268,26.7538580703781,15.5243884069897));
#48703=CARTESIAN_POINT('Ctrl Pts',(-24.0136809531081,26.7395081910489,15.5305521357285));
#48704=CARTESIAN_POINT('Ctrl Pts',(-24.112330383241,26.72517351407,15.5367093345751));
#48705=CARTESIAN_POINT('Ctrl Pts',(-24.2104222186818,26.7062417285075,15.5428665334218));
#48706=CARTESIAN_POINT('Ctrl Pts',(-24.3074973562965,26.6827751314711,15.5490237322685));
#48707=CARTESIAN_POINT('Ctrl Pts',(-24.4045015378728,26.659325687094,15.5551764305762));
#48708=CARTESIAN_POINT('Ctrl Pts',(-24.5004900781541,26.6313481231318,15.5613291288839));
#48709=CARTESIAN_POINT('Ctrl Pts',(-24.5950132198864,26.598955971996,15.5674818271916));
#48710=CARTESIAN_POINT('Ctrl Pts',(-24.6895005183089,26.5665761040101,15.5736321923874));
#48711=CARTESIAN_POINT('Ctrl Pts',(-24.7825231118306,26.5297851157756,15.5797825575831));
#48712=CARTESIAN_POINT('Ctrl Pts',(-24.8736464464446,26.4887463821049,15.5859329227789));
#48713=CARTESIAN_POINT('Ctrl Pts',(-24.9647596051343,26.4477122313114,15.5920826011511));
#48714=CARTESIAN_POINT('Ctrl Pts',(-25.0539735305013,26.4024314565456,15.5982322795233));
#48715=CARTESIAN_POINT('Ctrl Pts',(-25.1408746332202,26.3531151563401,15.6043819578956));
#48716=CARTESIAN_POINT('Ctrl Pts',(-25.2277892799402,26.3037911699258,15.610532594728));
#48717=CARTESIAN_POINT('Ctrl Pts',(-25.3123900101946,26.250430623224,15.6166832315605));
#48718=CARTESIAN_POINT('Ctrl Pts',(-25.3942896628079,26.1932895389217,15.6228338683929));
#48719=CARTESIAN_POINT('Ctrl Pts',(-25.476276930845,26.1360873256626,15.6289910851147));
#48720=CARTESIAN_POINT('Ctrl Pts',(-25.5555569940663,26.0750967476206,15.6351483018365));
#48721=CARTESIAN_POINT('Ctrl Pts',(-25.6317735251724,26.0106159024607,15.6413055185584));
#48722=CARTESIAN_POINT('Ctrl Pts',(-25.7080325771692,25.9460990837013,15.6474661703662));
#48723=CARTESIAN_POINT('Ctrl Pts',(-25.7812243751031,25.8780884157034,15.653626822174));
#48724=CARTESIAN_POINT('Ctrl Pts',(-25.8510289554246,25.806919412407,15.6597874739818));
#48725=CARTESIAN_POINT('Ctrl Pts',(-25.9209503436319,25.7356313180602,15.6659584347508));
#48726=CARTESIAN_POINT('Ctrl Pts',(-25.9874729029315,25.6611746558161,15.6721293955199));
#48727=CARTESIAN_POINT('Ctrl Pts',(-26.05031642152,25.5839187061902,15.6783003562889));
#48728=CARTESIAN_POINT('Ctrl Pts',(-26.0982860592022,25.5249477892907,15.6830107665093));
#48729=CARTESIAN_POINT('Ctrl Pts',(-26.1441129048545,25.4643465513133,15.6877211767296));
#48730=CARTESIAN_POINT('Ctrl Pts',(-26.1876898325281,25.4022898009386,15.69243158695));
#48731=CARTESIAN_POINT('Ctrl Pts',(-26.2454387822507,25.3200510487213,15.6986739096081));
#48732=CARTESIAN_POINT('Ctrl Pts',(-26.2994360637396,25.2349687783033,15.7049162322662));
#48733=CARTESIAN_POINT('Ctrl Pts',(-26.3493933091914,25.1474151628162,15.7111585549243));
#48734=CARTESIAN_POINT('Ctrl Pts',(-26.399279228004,25.0599865523226,15.7173919650835));
#48735=CARTESIAN_POINT('Ctrl Pts',(-26.4451363713419,24.9700939741101,15.7236253752428));
#48736=CARTESIAN_POINT('Ctrl Pts',(-26.4867185018539,24.8781400151031,15.729858785402));
#48737=CARTESIAN_POINT('Ctrl Pts',(-26.5282515144078,24.7862946746457,15.7360848324854));
#48738=CARTESIAN_POINT('Ctrl Pts',(-26.5655193832855,24.6923931770856,15.7423108795688));
#48739=CARTESIAN_POINT('Ctrl Pts',(-26.5983212629338,24.596863525397,15.7485369266522));
#48740=CARTESIAN_POINT('Ctrl Pts',(-26.631088380122,24.5014351132025,15.7547563755553));
#48741=CARTESIAN_POINT('Ctrl Pts',(-26.6593987923052,24.4043823783789,15.7609758244585));
#48742=CARTESIAN_POINT('Ctrl Pts',(-26.6830997521404,24.3061532234802,15.7671952733617));
#48743=CARTESIAN_POINT('Ctrl Pts',(-26.7067859713451,24.207985161452,15.7734108541262));
#48744=CARTESIAN_POINT('Ctrl Pts',(-26.7258683414404,24.1086425433305,15.7796264348908));
#48745=CARTESIAN_POINT('Ctrl Pts',(-26.7402441209884,24.0085878049735,15.7858420156554));
#48746=CARTESIAN_POINT('Ctrl Pts',(-26.7546153903739,23.9085644571325,15.7920556463845));
#48747=CARTESIAN_POINT('Ctrl Pts',(-26.7642829443631,23.8078298499944,15.7982692771136));
#48748=CARTESIAN_POINT('Ctrl Pts',(-26.7691953950023,23.7068552304513,15.8044829078427));
#48749=CARTESIAN_POINT('Ctrl Pts',(-26.7717631457426,23.6540755338959,15.807730788804));
#48750=CARTESIAN_POINT('Ctrl Pts',(-26.77303257297,23.6012303765799,15.8109786697653));
#48751=CARTESIAN_POINT('Ctrl Pts',(-26.7730019920283,23.5483874803723,15.8142265507266));
#48752=CARTESIAN_POINT('Ctrl Pts',(-26.7730018961391,23.5482285578474,15.8117750777804));
#48753=CARTESIAN_POINT('Ctrl Pts',(-26.7728046263283,23.2341181960848,15.8321379522218));
#48754=CARTESIAN_POINT('Ctrl Pts',(-26.7266920806876,22.921780688606,15.8538922170526));
#48755=CARTESIAN_POINT('Ctrl Pts',(-26.6171748740879,22.558066115835,15.8790274192304));
#48756=CARTESIAN_POINT('Ctrl Pts',(-26.5962785012017,22.4956561139789,15.8833234263691));
#48757=CARTESIAN_POINT('Ctrl Pts',(-26.5636287593405,22.4072342349994,15.8893442082632));
#48758=CARTESIAN_POINT('Ctrl Pts',(-26.5534195926227,22.3806736086413,15.8911440443552));
#48759=CARTESIAN_POINT('Ctrl Pts',(-26.5412092483208,22.3501211816968,15.8932013752921));
#48760=CARTESIAN_POINT('Ctrl Pts',(-26.5395503688379,22.3459951757296,15.8934789349227));
#48761=CARTESIAN_POINT('Ctrl Pts',(-26.5370198851222,22.3397387411227,15.8938993759731));
#48762=CARTESIAN_POINT('Ctrl Pts',(-26.5361545385679,22.3376058122847,15.8940426350278));
#48763=CARTESIAN_POINT('Ctrl Pts',(-26.5345837512811,22.33374597021,15.8943017415655));
#48764=CARTESIAN_POINT('Ctrl Pts',(-26.5338790984175,22.33201874759,15.8944176364623));
#48765=CARTESIAN_POINT('Ctrl Pts',(-26.5324602414214,22.3285495059147,15.8946503154213));
#48766=CARTESIAN_POINT('Ctrl Pts',(-26.5317460133275,22.3268075079281,15.8947670973482));
#48767=CARTESIAN_POINT('Ctrl Pts',(-26.5297062122066,22.3218448395999,15.8950996435703));
#48768=CARTESIAN_POINT('Ctrl Pts',(-26.5283769391468,22.3186256781698,15.8953151822458));
#48769=CARTESIAN_POINT('Ctrl Pts',(-26.5226881611175,22.3049119630758,15.8962326583744));
#48770=CARTESIAN_POINT('Ctrl Pts',(-26.5182783134091,22.2944381859082,15.8969315653357));
#48771=CARTESIAN_POINT('Ctrl Pts',(-26.4365297888622,22.1031142941592,15.9096691081607));
#48772=CARTESIAN_POINT('Ctrl Pts',(-26.3428363640157,21.9296642434892,15.9207480771629));
#48773=CARTESIAN_POINT('Ctrl Pts',(-26.1429810057039,21.6290979916271,15.9409467374906));
#48774=CARTESIAN_POINT('Ctrl Pts',(-26.0417556556983,21.4995245614739,15.9500594765916));
#48775=CARTESIAN_POINT('Ctrl Pts',(-25.8889610684588,21.3320393289377,15.9630482950718));
#48776=CARTESIAN_POINT('Ctrl Pts',(-25.8454851776859,21.2870835365266,15.9666685772429));
#48777=CARTESIAN_POINT('Ctrl Pts',(-25.7620089369155,21.2056464709397,15.9735154644692));
#48778=CARTESIAN_POINT('Ctrl Pts',(-25.7223438230463,21.1688531752513,15.9767281623027));
#48779=CARTESIAN_POINT('Ctrl Pts',(-25.6670583362606,21.1201011685873,15.981163379127));
#48780=CARTESIAN_POINT('Ctrl Pts',(-25.6522255844581,21.1072601614108,15.9823492686703));
#48781=CARTESIAN_POINT('Ctrl Pts',(-25.626890928256,21.0857289860596,15.9843685178538));
#48782=CARTESIAN_POINT('Ctrl Pts',(-25.6164493334037,21.0769684589018,15.985198970323));
#48783=CARTESIAN_POINT('Ctrl Pts',(-25.6020002200609,21.0650009703118,15.9863458515667));
#48784=CARTESIAN_POINT('Ctrl Pts',(-25.5980400401563,21.0617368657247,15.9866599502281));
#48785=CARTESIAN_POINT('Ctrl Pts',(-25.591650143486,21.0564956940417,15.9871663881908));
#48786=CARTESIAN_POINT('Ctrl Pts',(-25.5892253001927,21.0545126766654,15.9873584858278));
#48787=CARTESIAN_POINT('Ctrl Pts',(-25.5841679473789,21.0503891041346,15.9877589559783));
#48788=CARTESIAN_POINT('Ctrl Pts',(-25.5815349420605,21.048249165628,15.9879673530847));
#48789=CARTESIAN_POINT('Ctrl Pts',(-25.5754577119258,21.0433258973237,15.9884481278494));
#48790=CARTESIAN_POINT('Ctrl Pts',(-25.572011125737,21.0405455051164,15.9887206234925));
#48791=CARTESIAN_POINT('Ctrl Pts',(-25.5612736199777,21.031919934766,15.9895690478977));
#48792=CARTESIAN_POINT('Ctrl Pts',(-25.5539630491226,21.0260993973405,15.9901459649327));
#48793=CARTESIAN_POINT('Ctrl Pts',(-25.4919343253948,20.9771525862421,15.9950350486004));
#48794=CARTESIAN_POINT('Ctrl Pts',(-25.4358599983036,20.9357822649959,15.9994165019083));
#48795=CARTESIAN_POINT('Ctrl Pts',(-25.3726372178957,20.8922303022475,16.0043210452401));
#48796=CARTESIAN_POINT('Ctrl Pts',(-25.3667685945868,20.8882161854501,16.0047759728684));
#48797=CARTESIAN_POINT('Ctrl Pts',(-25.2447915163293,20.8053754849056,16.0142245766527));
#48798=CARTESIAN_POINT('Ctrl Pts',(-25.1236837315748,20.7342059427412,16.0234868806989));
#48799=CARTESIAN_POINT('Ctrl Pts',(-24.9114186690282,20.6274439134964,16.0394321673669));
#48800=CARTESIAN_POINT('Ctrl Pts',(-24.8225673036688,20.5876864548579,16.0460247431171));
#48801=CARTESIAN_POINT('Ctrl Pts',(-24.552109253191,20.4810812344191,16.065696558887));
#48802=CARTESIAN_POINT('Ctrl Pts',(-24.3661168695984,20.4264864061892,16.0787277483863));
#48803=CARTESIAN_POINT('Ctrl Pts',(-24.168604770611,20.3873709206322,16.0913685036925));
#48804=CARTESIAN_POINT('Ctrl Pts',(-24.160874195007,20.3858693746855,16.0918613554545));
#48805=CARTESIAN_POINT('Ctrl Pts',(-24.1502857383422,20.3838529762968,16.0925337296076));
#48806=CARTESIAN_POINT('Ctrl Pts',(-24.1474326332544,20.383313643752,16.0927146379334));
#48807=CARTESIAN_POINT('Ctrl Pts',(-24.1426489033622,20.3824160528144,16.0930175124967));
#48808=CARTESIAN_POINT('Ctrl Pts',(-24.1407186802346,20.3820557029658,16.0931395989234));
#48809=CARTESIAN_POINT('Ctrl Pts',(-24.1369094771843,20.3813481718437,16.093380286931));
#48810=CARTESIAN_POINT('Ctrl Pts',(-24.1350305174239,20.3810008974731,16.0934988937221));
#48811=CARTESIAN_POINT('Ctrl Pts',(-24.1308788305256,20.3802373894404,16.0937607070686));
#48812=CARTESIAN_POINT('Ctrl Pts',(-24.1286059585695,20.3798219277047,16.0939038691588));
#48813=CARTESIAN_POINT('Ctrl Pts',(-24.1208446038823,20.3784118417686,16.0943921632216));
#48814=CARTESIAN_POINT('Ctrl Pts',(-24.1153539463309,20.3774290151097,16.0947366222004));
#48815=CARTESIAN_POINT('Ctrl Pts',(-24.0610541735627,20.3678547908458,16.0981337322372));
#48816=CARTESIAN_POINT('Ctrl Pts',(-24.0120522970798,20.3603755218276,16.1011242782874));
#48817=CARTESIAN_POINT('Ctrl Pts',(-23.9573550715616,20.3533139527502,16.1043985952163));
#48818=CARTESIAN_POINT('Ctrl Pts',(-23.9518140873578,20.3526132347569,16.1047295667845));
#48819=CARTESIAN_POINT('Ctrl Pts',(-23.9424677781203,20.3514559687116,16.1052866543154));
#48820=CARTESIAN_POINT('Ctrl Pts',(-23.9386634286815,20.3509918004893,16.1055130829104));
#48821=CARTESIAN_POINT('Ctrl Pts',(-23.6839352924637,20.3203735107428,16.1206525324504));
#48822=CARTESIAN_POINT('Ctrl Pts',(-23.4303091735725,20.3198295495388,16.1343854323784));
#48823=CARTESIAN_POINT('Ctrl Pts',(-23.0677411940706,20.3618530963051,16.154960166579));
#48824=CARTESIAN_POINT('Ctrl Pts',(-22.9570375205518,20.3805835952993,16.1613625019256));
#48825=CARTESIAN_POINT('Ctrl Pts',(-22.7898196956833,20.4179438469617,16.1713903776175));
#48826=CARTESIAN_POINT('Ctrl Pts',(-22.7324658839398,20.4324263426966,16.1748947941917));
#48827=CARTESIAN_POINT('Ctrl Pts',(-22.655366143927,20.4541686332814,16.1797096000117));
#48828=CARTESIAN_POINT('Ctrl Pts',(-22.6352431548661,20.4600559422142,16.1809759395686));
#48829=CARTESIAN_POINT('Ctrl Pts',(-22.6059026853705,20.4689516865248,16.1828370969296));
#48830=CARTESIAN_POINT('Ctrl Pts',(-22.5966387889225,20.4718061122993,16.183426898248));
#48831=CARTESIAN_POINT('Ctrl Pts',(-22.5800311541497,20.4770054754259,16.1844882015277));
#48832=CARTESIAN_POINT('Ctrl Pts',(-22.5726826570633,20.4793350582195,16.1849591975514));
#48833=CARTESIAN_POINT('Ctrl Pts',(-22.5614771997892,20.4829316507903,16.1856795566684));
#48834=CARTESIAN_POINT('Ctrl Pts',(-22.5576141223763,20.4841796311387,16.1859282920167));
#48835=CARTESIAN_POINT('Ctrl Pts',(-22.5506047118037,20.486458680728,16.1863803288407));
#48836=CARTESIAN_POINT('Ctrl Pts',(-22.5474575852717,20.487487307207,16.186583549398));
#48837=CARTESIAN_POINT('Ctrl Pts',(-22.5411568109731,20.489557444106,16.1869909397812));
#48838=CARTESIAN_POINT('Ctrl Pts',(-22.5380031768769,20.4905989832829,16.1871951103564));
#48839=CARTESIAN_POINT('Ctrl Pts',(-22.5292024394174,20.4935206663934,16.1877656267725));
#48840=CARTESIAN_POINT('Ctrl Pts',(-22.5235589475374,20.4954115749872,16.1881323286722));
#48841=CARTESIAN_POINT('Ctrl Pts',(-22.5008637480211,20.5030858228637,16.1896104913225));
#48842=CARTESIAN_POINT('Ctrl Pts',(-22.4838556624521,20.5089963000042,16.1907261631966));
#48843=CARTESIAN_POINT('Ctrl Pts',(-22.238943061262,20.5964128761868,16.2069083962712));
#48844=CARTESIAN_POINT('Ctrl Pts',(-22.0209283932317,20.7031798509227,16.2228694379229));
#48845=CARTESIAN_POINT('Ctrl Pts',(-21.6897723810268,20.9144433432028,16.2493873880407));
#48846=CARTESIAN_POINT('Ctrl Pts',(-21.5684413600974,21.004412244643,16.259661852537));
#48847=CARTESIAN_POINT('Ctrl Pts',(-21.3807788396897,21.1651405073939,16.2760967010109));
#48848=CARTESIAN_POINT('Ctrl Pts',(-21.3105320186083,21.230978623866,16.2823883777088));
#48849=CARTESIAN_POINT('Ctrl Pts',(-21.2371432988625,21.3062111442115,16.2890219083685));
#48850=CARTESIAN_POINT('Ctrl Pts',(-21.2309822508871,21.3125793114501,16.2895792801893));
#48851=CARTESIAN_POINT('Ctrl Pts',(-21.2204005971008,21.3236073470871,16.2905372742825));
#48852=CARTESIAN_POINT('Ctrl Pts',(-21.2159675512014,21.3282551314257,16.2909388285018));
#48853=CARTESIAN_POINT('Ctrl Pts',(-21.2097078788499,21.3348574322945,16.291506106839));
#48854=CARTESIAN_POINT('Ctrl Pts',(-21.2078697828678,21.3368009789089,16.2916727154789));
#48855=CARTESIAN_POINT('Ctrl Pts',(-21.2047183466866,21.3401415331483,16.2919584201328));
#48856=CARTESIAN_POINT('Ctrl Pts',(-21.2034038315663,21.3415374260929,16.2920776078245));
#48857=CARTESIAN_POINT('Ctrl Pts',(-21.200891551821,21.3442100086932,16.2923054259543));
#48858=CARTESIAN_POINT('Ctrl Pts',(-21.1996935832901,21.3454864994013,16.292414072509));
#48859=CARTESIAN_POINT('Ctrl Pts',(-21.1968799906056,21.3484894118067,16.2926692751785));
#48860=CARTESIAN_POINT('Ctrl Pts',(-21.1952652224529,21.3502166395682,16.2928157646713));
#48861=CARTESIAN_POINT('Ctrl Pts',(-21.190519176012,21.3553044341759,16.2932463967786));
#48862=CARTESIAN_POINT('Ctrl Pts',(-21.1873931628272,21.3586699381573,16.2935301347626));
#48863=CARTESIAN_POINT('Ctrl Pts',(-21.1608849768732,21.3873316199847,16.295937161982));
#48864=CARTESIAN_POINT('Ctrl Pts',(-21.1379014396724,21.4129957326738,16.2980305477768));
#48865=CARTESIAN_POINT('Ctrl Pts',(-21.1115917740185,21.4433391777641,16.3004413494327));
#48866=CARTESIAN_POINT('Ctrl Pts',(-21.1078622827492,21.4476636406365,16.300783436523));
#48867=CARTESIAN_POINT('Ctrl Pts',(-20.9034181048028,21.6860010726898,16.3195566678349));
#48868=CARTESIAN_POINT('Ctrl Pts',(-20.7372799891048,21.9476264136509,16.3360382288832));
#48869=CARTESIAN_POINT('Ctrl Pts',(-20.5695687409252,22.3207109646318,16.359312903484));
#48870=CARTESIAN_POINT('Ctrl Pts',(-20.5326273929913,22.4143897292331,16.3651257639763));
#48871=CARTESIAN_POINT('Ctrl Pts',(-20.4862942302259,22.5501957876227,16.3736127145109));
#48872=CARTESIAN_POINT('Ctrl Pts',(-20.4732679082469,22.5910240219667,16.3761713397166));
#48873=CARTESIAN_POINT('Ctrl Pts',(-20.4563592655472,22.6479143148062,16.379751794366));
#48874=CARTESIAN_POINT('Ctrl Pts',(-20.4517801593,22.6637657907418,16.3807510367652));
#48875=CARTESIAN_POINT('Ctrl Pts',(-20.4451299067435,22.6874681115356,16.3822478508855));
#48876=CARTESIAN_POINT('Ctrl Pts',(-20.4429663315177,22.6952929186405,16.3827424238359));
#48877=CARTESIAN_POINT('Ctrl Pts',(-20.4390779389906,22.7095654532638,16.3836453529233));
#48878=CARTESIAN_POINT('Ctrl Pts',(-20.4373435369129,22.7160105408574,16.3840533958741));
#48879=CARTESIAN_POINT('Ctrl Pts',(-20.43464622549,22.7261593623094,16.3846964199982));
#48880=CARTESIAN_POINT('Ctrl Pts',(-20.4336698637091,22.7298595280059,16.3849309639778));
#48881=CARTESIAN_POINT('Ctrl Pts',(-20.4319323877105,22.7364919896466,16.3853515670648));
#48882=CARTESIAN_POINT('Ctrl Pts',(-20.4311688120609,22.739423640998,16.3855375460546));
#48883=CARTESIAN_POINT('Ctrl Pts',(-20.4295583925683,22.7456425790151,16.3859322064378));
#48884=CARTESIAN_POINT('Ctrl Pts',(-20.4287126071909,22.7489301337069,16.3861409218915));
#48885=CARTESIAN_POINT('Ctrl Pts',(-20.4263079516749,22.7583385724532,16.3867384739902));
#48886=CARTESIAN_POINT('Ctrl Pts',(-20.4247618861351,22.76446268607,16.3871277247842));
#48887=CARTESIAN_POINT('Ctrl Pts',(-20.4181745419809,22.7908828114572,16.3888082948649));
#48888=CARTESIAN_POINT('Ctrl Pts',(-20.4133129706029,22.8112227200402,16.3901054078012));
#48889=CARTESIAN_POINT('Ctrl Pts',(-20.3236170564444,23.2033344889079,16.4151788063718));
#48890=CARTESIAN_POINT('Ctrl Pts',(-20.3052567811658,23.5871522308096,16.4414266759297));
#48891=CARTESIAN_POINT('Ctrl Pts',(-20.3614447576155,24.020031485543,16.4705448497468));
#48892=CARTESIAN_POINT('Ctrl Pts',(-20.3699926179472,24.0747854490492,16.474208191151));
#48893=CARTESIAN_POINT('Ctrl Pts',(-20.3862101741792,24.1635779747463,16.4800899704882));
#48894=CARTESIAN_POINT('Ctrl Pts',(-20.3930279092952,24.1977593167627,16.4823397899832));
#48895=CARTESIAN_POINT('Ctrl Pts',(-20.4060283107048,24.2578400475598,16.4862610472686));
#48896=CARTESIAN_POINT('Ctrl Pts',(-20.4119798587934,24.2837856174466,16.4879433807958));
#48897=CARTESIAN_POINT('Ctrl Pts',(-20.4192823851471,24.3139033742627,16.4898809808332));
#48898=CARTESIAN_POINT('Ctrl Pts',(-20.4203210020499,24.3181491967485,16.4901537775683));
#48899=CARTESIAN_POINT('Ctrl Pts',(-20.4219159178755,24.3246121497252,16.4905684720561));
#48900=CARTESIAN_POINT('Ctrl Pts',(-20.4224659376056,24.3268308016153,16.4907107319728));
#48901=CARTESIAN_POINT('Ctrl Pts',(-20.4234689031042,24.3308581805945,16.4909687842031));
#48902=CARTESIAN_POINT('Ctrl Pts',(-20.4239210565671,24.3326670936724,16.4910846220363));
#48903=CARTESIAN_POINT('Ctrl Pts',(-20.4249047552221,24.3365880719622,16.4913355645832));
#48904=CARTESIAN_POINT('Ctrl Pts',(-20.4254368701059,24.3386999852049,16.4914706353187));
#48905=CARTESIAN_POINT('Ctrl Pts',(-20.42689564839,24.3444650638738,16.4918391036701));
#48906=CARTESIAN_POINT('Ctrl Pts',(-20.4278265835876,24.348117160369,16.4920722529825));
#48907=CARTESIAN_POINT('Ctrl Pts',(-20.4323457858973,24.3657171262349,16.4931945660176));
#48908=CARTESIAN_POINT('Ctrl Pts',(-20.4360211891225,24.3796427556997,16.4940787375349));
#48909=CARTESIAN_POINT('Ctrl Pts',(-20.5044369579604,24.6319929870953,16.5100390938856));
#48910=CARTESIAN_POINT('Ctrl Pts',(-20.596300950982,24.8622617147293,16.5236358568257));
#48911=CARTESIAN_POINT('Ctrl Pts',(-20.7825040977251,25.2075892230795,16.5455764208667));
#48912=CARTESIAN_POINT('Ctrl Pts',(-20.8599632540827,25.3305714729923,16.5537392769632));
#48913=CARTESIAN_POINT('Ctrl Pts',(-20.9980124017785,25.5200642275414,16.5673467523794));
#48914=CARTESIAN_POINT('Ctrl Pts',(-21.0535524555293,25.5900011333779,16.5726195010925));
#48915=CARTESIAN_POINT('Ctrl Pts',(-21.1219830814292,25.6691819488672,16.5789390759949));
#48916=CARTESIAN_POINT('Ctrl Pts',(-21.132129049664,25.6807532266075,16.5798717415497));
#48917=CARTESIAN_POINT('Ctrl Pts',(-21.1474834237992,25.6980136119804,16.5812769833772));
#48918=CARTESIAN_POINT('Ctrl Pts',(-21.1526301087282,25.7037575256785,16.5817469810553));
#48919=CARTESIAN_POINT('Ctrl Pts',(-21.1609474455475,25.712973242686,16.5825048997269));
#48920=CARTESIAN_POINT('Ctrl Pts',(-21.1641051849347,25.7164567020401,16.5827922756422));
#48921=CARTESIAN_POINT('Ctrl Pts',(-21.1701573225114,25.7231038252824,16.5833423559056));
#48922=CARTESIAN_POINT('Ctrl Pts',(-21.1730504359872,25.7262686494441,16.5836050054352));
#48923=CARTESIAN_POINT('Ctrl Pts',(-21.1781890537828,25.7318673889729,16.5840709747375));
#48924=CARTESIAN_POINT('Ctrl Pts',(-21.1804320139563,25.734303639685,16.5842741858061));
#48925=CARTESIAN_POINT('Ctrl Pts',(-21.1848613711635,25.7390998470488,16.5846751307482));
#48926=CARTESIAN_POINT('Ctrl Pts',(-21.1870475553137,25.7414599960242,16.5848728553873));
#48927=CARTESIAN_POINT('Ctrl Pts',(-21.1923137503684,25.7471281985788,16.5853487427258));
#48928=CARTESIAN_POINT('Ctrl Pts',(-21.1953971878599,25.7504330473613,16.5856270524828));
#48929=CARTESIAN_POINT('Ctrl Pts',(-21.2048640331644,25.7605369769652,16.5864805271361));
#48930=CARTESIAN_POINT('Ctrl Pts',(-21.2112699675271,25.767314799568,16.5870566633853));
#48931=CARTESIAN_POINT('Ctrl Pts',(-21.2852088855516,25.8448690250561,16.5936909928919));
#48932=CARTESIAN_POINT('Ctrl Pts',(-21.3558947246034,25.9125560747297,16.5998873210614));
#48933=CARTESIAN_POINT('Ctrl Pts',(-21.6041877538224,26.1295440309248,16.6212151733245));
#48934=CARTESIAN_POINT('Ctrl Pts',(-21.7947785989043,26.2628519286952,16.6369461197535));
#48935=CARTESIAN_POINT('Ctrl Pts',(-22.023487943234,26.3885538358758,16.6545854676908));
#48936=CARTESIAN_POINT('Ctrl Pts',(-22.0491739137977,26.4022214472271,16.6565491544851));
#48937=CARTESIAN_POINT('Ctrl Pts',(-22.075036069343,26.4155368023571,16.6585071611381));
#48938=CARTESIAN_POINT('Origin',(-23.5502525316942,23.5502525316942,-77.3107734492734));
#48939=CARTESIAN_POINT('',(-22.0750359582753,26.4155367451729,18.1566419298442));
#48940=CARTESIAN_POINT('',(-22.075036043603,26.4155367891046,17.9090429972639));
#48941=CARTESIAN_POINT('',(-22.0750360153461,26.4155367745563,-77.3107734492734));
#48942=CARTESIAN_POINT('',(-26.7741131953272,23.5531281751,17.3107734492729));
#48943=CARTESIAN_POINT('Ctrl Pts',(-22.0750359582753,26.4155367451729,18.1566419298442));
#48944=CARTESIAN_POINT('Ctrl Pts',(-21.9853865332552,26.3693799566194,18.1502524745867));
#48945=CARTESIAN_POINT('Ctrl Pts',(-21.8979439411704,26.3190367025206,18.1437182804855));
#48946=CARTESIAN_POINT('Ctrl Pts',(-21.5963525737374,26.1260149599978,18.1201039190352));
#48947=CARTESIAN_POINT('Ctrl Pts',(-21.3971129691064,25.961942231366,18.1023842227795));
#48948=CARTESIAN_POINT('Ctrl Pts',(-21.1502391614448,25.7034156973081,18.0786444313708));
#48949=CARTESIAN_POINT('Ctrl Pts',(-21.0843914208312,25.6276811021549,18.0721070584265));
#48950=CARTESIAN_POINT('Ctrl Pts',(-21.0181042130766,25.5438386420243,18.0654055123364));
#48951=CARTESIAN_POINT('Ctrl Pts',(-21.0140471546462,25.5386747640157,18.0649948414849));
#48952=CARTESIAN_POINT('Ctrl Pts',(-21.008465833625,25.5315259117947,18.0644292176641));
#48953=CARTESIAN_POINT('Ctrl Pts',(-21.0069280926294,25.5295515548174,18.0642733096723));
#48954=CARTESIAN_POINT('Ctrl Pts',(-21.0042964858974,25.5261646165937,18.0640063802929));
#48955=CARTESIAN_POINT('Ctrl Pts',(-21.0032014953747,25.5247529173109,18.0638952783044));
#48956=CARTESIAN_POINT('Ctrl Pts',(-21.0010652377073,25.5219940466406,18.0636784584793));
#48957=CARTESIAN_POINT('Ctrl Pts',(-21.0000238669761,25.5206469640978,18.0635727334399));
#48958=CARTESIAN_POINT('Ctrl Pts',(-20.9975342125294,25.5174211499465,18.0633198961075));
#48959=CARTESIAN_POINT('Ctrl Pts',(-20.9960869314369,25.5155416392266,18.0631728558421));
#48960=CARTESIAN_POINT('Ctrl Pts',(-20.9916883177115,25.5098163163054,18.0627257744343));
#48961=CARTESIAN_POINT('Ctrl Pts',(-20.9887435688603,25.5059654188744,18.0624262009121));
#48962=CARTESIAN_POINT('Ctrl Pts',(-20.9602376984585,25.4685129823811,18.0595235176891));
#48963=CARTESIAN_POINT('Ctrl Pts',(-20.935328999713,25.4344168919973,18.0569656526082));
#48964=CARTESIAN_POINT('Ctrl Pts',(-20.8625306830649,25.3305417116966,18.0493912469974));
#48965=CARTESIAN_POINT('Ctrl Pts',(-20.8167095540322,25.2593526855464,18.0444876241887));
#48966=CARTESIAN_POINT('Ctrl Pts',(-20.6797538339028,25.0269466652182,18.0291012268428));
#48967=CARTESIAN_POINT('Ctrl Pts',(-20.5996812653384,24.8596503216587,18.0189194005167));
#48968=CARTESIAN_POINT('Ctrl Pts',(-20.4656278811494,24.5038129862667,17.9974883183425));
#48969=CARTESIAN_POINT('Ctrl Pts',(-20.4135760583289,24.3153866415243,17.9862465660744));
#48970=CARTESIAN_POINT('Ctrl Pts',(-20.3766117710329,24.1108637077341,17.9736185105692));
#48971=CARTESIAN_POINT('Ctrl Pts',(-20.3744157637794,24.0982866407056,17.9728404249817));
#48972=CARTESIAN_POINT('Ctrl Pts',(-20.371522774628,24.0811162365012,17.9717759858902));
#48973=CARTESIAN_POINT('Ctrl Pts',(-20.370760884531,24.0765338317529,17.9714916986339));
#48974=CARTESIAN_POINT('Ctrl Pts',(-20.3694826064335,24.0687415048657,17.9710079057921));
#48975=CARTESIAN_POINT('Ctrl Pts',(-20.3689611617789,24.0655324093624,17.9708085612173));
#48976=CARTESIAN_POINT('Ctrl Pts',(-20.3679632076025,24.0593315022743,17.9704231638871));
#48977=CARTESIAN_POINT('Ctrl Pts',(-20.3674860588078,24.0563397963894,17.9702371317124));
#48978=CARTESIAN_POINT('Ctrl Pts',(-20.3663656842612,24.04925083482,17.9697961005106));
#48979=CARTESIAN_POINT('Ctrl Pts',(-20.3657261491367,24.0451530088802,17.9695409845249));
#48980=CARTESIAN_POINT('Ctrl Pts',(-20.3638693176157,24.0331027146917,17.9687902565791));
#48981=CARTESIAN_POINT('Ctrl Pts',(-20.3626738937624,24.0251469529094,17.9682939510579));
#48982=CARTESIAN_POINT('Ctrl Pts',(-20.3539714746155,23.9657172053102,17.9645814627081));
#48983=CARTESIAN_POINT('Ctrl Pts',(-20.3476823110469,23.9140752378386,17.9613268812482));
#48984=CARTESIAN_POINT('Ctrl Pts',(-20.3309580353865,23.7421659362329,17.950389430731));
#48985=CARTESIAN_POINT('Ctrl Pts',(-20.3260303021233,23.6214776604979,17.9425389830137));
#48986=CARTESIAN_POINT('Ctrl Pts',(-20.330999400122,23.2976302996741,17.9210562763047));
#48987=CARTESIAN_POINT('Ctrl Pts',(-20.3533268589019,23.0952077731006,17.907162137017));
#48988=CARTESIAN_POINT('Ctrl Pts',(-20.4128509865743,22.8079893030754,17.8874748037311));
#48989=CARTESIAN_POINT('Ctrl Pts',(-20.4348403588532,22.7205220738277,17.8814897982656));
#48990=CARTESIAN_POINT('Ctrl Pts',(-20.4607783097774,22.6330460275923,17.8755852394988));
#48991=CARTESIAN_POINT('Ctrl Pts',(-20.4610871922827,22.6320062440132,17.8755150668739));
#48992=CARTESIAN_POINT('Ctrl Pts',(-20.4622631571238,22.6280549314678,17.8752484474633));
#48993=CARTESIAN_POINT('Ctrl Pts',(-20.4631338340247,22.6251444634327,17.875052154516));
#48994=CARTESIAN_POINT('Ctrl Pts',(-20.4644504044655,22.6207660348791,17.8747570030792));
#48995=CARTESIAN_POINT('Ctrl Pts',(-20.4648932305682,22.6192971626541,17.8746580106796));
#48996=CARTESIAN_POINT('Ctrl Pts',(-20.4660956504074,22.6153189684004,17.8743899745764));
#48997=CARTESIAN_POINT('Ctrl Pts',(-20.4668572592981,22.6128102505805,17.8742210199547));
#48998=CARTESIAN_POINT('Ctrl Pts',(-20.4791059581997,22.5726398042475,17.8715168697231));
#48999=CARTESIAN_POINT('Ctrl Pts',(-20.4912799107272,22.5351886048407,17.869012773425));
#49000=CARTESIAN_POINT('Ctrl Pts',(-20.5056968113425,22.493455094257,17.8662488482477));
#49001=CARTESIAN_POINT('Ctrl Pts',(-20.5072657996468,22.488945739395,17.8659505527941));
#49002=CARTESIAN_POINT('Ctrl Pts',(-20.5096421177249,22.4821646677413,17.8655025273824));
#49003=CARTESIAN_POINT('Ctrl Pts',(-20.5104419761549,22.4798903681314,17.8653523567964));
#49004=CARTESIAN_POINT('Ctrl Pts',(-20.5118309609554,22.4759550743302,17.8650926744561));
#49005=CARTESIAN_POINT('Ctrl Pts',(-20.5124188976409,22.47429366618,17.8649830916152));
#49006=CARTESIAN_POINT('Ctrl Pts',(-20.5136460132842,22.4708350715534,17.8647550761786));
#49007=CARTESIAN_POINT('Ctrl Pts',(-20.5142854242678,22.4690379722521,17.864636658223));
#49008=CARTESIAN_POINT('Ctrl Pts',(-20.5155610692619,22.465462756293,17.8644011902862));
#49009=CARTESIAN_POINT('Ctrl Pts',(-20.5161972722307,22.4636846269866,17.8642841382821));
#49010=CARTESIAN_POINT('Ctrl Pts',(-20.5183870341317,22.4575813609004,17.8638825627961));
#49011=CARTESIAN_POINT('Ctrl Pts',(-20.5199482908632,22.4532589622432,17.8635984988085));
#49012=CARTESIAN_POINT('Ctrl Pts',(-20.5327980874533,22.4179205753246,17.861278730786));
#49013=CARTESIAN_POINT('Ctrl Pts',(-20.5445537828858,22.3870748920817,17.8592705235968));
#49014=CARTESIAN_POINT('Ctrl Pts',(-20.5882986686502,22.2773875189196,17.8521706846177));
#49015=CARTESIAN_POINT('Ctrl Pts',(-20.6229352717839,22.1996333647415,17.8472147400845));
#49016=CARTESIAN_POINT('Ctrl Pts',(-20.726317313881,21.9902750655033,17.8338475489804));
#49017=CARTESIAN_POINT('Ctrl Pts',(-20.8011379487566,21.8619063619264,17.8256192126946));
#49018=CARTESIAN_POINT('Ctrl Pts',(-20.9480701938823,21.6456413675228,17.8109895203003));
#49019=CARTESIAN_POINT('Ctrl Pts',(-21.0164715552259,21.5555473988262,17.8046318458246));
#49020=CARTESIAN_POINT('Ctrl Pts',(-21.096159377385,21.4613169320937,17.7975381381758));
#49021=CARTESIAN_POINT('Ctrl Pts',(-21.1028952704148,21.453429319724,17.7969408107351));
#49022=CARTESIAN_POINT('Ctrl Pts',(-21.1883104503336,21.3543819297502,17.7893940243236));
#49023=CARTESIAN_POINT('Ctrl Pts',(-21.2719924370995,21.2676785876644,17.7822893538589));
#49024=CARTESIAN_POINT('Ctrl Pts',(-21.3681564369958,21.1786100137202,17.77431394968));
#49025=CARTESIAN_POINT('Ctrl Pts',(-21.3760269436794,21.1713925762382,17.7736625415275));
#49026=CARTESIAN_POINT('Ctrl Pts',(-21.3871200056261,21.1613210204344,17.7727462205949));
#49027=CARTESIAN_POINT('Ctrl Pts',(-21.3903126898197,21.1584339829715,17.7724827031413));
#49028=CARTESIAN_POINT('Ctrl Pts',(-21.3958593033952,21.1534385283207,17.7720252527943));
#49029=CARTESIAN_POINT('Ctrl Pts',(-21.3982105735938,21.1513271557445,17.7718314448803));
#49030=CARTESIAN_POINT('Ctrl Pts',(-21.403105695686,21.1469444662964,17.7714281820327));
#49031=CARTESIAN_POINT('Ctrl Pts',(-21.4056500535295,21.1446737233623,17.7712187033576));
#49032=CARTESIAN_POINT('Ctrl Pts',(-21.4116433980227,21.1393419565592,17.7707255625168));
#49033=CARTESIAN_POINT('Ctrl Pts',(-21.4150953531824,21.1362842944099,17.7704417599226));
#49034=CARTESIAN_POINT('Ctrl Pts',(-21.4263754784265,21.1263357447834,17.7695151004359));
#49035=CARTESIAN_POINT('Ctrl Pts',(-21.4342304760902,21.1194754988592,17.7688709666022));
#49036=CARTESIAN_POINT('Ctrl Pts',(-21.4526488296631,21.1035465633013,17.7673632110331));
#49037=CARTESIAN_POINT('Ctrl Pts',(-21.4632378645824,21.0945080099667,17.7664983558942));
#49038=CARTESIAN_POINT('Ctrl Pts',(-21.499969069993,21.0635642654826,17.7635049208441));
#49039=CARTESIAN_POINT('Ctrl Pts',(-21.5263994779672,21.0420062360684,17.7613622961688));
#49040=CARTESIAN_POINT('Ctrl Pts',(-21.6470748142823,20.946726347749,17.7516271211319));
#49041=CARTESIAN_POINT('Ctrl Pts',(-21.7450291454913,20.877875897007,17.743848130787));
#49042=CARTESIAN_POINT('Ctrl Pts',(-21.9931448464149,20.723355258478,17.72446837006));
#49043=CARTESIAN_POINT('Ctrl Pts',(-22.146807418224,20.6440062475546,17.7127222203497));
#49044=CARTESIAN_POINT('Ctrl Pts',(-22.4570544134878,20.5141656499843,17.6900179993355));
#49045=CARTESIAN_POINT('Ctrl Pts',(-22.6126521882927,20.4625631410496,17.6790882517949));
#49046=CARTESIAN_POINT('Ctrl Pts',(-22.78075895697,20.4207017756407,17.6681917199969));
#49047=CARTESIAN_POINT('Ctrl Pts',(-22.7900124118544,20.4184410332337,17.6675948125554));
#49048=CARTESIAN_POINT('Ctrl Pts',(-22.8024328705745,20.4154648425978,17.6667976146599));
#49049=CARTESIAN_POINT('Ctrl Pts',(-22.8055910068597,20.4147131339317,17.6665952583028));
#49050=CARTESIAN_POINT('Ctrl Pts',(-22.8105360492825,20.4135439932198,17.6662789543104));
#49051=CARTESIAN_POINT('Ctrl Pts',(-22.8123221740602,20.4131233158326,17.6661648186313));
#49052=CARTESIAN_POINT('Ctrl Pts',(-22.815750243044,20.4123190088805,17.6659459763011));
#49053=CARTESIAN_POINT('Ctrl Pts',(-22.8173921184103,20.4119351448947,17.665841256731));
#49054=CARTESIAN_POINT('Ctrl Pts',(-22.8207816844031,20.4111454827867,17.665625264136));
#49055=CARTESIAN_POINT('Ctrl Pts',(-22.8225294074149,20.4107398567755,17.6655140014579));
#49056=CARTESIAN_POINT('Ctrl Pts',(-22.8264725579163,20.4098281673713,17.665263214239));
#49057=CARTESIAN_POINT('Ctrl Pts',(-22.8286681820471,20.4093229455853,17.6651237384707));
#49058=CARTESIAN_POINT('Ctrl Pts',(-22.8389579928719,20.4069665784305,17.6644708610754));
#49059=CARTESIAN_POINT('Ctrl Pts',(-22.8470588816145,20.4051443938036,17.6639591201188));
#49060=CARTESIAN_POINT('Ctrl Pts',(-22.9378473154056,20.3850910835219,17.658248196046));
#49061=CARTESIAN_POINT('Ctrl Pts',(-23.0212240069743,20.370092335886,17.6532284906616));
#49062=CARTESIAN_POINT('Ctrl Pts',(-23.2409821432845,20.3394439554974,17.6403559575622));
#49063=CARTESIAN_POINT('Ctrl Pts',(-23.3779422902423,20.3291884121211,17.6326858849033));
#49064=CARTESIAN_POINT('Ctrl Pts',(-23.7890621172635,20.324709781385,17.6097100754186));
#49065=CARTESIAN_POINT('Ctrl Pts',(-24.0621947075556,20.3566581345049,17.5944018402668));
#49066=CARTESIAN_POINT('Ctrl Pts',(-24.3451851097992,20.4270308070112,17.5767389446504));
#49067=CARTESIAN_POINT('Ctrl Pts',(-24.3623505723028,20.4314501176043,17.5756608323302));
#49068=CARTESIAN_POINT('Ctrl Pts',(-24.3851933379854,20.4375324369718,17.5742168754131));
#49069=CARTESIAN_POINT('Ctrl Pts',(-24.3909040035974,20.4390698562235,17.5738551125578));
#49070=CARTESIAN_POINT('Ctrl Pts',(-24.3998075174263,20.4414931541219,17.5732898656764));
#49071=CARTESIAN_POINT('Ctrl Pts',(-24.4030033063273,20.4423682581639,17.5730867324745));
#49072=CARTESIAN_POINT('Ctrl Pts',(-24.4091053214691,20.4440492956363,17.572698399261));
#49073=CARTESIAN_POINT('Ctrl Pts',(-24.4120117788116,20.4448543836125,17.5725132269617));
#49074=CARTESIAN_POINT('Ctrl Pts',(-24.4187920126221,20.4467427585085,17.5720807734642));
#49075=CARTESIAN_POINT('Ctrl Pts',(-24.4226648933597,20.4478292186741,17.5718333890171));
#49076=CARTESIAN_POINT('Ctrl Pts',(-24.4337099433469,20.4509500064635,17.5711268231215));
#49077=CARTESIAN_POINT('Ctrl Pts',(-24.4408770663861,20.4530019642048,17.5706670666924));
#49078=CARTESIAN_POINT('Ctrl Pts',(-24.485508997073,20.4659478778045,17.5677960426716));
#49079=CARTESIAN_POINT('Ctrl Pts',(-24.5227791604296,20.4774961803814,17.5653634349968));
#49080=CARTESIAN_POINT('Ctrl Pts',(-24.6327200385592,20.5137623098223,17.5580790782686));
#49081=CARTESIAN_POINT('Ctrl Pts',(-24.7047232213128,20.540401270972,17.5531652266081));
#49082=CARTESIAN_POINT('Ctrl Pts',(-24.8812651598506,20.6129833870207,17.5407538642089));
#49083=CARTESIAN_POINT('Ctrl Pts',(-24.9844390086464,20.6619572188259,17.533170363488));
#49084=CARTESIAN_POINT('Ctrl Pts',(-25.1703845264907,20.7626434619606,17.5189534929859));
#49085=CARTESIAN_POINT('Ctrl Pts',(-25.2538335988041,20.8128444649431,17.5123524518107));
#49086=CARTESIAN_POINT('Ctrl Pts',(-25.4504856959374,20.9436250804692,17.4963805482037));
#49087=CARTESIAN_POINT('Ctrl Pts',(-25.5610119001646,21.027903213778,17.4870416528789));
#49088=CARTESIAN_POINT('Ctrl Pts',(-25.6667271801104,21.1198916013487,17.4779683457058));
#49089=CARTESIAN_POINT('Ctrl Pts',(-25.6676888268072,21.1207293839784,17.4778857978256));
#49090=CARTESIAN_POINT('Ctrl Pts',(-25.6764436462157,21.1283656927844,17.477134176601));
#49091=CARTESIAN_POINT('Ctrl Pts',(-25.6842046508822,21.1352012124491,17.4764671083267));
#49092=CARTESIAN_POINT('Ctrl Pts',(-25.7196162637281,21.1666940401315,17.4734204263193));
#49093=CARTESIAN_POINT('Ctrl Pts',(-25.7468747290597,21.1917908930872,17.4710667313149));
#49094=CARTESIAN_POINT('Ctrl Pts',(-25.7774201488496,21.2209031721931,17.4684256094629));
#49095=CARTESIAN_POINT('Ctrl Pts',(-25.7811360593238,21.2244617585294,17.4681042500663));
#49096=CARTESIAN_POINT('Ctrl Pts',(-25.7866110343877,21.2297301277515,17.4676306938716));
#49097=CARTESIAN_POINT('Ctrl Pts',(-25.7883766709034,21.2314330222551,17.4674779650133));
#49098=CARTESIAN_POINT('Ctrl Pts',(-25.7914968601221,21.2344492191657,17.4672080502637));
#49099=CARTESIAN_POINT('Ctrl Pts',(-25.7928522047507,21.2357616960006,17.4670907996523));
#49100=CARTESIAN_POINT('Ctrl Pts',(-25.7956778556885,21.2385027875506,17.4668463430857));
#49101=CARTESIAN_POINT('Ctrl Pts',(-25.7971479485206,21.2399316121933,17.4667191544568));
#49102=CARTESIAN_POINT('Ctrl Pts',(-25.8001270856233,21.2428326525475,17.4664613926171));
#49103=CARTESIAN_POINT('Ctrl Pts',(-25.8016360508921,21.2443049484555,17.466330825827));
#49104=CARTESIAN_POINT('Ctrl Pts',(-25.8053486611656,21.2479344565997,17.466009561327));
#49105=CARTESIAN_POINT('Ctrl Pts',(-25.807550662358,21.2500933586037,17.4658189956201));
#49106=CARTESIAN_POINT('Ctrl Pts',(-25.8279328235101,21.2701340421791,17.4640548638619));
#49107=CARTESIAN_POINT('Ctrl Pts',(-25.8459039194147,21.2882285172376,17.462497808267));
#49108=CARTESIAN_POINT('Ctrl Pts',(-25.939113719498,21.3843333788518,17.4544008172419));
#49109=CARTESIAN_POINT('Ctrl Pts',(-26.0106042154937,21.4658969714548,17.448116204365));
#49110=CARTESIAN_POINT('Ctrl Pts',(-26.1014921883155,21.5807994355283,17.4397792577676));
#49111=CARTESIAN_POINT('Ctrl Pts',(-26.1245982785293,21.6110997879473,17.4376261707485));
#49112=CARTESIAN_POINT('Ctrl Pts',(-26.1715372244686,21.6749716422224,17.4331656572905));
#49113=CARTESIAN_POINT('Ctrl Pts',(-26.1952749820359,21.7086043135896,17.430860134811));
#49114=CARTESIAN_POINT('Ctrl Pts',(-26.2768363928449,21.8289951229054,17.4227274554058));
#49115=CARTESIAN_POINT('Ctrl Pts',(-26.3310873937282,21.9180933376937,17.4169219001377));
#49116=CARTESIAN_POINT('Ctrl Pts',(-26.4720715730959,22.1771368796409,17.4002825862503));
#49117=CARTESIAN_POINT('Ctrl Pts',(-26.5481633465448,22.3523429349545,17.3892800956125));
#49118=CARTESIAN_POINT('Ctrl Pts',(-26.6123038599256,22.5452060091682,17.3769295735889));
#49119=CARTESIAN_POINT('Ctrl Pts',(-26.6162162774602,22.5572051251165,17.376160367814));
#49120=CARTESIAN_POINT('Ctrl Pts',(-26.6214652804226,22.5736301968753,17.3751062318943));
#49121=CARTESIAN_POINT('Ctrl Pts',(-26.6228630096105,22.5780366176833,17.3748233166947));
#49122=CARTESIAN_POINT('Ctrl Pts',(-26.6252257362638,22.5855412361682,17.3743412749088));
#49123=CARTESIAN_POINT('Ctrl Pts',(-26.626195547031,22.5886379213526,17.3741423068719));
#49124=CARTESIAN_POINT('Ctrl Pts',(-26.628062267765,22.5946302317464,17.3737571718536));
#49125=CARTESIAN_POINT('Ctrl Pts',(-26.6289597727228,22.5975256686586,17.3735710247027));
#49126=CARTESIAN_POINT('Ctrl Pts',(-26.6310797574491,22.6043992198992,17.3731289975566));
#49127=CARTESIAN_POINT('Ctrl Pts',(-26.6322986170293,22.6083784371368,17.3728729990347));
#49128=CARTESIAN_POINT('Ctrl Pts',(-26.6358710180386,22.6201224597623,17.3721171550486));
#49129=CARTESIAN_POINT('Ctrl Pts',(-26.6382029348119,22.6278937620511,17.3716166015833));
#49130=CARTESIAN_POINT('Ctrl Pts',(-26.6434009856207,22.6454573571574,17.3704844005209));
#49131=CARTESIAN_POINT('Ctrl Pts',(-26.6462500027706,22.6552545869331,17.3698521976048));
#49132=CARTESIAN_POINT('Ctrl Pts',(-26.6552224627898,22.6866647231777,17.3678231934226));
#49133=CARTESIAN_POINT('Ctrl Pts',(-26.6611663707847,22.708327819782,17.3664205673953));
#49134=CARTESIAN_POINT('Ctrl Pts',(-26.7375947597152,22.9987430515741,17.3475705571188));
#49135=CARTESIAN_POINT('Ctrl Pts',(-26.7732452352441,23.275386012713,17.3289302935924));
#49136=CARTESIAN_POINT('Ctrl Pts',(-26.7730012882014,23.5530835971147,17.3101346383694));
#49137=CARTESIAN_POINT('Ctrl Pts',(-22.0738786772418,26.4178312615861,16.9038400528878));
#49138=CARTESIAN_POINT('Ctrl Pts',(-22.8848601554831,26.8257766505266,16.9600102888025));
#49139=CARTESIAN_POINT('Ctrl Pts',(-25.0566874879774,26.9584629849414,17.0824761618423));
#49140=CARTESIAN_POINT('Ctrl Pts',(-26.6594709648069,25.0501006738249,17.218120627304));
#49141=CARTESIAN_POINT('Ctrl Pts',(-26.7760869353403,23.7663575325862,17.2975948568509));
#49142=CARTESIAN_POINT('Ctrl Pts',(-26.7741131953272,23.5531281751,17.3107734492729));
#49143=CARTESIAN_POINT('Ctrl Pts',(-22.075036069343,26.4155368023571,16.6585071611381));
#49144=CARTESIAN_POINT('Ctrl Pts',(-22.203393445971,26.4816227111811,16.6682250130379));
#49145=CARTESIAN_POINT('Ctrl Pts',(-22.3360903487222,26.5390313531522,16.6778097090526));
#49146=CARTESIAN_POINT('Ctrl Pts',(-22.4821328897951,26.5908689608885,16.6875644177171));
#49147=CARTESIAN_POINT('Ctrl Pts',(-22.4920464967325,26.5943333180319,16.6882227385446));
#49148=CARTESIAN_POINT('Ctrl Pts',(-22.505044801427,26.5988044646475,16.6890807117283));
#49149=CARTESIAN_POINT('Ctrl Pts',(-22.5081141880536,26.5998550894481,16.6892829336088));
#49150=CARTESIAN_POINT('Ctrl Pts',(-22.5131144720326,26.6015582131558,16.6896117489145));
#49151=CARTESIAN_POINT('Ctrl Pts',(-22.5150444014581,26.6022135150076,16.6897385093671));
#49152=CARTESIAN_POINT('Ctrl Pts',(-22.5187661564798,26.6034732895566,16.6899826677612));
#49153=CARTESIAN_POINT('Ctrl Pts',(-22.520557887755,26.6040780143883,16.6901000803396));
#49154=CARTESIAN_POINT('Ctrl Pts',(-22.5247005673667,26.6054721442679,16.6903712515863));
#49155=CARTESIAN_POINT('Ctrl Pts',(-22.5270519018028,26.6062604151395,16.6905249423718));
#49156=CARTESIAN_POINT('Ctrl Pts',(-22.5344107843417,26.6087179915011,16.6910052530175));
#49157=CARTESIAN_POINT('Ctrl Pts',(-22.5394215577847,26.6103777199208,16.691331305525));
#49158=CARTESIAN_POINT('Ctrl Pts',(-22.5829446231347,26.6246753852068,16.6941548916166));
#49159=CARTESIAN_POINT('Ctrl Pts',(-22.6216902456656,26.6365987414654,16.6966110253976));
#49160=CARTESIAN_POINT('Ctrl Pts',(-22.6673420324709,26.6497097505165,16.699449181005));
#49161=CARTESIAN_POINT('Ctrl Pts',(-22.6740376593446,26.6516092509473,16.6998640504444));
#49162=CARTESIAN_POINT('Ctrl Pts',(-22.6844324151706,26.6545218172238,16.7005060350336));
#49163=CARTESIAN_POINT('Ctrl Pts',(-22.6881272478295,26.6555499838628,16.7007338211858));
#49164=CARTESIAN_POINT('Ctrl Pts',(-22.6976219044861,26.658173824116,16.7013181385336));
#49165=CARTESIAN_POINT('Ctrl Pts',(-22.703424399568,26.6597598659795,16.7016742503375));
#49166=CARTESIAN_POINT('Ctrl Pts',(-22.709830556491,26.6614916500195,16.7020663600588));
#49167=CARTESIAN_POINT('Ctrl Pts',(-22.7104298192741,26.6616534636702,16.7021030297633));
#49168=CARTESIAN_POINT('Ctrl Pts',(-22.7171976109482,26.6634788131658,16.7025170461531));
#49169=CARTESIAN_POINT('Ctrl Pts',(-22.7233710713558,26.6651241875254,16.7028936354194));
#49170=CARTESIAN_POINT('Ctrl Pts',(-22.7420979277533,26.6700557439983,16.7040328723909));
#49171=CARTESIAN_POINT('Ctrl Pts',(-22.7546664385469,26.6732845079295,16.7047932191728));
#49172=CARTESIAN_POINT('Ctrl Pts',(-22.9367178240878,26.7188819144376,16.7157497062546));
#49173=CARTESIAN_POINT('Ctrl Pts',(-23.1093662734825,26.7474804626039,16.7254405211916));
#49174=CARTESIAN_POINT('Ctrl Pts',(-23.4312041113768,26.7742118812468,16.7434931444036));
#49175=CARTESIAN_POINT('Ctrl Pts',(-23.5795773170386,26.7762751801357,16.7518113925727));
#49176=CARTESIAN_POINT('Ctrl Pts',(-23.8272576200464,26.7626279937179,16.7661874766666));
#49177=CARTESIAN_POINT('Ctrl Pts',(-23.9266400805841,26.7525044439856,16.7720868025484));
#49178=CARTESIAN_POINT('Ctrl Pts',(-24.0370510660604,26.7360466014992,16.7788495708175));
#49179=CARTESIAN_POINT('Ctrl Pts',(-24.0487067366648,26.7342437484007,16.7795660786807));
#49180=CARTESIAN_POINT('Ctrl Pts',(-24.0666223172816,26.7313718523986,16.7806714832075));
#49181=CARTESIAN_POINT('Ctrl Pts',(-24.0728894852024,26.7303482066616,16.7810589418499));
#49182=CARTESIAN_POINT('Ctrl Pts',(-24.0832266041961,26.7286284140417,16.7816993053104));
#49183=CARTESIAN_POINT('Ctrl Pts',(-24.0872983355942,26.7279429533228,16.7819518703907));
#49184=CARTESIAN_POINT('Ctrl Pts',(-24.0951853648166,26.7265996095837,16.7824417377792));
#49185=CARTESIAN_POINT('Ctrl Pts',(-24.0990008183009,26.7259426723673,16.7826790096245));
#49186=CARTESIAN_POINT('Ctrl Pts',(-24.1059027251022,26.7247415059167,16.7831087510774));
#49187=CARTESIAN_POINT('Ctrl Pts',(-24.1089895905496,26.7241996459114,16.7833011449433));
#49188=CARTESIAN_POINT('Ctrl Pts',(-24.1154124768224,26.7230625295216,16.7837018650197));
#49189=CARTESIAN_POINT('Ctrl Pts',(-24.1187483573803,26.7224665128009,16.7839102152615));
#49190=CARTESIAN_POINT('Ctrl Pts',(-24.128270500228,26.7207497035339,16.7845055936798));
#49191=CARTESIAN_POINT('Ctrl Pts',(-24.1344544059581,26.7196160731329,16.7848930311963));
#49192=CARTESIAN_POINT('Ctrl Pts',(-24.1609506111018,26.7146786214358,16.7865564827146));
#49193=CARTESIAN_POINT('Ctrl Pts',(-24.1812290262424,26.7106976353016,16.7878381460078));
#49194=CARTESIAN_POINT('Ctrl Pts',(-24.5386775994443,26.6369473353225,16.81058556711));
#49195=CARTESIAN_POINT('Ctrl Pts',(-24.862495103852,26.5137914170664,16.8340027861256));
#49196=CARTESIAN_POINT('Ctrl Pts',(-25.2916157992142,26.2662521184879,16.8673558209928));
#49197=CARTESIAN_POINT('Ctrl Pts',(-25.4171817976899,26.181523656607,16.8773946094422));
#49198=CARTESIAN_POINT('Ctrl Pts',(-25.541166820741,26.0845010108741,16.8872593990503));
#49199=CARTESIAN_POINT('Ctrl Pts',(-25.5459786129662,26.0807134522688,16.8876421552228));
#49200=CARTESIAN_POINT('Ctrl Pts',(-25.5528364703138,26.0752836233906,16.8881875004019));
#49201=CARTESIAN_POINT('Ctrl Pts',(-25.5548913327615,26.0736525639173,16.8883508841691));
#49202=CARTESIAN_POINT('Ctrl Pts',(-25.5584371401185,26.0708309933106,16.8886327737449));
#49203=CARTESIAN_POINT('Ctrl Pts',(-25.5599290215553,26.0696416657602,16.8887513650174));
#49204=CARTESIAN_POINT('Ctrl Pts',(-25.5627966392919,26.0673514336195,16.8889792898488));
#49205=CARTESIAN_POINT('Ctrl Pts',(-25.5641725262492,26.0662507277723,16.8890886374592));
#49206=CARTESIAN_POINT('Ctrl Pts',(-25.5674274998922,26.0636423769247,16.889347299826));
#49207=CARTESIAN_POINT('Ctrl Pts',(-25.5693058033178,26.0621337495998,16.8894965434142));
#49208=CARTESIAN_POINT('Ctrl Pts',(-25.5748960718123,26.0576334016326,16.8899406758766));
#49209=CARTESIAN_POINT('Ctrl Pts',(-25.5786031128428,26.0546355319797,16.8902351233657));
#49210=CARTESIAN_POINT('Ctrl Pts',(-25.6127034566538,26.0269333342815,16.8929432098302));
#49211=CARTESIAN_POINT('Ctrl Pts',(-25.6426523481806,26.001683738597,16.8953181015725));
#49212=CARTESIAN_POINT('Ctrl Pts',(-25.6762951083699,25.9722539918827,16.8979917156576));
#49213=CARTESIAN_POINT('Ctrl Pts',(-25.6804457815069,25.9686042079968,16.8983216754071));
#49214=CARTESIAN_POINT('Ctrl Pts',(-25.9066958234451,25.7686228282329,16.9163144806829));
#49215=CARTESIAN_POINT('Ctrl Pts',(-26.100684783078,25.5425722949492,16.9322195447708));
#49216=CARTESIAN_POINT('Ctrl Pts',(-26.326384589936,25.1915337933888,16.9559171470612));
#49217=CARTESIAN_POINT('Ctrl Pts',(-26.3859499603648,25.0863284095013,16.9628952520117));
#49218=CARTESIAN_POINT('Ctrl Pts',(-26.4625494529594,24.9313241960944,16.9731825732099));
#49219=CARTESIAN_POINT('Ctrl Pts',(-26.4844955586872,24.8840627428085,16.9763192104321));
#49220=CARTESIAN_POINT('Ctrl Pts',(-26.508483182764,24.8289445154798,16.9799845001277));
#49221=CARTESIAN_POINT('Ctrl Pts',(-26.5116534261184,24.8215851062008,16.9804740331189));
#49222=CARTESIAN_POINT('Ctrl Pts',(-26.5164202373603,24.8104048445706,16.9812179636424));
#49223=CARTESIAN_POINT('Ctrl Pts',(-26.51803695876,24.8065925748335,16.9814716732277));
#49224=CARTESIAN_POINT('Ctrl Pts',(-26.5208234869384,24.7999864778937,16.9819113919028));
#49225=CARTESIAN_POINT('Ctrl Pts',(-26.5219967136411,24.7971940914264,16.9820972842513));
#49226=CARTESIAN_POINT('Ctrl Pts',(-26.5244223507065,24.7913979869309,16.9824831890764));
#49227=CARTESIAN_POINT('Ctrl Pts',(-26.5256741508472,24.7883940185744,16.9826832220561));
#49228=CARTESIAN_POINT('Ctrl Pts',(-26.5290746197132,24.7801989106864,16.9832290118291));
#49229=CARTESIAN_POINT('Ctrl Pts',(-26.5312142598612,24.7750040582621,16.9835750747256));
#49230=CARTESIAN_POINT('Ctrl Pts',(-26.539257206653,24.7553305771579,16.9848860074838));
#49231=CARTESIAN_POINT('Ctrl Pts',(-26.545068626038,24.7408148315268,16.9858539830078));
#49232=CARTESIAN_POINT('Ctrl Pts',(-26.6374030443426,24.5052279045971,17.0015773089992));
#49233=CARTESIAN_POINT('Ctrl Pts',(-26.6993261250103,24.2753510642032,17.0171925038953));
#49234=CARTESIAN_POINT('Ctrl Pts',(-26.7605361386873,23.8779128292599,17.0443129103014));
#49235=CARTESIAN_POINT('Ctrl Pts',(-26.7730913015098,23.7133304407264,17.0555543233618));
#49236=CARTESIAN_POINT('Ctrl Pts',(-26.7729828646908,23.5130563265239,17.0688456133548));
#49237=CARTESIAN_POINT('Ctrl Pts',(-26.7723787071759,23.4776066007037,17.0711828109468));
#49238=CARTESIAN_POINT('Ctrl Pts',(-26.7709592611565,23.4353049460033,17.0739481510603));
#49239=CARTESIAN_POINT('Ctrl Pts',(-26.7707068361009,23.4284376748799,17.0743963336792));
#49240=CARTESIAN_POINT('Ctrl Pts',(-26.7704043778455,23.42086882187,17.0748894476697));
#49241=CARTESIAN_POINT('Ctrl Pts',(-26.7703760798166,23.4201664391476,17.0749352000718));
#49242=CARTESIAN_POINT('Ctrl Pts',(-26.7700668842762,23.4125538487842,17.0754309869418));
#49243=CARTESIAN_POINT('Ctrl Pts',(-26.7697639713918,23.4056444974206,17.0758801834118));
#49244=CARTESIAN_POINT('Ctrl Pts',(-26.7692581165855,23.394896877251,17.076577634149));
#49245=CARTESIAN_POINT('Ctrl Pts',(-26.7690705474334,23.3910579439773,17.0768265013508));
#49246=CARTESIAN_POINT('Ctrl Pts',(-26.7686766104764,23.3832807867885,17.0773301446878));
#49247=CARTESIAN_POINT('Ctrl Pts',(-26.7684698806755,23.3793425860954,17.077584905576));
#49248=CARTESIAN_POINT('Ctrl Pts',(-26.768181083878,23.374027396544,17.0779283645859));
#49249=CARTESIAN_POINT('Ctrl Pts',(-26.7681053617023,23.3726500833997,17.0780173300082));
#49250=CARTESIAN_POINT('Ctrl Pts',(-26.7677543190166,23.3663388832228,17.0784248336488));
#49251=CARTESIAN_POINT('Ctrl Pts',(-26.767468533422,23.3614055556319,17.0787429261173));
#49252=CARTESIAN_POINT('Ctrl Pts',(-26.7649726004756,23.3199707948098,17.0814107300028));
#49253=CARTESIAN_POINT('Ctrl Pts',(-26.7621525620342,23.2835068149709,17.0837334805551));
#49254=CARTESIAN_POINT('Ctrl Pts',(-26.7582725994224,23.2424430798982,17.0863150844098));
#49255=CARTESIAN_POINT('Ctrl Pts',(-26.7578227522447,23.2377902228413,17.0866071055414));
#49256=CARTESIAN_POINT('Ctrl Pts',(-26.7571280613425,23.2307645195658,17.0870472847863));
#49257=CARTESIAN_POINT('Ctrl Pts',(-26.7568907065372,23.2283909647421,17.0871958623471));
#49258=CARTESIAN_POINT('Ctrl Pts',(-26.7564740594076,23.224270690389,17.0874535475621));
#49259=CARTESIAN_POINT('Ctrl Pts',(-26.7562959748801,23.2225238541687,17.0875627237091));
#49260=CARTESIAN_POINT('Ctrl Pts',(-26.7559209092336,23.2188743873842,17.0877906605835));
#49261=CARTESIAN_POINT('Ctrl Pts',(-26.7557236620015,23.216971788072,17.0879094055793));
#49262=CARTESIAN_POINT('Ctrl Pts',(-26.7552490795484,23.2124334756641,17.0881924459315));
#49263=CARTESIAN_POINT('Ctrl Pts',(-26.7549701859103,23.209797919079,17.0883566526268));
#49264=CARTESIAN_POINT('Ctrl Pts',(-26.7540197228722,23.2009206595064,17.0889091987368));
#49265=CARTESIAN_POINT('Ctrl Pts',(-26.753333161597,23.1946805247733,17.0892966931835));
#49266=CARTESIAN_POINT('Ctrl Pts',(-26.7395253105707,23.0724674594848,17.0968686484191));
#49267=CARTESIAN_POINT('Ctrl Pts',(-26.7201300397475,22.9572744117898,17.1037043248199));
#49268=CARTESIAN_POINT('Ctrl Pts',(-26.6211092682994,22.5168192196363,17.1295373365877));
#49269=CARTESIAN_POINT('Ctrl Pts',(-26.4972804191143,22.2037046951988,17.147481641968));
#49270=CARTESIAN_POINT('Ctrl Pts',(-26.3253791337552,21.9117145515364,17.1675571083032));
#49271=CARTESIAN_POINT('Ctrl Pts',(-26.323292500491,21.9081856325931,17.1678002325554));
#49272=CARTESIAN_POINT('Ctrl Pts',(-26.3194914566779,21.9017852060803,17.1682420995423));
#49273=CARTESIAN_POINT('Ctrl Pts',(-26.3177792969328,21.8989123635793,17.1684407664592));
#49274=CARTESIAN_POINT('Ctrl Pts',(-26.3145647813033,21.8935377508397,17.1688130694243));
#49275=CARTESIAN_POINT('Ctrl Pts',(-26.313063492128,21.8910353442028,17.1689866691995));
#49276=CARTESIAN_POINT('Ctrl Pts',(-26.307967515529,21.882567267175,17.1695749997308));
#49277=CARTESIAN_POINT('Ctrl Pts',(-26.3043569053319,21.8766112405062,17.1699902728998));
#49278=CARTESIAN_POINT('Ctrl Pts',(-26.2992160838801,21.8681926764866,17.1705793531379));
#49279=CARTESIAN_POINT('Ctrl Pts',(-26.2977017969995,21.8657204001393,17.1707526068798));
#49280=CARTESIAN_POINT('Ctrl Pts',(-26.2930747891287,21.8581890251485,17.1712811886394));
#49281=CARTESIAN_POINT('Ctrl Pts',(-26.289951427309,21.8531365053921,17.171636887715));
#49282=CARTESIAN_POINT('Ctrl Pts',(-26.2833419111319,21.8425103893565,17.1723872980491));
#49283=CARTESIAN_POINT('Ctrl Pts',(-26.2798526387113,21.8369387730597,17.1727821184688));
#49284=CARTESIAN_POINT('Ctrl Pts',(-26.2616963376852,21.808143316208,17.1748297484953));
#49285=CARTESIAN_POINT('Ctrl Pts',(-26.246750231627,21.7850975486398,17.1764925275838));
#49286=CARTESIAN_POINT('Ctrl Pts',(-26.2266589156883,21.7549690061379,17.1786993593265));
#49287=CARTESIAN_POINT('Ctrl Pts',(-26.2217765431543,21.7477116796648,17.1792334985503));
#49288=CARTESIAN_POINT('Ctrl Pts',(-26.2144550102438,21.7369237889745,17.1800313489825));
#49289=CARTESIAN_POINT('Ctrl Pts',(-26.2120382164435,21.7333780329837,17.1802942111124));
#49290=CARTESIAN_POINT('Ctrl Pts',(-26.2077146842624,21.7270619820367,17.1807635685288));
#49291=CARTESIAN_POINT('Ctrl Pts',(-26.2058106740334,21.7242898198042,17.1809699597234));
#49292=CARTESIAN_POINT('Ctrl Pts',(-26.2017869782356,21.7184510855031,17.1814054800818));
#49293=CARTESIAN_POINT('Ctrl Pts',(-26.1996663054006,21.7153852027105,17.1816346467471));
#49294=CARTESIAN_POINT('Ctrl Pts',(-26.1940500130129,21.7072956964706,17.1822405835769));
#49295=CARTESIAN_POINT('Ctrl Pts',(-26.1905454070001,21.7022783569541,17.1826176974889));
#49296=CARTESIAN_POINT('Ctrl Pts',(-26.1746179528444,21.6796137497295,17.1843271201599));
#49297=CARTESIAN_POINT('Ctrl Pts',(-26.1620325553196,21.6620818857996,17.1856656718201));
#49298=CARTESIAN_POINT('Ctrl Pts',(-26.0684510537562,21.5344457446201,17.1955325137109));
#49299=CARTESIAN_POINT('Ctrl Pts',(-25.980710036165,21.4294818518882,17.2043273003613));
#49300=CARTESIAN_POINT('Ctrl Pts',(-25.778350100587,21.2165025674078,17.2237051598486));
#49301=CARTESIAN_POINT('Ctrl Pts',(-25.6619391534872,21.1106664166353,17.2343363776029));
#49302=CARTESIAN_POINT('Ctrl Pts',(-25.3865767566106,20.8948459038679,17.2580151878347));
#49303=CARTESIAN_POINT('Ctrl Pts',(-25.2244872148298,20.789776487479,17.2710215678252));
#49304=CARTESIAN_POINT('Ctrl Pts',(-25.0433904789264,20.6942414257646,17.2839302350354));
#49305=CARTESIAN_POINT('Ctrl Pts',(-25.0327898358473,20.6887243527105,17.2846801895551));
#49306=CARTESIAN_POINT('Ctrl Pts',(-25.0189986643707,20.6816439880012,17.2856482930714));
#49307=CARTESIAN_POINT('Ctrl Pts',(-25.0158360768246,20.6800269217928,17.2858697843376));
#49308=CARTESIAN_POINT('Ctrl Pts',(-25.0109806482107,20.6775544045836,17.2862090381496));
#49309=CARTESIAN_POINT('Ctrl Pts',(-25.0092897277077,20.6766952205242,17.2863270368157));
#49310=CARTESIAN_POINT('Ctrl Pts',(-25.0059512169783,20.6750025757172,17.2865597175737));
#49311=CARTESIAN_POINT('Ctrl Pts',(-25.0043036777437,20.6741690425738,17.2866744036544));
#49312=CARTESIAN_POINT('Ctrl Pts',(-25.0006694538914,20.6723343147293,17.2869270741811));
#49313=CARTESIAN_POINT('Ctrl Pts',(-24.9986824535812,20.6713337636168,17.2870650174024));
#49314=CARTESIAN_POINT('Ctrl Pts',(-24.9930007261856,20.6684801092578,17.2874588820946));
#49315=CARTESIAN_POINT('Ctrl Pts',(-24.9893034506443,20.6666320468618,17.2877144854428));
#49316=CARTESIAN_POINT('Ctrl Pts',(-24.9809648049732,20.6624840532316,17.2882894150135));
#49317=CARTESIAN_POINT('Ctrl Pts',(-24.9763214115896,20.6601881821031,17.2886084899302));
#49318=CARTESIAN_POINT('Ctrl Pts',(-24.8179767615122,20.5823710724214,17.2994533631232));
#49319=CARTESIAN_POINT('Ctrl Pts',(-24.6584790065058,20.5191969735644,17.3092320109603));
#49320=CARTESIAN_POINT('Ctrl Pts',(-24.2365863909219,20.3898821146604,17.3340416157873));
#49321=CARTESIAN_POINT('Ctrl Pts',(-23.9695862302417,20.3435179636237,17.3488414563069));
#49322=CARTESIAN_POINT('Ctrl Pts',(-23.6907261721221,20.3305522852027,17.3653221725283));
#49323=CARTESIAN_POINT('Ctrl Pts',(-23.6815171031978,20.3301636927435,17.3658674361528));
#49324=CARTESIAN_POINT('Ctrl Pts',(-23.6137344471982,20.3275947420582,17.3698885249926));
#49325=CARTESIAN_POINT('Ctrl Pts',(-23.5551158161485,20.3269733231394,17.3734086717156));
#49326=CARTESIAN_POINT('Ctrl Pts',(-23.4875134029064,20.3281007001469,17.3775281509878));
#49327=CARTESIAN_POINT('Ctrl Pts',(-23.4785119898456,20.3282885474309,17.3780778863707));
#49328=CARTESIAN_POINT('Ctrl Pts',(-23.4652173706675,20.3286217279744,17.3788916533468));
#49329=CARTESIAN_POINT('Ctrl Pts',(-23.4609234239531,20.3287379307163,17.3791547699035));
#49330=CARTESIAN_POINT('Ctrl Pts',(-23.4532584100905,20.3289606979213,17.3796249624165));
#49331=CARTESIAN_POINT('Ctrl Pts',(-23.4498872475059,20.3290639703787,17.3798319346804));
#49332=CARTESIAN_POINT('Ctrl Pts',(-23.4428300935526,20.3292912490605,17.3802655793531));
#49333=CARTESIAN_POINT('Ctrl Pts',(-23.4391441424881,20.3294162908851,17.3804922840004));
#49334=CARTESIAN_POINT('Ctrl Pts',(-23.4295197645335,20.3297593281706,17.3810847897676));
#49335=CARTESIAN_POINT('Ctrl Pts',(-23.4235817316131,20.3299874210771,17.3814509076436));
#49336=CARTESIAN_POINT('Ctrl Pts',(-23.3994972087006,20.3309792792366,17.3829381481657));
#49337=CARTESIAN_POINT('Ctrl Pts',(-23.381356971284,20.3318800067527,17.3840635661922));
#49338=CARTESIAN_POINT('Ctrl Pts',(-23.257137183239,20.3391010649941,17.3918071169068));
#49339=CARTESIAN_POINT('Ctrl Pts',(-23.1514300689748,20.3505108633688,17.3985847757824));
#49340=CARTESIAN_POINT('Ctrl Pts',(-22.8168345509397,20.4034640762691,17.420660991824));
#49341=CARTESIAN_POINT('Ctrl Pts',(-22.5918082394972,20.4645533608228,17.4365075035587));
#49342=CARTESIAN_POINT('Ctrl Pts',(-22.2708968236224,20.5901936211964,17.4597425212286));
#49343=CARTESIAN_POINT('Ctrl Pts',(-22.1686432731656,20.6365161302416,17.4672362312153));
#49344=CARTESIAN_POINT('Ctrl Pts',(-22.0679029185401,20.6886518029306,17.4745803501861));
#49345=CARTESIAN_POINT('Ctrl Pts',(-22.0667997029764,20.6892235539561,17.4746607710712));
#49346=CARTESIAN_POINT('Ctrl Pts',(-22.0559681363789,20.694845056538,17.4754503051783));
#49347=CARTESIAN_POINT('Ctrl Pts',(-22.0462651414434,20.6999438396518,17.4761571600226));
#49348=CARTESIAN_POINT('Ctrl Pts',(-22.0044216299058,20.7222051608535,17.4792030300762));
#49349=CARTESIAN_POINT('Ctrl Pts',(-21.9725458417482,20.7398634145975,17.4815172131766));
#49350=CARTESIAN_POINT('Ctrl Pts',(-21.9369290421668,20.7603911219688,17.4840901801243));
#49351=CARTESIAN_POINT('Ctrl Pts',(-21.9328883697418,20.7627316733649,17.4843818907656));
#49352=CARTESIAN_POINT('Ctrl Pts',(-21.9267923649877,20.7662804891594,17.4848216811508));
#49353=CARTESIAN_POINT('Ctrl Pts',(-21.9247332848705,20.7674822528544,17.4849701793072));
#49354=CARTESIAN_POINT('Ctrl Pts',(-21.9211603013957,20.7695729115873,17.4852277649209));
#49355=CARTESIAN_POINT('Ctrl Pts',(-21.9196457910503,20.7704607585756,17.4853369207428));
#49356=CARTESIAN_POINT('Ctrl Pts',(-21.9164824107231,20.7723186926438,17.4855648539608));
#49357=CARTESIAN_POINT('Ctrl Pts',(-21.914833680252,20.7732890096639,17.4856836155706));
#49358=CARTESIAN_POINT('Ctrl Pts',(-21.9109476610757,20.7755806853145,17.4859634523854));
#49359=CARTESIAN_POINT('Ctrl Pts',(-21.9087110981058,20.776903286494,17.4861244461464));
#49360=CARTESIAN_POINT('Ctrl Pts',(-21.9012944167472,20.7813012881344,17.4866581152386));
#49361=CARTESIAN_POINT('Ctrl Pts',(-21.896121282052,20.784388532072,17.4870300196998));
#49362=CARTESIAN_POINT('Ctrl Pts',(-21.8838865410553,20.7917366322493,17.487908885957));
#49363=CARTESIAN_POINT('Ctrl Pts',(-21.8768325343594,20.796010149805,17.4884150402478));
#49364=CARTESIAN_POINT('Ctrl Pts',(-21.6175917980384,20.954429164875,17.5069989100566));
#49365=CARTESIAN_POINT('Ctrl Pts',(-21.3877394375596,21.1425394854986,17.5229462899249));
#49366=CARTESIAN_POINT('Ctrl Pts',(-21.0493874336616,21.5075561421739,17.5509583986936));
#49367=CARTESIAN_POINT('Ctrl Pts',(-20.926301710661,21.668285936696,17.5625739832365));
#49368=CARTESIAN_POINT('Ctrl Pts',(-20.8123906606256,21.8501382378066,17.5756134444197));
#49369=CARTESIAN_POINT('Ctrl Pts',(-20.8057664954906,21.8608524525673,17.5763811793827));
#49370=CARTESIAN_POINT('Ctrl Pts',(-20.7967993612295,21.875548218203,17.5774336168578));
#49371=CARTESIAN_POINT('Ctrl Pts',(-20.7944018259461,21.8794964792332,17.5777163128799));
#49372=CARTESIAN_POINT('Ctrl Pts',(-20.7903349381036,21.8862264010545,17.5781980819669));
#49373=CARTESIAN_POINT('Ctrl Pts',(-20.7886612769601,21.8890054614112,17.5783969968857));
#49374=CARTESIAN_POINT('Ctrl Pts',(-20.7854315929023,21.894386615916,17.5787821095743));
#49375=CARTESIAN_POINT('Ctrl Pts',(-20.7838750398147,21.8969883885692,17.57896828764));
#49376=CARTESIAN_POINT('Ctrl Pts',(-20.7801891821573,21.9031690655086,17.579410513511));
#49377=CARTESIAN_POINT('Ctrl Pts',(-20.7780631424843,21.9067499016012,17.5796666801297));
#49378=CARTESIAN_POINT('Ctrl Pts',(-20.7718090513784,21.9173301752278,17.5804234587369));
#49379=CARTESIAN_POINT('Ctrl Pts',(-20.7677005487745,21.9243410777805,17.5809247813381));
#49380=CARTESIAN_POINT('Ctrl Pts',(-20.7379670817228,21.9755221561321,17.5845835748412));
#49381=CARTESIAN_POINT('Ctrl Pts',(-20.7133698857937,22.0202781601466,17.5877779976963));
#49382=CARTESIAN_POINT('Ctrl Pts',(-20.6355792757842,22.1701531646646,17.598467039943));
#49383=CARTESIAN_POINT('Ctrl Pts',(-20.5870905309683,22.2775939014891,17.6061208766361));
#49384=CARTESIAN_POINT('Ctrl Pts',(-20.4617147282357,22.601666681875,17.6291428712486));
#49385=CARTESIAN_POINT('Ctrl Pts',(-20.4019826547138,22.8241220955053,17.6449122698399));
#49386=CARTESIAN_POINT('Ctrl Pts',(-20.3606170445335,23.0879336879652,17.6627235615881));
#49387=CARTESIAN_POINT('Ctrl Pts',(-20.3554718989437,23.1249407187237,17.6652006099861));
#49388=CARTESIAN_POINT('Ctrl Pts',(-20.3498470207476,23.1712944562916,17.6682703313811));
#49389=CARTESIAN_POINT('Ctrl Pts',(-20.3487630393551,23.1805638907707,17.6688825457223));
#49390=CARTESIAN_POINT('Ctrl Pts',(-20.3470430970871,23.1958467708995,17.6698890888089));
#49391=CARTESIAN_POINT('Ctrl Pts',(-20.3463837743223,23.2018574804853,17.6702842363054));
#49392=CARTESIAN_POINT('Ctrl Pts',(-20.3442537144492,23.2217936658776,17.6715923831275));
#49393=CARTESIAN_POINT('Ctrl Pts',(-20.3428567994693,23.2357270598757,17.6725026542787));
#49394=CARTESIAN_POINT('Ctrl Pts',(-20.3414157510964,23.2511101373458,17.6735029225086));
#49395=CARTESIAN_POINT('Ctrl Pts',(-20.3412817510102,23.252551027927,17.6735965693101));
#49396=CARTESIAN_POINT('Ctrl Pts',(-20.3406079059697,23.2598501398061,17.6740707230023));
#49397=CARTESIAN_POINT('Ctrl Pts',(-20.3400831284815,23.2657097820843,17.674450609806));
#49398=CARTESIAN_POINT('Ctrl Pts',(-20.3389934715365,23.2782636678585,17.6752628224561));
#49399=CARTESIAN_POINT('Ctrl Pts',(-20.3384334711,23.2849583231629,17.6756949381677));
#49400=CARTESIAN_POINT('Ctrl Pts',(-20.3351183696794,23.3261392353261,17.6783465760054));
#49401=CARTESIAN_POINT('Ctrl Pts',(-20.3328976580148,23.360667966073,17.6805421273777));
#49402=CARTESIAN_POINT('Ctrl Pts',(-20.3310120703815,23.3998212624171,17.682995293457));
#49403=CARTESIAN_POINT('Ctrl Pts',(-20.330800668884,23.4044155740968,17.6832825838584));
#49404=CARTESIAN_POINT('Ctrl Pts',(-20.3304954083529,23.4113740701244,17.6837168344498));
#49405=CARTESIAN_POINT('Ctrl Pts',(-20.33039431779,23.4137379067005,17.6838641984526));
#49406=CARTESIAN_POINT('Ctrl Pts',(-20.3302229442287,23.4178513073028,17.6841203630898));
#49407=CARTESIAN_POINT('Ctrl Pts',(-20.3301514839202,23.4196008170745,17.6842292302647));
#49408=CARTESIAN_POINT('Ctrl Pts',(-20.3300047713661,23.4232659192614,17.6844571209012));
#49409=CARTESIAN_POINT('Ctrl Pts',(-20.3299298025851,23.4251815197006,17.6845761277844));
#49410=CARTESIAN_POINT('Ctrl Pts',(-20.329756440007,23.4297147875335,17.6848575177043));
#49411=CARTESIAN_POINT('Ctrl Pts',(-20.3296595281043,23.4323325177674,17.6850198167942));
#49412=CARTESIAN_POINT('Ctrl Pts',(-20.3293470039096,23.4410621248112,17.6855604295797));
#49413=CARTESIAN_POINT('Ctrl Pts',(-20.329145595566,23.4471745449709,17.6859379465033));
#49414=CARTESIAN_POINT('Ctrl Pts',(-20.3287082972051,23.4617021133822,17.6868328635982));
#49415=CARTESIAN_POINT('Ctrl Pts',(-20.3284879764787,23.4701177343231,17.6873494125506));
#49416=CARTESIAN_POINT('Ctrl Pts',(-20.3278231210125,23.4999864327357,17.689176436301));
#49417=CARTESIAN_POINT('Ctrl Pts',(-20.3275598557561,23.5214435163952,17.6904773838207));
#49418=CARTESIAN_POINT('Ctrl Pts',(-20.3273240505194,23.6248329131841,17.6966971091828));
#49419=CARTESIAN_POINT('Ctrl Pts',(-20.3302615913328,23.7067478765591,17.7014776249486));
#49420=CARTESIAN_POINT('Ctrl Pts',(-20.3481687975102,23.9483465753992,17.7153702898887));
#49421=CARTESIAN_POINT('Ctrl Pts',(-20.3719327159962,24.1071252931762,17.7242409693559));
#49422=CARTESIAN_POINT('Ctrl Pts',(-20.4584434164475,24.4883334557849,17.7461319409387));
#49423=CARTESIAN_POINT('Ctrl Pts',(-20.5334427016099,24.7070215811852,17.7592450734469));
#49424=CARTESIAN_POINT('Ctrl Pts',(-20.6373126975939,24.9290609648792,17.7741214881741));
#49425=CARTESIAN_POINT('Ctrl Pts',(-20.6435955585754,24.9422569864725,17.7750115181377));
#49426=CARTESIAN_POINT('Ctrl Pts',(-20.6523498410436,24.9603260769482,17.7762385242081));
#49427=CARTESIAN_POINT('Ctrl Pts',(-20.6547442846688,24.9652364179389,17.7765728146781));
#49428=CARTESIAN_POINT('Ctrl Pts',(-20.6585714867536,24.9730345560819,17.7771050605018));
#49429=CARTESIAN_POINT('Ctrl Pts',(-20.6599961202256,24.975926347976,17.7773027314045));
#49430=CARTESIAN_POINT('Ctrl Pts',(-20.6627720697436,24.9815398467077,17.7776870275861));
#49431=CARTESIAN_POINT('Ctrl Pts',(-20.6641229015853,24.984261790512,17.7778736357476));
#49432=CARTESIAN_POINT('Ctrl Pts',(-20.6673565524502,24.9907545620797,17.7783193973696));
#49433=CARTESIAN_POINT('Ctrl Pts',(-20.6692429194343,24.994523607525,17.7785786751864));
#49434=CARTESIAN_POINT('Ctrl Pts',(-20.6748974798819,25.0057665118734,17.7793536323631));
#49435=CARTESIAN_POINT('Ctrl Pts',(-20.6786873801292,25.0132293594935,17.779870074934));
#49436=CARTESIAN_POINT('Ctrl Pts',(-20.7040843213504,25.0627606135958,17.7833114256486));
#49437=CARTESIAN_POINT('Ctrl Pts',(-20.7265850919819,25.1043619181183,17.7862678378873));
#49438=CARTESIAN_POINT('Ctrl Pts',(-20.7806130000444,25.1992041458146,17.7931666935691));
#49439=CARTESIAN_POINT('Ctrl Pts',(-20.8127734328294,25.2520609569822,17.7971309278524));
#49440=CARTESIAN_POINT('Ctrl Pts',(-20.9082596364963,25.3992792940821,17.8085179043822));
#49441=CARTESIAN_POINT('Ctrl Pts',(-20.9750782501858,25.4912573793737,17.8160539628812));
#49442=CARTESIAN_POINT('Ctrl Pts',(-21.1427777845634,25.6981607693801,17.8339413576312));
#49443=CARTESIAN_POINT('Ctrl Pts',(-21.2472582707796,25.8098234633157,17.844351256109));
#49444=CARTESIAN_POINT('Ctrl Pts',(-21.4268043854254,25.9762715662232,17.8607831257435));
#49445=CARTESIAN_POINT('Ctrl Pts',(-21.4970063467623,26.0359683570262,17.866896329439));
#49446=CARTESIAN_POINT('Ctrl Pts',(-21.6053125587343,26.1203433784426,17.8757697598378));
#49447=CARTESIAN_POINT('Ctrl Pts',(-21.6415328908282,26.1473563632304,17.8786500559585));
#49448=CARTESIAN_POINT('Ctrl Pts',(-21.68274006518,26.1767605458619,17.8818197374122));
#49449=CARTESIAN_POINT('Ctrl Pts',(-21.6871766805196,26.1799094551112,17.8821596381275));
#49450=CARTESIAN_POINT('Ctrl Pts',(-21.693488848406,26.1843655537412,17.8826412675634));
#49451=CARTESIAN_POINT('Ctrl Pts',(-21.6953578191684,26.1856819832294,17.8827836297871));
#49452=CARTESIAN_POINT('Ctrl Pts',(-21.6987863063782,26.1880914209618,17.883044334208));
#49453=CARTESIAN_POINT('Ctrl Pts',(-21.700345393224,26.1891850371433,17.8831627185442));
#49454=CARTESIAN_POINT('Ctrl Pts',(-21.7035209145941,26.1914082987448,17.8834034951055));
#49455=CARTESIAN_POINT('Ctrl Pts',(-21.705137416757,26.1925378425761,17.8835258802623));
#49456=CARTESIAN_POINT('Ctrl Pts',(-21.7083894441172,26.1948057831869,17.8837717265871));
#49457=CARTESIAN_POINT('Ctrl Pts',(-21.7100249904788,26.1959441482594,17.8838951855432));
#49458=CARTESIAN_POINT('Ctrl Pts',(-21.7162368285864,26.2002591348075,17.8843633882847));
#49459=CARTESIAN_POINT('Ctrl Pts',(-21.7208203335501,26.2034254301845,17.8847074252938));
#49460=CARTESIAN_POINT('Ctrl Pts',(-21.7694508054668,26.2368335317796,17.8883427230564));
#49461=CARTESIAN_POINT('Ctrl Pts',(-21.8142382895746,26.2659895644503,17.891561613544));
#49462=CARTESIAN_POINT('Ctrl Pts',(-21.897355772363,26.3172007877149,17.8973432559573));
#49463=CARTESIAN_POINT('Ctrl Pts',(-21.9354527552926,26.3396059275947,17.8999225232389));
#49464=CARTESIAN_POINT('Ctrl Pts',(-22.0073597967404,26.3799278442835,17.9046830920078));
#49465=CARTESIAN_POINT('Ctrl Pts',(-22.0410439079389,26.3980356427987,17.906870386349));
#49466=CARTESIAN_POINT('Ctrl Pts',(-22.075036043603,26.4155367891046,17.9090429972639));
#49467=CARTESIAN_POINT('Origin',(-23.5502525316942,23.5502525316942,-77.3107734492734));
#49468=CARTESIAN_POINT('',(-22.0750358228142,26.4155366754296,19.4043601800006));
#49469=CARTESIAN_POINT('',(-22.0750360918396,26.4155368139396,19.1544452962233));
#49470=CARTESIAN_POINT('',(-22.0750360153461,26.4155367745563,-77.3107734492734));
#49471=CARTESIAN_POINT('Ctrl Pts',(-22.0750358228142,26.4155366754296,19.4043601800006));
#49472=CARTESIAN_POINT('Ctrl Pts',(-21.9939687733971,26.3737985929776,19.3992424347326));
#49473=CARTESIAN_POINT('Ctrl Pts',(-21.9146767412259,26.3286220321774,19.3940856294656));
#49474=CARTESIAN_POINT('Ctrl Pts',(-21.7630209617868,26.2334644961253,19.3837857518897));
#49475=CARTESIAN_POINT('Ctrl Pts',(-21.6906072610263,26.1837940049789,19.3786563162919));
#49476=CARTESIAN_POINT('Ctrl Pts',(-21.5963489247256,26.113311991075,19.3716309920995));
#49477=CARTESIAN_POINT('Ctrl Pts',(-21.5726341194396,26.0950586977324,19.3698324915126));
#49478=CARTESIAN_POINT('Ctrl Pts',(-21.5342698855086,26.0646696042408,19.3668698112217));
#49479=CARTESIAN_POINT('Ctrl Pts',(-21.5194673187915,26.0527294325543,19.3657134077547));
#49480=CARTESIAN_POINT('Ctrl Pts',(-21.5014090490665,26.0378973777065,19.364285916325));
#49481=CARTESIAN_POINT('Ctrl Pts',(-21.498052166134,26.0351288174475,19.3640198389897));
#49482=CARTESIAN_POINT('Ctrl Pts',(-21.4915500683505,26.0297441059023,19.3635030600241));
#49483=CARTESIAN_POINT('Ctrl Pts',(-21.4884042063588,26.0271287462459,19.3632523909296));
#49484=CARTESIAN_POINT('Ctrl Pts',(-21.4829425933211,26.0225705368421,19.3628160796802));
#49485=CARTESIAN_POINT('Ctrl Pts',(-21.480624574812,26.0206304015486,19.3626305487979));
#49486=CARTESIAN_POINT('Ctrl Pts',(-21.4757990232422,26.0165799521604,19.3622435830534));
#49487=CARTESIAN_POINT('Ctrl Pts',(-21.4732919738792,26.0144690694236,19.3620421249607));
#49488=CARTESIAN_POINT('Ctrl Pts',(-21.4671669892207,26.0092959741506,19.3615489217591));
#49489=CARTESIAN_POINT('Ctrl Pts',(-21.4635525890867,26.0062296037161,19.36125700556));
#49490=CARTESIAN_POINT('Ctrl Pts',(-21.4497506963997,25.9944679468523,19.3601389398655));
#49491=CARTESIAN_POINT('Ctrl Pts',(-21.4396107931277,25.9857172508981,19.3593105004364));
#49492=CARTESIAN_POINT('Ctrl Pts',(-21.2668848763215,25.8347666472278,19.3450765877454));
#49493=CARTESIAN_POINT('Ctrl Pts',(-21.118978638314,25.6766688085267,19.3309670697052));
#49494=CARTESIAN_POINT('Ctrl Pts',(-20.890236741997,25.3768393788007,19.3056351346649));
#49495=CARTESIAN_POINT('Ctrl Pts',(-20.8022160732772,25.2415237211257,19.2946381336349));
#49496=CARTESIAN_POINT('Ctrl Pts',(-20.6944896714971,25.0451368541745,19.2796395511465));
#49497=CARTESIAN_POINT('Ctrl Pts',(-20.665903620107,24.9892079957519,19.2754706720324));
#49498=CARTESIAN_POINT('Ctrl Pts',(-20.6117146366385,24.8750734769832,19.2672133221891));
#49499=CARTESIAN_POINT('Ctrl Pts',(-20.5861619348849,24.8168715701283,19.2631281095782));
#49500=CARTESIAN_POINT('Ctrl Pts',(-20.5598458390541,24.7517640199359,19.2587248604777));
#49501=CARTESIAN_POINT('Ctrl Pts',(-20.55736570862,24.7455727858205,19.2583077876028));
#49502=CARTESIAN_POINT('Ctrl Pts',(-20.5541270688489,24.7374147851807,19.2577604252961));
#49503=CARTESIAN_POINT('Ctrl Pts',(-20.5533512676259,24.7354549695498,19.2576290980631));
#49504=CARTESIAN_POINT('Ctrl Pts',(-20.5518248208036,24.7315878043744,19.2573702904512));
#49505=CARTESIAN_POINT('Ctrl Pts',(-20.5510740711862,24.729680497276,19.2572428037973));
#49506=CARTESIAN_POINT('Ctrl Pts',(-20.5496357517992,24.7260161400179,19.2569981802938));
#49507=CARTESIAN_POINT('Ctrl Pts',(-20.5489479074034,24.7242592074295,19.2568810271682));
#49508=CARTESIAN_POINT('Ctrl Pts',(-20.547369099053,24.7202160665978,19.2566117381872));
#49509=CARTESIAN_POINT('Ctrl Pts',(-20.5464792006397,24.7179294385384,19.2564596672537));
#49510=CARTESIAN_POINT('Ctrl Pts',(-20.5436607212805,24.7106627043547,19.2559771124902));
#49511=CARTESIAN_POINT('Ctrl Pts',(-20.5417418945066,24.705678786442,19.2556472167962));
#49512=CARTESIAN_POINT('Ctrl Pts',(-20.5254238854341,24.6629784996152,19.2528297288971));
#49513=CARTESIAN_POINT('Ctrl Pts',(-20.5117213950144,24.6249973011818,19.2503831860559));
#49514=CARTESIAN_POINT('Ctrl Pts',(-20.4974742566202,24.5830534531615,19.2477359113866));
#49515=CARTESIAN_POINT('Ctrl Pts',(-20.4962198009907,24.5793380578943,19.2475018809614));
#49516=CARTESIAN_POINT('Ctrl Pts',(-20.4942930392616,24.5735969012346,19.247140954578));
#49517=CARTESIAN_POINT('Ctrl Pts',(-20.4936159631903,24.5715727587486,19.2470138390893));
#49518=CARTESIAN_POINT('Ctrl Pts',(-20.4924810177359,24.5681685621686,19.2468002816303));
#49519=CARTESIAN_POINT('Ctrl Pts',(-20.4920220714973,24.5667888709415,19.2467137907331));
#49520=CARTESIAN_POINT('Ctrl Pts',(-20.4907437289591,24.562937196623,19.2464725067111));
#49521=CARTESIAN_POINT('Ctrl Pts',(-20.4899263933318,24.5604645250611,19.2463178064965));
#49522=CARTESIAN_POINT('Ctrl Pts',(-20.4875939940553,24.5533795490743,19.2458751007526));
#49523=CARTESIAN_POINT('Ctrl Pts',(-20.4860863482267,24.5487647909272,19.2455874244867));
#49524=CARTESIAN_POINT('Ctrl Pts',(-20.4810764566643,24.5333117950062,19.2446263217008));
#49525=CARTESIAN_POINT('Ctrl Pts',(-20.4776212072329,24.5224582943791,19.2439549199208));
#49526=CARTESIAN_POINT('Ctrl Pts',(-20.4423262988046,24.4095233962173,19.2370042346074));
#49527=CARTESIAN_POINT('Ctrl Pts',(-20.4155260936426,24.3059280116781,19.2309277764199));
#49528=CARTESIAN_POINT('Ctrl Pts',(-20.3520882483359,23.998322179048,19.2132659261849));
#49529=CARTESIAN_POINT('Ctrl Pts',(-20.329907442405,23.791906734035,19.2018647192872));
#49530=CARTESIAN_POINT('Ctrl Pts',(-20.3271722222006,23.5367037534076,19.1871822645609));
#49531=CARTESIAN_POINT('Ctrl Pts',(-20.3277332641241,23.4886122415337,19.1843918322158));
#49532=CARTESIAN_POINT('Ctrl Pts',(-20.332177037631,23.358139113304,19.1767362858181));
#49533=CARTESIAN_POINT('Ctrl Pts',(-20.3381457857551,23.2758697896039,19.1718161228541));
#49534=CARTESIAN_POINT('Ctrl Pts',(-20.3483027899385,23.1845695835809,19.1662210817039));
#49535=CARTESIAN_POINT('Ctrl Pts',(-20.3493845256441,23.1752189703199,19.1656464916665));
#49536=CARTESIAN_POINT('Ctrl Pts',(-20.3510404969964,23.1614339208957,19.1647970510978));
#49537=CARTESIAN_POINT('Ctrl Pts',(-20.3515830281681,23.1569956665904,19.1645232032897));
#49538=CARTESIAN_POINT('Ctrl Pts',(-20.3525528186471,23.1491969458152,19.1640413696622));
#49539=CARTESIAN_POINT('Ctrl Pts',(-20.3529761441711,23.1458359897085,19.1638335085994));
#49540=CARTESIAN_POINT('Ctrl Pts',(-20.3538094635,23.1393030164193,19.1634290630346));
#49541=CARTESIAN_POINT('Ctrl Pts',(-20.3542188819947,23.1361309285679,19.1632324969657));
#49542=CARTESIAN_POINT('Ctrl Pts',(-20.3552093077928,23.1285462734236,19.162762044955));
#49543=CARTESIAN_POINT('Ctrl Pts',(-20.3557947339459,23.1241342981496,19.1624880192802));
#49544=CARTESIAN_POINT('Ctrl Pts',(-20.35793153699,23.1082825036289,19.1615021507453));
#49545=CARTESIAN_POINT('Ctrl Pts',(-20.3595352274609,23.0968499315331,19.1607886518034));
#49546=CARTESIAN_POINT('Ctrl Pts',(-20.3871471964499,22.9074113558644,19.1489241641714));
#49547=CARTESIAN_POINT('Ctrl Pts',(-20.4279486276348,22.7319136607659,19.1372930771706));
#49548=CARTESIAN_POINT('Ctrl Pts',(-20.5454558720408,22.3676817041711,19.1118161968531));
#49549=CARTESIAN_POINT('Ctrl Pts',(-20.6258337004218,22.1809299208933,19.0979283571476));
#49550=CARTESIAN_POINT('Ctrl Pts',(-20.7649219265749,21.9268018062588,19.078545840006));
#49551=CARTESIAN_POINT('Ctrl Pts',(-20.8096804505141,21.8523344086307,19.0728070760287));
#49552=CARTESIAN_POINT('Ctrl Pts',(-20.8789163561314,21.7470290051285,19.064696294153));
#49553=CARTESIAN_POINT('Ctrl Pts',(-20.9010329188371,21.714690536262,19.0622063313632));
#49554=CARTESIAN_POINT('Ctrl Pts',(-20.9265591586669,21.678789360174,19.0594501909739));
#49555=CARTESIAN_POINT('Ctrl Pts',(-20.9293925102899,21.6748234962539,19.0591458446519));
#49556=CARTESIAN_POINT('Ctrl Pts',(-20.9336397571248,21.6689070147482,19.0586919943347));
#49557=CARTESIAN_POINT('Ctrl Pts',(-20.935046843624,21.6669515532659,19.058542022871));
#49558=CARTESIAN_POINT('Ctrl Pts',(-20.937451060458,21.6636182462294,19.0582864349631));
#49559=CARTESIAN_POINT('Ctrl Pts',(-20.9384470888343,21.6622396122766,19.0581807417731));
#49560=CARTESIAN_POINT('Ctrl Pts',(-20.9404940071553,21.6594111283792,19.0579639298355));
#49561=CARTESIAN_POINT('Ctrl Pts',(-20.9415450118077,21.6579613689445,19.0578528196451));
#49562=CARTESIAN_POINT('Ctrl Pts',(-20.9440766026882,21.654475401381,19.0575856956546));
#49563=CARTESIAN_POINT('Ctrl Pts',(-20.9455583704911,21.652440046899,19.0574297643579));
#49564=CARTESIAN_POINT('Ctrl Pts',(-20.9509677067775,21.6450280579651,19.056862039518));
#49565=CARTESIAN_POINT('Ctrl Pts',(-20.9549095856943,21.6396618139071,19.0564512357335));
#49566=CARTESIAN_POINT('Ctrl Pts',(-21.0227071630899,21.547963144304,19.049434553622));
#49567=CARTESIAN_POINT('Ctrl Pts',(-21.0908298682319,21.4648522936563,19.0431224328856));
#49568=CARTESIAN_POINT('Ctrl Pts',(-21.3042384201018,21.2295302323977,19.0248763984484));
#49569=CARTESIAN_POINT('Ctrl Pts',(-21.460403216922,21.0879628364222,19.0133648127743));
#49570=CARTESIAN_POINT('Ctrl Pts',(-21.7395193597168,20.8807540200798,18.99373476062));
#49571=CARTESIAN_POINT('Ctrl Pts',(-21.8548935695579,20.806035152707,18.9858527329255));
#49572=CARTESIAN_POINT('Ctrl Pts',(-22.0214577861786,20.712686594495,18.974515501888));
#49573=CARTESIAN_POINT('Ctrl Pts',(-22.0688871754188,20.6876400912057,18.9712927526491));
#49574=CARTESIAN_POINT('Ctrl Pts',(-22.1257271873096,20.6594149615546,18.9674287355809));
#49575=CARTESIAN_POINT('Ctrl Pts',(-22.1345569227314,20.6550806450673,18.9668284406048));
#49576=CARTESIAN_POINT('Ctrl Pts',(-22.1475081993767,20.6487965717359,18.9659478257234));
#49577=CARTESIAN_POINT('Ctrl Pts',(-22.1516143149421,20.6468150021908,18.9656686159543));
#49578=CARTESIAN_POINT('Ctrl Pts',(-22.1587911730526,20.6433702808665,18.9651805655811));
#49579=CARTESIAN_POINT('Ctrl Pts',(-22.1618600600835,20.6419032615066,18.9649718599543));
#49580=CARTESIAN_POINT('Ctrl Pts',(-22.1677965407446,20.6390769845509,18.9645681142963));
#49581=CARTESIAN_POINT('Ctrl Pts',(-22.1706638321687,20.6377170978809,18.9643730964098));
#49582=CARTESIAN_POINT('Ctrl Pts',(-22.1774715710409,20.6345006611618,18.9639100425926));
#49583=CARTESIAN_POINT('Ctrl Pts',(-22.1814137761389,20.6326478639152,18.9636418767937));
#49584=CARTESIAN_POINT('Ctrl Pts',(-22.195305189327,20.6261533893928,18.9626968369711));
#49585=CARTESIAN_POINT('Ctrl Pts',(-22.2052742624308,20.6215546051389,18.962018480617));
#49586=CARTESIAN_POINT('Ctrl Pts',(-22.33953767958,20.5604483074986,18.9528798131984));
#49587=CARTESIAN_POINT('Ctrl Pts',(-22.4672600020242,20.5118519689857,18.9441476540586));
#49588=CARTESIAN_POINT('Ctrl Pts',(-22.6859506076536,20.4441874300084,18.9291170118164));
#49589=CARTESIAN_POINT('Ctrl Pts',(-22.77536574582,20.4206827871727,18.9229526621681));
#49590=CARTESIAN_POINT('Ctrl Pts',(-23.1308653736768,20.3434023059526,18.8984721590692));
#49591=CARTESIAN_POINT('Ctrl Pts',(-23.4023012973465,20.3194780459966,18.8797455299965));
#49592=CARTESIAN_POINT('Ctrl Pts',(-23.6854704775301,20.3303183206974,18.8618832599947));
#49593=CARTESIAN_POINT('Ctrl Pts',(-23.6974030923726,20.330841570171,18.8611338474292));
#49594=CARTESIAN_POINT('Ctrl Pts',(-23.7127207889739,20.3315985995718,18.8601763094219));
#49595=CARTESIAN_POINT('Ctrl Pts',(-23.7161085867543,20.331771393231,18.8599648127063));
#49596=CARTESIAN_POINT('Ctrl Pts',(-23.7215799893495,20.3320591224571,18.8596236993352));
#49597=CARTESIAN_POINT('Ctrl Pts',(-23.7236637549415,20.332170732747,18.8594938953682));
#49598=CARTESIAN_POINT('Ctrl Pts',(-23.7276212104647,20.3323865562638,18.8592475805764));
#49599=CARTESIAN_POINT('Ctrl Pts',(-23.7294949038697,20.3324903813674,18.8591310489398));
#49600=CARTESIAN_POINT('Ctrl Pts',(-23.7337859410432,20.3327319159725,18.858864375087));
#49601=CARTESIAN_POINT('Ctrl Pts',(-23.7362032177593,20.3328707129811,18.8587142952012));
#49602=CARTESIAN_POINT('Ctrl Pts',(-23.7436470425617,20.3333065452079,18.8582525783987));
#49603=CARTESIAN_POINT('Ctrl Pts',(-23.748673083574,20.3336126385431,18.8579414513442));
#49604=CARTESIAN_POINT('Ctrl Pts',(-23.7866040565641,20.3360119321182,18.8555979691074));
#49605=CARTESIAN_POINT('Ctrl Pts',(-23.8194773706145,20.3385983056942,18.853592863262));
#49606=CARTESIAN_POINT('Ctrl Pts',(-24.0618965207586,20.3614196460397,18.8389598990507));
#49607=CARTESIAN_POINT('Ctrl Pts',(-24.2690792896872,20.4016421106844,18.8272799691827));
#49608=CARTESIAN_POINT('Ctrl Pts',(-24.6161640039729,20.5051033841715,18.807041473112));
#49609=CARTESIAN_POINT('Ctrl Pts',(-24.7582047484528,20.5586061864045,18.7985536470922));
#49610=CARTESIAN_POINT('Ctrl Pts',(-24.9912286860579,20.6656899015113,18.783723921007));
#49611=CARTESIAN_POINT('Ctrl Pts',(-25.0843098032605,20.7140969178985,18.7775388398014));
#49612=CARTESIAN_POINT('Ctrl Pts',(-25.1853490326489,20.7730732961667,18.7704536002071));
#49613=CARTESIAN_POINT('Ctrl Pts',(-25.195803515989,20.7792550532593,18.7697159437129));
#49614=CARTESIAN_POINT('Ctrl Pts',(-25.2140277012111,20.7901705546093,18.7684219601541));
#49615=CARTESIAN_POINT('Ctrl Pts',(-25.2218128112853,20.7948784075593,18.7678665798065));
#49616=CARTESIAN_POINT('Ctrl Pts',(-25.2334169036998,20.8019629742593,18.7670348091106));
#49617=CARTESIAN_POINT('Ctrl Pts',(-25.2372510607793,20.8043148490011,18.7667593327141));
#49618=CARTESIAN_POINT('Ctrl Pts',(-25.2439676326581,20.8084541761313,18.7662756181294));
#49619=CARTESIAN_POINT('Ctrl Pts',(-25.2468521793936,20.8102381702201,18.7660675077908));
#49620=CARTESIAN_POINT('Ctrl Pts',(-25.2524446884456,20.8137091640413,18.765663304303));
#49621=CARTESIAN_POINT('Ctrl Pts',(-25.2551529735356,20.8153956387586,18.7654672307376));
#49622=CARTESIAN_POINT('Ctrl Pts',(-25.2616079057645,20.819428500549,18.7649991184978));
#49623=CARTESIAN_POINT('Ctrl Pts',(-25.2653522312026,20.8217785761866,18.7647269432263));
#49624=CARTESIAN_POINT('Ctrl Pts',(-25.2787044244436,20.8301972462065,18.7637540867385));
#49625=CARTESIAN_POINT('Ctrl Pts',(-25.2882849285634,20.8363088912,18.7630518059237));
#49626=CARTESIAN_POINT('Ctrl Pts',(-25.4348154597044,20.9308785103109,18.7522448539084));
#49627=CARTESIAN_POINT('Ctrl Pts',(-25.5648695209389,21.0295381352834,18.741748724936));
#49628=CARTESIAN_POINT('Ctrl Pts',(-25.7533631149592,21.1964670687975,18.7250702899455));
#49629=CARTESIAN_POINT('Ctrl Pts',(-25.8173739142267,21.2580567549753,18.7191102224521));
#49630=CARTESIAN_POINT('Ctrl Pts',(-25.9991195617505,21.4479971116604,18.7013608192772));
#49631=CARTESIAN_POINT('Ctrl Pts',(-26.1090943648255,21.5833361132422,18.6894868539506));
#49632=CARTESIAN_POINT('Ctrl Pts',(-26.2495643839562,21.7880567003575,18.6731300066926));
#49633=CARTESIAN_POINT('Ctrl Pts',(-26.2894077053364,21.8506497652239,18.6683243633542));
#49634=CARTESIAN_POINT('Ctrl Pts',(-26.3329202173558,21.9245183921427,18.6629225602625));
#49635=CARTESIAN_POINT('Ctrl Pts',(-26.3387283964037,21.9345009100291,18.6621981112299));
#49636=CARTESIAN_POINT('Ctrl Pts',(-26.3461568706378,21.9474275950149,18.6612673503688));
#49637=CARTESIAN_POINT('Ctrl Pts',(-26.3478263029087,21.9503432076939,18.6610578977681));
#49638=CARTESIAN_POINT('Ctrl Pts',(-26.350513923626,21.9550541242638,18.6607202552193));
#49639=CARTESIAN_POINT('Ctrl Pts',(-26.3515349465715,21.9568477951727,18.6605918811234));
#49640=CARTESIAN_POINT('Ctrl Pts',(-26.353483903977,21.9602792679645,18.66034663927));
#49641=CARTESIAN_POINT('Ctrl Pts',(-26.3544121197424,21.9619168899933,18.6602297537771));
#49642=CARTESIAN_POINT('Ctrl Pts',(-26.3565325129072,21.9656654854992,18.659962544937));
#49643=CARTESIAN_POINT('Ctrl Pts',(-26.3577237422088,21.9677769893398,18.6598122836948));
#49644=CARTESIAN_POINT('Ctrl Pts',(-26.3608718725082,21.9733719251763,18.6594147914113));
#49645=CARTESIAN_POINT('Ctrl Pts',(-26.3628246879521,21.9768576694868,18.6591678241217));
#49646=CARTESIAN_POINT('Ctrl Pts',(-26.3721180914058,21.9935188356319,18.6579905570476));
#49647=CARTESIAN_POINT('Ctrl Pts',(-26.3793727676114,22.0067423279321,18.6570656962839));
#49648=CARTESIAN_POINT('Ctrl Pts',(-26.5342045727174,22.2937220276107,18.6371880973738));
#49649=CARTESIAN_POINT('Ctrl Pts',(-26.6415068501997,22.5874125034123,18.6205282053894));
#49650=CARTESIAN_POINT('Ctrl Pts',(-26.729078011321,23.007098211841,18.5962912344066));
#49651=CARTESIAN_POINT('Ctrl Pts',(-26.7467781866622,23.1234409793876,18.5895460908354));
#49652=CARTESIAN_POINT('Ctrl Pts',(-26.7648888558905,23.310987155942,18.578434092643));
#49653=CARTESIAN_POINT('Ctrl Pts',(-26.7693704969407,23.3816910617989,18.5741922271389));
#49654=CARTESIAN_POINT('Ctrl Pts',(-26.7717798780515,23.4610729241815,18.5693519043927));
#49655=CARTESIAN_POINT('Ctrl Pts',(-26.7720062722793,23.4696654452892,18.5688269623596));
#49656=CARTESIAN_POINT('Ctrl Pts',(-26.7722934633981,23.4825181333479,18.568040208278));
#49657=CARTESIAN_POINT('Ctrl Pts',(-26.7723801926752,23.4867777306864,18.5677792107976));
#49658=CARTESIAN_POINT('Ctrl Pts',(-26.7725144287698,23.4940822295859,18.5673312038727));
#49659=CARTESIAN_POINT('Ctrl Pts',(-26.7725660670323,23.4971270570738,18.5671443244059));
#49660=CARTESIAN_POINT('Ctrl Pts',(-26.7726632157123,23.5033779443067,18.5667603988557));
#49661=CARTESIAN_POINT('Ctrl Pts',(-26.7727082572685,23.5065840075025,18.5665633382302));
#49662=CARTESIAN_POINT('Ctrl Pts',(-26.7728047679902,23.5142702877264,18.5660905480944));
#49663=CARTESIAN_POINT('Ctrl Pts',(-26.7728516786828,23.5187505468328,18.5658146757019));
#49664=CARTESIAN_POINT('Ctrl Pts',(-26.7729661063602,23.532397333681,18.5649734894999));
#49665=CARTESIAN_POINT('Ctrl Pts',(-26.773003856129,23.5415640048235,18.5644072421497));
#49666=CARTESIAN_POINT('Ctrl Pts',(-26.7729774855936,23.7193191145127,18.5534029123502));
#49667=CARTESIAN_POINT('Ctrl Pts',(-26.759724207419,23.8876167449681,18.5425445142253));
#49668=CARTESIAN_POINT('Ctrl Pts',(-26.6851551362351,24.3587319883457,18.5109155132179));
#49669=CARTESIAN_POINT('Ctrl Pts',(-26.5934574051106,24.6548536111985,18.4894279314694));
#49670=CARTESIAN_POINT('Ctrl Pts',(-26.4464364805558,24.964254447275,18.4674489425529));
#49671=CARTESIAN_POINT('Ctrl Pts',(-26.4312956327195,24.994854125605,18.4652829833665));
#49672=CARTESIAN_POINT('Ctrl Pts',(-26.4133422188169,25.029732470811,18.4628280545854));
#49673=CARTESIAN_POINT('Ctrl Pts',(-26.4110030224564,25.0342505361426,18.4625103193415));
#49674=CARTESIAN_POINT('Ctrl Pts',(-26.4075420818362,25.0408966124564,18.4620433513688));
#49675=CARTESIAN_POINT('Ctrl Pts',(-26.4064286531782,25.0430289087907,18.4618935954643));
#49676=CARTESIAN_POINT('Ctrl Pts',(-26.4044408990487,25.0468252360948,18.4616270876595));
#49677=CARTESIAN_POINT('Ctrl Pts',(-26.4035675050717,25.0484897487831,18.4615102765119));
#49678=CARTESIAN_POINT('Ctrl Pts',(-26.4017275576152,25.0519888730713,18.4612648024197));
#49679=CARTESIAN_POINT('Ctrl Pts',(-26.4007606919483,25.0538233118195,18.461136160108));
#49680=CARTESIAN_POINT('Ctrl Pts',(-26.3982023953352,25.0586658430597,18.4607966978592));
#49681=CARTESIAN_POINT('Ctrl Pts',(-26.3966079636667,25.061672360482,18.4605860693574));
#49682=CARTESIAN_POINT('Ctrl Pts',(-26.3893856315562,25.0752390872169,18.4596361779436));
#49683=CARTESIAN_POINT('Ctrl Pts',(-26.3837036087039,25.0857706065013,18.4589003261876));
#49684=CARTESIAN_POINT('Ctrl Pts',(-26.2477779840406,25.3343824152357,18.4415598674329));
#49685=CARTESIAN_POINT('Ctrl Pts',(-26.0880134128168,25.5551436383689,18.4267643978409));
#49686=CARTESIAN_POINT('Ctrl Pts',(-25.7995507955885,25.8631351799909,18.4031134955261));
#49687=CARTESIAN_POINT('Ctrl Pts',(-25.6891074234568,25.9656329454133,18.3945916135063));
#49688=CARTESIAN_POINT('Ctrl Pts',(-25.5611646820118,26.0686926170247,18.3849513563897));
#49689=CARTESIAN_POINT('Ctrl Pts',(-25.5503583709244,26.0772833513782,18.3841389057398));
#49690=CARTESIAN_POINT('Ctrl Pts',(-25.5313017932551,26.0922340213092,18.3827090160906));
#49691=CARTESIAN_POINT('Ctrl Pts',(-25.523075219718,26.0986239152174,18.3820926614613));
#49692=CARTESIAN_POINT('Ctrl Pts',(-25.5077119512946,26.110438176749,18.3809431908327));
#49693=CARTESIAN_POINT('Ctrl Pts',(-25.500583308482,26.1158728807192,18.3804104575248));
#49694=CARTESIAN_POINT('Ctrl Pts',(-25.4880697714028,26.1253306059875,18.3794763311537));
#49695=CARTESIAN_POINT('Ctrl Pts',(-25.4826947708341,26.1293666692643,18.3790754204742));
#49696=CARTESIAN_POINT('Ctrl Pts',(-25.4760872761785,26.1342959554673,18.3785829643391));
#49697=CARTESIAN_POINT('Ctrl Pts',(-25.4748666970248,26.1352051799269,18.3784920106688));
#49698=CARTESIAN_POINT('Ctrl Pts',(-25.468137130815,26.1402107081172,18.3779906320603));
#49699=CARTESIAN_POINT('Ctrl Pts',(-25.4626157401535,26.1442902432589,18.3775795890068));
#49700=CARTESIAN_POINT('Ctrl Pts',(-25.4522160684438,26.1519228969457,18.3768059535564));
#49701=CARTESIAN_POINT('Ctrl Pts',(-25.4473407530092,26.155480019719,18.3764435125562));
#49702=CARTESIAN_POINT('Ctrl Pts',(-25.4220335484386,26.1738359313111,18.3745632877946));
#49703=CARTESIAN_POINT('Ctrl Pts',(-25.4014388312545,26.1884078072986,18.3730370941155));
#49704=CARTESIAN_POINT('Ctrl Pts',(-25.3729454554866,26.2080704861453,18.3709299746131));
#49705=CARTESIAN_POINT('Ctrl Pts',(-25.365192099182,26.2133710301615,18.370357047914));
#49706=CARTESIAN_POINT('Ctrl Pts',(-25.3536600198904,26.2211811284998,18.3695055075776));
#49707=CARTESIAN_POINT('Ctrl Pts',(-25.3498989417305,26.2237167518059,18.3692278817039));
#49708=CARTESIAN_POINT('Ctrl Pts',(-25.3434577233645,26.2280395060532,18.3687525783677));
#49709=CARTESIAN_POINT('Ctrl Pts',(-25.3407802260418,26.2298305796603,18.3685550500762));
#49710=CARTESIAN_POINT('Ctrl Pts',(-25.3355712931256,26.2333037276535,18.3681708574594));
#49711=CARTESIAN_POINT('Ctrl Pts',(-25.333040154162,26.2349862416059,18.3679842100195));
#49712=CARTESIAN_POINT('Ctrl Pts',(-25.3269888512035,26.2389963690301,18.3675380784522));
#49713=CARTESIAN_POINT('Ctrl Pts',(-25.323466494768,26.2413206491456,18.3672784693663));
#49714=CARTESIAN_POINT('Ctrl Pts',(-25.3129219271122,26.2482489500659,18.366501521293));
#49715=CARTESIAN_POINT('Ctrl Pts',(-25.3058863174607,26.252832424912,18.3659834131772));
#49716=CARTESIAN_POINT('Ctrl Pts',(-25.246822548433,26.2909826164312,18.3616362055157));
#49717=CARTESIAN_POINT('Ctrl Pts',(-25.1938580202495,26.3230690341703,18.3577524073316));
#49718=CARTESIAN_POINT('Ctrl Pts',(-25.0585206447413,26.3998173825195,18.3478539267582));
#49719=CARTESIAN_POINT('Ctrl Pts',(-24.9750673048491,26.4424476633357,18.3417719692439));
#49720=CARTESIAN_POINT('Ctrl Pts',(-24.6005285548807,26.6136251948325,18.3145978660624));
#49721=CARTESIAN_POINT('Ctrl Pts',(-24.2932262725778,26.7022829520062,18.292403927592));
#49722=CARTESIAN_POINT('Ctrl Pts',(-23.9384789597551,26.7497810605417,18.2693512188369));
#49723=CARTESIAN_POINT('Ctrl Pts',(-23.8989221725548,26.7543331189928,18.2668188131076));
#49724=CARTESIAN_POINT('Ctrl Pts',(-23.853994149863,26.7586613098232,18.2639933266338));
#49725=CARTESIAN_POINT('Ctrl Pts',(-23.8486979942297,26.7591582898991,18.263661054207));
#49726=CARTESIAN_POINT('Ctrl Pts',(-23.8409610393328,26.7598649891623,18.2631768398688));
#49727=CARTESIAN_POINT('Ctrl Pts',(-23.83852122824,26.7600850385761,18.2630243179845));
#49728=CARTESIAN_POINT('Ctrl Pts',(-23.8342024290891,26.7604695922494,18.2627546419912));
#49729=CARTESIAN_POINT('Ctrl Pts',(-23.8323235463584,26.7606352289548,18.2626374235443));
#49730=CARTESIAN_POINT('Ctrl Pts',(-23.828400684816,26.7609775863254,18.2623929037031));
#49731=CARTESIAN_POINT('Ctrl Pts',(-23.8263566867247,26.7611540043577,18.2622656198565));
#49732=CARTESIAN_POINT('Ctrl Pts',(-23.8210858197778,26.7616038640724,18.261937705488));
#49733=CARTESIAN_POINT('Ctrl Pts',(-23.8178586947188,26.7618743948082,18.2617372401072));
#49734=CARTESIAN_POINT('Ctrl Pts',(-23.8041533776775,26.7630025142568,18.2608871447448));
#49735=CARTESIAN_POINT('Ctrl Pts',(-23.793671275944,26.7638137046344,18.2602401102242));
#49736=CARTESIAN_POINT('Ctrl Pts',(-23.6099874905405,26.7771247452182,18.2489537321667));
#49737=CARTESIAN_POINT('Ctrl Pts',(-23.4360299109877,26.7756586374206,18.2390672455414));
#49738=CARTESIAN_POINT('Ctrl Pts',(-23.0236863167386,26.7387604178823,18.2158190635991));
#49739=CARTESIAN_POINT('Ctrl Pts',(-22.7875207352575,26.6906487727123,18.2026029839764));
#49740=CARTESIAN_POINT('Ctrl Pts',(-22.5345226184829,26.6088578677429,18.1870643707998));
#49741=CARTESIAN_POINT('Ctrl Pts',(-22.5102418371693,26.6006871832642,18.1855592673859));
#49742=CARTESIAN_POINT('Ctrl Pts',(-22.4244526234141,26.5706750705763,18.1801885299608));
#49743=CARTESIAN_POINT('Ctrl Pts',(-22.3635164086128,26.5472567355454,18.1762761226659));
#49744=CARTESIAN_POINT('Ctrl Pts',(-22.2956262906693,26.5187707591597,18.1717912697586));
#49745=CARTESIAN_POINT('Ctrl Pts',(-22.2879289994945,26.5155057703646,18.1712809348704));
#49746=CARTESIAN_POINT('Ctrl Pts',(-22.2763134255835,26.5105253250946,18.1705079859855));
#49747=CARTESIAN_POINT('Ctrl Pts',(-22.2723856680729,26.5088319435059,18.1702461258786));
#49748=CARTESIAN_POINT('Ctrl Pts',(-22.2655682641414,26.5058766346074,18.1697907579196));
#49749=CARTESIAN_POINT('Ctrl Pts',(-22.262677069916,26.504618273294,18.1695973722789));
#49750=CARTESIAN_POINT('Ctrl Pts',(-22.2566581880681,26.5019881060544,18.1691942205861));
#49751=CARTESIAN_POINT('Ctrl Pts',(-22.253530826812,26.5006155681274,18.1689844296504));
#49752=CARTESIAN_POINT('Ctrl Pts',(-22.2461594411969,26.49736642621,18.1684891889923));
#49753=CARTESIAN_POINT('Ctrl Pts',(-22.2419172850053,26.4954856256687,18.1682035954275));
#49754=CARTESIAN_POINT('Ctrl Pts',(-22.2280074702871,26.4892825937356,18.1672652081352));
#49755=CARTESIAN_POINT('Ctrl Pts',(-22.2183571290502,26.4849219066182,18.1666110920534));
#49756=CARTESIAN_POINT('Ctrl Pts',(-22.1958266452942,26.4746070637364,18.1650766336545));
#49757=CARTESIAN_POINT('Ctrl Pts',(-22.1829640647156,26.468615283051,18.1641949979318));
#49758=CARTESIAN_POINT('Ctrl Pts',(-22.1381767416871,26.4473909025699,18.1611052362202));
#49759=CARTESIAN_POINT('Ctrl Pts',(-22.1064706926468,26.4317211923938,18.1588823327108));
#49760=CARTESIAN_POINT('Ctrl Pts',(-22.0750359582753,26.4155367451729,18.1566419298442));
#49761=CARTESIAN_POINT('',(-26.77300128901,23.5530826764189,18.3151727310146));
#49762=CARTESIAN_POINT('Ctrl Pts',(-22.075036043603,26.4155367891046,17.9090429972639));
#49763=CARTESIAN_POINT('Ctrl Pts',(-22.1593709209768,26.4589573332622,17.9144332697937));
#49764=CARTESIAN_POINT('Ctrl Pts',(-22.2456017632402,26.4986436538479,17.9197342182951));
#49765=CARTESIAN_POINT('Ctrl Pts',(-22.5828848797567,26.6361659770632,17.9400867616632));
#49766=CARTESIAN_POINT('Ctrl Pts',(-22.8440119014111,26.7061771069153,17.9551681507764));
#49767=CARTESIAN_POINT('Ctrl Pts',(-23.1279342739914,26.7452586977883,17.9725320114714));
#49768=CARTESIAN_POINT('Ctrl Pts',(-23.1450985728928,26.7474806067005,17.9735848827722));
#49769=CARTESIAN_POINT('Ctrl Pts',(-23.1680935824315,26.7502691564238,17.9749998907517));
#49770=CARTESIAN_POINT('Ctrl Pts',(-23.1739093659091,26.7509583416521,17.9753581499044));
#49771=CARTESIAN_POINT('Ctrl Pts',(-23.1830070740183,26.7520113045491,17.9759191879348));
#49772=CARTESIAN_POINT('Ctrl Pts',(-23.1862877543506,26.7523858996942,17.9761216247724));
#49773=CARTESIAN_POINT('Ctrl Pts',(-23.1925680715832,26.7530932236497,17.9765093952954));
#49774=CARTESIAN_POINT('Ctrl Pts',(-23.1955676132172,26.7534267822709,17.9766947025629));
#49775=CARTESIAN_POINT('Ctrl Pts',(-23.2025871946223,26.7541974013315,17.9771286078435));
#49776=CARTESIAN_POINT('Ctrl Pts',(-23.2066075906324,26.754631109285,17.97737731143));
#49777=CARTESIAN_POINT('Ctrl Pts',(-23.2181405715713,26.755853297414,17.9780912936677));
#49778=CARTESIAN_POINT('Ctrl Pts',(-23.2256550890969,26.7566229285671,17.9785571664226));
#49779=CARTESIAN_POINT('Ctrl Pts',(-23.2738374529727,26.7613866139933,17.9815486375649));
#49780=CARTESIAN_POINT('Ctrl Pts',(-23.3145739023543,26.7646331447969,17.984097697682));
#49781=CARTESIAN_POINT('Ctrl Pts',(-23.6362581363628,26.784122380873,18.0043946255653));
#49782=CARTESIAN_POINT('Ctrl Pts',(-23.9181230683341,26.7642713426485,18.0233460331938));
#49783=CARTESIAN_POINT('Ctrl Pts',(-24.2582316810359,26.6949644254206,18.0468281372735));
#49784=CARTESIAN_POINT('Ctrl Pts',(-24.3222918716227,26.6798536289996,18.0512706168892));
#49785=CARTESIAN_POINT('Ctrl Pts',(-24.4389410612335,26.6485379508687,18.0593543410877));
#49786=CARTESIAN_POINT('Ctrl Pts',(-24.4916653341009,26.632927071347,18.0630058012206));
#49787=CARTESIAN_POINT('Ctrl Pts',(-24.556180404919,26.6120153452683,18.0674517491555));
#49788=CARTESIAN_POINT('Ctrl Pts',(-24.5683706116794,26.6079833892319,18.0682908242658));
#49789=CARTESIAN_POINT('Ctrl Pts',(-24.5844689418244,26.6025518622694,18.0693973060509));
#49790=CARTESIAN_POINT('Ctrl Pts',(-24.5883987711514,26.6012174892516,18.0696672874815));
#49791=CARTESIAN_POINT('Ctrl Pts',(-24.6434553177094,26.5824043545499,18.0734478277039));
#49792=CARTESIAN_POINT('Ctrl Pts',(-24.6941410387773,26.5636487812901,18.076905654466));
#49793=CARTESIAN_POINT('Ctrl Pts',(-24.7491707744381,26.5416969518634,18.0806165318587));
#49794=CARTESIAN_POINT('Ctrl Pts',(-24.7540022074882,26.5397560675131,18.0809419638411));
#49795=CARTESIAN_POINT('Ctrl Pts',(-24.7611639354832,26.5368588798842,18.0814237840309));
#49796=CARTESIAN_POINT('Ctrl Pts',(-24.7634978168552,26.5359115519134,18.0815807101432));
#49797=CARTESIAN_POINT('Ctrl Pts',(-24.7674893370015,26.5342859313238,18.0818489348554));
#49798=CARTESIAN_POINT('Ctrl Pts',(-24.7691475204817,26.5336089932396,18.0819603157734));
#49799=CARTESIAN_POINT('Ctrl Pts',(-24.7723792126486,26.5322865406882,18.0821772975571));
#49800=CARTESIAN_POINT('Ctrl Pts',(-24.7739527703477,26.5316411647018,18.0822829062019));
#49801=CARTESIAN_POINT('Ctrl Pts',(-24.7772125016097,26.5303012092041,18.0825015937837));
#49802=CARTESIAN_POINT('Ctrl Pts',(-24.7788985990924,26.5296064430667,18.0826146613269));
#49803=CARTESIAN_POINT('Ctrl Pts',(-24.7827541842522,26.5280138974851,18.0828731024805));
#49804=CARTESIAN_POINT('Ctrl Pts',(-24.7849232855657,26.5271151762872,18.0830184187132));
#49805=CARTESIAN_POINT('Ctrl Pts',(-24.7958446118895,26.522576165691,18.0837496888347));
#49806=CARTESIAN_POINT('Ctrl Pts',(-24.8045818495212,26.5188995944528,18.0843334526516));
#49807=CARTESIAN_POINT('Ctrl Pts',(-24.8267748971703,26.5094454360285,18.0858133331251));
#49808=CARTESIAN_POINT('Ctrl Pts',(-24.8402079436402,26.5036145224046,18.0867063433077));
#49809=CARTESIAN_POINT('Ctrl Pts',(-24.8952502273871,26.4792749973688,18.0903560648737));
#49810=CARTESIAN_POINT('Ctrl Pts',(-24.9365066850428,26.4599761078044,18.0930694824104));
#49811=CARTESIAN_POINT('Ctrl Pts',(-25.0449809601033,26.4064029766522,18.1001801172965));
#49812=CARTESIAN_POINT('Ctrl Pts',(-25.1114298614343,26.3706310768825,18.1045114866027));
#49813=CARTESIAN_POINT('Ctrl Pts',(-25.2346539171695,26.2986041549622,18.1126083357575));
#49814=CARTESIAN_POINT('Ctrl Pts',(-25.2916660278783,26.2628387740627,18.1163822846199));
#49815=CARTESIAN_POINT('Ctrl Pts',(-25.4351209230382,26.1664572524652,18.1260501961543));
#49816=CARTESIAN_POINT('Ctrl Pts',(-25.51977927485,26.1033330210452,18.1319252629363));
#49817=CARTESIAN_POINT('Ctrl Pts',(-25.7494657981449,25.9138368255922,18.1487185666196));
#49818=CARTESIAN_POINT('Ctrl Pts',(-25.8864794801201,25.7785022074225,18.1598048861253));
#49819=CARTESIAN_POINT('Ctrl Pts',(-26.0188124193252,25.6220852798301,18.1722542236531));
#49820=CARTESIAN_POINT('Ctrl Pts',(-26.026957756158,25.6123412977142,18.1730282313038));
#49821=CARTESIAN_POINT('Ctrl Pts',(-26.0379969365708,25.5989757495079,18.1740879495156));
#49822=CARTESIAN_POINT('Ctrl Pts',(-26.0409409519824,25.5953956171238,18.1743716174894));
#49823=CARTESIAN_POINT('Ctrl Pts',(-26.0459350951808,25.5892956056901,18.174854626741));
#49824=CARTESIAN_POINT('Ctrl Pts',(-26.047989161613,25.5867789476161,18.1750538081315));
#49825=CARTESIAN_POINT('Ctrl Pts',(-26.0519521045666,25.5819085049629,18.1754391050685));
#49826=CARTESIAN_POINT('Ctrl Pts',(-26.0538614734124,25.5795551245766,18.1756252003789));
#49827=CARTESIAN_POINT('Ctrl Pts',(-26.0583803260914,25.5739693565596,18.1760667146648));
#49828=CARTESIAN_POINT('Ctrl Pts',(-26.0609868802473,25.5707346155073,18.1763222513332));
#49829=CARTESIAN_POINT('Ctrl Pts',(-26.0686429142025,25.5611957638535,18.1770753744441));
#49830=CARTESIAN_POINT('Ctrl Pts',(-26.0736749293973,25.5548777342057,18.1775736611483));
#49831=CARTESIAN_POINT('Ctrl Pts',(-26.1098001095368,25.509168610678,18.181174831277));
#49832=CARTESIAN_POINT('Ctrl Pts',(-26.139991704264,25.4690767984572,18.1843133826985));
#49833=CARTESIAN_POINT('Ctrl Pts',(-26.2255943349372,25.3497018129674,18.1936079572374));
#49834=CARTESIAN_POINT('Ctrl Pts',(-26.2783832871799,25.268615414298,18.1998599632387));
#49835=CARTESIAN_POINT('Ctrl Pts',(-26.3759193915409,25.1029450781843,18.2125074272295));
#49836=CARTESIAN_POINT('Ctrl Pts',(-26.4207070191574,25.0184951409874,18.2188939977021));
#49837=CARTESIAN_POINT('Ctrl Pts',(-26.4797474821498,24.8941101254458,18.2281720852229));
#49838=CARTESIAN_POINT('Ctrl Pts',(-26.4970713378648,24.8556845488706,18.2310209836414));
#49839=CARTESIAN_POINT('Ctrl Pts',(-26.5221377235852,24.7970419296003,18.2353365054403));
#49840=CARTESIAN_POINT('Ctrl Pts',(-26.530438581115,24.7770681274158,18.2368007952246));
#49841=CARTESIAN_POINT('Ctrl Pts',(-26.5480357324656,24.7334925057867,18.239981837975));
#49842=CARTESIAN_POINT('Ctrl Pts',(-26.5572557570492,24.7098613301621,18.2416984126455));
#49843=CARTESIAN_POINT('Ctrl Pts',(-26.6197949787713,24.5438083895534,18.2536931436854));
#49844=CARTESIAN_POINT('Ctrl Pts',(-26.6632594866092,24.397861847395,18.2639001399837));
#49845=CARTESIAN_POINT('Ctrl Pts',(-26.6970703684272,24.2457157861125,18.2738744715837));
#49846=CARTESIAN_POINT('Ctrl Pts',(-26.6978777948418,24.2420522418077,18.2741142507117));
#49847=CARTESIAN_POINT('Ctrl Pts',(-26.6997733447593,24.2333795229206,18.2746809351109));
#49848=CARTESIAN_POINT('Ctrl Pts',(-26.7008559218518,24.2283691269678,18.2750075739379));
#49849=CARTESIAN_POINT('Ctrl Pts',(-26.7035826174974,24.2156019158064,18.2758379621959));
#49850=CARTESIAN_POINT('Ctrl Pts',(-26.7052100834911,24.207841523553,18.2763408869864));
#49851=CARTESIAN_POINT('Ctrl Pts',(-26.7085385716168,24.1916731712987,18.2773848129824));
#49852=CARTESIAN_POINT('Ctrl Pts',(-26.7102347026844,24.1832642454433,18.2779255584563));
#49853=CARTESIAN_POINT('Ctrl Pts',(-26.713520599817,24.1666313511673,18.2789907046412));
#49854=CARTESIAN_POINT('Ctrl Pts',(-26.7151119196564,24.1584077569837,18.2795151862882));
#49855=CARTESIAN_POINT('Ctrl Pts',(-26.7172441225985,24.1471539460552,18.2802299089252));
#49856=CARTESIAN_POINT('Ctrl Pts',(-26.7178127348494,24.1441291139079,18.2804217162835));
#49857=CARTESIAN_POINT('Ctrl Pts',(-26.7187072817134,24.1393325811412,18.2807253916173));
#49858=CARTESIAN_POINT('Ctrl Pts',(-26.7190360637595,24.1375614236127,18.2808374230448));
#49859=CARTESIAN_POINT('Ctrl Pts',(-26.7196715892146,24.1341217621749,18.2810547913491));
#49860=CARTESIAN_POINT('Ctrl Pts',(-26.7199784981517,24.1324533029505,18.2811601369571));
#49861=CARTESIAN_POINT('Ctrl Pts',(-26.7206111286237,24.1289987847561,18.2813780636562));
#49862=CARTESIAN_POINT('Ctrl Pts',(-26.7209366575876,24.1272126970475,18.2814906333223));
#49863=CARTESIAN_POINT('Ctrl Pts',(-26.7216752316503,24.1231408419372,18.2817470283648));
#49864=CARTESIAN_POINT('Ctrl Pts',(-26.7220873157904,24.1208548978728,18.2818907986511));
#49865=CARTESIAN_POINT('Ctrl Pts',(-26.7231311708739,24.1150282739246,18.2822568245388));
#49866=CARTESIAN_POINT('Ctrl Pts',(-26.7237594888756,24.1114869666606,18.2824788843357));
#49867=CARTESIAN_POINT('Ctrl Pts',(-26.7255493011093,24.1013001701885,18.2831165126908));
#49868=CARTESIAN_POINT('Ctrl Pts',(-26.726695867416,24.0946520270956,18.283531248641));
#49869=CARTESIAN_POINT('Ctrl Pts',(-26.7577276780134,23.9112840378948,18.2949332019275));
#49870=CARTESIAN_POINT('Ctrl Pts',(-26.7728438545236,23.7323568284758,18.3051144236182));
#49871=CARTESIAN_POINT('Ctrl Pts',(-26.77300128901,23.5530826764189,18.3151727310146));
#49872=CARTESIAN_POINT('Ctrl Pts',(-26.7730012867183,23.5530852849271,18.3151725846623));
#49873=CARTESIAN_POINT('Ctrl Pts',(-26.7732621727642,23.2562821006184,18.3318249468147));
#49874=CARTESIAN_POINT('Ctrl Pts',(-26.732525495111,22.9608856091882,18.3481471325133));
#49875=CARTESIAN_POINT('Ctrl Pts',(-26.6460420560006,22.6543306208819,18.3672803403713));
#49876=CARTESIAN_POINT('Ctrl Pts',(-26.6399368259007,22.6334975065806,18.3685909740539));
#49877=CARTESIAN_POINT('Ctrl Pts',(-26.6307278710816,22.6032107165283,18.3705121396507));
#49878=CARTESIAN_POINT('Ctrl Pts',(-26.6277900230134,22.5937069225832,18.3711172685335));
#49879=CARTESIAN_POINT('Ctrl Pts',(-26.6224256344382,22.576633936743,18.3722085196104));
#49880=CARTESIAN_POINT('Ctrl Pts',(-26.6200149931421,22.569059803348,18.372694117643));
#49881=CARTESIAN_POINT('Ctrl Pts',(-26.6163100688392,22.557566389597,18.3734332742031));
#49882=CARTESIAN_POINT('Ctrl Pts',(-26.6150362236821,22.553640511463,18.3736861582342));
#49883=CARTESIAN_POINT('Ctrl Pts',(-26.6127156377682,22.5465351955185,18.3741445838738));
#49884=CARTESIAN_POINT('Ctrl Pts',(-26.6116714769357,22.5433549159534,18.3743500399861));
#49885=CARTESIAN_POINT('Ctrl Pts',(-26.6095758221902,22.5370054165498,18.3747607770218));
#49886=CARTESIAN_POINT('Ctrl Pts',(-26.6085243537364,22.5338361925446,18.3749660568948));
#49887=CARTESIAN_POINT('Ctrl Pts',(-26.6055568177495,22.5249380560657,18.375543173812));
#49888=CARTESIAN_POINT('Ctrl Pts',(-26.6036295725149,22.5192129106733,18.3759153807552));
#49889=CARTESIAN_POINT('Ctrl Pts',(-26.595676057549,22.4958037894202,18.3774409195437));
#49890=CARTESIAN_POINT('Ctrl Pts',(-26.5895122598523,22.4781672351598,18.3785988086754));
#49891=CARTESIAN_POINT('Ctrl Pts',(-26.4789744263992,22.1704998815299,18.3989508001601));
#49892=CARTESIAN_POINT('Ctrl Pts',(-26.3336965646268,21.8969295658616,18.4196657769884));
#49893=CARTESIAN_POINT('Ctrl Pts',(-26.1133484598985,21.5955362451533,18.4449212373623));
#49894=CARTESIAN_POINT('Ctrl Pts',(-26.0732400943779,21.5440345327491,18.4493260544867));
#49895=CARTESIAN_POINT('Ctrl Pts',(-25.9770859141895,21.4280144950163,18.4594080168989));
#49896=CARTESIAN_POINT('Ctrl Pts',(-25.9199790797709,21.3644316439589,18.4650544604467));
#49897=CARTESIAN_POINT('Ctrl Pts',(-25.8320286235718,21.2740117349124,18.4731801369943));
#49898=CARTESIAN_POINT('Ctrl Pts',(-25.8030965238802,21.2453732219491,18.4757689307404));
#49899=CARTESIAN_POINT('Ctrl Pts',(-25.7711441438369,21.2149217665841,18.4785305447537));
#49900=CARTESIAN_POINT('Ctrl Pts',(-25.7686565191387,21.2125585645322,18.4787449208681));
#49901=CARTESIAN_POINT('Ctrl Pts',(-25.7645289691869,21.2086499825209,18.4790995764501));
#49902=CARTESIAN_POINT('Ctrl Pts',(-25.7628911965901,21.2071023490106,18.4792400289443));
#49903=CARTESIAN_POINT('Ctrl Pts',(-25.759946340738,21.2043254116858,18.479492085177));
#49904=CARTESIAN_POINT('Ctrl Pts',(-25.7586398535715,21.2030954814041,18.4796037374905));
#49905=CARTESIAN_POINT('Ctrl Pts',(-25.7561035657478,21.2007118060244,18.4798201527281));
#49906=CARTESIAN_POINT('Ctrl Pts',(-25.7548738879936,21.1995579361732,18.4799249252746));
#49907=CARTESIAN_POINT('Ctrl Pts',(-25.7523041854047,21.1971504420933,18.480143552967));
#49908=CARTESIAN_POINT('Ctrl Pts',(-25.7509639992447,21.1958970006996,18.4802573939115));
#49909=CARTESIAN_POINT('Ctrl Pts',(-25.7472501258108,21.1924294529701,18.4805723680604));
#49910=CARTESIAN_POINT('Ctrl Pts',(-25.7448741544107,21.1902177793136,18.4807733126687));
#49911=CARTESIAN_POINT('Ctrl Pts',(-25.7355151397509,21.1815322930234,18.4815626511543));
#49912=CARTESIAN_POINT('Ctrl Pts',(-25.7285066689296,21.1750857682295,18.4821489657017));
#49913=CARTESIAN_POINT('Ctrl Pts',(-25.6002702175479,21.0581764412491,18.4927924934992));
#49914=CARTESIAN_POINT('Ctrl Pts',(-25.4707933282463,20.9570777945746,18.5021745934769));
#49915=CARTESIAN_POINT('Ctrl Pts',(-25.2467827176668,20.8081892338114,18.5173125950322));
#49916=CARTESIAN_POINT('Ctrl Pts',(-25.1566178315228,20.7544133373306,18.52314633299));
#49917=CARTESIAN_POINT('Ctrl Pts',(-24.9567521127659,20.6480754642722,18.5358269566377));
#49918=CARTESIAN_POINT('Ctrl Pts',(-24.8463799447167,20.5971315203825,18.5426798235965));
#49919=CARTESIAN_POINT('Ctrl Pts',(-24.6604515300494,20.5237485305611,18.5542466855335));
#49920=CARTESIAN_POINT('Ctrl Pts',(-24.5864794401575,20.497630599832,18.5588530952495));
#49921=CARTESIAN_POINT('Ctrl Pts',(-24.4737050919773,20.4623840234399,18.5659262681683));
#49922=CARTESIAN_POINT('Ctrl Pts',(-24.4355631785849,20.451233106415,18.5683268352314));
#49923=CARTESIAN_POINT('Ctrl Pts',(-24.3899954388643,20.4388210968377,18.5712077364301));
#49924=CARTESIAN_POINT('Ctrl Pts',(-24.3827579820393,20.4368768078849,18.5716656896485));
#49925=CARTESIAN_POINT('Ctrl Pts',(-24.3716173413197,20.433925581532,18.5723712308527));
#49926=CARTESIAN_POINT('Ctrl Pts',(-24.3677189062523,20.432900684849,18.5726182353697));
#49927=CARTESIAN_POINT('Ctrl Pts',(-24.3608994532933,20.431121525746,18.573050520196));
#49928=CARTESIAN_POINT('Ctrl Pts',(-24.3579792738536,20.4303640443171,18.5732356958418));
#49929=CARTESIAN_POINT('Ctrl Pts',(-24.3518538774911,20.4287843203488,18.573624261377));
#49930=CARTESIAN_POINT('Ctrl Pts',(-24.3486484507918,20.4279629121581,18.5738276780635));
#49931=CARTESIAN_POINT('Ctrl Pts',(-24.3397325897602,20.4256928013833,18.5743937046577));
#49932=CARTESIAN_POINT('Ctrl Pts',(-24.3340194607758,20.4242548236809,18.5747566613333));
#49933=CARTESIAN_POINT('Ctrl Pts',(-24.3112653722913,20.4185939860938,18.576203279548));
#49934=CARTESIAN_POINT('Ctrl Pts',(-24.2941942211302,20.4144948030307,18.5772909298422));
#49935=CARTESIAN_POINT('Ctrl Pts',(-24.0121253996711,20.349196442041,18.5953029694333));
#49936=CARTESIAN_POINT('Ctrl Pts',(-23.7405203953988,20.3216583432215,18.6133805773614));
#49937=CARTESIAN_POINT('Ctrl Pts',(-23.3825897203145,20.3307128718005,18.637609342451));
#49938=CARTESIAN_POINT('Ctrl Pts',(-23.2965473425115,20.3363482818765,18.6434515911861));
#49939=CARTESIAN_POINT('Ctrl Pts',(-23.1170846443395,20.3553549505097,18.6555761112768));
#49940=CARTESIAN_POINT('Ctrl Pts',(-23.0238090015002,20.3693933779458,18.6618428110768));
#49941=CARTESIAN_POINT('Ctrl Pts',(-22.899165600216,20.3937871060456,18.6700628548338));
#49942=CARTESIAN_POINT('Ctrl Pts',(-22.8671506764707,20.4005604483396,18.672160164801));
#49943=CARTESIAN_POINT('Ctrl Pts',(-22.8182797019714,20.4116802458582,18.6753345097436));
#49944=CARTESIAN_POINT('Ctrl Pts',(-22.8013473819751,20.4156773888759,18.6764292834792));
#49945=CARTESIAN_POINT('Ctrl Pts',(-22.780695277739,20.4207295457401,18.6777576922173));
#49946=CARTESIAN_POINT('Ctrl Pts',(-22.7769443718859,20.4216542869404,18.6779986845668));
#49947=CARTESIAN_POINT('Ctrl Pts',(-22.7714365377854,20.4230226882679,18.6783521404281));
#49948=CARTESIAN_POINT('Ctrl Pts',(-22.7696783246011,20.4234610846603,18.6784649081997));
#49949=CARTESIAN_POINT('Ctrl Pts',(-22.7662764963319,20.4243123514623,18.6786829713214));
#49950=CARTESIAN_POINT('Ctrl Pts',(-22.7646328365011,20.4247250355764,18.6787882773996));
#49951=CARTESIAN_POINT('Ctrl Pts',(-22.7612380125919,20.4255802427166,18.6790056620811));
#49952=CARTESIAN_POINT('Ctrl Pts',(-22.7594868993271,20.4260229403287,18.6791177300608));
#49953=CARTESIAN_POINT('Ctrl Pts',(-22.7547294404244,20.4272299259531,18.6794220294055));
#49954=CARTESIAN_POINT('Ctrl Pts',(-22.7517238146208,20.4279970852396,18.6796140933608));
#49955=CARTESIAN_POINT('Ctrl Pts',(-22.7404520246233,20.4308914504133,18.6803337044668));
#49956=CARTESIAN_POINT('Ctrl Pts',(-22.7321931188203,20.4330471779246,18.6808596089252));
#49957=CARTESIAN_POINT('Ctrl Pts',(-22.5903807423052,20.4706652579848,18.6898679916159));
#49958=CARTESIAN_POINT('Ctrl Pts',(-22.4592159993945,20.5146534782014,18.6978688355037));
#49959=CARTESIAN_POINT('Ctrl Pts',(-22.2030351178869,20.6193293121198,18.7135601885615));
#49960=CARTESIAN_POINT('Ctrl Pts',(-22.0783139288904,20.6799381972539,18.7212359910517));
#49961=CARTESIAN_POINT('Ctrl Pts',(-21.8245308789571,20.8241698444795,18.7375998408844));
#49962=CARTESIAN_POINT('Ctrl Pts',(-21.6967770383129,20.9093693211074,18.7462908924542));
#49963=CARTESIAN_POINT('Ctrl Pts',(-21.5345049896295,21.0351817804683,18.758362427032));
#49964=CARTESIAN_POINT('Ctrl Pts',(-21.4942072190887,21.0680163905278,18.7614522388853));
#49965=CARTESIAN_POINT('Ctrl Pts',(-21.4402540199457,21.1141929007656,18.7657273202795));
#49966=CARTESIAN_POINT('Ctrl Pts',(-21.4258957077714,21.1267038307557,18.766878870827));
#49967=CARTESIAN_POINT('Ctrl Pts',(-21.4016282934038,21.1482302826906,18.7688493901622));
#49968=CARTESIAN_POINT('Ctrl Pts',(-21.3916628719584,21.1571817691656,18.7696656827057));
#49969=CARTESIAN_POINT('Ctrl Pts',(-21.3779779927971,21.1696293065327,18.7707966233747));
#49970=CARTESIAN_POINT('Ctrl Pts',(-21.3742105029472,21.1730725424693,18.7711090296579));
#49971=CARTESIAN_POINT('Ctrl Pts',(-21.3678694926731,21.1788955110008,18.7716366269148));
#49972=CARTESIAN_POINT('Ctrl Pts',(-21.3652916374998,21.1812705268479,18.7718516164624));
#49973=CARTESIAN_POINT('Ctrl Pts',(-21.3602023552384,21.1859747308603,18.7722770518383));
#49974=CARTESIAN_POINT('Ctrl Pts',(-21.3576907563221,21.1883037270129,18.772487489294));
#49975=CARTESIAN_POINT('Ctrl Pts',(-21.3521683077166,21.1934410715056,18.7729512600517));
#49976=CARTESIAN_POINT('Ctrl Pts',(-21.3491591203794,21.1962511916357,18.7732046693508));
#49977=CARTESIAN_POINT('Ctrl Pts',(-21.338694461284,21.206061190054,18.7740883688125));
#49978=CARTESIAN_POINT('Ctrl Pts',(-21.3312669887428,21.2130907270002,18.7747199380871));
#49979=CARTESIAN_POINT('Ctrl Pts',(-21.2567314689116,21.2843085072664,18.7811021342728));
#49980=CARTESIAN_POINT('Ctrl Pts',(-21.1924002714926,21.3513275601838,18.786976779649));
#49981=CARTESIAN_POINT('Ctrl Pts',(-21.0245305144246,21.5420586050068,18.8033763816188));
#49982=CARTESIAN_POINT('Ctrl Pts',(-20.9272497692448,21.6709016278839,18.8141281244192));
#49983=CARTESIAN_POINT('Ctrl Pts',(-20.7633689273673,21.9256084155561,18.8345781253659));
#49984=CARTESIAN_POINT('Ctrl Pts',(-20.6946504529148,22.0496770256632,18.8442204537916));
#49985=CARTESIAN_POINT('Ctrl Pts',(-20.608087421323,22.2335991202733,18.8577764202769));
#49986=CARTESIAN_POINT('Ctrl Pts',(-20.5834584653595,22.2900757257041,18.8618435316533));
#49987=CARTESIAN_POINT('Ctrl Pts',(-20.5410451240753,22.3954824301734,18.8692186858429));
#49988=CARTESIAN_POINT('Ctrl Pts',(-20.5227977498563,22.4442048250223,18.8725452832844));
#49989=CARTESIAN_POINT('Ctrl Pts',(-20.5038544929749,22.4987728638809,18.8761637403054));
#49990=CARTESIAN_POINT('Ctrl Pts',(-20.5019867559543,22.5041998256637,18.8765224406163));
#49991=CARTESIAN_POINT('Ctrl Pts',(-20.4992878364492,22.5121105134405,18.8770435777598));
#49992=CARTESIAN_POINT('Ctrl Pts',(-20.4984451817377,22.5145902698713,18.8772066913998));
#49993=CARTESIAN_POINT('Ctrl Pts',(-20.49699098988,22.5188868378188,18.8774888807997));
#49994=CARTESIAN_POINT('Ctrl Pts',(-20.4963780500238,22.5207031703242,18.8776080404735));
#49995=CARTESIAN_POINT('Ctrl Pts',(-20.495208311564,22.5241797068842,18.8778358609589));
#49996=CARTESIAN_POINT('Ctrl Pts',(-20.4946512462187,22.5258398155485,18.8779445377943));
#49997=CARTESIAN_POINT('Ctrl Pts',(-20.4933445366224,22.529744485591,18.8781998915076));
#49998=CARTESIAN_POINT('Ctrl Pts',(-20.4925960097676,22.5319894239958,18.8783465015648));
#49999=CARTESIAN_POINT('Ctrl Pts',(-20.490399470245,22.5386014195644,18.8787777213208));
#50000=CARTESIAN_POINT('Ctrl Pts',(-20.4889583279969,22.5429707789737,18.879061924823));
#50001=CARTESIAN_POINT('Ctrl Pts',(-20.4704684067996,22.5994360673582,18.8827251092045));
#50002=CARTESIAN_POINT('Ctrl Pts',(-20.4547408247555,22.6519595033828,18.8860273484791));
#50003=CARTESIAN_POINT('Ctrl Pts',(-20.4357700432927,22.7217463307329,18.890308460098));
#50004=CARTESIAN_POINT('Ctrl Pts',(-20.4313178155637,22.7386676901932,18.8913383433506));
#50005=CARTESIAN_POINT('Ctrl Pts',(-20.4136595489179,22.8080727210672,18.8955322877156));
#50006=CARTESIAN_POINT('Ctrl Pts',(-20.40163819652,22.8608508378501,18.8986510384199));
#50007=CARTESIAN_POINT('Ctrl Pts',(-20.3449352062036,23.1423682602968,18.915030973668));
#50008=CARTESIAN_POINT('Ctrl Pts',(-20.3238344023615,23.3751464847635,18.9277386686169));
#50009=CARTESIAN_POINT('Ctrl Pts',(-20.330475670023,23.744618609732,18.9488393677481));
#50010=CARTESIAN_POINT('Ctrl Pts',(-20.3415920672979,23.880755601025,18.956803959716));
#50011=CARTESIAN_POINT('Ctrl Pts',(-20.3644152311688,24.0371027580157,18.9663551127334));
#50012=CARTESIAN_POINT('Ctrl Pts',(-20.3677436420847,24.0584056392652,18.9676650689775));
#50013=CARTESIAN_POINT('Ctrl Pts',(-20.3722905562745,24.0857081101304,18.9693554722631));
#50014=CARTESIAN_POINT('Ctrl Pts',(-20.3733127918394,24.0917401882549,18.9697296653212));
#50015=CARTESIAN_POINT('Ctrl Pts',(-20.3749854454469,24.1014425053354,18.9703327146693));
#50016=CARTESIAN_POINT('Ctrl Pts',(-20.3756250686452,24.1051146106994,18.97056122673));
#50017=CARTESIAN_POINT('Ctrl Pts',(-20.3768539265151,24.1120978538251,18.9709963082669));
#50018=CARTESIAN_POINT('Ctrl Pts',(-20.3774419769011,24.1154091972396,18.9712028397155));
#50019=CARTESIAN_POINT('Ctrl Pts',(-20.3787922663608,24.1229442187455,18.9716733154238));
#50020=CARTESIAN_POINT('Ctrl Pts',(-20.3795577604538,24.1271673003994,18.9719373632407));
#50021=CARTESIAN_POINT('Ctrl Pts',(-20.3819096868659,24.1399963400945,18.9727406140464));
#50022=CARTESIAN_POINT('Ctrl Pts',(-20.3835227281266,24.1485973241805,18.9732806658422));
#50023=CARTESIAN_POINT('Ctrl Pts',(-20.3952090735637,24.2095395882958,18.9771181766755));
#50024=CARTESIAN_POINT('Ctrl Pts',(-20.4065439988443,24.2616277887642,18.9804558235301));
#50025=CARTESIAN_POINT('Ctrl Pts',(-20.4221885535364,24.3258144965168,18.9846439589303));
#50026=CARTESIAN_POINT('Ctrl Pts',(-20.4252859842404,24.3382022017755,18.9854557414291));
#50027=CARTESIAN_POINT('Ctrl Pts',(-20.4328415525951,24.3676741434262,18.9873954510713));
#50028=CARTESIAN_POINT('Ctrl Pts',(-20.4373665964263,24.3847406613282,18.9885254237405));
#50029=CARTESIAN_POINT('Ctrl Pts',(-20.4498479845517,24.4303004588519,18.9915600234238));
#50030=CARTESIAN_POINT('Ctrl Pts',(-20.4580566691105,24.4587223277285,18.9934721549165));
#50031=CARTESIAN_POINT('Ctrl Pts',(-20.4834009050462,24.5421484494063,18.9991407505608));
#50032=CARTESIAN_POINT('Ctrl Pts',(-20.5016207954039,24.5968089696668,19.0029273106996));
#50033=CARTESIAN_POINT('Ctrl Pts',(-20.5795558501787,24.8112748608555,19.0180597082608));
#50034=CARTESIAN_POINT('Ctrl Pts',(-20.6504514343432,24.9667139841629,19.0296612606917));
#50035=CARTESIAN_POINT('Ctrl Pts',(-20.8147837710453,25.2624029041648,19.0525020611909));
#50036=CARTESIAN_POINT('Ctrl Pts',(-20.9075920906761,25.4024430332882,19.0637055765542));
#50037=CARTESIAN_POINT('Ctrl Pts',(-21.0155672199061,25.5406156962828,19.0747119513928));
#50038=CARTESIAN_POINT('Ctrl Pts',(-21.02026130586,25.5465790472532,19.0751868492034));
#50039=CARTESIAN_POINT('Ctrl Pts',(-21.026754427525,25.5547682014029,19.0758387657944));
#50040=CARTESIAN_POINT('Ctrl Pts',(-21.0285353799432,25.5570082115343,19.0760170626121));
#50041=CARTESIAN_POINT('Ctrl Pts',(-21.0315455938497,25.5607840020739,19.0763175565553));
#50042=CARTESIAN_POINT('Ctrl Pts',(-21.032773277803,25.5623210291393,19.0764398671393));
#50043=CARTESIAN_POINT('Ctrl Pts',(-21.0351945148126,25.5653466671435,19.0766806087399));
#50044=CARTESIAN_POINT('Ctrl Pts',(-21.0363879825817,25.5668353422307,19.076799045586));
#50045=CARTESIAN_POINT('Ctrl Pts',(-21.0390230075859,25.5701161730401,19.0770600374898));
#50046=CARTESIAN_POINT('Ctrl Pts',(-21.0404651652092,25.5719078503611,19.0772025490961));
#50047=CARTESIAN_POINT('Ctrl Pts',(-21.0455133438864,25.5781657729807,19.0777002553674));
#50048=CARTESIAN_POINT('Ctrl Pts',(-21.0491294061749,25.5826239606709,19.0780547276707));
#50049=CARTESIAN_POINT('Ctrl Pts',(-21.0859741687391,25.6278020405361,19.081646143433));
#50050=CARTESIAN_POINT('Ctrl Pts',(-21.120184686196,25.6677158398477,19.0848132050792));
#50051=CARTESIAN_POINT('Ctrl Pts',(-21.1588808458317,25.7106892303487,19.0882393912895));
#50052=CARTESIAN_POINT('Ctrl Pts',(-21.1624126725212,25.7145921715007,19.0885507174151));
#50053=CARTESIAN_POINT('Ctrl Pts',(-21.1840586759457,25.7383951993707,19.0904504734818));
#50054=CARTESIAN_POINT('Ctrl Pts',(-21.2024124244594,25.7580769373223,19.0920258431045));
#50055=CARTESIAN_POINT('Ctrl Pts',(-21.4104717479984,25.9756614424703,19.1095239240565));
#50056=CARTESIAN_POINT('Ctrl Pts',(-21.6244484203686,26.1488240801276,19.1243133314771));
#50057=CARTESIAN_POINT('Ctrl Pts',(-21.9286096189419,26.336525848778,19.1447236161856));
#50058=CARTESIAN_POINT('Ctrl Pts',(-22.0010828502014,26.3774613466915,19.1495385378434));
#50059=CARTESIAN_POINT('Ctrl Pts',(-22.0750360918396,26.4155368139396,19.1544452962233));
#50060=CARTESIAN_POINT('Origin',(-23.5502525316942,23.5502525316942,-77.3107734492734));
#50061=CARTESIAN_POINT('',(-22.075036015346,26.4155367745563,20.6506247785903));
#50062=CARTESIAN_POINT('',(-22.0750362907684,26.4155369163599,20.4058188292237));
#50063=CARTESIAN_POINT('',(-22.0750360153461,26.4155367745563,-77.3107734492734));
#50064=CARTESIAN_POINT('',(-26.7730011713685,23.5472761317935,19.8107470580795));
#50065=CARTESIAN_POINT('Ctrl Pts',(-22.075036015346,26.4155367745563,20.6506247785903));
#50066=CARTESIAN_POINT('Ctrl Pts',(-22.072560474055,26.4142622205889,20.6504507389726));
#50067=CARTESIAN_POINT('Ctrl Pts',(-22.0700865732599,26.4129844525941,20.6502768975117));
#50068=CARTESIAN_POINT('Ctrl Pts',(-22.0654139248161,26.4105633566968,20.6499487107652));
#50069=CARTESIAN_POINT('Ctrl Pts',(-22.0632148371251,26.4094206972861,20.6497943238681));
#50070=CARTESIAN_POINT('Ctrl Pts',(-22.0594384410939,26.4074529234129,20.6495293211251));
#50071=CARTESIAN_POINT('Ctrl Pts',(-22.0578604987564,26.4066290389546,20.6494186272314));
#50072=CARTESIAN_POINT('Ctrl Pts',(-22.0546035330675,26.4049250574096,20.6491902236996));
#50073=CARTESIAN_POINT('Ctrl Pts',(-22.0529246068518,26.4040447879155,20.6490725259673));
#50074=CARTESIAN_POINT('Ctrl Pts',(-22.04898654242,26.4019756089116,20.6487965514193));
#50075=CARTESIAN_POINT('Ctrl Pts',(-22.0467280324998,26.4007854924081,20.6486383516743));
#50076=CARTESIAN_POINT('Ctrl Pts',(-22.0395072967062,26.3969695734542,20.648132795953));
#50077=CARTESIAN_POINT('Ctrl Pts',(-22.0345504821422,26.3943334691845,20.6477860929522));
#50078=CARTESIAN_POINT('Ctrl Pts',(-21.991076657609,26.371067538132,20.6447481438429));
#50079=CARTESIAN_POINT('Ctrl Pts',(-21.952973697836,26.3496680949984,20.6421049480978));
#50080=CARTESIAN_POINT('Ctrl Pts',(-21.8439751245489,26.2855017334446,20.6345659071814));
#50081=CARTESIAN_POINT('Ctrl Pts',(-21.7742738814189,26.2407678530585,20.6297724084636));
#50082=CARTESIAN_POINT('Ctrl Pts',(-21.5196112404683,26.0631125329695,20.6120673256177));
#50083=CARTESIAN_POINT('Ctrl Pts',(-21.3471863889556,25.9134021019666,20.5996385350445));
#50084=CARTESIAN_POINT('Ctrl Pts',(-21.0870901019026,25.6341505812422,20.5778787888727));
#50085=CARTESIAN_POINT('Ctrl Pts',(-20.9904176757937,25.5141862844442,20.568889559747));
#50086=CARTESIAN_POINT('Ctrl Pts',(-20.8962786959699,25.3785487079577,20.5588475412572));
#50087=CARTESIAN_POINT('Ctrl Pts',(-20.8899151182754,25.3692766850782,20.5581617309221));
#50088=CARTESIAN_POINT('Ctrl Pts',(-20.8811288676558,25.356329993468,20.5572049515081));
#50089=CARTESIAN_POINT('Ctrl Pts',(-20.8786649447082,25.3526833061227,20.5569355470693));
#50090=CARTESIAN_POINT('Ctrl Pts',(-20.8744306518186,25.3463886555988,20.5564706722689));
#50091=CARTESIAN_POINT('Ctrl Pts',(-20.8726567187406,25.3437430866623,20.5562753368408));
#50092=CARTESIAN_POINT('Ctrl Pts',(-20.8690004286177,25.3382727343037,20.5558715266286));
#50093=CARTESIAN_POINT('Ctrl Pts',(-20.8671186075487,25.33544759951,20.5556630320064));
#50094=CARTESIAN_POINT('Ctrl Pts',(-20.8627435884399,25.3288569390012,20.5551767579921));
#50095=CARTESIAN_POINT('Ctrl Pts',(-20.8602538396143,25.3250891422138,20.5548988493104));
#50096=CARTESIAN_POINT('Ctrl Pts',(-20.8524801731188,25.3132711333183,20.554027432081));
#50097=CARTESIAN_POINT('Ctrl Pts',(-20.8472244479114,25.3052025205593,20.5534328679231));
#50098=CARTESIAN_POINT('Ctrl Pts',(-20.7962497567405,25.2261737270593,20.5476128702779));
#50099=CARTESIAN_POINT('Ctrl Pts',(-20.7533030862974,25.1534726570134,20.5422851310259));
#50100=CARTESIAN_POINT('Ctrl Pts',(-20.679298253231,25.0161530779108,20.5322550777931));
#50101=CARTESIAN_POINT('Ctrl Pts',(-20.6474457364108,24.9520208499752,20.5275836421032));
#50102=CARTESIAN_POINT('Ctrl Pts',(-20.5343016784098,24.7037891627103,20.5095675508202));
#50103=CARTESIAN_POINT('Ctrl Pts',(-20.4681824127434,24.5132886660916,20.4958398508168));
#50104=CARTESIAN_POINT('Ctrl Pts',(-20.3849977282559,24.1741083888681,20.4723216071046));
#50105=CARTESIAN_POINT('Ctrl Pts',(-20.3596792667438,24.0280475681586,20.4624879847602));
#50106=CARTESIAN_POINT('Ctrl Pts',(-20.3435301800228,23.8714028824876,20.4525844135398));
#50107=CARTESIAN_POINT('Ctrl Pts',(-20.3426077769034,23.8620552270192,20.4519958637404));
#50108=CARTESIAN_POINT('Ctrl Pts',(-20.3414234118372,23.8494909888088,20.4512081868314));
#50109=CARTESIAN_POINT('Ctrl Pts',(-20.341125405344,23.8462779728308,20.4510070547097));
#50110=CARTESIAN_POINT('Ctrl Pts',(-20.3406658571961,23.8412410094248,20.4506922181251));
#50111=CARTESIAN_POINT('Ctrl Pts',(-20.3405010445339,23.8394173739571,20.4505783285407));
#50112=CARTESIAN_POINT('Ctrl Pts',(-20.3401873637631,23.8359132157796,20.450359675045));
#50113=CARTESIAN_POINT('Ctrl Pts',(-20.3400382620349,23.8342327276363,20.4502548986893));
#50114=CARTESIAN_POINT('Ctrl Pts',(-20.3396881061396,23.8302506912446,20.4500068200053));
#50115=CARTESIAN_POINT('Ctrl Pts',(-20.3394882074012,23.8279490457455,20.4498635839705));
#50116=CARTESIAN_POINT('Ctrl Pts',(-20.3389149508691,23.8212651656581,20.4494480781631));
#50117=CARTESIAN_POINT('Ctrl Pts',(-20.3385480866145,23.8168823570847,20.4491761752683));
#50118=CARTESIAN_POINT('Ctrl Pts',(-20.3359474792782,23.7850294214405,20.4472040170497));
#50119=CARTESIAN_POINT('Ctrl Pts',(-20.3340571413745,23.7575313103799,20.4455228291897));
#50120=CARTESIAN_POINT('Ctrl Pts',(-20.3291479997729,23.6696562541669,20.4402087644271));
#50121=CARTESIAN_POINT('Ctrl Pts',(-20.3274748216364,23.6092141864215,20.4366415889358));
#50122=CARTESIAN_POINT('Ctrl Pts',(-20.3276020837555,23.3349905464978,20.4207134310528));
#50123=CARTESIAN_POINT('Ctrl Pts',(-20.3489695094329,23.1217494828009,20.4090022161768));
#50124=CARTESIAN_POINT('Ctrl Pts',(-20.432139291801,22.7099932727689,20.3853798340065));
#50125=CARTESIAN_POINT('Ctrl Pts',(-20.4922881997836,22.5122252915948,20.3735373528332));
#50126=CARTESIAN_POINT('Ctrl Pts',(-20.5757325587474,22.3098863033267,20.3602378319656));
#50127=CARTESIAN_POINT('Ctrl Pts',(-20.5806220487365,22.2982252806014,20.3594671848225));
#50128=CARTESIAN_POINT('Ctrl Pts',(-20.5873940502132,22.2823374771766,20.3584113757057));
#50129=CARTESIAN_POINT('Ctrl Pts',(-20.5892172723998,22.2780854201839,20.3581282369605));
#50130=CARTESIAN_POINT('Ctrl Pts',(-20.5923352640829,22.2708567614023,20.357645909961));
#50131=CARTESIAN_POINT('Ctrl Pts',(-20.5936253902236,22.2678781537225,20.3574468806562));
#50132=CARTESIAN_POINT('Ctrl Pts',(-20.5961289047747,22.2621219689643,20.357061703376));
#50133=CARTESIAN_POINT('Ctrl Pts',(-20.5973417161966,22.2593441440145,20.3568755753546));
#50134=CARTESIAN_POINT('Ctrl Pts',(-20.6002281053644,22.2527585059289,20.3564337123175));
#50135=CARTESIAN_POINT('Ctrl Pts',(-20.6019051364866,22.2489522205618,20.3561778590329));
#50136=CARTESIAN_POINT('Ctrl Pts',(-20.6067840440001,22.2379366204899,20.3554360344297));
#50137=CARTESIAN_POINT('Ctrl Pts',(-20.6100050104238,22.2307358395915,20.3549494074501));
#50138=CARTESIAN_POINT('Ctrl Pts',(-20.6338937235263,22.1778520961784,20.3513628785029));
#50139=CARTESIAN_POINT('Ctrl Pts',(-20.6555976704853,22.1326473574772,20.3482273276369));
#50140=CARTESIAN_POINT('Ctrl Pts',(-20.7298966080705,21.9867251649323,20.3378673877354));
#50141=CARTESIAN_POINT('Ctrl Pts',(-20.7867589832719,21.8882886703817,20.3304961124719));
#50142=CARTESIAN_POINT('Ctrl Pts',(-20.9362060749194,21.658523339557,20.3123662560774));
#50143=CARTESIAN_POINT('Ctrl Pts',(-21.0336421296137,21.5307120466303,20.301482905443));
#50144=CARTESIAN_POINT('Ctrl Pts',(-21.2039269233998,21.3388971849937,20.2841336404195));
#50145=CARTESIAN_POINT('Ctrl Pts',(-21.2708498916183,21.2699758835756,20.2776616171758));
#50146=CARTESIAN_POINT('Ctrl Pts',(-21.4074702823327,21.14131067269,20.2652401078896));
#50147=CARTESIAN_POINT('Ctrl Pts',(-21.4768450024346,21.0813455736983,20.2592859857762));
#50148=CARTESIAN_POINT('Ctrl Pts',(-21.55373587608,21.0204145385827,20.2531355324438));
#50149=CARTESIAN_POINT('Ctrl Pts',(-21.5587947480632,21.0164303348454,20.2527328785433));
#50150=CARTESIAN_POINT('Ctrl Pts',(-21.5658200780055,21.0109314492602,20.2521765149781));
#50151=CARTESIAN_POINT('Ctrl Pts',(-21.5677763513883,21.0094038707999,20.2520218903603));
#50152=CARTESIAN_POINT('Ctrl Pts',(-21.5711394668655,21.0067839921988,20.2517565867457));
#50153=CARTESIAN_POINT('Ctrl Pts',(-21.5725454493427,21.0056905986239,20.2516458293041));
#50154=CARTESIAN_POINT('Ctrl Pts',(-21.5754492925373,21.0034362209715,20.2514173981795));
#50155=CARTESIAN_POINT('Ctrl Pts',(-21.5769472679677,21.0022753948047,20.2512997362533));
#50156=CARTESIAN_POINT('Ctrl Pts',(-21.5804627221012,20.9995561233638,20.2510240184491));
#50157=CARTESIAN_POINT('Ctrl Pts',(-21.5824810328613,20.9979987453448,20.2508660392221));
#50158=CARTESIAN_POINT('Ctrl Pts',(-21.5889348320804,20.9930310419869,20.2503618862016));
#50159=CARTESIAN_POINT('Ctrl Pts',(-21.5933773854662,20.9896298477696,20.2500163602798));
#50160=CARTESIAN_POINT('Ctrl Pts',(-21.6502078962411,20.946355002237,20.2456152566793));
#50161=CARTESIAN_POINT('Ctrl Pts',(-21.7038014176244,20.9080807497137,20.2416701138543));
#50162=CARTESIAN_POINT('Ctrl Pts',(-21.8097386442837,20.8372240045645,20.2341811529989));
#50163=CARTESIAN_POINT('Ctrl Pts',(-21.8619170329008,20.8044491155372,20.2306294269077));
#50164=CARTESIAN_POINT('Ctrl Pts',(-22.0430566289472,20.6977868229801,20.21864751512));
#50165=CARTESIAN_POINT('Ctrl Pts',(-22.1761739706156,20.6313295401935,20.2104183943869));
#50166=CARTESIAN_POINT('Ctrl Pts',(-22.4291889204723,20.5261733060566,20.195068347843));
#50167=CARTESIAN_POINT('Ctrl Pts',(-22.5476748270093,20.4848531222669,20.1879894423084));
#50168=CARTESIAN_POINT('Ctrl Pts',(-22.7719066833979,20.4210501230689,20.1744694255498));
#50169=CARTESIAN_POINT('Ctrl Pts',(-22.8769572253449,20.3967783284897,20.1680880655503));
#50170=CARTESIAN_POINT('Ctrl Pts',(-22.9932549748866,20.3759842024976,20.1608981705086));
#50171=CARTESIAN_POINT('Ctrl Pts',(-23.0035004444638,20.3742034364886,20.1602637405125));
#50172=CARTESIAN_POINT('Ctrl Pts',(-23.0179505484794,20.3717638543657,20.1593674504804));
#50173=CARTESIAN_POINT('Ctrl Pts',(-23.0221482201102,20.3710637186408,20.1591069057435));
#50174=CARTESIAN_POINT('Ctrl Pts',(-23.0294530816759,20.3698601968729,20.1586531877796));
#50175=CARTESIAN_POINT('Ctrl Pts',(-23.0325596526911,20.3693530435851,20.1584601345776));
#50176=CARTESIAN_POINT('Ctrl Pts',(-23.0390425591581,20.3683044461174,20.1580570564227));
#50177=CARTESIAN_POINT('Ctrl Pts',(-23.0424190213462,20.3677638230021,20.1578470056645));
#50178=CARTESIAN_POINT('Ctrl Pts',(-23.0504029657552,20.3664985009849,20.1573500415326));
#50179=CARTESIAN_POINT('Ctrl Pts',(-23.0550111640947,20.3657784300442,20.1570629815103));
#50180=CARTESIAN_POINT('Ctrl Pts',(-23.0647056121414,20.3642851402639,20.1564586117059));
#50181=CARTESIAN_POINT('Ctrl Pts',(-23.0697921785769,20.3635140926417,20.1561412337253));
#50182=CARTESIAN_POINT('Ctrl Pts',(-23.1088709830409,20.3576860190373,20.1537007807977));
#50183=CARTESIAN_POINT('Ctrl Pts',(-23.1429392146725,20.3531609903922,20.1515608971636));
#50184=CARTESIAN_POINT('Ctrl Pts',(-23.2724144644833,20.3380667884513,20.1433782420711));
#50185=CARTESIAN_POINT('Ctrl Pts',(-23.368196675357,20.3312179213867,20.1372201197725));
#50186=CARTESIAN_POINT('Ctrl Pts',(-23.626104304556,20.3243236550995,20.1203551604916));
#50187=CARTESIAN_POINT('Ctrl Pts',(-23.788155554582,20.3322153323776,20.1094472614723));
#50188=CARTESIAN_POINT('Ctrl Pts',(-24.1276121200365,20.3745315075581,20.0862940275642));
#50189=CARTESIAN_POINT('Ctrl Pts',(-24.3041469902702,20.4117493928719,20.074074409829));
#50190=CARTESIAN_POINT('Ctrl Pts',(-24.4779880759,20.4639236045081,20.0623634130065));
#50191=CARTESIAN_POINT('Ctrl Pts',(-24.4793164521329,20.4643232197168,20.0622739460019));
#50192=CARTESIAN_POINT('Ctrl Pts',(-24.4854452191336,20.4661712517186,20.0618612655817));
#50193=CARTESIAN_POINT('Ctrl Pts',(-24.4902425124173,20.4676300214071,20.0615385118575));
#50194=CARTESIAN_POINT('Ctrl Pts',(-24.5299162114739,20.4797952975062,20.0588716940903));
#50195=CARTESIAN_POINT('Ctrl Pts',(-24.5646137611495,20.4910826884122,20.0565544633859));
#50196=CARTESIAN_POINT('Ctrl Pts',(-24.6035307601066,20.5044776950365,20.0539784356544));
#50197=CARTESIAN_POINT('Ctrl Pts',(-24.6079443153364,20.5060075557545,20.0536866260606));
#50198=CARTESIAN_POINT('Ctrl Pts',(-24.6146058010105,20.508332847317,20.0532467159547));
#50199=CARTESIAN_POINT('Ctrl Pts',(-24.6168561764672,20.509121177551,20.0530981966922));
#50200=CARTESIAN_POINT('Ctrl Pts',(-24.620761898699,20.5104942617451,20.052840588665));
#50201=CARTESIAN_POINT('Ctrl Pts',(-24.6224176422898,20.5110778706678,20.0527314314958));
#50202=CARTESIAN_POINT('Ctrl Pts',(-24.6258764593825,20.5123001970292,20.0525035099681));
#50203=CARTESIAN_POINT('Ctrl Pts',(-24.6276794397758,20.512939166354,20.0523847613738));
#50204=CARTESIAN_POINT('Ctrl Pts',(-24.631979812862,20.5144675130185,20.0521016700542));
#50205=CARTESIAN_POINT('Ctrl Pts',(-24.6344766865021,20.5153583699992,20.0519374160915));
#50206=CARTESIAN_POINT('Ctrl Pts',(-24.639748929766,20.5172467851115,20.0515908227374));
#50207=CARTESIAN_POINT('Ctrl Pts',(-24.6425240374505,20.518245074894,20.051408527018));
#50208=CARTESIAN_POINT('Ctrl Pts',(-24.6652330762305,20.5264494236802,20.0499178777842));
#50209=CARTESIAN_POINT('Ctrl Pts',(-24.685097461857,20.53384839891,20.0486208891082));
#50210=CARTESIAN_POINT('Ctrl Pts',(-24.744841011723,20.5567750826569,20.0447369715125));
#50211=CARTESIAN_POINT('Ctrl Pts',(-24.7844867929744,20.5729021909588,20.0421824525041));
#50212=CARTESIAN_POINT('Ctrl Pts',(-24.9200623421056,20.6312253673563,20.0334875650309));
#50213=CARTESIAN_POINT('Ctrl Pts',(-25.0142537181823,20.677309375235,20.027517050072));
#50214=CARTESIAN_POINT('Ctrl Pts',(-25.1835357264081,20.7706240730417,20.0166305341263));
#50215=CARTESIAN_POINT('Ctrl Pts',(-25.2592416907778,20.8165179367233,20.0116998545898));
#50216=CARTESIAN_POINT('Ctrl Pts',(-25.5385387417953,21.0019727839191,19.9929551592416));
#50217=CARTESIAN_POINT('Ctrl Pts',(-25.7277219196129,21.1616098796913,19.9790121290229));
#50218=CARTESIAN_POINT('Ctrl Pts',(-25.9077998213481,21.3529031264863,19.96308235942));
#50219=CARTESIAN_POINT('Ctrl Pts',(-25.9186812437433,21.3646361305302,19.9621084122673));
#50220=CARTESIAN_POINT('Ctrl Pts',(-25.9333001271394,21.3806364631637,19.9607842104077));
#50221=CARTESIAN_POINT('Ctrl Pts',(-25.9371144927983,21.3848334717968,19.9604372283508));
#50222=CARTESIAN_POINT('Ctrl Pts',(-25.9431071649807,21.3914623785057,19.9598897581432));
#50223=CARTESIAN_POINT('Ctrl Pts',(-25.9452929011663,21.3938875695376,19.9596895844265));
#50224=CARTESIAN_POINT('Ctrl Pts',(-25.9494972664826,21.3985668156243,19.9593035886894));
#50225=CARTESIAN_POINT('Ctrl Pts',(-25.9515164147517,21.4008204015783,19.9591177888285));
#50226=CARTESIAN_POINT('Ctrl Pts',(-25.9562755687793,21.4061472031627,19.9586788490698));
#50227=CARTESIAN_POINT('Ctrl Pts',(-25.9590128600108,21.409222827253,19.9584255955199));
#50228=CARTESIAN_POINT('Ctrl Pts',(-25.9646550022389,21.4155868612522,19.9579019430556));
#50229=CARTESIAN_POINT('Ctrl Pts',(-25.9675590451417,21.4188759732056,19.9576315110176));
#50230=CARTESIAN_POINT('Ctrl Pts',(-25.9750548592444,21.4274007395656,19.9569311278913));
#50231=CARTESIAN_POINT('Ctrl Pts',(-25.9796363753429,21.4326453447889,19.9565007499159));
#50232=CARTESIAN_POINT('Ctrl Pts',(-26.0206281134546,21.4798779884141,19.9526292868828));
#50233=CARTESIAN_POINT('Ctrl Pts',(-26.0559615865926,21.522784215348,19.9491440072573));
#50234=CARTESIAN_POINT('Ctrl Pts',(-26.1694590638123,21.6681075369293,19.9374319839413));
#50235=CARTESIAN_POINT('Ctrl Pts',(-26.2425837190717,21.7742856022025,19.9290157745398));
#50236=CARTESIAN_POINT('Ctrl Pts',(-26.3324280119512,21.9230939498599,19.917437614496));
#50237=CARTESIAN_POINT('Ctrl Pts',(-26.3548921693095,21.9621272932523,19.9144203184837));
#50238=CARTESIAN_POINT('Ctrl Pts',(-26.3984164449929,22.0415596401807,19.9083266125955));
#50239=CARTESIAN_POINT('Ctrl Pts',(-26.419452868962,22.081960586013,19.9052505801569));
#50240=CARTESIAN_POINT('Ctrl Pts',(-26.527007284457,22.2996654614514,19.8888249318512));
#50241=CARTESIAN_POINT('Ctrl Pts',(-26.5979703996108,22.4842013426492,19.8753952508325));
#50242=CARTESIAN_POINT('Ctrl Pts',(-26.6517887457057,22.6747006539352,19.8626580601752));
#50243=CARTESIAN_POINT('Ctrl Pts',(-26.6519636946625,22.6753206263487,19.86261661942));
#50244=CARTESIAN_POINT('Ctrl Pts',(-26.6623614284191,22.7122097327893,19.8601515555321));
#50245=CARTESIAN_POINT('Ctrl Pts',(-26.671948059372,22.7486573350335,19.8577568637881));
#50246=CARTESIAN_POINT('Ctrl Pts',(-26.6821367671859,22.7903537737573,19.8550701721256));
#50247=CARTESIAN_POINT('Ctrl Pts',(-26.6833674441765,22.7954439911105,19.8547430788028));
#50248=CARTESIAN_POINT('Ctrl Pts',(-26.6851519636326,22.8029045278345,19.8542650003894));
#50249=CARTESIAN_POINT('Ctrl Pts',(-26.6857155288178,22.8052724775964,19.8541134558773));
#50250=CARTESIAN_POINT('Ctrl Pts',(-26.6867104956009,22.8094741897516,19.8538449042907));
#50251=CARTESIAN_POINT('Ctrl Pts',(-26.6871429722808,22.811307692701,19.8537278346775));
#50252=CARTESIAN_POINT('Ctrl Pts',(-26.6880447984773,22.8151460817064,19.8534830012882));
#50253=CARTESIAN_POINT('Ctrl Pts',(-26.6885138332297,22.8171510341922,19.8533552561223));
#50254=CARTESIAN_POINT('Ctrl Pts',(-26.6894621680707,22.8212224080561,19.8530961342577));
#50255=CARTESIAN_POINT('Ctrl Pts',(-26.6899413501817,22.8232888562484,19.8529647644553));
#50256=CARTESIAN_POINT('Ctrl Pts',(-26.6911192061183,22.8283911872046,19.8526407593817));
#50257=CARTESIAN_POINT('Ctrl Pts',(-26.6918155208285,22.831427620697,19.8524482597279));
#50258=CARTESIAN_POINT('Ctrl Pts',(-26.6937335586961,22.8398476675008,19.851915326501));
#50259=CARTESIAN_POINT('Ctrl Pts',(-26.6949458604707,22.8452334488394,19.8515754267017));
#50260=CARTESIAN_POINT('Ctrl Pts',(-26.6987739321953,22.8624463993464,19.8504921728693));
#50261=CARTESIAN_POINT('Ctrl Pts',(-26.7013369010583,22.874285378037,19.8497517341361));
#50262=CARTESIAN_POINT('Ctrl Pts',(-26.7496109339278,23.1035172561767,19.8354992558051));
#50263=CARTESIAN_POINT('Ctrl Pts',(-26.7727959465012,23.3250751626967,19.8231626665619));
#50264=CARTESIAN_POINT('Ctrl Pts',(-26.773001157321,23.547276205028,19.8107470336484));
#50265=CARTESIAN_POINT('Ctrl Pts',(-26.7730011572524,23.5472761306737,19.810747037803));
#50266=CARTESIAN_POINT('Ctrl Pts',(-26.7732080179902,23.771258098769,19.7982318944655));
#50267=CARTESIAN_POINT('Ctrl Pts',(-26.7500658446963,23.9946323456618,19.7856820690413));
#50268=CARTESIAN_POINT('Ctrl Pts',(-26.6939559325066,24.2613106454192,19.7694639610157));
#50269=CARTESIAN_POINT('Ctrl Pts',(-26.6828877456993,24.3085868526511,19.7665428526371));
#50270=CARTESIAN_POINT('Ctrl Pts',(-26.6690358335551,24.3622597248724,19.763167900945));
#50271=CARTESIAN_POINT('Ctrl Pts',(-26.667293975931,24.3689207181373,19.762748022063));
#50272=CARTESIAN_POINT('Ctrl Pts',(-26.6644156540831,24.3797852741851,19.7620614587238));
#50273=CARTESIAN_POINT('Ctrl Pts',(-26.6632919853483,24.3839922293285,19.7617951892557));
#50274=CARTESIAN_POINT('Ctrl Pts',(-26.6610954963404,24.3921494179704,19.7612780790345));
#50275=CARTESIAN_POINT('Ctrl Pts',(-26.6600236690352,24.3960999120911,19.7610272709476));
#50276=CARTESIAN_POINT('Ctrl Pts',(-26.658147181009,24.402964411624,19.7605908052699));
#50277=CARTESIAN_POINT('Ctrl Pts',(-26.6573459392905,24.4058793532612,19.7604052592023));
#50278=CARTESIAN_POINT('Ctrl Pts',(-26.6556678045662,24.4119510168808,19.7600183472402));
#50279=CARTESIAN_POINT('Ctrl Pts',(-26.6547901972954,24.4151075363621,19.7598169582459));
#50280=CARTESIAN_POINT('Ctrl Pts',(-26.6523648353984,24.4237796549975,19.7592629995069));
#50281=CARTESIAN_POINT('Ctrl Pts',(-26.6508071907041,24.4292924544245,19.7589101074531));
#50282=CARTESIAN_POINT('Ctrl Pts',(-26.6447338587181,24.4505701438646,19.7575451539757));
#50283=CARTESIAN_POINT('Ctrl Pts',(-26.6401126269463,24.4663044198852,19.7565296489241));
#50284=CARTESIAN_POINT('Ctrl Pts',(-26.5605903646619,24.7296107269387,19.7394301746216));
#50285=CARTESIAN_POINT('Ctrl Pts',(-26.456289534761,24.9672608676275,19.7223118255461));
#50286=CARTESIAN_POINT('Ctrl Pts',(-26.3020524794845,25.2282589246837,19.7018156883449));
#50287=CARTESIAN_POINT('Ctrl Pts',(-26.2785571134124,25.2661961487095,19.6987938624216));
#50288=CARTESIAN_POINT('Ctrl Pts',(-26.2311012533038,25.3393816444652,19.692891138698));
#50289=CARTESIAN_POINT('Ctrl Pts',(-26.2072139045869,25.3746672832872,19.6900105876434));
#50290=CARTESIAN_POINT('Ctrl Pts',(-26.1187212381181,25.4999600648115,19.6796771175798));
#50291=CARTESIAN_POINT('Ctrl Pts',(-26.0501793682702,25.5871032821835,19.6722875917451));
#50292=CARTESIAN_POINT('Ctrl Pts',(-25.9473997362857,25.7047514145999,19.6621936868112));
#50293=CARTESIAN_POINT('Ctrl Pts',(-25.9167983800514,25.738320500189,19.6592992743473));
#50294=CARTESIAN_POINT('Ctrl Pts',(-25.8830669111001,25.7737873424771,19.6562363191723));
#50295=CARTESIAN_POINT('Ctrl Pts',(-25.8806338806549,25.7763371554726,19.6560160868005));
#50296=CARTESIAN_POINT('Ctrl Pts',(-25.8766114007856,25.7805388876922,19.6556531369521));
#50297=CARTESIAN_POINT('Ctrl Pts',(-25.8750243706366,25.7821931031453,19.6555102344151));
#50298=CARTESIAN_POINT('Ctrl Pts',(-25.8719249074114,25.7854168865646,19.6552317253192));
#50299=CARTESIAN_POINT('Ctrl Pts',(-25.8704126448489,25.7869866157653,19.6550961056412));
#50300=CARTESIAN_POINT('Ctrl Pts',(-25.8677340267511,25.7897613829913,19.65485636295));
#50301=CARTESIAN_POINT('Ctrl Pts',(-25.8665683293519,25.7909670383901,19.6547521894062));
#50302=CARTESIAN_POINT('Ctrl Pts',(-25.8640727789466,25.7935441032749,19.6545295123336));
#50303=CARTESIAN_POINT('Ctrl Pts',(-25.8627426513436,25.7949152364879,19.6544110313541));
#50304=CARTESIAN_POINT('Ctrl Pts',(-25.85888840702,25.7988812387329,19.6540683073747));
#50305=CARTESIAN_POINT('Ctrl Pts',(-25.8563611259656,25.8014730492565,19.6538443127368));
#50306=CARTESIAN_POINT('Ctrl Pts',(-25.8450519415401,25.8130319644344,19.6528452156392));
#50307=CARTESIAN_POINT('Ctrl Pts',(-25.8362219107491,25.8219521383498,19.652073849914));
#50308=CARTESIAN_POINT('Ctrl Pts',(-25.6811006934994,25.9768365929316,19.6386692228917));
#50309=CARTESIAN_POINT('Ctrl Pts',(-25.5211299577579,26.1084735177093,19.6270868547006));
#50310=CARTESIAN_POINT('Ctrl Pts',(-25.2935589334931,26.261630055973,19.6117507860844));
#50311=CARTESIAN_POINT('Ctrl Pts',(-25.2363164516622,26.2975919131558,19.6079808065677));
#50312=CARTESIAN_POINT('Ctrl Pts',(-25.1200028285245,26.3656592524351,19.6004232380903));
#50313=CARTESIAN_POINT('Ctrl Pts',(-25.0609742534985,26.3977690716029,19.5966377712355));
#50314=CARTESIAN_POINT('Ctrl Pts',(-24.9003224223795,26.4787568289068,19.5863903346175));
#50315=CARTESIAN_POINT('Ctrl Pts',(-24.7970735399735,26.5241825595476,19.5798587432113));
#50316=CARTESIAN_POINT('Ctrl Pts',(-24.660920080862,26.5757468561927,19.5711871728024));
#50317=CARTESIAN_POINT('Ctrl Pts',(-24.630000798755,26.5869187749611,19.5692144758437));
#50318=CARTESIAN_POINT('Ctrl Pts',(-24.5795741789903,26.6042716791821,19.5659889188362));
#50319=CARTESIAN_POINT('Ctrl Pts',(-24.5601689319877,26.6107434794377,19.5647457006038));
#50320=CARTESIAN_POINT('Ctrl Pts',(-24.5364710982792,26.6183969685199,19.5632247026338));
#50321=CARTESIAN_POINT('Ctrl Pts',(-24.5322356576063,26.6197551764907,19.5629527522995));
#50322=CARTESIAN_POINT('Ctrl Pts',(-24.5240327402928,26.622366946906,19.5624258442157));
#50323=CARTESIAN_POINT('Ctrl Pts',(-24.5200656190738,26.6236216032669,19.5621709230302));
#50324=CARTESIAN_POINT('Ctrl Pts',(-24.5132041884625,26.6257770166596,19.5617298476214));
#50325=CARTESIAN_POINT('Ctrl Pts',(-24.5103110105933,26.6266813814951,19.5615438123409));
#50326=CARTESIAN_POINT('Ctrl Pts',(-24.5043176195188,26.6285455494661,19.5611583191323));
#50327=CARTESIAN_POINT('Ctrl Pts',(-24.5012172248136,26.6295047538073,19.5609588417614));
#50328=CARTESIAN_POINT('Ctrl Pts',(-24.4927882405287,26.6320985800857,19.5604163582315));
#50329=CARTESIAN_POINT('Ctrl Pts',(-24.4874568689306,26.6337240587324,19.5600730524032));
#50330=CARTESIAN_POINT('Ctrl Pts',(-24.4674367735109,26.6397712546686,19.558783184522));
#50331=CARTESIAN_POINT('Ctrl Pts',(-24.4527209399813,26.644101854464,19.5578336431804));
#50332=CARTESIAN_POINT('Ctrl Pts',(-24.1998127643054,26.7165701723658,19.5414887879166));
#50333=CARTESIAN_POINT('Ctrl Pts',(-23.9546286125756,26.7571086681741,19.5251505746842));
#50334=CARTESIAN_POINT('Ctrl Pts',(-23.5522376874651,26.7767378965417,19.4979461876095));
#50335=CARTESIAN_POINT('Ctrl Pts',(-23.3968522552404,26.7730901752822,19.4873734420729));
#50336=CARTESIAN_POINT('Ctrl Pts',(-23.1449115386135,26.7489076212686,19.4705785628578));
#50337=CARTESIAN_POINT('Ctrl Pts',(-23.0479560850018,26.735122760423,19.4642040814213));
#50338=CARTESIAN_POINT('Ctrl Pts',(-22.9450585744924,26.7156757999477,19.457636985126));
#50339=CARTESIAN_POINT('Ctrl Pts',(-22.9383526754118,26.714386340645,19.457209916703));
#50340=CARTESIAN_POINT('Ctrl Pts',(-22.9295754519718,26.7126696448002,19.4566521778557));
#50341=CARTESIAN_POINT('Ctrl Pts',(-22.9275004440197,26.7122616828379,19.4565204148608));
#50342=CARTESIAN_POINT('Ctrl Pts',(-22.9234102751695,26.7114533429485,19.4562608707779));
#50343=CARTESIAN_POINT('Ctrl Pts',(-22.9213950929089,26.7110530798751,19.4561330831635));
#50344=CARTESIAN_POINT('Ctrl Pts',(-22.9175315401428,26.7102818453892,19.4558882545023));
#50345=CARTESIAN_POINT('Ctrl Pts',(-22.9156831180002,26.7099111803112,19.4557711965168));
#50346=CARTESIAN_POINT('Ctrl Pts',(-22.9114396690411,26.7090563653522,19.4555026337744));
#50347=CARTESIAN_POINT('Ctrl Pts',(-22.9090448612226,26.7085711122758,19.4553511927897));
#50348=CARTESIAN_POINT('Ctrl Pts',(-22.9014707621504,26.7070274244021,19.4548726119676));
#50349=CARTESIAN_POINT('Ctrl Pts',(-22.8962934879563,26.7059589625554,19.4545460465987));
#50350=CARTESIAN_POINT('Ctrl Pts',(-22.8529926226232,26.6969115930808,19.4518193522959));
#50351=CARTESIAN_POINT('Ctrl Pts',(-22.8150118692957,26.6882544645851,19.4494574034476));
#50352=CARTESIAN_POINT('Ctrl Pts',(-22.6169125669422,26.6393062916057,19.4372498471567));
#50353=CARTESIAN_POINT('Ctrl Pts',(-22.4598900640844,26.5874386098432,19.4279513984257));
#50354=CARTESIAN_POINT('Ctrl Pts',(-22.2285849796288,26.4907680364883,19.4139211743695));
#50355=CARTESIAN_POINT('Ctrl Pts',(-22.1510304824955,26.4546631934723,19.4091577064034));
#50356=CARTESIAN_POINT('Ctrl Pts',(-22.0750358228142,26.4155366754296,19.4043601800006));
#50357=CARTESIAN_POINT('Ctrl Pts',(-22.0750360918396,26.4155368139396,19.1544452962233));
#50358=CARTESIAN_POINT('Ctrl Pts',(-22.1221684381613,26.4398033108361,19.1575725024168));
#50359=CARTESIAN_POINT('Ctrl Pts',(-22.1699019589603,26.4629081104642,19.1607367299289));
#50360=CARTESIAN_POINT('Ctrl Pts',(-22.2311167606217,26.4906946378061,19.1648005015267));
#50361=CARTESIAN_POINT('Ctrl Pts',(-22.2440777421048,26.4964749216358,19.1656612367655));
#50362=CARTESIAN_POINT('Ctrl Pts',(-22.2667773444303,26.5064191672319,19.1671694570337));
#50363=CARTESIAN_POINT('Ctrl Pts',(-22.2764991666115,26.5106211057269,19.1678156369838));
#50364=CARTESIAN_POINT('Ctrl Pts',(-22.2905103687364,26.5165951926559,19.1687473200759));
#50365=CARTESIAN_POINT('Ctrl Pts',(-22.2947832119106,26.5184061473449,19.1690314986718));
#50366=CARTESIAN_POINT('Ctrl Pts',(-22.3022075366949,26.5215338914312,19.1695253746352));
#50367=CARTESIAN_POINT('Ctrl Pts',(-22.3053572355772,26.522854915099,19.169734927461));
#50368=CARTESIAN_POINT('Ctrl Pts',(-22.3114188786681,26.5253859213306,19.1701382764341));
#50369=CARTESIAN_POINT('Ctrl Pts',(-22.3143305119638,26.5265966426845,19.1703320471834));
#50370=CARTESIAN_POINT('Ctrl Pts',(-22.3211958694961,26.5294395986256,19.1707890067172));
#50371=CARTESIAN_POINT('Ctrl Pts',(-22.3251510689515,26.5310682362249,19.1710523173265));
#50372=CARTESIAN_POINT('Ctrl Pts',(-22.3368472582525,26.5358571799129,19.1718311307625));
#50373=CARTESIAN_POINT('Ctrl Pts',(-22.3445972732346,26.5389952219764,19.1723473870162));
#50374=CARTESIAN_POINT('Ctrl Pts',(-22.4129474566528,26.5663616355136,19.1769023961048));
#50375=CARTESIAN_POINT('Ctrl Pts',(-22.4742545484936,26.5887726144032,19.1810020445709));
#50376=CARTESIAN_POINT('Ctrl Pts',(-22.5559465616559,26.6158529850348,19.1864889905916));
#50377=CARTESIAN_POINT('Ctrl Pts',(-22.5757594394291,26.6222085344844,19.1878215451431));
#50378=CARTESIAN_POINT('Ctrl Pts',(-22.6197713040256,26.6358579816365,19.1907856651333));
#50379=CARTESIAN_POINT('Ctrl Pts',(-22.6439971898261,26.6430599147796,19.1924199049347));
#50380=CARTESIAN_POINT('Ctrl Pts',(-22.8919476578913,26.7136079364999,19.2091725434781));
#50381=CARTESIAN_POINT('Ctrl Pts',(-23.1217985524594,26.7528426763249,19.2249927352846));
#50382=CARTESIAN_POINT('Ctrl Pts',(-23.5143236361743,26.7768112620511,19.2515346001324));
#50383=CARTESIAN_POINT('Ctrl Pts',(-23.6753494629523,26.7745876123904,19.2622670309256));
#50384=CARTESIAN_POINT('Ctrl Pts',(-23.8461464369167,26.7594077841469,19.2730621890972));
#50385=CARTESIAN_POINT('Ctrl Pts',(-23.856733812609,26.7584139786132,19.273728891487));
#50386=CARTESIAN_POINT('Ctrl Pts',(-23.8705523789893,26.7570478393502,19.2745956702543));
#50387=CARTESIAN_POINT('Ctrl Pts',(-23.8737880381372,26.7567230077279,19.2747983857727));
#50388=CARTESIAN_POINT('Ctrl Pts',(-23.8790673704782,26.7561849368245,19.2751287350096));
#50389=CARTESIAN_POINT('Ctrl Pts',(-23.8811113310427,26.7559746405832,19.2752565352198));
#50390=CARTESIAN_POINT('Ctrl Pts',(-23.8850303136261,26.7555676415691,19.2755013815332));
#50391=CARTESIAN_POINT('Ctrl Pts',(-23.8869053584619,26.7553712488577,19.2756184445885));
#50392=CARTESIAN_POINT('Ctrl Pts',(-23.8912101482216,26.7549165447518,19.2758870102717));
#50393=CARTESIAN_POINT('Ctrl Pts',(-23.8936397781588,26.7546571147509,19.2760384491387));
#50394=CARTESIAN_POINT('Ctrl Pts',(-23.9013243076711,26.7538277390682,19.2765169896524));
#50395=CARTESIAN_POINT('Ctrl Pts',(-23.9065781359438,26.7532476247106,19.2768435169965));
#50396=CARTESIAN_POINT('Ctrl Pts',(-23.9505128715198,26.7482870249172,19.2795688534602));
#50397=CARTESIAN_POINT('Ctrl Pts',(-23.9891150081016,26.7432187104726,19.2819295250954));
#50398=CARTESIAN_POINT('Ctrl Pts',(-24.2415425939763,26.7054111634755,19.2971994977883));
#50399=CARTESIAN_POINT('Ctrl Pts',(-24.4517273585479,26.6519095192429,19.3091514917754));
#50400=CARTESIAN_POINT('Ctrl Pts',(-24.7930242195584,26.527369874711,19.329463976096));
#50401=CARTESIAN_POINT('Ctrl Pts',(-24.9274482323011,26.4676206565251,19.3377172356267));
#50402=CARTESIAN_POINT('Ctrl Pts',(-25.1175670466377,26.3670394423618,19.3501912124659));
#50403=CARTESIAN_POINT('Ctrl Pts',(-25.176785098103,26.3332642386176,19.3541967624321));
#50404=CARTESIAN_POINT('Ctrl Pts',(-25.2724362956922,26.274613174753,19.3608992083727));
#50405=CARTESIAN_POINT('Ctrl Pts',(-25.3095099823458,26.2508211311688,19.3635570334656));
#50406=CARTESIAN_POINT('Ctrl Pts',(-25.3524523707585,26.2220032948189,19.3667112388306));
#50407=CARTESIAN_POINT('Ctrl Pts',(-25.3588063409578,26.217706283416,19.3671799287843));
#50408=CARTESIAN_POINT('Ctrl Pts',(-25.3685070153102,26.2110953961325,19.3678985411106));
#50409=CARTESIAN_POINT('Ctrl Pts',(-25.3718648093741,26.2087977778744,19.368147845381));
#50410=CARTESIAN_POINT('Ctrl Pts',(-25.3779742313419,26.2046003107227,19.3686024803885));
#50411=CARTESIAN_POINT('Ctrl Pts',(-25.3807272744784,26.2027025235491,19.3688077323191));
#50412=CARTESIAN_POINT('Ctrl Pts',(-25.3862513430826,26.1988818570536,19.3692203496874));
#50413=CARTESIAN_POINT('Ctrl Pts',(-25.3890223132415,26.1969589054547,19.3694277177221));
#50414=CARTESIAN_POINT('Ctrl Pts',(-25.3968850818184,26.1914841249653,19.3700172528225));
#50415=CARTESIAN_POINT('Ctrl Pts',(-25.4019696223125,26.1879219423522,19.3703998164226));
#50416=CARTESIAN_POINT('Ctrl Pts',(-25.4234008895915,26.1728148840466,19.3720179943156));
#50417=CARTESIAN_POINT('Ctrl Pts',(-25.4396499087571,26.1611327635552,19.3732588855011));
#50418=CARTESIAN_POINT('Ctrl Pts',(-25.4596399902921,26.1464766937902,19.3748031749391));
#50419=CARTESIAN_POINT('Ctrl Pts',(-25.46348490088,26.1436445707051,19.3751010242227));
#50420=CARTESIAN_POINT('Ctrl Pts',(-25.4767365107887,26.1338380574963,19.37613041216));
#50421=CARTESIAN_POINT('Ctrl Pts',(-25.4861113970156,26.126821012941,19.3768636120134));
#50422=CARTESIAN_POINT('Ctrl Pts',(-25.4992549830674,26.1168708923668,19.37789860532));
#50423=CARTESIAN_POINT('Ctrl Pts',(-25.5030558061851,26.1139802347747,19.378198737437));
#50424=CARTESIAN_POINT('Ctrl Pts',(-25.7629431667796,25.9154136486053,19.3987782124467));
#50425=CARTESIAN_POINT('Ctrl Pts',(-25.9881914708585,25.6824682780081,19.4207202399));
#50426=CARTESIAN_POINT('Ctrl Pts',(-26.2567280121358,25.3055027570072,19.4518888945861));
#50427=CARTESIAN_POINT('Ctrl Pts',(-26.3307787988262,25.1856718639464,19.4612409598152));
#50428=CARTESIAN_POINT('Ctrl Pts',(-26.404161828062,25.0474392492601,19.4711390827669));
#50429=CARTESIAN_POINT('Ctrl Pts',(-26.4114552908466,25.033453507432,19.4721307653669));
#50430=CARTESIAN_POINT('Ctrl Pts',(-26.4203523494708,25.0160828798621,19.4733498958589));
#50431=CARTESIAN_POINT('Ctrl Pts',(-26.4220529483252,25.0127483234791,19.4735833568619));
#50432=CARTESIAN_POINT('Ctrl Pts',(-26.4247210457587,25.0074940851889,19.4739503147396));
#50433=CARTESIAN_POINT('Ctrl Pts',(-26.4256924330077,25.005576398598,19.4740840572156));
#50434=CARTESIAN_POINT('Ctrl Pts',(-26.4275037960429,25.0019915610038,19.4743337136073));
#50435=CARTESIAN_POINT('Ctrl Pts',(-26.4283442364047,25.0003246632521,19.4744496564478));
#50436=CARTESIAN_POINT('Ctrl Pts',(-26.430226898428,24.9965825777111,19.4747096195221));
#50437=CARTESIAN_POINT('Ctrl Pts',(-26.4312683235059,24.9945069976658,19.4748535888132));
#50438=CARTESIAN_POINT('Ctrl Pts',(-26.4339079191944,24.9892320169122,19.4752189217445));
#50439=CARTESIAN_POINT('Ctrl Pts',(-26.4355030139769,24.986031068763,19.4754400915411));
#50440=CARTESIAN_POINT('Ctrl Pts',(-26.4442432846729,24.9684181922014,19.4766542320184));
#50441=CARTESIAN_POINT('Ctrl Pts',(-26.4512859755424,24.9539552430897,19.4776408544205));
#50442=CARTESIAN_POINT('Ctrl Pts',(-26.5936168007394,24.6560159732322,19.497765497533));
#50443=CARTESIAN_POINT('Ctrl Pts',(-26.6868774443053,24.3542676692754,19.5145701044672));
#50444=CARTESIAN_POINT('Ctrl Pts',(-26.7602784156923,23.8805777174499,19.5416913708803));
#50445=CARTESIAN_POINT('Ctrl Pts',(-26.7729823325598,23.7157290758983,19.5512353328095));
#50446=CARTESIAN_POINT('Ctrl Pts',(-26.7730053753846,23.5271809363017,19.5626176023256));
#50447=CARTESIAN_POINT('Ctrl Pts',(-26.7727519586169,23.503716649047,19.5640419645022));
#50448=CARTESIAN_POINT('Ctrl Pts',(-26.7721006155328,23.4737341420675,19.5658727087148));
#50449=CARTESIAN_POINT('Ctrl Pts',(-26.7719390861145,23.4672110759976,19.5662716570329));
#50450=CARTESIAN_POINT('Ctrl Pts',(-26.7716505731733,23.4568336198899,19.5669073833977));
#50451=CARTESIAN_POINT('Ctrl Pts',(-26.771536478879,23.4529788655141,19.5671437563493));
#50452=CARTESIAN_POINT('Ctrl Pts',(-26.7713209926038,23.4461151375993,19.5675650510075));
#50453=CARTESIAN_POINT('Ctrl Pts',(-26.7712223024683,23.4431060787663,19.5677498876086));
#50454=CARTESIAN_POINT('Ctrl Pts',(-26.7709843500903,23.4361485151568,19.5681775959124));
#50455=CARTESIAN_POINT('Ctrl Pts',(-26.7708420432158,23.4322001252137,19.5684205630126));
#50456=CARTESIAN_POINT('Ctrl Pts',(-26.7704227503542,23.4211320774625,19.5691023337704));
#50457=CARTESIAN_POINT('Ctrl Pts',(-26.7701294149431,23.4140130944565,19.5695416504755));
#50458=CARTESIAN_POINT('Ctrl Pts',(-26.7682957071976,23.3728311649924,19.5720877061208));
#50459=CARTESIAN_POINT('Ctrl Pts',(-26.7662384713044,23.3387944675573,19.574210629688));
#50460=CARTESIAN_POINT('Ctrl Pts',(-26.758744417175,23.2406854771148,19.5803861495505));
#50461=CARTESIAN_POINT('Ctrl Pts',(-26.7519298902201,23.1767380245799,19.5844811522186));
#50462=CARTESIAN_POINT('Ctrl Pts',(-26.7324550949608,23.03451373876,19.5937487862557));
#50463=CARTESIAN_POINT('Ctrl Pts',(-26.7188098773828,22.9564154519873,19.5989475356285));
#50464=CARTESIAN_POINT('Ctrl Pts',(-26.640513763091,22.5888073664287,19.6239019810644));
#50465=CARTESIAN_POINT('Ctrl Pts',(-26.5389826579718,22.3086518958653,19.6445200722151));
#50466=CARTESIAN_POINT('Ctrl Pts',(-26.3982318458674,22.0418902706163,19.6639646380911));
#50467=CARTESIAN_POINT('Ctrl Pts',(-26.3958731529694,22.0374451529986,19.6642885457887));
#50468=CARTESIAN_POINT('Ctrl Pts',(-26.3763375012322,22.0008362343624,19.6669552187952));
#50469=CARTESIAN_POINT('Ctrl Pts',(-26.358625312654,21.9689588456189,19.6692711804535));
#50470=CARTESIAN_POINT('Ctrl Pts',(-26.3380375357719,21.9333437068122,19.6718459405409));
#50471=CARTESIAN_POINT('Ctrl Pts',(-26.3356912742873,21.9293051578241,19.6721377157322));
#50472=CARTESIAN_POINT('Ctrl Pts',(-26.3321339688191,21.9232126066965,19.6725775869626));
#50473=CARTESIAN_POINT('Ctrl Pts',(-26.3309294240693,21.921154846453,19.6727261016302));
#50474=CARTESIAN_POINT('Ctrl Pts',(-26.3288340028151,21.9175842698979,19.6729837079539));
#50475=CARTESIAN_POINT('Ctrl Pts',(-26.3279441739946,21.9160708450198,19.6730928680008));
#50476=CARTESIAN_POINT('Ctrl Pts',(-26.3260821660831,21.9129098482735,19.6733208019718));
#50477=CARTESIAN_POINT('Ctrl Pts',(-26.3251097574168,21.9112624161112,19.673439560121));
#50478=CARTESIAN_POINT('Ctrl Pts',(-26.3227860944382,21.9073337156819,19.673722685608));
#50479=CARTESIAN_POINT('Ctrl Pts',(-26.3214334866078,21.9050532404853,19.6738869641445));
#50480=CARTESIAN_POINT('Ctrl Pts',(-26.3168654170688,21.8973731653502,19.6744399998086));
#50481=CARTESIAN_POINT('Ctrl Pts',(-26.3136369498494,21.8919812582657,19.6748279099213));
#50482=CARTESIAN_POINT('Ctrl Pts',(-26.2496409394764,21.7858065460386,19.6824601002862));
#50483=CARTESIAN_POINT('Ctrl Pts',(-26.1834055976511,21.6884041134285,19.6893497353751));
#50484=CARTESIAN_POINT('Ctrl Pts',(-25.9012697710289,21.3187875975391,19.7159468684082));
#50485=CARTESIAN_POINT('Ctrl Pts',(-25.6473419314238,21.0786227451493,19.7345418995362));
#50486=CARTESIAN_POINT('Ctrl Pts',(-25.3581568800172,20.8823686867559,19.7553762604681));
#50487=CARTESIAN_POINT('Ctrl Pts',(-25.3563465179536,20.8811427820714,19.7555066637219));
#50488=CARTESIAN_POINT('Ctrl Pts',(-25.343642361796,20.8725588795465,19.7564215967776));
#50489=CARTESIAN_POINT('Ctrl Pts',(-25.3327050015424,20.8652658347717,19.7572084259371));
#50490=CARTESIAN_POINT('Ctrl Pts',(-25.3114134142272,20.8512560093806,19.75873868261));
#50491=CARTESIAN_POINT('Ctrl Pts',(-25.3010646095662,20.8445313813898,19.7594818087199));
#50492=CARTESIAN_POINT('Ctrl Pts',(-25.2714667477881,20.8255396681928,19.7616055420286));
#50493=CARTESIAN_POINT('Ctrl Pts',(-25.2521259344205,20.8134175995629,19.7629913605956));
#50494=CARTESIAN_POINT('Ctrl Pts',(-25.2270856955448,20.798091418781,19.7647836729528));
#50495=CARTESIAN_POINT('Ctrl Pts',(-25.2215027003002,20.7946975742015,19.7651831687931));
#50496=CARTESIAN_POINT('Ctrl Pts',(-25.2126389454609,20.7893462368768,19.7658172477574));
#50497=CARTESIAN_POINT('Ctrl Pts',(-25.2093649383193,20.7873775472944,19.7660514200929));
#50498=CARTESIAN_POINT('Ctrl Pts',(-25.2032421028685,20.7837106397512,19.7664892873017));
#50499=CARTESIAN_POINT('Ctrl Pts',(-25.2003941359271,20.7820109872954,19.7666929293568));
#50500=CARTESIAN_POINT('Ctrl Pts',(-25.1939951118856,20.7782054654818,19.7671504297941));
#50501=CARTESIAN_POINT('Ctrl Pts',(-25.1904426264056,20.7761020202424,19.767404376192));
#50502=CARTESIAN_POINT('Ctrl Pts',(-25.1806362418608,20.7703210296929,19.7681052735706));
#50503=CARTESIAN_POINT('Ctrl Pts',(-25.1743739795188,20.7666577839746,19.7685527439357));
#50504=CARTESIAN_POINT('Ctrl Pts',(-25.1600407254038,20.7583380707227,19.7695766881891));
#50505=CARTESIAN_POINT('Ctrl Pts',(-25.151961829298,20.7536954146261,19.7701536589006));
#50506=CARTESIAN_POINT('Ctrl Pts',(-24.9730071160529,20.6518862965419,19.7829307351051));
#50507=CARTESIAN_POINT('Ctrl Pts',(-24.7936498200508,20.5705386269109,19.7957091504999));
#50508=CARTESIAN_POINT('Ctrl Pts',(-24.3538006150174,20.4177032833967,19.8268598330285));
#50509=CARTESIAN_POINT('Ctrl Pts',(-24.0895115242429,20.3615605207254,19.8454755720337));
#50510=CARTESIAN_POINT('Ctrl Pts',(-23.8158369890735,20.3384597720983,19.8631654151476));
#50511=CARTESIAN_POINT('Ctrl Pts',(-23.810353261897,20.3380110330498,19.8635191898669));
#50512=CARTESIAN_POINT('Ctrl Pts',(-23.7703328973437,20.3348392789799,19.8660959299755));
#50513=CARTESIAN_POINT('Ctrl Pts',(-23.73575375873,20.3326591313163,19.8682945563317));
#50514=CARTESIAN_POINT('Ctrl Pts',(-23.696548532263,20.3308214931447,19.8707508326875));
#50515=CARTESIAN_POINT('Ctrl Pts',(-23.6919520819407,20.3306159109181,19.8710382406109));
#50516=CARTESIAN_POINT('Ctrl Pts',(-23.6849908452259,20.3303194967462,19.8714726385841));
#50517=CARTESIAN_POINT('Ctrl Pts',(-23.6826263976341,20.3302214258837,19.8716200328316));
#50518=CARTESIAN_POINT('Ctrl Pts',(-23.6785121752119,20.3300553183786,19.8718762353191));
#50519=CARTESIAN_POINT('Ctrl Pts',(-23.67676245317,20.3299861034925,19.8719851101476));
#50520=CARTESIAN_POINT('Ctrl Pts',(-23.6730971532589,20.3298441047758,19.8722130016775));
#50521=CARTESIAN_POINT('Ctrl Pts',(-23.67118156776,20.3297716040263,19.8723320018219));
#50522=CARTESIAN_POINT('Ctrl Pts',(-23.6665951046673,20.329602114281,19.8726166801285));
#50523=CARTESIAN_POINT('Ctrl Pts',(-23.6639241609116,20.3295067382009,19.8727822669157));
#50524=CARTESIAN_POINT('Ctrl Pts',(-23.6552740239779,20.3292086263199,19.8733179094199));
#50525=CARTESIAN_POINT('Ctrl Pts',(-23.6492943389985,20.3290192157176,19.8736872178646));
#50526=CARTESIAN_POINT('Ctrl Pts',(-23.6349953446451,20.328606139293,19.8745680818306));
#50527=CARTESIAN_POINT('Ctrl Pts',(-23.6266755794775,20.3283980434681,19.8750787859253));
#50528=CARTESIAN_POINT('Ctrl Pts',(-23.3231260499265,20.32198206696,19.8936486340493));
#50529=CARTESIAN_POINT('Ctrl Pts',(-23.0283825337816,20.3563463589111,19.9095827325815));
#50530=CARTESIAN_POINT('Ctrl Pts',(-22.5466903300657,20.4810747204834,19.9375864837191));
#50531=CARTESIAN_POINT('Ctrl Pts',(-22.356211274837,20.5500464758041,19.9492093617702));
#50532=CARTESIAN_POINT('Ctrl Pts',(-22.162075288751,20.6417752478567,19.9622569094588));
#50533=CARTESIAN_POINT('Ctrl Pts',(-22.1507202607469,20.6472221178088,19.9630244786));
#50534=CARTESIAN_POINT('Ctrl Pts',(-22.135244909394,20.6547573539238,19.9640767235219));
#50535=CARTESIAN_POINT('Ctrl Pts',(-22.131096612386,20.6567882806639,19.9643593937625));
#50536=CARTESIAN_POINT('Ctrl Pts',(-22.124042212541,20.6602607995865,19.9648411299618));
#50537=CARTESIAN_POINT('Ctrl Pts',(-22.1211338853,20.6616978791867,19.9650400378205));
#50538=CARTESIAN_POINT('Ctrl Pts',(-22.1155116134188,20.6644865584628,19.9654251456702));
#50539=CARTESIAN_POINT('Ctrl Pts',(-22.1127973960015,20.6658376018329,19.9656113259712));
#50540=CARTESIAN_POINT('Ctrl Pts',(-22.1063593633346,20.6690535754149,19.9660535709041));
#50541=CARTESIAN_POINT('Ctrl Pts',(-22.102637255469,20.6709218943619,19.9663097543792));
#50542=CARTESIAN_POINT('Ctrl Pts',(-22.0918072557449,20.6763843406391,19.9670566273743));
#50543=CARTESIAN_POINT('Ctrl Pts',(-22.0847090916876,20.6799975907308,19.9675479896227));
#50544=CARTESIAN_POINT('Ctrl Pts',(-22.0354514188585,20.7053020774889,19.9709707753497));
#50545=CARTESIAN_POINT('Ctrl Pts',(-21.9937635636994,20.7278940846513,19.973933964329));
#50546=CARTESIAN_POINT('Ctrl Pts',(-21.8627109358804,20.8027024162582,19.9834696659796));
#50547=CARTESIAN_POINT('Ctrl Pts',(-21.7753633092832,20.8583029092912,19.9901618560945));
#50548=CARTESIAN_POINT('Ctrl Pts',(-21.5096593793589,21.0459945083397,20.011591176318));
#50549=CARTESIAN_POINT('Ctrl Pts',(-21.3421788093365,21.1923459767152,20.0267643235587));
#50550=CARTESIAN_POINT('Ctrl Pts',(-21.0977106554621,21.4550348037051,20.0508675102469));
#50551=CARTESIAN_POINT('Ctrl Pts',(-21.0108278513863,21.5612248040067,20.0599288595187));
#50552=CARTESIAN_POINT('Ctrl Pts',(-20.9262936562505,21.6791508259306,20.069040880182));
#50553=CARTESIAN_POINT('Ctrl Pts',(-20.921649332455,21.6856809998023,20.0695425177494));
#50554=CARTESIAN_POINT('Ctrl Pts',(-20.9154611523959,21.6944509936076,20.0702122089207));
#50555=CARTESIAN_POINT('Ctrl Pts',(-20.9138957574328,21.6966754709474,20.0703817300026));
#50556=CARTESIAN_POINT('Ctrl Pts',(-20.9112722856753,21.7004135565131,20.0706660186533));
#50557=CARTESIAN_POINT('Ctrl Pts',(-20.9102126939653,21.7019260918515,20.070780890745));
#50558=CARTESIAN_POINT('Ctrl Pts',(-20.9081894902481,21.7048194435807,20.0710003259035));
#50559=CARTESIAN_POINT('Ctrl Pts',(-20.9072256662455,21.7062000958305,20.0711049032782));
#50560=CARTESIAN_POINT('Ctrl Pts',(-20.9049595853342,21.7094516227353,20.0713508779354));
#50561=CARTESIAN_POINT('Ctrl Pts',(-20.9036582326742,21.7113231216956,20.0714922123503));
#50562=CARTESIAN_POINT('Ctrl Pts',(-20.8999339880381,21.7166911676228,20.0718969139673));
#50563=CARTESIAN_POINT('Ctrl Pts',(-20.8975160203309,21.7201911500907,20.0721599431113));
#50564=CARTESIAN_POINT('Ctrl Pts',(-20.881360425045,21.7436754973192,20.0739192981064));
#50565=CARTESIAN_POINT('Ctrl Pts',(-20.8678413342444,21.7638102822884,20.0754009323319));
#50566=CARTESIAN_POINT('Ctrl Pts',(-20.82667936833,21.8266362151061,20.0799480632555));
#50567=CARTESIAN_POINT('Ctrl Pts',(-20.7998175588995,21.8698323264605,20.0829674235431));
#50568=CARTESIAN_POINT('Ctrl Pts',(-20.7374681984873,21.9755991086126,20.09015120636));
#50569=CARTESIAN_POINT('Ctrl Pts',(-20.7030302768715,22.0387580218041,20.0942704244645));
#50570=CARTESIAN_POINT('Ctrl Pts',(-20.5797308110551,22.2840835684309,20.1098259223461));
#50571=CARTESIAN_POINT('Ctrl Pts',(-20.5060093991629,22.4733265249975,20.1209453317185));
#50572=CARTESIAN_POINT('Ctrl Pts',(-20.431458465614,22.7353257430847,20.1364458983841));
#50573=CARTESIAN_POINT('Ctrl Pts',(-20.4145537565109,22.8030079353775,20.1404558476725));
#50574=CARTESIAN_POINT('Ctrl Pts',(-20.3803645103059,22.9616213405645,20.149926155676));
#50575=CARTESIAN_POINT('Ctrl Pts',(-20.3647753543345,23.052849891687,20.1554287935116));
#50576=CARTESIAN_POINT('Ctrl Pts',(-20.3518464650915,23.154752114926,20.1616818059197));
#50577=CARTESIAN_POINT('Ctrl Pts',(-20.3506087239092,23.1648936780674,20.1623052624745));
#50578=CARTESIAN_POINT('Ctrl Pts',(-20.3489400661048,23.1791285644539,20.1631820108497));
#50579=CARTESIAN_POINT('Ctrl Pts',(-20.3484687258045,23.1832171635281,20.1634340250008));
#50580=CARTESIAN_POINT('Ctrl Pts',(-20.3476195150417,23.1907096932295,20.1638962058187));
#50581=CARTESIAN_POINT('Ctrl Pts',(-20.3472392355953,23.1941133497434,20.1641062961199));
#50582=CARTESIAN_POINT('Ctrl Pts',(-20.346480683599,23.2010021952454,20.164531782781));
#50583=CARTESIAN_POINT('Ctrl Pts',(-20.3461026708638,23.2044874071619,20.1647471870109));
#50584=CARTESIAN_POINT('Ctrl Pts',(-20.3453571360882,23.2114673286247,20.1651788685839));
#50585=CARTESIAN_POINT('Ctrl Pts',(-20.3449896416838,23.2149620362115,20.1653951464871));
#50586=CARTESIAN_POINT('Ctrl Pts',(-20.3436633612314,23.2277758360225,20.1661886884369));
#50587=CARTESIAN_POINT('Ctrl Pts',(-20.3427395027563,23.2370984264986,20.1667670536321));
#50588=CARTESIAN_POINT('Ctrl Pts',(-20.3345237838355,23.3238557621488,20.1721591850645));
#50589=CARTESIAN_POINT('Ctrl Pts',(-20.3299972583153,23.4015207178485,20.1770596360268));
#50590=CARTESIAN_POINT('Ctrl Pts',(-20.3266525377133,23.5533372312413,20.1867945918078));
#50591=CARTESIAN_POINT('Ctrl Pts',(-20.3275754000759,23.6274355780089,20.1916182394667));
#50592=CARTESIAN_POINT('Ctrl Pts',(-20.3394530511492,23.8803571235831,20.2083152429478));
#50593=CARTESIAN_POINT('Ctrl Pts',(-20.3627578147318,24.0582587728889,20.2204787370895));
#50594=CARTESIAN_POINT('Ctrl Pts',(-20.4327290048486,24.3809030269292,20.2427930836691));
#50595=CARTESIAN_POINT('Ctrl Pts',(-20.4750845141968,24.5261032114347,20.2529267256994));
#50596=CARTESIAN_POINT('Ctrl Pts',(-20.5282528740876,24.669913491748,20.2627358800894));
#50597=CARTESIAN_POINT('Ctrl Pts',(-20.5290330741311,24.6720170280783,20.2628793076616));
#50598=CARTESIAN_POINT('Ctrl Pts',(-20.5395737845785,24.7003455991233,20.264810139642));
#50599=CARTESIAN_POINT('Ctrl Pts',(-20.5496736650995,24.7264443433088,20.2665806331491));
#50600=CARTESIAN_POINT('Ctrl Pts',(-20.5618767873656,24.7567973258967,20.268627148015));
#50601=CARTESIAN_POINT('Ctrl Pts',(-20.5636506276377,24.7611815127145,20.2689224376951));
#50602=CARTESIAN_POINT('Ctrl Pts',(-20.5663364092402,24.7677778339064,20.2693662387598));
#50603=CARTESIAN_POINT('Ctrl Pts',(-20.5672411636836,24.7699928588856,20.2695151836221));
#50604=CARTESIAN_POINT('Ctrl Pts',(-20.5688586858143,24.7739403217712,20.2697804734307));
#50605=CARTESIAN_POINT('Ctrl Pts',(-20.5695704965715,24.7756731441364,20.2698968765268));
#50606=CARTESIAN_POINT('Ctrl Pts',(-20.5710846828366,24.7793501333349,20.2701437698795));
#50607=CARTESIAN_POINT('Ctrl Pts',(-20.5718874486279,24.7812941305275,20.2702742355541));
#50608=CARTESIAN_POINT('Ctrl Pts',(-20.5735278516248,24.7852555734926,20.2705399662989));
#50609=CARTESIAN_POINT('Ctrl Pts',(-20.5743656382996,24.7872729567382,20.2706752221589));
#50610=CARTESIAN_POINT('Ctrl Pts',(-20.5780851993441,24.7962039809633,20.2712737064504));
#50611=CARTESIAN_POINT('Ctrl Pts',(-20.5809890510276,24.803108489278,20.2717355987693));
#50612=CARTESIAN_POINT('Ctrl Pts',(-20.6098847715482,24.8711492739382,20.2762801124419));
#50613=CARTESIAN_POINT('Ctrl Pts',(-20.6377392441712,24.9314833644604,20.2802522746689));
#50614=CARTESIAN_POINT('Ctrl Pts',(-20.6970417829515,25.0501493669342,20.2880320052594));
#50615=CARTESIAN_POINT('Ctrl Pts',(-20.7284622767839,25.108457515148,20.29183823175));
#50616=CARTESIAN_POINT('Ctrl Pts',(-20.8459079131071,25.311185393177,20.3051542435726));
#50617=CARTESIAN_POINT('Ctrl Pts',(-20.9414059160023,25.4498016839362,20.3144241374528));
#50618=CARTESIAN_POINT('Ctrl Pts',(-21.1750143140624,25.7378261411087,20.3352932122986));
#50619=CARTESIAN_POINT('Ctrl Pts',(-21.3173030170811,25.8828803648416,20.346948684621));
#50620=CARTESIAN_POINT('Ctrl Pts',(-21.4818793559255,26.0217112784928,20.3600325517818));
#50621=CARTESIAN_POINT('Ctrl Pts',(-21.4915457702573,26.0297690964178,20.3607995501883));
#50622=CARTESIAN_POINT('Ctrl Pts',(-21.5048229623825,26.0407056549606,20.3618511323362));
#50623=CARTESIAN_POINT('Ctrl Pts',(-21.5083931900323,26.043633631869,20.3621337138052));
#50624=CARTESIAN_POINT('Ctrl Pts',(-21.514482143933,26.0486053914465,20.3626153367678));
#50625=CARTESIAN_POINT('Ctrl Pts',(-21.5169976935598,26.0506530689293,20.3628142203202));
#50626=CARTESIAN_POINT('Ctrl Pts',(-21.5218706589228,26.0546074853283,20.3631993115273));
#50627=CARTESIAN_POINT('Ctrl Pts',(-21.5242276830347,26.056514702357,20.3633854995411));
#50628=CARTESIAN_POINT('Ctrl Pts',(-21.5298293836071,26.0610343258377,20.3638278101826));
#50629=CARTESIAN_POINT('Ctrl Pts',(-21.5330764346591,26.0636437683343,20.3640840517568));
#50630=CARTESIAN_POINT('Ctrl Pts',(-21.5425501950049,26.0712270259358,20.3648312574925));
#50631=CARTESIAN_POINT('Ctrl Pts',(-21.5487902721732,26.0761840223029,20.3653228953021));
#50632=CARTESIAN_POINT('Ctrl Pts',(-21.5956245381427,26.1131057470584,20.3690090322622));
#50633=CARTESIAN_POINT('Ctrl Pts',(-21.6369617977468,26.1441116765048,20.3722414206852));
#50634=CARTESIAN_POINT('Ctrl Pts',(-21.7320652509628,26.2119355928824,20.3796371593369));
#50635=CARTESIAN_POINT('Ctrl Pts',(-21.7862373774116,26.2481426855665,20.3838217599413));
#50636=CARTESIAN_POINT('Ctrl Pts',(-21.9174781507999,26.330217061326,20.393894382062));
#50637=CARTESIAN_POINT('Ctrl Pts',(-21.9954043122551,26.3745377092206,20.3998249117356));
#50638=CARTESIAN_POINT('Ctrl Pts',(-22.0750362907684,26.4155369163599,20.4058188292237));
#50639=CARTESIAN_POINT('Origin',(-23.5502525316942,23.5502525316942,-77.3107734492734));
#50640=CARTESIAN_POINT('',(-22.0750357484432,26.415536637139,21.9049549578222));
#50641=CARTESIAN_POINT('',(-22.075036015355,26.4155367745608,21.6601868380444));
#50642=CARTESIAN_POINT('',(-22.0750360153461,26.4155367745563,-77.3107734492734));
#50643=CARTESIAN_POINT('Ctrl Pts',(-22.0750357484432,26.415536637139,21.9049549578222));
#50644=CARTESIAN_POINT('Ctrl Pts',(-22.0088770685692,26.3814742575228,21.8999718987017));
#50645=CARTESIAN_POINT('Ctrl Pts',(-21.9438937780695,26.3451182736942,21.8949460589944));
#50646=CARTESIAN_POINT('Ctrl Pts',(-21.7492298965475,26.2271700388232,21.8795449272302));
#50647=CARTESIAN_POINT('Ctrl Pts',(-21.6240713338848,26.1385725783133,21.8691464575743));
#50648=CARTESIAN_POINT('Ctrl Pts',(-21.4522955103917,25.9975906616431,21.8545440013663));
#50649=CARTESIAN_POINT('Ctrl Pts',(-21.4003261726026,25.9520655740068,21.8500790058873));
#50650=CARTESIAN_POINT('Ctrl Pts',(-21.3417756085546,25.8973506447596,21.845032046154));
#50651=CARTESIAN_POINT('Ctrl Pts',(-21.3337340360379,25.8897579579112,21.8443385068057));
#50652=CARTESIAN_POINT('Ctrl Pts',(-21.323338804554,25.8798412829584,21.8434416871175));
#50653=CARTESIAN_POINT('Ctrl Pts',(-21.3209495410501,25.8775549775061,21.8432355399513));
#50654=CARTESIAN_POINT('Ctrl Pts',(-21.3170833391493,25.8738439611435,21.8429019354042));
#50655=CARTESIAN_POINT('Ctrl Pts',(-21.3156042428099,25.8724215174885,21.8427743017775));
#50656=CARTESIAN_POINT('Ctrl Pts',(-21.3127683599552,25.8696890366998,21.8425295786826));
#50657=CARTESIAN_POINT('Ctrl Pts',(-21.3114113688423,25.8683792251839,21.842412472614));
#50658=CARTESIAN_POINT('Ctrl Pts',(-21.3082952005647,25.8653661107243,21.8421435410459));
#50659=CARTESIAN_POINT('Ctrl Pts',(-21.3065368100737,25.8636619894132,21.8419917799025));
#50660=CARTESIAN_POINT('Ctrl Pts',(-21.3009687201596,25.8582534273265,21.8415111818616));
#50661=CARTESIAN_POINT('Ctrl Pts',(-21.2971662144503,25.854541542881,21.8411829263497));
#50662=CARTESIAN_POINT('Ctrl Pts',(-21.2650690569451,25.8230539141596,21.8384114951209));
#50663=CARTESIAN_POINT('Ctrl Pts',(-21.2372784762305,25.7947660662278,21.8360078984496));
#50664=CARTESIAN_POINT('Ctrl Pts',(-21.0677861626997,25.6157486533297,21.8212673586743));
#50665=CARTESIAN_POINT('Ctrl Pts',(-20.9403324311978,25.4521602224927,21.8097994840551));
#50666=CARTESIAN_POINT('Ctrl Pts',(-20.7528924864414,25.1568918490335,21.7902540007185));
#50667=CARTESIAN_POINT('Ctrl Pts',(-20.6844553229816,25.0313723529527,21.7822526729934));
#50668=CARTESIAN_POINT('Ctrl Pts',(-20.5900289670077,24.8269587000176,21.7692581437212));
#50669=CARTESIAN_POINT('Ctrl Pts',(-20.5583687786117,24.7508907736037,21.7644318311119));
#50670=CARTESIAN_POINT('Ctrl Pts',(-20.5198901978335,24.6474338783318,21.7578337597834));
#50671=CARTESIAN_POINT('Ctrl Pts',(-20.5104650608245,24.6210442197741,21.7561479562325));
#50672=CARTESIAN_POINT('Ctrl Pts',(-20.4955296043008,24.5774389733186,21.7533562302207));
#50673=CARTESIAN_POINT('Ctrl Pts',(-20.4898177477939,24.5602936505351,21.7522569909421));
#50674=CARTESIAN_POINT('Ctrl Pts',(-20.4825476991702,24.5378431212792,21.7508153106236));
#50675=CARTESIAN_POINT('Ctrl Pts',(-20.4808584540624,24.5325804340391,21.7504771979234));
#50676=CARTESIAN_POINT('Ctrl Pts',(-20.4780762919761,24.5238356222411,21.7499150859459));
#50677=CARTESIAN_POINT('Ctrl Pts',(-20.4769757321614,24.5203559258572,21.7496913386986));
#50678=CARTESIAN_POINT('Ctrl Pts',(-20.4748722516965,24.5136657395236,21.7492610089146));
#50679=CARTESIAN_POINT('Ctrl Pts',(-20.4738684411419,24.5104555325638,21.7490544559785));
#50680=CARTESIAN_POINT('Ctrl Pts',(-20.4715939360499,24.5031414394652,21.7485836994924));
#50681=CARTESIAN_POINT('Ctrl Pts',(-20.4703264203127,24.4990365783731,21.748319391891));
#50682=CARTESIAN_POINT('Ctrl Pts',(-20.4664956077023,24.4865418866063,21.7475145404217));
#50683=CARTESIAN_POINT('Ctrl Pts',(-20.4639583724657,24.478144164732,21.746973142721));
#50684=CARTESIAN_POINT('Ctrl Pts',(-20.4461250823004,24.4182372704553,21.7431076001775));
#50685=CARTESIAN_POINT('Ctrl Pts',(-20.4320858357014,24.3663656498333,21.7397426037319));
#50686=CARTESIAN_POINT('Ctrl Pts',(-20.4149776543517,24.2962480506356,21.7351662565127));
#50687=CARTESIAN_POINT('Ctrl Pts',(-20.4107589248725,24.2782894408829,21.7339917634516));
#50688=CARTESIAN_POINT('Ctrl Pts',(-20.3475228100442,23.9983257138685,21.7156443340768));
#50689=CARTESIAN_POINT('Ctrl Pts',(-20.3213394005373,23.7300232487341,21.6974144067586));
#50690=CARTESIAN_POINT('Ctrl Pts',(-20.3334163008781,23.2909265648678,21.6677520103089));
#50691=CARTESIAN_POINT('Ctrl Pts',(-20.3516759376082,23.1208231680326,21.6563413863853));
#50692=CARTESIAN_POINT('Ctrl Pts',(-20.3844797145807,22.9468969458099,21.6452506482799));
#50693=CARTESIAN_POINT('Ctrl Pts',(-20.3856385311446,22.9408481326202,21.644865682947));
#50694=CARTESIAN_POINT('Ctrl Pts',(-20.3873168591515,22.9322214576985,21.6443177600331));
#50695=CARTESIAN_POINT('Ctrl Pts',(-20.3878221877036,22.9296409006454,21.6441539973687));
#50696=CARTESIAN_POINT('Ctrl Pts',(-20.3886998114812,22.9251880519513,21.6438716661104));
#50697=CARTESIAN_POINT('Ctrl Pts',(-20.3890706123262,22.9233154700552,21.6437530113181));
#50698=CARTESIAN_POINT('Ctrl Pts',(-20.3897865672665,22.9197166093846,21.6435251187672));
#50699=CARTESIAN_POINT('Ctrl Pts',(-20.3901314713808,22.9179902871866,21.643415866705));
#50700=CARTESIAN_POINT('Ctrl Pts',(-20.3909505885342,22.9139078368668,21.6431576559813));
#50701=CARTESIAN_POINT('Ctrl Pts',(-20.3914260238173,22.9115519508961,21.6430087679043));
#50702=CARTESIAN_POINT('Ctrl Pts',(-20.3928479760104,22.9045462900902,21.6425663706255));
#50703=CARTESIAN_POINT('Ctrl Pts',(-20.3938021326733,22.8998980453558,21.6422732980125));
#50704=CARTESIAN_POINT('Ctrl Pts',(-20.402597791818,22.857524683748,21.6396056824188));
#50705=CARTESIAN_POINT('Ctrl Pts',(-20.4111054261117,22.8199388968835,21.6372686294094));
#50706=CARTESIAN_POINT('Ctrl Pts',(-20.4597091592694,22.6217883278776,21.6250592180799));
#50707=CARTESIAN_POINT('Ctrl Pts',(-20.5114590835634,22.464319025119,21.6157387628019));
#50708=CARTESIAN_POINT('Ctrl Pts',(-20.6472401573578,22.1382055704558,21.5959687067993));
#50709=CARTESIAN_POINT('Ctrl Pts',(-20.7343954175306,21.9715500120746,21.5855609917238));
#50710=CARTESIAN_POINT('Ctrl Pts',(-20.8934796775097,21.7228973687797,21.5685105705931));
#50711=CARTESIAN_POINT('Ctrl Pts',(-20.9558888351996,21.63532637298,21.5621768312115));
#50712=CARTESIAN_POINT('Ctrl Pts',(-21.030197333126,21.5413744128405,21.5549235906861));
#50713=CARTESIAN_POINT('Ctrl Pts',(-21.0378991874546,21.5317505704931,21.554175042109));
#50714=CARTESIAN_POINT('Ctrl Pts',(-21.0497820876604,21.517075679911,21.5530249329338));
#50715=CARTESIAN_POINT('Ctrl Pts',(-21.0539237114035,21.5119927415542,21.5526249580603));
#50716=CARTESIAN_POINT('Ctrl Pts',(-21.0616365231719,21.5025857190596,21.5518817057441));
#50717=CARTESIAN_POINT('Ctrl Pts',(-21.0652035487046,21.4982582419964,21.5515385976982));
#50718=CARTESIAN_POINT('Ctrl Pts',(-21.0710664908655,21.4911830917973,21.5509756700158));
#50719=CARTESIAN_POINT('Ctrl Pts',(-21.0733557337106,21.4884298828391,21.5507561228822));
#50720=CARTESIAN_POINT('Ctrl Pts',(-21.0778165664352,21.4830831137278,21.5503288009968));
#50721=CARTESIAN_POINT('Ctrl Pts',(-21.0799876614808,21.480489145282,21.5501210466682));
#50722=CARTESIAN_POINT('Ctrl Pts',(-21.08496922953,21.4745562992279,21.5496448644687));
#50723=CARTESIAN_POINT('Ctrl Pts',(-21.0877824044507,21.4712197081104,21.5493763258121));
#50724=CARTESIAN_POINT('Ctrl Pts',(-21.0966509818181,21.4607443054288,21.5485309046173));
#50725=CARTESIAN_POINT('Ctrl Pts',(-21.1027306749654,21.4536262056518,21.5479530211095));
#50726=CARTESIAN_POINT('Ctrl Pts',(-21.1262269557873,21.4263582489577,21.5457260034582));
#50727=CARTESIAN_POINT('Ctrl Pts',(-21.143861678723,21.4063985462462,21.5440678168645));
#50728=CARTESIAN_POINT('Ctrl Pts',(-21.1658906469998,21.3820795302137,21.5420120308799));
#50729=CARTESIAN_POINT('Ctrl Pts',(-21.170053093519,21.3775108546454,21.5416242561158));
#50730=CARTESIAN_POINT('Ctrl Pts',(-21.1788530448962,21.3679077173373,21.5408058549723));
#50731=CARTESIAN_POINT('Ctrl Pts',(-21.1834934933002,21.3628760054068,21.5403751053906));
#50732=CARTESIAN_POINT('Ctrl Pts',(-21.1889370405964,21.3570110828813,21.5398707521407));
#50733=CARTESIAN_POINT('Ctrl Pts',(-21.1897246292117,21.3561634444223,21.5397978038088));
#50734=CARTESIAN_POINT('Ctrl Pts',(-21.1927233739582,21.3529395433453,21.5395201403116));
#50735=CARTESIAN_POINT('Ctrl Pts',(-21.1949376574447,21.3505662037471,21.5393152932233));
#50736=CARTESIAN_POINT('Ctrl Pts',(-21.2018592282405,21.343169877187,21.5386755283866));
#50737=CARTESIAN_POINT('Ctrl Pts',(-21.2065790035263,21.3381586494819,21.5382400844483));
#50738=CARTESIAN_POINT('Ctrl Pts',(-21.2150248724087,21.3292486086665,21.5374623019707));
#50739=CARTESIAN_POINT('Ctrl Pts',(-21.2187447761126,21.3253439421346,21.5371202250601));
#50740=CARTESIAN_POINT('Ctrl Pts',(-21.225243647245,21.3185564764754,21.5365234475031));
#50741=CARTESIAN_POINT('Ctrl Pts',(-21.2280182269136,21.3156694768229,21.5362689316827));
#50742=CARTESIAN_POINT('Ctrl Pts',(-21.2338451637871,21.3096290181086,21.5357349786288));
#50743=CARTESIAN_POINT('Ctrl Pts',(-21.2368985947419,21.3064766102146,21.5354554966424));
#50744=CARTESIAN_POINT('Ctrl Pts',(-21.2542941347665,21.2885904477104,21.5338650871084));
#50745=CARTESIAN_POINT('Ctrl Pts',(-21.2687702968871,21.2739882403019,21.532548564287));
#50746=CARTESIAN_POINT('Ctrl Pts',(-21.3015867580189,21.2415135798956,21.529579566751));
#50747=CARTESIAN_POINT('Ctrl Pts',(-21.3200022065971,21.2237193296554,21.5279240498435));
#50748=CARTESIAN_POINT('Ctrl Pts',(-21.4877190743648,21.0654812259741,21.5129415003928));
#50749=CARTESIAN_POINT('Ctrl Pts',(-21.6498750049879,20.9393755166254,21.4990790960961));
#50750=CARTESIAN_POINT('Ctrl Pts',(-21.9768945191604,20.7317522576256,21.4728685293787));
#50751=CARTESIAN_POINT('Ctrl Pts',(-22.1389528790534,20.6472112186308,21.4605802639441));
#50752=CARTESIAN_POINT('Ctrl Pts',(-22.3220088801862,20.5706906829568,21.4480303402257));
#50753=CARTESIAN_POINT('Ctrl Pts',(-22.3367507131747,20.5646563367365,21.4470287814219));
#50754=CARTESIAN_POINT('Ctrl Pts',(-22.3550227095693,20.5573346685479,21.4457991494938));
#50755=CARTESIAN_POINT('Ctrl Pts',(-22.3585108400397,20.5559440298942,21.4455649398828));
#50756=CARTESIAN_POINT('Ctrl Pts',(-22.3640020249789,20.5537659340301,21.4451970741876));
#50757=CARTESIAN_POINT('Ctrl Pts',(-22.3660034372074,20.5529743869543,21.4450631704608));
#50758=CARTESIAN_POINT('Ctrl Pts',(-22.3697419484449,20.5515001563102,21.4448133753987));
#50759=CARTESIAN_POINT('Ctrl Pts',(-22.3714788360296,20.5508169813828,21.4446974548023));
#50760=CARTESIAN_POINT('Ctrl Pts',(-22.3753745595173,20.549288571912,21.4444377488541));
#50761=CARTESIAN_POINT('Ctrl Pts',(-22.3775337098141,20.548444159676,21.4442940140166));
#50762=CARTESIAN_POINT('Ctrl Pts',(-22.3830147101582,20.5463074364644,21.4439296550492));
#50763=CARTESIAN_POINT('Ctrl Pts',(-22.3863378061927,20.5450183013521,21.4437092229923));
#50764=CARTESIAN_POINT('Ctrl Pts',(-22.4045323413241,20.5379947654678,21.4425048886088));
#50765=CARTESIAN_POINT('Ctrl Pts',(-22.4194443682585,20.5323651038765,21.4415272156349));
#50766=CARTESIAN_POINT('Ctrl Pts',(-22.7047422274933,20.4270696531969,21.4229897534602));
#50767=CARTESIAN_POINT('Ctrl Pts',(-22.9872980339362,20.3639845908132,21.4074088819883));
#50768=CARTESIAN_POINT('Ctrl Pts',(-23.4776899933444,20.3218728230987,21.3797236754214));
#50769=CARTESIAN_POINT('Ctrl Pts',(-23.6820262323926,20.3237501344491,21.3680127498266));
#50770=CARTESIAN_POINT('Ctrl Pts',(-23.8939507061801,20.3458690022281,21.3550717404019));
#50771=CARTESIAN_POINT('Ctrl Pts',(-23.9030987697753,20.3468634250469,21.354511645616));
#50772=CARTESIAN_POINT('Ctrl Pts',(-23.9195910549072,20.34872769017,21.3534991829551));
#50773=CARTESIAN_POINT('Ctrl Pts',(-23.9269368043547,20.3495836620799,21.3530472543973));
#50774=CARTESIAN_POINT('Ctrl Pts',(-23.9382381784198,20.3509400122082,21.3523504472496));
#50775=CARTESIAN_POINT('Ctrl Pts',(-23.9421959630792,20.3514224634079,21.3521061357713));
#50776=CARTESIAN_POINT('Ctrl Pts',(-23.9494711209888,20.3523230046028,21.3516565134875));
#50777=CARTESIAN_POINT('Ctrl Pts',(-23.9527887625422,20.3527389156166,21.3514512718982));
#50778=CARTESIAN_POINT('Ctrl Pts',(-23.9594512463146,20.3535846810685,21.3510386950811));
#50779=CARTESIAN_POINT('Ctrl Pts',(-23.9627960728795,20.3540146241285,21.3508313572882));
#50780=CARTESIAN_POINT('Ctrl Pts',(-23.9722947016508,20.3552507338016,21.3502419653532));
#50781=CARTESIAN_POINT('Ctrl Pts',(-23.9784468337084,20.3560694247609,21.3498595149603));
#50782=CARTESIAN_POINT('Ctrl Pts',(-24.0044133431682,20.3596012672809,21.3482422684021));
#50783=CARTESIAN_POINT('Ctrl Pts',(-24.0242042684565,20.3624810129112,21.347002202715));
#50784=CARTESIAN_POINT('Ctrl Pts',(-24.3790082545516,20.4174850463712,21.3246333413055));
#50785=CARTESIAN_POINT('Ctrl Pts',(-24.7036891996217,20.5219639699789,21.3016197148811));
#50786=CARTESIAN_POINT('Ctrl Pts',(-25.1468697287346,20.7463520463564,21.2681403038743));
#50787=CARTESIAN_POINT('Ctrl Pts',(-25.2823165760869,20.8279350089339,21.2576409852094));
#50788=CARTESIAN_POINT('Ctrl Pts',(-25.4159422793815,20.9224488219498,21.247389895776));
#50789=CARTESIAN_POINT('Ctrl Pts',(-25.4206240696381,20.9257790830124,21.2470308877893));
#50790=CARTESIAN_POINT('Ctrl Pts',(-25.4273756936981,20.9306089052621,21.2465134160943));
#50791=CARTESIAN_POINT('Ctrl Pts',(-25.4294526544687,20.9320984121835,21.2463542644137));
#50792=CARTESIAN_POINT('Ctrl Pts',(-25.4330674215601,20.9346972850043,21.2460773391012));
#50793=CARTESIAN_POINT('Ctrl Pts',(-25.434606022495,20.9358055385864,21.2459594880669));
#50794=CARTESIAN_POINT('Ctrl Pts',(-25.437586446444,20.9379563343926,21.2457312394325));
#50795=CARTESIAN_POINT('Ctrl Pts',(-25.4390283804383,20.9389987099754,21.2456208306434));
#50796=CARTESIAN_POINT('Ctrl Pts',(-25.4424741162307,20.9414939833386,21.2453570326675));
#50797=CARTESIAN_POINT('Ctrl Pts',(-25.4444771126155,20.9429479990909,21.245203721492));
#50798=CARTESIAN_POINT('Ctrl Pts',(-25.4516512214461,20.9481684608988,21.2446547222017));
#50799=CARTESIAN_POINT('Ctrl Pts',(-25.4568128359416,20.9519480274436,21.244259941028));
#50800=CARTESIAN_POINT('Ctrl Pts',(-25.5336176212561,21.0085400443383,21.2383882031243));
#50801=CARTESIAN_POINT('Ctrl Pts',(-25.6030619142668,21.0642886397747,21.2331128075798));
#50802=CARTESIAN_POINT('Ctrl Pts',(-25.8952026840257,21.3194163486235,21.2106332411874));
#50803=CARTESIAN_POINT('Ctrl Pts',(-26.0918650738679,21.546342504079,21.1945976724144));
#50804=CARTESIAN_POINT('Ctrl Pts',(-26.2992994144198,21.8663121079944,21.1725912511314));
#50805=CARTESIAN_POINT('Ctrl Pts',(-26.3414719885852,21.9371789314685,21.1677606118491));
#50806=CARTESIAN_POINT('Ctrl Pts',(-26.4012692396846,22.0470424871649,21.1602834321609));
#50807=CARTESIAN_POINT('Ctrl Pts',(-26.4209127537955,22.0849039961281,21.1577088655693));
#50808=CARTESIAN_POINT('Ctrl Pts',(-26.4431651964723,22.1299597163883,21.1546438123051));
#50809=CARTESIAN_POINT('Ctrl Pts',(-26.4465078023684,22.1367884278796,21.1541792366905));
#50810=CARTESIAN_POINT('Ctrl Pts',(-26.4515956676129,22.1472764072274,21.153465639436));
#50811=CARTESIAN_POINT('Ctrl Pts',(-26.4533582540513,22.1509272790293,21.1532172225354));
#50812=CARTESIAN_POINT('Ctrl Pts',(-26.4565616631364,22.1575946518619,21.1527635251345));
#50813=CARTESIAN_POINT('Ctrl Pts',(-26.4580046921053,22.1606100916206,21.1525583217946));
#50814=CARTESIAN_POINT('Ctrl Pts',(-26.4608979412386,22.1666802362267,21.1521452196053));
#50815=CARTESIAN_POINT('Ctrl Pts',(-26.4623480505527,22.1697349889617,21.1519373172263));
#50816=CARTESIAN_POINT('Ctrl Pts',(-26.4664654128397,22.178443843313,21.1513445669054));
#50817=CARTESIAN_POINT('Ctrl Pts',(-26.469121014194,22.1841034085512,21.150959315377));
#50818=CARTESIAN_POINT('Ctrl Pts',(-26.4803602394371,22.2082385931714,21.1493161914307));
#50819=CARTESIAN_POINT('Ctrl Pts',(-26.4887848911462,22.2267873330876,21.1480528384583));
#50820=CARTESIAN_POINT('Ctrl Pts',(-26.6420104939896,22.572824274073,21.1244701309282));
#50821=CARTESIAN_POINT('Ctrl Pts',(-26.7313776087769,22.9220523620919,21.1000146521633));
#50822=CARTESIAN_POINT('Ctrl Pts',(-26.7692016465279,23.3692710965809,21.0698813376803));
#50823=CARTESIAN_POINT('Ctrl Pts',(-26.773027258957,23.4601788548242,21.063840734755));
#50824=CARTESIAN_POINT('Ctrl Pts',(-26.7730018072047,23.5533447254896,21.05780963281));
#50825=CARTESIAN_POINT('Ctrl Pts',(-26.7729989260515,23.5555565090896,21.0576665454831));
#50826=CARTESIAN_POINT('Ctrl Pts',(-26.7728873014182,23.6034208899777,21.0545720766094));
#50827=CARTESIAN_POINT('Ctrl Pts',(-26.7718107820078,23.6490690752659,21.0516608112858));
#50828=CARTESIAN_POINT('Ctrl Pts',(-26.769541542956,23.6996533018269,21.0484902808158));
#50829=CARTESIAN_POINT('Ctrl Pts',(-26.7693070011791,23.7046243277756,21.0481793015351));
#50830=CARTESIAN_POINT('Ctrl Pts',(-26.7689392265204,23.7120535928113,21.0477154497589));
#50831=CARTESIAN_POINT('Ctrl Pts',(-26.7688146914049,23.7145122254959,21.0475620923194));
#50832=CARTESIAN_POINT('Ctrl Pts',(-26.7685954786253,23.7187440494801,21.0472983914782));
#50833=CARTESIAN_POINT('Ctrl Pts',(-26.768502152638,23.7205173047894,21.0471879717434));
#50834=CARTESIAN_POINT('Ctrl Pts',(-26.7683060238771,23.7241861040194,21.0469596810447));
#50835=CARTESIAN_POINT('Ctrl Pts',(-26.7682030120461,23.7260816309643,21.0468418226378));
#50836=CARTESIAN_POINT('Ctrl Pts',(-26.7679566700315,23.7305418513955,21.0465647101373));
#50837=CARTESIAN_POINT('Ctrl Pts',(-26.7678119478885,23.733106473519,21.0464055349741));
#50838=CARTESIAN_POINT('Ctrl Pts',(-26.7673295353918,23.7414773773002,21.0458865168385));
#50839=CARTESIAN_POINT('Ctrl Pts',(-26.7669791909521,23.7472829612408,21.0455273848965));
#50840=CARTESIAN_POINT('Ctrl Pts',(-26.7581535166614,23.8872318797028,21.0368895022321));
#50841=CARTESIAN_POINT('Ctrl Pts',(-26.7413087671498,24.0207354106358,21.0290757419086));
#50842=CARTESIAN_POINT('Ctrl Pts',(-26.6882718021546,24.2993972774105,21.0129497331154));
#50843=CARTESIAN_POINT('Ctrl Pts',(-26.6502254734612,24.4438706194493,21.0046923196446));
#50844=CARTESIAN_POINT('Ctrl Pts',(-26.5585486132173,24.7142272253037,20.9886819832602));
#50845=CARTESIAN_POINT('Ctrl Pts',(-26.5066568509048,24.8403499684541,20.9809639523108));
#50846=CARTESIAN_POINT('Ctrl Pts',(-26.4355590366025,24.9861489744099,20.9714849461523));
#50847=CARTESIAN_POINT('Ctrl Pts',(-26.4238927951812,25.0093562995406,20.9699589125314));
#50848=CARTESIAN_POINT('Ctrl Pts',(-26.4096615937357,25.0368332000321,20.9681302095878));
#50849=CARTESIAN_POINT('Ctrl Pts',(-26.4073654619362,25.0412414555393,20.9678361441981));
#50850=CARTESIAN_POINT('Ctrl Pts',(-26.4031901239435,25.0492124650575,20.967303174538));
#50851=CARTESIAN_POINT('Ctrl Pts',(-26.4013144161027,25.0527770466902,20.9670643835585));
#50852=CARTESIAN_POINT('Ctrl Pts',(-26.3974786620677,25.0600334417291,20.9665773520772));
#50853=CARTESIAN_POINT('Ctrl Pts',(-26.3955181069003,25.0637249761414,20.9663290953305));
#50854=CARTESIAN_POINT('Ctrl Pts',(-26.3687145288299,25.1139573503009,20.9629442192677));
#50855=CARTESIAN_POINT('Ctrl Pts',(-26.3427407212253,25.1598829254286,20.9597705125149));
#50856=CARTESIAN_POINT('Ctrl Pts',(-26.311173177963,25.2126336074033,20.9560241672819));
#50857=CARTESIAN_POINT('Ctrl Pts',(-26.306663465352,25.2201005542173,20.9554914670565));
#50858=CARTESIAN_POINT('Ctrl Pts',(-26.2998927574783,25.2312089745229,20.9546953591865));
#50859=CARTESIAN_POINT('Ctrl Pts',(-26.2976546968246,25.2348644385419,20.9544327951914));
#50860=CARTESIAN_POINT('Ctrl Pts',(-26.2936479786439,25.2413794605155,20.9539637809001));
#50861=CARTESIAN_POINT('Ctrl Pts',(-26.2918821226178,25.244240741147,20.9537574341554));
#50862=CARTESIAN_POINT('Ctrl Pts',(-26.2881477534328,25.2502705409727,20.9533218122562));
#50863=CARTESIAN_POINT('Ctrl Pts',(-26.2861782115737,25.2534384144091,20.9530924992705));
#50864=CARTESIAN_POINT('Ctrl Pts',(-26.2809568396855,25.2618042071213,20.9524857278489));
#50865=CARTESIAN_POINT('Ctrl Pts',(-26.2776956799303,25.2669962597002,20.952107923928));
#50866=CARTESIAN_POINT('Ctrl Pts',(-26.2628288426025,25.2905162838023,20.9503908749893));
#50867=CARTESIAN_POINT('Ctrl Pts',(-26.2510533221876,25.3087357481076,20.9490453184085));
#50868=CARTESIAN_POINT('Ctrl Pts',(-26.1630777561412,25.4418860498269,20.9390954298873));
#50869=CARTESIAN_POINT('Ctrl Pts',(-26.0797652834811,25.5519241303697,20.9302197366731));
#50870=CARTESIAN_POINT('Ctrl Pts',(-25.7855138590326,25.8927570860636,20.9005066776176));
#50871=CARTESIAN_POINT('Ctrl Pts',(-25.5480825583942,26.0982655623259,20.8787385536476));
#50872=CARTESIAN_POINT('Ctrl Pts',(-25.246700280964,26.2907319727763,20.855626032057));
#50873=CARTESIAN_POINT('Ctrl Pts',(-25.2080770796704,26.3142678758738,20.852742807674));
#50874=CARTESIAN_POINT('Ctrl Pts',(-25.1642634226804,26.3397177167375,20.8495702199671));
#50875=CARTESIAN_POINT('Ctrl Pts',(-25.1595509793027,26.342439073161,20.84923024015));
#50876=CARTESIAN_POINT('Ctrl Pts',(-25.1528489461287,26.3462867807029,20.848748522453));
#50877=CARTESIAN_POINT('Ctrl Pts',(-25.1508650492827,26.3474229515662,20.8486061507337));
#50878=CARTESIAN_POINT('Ctrl Pts',(-25.1472263888802,26.349501661112,20.8483454390283));
#50879=CARTESIAN_POINT('Ctrl Pts',(-25.1455719964545,26.350444845536,20.8482270568815));
#50880=CARTESIAN_POINT('Ctrl Pts',(-25.1422029046419,26.3523616410342,20.8479862957927));
#50881=CARTESIAN_POINT('Ctrl Pts',(-25.1404881475576,26.3533351449371,20.8478639239));
#50882=CARTESIAN_POINT('Ctrl Pts',(-25.1362120997725,26.3557575611737,20.8475591828491));
#50883=CARTESIAN_POINT('Ctrl Pts',(-25.1336497093308,26.3572045441147,20.8473769394166));
#50884=CARTESIAN_POINT('Ctrl Pts',(-25.1241508416554,26.3625514126747,20.8467027143346));
#50885=CARTESIAN_POINT('Ctrl Pts',(-25.1172018345671,26.3664291546104,20.8462121548542));
#50886=CARTESIAN_POINT('Ctrl Pts',(-24.9968316091776,26.4330156616264,20.8377596558871));
#50887=CARTESIAN_POINT('Ctrl Pts',(-24.8797276158142,26.4888609453313,20.8302230754313));
#50888=CARTESIAN_POINT('Ctrl Pts',(-24.494364114994,26.6448651712481,20.8065735411277));
#50889=CARTESIAN_POINT('Ctrl Pts',(-24.2160600643983,26.7164302572485,20.7910796570363));
#50890=CARTESIAN_POINT('Ctrl Pts',(-23.8414481126276,26.7611139310924,20.7690468673939));
#50891=CARTESIAN_POINT('Ctrl Pts',(-23.7505304943422,26.768064229153,20.7636233801982));
#50892=CARTESIAN_POINT('Ctrl Pts',(-23.6502912030961,26.7714625129638,20.7575176537741));
#50893=CARTESIAN_POINT('Ctrl Pts',(-23.6411346500995,26.7717338550978,20.756958775833));
#50894=CARTESIAN_POINT('Ctrl Pts',(-23.6274995895303,26.7720797331281,20.7561248126053));
#50895=CARTESIAN_POINT('Ctrl Pts',(-23.6230218268349,26.7721839793198,20.7558506599002));
#50896=CARTESIAN_POINT('Ctrl Pts',(-23.6153386226538,26.7723468260231,20.7553797695941));
#50897=CARTESIAN_POINT('Ctrl Pts',(-23.6121332752645,26.7724099788478,20.7551831751004));
#50898=CARTESIAN_POINT('Ctrl Pts',(-23.6058829070043,26.77252379566,20.7547995360351));
#50899=CARTESIAN_POINT('Ctrl Pts',(-23.6028378976609,26.7725749265559,20.7546125063621));
#50900=CARTESIAN_POINT('Ctrl Pts',(-23.5955316897556,26.7726872512719,20.7541634297809));
#50901=CARTESIAN_POINT('Ctrl Pts',(-23.5912704419927,26.7727443090068,20.7539012533242));
#50902=CARTESIAN_POINT('Ctrl Pts',(-23.5785803446872,26.7728890533702,20.7531197086612));
#50903=CARTESIAN_POINT('Ctrl Pts',(-23.5701512995601,26.7729521225188,20.7525995685115));
#50904=CARTESIAN_POINT('Ctrl Pts',(-23.5073406835446,26.7731756643591,20.7487159143166));
#50905=CARTESIAN_POINT('Ctrl Pts',(-23.4529659093277,26.771992694252,20.7453104418377));
#50906=CARTESIAN_POINT('Ctrl Pts',(-23.2670113586736,26.7632354247391,20.7335055310453));
#50907=CARTESIAN_POINT('Ctrl Pts',(-23.13589320398,26.7489684563823,20.7249026666826));
#50908=CARTESIAN_POINT('Ctrl Pts',(-22.7744937684843,26.6870499851088,20.7004848184321));
#50909=CARTESIAN_POINT('Ctrl Pts',(-22.548004468906,26.6221886440398,20.6843225063893));
#50910=CARTESIAN_POINT('Ctrl Pts',(-22.2470990819667,26.4991579554132,20.6628185173757));
#50911=CARTESIAN_POINT('Ctrl Pts',(-22.1650760488437,26.4615309056342,20.6569622107838));
#50912=CARTESIAN_POINT('Ctrl Pts',(-22.0814970208994,26.4188563737905,20.6510791518621));
#50913=CARTESIAN_POINT('Ctrl Pts',(-22.0782651224947,26.4171993084604,20.6508517966473));
#50914=CARTESIAN_POINT('Ctrl Pts',(-22.075036015346,26.4155367745563,20.6506247785903));
#50915=CARTESIAN_POINT('',(-26.7730010559745,23.5472555922587,20.8139447069714));
#50916=CARTESIAN_POINT('Ctrl Pts',(-22.0750362907684,26.4155369163599,20.4058188292237));
#50917=CARTESIAN_POINT('Ctrl Pts',(-22.1523064855167,26.4553201388708,20.4116349747003));
#50918=CARTESIAN_POINT('Ctrl Pts',(-22.2311828084613,26.4919760493018,20.4175106537931));
#50919=CARTESIAN_POINT('Ctrl Pts',(-22.5058363542375,26.6063346039196,20.437648250673));
#50920=CARTESIAN_POINT('Ctrl Pts',(-22.7076827246404,26.6680305312452,20.4519346842536));
#50921=CARTESIAN_POINT('Ctrl Pts',(-22.9264732946551,26.7120835996383,20.4660137596104));
#50922=CARTESIAN_POINT('Ctrl Pts',(-22.9388368567904,26.7144976428897,20.4668045901101));
#50923=CARTESIAN_POINT('Ctrl Pts',(-22.9547765093788,26.7175130216683,20.4678177616358));
#50924=CARTESIAN_POINT('Ctrl Pts',(-22.9583396781558,26.7181808576871,20.4680438359248));
#50925=CARTESIAN_POINT('Ctrl Pts',(-22.9637832674892,26.7191916314723,20.4683885823665));
#50926=CARTESIAN_POINT('Ctrl Pts',(-22.9656628636199,26.7195389081493,20.4685075028351));
#50927=CARTESIAN_POINT('Ctrl Pts',(-22.9691922350996,26.7201877529406,20.468730584559));
#50928=CARTESIAN_POINT('Ctrl Pts',(-22.9708419306316,26.7204897043026,20.468834767424));
#50929=CARTESIAN_POINT('Ctrl Pts',(-22.9746350755554,26.7211809213828,20.4690741088026));
#50930=CARTESIAN_POINT('Ctrl Pts',(-22.9767786805125,26.7215693008648,20.4692092157328));
#50931=CARTESIAN_POINT('Ctrl Pts',(-22.981177103669,26.7223616040677,20.4694861322266));
#50932=CARTESIAN_POINT('Ctrl Pts',(-22.9834319627591,26.7227652980241,20.4696279285624));
#50933=CARTESIAN_POINT('Ctrl Pts',(-22.9943115308698,26.7247011293229,20.4703112986211));
#50934=CARTESIAN_POINT('Ctrl Pts',(-23.0029421421396,26.7262005219933,20.4708510145859));
#50935=CARTESIAN_POINT('Ctrl Pts',(-23.1114218682976,26.7445913277403,20.4776059942336));
#50936=CARTESIAN_POINT('Ctrl Pts',(-23.2120190386022,26.7568044977116,20.4835642969508));
#50937=CARTESIAN_POINT('Ctrl Pts',(-23.4775917041439,26.7764057110331,20.4988830161048));
#50938=CARTESIAN_POINT('Ctrl Pts',(-23.642846677961,26.7758960733521,20.5080116531318));
#50939=CARTESIAN_POINT('Ctrl Pts',(-24.038989460624,26.7441932777891,20.5302612977874));
#50940=CARTESIAN_POINT('Ctrl Pts',(-24.2679119404094,26.7006593014154,20.5434666341156));
#50941=CARTESIAN_POINT('Ctrl Pts',(-24.5044768630513,26.6285309283383,20.5584720689336));
#50942=CARTESIAN_POINT('Ctrl Pts',(-24.5187747733948,26.6240623204228,20.559384166739));
#50943=CARTESIAN_POINT('Ctrl Pts',(-24.5382971150868,26.6178111578869,20.5606368090709));
#50944=CARTESIAN_POINT('Ctrl Pts',(-24.5435490478157,26.6161145726807,20.560974519208));
#50945=CARTESIAN_POINT('Ctrl Pts',(-24.5518721152959,26.613402256363,20.5615108651133));
#50946=CARTESIAN_POINT('Ctrl Pts',(-24.5549461401831,26.6123953727339,20.5617092084694));
#50947=CARTESIAN_POINT('Ctrl Pts',(-24.5609012922427,26.6104348556145,20.5620939367427));
#50948=CARTESIAN_POINT('Ctrl Pts',(-24.5637825997442,26.6094817767644,20.5622803031566));
#50949=CARTESIAN_POINT('Ctrl Pts',(-24.5706358335474,26.6072041195578,20.5627241082573));
#50950=CARTESIAN_POINT('Ctrl Pts',(-24.5746065257973,26.6058758703509,20.5629816682379));
#50951=CARTESIAN_POINT('Ctrl Pts',(-24.5828242414452,26.6031091174612,20.563515595594));
#50952=CARTESIAN_POINT('Ctrl Pts',(-24.587070871416,26.6016694811014,20.5637920001121));
#50953=CARTESIAN_POINT('Ctrl Pts',(-24.6112042972258,26.5934318906887,20.5653655957975));
#50954=CARTESIAN_POINT('Ctrl Pts',(-24.6310268506934,26.586448522978,20.566668934191));
#50955=CARTESIAN_POINT('Ctrl Pts',(-24.682777722786,26.5676459952776,20.5701006378737));
#50956=CARTESIAN_POINT('Ctrl Pts',(-24.7145888631145,26.5555141486923,20.5722393412261));
#50957=CARTESIAN_POINT('Ctrl Pts',(-24.856988589716,26.4986067439709,20.5819483954631));
#50958=CARTESIAN_POINT('Ctrl Pts',(-24.9652199125761,26.4482196433584,20.5897040854235));
#50959=CARTESIAN_POINT('Ctrl Pts',(-25.1612393851782,26.3433605112384,20.604441217498));
#50960=CARTESIAN_POINT('Ctrl Pts',(-25.249692367879,26.2904410367293,20.6113746009179));
#50961=CARTESIAN_POINT('Ctrl Pts',(-25.5259268831231,26.1066500617984,20.6338118853973));
#50962=CARTESIAN_POINT('Ctrl Pts',(-25.7023821753626,25.9599863460388,20.6494234485337));
#50963=CARTESIAN_POINT('Ctrl Pts',(-25.8713237679461,25.7860815953571,20.6647326967004));
#50964=CARTESIAN_POINT('Ctrl Pts',(-25.8807578478583,25.776246303639,20.6655887769634));
#50965=CARTESIAN_POINT('Ctrl Pts',(-25.8926679872287,25.7636709341808,20.6666706997264));
#50966=CARTESIAN_POINT('Ctrl Pts',(-25.8952019304493,25.7609862353312,20.6669009515372));
#50967=CARTESIAN_POINT('Ctrl Pts',(-25.899211145194,25.7567238457955,20.6672653548127));
#50968=CARTESIAN_POINT('Ctrl Pts',(-25.9006894434654,25.7551490262573,20.6673997406585));
#50969=CARTESIAN_POINT('Ctrl Pts',(-25.9033141903275,25.7523472646403,20.6676383810484));
#50970=CARTESIAN_POINT('Ctrl Pts',(-25.9044612566809,25.7511209197223,20.66774268363));
#50971=CARTESIAN_POINT('Ctrl Pts',(-25.9071257028015,25.7482678561199,20.6679849896626));
#50972=CARTESIAN_POINT('Ctrl Pts',(-25.9086423546224,25.7466404651604,20.668122936356));
#50973=CARTESIAN_POINT('Ctrl Pts',(-25.91176124163,25.7432868958118,20.6684066618127));
#50974=CARTESIAN_POINT('Ctrl Pts',(-25.9133632726611,25.7415605281462,20.6685524248168));
#50975=CARTESIAN_POINT('Ctrl Pts',(-25.9174593716336,25.7371368074287,20.6689251857035));
#50976=CARTESIAN_POINT('Ctrl Pts',(-25.919950730959,25.7344369339888,20.6691519772616));
#50977=CARTESIAN_POINT('Ctrl Pts',(-25.9533030182125,25.6981689945561,20.6721890899786));
#50978=CARTESIAN_POINT('Ctrl Pts',(-25.9834546994167,25.6639517788309,20.674946405766));
#50979=CARTESIAN_POINT('Ctrl Pts',(-26.0900465954939,25.5376824124136,20.6847866983229));
#50980=CARTESIAN_POINT('Ctrl Pts',(-26.1620782633659,25.4420250354175,20.6916186736561));
#50981=CARTESIAN_POINT('Ctrl Pts',(-26.2542866093905,25.3042325015594,20.7009601914171));
#50982=CARTESIAN_POINT('Ctrl Pts',(-26.2791186285383,25.2653431866167,20.7035448255219));
#50983=CARTESIAN_POINT('Ctrl Pts',(-26.32806496526,25.1849328068545,20.7088096288835));
#50984=CARTESIAN_POINT('Ctrl Pts',(-26.3521033959923,25.1433794116713,20.7114887703956));
#50985=CARTESIAN_POINT('Ctrl Pts',(-26.4926565797461,24.8873879938935,20.7278213538405));
#50986=CARTESIAN_POINT('Ctrl Pts',(-26.5854126861312,24.6608607622563,20.7416314138394));
#50987=CARTESIAN_POINT('Ctrl Pts',(-26.6558067190603,24.4115754219983,20.7573471200967));
#50988=CARTESIAN_POINT('Ctrl Pts',(-26.6597939469514,24.397067804836,20.7582631894038));
#50989=CARTESIAN_POINT('Ctrl Pts',(-26.6651073179554,24.3771913415142,20.7595204413289));
#50990=CARTESIAN_POINT('Ctrl Pts',(-26.6665214895856,24.3718460541619,20.7598587623665));
#50991=CARTESIAN_POINT('Ctrl Pts',(-26.6687416724536,24.3633660033418,20.7603958410737));
#50992=CARTESIAN_POINT('Ctrl Pts',(-26.6695567335596,24.3602336024056,20.7605943048999));
#50993=CARTESIAN_POINT('Ctrl Pts',(-26.6711267140367,24.3541624189672,20.7609791129234));
#50994=CARTESIAN_POINT('Ctrl Pts',(-26.6718822050751,24.3512237865074,20.7611654383721));
#50995=CARTESIAN_POINT('Ctrl Pts',(-26.6736691436834,24.3442322044633,20.761608904425));
#50996=CARTESIAN_POINT('Ctrl Pts',(-26.6746968523132,24.3401783129604,20.7618661657917));
#50997=CARTESIAN_POINT('Ctrl Pts',(-26.6768084680937,24.3317802571916,20.7623993805358));
#50998=CARTESIAN_POINT('Ctrl Pts',(-26.6778912184387,24.3274358138165,20.7626753707722));
#50999=CARTESIAN_POINT('Ctrl Pts',(-26.6806859772603,24.3161216545832,20.7633945245292));
#51000=CARTESIAN_POINT('Ctrl Pts',(-26.6823837565231,24.3091484795207,20.7638381472929));
#51001=CARTESIAN_POINT('Ctrl Pts',(-26.7433977334457,24.0548572535618,20.7800303986883));
#51002=CARTESIAN_POINT('Ctrl Pts',(-26.7732375911853,23.8014572351736,20.7967802754889));
#51003=CARTESIAN_POINT('Ctrl Pts',(-26.7730011374811,23.547254799421,20.8139446178767));
#51004=CARTESIAN_POINT('Ctrl Pts',(-26.7730011382095,23.5472555825959,20.8139445649949));
#51005=CARTESIAN_POINT('Ctrl Pts',(-26.7727921327512,23.3225030001619,20.8291203840233));
#51006=CARTESIAN_POINT('Ctrl Pts',(-26.7490729694072,23.098366539446,20.8445032138022));
#51007=CARTESIAN_POINT('Ctrl Pts',(-26.6958354141065,22.8485668667248,20.8608633304296));
#51008=CARTESIAN_POINT('Ctrl Pts',(-26.6890289325242,22.8187217283387,20.8628040760745));
#51009=CARTESIAN_POINT('Ctrl Pts',(-26.6808645071488,22.7851369604993,20.8649687743573));
#51010=CARTESIAN_POINT('Ctrl Pts',(-26.6799239803867,22.7812988258202,20.8652158755795));
#51011=CARTESIAN_POINT('Ctrl Pts',(-26.6783836822329,22.7750627632368,20.8656168825299));
#51012=CARTESIAN_POINT('Ctrl Pts',(-26.677788211022,22.7726637928861,20.8657710329596));
#51013=CARTESIAN_POINT('Ctrl Pts',(-26.6766313305607,22.7680259044466,20.866068825276));
#51014=CARTESIAN_POINT('Ctrl Pts',(-26.6760702750183,22.7657869008487,20.8662124874847));
#51015=CARTESIAN_POINT('Ctrl Pts',(-26.675095017184,22.761912599239,20.8664608987368));
#51016=CARTESIAN_POINT('Ctrl Pts',(-26.6746819371511,22.7602770266377,20.866565713036));
#51017=CARTESIAN_POINT('Ctrl Pts',(-26.6738175161176,22.7568656729399,20.8667842119649));
#51018=CARTESIAN_POINT('Ctrl Pts',(-26.6733659462046,22.7550899573075,20.866897882724));
#51019=CARTESIAN_POINT('Ctrl Pts',(-26.6721135711785,22.7501827471399,20.8672118366497));
#51020=CARTESIAN_POINT('Ctrl Pts',(-26.6713095661025,22.7470520597101,20.8674119332869));
#51021=CARTESIAN_POINT('Ctrl Pts',(-26.668141971071,22.7347944436667,20.8681946141552));
#51022=CARTESIAN_POINT('Ctrl Pts',(-26.6657430147599,22.725676577237,20.8687751628499));
#51023=CARTESIAN_POINT('Ctrl Pts',(-26.6241969350058,22.5705396240489,20.8786268739988));
#51024=CARTESIAN_POINT('Ctrl Pts',(-26.5748570347339,22.4274201563866,20.8873245034422));
#51025=CARTESIAN_POINT('Ctrl Pts',(-26.4785941222552,22.2012217046486,20.9012044275201));
#51026=CARTESIAN_POINT('Ctrl Pts',(-26.437730163035,22.1158389861431,20.9064762155067));
#51027=CARTESIAN_POINT('Ctrl Pts',(-26.3729040947183,21.9944225721862,20.9141700201257));
#51028=CARTESIAN_POINT('Ctrl Pts',(-26.3518820032506,21.9568784520925,20.9165775372235));
#51029=CARTESIAN_POINT('Ctrl Pts',(-26.3091304509788,21.883990097554,20.9213244954035));
#51030=CARTESIAN_POINT('Ctrl Pts',(-26.2874577979167,21.8486224010182,20.9236628076672));
#51031=CARTESIAN_POINT('Ctrl Pts',(-26.2017602772345,21.7146476270852,20.9326818725866));
#51032=CARTESIAN_POINT('Ctrl Pts',(-26.1330455956362,21.6191609344149,20.939456392972));
#51033=CARTESIAN_POINT('Ctrl Pts',(-26.0242522802773,21.4842039971169,20.9497337895205));
#51034=CARTESIAN_POINT('Ctrl Pts',(-25.9881108910112,21.4416801848879,20.953083329168));
#51035=CARTESIAN_POINT('Ctrl Pts',(-25.9459926343167,21.3946550029867,20.9569250267958));
#51036=CARTESIAN_POINT('Ctrl Pts',(-25.9410812066175,21.3892088970462,20.9573720887902));
#51037=CARTESIAN_POINT('Ctrl Pts',(-25.9330971512043,21.3804161963649,20.9580973752472));
#51038=CARTESIAN_POINT('Ctrl Pts',(-25.9300359417327,21.3770592306239,20.9583751162673));
#51039=CARTESIAN_POINT('Ctrl Pts',(-25.924111034239,21.3705894240193,20.9589120199538));
#51040=CARTESIAN_POINT('Ctrl Pts',(-25.9212482847561,21.3674757241033,20.9591711419717));
#51041=CARTESIAN_POINT('Ctrl Pts',(-25.9163169114261,21.362133211301,20.9596170042816));
#51042=CARTESIAN_POINT('Ctrl Pts',(-25.9142512425142,21.3599016683733,20.9598036180266));
#51043=CARTESIAN_POINT('Ctrl Pts',(-25.9099931098655,21.3553146461409,20.9601879929204));
#51044=CARTESIAN_POINT('Ctrl Pts',(-25.9078002707893,21.3529595208566,20.9603857700791));
#51045=CARTESIAN_POINT('Ctrl Pts',(-25.9018950916233,21.3466363310161,20.9609179262825));
#51046=CARTESIAN_POINT('Ctrl Pts',(-25.8981762491165,21.3426743776647,20.961252585113));
#51047=CARTESIAN_POINT('Ctrl Pts',(-25.884545626096,21.3282260874537,20.9624775037632));
#51048=CARTESIAN_POINT('Ctrl Pts',(-25.8745735838389,21.3177970662608,20.9633703702267));
#51049=CARTESIAN_POINT('Ctrl Pts',(-25.7040340205788,21.1418236369081,20.978586120084));
#51050=CARTESIAN_POINT('Ctrl Pts',(-25.5262578946383,20.9939531096286,20.9937178731558));
#51051=CARTESIAN_POINT('Ctrl Pts',(-25.2617521789707,20.8181345998484,21.0151120521346));
#51052=CARTESIAN_POINT('Ctrl Pts',(-25.187313697625,20.7728923044465,21.0210163202554));
#51053=CARTESIAN_POINT('Ctrl Pts',(-25.0303236950414,20.6859831761106,21.0331509988955));
#51054=CARTESIAN_POINT('Ctrl Pts',(-24.9476218454735,20.644738790083,21.0393741091326));
#51055=CARTESIAN_POINT('Ctrl Pts',(-24.8022532128371,20.5798865100468,21.0499124629924));
#51056=CARTESIAN_POINT('Ctrl Pts',(-24.7404110827491,20.5545716480462,21.0542761233911));
#51057=CARTESIAN_POINT('Ctrl Pts',(-24.6600439154961,20.5245557835005,21.0597568338974));
#51058=CARTESIAN_POINT('Ctrl Pts',(-24.6422066007105,20.5180727747416,21.0609614422618));
#51059=CARTESIAN_POINT('Ctrl Pts',(-24.6133983214508,20.5078895360428,21.0628867985817));
#51060=CARTESIAN_POINT('Ctrl Pts',(-24.6024631629157,20.5040902962169,21.0636129898798));
#51061=CARTESIAN_POINT('Ctrl Pts',(-24.5891467335978,20.4995439872799,21.0644914800653));
#51062=CARTESIAN_POINT('Ctrl Pts',(-24.5867849486927,20.4987407204238,21.0646470653156));
#51063=CARTESIAN_POINT('Ctrl Pts',(-24.5822204951197,20.4971942143576,21.0649473206063));
#51064=CARTESIAN_POINT('Ctrl Pts',(-24.5800179513921,20.4964506148909,21.0650920119377));
#51065=CARTESIAN_POINT('Ctrl Pts',(-24.5760450698021,20.4951141196346,21.0653526484068));
#51066=CARTESIAN_POINT('Ctrl Pts',(-24.5742750256108,20.4945203804592,21.0654686436767));
#51067=CARTESIAN_POINT('Ctrl Pts',(-24.5704675102114,20.4932468769059,21.0657178870387));
#51068=CARTESIAN_POINT('Ctrl Pts',(-24.5684298807565,20.4925676130474,21.065851104851));
#51069=CARTESIAN_POINT('Ctrl Pts',(-24.5629373876685,20.490742735431,21.0662097509332));
#51070=CARTESIAN_POINT('Ctrl Pts',(-24.5594812467131,20.489600932436,21.0664349524636));
#51071=CARTESIAN_POINT('Ctrl Pts',(-24.5435500831238,20.4843676835179,21.0674708652545));
#51072=CARTESIAN_POINT('Ctrl Pts',(-24.5310518349036,20.4803465610326,21.0682774615541));
#51073=CARTESIAN_POINT('Ctrl Pts',(-24.3011750431544,20.4079343535329,21.0830073033051));
#51074=CARTESIAN_POINT('Ctrl Pts',(-24.077132272913,20.3627014815647,21.0956590075224));
#51075=CARTESIAN_POINT('Ctrl Pts',(-23.6933945807891,20.3268353959293,21.1171940481115));
#51076=CARTESIAN_POINT('Ctrl Pts',(-23.5357730024209,20.3236918946058,21.1259991396484));
#51077=CARTESIAN_POINT('Ctrl Pts',(-23.2775269301755,20.3374693997469,21.1409600060509));
#51078=CARTESIAN_POINT('Ctrl Pts',(-23.176810728117,20.3476141174725,21.1469264847005));
#51079=CARTESIAN_POINT('Ctrl Pts',(-23.0565669544134,20.3654749477016,21.1542793837881));
#51080=CARTESIAN_POINT('Ctrl Pts',(-23.0364179664536,20.3686636647107,21.1555192090957));
#51081=CARTESIAN_POINT('Ctrl Pts',(-23.0119189485747,20.3727795955675,21.1570365092037));
#51082=CARTESIAN_POINT('Ctrl Pts',(-23.0075384791076,20.3735248500468,21.157308187671));
#51083=CARTESIAN_POINT('Ctrl Pts',(-22.9990622995055,20.374984956148,21.1578346300345));
#51084=CARTESIAN_POINT('Ctrl Pts',(-22.9949664018427,20.3756986792431,21.1580893575627));
#51085=CARTESIAN_POINT('Ctrl Pts',(-22.9878869511581,20.3769464161276,21.158530223052));
#51086=CARTESIAN_POINT('Ctrl Pts',(-22.9849027421508,20.3774767178956,21.1587162424331));
#51087=CARTESIAN_POINT('Ctrl Pts',(-22.9787231375743,20.3785838451094,21.1591018219234));
#51088=CARTESIAN_POINT('Ctrl Pts',(-22.9755278578233,20.3791612912977,21.1593014016571));
#51089=CARTESIAN_POINT('Ctrl Pts',(-22.9677786809363,20.3805738080612,21.1597859303523));
#51090=CARTESIAN_POINT('Ctrl Pts',(-22.9632257093455,20.3814138631338,21.160071038233));
#51091=CARTESIAN_POINT('Ctrl Pts',(-22.9462243019876,20.3845886400384,21.1611372746563));
#51092=CARTESIAN_POINT('Ctrl Pts',(-22.9337879809414,20.3869869046054,21.1619204313958));
#51093=CARTESIAN_POINT('Ctrl Pts',(-22.7251617949627,20.4284961387105,21.175113338792));
#51094=CARTESIAN_POINT('Ctrl Pts',(-22.533056844298,20.4857095673268,21.1881221420755));
#51095=CARTESIAN_POINT('Ctrl Pts',(-22.2374529887695,20.6046200509834,21.2094483280828));
#51096=CARTESIAN_POINT('Ctrl Pts',(-22.129915157384,20.6549402092976,21.2174958706886));
#51097=CARTESIAN_POINT('Ctrl Pts',(-21.9261477253604,20.7643785578314,21.2331388246394));
#51098=CARTESIAN_POINT('Ctrl Pts',(-21.8297522837839,20.8228559415908,21.2407254515604));
#51099=CARTESIAN_POINT('Ctrl Pts',(-21.6947137898143,20.9147900048912,21.2514523838317));
#51100=CARTESIAN_POINT('Ctrl Pts',(-21.6534909437703,20.9443011012999,21.2547407511839));
#51101=CARTESIAN_POINT('Ctrl Pts',(-21.5992484807865,20.9851022524049,21.2590685511161));
#51102=CARTESIAN_POINT('Ctrl Pts',(-21.5856003573141,20.9955402924251,21.2601575485867));
#51103=CARTESIAN_POINT('Ctrl Pts',(-21.5635678890573,21.0126716449259,21.2619147634004));
#51104=CARTESIAN_POINT('Ctrl Pts',(-21.5551325360386,21.0192983960233,21.2625873428073));
#51105=CARTESIAN_POINT('Ctrl Pts',(-21.5448206954604,21.0274828917107,21.2634091442458));
#51106=CARTESIAN_POINT('Ctrl Pts',(-21.5429128174517,21.0290007041448,21.2635611756874));
#51107=CARTESIAN_POINT('Ctrl Pts',(-21.5392209425244,21.0319446223573,21.2638553313842));
#51108=CARTESIAN_POINT('Ctrl Pts',(-21.5374367364749,21.0333704618583,21.2639974745525));
#51109=CARTESIAN_POINT('Ctrl Pts',(-21.5341987584375,21.0359637212908,21.2642554043354));
#51110=CARTESIAN_POINT('Ctrl Pts',(-21.5327444888813,21.037130502023,21.2643712362386));
#51111=CARTESIAN_POINT('Ctrl Pts',(-21.5298154179576,21.0394847174763,21.2646045114512));
#51112=CARTESIAN_POINT('Ctrl Pts',(-21.5283406564428,21.0406721850546,21.264721951451));
#51113=CARTESIAN_POINT('Ctrl Pts',(-21.5241149268194,21.0440808555849,21.2650584281871));
#51114=CARTESIAN_POINT('Ctrl Pts',(-21.5213665554737,21.0463052958682,21.265277230641));
#51115=CARTESIAN_POINT('Ctrl Pts',(-21.5094538822647,21.055979507756,21.2662254785313));
#51116=CARTESIAN_POINT('Ctrl Pts',(-21.5003267579419,21.0634752240618,21.2669516365414));
#51117=CARTESIAN_POINT('Ctrl Pts',(-21.3429697090199,21.1941608836205,21.2794688742194));
#51118=CARTESIAN_POINT('Ctrl Pts',(-21.2060186076234,21.3303749077204,21.290341154348));
#51119=CARTESIAN_POINT('Ctrl Pts',(-20.9830677574113,21.5959300012872,21.3097517552693));
#51120=CARTESIAN_POINT('Ctrl Pts',(-20.8926622071128,21.720764605568,21.3182942230691));
#51121=CARTESIAN_POINT('Ctrl Pts',(-20.7539003391431,21.9444863795487,21.3333094040662));
#51122=CARTESIAN_POINT('Ctrl Pts',(-20.7010439386487,22.0402599832638,21.3396520222094));
#51123=CARTESIAN_POINT('Ctrl Pts',(-20.6316748945658,22.1826167835442,21.3490880874659));
#51124=CARTESIAN_POINT('Ctrl Pts',(-20.6112009948454,22.2271884265678,21.352043084181));
#51125=CARTESIAN_POINT('Ctrl Pts',(-20.5886419645478,22.2794095243182,21.3555118811041));
#51126=CARTESIAN_POINT('Ctrl Pts',(-20.5855573468342,22.2866222218401,21.3559911276612));
#51127=CARTESIAN_POINT('Ctrl Pts',(-20.5808811351877,22.2976678853251,21.3567252970675));
#51128=CARTESIAN_POINT('Ctrl Pts',(-20.5792705450404,22.3014928184456,21.356979572175));
#51129=CARTESIAN_POINT('Ctrl Pts',(-20.5764968737343,22.3081156510503,21.3574199274378));
#51130=CARTESIAN_POINT('Ctrl Pts',(-20.5753303389889,22.3109121060032,21.3576058898303));
#51131=CARTESIAN_POINT('Ctrl Pts',(-20.57292065159,22.3167116922946,21.3579916116321));
#51132=CARTESIAN_POINT('Ctrl Pts',(-20.5716780952815,22.3197150664502,21.358191391055));
#51133=CARTESIAN_POINT('Ctrl Pts',(-20.5686721361914,22.327011978183,21.3586768435755));
#51134=CARTESIAN_POINT('Ctrl Pts',(-20.5669134651032,22.331307446794,21.358962676875));
#51135=CARTESIAN_POINT('Ctrl Pts',(-20.5603617259512,22.3474088650356,21.3600343573398));
#51136=CARTESIAN_POINT('Ctrl Pts',(-20.5556294573177,22.3592392859217,21.3608222594028));
#51137=CARTESIAN_POINT('Ctrl Pts',(-20.4802408410799,22.5509968637151,21.37360207209));
#51138=CARTESIAN_POINT('Ctrl Pts',(-20.4258562455587,22.7368602445359,21.3861513337721));
#51139=CARTESIAN_POINT('Ctrl Pts',(-20.3442029508427,23.1507244204699,21.4143419722727));
#51140=CARTESIAN_POINT('Ctrl Pts',(-20.3239437527184,23.3790652436216,21.4300617275792));
#51141=CARTESIAN_POINT('Ctrl Pts',(-20.3290578705046,23.6662949112184,21.4490063443225));
#51142=CARTESIAN_POINT('Ctrl Pts',(-20.3317047874976,23.7249300410336,21.4528265863884));
#51143=CARTESIAN_POINT('Ctrl Pts',(-20.3379328850167,23.8107705269663,21.4583199875463));
#51144=CARTESIAN_POINT('Ctrl Pts',(-20.3402620674178,23.8380519064616,21.460051075185));
#51145=CARTESIAN_POINT('Ctrl Pts',(-20.3433680176967,23.8696716290291,21.4620376861545));
#51146=CARTESIAN_POINT('Ctrl Pts',(-20.3438062345163,23.8740410270414,21.4623117690602));
#51147=CARTESIAN_POINT('Ctrl Pts',(-20.3444884906843,23.8807064725274,21.4627291945464));
#51148=CARTESIAN_POINT('Ctrl Pts',(-20.3447260667965,23.8830031538801,21.4628729010207));
#51149=CARTESIAN_POINT('Ctrl Pts',(-20.345141498621,23.8869774552983,21.4631213617196));
#51150=CARTESIAN_POINT('Ctrl Pts',(-20.3453182030785,23.8886551880261,21.4632261812815));
#51151=CARTESIAN_POINT('Ctrl Pts',(-20.345689535868,23.8921544534432,21.4634446644937));
#51152=CARTESIAN_POINT('Ctrl Pts',(-20.3458843993825,23.8939759539105,21.4635583143144));
#51153=CARTESIAN_POINT('Ctrl Pts',(-20.3464271993913,23.8990092365172,21.4638721426703));
#51154=CARTESIAN_POINT('Ctrl Pts',(-20.3467784135314,23.9022206744904,21.4640721349297));
#51155=CARTESIAN_POINT('Ctrl Pts',(-20.3481722795643,23.9147910029119,21.4648540197704));
#51156=CARTESIAN_POINT('Ctrl Pts',(-20.349251133385,23.9241459540982,21.4654338819899));
#51157=CARTESIAN_POINT('Ctrl Pts',(-20.3678383229033,24.0793391451392,21.4750218515815));
#51158=CARTESIAN_POINT('Ctrl Pts',(-20.3952587229793,24.2238394442988,21.4834886618475));
#51159=CARTESIAN_POINT('Ctrl Pts',(-20.4779894461166,24.5400448355368,21.5019653230839));
#51160=CARTESIAN_POINT('Ctrl Pts',(-20.5380265742129,24.7099877412166,21.511873670238));
#51161=CARTESIAN_POINT('Ctrl Pts',(-20.6641771469372,24.9899966658131,21.5292730739882));
#51162=CARTESIAN_POINT('Ctrl Pts',(-20.7232348438092,25.1027538509832,21.5366013667223));
#51163=CARTESIAN_POINT('Ctrl Pts',(-20.8164992027969,25.2577647350456,21.5473562742163));
#51164=CARTESIAN_POINT('Ctrl Pts',(-20.8453487016055,25.3031073269847,21.5505896710549));
#51165=CARTESIAN_POINT('Ctrl Pts',(-20.8797457091292,25.3542963018213,21.5543498233421));
#51166=CARTESIAN_POINT('Ctrl Pts',(-20.8841987414649,25.3608706028859,21.5548348674714));
#51167=CARTESIAN_POINT('Ctrl Pts',(-20.8910538229761,25.3709110866383,21.5555789236728));
#51168=CARTESIAN_POINT('Ctrl Pts',(-20.8934384767695,25.3743891558063,21.5558372740943));
#51169=CARTESIAN_POINT('Ctrl Pts',(-20.8975533697025,25.3803656304476,21.5562822539938));
#51170=CARTESIAN_POINT('Ctrl Pts',(-20.8992803330538,25.3828662935632,21.5564687583272));
#51171=CARTESIAN_POINT('Ctrl Pts',(-20.9028459573322,25.3880137726772,21.5568533226747));
#51172=CARTESIAN_POINT('Ctrl Pts',(-20.9046850561564,25.3906602802879,21.5570513993143));
#51173=CARTESIAN_POINT('Ctrl Pts',(-20.9091250170645,25.3970290839555,21.5575289353297));
#51174=CARTESIAN_POINT('Ctrl Pts',(-20.9117297775595,25.4007486430388,21.5578085440082));
#51175=CARTESIAN_POINT('Ctrl Pts',(-20.9197574111078,25.4121605754442,21.5586686144669));
#51176=CARTESIAN_POINT('Ctrl Pts',(-20.9252060905819,25.4198346566076,21.5592500682428));
#51177=CARTESIAN_POINT('Ctrl Pts',(-20.9357194584114,25.4345054273612,21.560367638263));
#51178=CARTESIAN_POINT('Ctrl Pts',(-20.940778819584,25.4415058488317,21.5609035446771));
#51179=CARTESIAN_POINT('Ctrl Pts',(-20.9585635744139,25.4659066287333,21.5627808116796));
#51180=CARTESIAN_POINT('Ctrl Pts',(-20.9714351430267,25.4831992744263,21.5641278470677));
#51181=CARTESIAN_POINT('Ctrl Pts',(-20.9870922822228,25.5037994980044,21.5657528767401));
#51182=CARTESIAN_POINT('Ctrl Pts',(-20.9897124830592,25.5072325707068,21.5660243768376));
#51183=CARTESIAN_POINT('Ctrl Pts',(-20.9933219173451,25.5119421105574,21.5663977694145));
#51184=CARTESIAN_POINT('Ctrl Pts',(-20.9943052300207,25.5132231278746,21.5664994302704));
#51185=CARTESIAN_POINT('Ctrl Pts',(-20.9980084283727,25.5180399947065,21.5668820569986));
#51186=CARTESIAN_POINT('Ctrl Pts',(-21.0007346821009,25.5215709222163,21.5671632715307));
#51187=CARTESIAN_POINT('Ctrl Pts',(-21.0047315642741,25.52672535396,21.5675748669832));
#51188=CARTESIAN_POINT('Ctrl Pts',(-21.0059964419694,25.5283533285691,21.5677050231817));
#51189=CARTESIAN_POINT('Ctrl Pts',(-21.0115175117565,25.5354452252886,21.5682727084125));
#51190=CARTESIAN_POINT('Ctrl Pts',(-21.0157897247628,25.5408966011455,21.5687108618133));
#51191=CARTESIAN_POINT('Ctrl Pts',(-21.0231841420782,25.5502695424442,21.5694673047606));
#51192=CARTESIAN_POINT('Ctrl Pts',(-21.0262979966671,25.5541976890649,21.5697852684233));
#51193=CARTESIAN_POINT('Ctrl Pts',(-21.0319193827821,25.5612552155092,21.5703582416768));
#51194=CARTESIAN_POINT('Ctrl Pts',(-21.0344236196825,25.5643872164846,21.5706131230165));
#51195=CARTESIAN_POINT('Ctrl Pts',(-21.0396774737558,25.5709330248627,21.5711470910116));
#51196=CARTESIAN_POINT('Ctrl Pts',(-21.0424282216541,25.5743459106381,21.5714262211045));
#51197=CARTESIAN_POINT('Ctrl Pts',(-21.0580547138129,25.593653132208,21.5730094337762));
#51198=CARTESIAN_POINT('Ctrl Pts',(-21.0710743638938,25.609429930542,21.5743190527707));
#51199=CARTESIAN_POINT('Ctrl Pts',(-21.1187575411656,25.6661031168661,21.5790815586127));
#51200=CARTESIAN_POINT('Ctrl Pts',(-21.1542885819883,25.7062552767034,21.5825670414861));
#51201=CARTESIAN_POINT('Ctrl Pts',(-21.3519508353203,25.9187023583864,21.6016165662394));
#51202=CARTESIAN_POINT('Ctrl Pts',(-21.5316726594639,26.0736231944658,21.6178177105776));
#51203=CARTESIAN_POINT('Ctrl Pts',(-21.8007811381698,26.2583036758534,21.6397169868783));
#51204=CARTESIAN_POINT('Ctrl Pts',(-21.8769664172572,26.3060295951644,21.6456797894781));
#51205=CARTESIAN_POINT('Ctrl Pts',(-21.9945809519448,26.3730300788114,21.6544338920038));
#51206=CARTESIAN_POINT('Ctrl Pts',(-22.034584504871,26.3947099625176,21.657336253066));
#51207=CARTESIAN_POINT('Ctrl Pts',(-22.075036015355,26.4155367745608,21.6601868380444));
#51208=CARTESIAN_POINT('Origin',(-23.5502525316942,23.5502525316942,-77.3107734492734));
#51209=CARTESIAN_POINT('',(-22.0750359362463,26.4155367338311,23.156397107556));
#51210=CARTESIAN_POINT('',(-22.0750361284943,26.4155368328116,22.9065074728514));
#51211=CARTESIAN_POINT('',(-22.0750360153461,26.4155367745563,-77.3107734492734));
#51212=CARTESIAN_POINT('',(-26.7730014957921,23.5528365025921,22.3125994347384));
#51213=CARTESIAN_POINT('Ctrl Pts',(-22.0750359362473,26.4155367338316,23.1563971075561));
#51214=CARTESIAN_POINT('Ctrl Pts',(-22.0294856266012,26.3920847590964,23.1533709924801));
#51215=CARTESIAN_POINT('Ctrl Pts',(-21.9844639750547,26.3675308704831,23.1503081910084));
#51216=CARTESIAN_POINT('Ctrl Pts',(-21.9225276784368,26.3318054693836,23.1459836548566));
#51217=CARTESIAN_POINT('Ctrl Pts',(-21.9051394521694,26.3215568942344,23.1447571047244));
#51218=CARTESIAN_POINT('Ctrl Pts',(-21.8825127524228,26.3079327868681,23.1431442266346));
#51219=CARTESIAN_POINT('Ctrl Pts',(-21.8771859189913,26.3047042865337,23.1427632888179));
#51220=CARTESIAN_POINT('Ctrl Pts',(-21.8689857199637,26.29970172628,23.1421749550518));
#51221=CARTESIAN_POINT('Ctrl Pts',(-21.8661057064932,26.2979385466644,23.1419679595713));
#51222=CARTESIAN_POINT('Ctrl Pts',(-21.8603798731074,26.294420736762,23.141555696188));
#51223=CARTESIAN_POINT('Ctrl Pts',(-21.8575340016088,26.2926661981049,23.1413504318406));
#51224=CARTESIAN_POINT('Ctrl Pts',(-21.8513069420466,26.2888137013258,23.1409005007039));
#51225=CARTESIAN_POINT('Ctrl Pts',(-21.847926902625,26.2867139052174,23.1406557661818));
#51226=CARTESIAN_POINT('Ctrl Pts',(-21.8383055833703,26.2807120878993,23.1399576589943));
#51227=CARTESIAN_POINT('Ctrl Pts',(-21.8320738009395,26.2767949556607,23.1395037266934));
#51228=CARTESIAN_POINT('Ctrl Pts',(-21.8181259413803,26.2679608956485,23.1384837523374));
#51229=CARTESIAN_POINT('Ctrl Pts',(-21.8104172973801,26.2630324031619,23.1379172815519));
#51230=CARTESIAN_POINT('Ctrl Pts',(-21.7170415781639,26.2027712809842,23.1310217507204));
#51231=CARTESIAN_POINT('Ctrl Pts',(-21.6340353818574,26.1434409488034,23.1245424034599));
#51232=CARTESIAN_POINT('Ctrl Pts',(-21.3901394501606,25.9510001068978,23.104378714728));
#51233=CARTESIAN_POINT('Ctrl Pts',(-21.2392551950895,25.8061222650276,23.0902632779117));
#51234=CARTESIAN_POINT('Ctrl Pts',(-20.9819764320549,25.5059912143173,23.0635158983552));
#51235=CARTESIAN_POINT('Ctrl Pts',(-20.8730238244339,25.35397655252,23.0509478955615));
#51236=CARTESIAN_POINT('Ctrl Pts',(-20.7720180192221,25.1835500448935,23.0384642857336));
#51237=CARTESIAN_POINT('Ctrl Pts',(-20.7662522234357,25.1737025819987,23.0377483911955));
#51238=CARTESIAN_POINT('Ctrl Pts',(-20.7587922121724,25.1608049261938,23.0368180249622));
#51239=CARTESIAN_POINT('Ctrl Pts',(-20.7570505668576,25.1577824738107,23.036600520672));
#51240=CARTESIAN_POINT('Ctrl Pts',(-20.7543759510902,25.153123473828,23.0362660512508));
#51241=CARTESIAN_POINT('Ctrl Pts',(-20.7534395093714,25.1514889381363,23.0361488603861));
#51242=CARTESIAN_POINT('Ctrl Pts',(-20.7515787066757,25.1482343409376,23.035915820993));
#51243=CARTESIAN_POINT('Ctrl Pts',(-20.7506543243926,25.1466143074897,23.0357999717045));
#51244=CARTESIAN_POINT('Ctrl Pts',(-20.748593382147,25.1429950911444,23.0355414945063));
#51245=CARTESIAN_POINT('Ctrl Pts',(-20.7474575579343,25.1409954983833,23.0353989149486));
#51246=CARTESIAN_POINT('Ctrl Pts',(-20.7441364176982,25.1351341065389,23.0349816330491));
#51247=CARTESIAN_POINT('Ctrl Pts',(-20.7419569245714,25.131268987992,23.0347073079793));
#51248=CARTESIAN_POINT('Ctrl Pts',(-20.725978249816,25.1027950757905,23.0326924581769));
#51249=CARTESIAN_POINT('Ctrl Pts',(-20.7124942154485,25.0780095282868,23.030971931129));
#51250=CARTESIAN_POINT('Ctrl Pts',(-20.66923713237,24.9959476580317,23.0253736443429));
#51251=CARTESIAN_POINT('Ctrl Pts',(-20.6408575420404,24.9379506648075,23.0215721522811));
#51252=CARTESIAN_POINT('Ctrl Pts',(-20.5511588992428,24.7397718903957,23.0089683042789));
#51253=CARTESIAN_POINT('Ctrl Pts',(-20.498079092189,24.5960835294767,23.0004573386922));
#51254=CARTESIAN_POINT('Ctrl Pts',(-20.4376789161569,24.3881318169421,22.988356280251));
#51255=CARTESIAN_POINT('Ctrl Pts',(-20.4217623318041,24.3265933669076,22.9848021771545));
#51256=CARTESIAN_POINT('Ctrl Pts',(-20.3635218342693,24.0703892983238,22.9700046316717));
#51257=CARTESIAN_POINT('Ctrl Pts',(-20.3374769326493,23.8725096185598,22.9585392420737));
#51258=CARTESIAN_POINT('Ctrl Pts',(-20.3293919729415,23.6612698640343,22.9456905723071));
#51259=CARTESIAN_POINT('Ctrl Pts',(-20.3289933059839,23.6490279400181,22.9449439449603));
#51260=CARTESIAN_POINT('Ctrl Pts',(-20.3285418857962,23.6322214874948,22.9439160776453));
#51261=CARTESIAN_POINT('Ctrl Pts',(-20.3284290261296,23.6276585666661,22.9436367251243));
#51262=CARTESIAN_POINT('Ctrl Pts',(-20.3282528759963,23.6198672411692,22.9431592243023));
#51263=CARTESIAN_POINT('Ctrl Pts',(-20.3281847432504,23.616638943348,22.9429612282145));
#51264=CARTESIAN_POINT('Ctrl Pts',(-20.3280619534226,23.6103745784463,22.9425767405232));
#51265=CARTESIAN_POINT('Ctrl Pts',(-20.3280067352895,23.6073385252698,22.9423902667769));
#51266=CARTESIAN_POINT('Ctrl Pts',(-20.327886781405,23.6001872227056,22.9419507269586));
#51267=CARTESIAN_POINT('Ctrl Pts',(-20.3278256380497,23.5960719257129,22.9416975483793));
#51268=CARTESIAN_POINT('Ctrl Pts',(-20.327669144174,23.5839796004908,22.9409528995672));
#51269=CARTESIAN_POINT('Ctrl Pts',(-20.3275955302543,23.5760023652272,22.9404607477067));
#51270=CARTESIAN_POINT('Ctrl Pts',(-20.3274958047619,23.5579190291457,22.9393430059669));
#51271=CARTESIAN_POINT('Ctrl Pts',(-20.3274876099435,23.5478129501646,22.9387168573638));
#51272=CARTESIAN_POINT('Ctrl Pts',(-20.3276132790061,23.5155305511483,22.9367118864099));
#51273=CARTESIAN_POINT('Ctrl Pts',(-20.3279285087689,23.4933559545997,22.9353273963986));
#51274=CARTESIAN_POINT('Ctrl Pts',(-20.3300367739292,23.4074480943806,22.9299345675532));
#51275=CARTESIAN_POINT('Ctrl Pts',(-20.3334920137916,23.3437737624049,22.9258749650053));
#51276=CARTESIAN_POINT('Ctrl Pts',(-20.3534447864056,23.1064572425327,22.9105047436555));
#51277=CARTESIAN_POINT('Ctrl Pts',(-20.3821376953363,22.9341612346731,22.8988430960653));
#51278=CARTESIAN_POINT('Ctrl Pts',(-20.4625867824517,22.6139189454461,22.8765199912576));
#51279=CARTESIAN_POINT('Ctrl Pts',(-20.5114663647476,22.4657329612724,22.8659182803312));
#51280=CARTESIAN_POINT('Ctrl Pts',(-20.6035473576453,22.2424335707768,22.849971039027));
#51281=CARTESIAN_POINT('Ctrl Pts',(-20.6393685890608,22.1645326518966,22.8444161986524));
#51282=CARTESIAN_POINT('Ctrl Pts',(-20.6811345435415,22.0824924127031,22.8386454412202));
#51283=CARTESIAN_POINT('Ctrl Pts',(-20.6840289919902,22.0768481680136,22.8382488373415));
#51284=CARTESIAN_POINT('Ctrl Pts',(-20.6880718719515,22.0690214508559,22.837699494469));
#51285=CARTESIAN_POINT('Ctrl Pts',(-20.6892061480703,22.0668317435498,22.8375458701627));
#51286=CARTESIAN_POINT('Ctrl Pts',(-20.6911620184713,22.0630665457324,22.8372818319936));
#51287=CARTESIAN_POINT('Ctrl Pts',(-20.691982402123,22.0614904331442,22.8371713413541));
#51288=CARTESIAN_POINT('Ctrl Pts',(-20.6936816357499,22.058232464826,22.8369430224617));
#51289=CARTESIAN_POINT('Ctrl Pts',(-20.6945606661568,22.0565507098397,22.8368252065961));
#51290=CARTESIAN_POINT('Ctrl Pts',(-20.6966311506284,22.0525979811106,22.8365483932295));
#51291=CARTESIAN_POINT('Ctrl Pts',(-20.6978238341719,22.0503276452347,22.8363894741691));
#51292=CARTESIAN_POINT('Ctrl Pts',(-20.7017195509733,22.0429333946192,22.8358721268964));
#51293=CARTESIAN_POINT('Ctrl Pts',(-20.7044337103009,22.0378153064557,22.8355144033565));
#51294=CARTESIAN_POINT('Ctrl Pts',(-20.7992985395595,21.8600882588314,22.8231042435046));
#51295=CARTESIAN_POINT('Ctrl Pts',(-20.9069815288534,21.6961899708524,22.8120389351957));
#51296=CARTESIAN_POINT('Ctrl Pts',(-21.1583310962629,21.3804545465824,22.789432643089));
#51297=CARTESIAN_POINT('Ctrl Pts',(-21.3031888274897,21.2307675540355,22.7779389305399));
#51298=CARTESIAN_POINT('Ctrl Pts',(-21.4872982626294,21.074068017082,22.7639063103323));
#51299=CARTESIAN_POINT('Ctrl Pts',(-21.5134960899819,21.0524748890101,22.7619226849152));
#51300=CARTESIAN_POINT('Ctrl Pts',(-21.5512996152547,21.0223061899788,22.7590751815641));
#51301=CARTESIAN_POINT('Ctrl Pts',(-21.5626298037318,21.0133880593897,22.7582236136345));
#51302=CARTESIAN_POINT('Ctrl Pts',(-21.577273874756,21.0020198584459,22.7571251399503));
#51303=CARTESIAN_POINT('Ctrl Pts',(-21.5805332464755,20.9994996085439,22.75688078633));
#51304=CARTESIAN_POINT('Ctrl Pts',(-21.5864756701902,20.9949229192107,22.7564355271128));
#51305=CARTESIAN_POINT('Ctrl Pts',(-21.5891571453894,20.9928644352364,22.7562346963609));
#51306=CARTESIAN_POINT('Ctrl Pts',(-21.6006062268373,20.9841039318333,22.7553775814658));
#51307=CARTESIAN_POINT('Ctrl Pts',(-21.6094049152077,20.9774428077131,22.7547198096132));
#51308=CARTESIAN_POINT('Ctrl Pts',(-21.6190793868246,20.9701965336061,22.7539975010224));
#51309=CARTESIAN_POINT('Ctrl Pts',(-21.6199215166211,20.9695664134344,22.7539346342481));
#51310=CARTESIAN_POINT('Ctrl Pts',(-21.6261806360865,20.9648878307536,22.7534674346821));
#51311=CARTESIAN_POINT('Ctrl Pts',(-21.6316100183117,20.9608560380786,22.7530624860344));
#51312=CARTESIAN_POINT('Ctrl Pts',(-21.6428613353737,20.952555763129,22.7522239330439));
#51313=CARTESIAN_POINT('Ctrl Pts',(-21.6486849982771,20.9482896972556,22.7517902418336));
#51314=CARTESIAN_POINT('Ctrl Pts',(-21.6780768720993,20.9269103527649,22.7496030462664));
#51315=CARTESIAN_POINT('Ctrl Pts',(-21.7018613904171,20.9100979924343,22.7478383699771));
#51316=CARTESIAN_POINT('Ctrl Pts',(-21.7311779365365,20.8899655844337,22.7456683788759));
#51317=CARTESIAN_POINT('Ctrl Pts',(-21.7364968265927,20.8863363795274,22.7452748825211));
#51318=CARTESIAN_POINT('Ctrl Pts',(-21.7452847580442,20.880378685516,22.7446250642391));
#51319=CARTESIAN_POINT('Ctrl Pts',(-21.7487475317798,20.8780409469868,22.7443690933184));
#51320=CARTESIAN_POINT('Ctrl Pts',(-21.7549959487003,20.873840270088,22.7439073483533));
#51321=CARTESIAN_POINT('Ctrl Pts',(-21.7577799748001,20.8719749274296,22.7437016655747));
#51322=CARTESIAN_POINT('Ctrl Pts',(-21.7631828130233,20.8683671356644,22.7433026022862));
#51323=CARTESIAN_POINT('Ctrl Pts',(-21.7658012776569,20.8666241709331,22.7431092415386));
#51324=CARTESIAN_POINT('Ctrl Pts',(-21.7731144436023,20.8617716431597,22.7425693193893));
#51325=CARTESIAN_POINT('Ctrl Pts',(-21.7778147327559,20.8586705581305,22.7422224395463));
#51326=CARTESIAN_POINT('Ctrl Pts',(-21.7970272382894,20.8460669730783,22.7408050985251));
#51327=CARTESIAN_POINT('Ctrl Pts',(-21.8116077253638,20.8366695343733,22.7397307115008));
#51328=CARTESIAN_POINT('Ctrl Pts',(-21.8487311888421,20.81316468755,22.7369979965829));
#51329=CARTESIAN_POINT('Ctrl Pts',(-21.8713738883013,20.7992179664644,22.7353337989818));
#51330=CARTESIAN_POINT('Ctrl Pts',(-21.9629085596965,20.744388311402,22.7286149681981));
#51331=CARTESIAN_POINT('Ctrl Pts',(-22.0331367067531,20.7058030794041,22.7234788606682));
#51332=CARTESIAN_POINT('Ctrl Pts',(-22.2092703441057,20.6174097294622,22.7106405432937));
#51333=CARTESIAN_POINT('Ctrl Pts',(-22.3165863799123,20.5706780978902,22.7028524618182));
#51334=CARTESIAN_POINT('Ctrl Pts',(-22.6744805295177,20.4374846590288,22.6771428471074));
#51335=CARTESIAN_POINT('Ctrl Pts',(-22.9332226815881,20.3760450274932,22.6588843291175));
#51336=CARTESIAN_POINT('Ctrl Pts',(-23.2111126328635,20.3453632170192,22.6412152730107));
#51337=CARTESIAN_POINT('Ctrl Pts',(-23.2256582477367,20.3438573657034,22.64029619405));
#51338=CARTESIAN_POINT('Ctrl Pts',(-23.2439868840392,20.3420858770928,22.6391457747624));
#51339=CARTESIAN_POINT('Ctrl Pts',(-23.2477604976396,20.3417278706833,22.638909329542));
#51340=CARTESIAN_POINT('Ctrl Pts',(-23.2537082232285,20.3411741904085,22.6385373157019));
#51341=CARTESIAN_POINT('Ctrl Pts',(-23.2558819020991,20.3409740676322,22.6384014960658));
#51342=CARTESIAN_POINT('Ctrl Pts',(-23.2598945234828,20.3406087510652,22.6381510291662));
#51343=CARTESIAN_POINT('Ctrl Pts',(-23.2617333937795,20.3404429300896,22.6380363470437));
#51344=CARTESIAN_POINT('Ctrl Pts',(-23.2658348342985,20.3400766338268,22.6377807804083));
#51345=CARTESIAN_POINT('Ctrl Pts',(-23.268097469101,20.3398769707092,22.6376399426855));
#51346=CARTESIAN_POINT('Ctrl Pts',(-23.2746474358085,20.3393059558921,22.6372326700662));
#51347=CARTESIAN_POINT('Ctrl Pts',(-23.2789353240046,20.3389407973937,22.6369665853078));
#51348=CARTESIAN_POINT('Ctrl Pts',(-23.3082474081903,20.3365036951715,22.6351511909765));
#51349=CARTESIAN_POINT('Ctrl Pts',(-23.3332952477626,20.3347156100164,22.6336176552514));
#51350=CARTESIAN_POINT('Ctrl Pts',(-23.4106018212385,20.3301044119027,22.6289323112359));
#51351=CARTESIAN_POINT('Ctrl Pts',(-23.4629126925399,20.328261119802,22.6258289724947));
#51352=CARTESIAN_POINT('Ctrl Pts',(-23.5977787730171,20.3267961732674,22.6179480650913));
#51353=CARTESIAN_POINT('Ctrl Pts',(-23.6803181577387,20.3290704273155,22.6132402428225));
#51354=CARTESIAN_POINT('Ctrl Pts',(-23.7867936240093,20.3361041671926,22.6072175979802));
#51355=CARTESIAN_POINT('Ctrl Pts',(-23.8108852856798,20.3379679887335,22.6058582751057));
#51356=CARTESIAN_POINT('Ctrl Pts',(-23.8553834212792,20.3419144337549,22.603350501961));
#51357=CARTESIAN_POINT('Ctrl Pts',(-23.8757952732173,20.3439212728061,22.6022013039689));
#51358=CARTESIAN_POINT('Ctrl Pts',(-23.9138389495851,20.3480286615516,22.6000595834871));
#51359=CARTESIAN_POINT('Ctrl Pts',(-23.9314752204364,20.3500803391235,22.5990667898238));
#51360=CARTESIAN_POINT('Ctrl Pts',(-24.0991207347398,20.3709885484075,22.5896238125828));
#51361=CARTESIAN_POINT('Ctrl Pts',(-24.2476409683955,20.4002331201207,22.5812033823822));
#51362=CARTESIAN_POINT('Ctrl Pts',(-24.4478027244104,20.4545005170167,22.5693095686106));
#51363=CARTESIAN_POINT('Ctrl Pts',(-24.5016559021833,20.4706246238554,22.5660549323881));
#51364=CARTESIAN_POINT('Ctrl Pts',(-24.5728059222371,20.4939719440984,22.5616648961709));
#51365=CARTESIAN_POINT('Ctrl Pts',(-24.5905025752557,20.4999498755925,22.5605654877765));
#51366=CARTESIAN_POINT('Ctrl Pts',(-24.6122975806048,20.5075239546534,22.559201690625));
#51367=CARTESIAN_POINT('Ctrl Pts',(-24.6164461753879,20.508975169575,22.5589416577133));
#51368=CARTESIAN_POINT('Ctrl Pts',(-24.6243753502341,20.511767082749,22.5584438088016));
#51369=CARTESIAN_POINT('Ctrl Pts',(-24.6281564234462,20.5131063625575,22.5582060361354));
#51370=CARTESIAN_POINT('Ctrl Pts',(-24.6365806748776,20.5161079981572,22.5576754428675));
#51371=CARTESIAN_POINT('Ctrl Pts',(-24.6412225510467,20.5177739577295,22.5573825126318));
#51372=CARTESIAN_POINT('Ctrl Pts',(-24.6523847688375,20.5218090004708,22.5566767305347));
#51373=CARTESIAN_POINT('Ctrl Pts',(-24.6589013016606,20.5241884884644,22.5562635581188));
#51374=CARTESIAN_POINT('Ctrl Pts',(-24.6672333612256,20.5272614358488,22.5557337979316));
#51375=CARTESIAN_POINT('Ctrl Pts',(-24.6690560467098,20.5279355341134,22.5556178192519));
#51376=CARTESIAN_POINT('Ctrl Pts',(-24.6762503746342,20.5306036695003,22.5551596800309));
#51377=CARTESIAN_POINT('Ctrl Pts',(-24.6816172821205,20.5326103736302,22.5548171205081));
#51378=CARTESIAN_POINT('Ctrl Pts',(-24.6900645748282,20.5357945465981,22.5542766829216));
#51379=CARTESIAN_POINT('Ctrl Pts',(-24.6931485696979,20.536962455419,22.554079110519));
#51380=CARTESIAN_POINT('Ctrl Pts',(-24.7049882715268,20.5414669413087,22.5533195862047));
#51381=CARTESIAN_POINT('Ctrl Pts',(-24.7137311424152,20.5448369402369,22.5527565633212));
#51382=CARTESIAN_POINT('Ctrl Pts',(-24.7474573256393,20.5580061457724,22.550576152204));
#51383=CARTESIAN_POINT('Ctrl Pts',(-24.7723320215965,20.5680789274423,22.548949875087));
#51384=CARTESIAN_POINT('Ctrl Pts',(-24.8033797758997,20.5811051148179,22.5468961950661));
#51385=CARTESIAN_POINT('Ctrl Pts',(-24.8096736299409,20.5837692990651,22.5464786459062));
#51386=CARTESIAN_POINT('Ctrl Pts',(-24.8199136360275,20.5881423489507,22.5457972638406));
#51387=CARTESIAN_POINT('Ctrl Pts',(-24.8238649488127,20.589839137378,22.5455338434655));
#51388=CARTESIAN_POINT('Ctrl Pts',(-24.8309012179966,20.5928773743596,22.5450638713835));
#51389=CARTESIAN_POINT('Ctrl Pts',(-24.8339874981815,20.5942157567827,22.5448574248266));
#51390=CARTESIAN_POINT('Ctrl Pts',(-24.8399474511042,20.5968114173135,22.5444581607208));
#51391=CARTESIAN_POINT('Ctrl Pts',(-24.8428213961254,20.5980680639046,22.5442653650037));
#51392=CARTESIAN_POINT('Ctrl Pts',(-24.8490362541187,20.6007963560008,22.5438478676805));
#51393=CARTESIAN_POINT('Ctrl Pts',(-24.8523765074184,20.6022694853319,22.543623115311));
#51394=CARTESIAN_POINT('Ctrl Pts',(-24.8655058465643,20.6080864969675,22.5427382588186));
#51395=CARTESIAN_POINT('Ctrl Pts',(-24.8752756717864,20.6124734501513,22.542076674785));
#51396=CARTESIAN_POINT('Ctrl Pts',(-24.8982429138315,20.6229243243866,22.5405138986608));
#51397=CARTESIAN_POINT('Ctrl Pts',(-24.911421479434,20.6290288859931,22.539611310803));
#51398=CARTESIAN_POINT('Ctrl Pts',(-24.9572124967345,20.6506172903928,22.5364543537283));
#51399=CARTESIAN_POINT('Ctrl Pts',(-24.9896047195518,20.666559416184,22.53418416907));
#51400=CARTESIAN_POINT('Ctrl Pts',(-25.0647688774001,20.7051340867787,22.5288274286654));
#51401=CARTESIAN_POINT('Ctrl Pts',(-25.1073115477299,20.728192016466,22.5257266239043));
#51402=CARTESIAN_POINT('Ctrl Pts',(-25.2238916655606,20.7948165780329,22.517035417073));
#51403=CARTESIAN_POINT('Ctrl Pts',(-25.2967272135852,20.8403965296302,22.51138127237));
#51404=CARTESIAN_POINT('Ctrl Pts',(-25.6035816771314,21.0499372675898,22.4866215705518));
#51405=CARTESIAN_POINT('Ctrl Pts',(-25.8170309507082,21.2416926638815,22.4668000165846));
#51406=CARTESIAN_POINT('Ctrl Pts',(-26.0278170006795,21.48886333833,22.4458862001614));
#51407=CARTESIAN_POINT('Ctrl Pts',(-26.0526837845216,21.5191224830323,22.4433959550025));
#51408=CARTESIAN_POINT('Ctrl Pts',(-26.0799531982397,21.5535665711086,22.4406459273989));
#51409=CARTESIAN_POINT('Ctrl Pts',(-26.0829039415134,21.5573107050079,22.4403480962656));
#51410=CARTESIAN_POINT('Ctrl Pts',(-26.0873332816242,21.5629567223269,22.4399006513088));
#51411=CARTESIAN_POINT('Ctrl Pts',(-26.0888180549757,21.5648537179306,22.4397505984412));
#51412=CARTESIAN_POINT('Ctrl Pts',(-26.0913850854771,21.5681410285696,22.4394910641656));
#51413=CARTESIAN_POINT('Ctrl Pts',(-26.0924683292816,21.5695305660347,22.4393815118633));
#51414=CARTESIAN_POINT('Ctrl Pts',(-26.0947221767741,21.5724265970931,22.4391535042866));
#51415=CARTESIAN_POINT('Ctrl Pts',(-26.0958925809651,21.5739332402133,22.4390350637315));
#51416=CARTESIAN_POINT('Ctrl Pts',(-26.0986691865047,21.5775140801665,22.4387539887334));
#51417=CARTESIAN_POINT('Ctrl Pts',(-26.1002741990882,21.5795892066713,22.4385914397221));
#51418=CARTESIAN_POINT('Ctrl Pts',(-26.1056171148346,21.5865145384822,22.4380500754735));
#51419=CARTESIAN_POINT('Ctrl Pts',(-26.1093437576189,21.5913734752935,22.4376720592038));
#51420=CARTESIAN_POINT('Ctrl Pts',(-26.2047948356282,21.716563455267,22.427978210685));
#51421=CARTESIAN_POINT('Ctrl Pts',(-26.287960429666,21.8432142291866,22.4192509232727));
#51422=CARTESIAN_POINT('Ctrl Pts',(-26.4579711859301,22.1467169014364,22.3995842960208));
#51423=CARTESIAN_POINT('Ctrl Pts',(-26.5381304636759,22.3265993257044,22.3887853651874));
#51424=CARTESIAN_POINT('Ctrl Pts',(-26.6076789564656,22.5311151579963,22.376489520812));
#51425=CARTESIAN_POINT('Ctrl Pts',(-26.6137855886801,22.5496214695126,22.3753770230729));
#51426=CARTESIAN_POINT('Ctrl Pts',(-26.63363539814,22.6116622401787,22.3716458693469));
#51427=CARTESIAN_POINT('Ctrl Pts',(-26.6466209849791,22.6554319910262,22.3690108293393));
#51428=CARTESIAN_POINT('Ctrl Pts',(-26.6840184469967,22.7920660319612,22.3607551023492));
#51429=CARTESIAN_POINT('Ctrl Pts',(-26.7052117208723,22.8857487288143,22.35505031585));
#51430=CARTESIAN_POINT('Ctrl Pts',(-26.7239911231415,22.990248510911,22.3485874383871));
#51431=CARTESIAN_POINT('Ctrl Pts',(-26.7257438333153,23.0002742232777,22.3479664124362));
#51432=CARTESIAN_POINT('Ctrl Pts',(-26.7281490532456,23.0144272622646,22.3470882958149));
#51433=CARTESIAN_POINT('Ctrl Pts',(-26.7288410849276,23.018547886206,22.3468324634961));
#51434=CARTESIAN_POINT('Ctrl Pts',(-26.7300372423039,23.0257560647712,22.346384635088));
#51435=CARTESIAN_POINT('Ctrl Pts',(-26.7305448905388,23.0288430363726,22.3461927512635));
#51436=CARTESIAN_POINT('Ctrl Pts',(-26.7315590723543,23.035066785749,22.3458056902112));
#51437=CARTESIAN_POINT('Ctrl Pts',(-26.7320654633471,23.0382035825448,22.3456105087088));
#51438=CARTESIAN_POINT('Ctrl Pts',(-26.7330959784469,23.0446475789257,22.3452093331585));
#51439=CARTESIAN_POINT('Ctrl Pts',(-26.7336195886335,23.0479548555506,22.3450033230348));
#51440=CARTESIAN_POINT('Ctrl Pts',(-26.7348240557317,23.0556401566997,22.344524340208));
#51441=CARTESIAN_POINT('Ctrl Pts',(-26.7355010393109,23.0600187735546,22.34425124472));
#51442=CARTESIAN_POINT('Ctrl Pts',(-26.7372342476121,23.0713840384052,22.3435418642406));
#51443=CARTESIAN_POINT('Ctrl Pts',(-26.7382765235008,23.0783727611506,22.3431051369837));
#51444=CARTESIAN_POINT('Ctrl Pts',(-26.7618657746906,23.2401906352954,22.332980949314));
#51445=CARTESIAN_POINT('Ctrl Pts',(-26.773126904686,23.3964255372188,22.3229329672665));
#51446=CARTESIAN_POINT('Ctrl Pts',(-26.7730014957921,23.5528365025921,22.3125994347384));
#51447=CARTESIAN_POINT('Ctrl Pts',(-26.7730014989634,23.5528325442904,22.3125996962497));
#51448=CARTESIAN_POINT('Ctrl Pts',(-26.7727816966704,23.8273922941403,22.2944604890385));
#51449=CARTESIAN_POINT('Ctrl Pts',(-26.7374794702398,24.1007806232849,22.2754700028552));
#51450=CARTESIAN_POINT('Ctrl Pts',(-26.6498300776261,24.4356096374394,22.2526975769606));
#51451=CARTESIAN_POINT('Ctrl Pts',(-26.6294062724549,24.5042191084543,22.2480663482769));
#51452=CARTESIAN_POINT('Ctrl Pts',(-26.6031299350747,24.5828147945174,22.2428459527465));
#51453=CARTESIAN_POINT('Ctrl Pts',(-26.5994904084202,24.5935135953152,22.242137184495));
#51454=CARTESIAN_POINT('Ctrl Pts',(-26.5947045595185,24.6073431252165,22.2412236243568));
#51455=CARTESIAN_POINT('Ctrl Pts',(-26.5936096103835,24.6104913559544,22.2410158321948));
#51456=CARTESIAN_POINT('Ctrl Pts',(-26.5918307224937,24.615580606502,22.2406802181609));
#51457=CARTESIAN_POINT('Ctrl Pts',(-26.5911498089548,24.6175226694417,22.2405522161276));
#51458=CARTESIAN_POINT('Ctrl Pts',(-26.5898419267614,24.6212415241408,22.2403072384408));
#51459=CARTESIAN_POINT('Ctrl Pts',(-26.5892152621287,24.6230184127659,22.2401902453797));
#51460=CARTESIAN_POINT('Ctrl Pts',(-26.5877746976747,24.6270916977328,22.2399221868232));
#51461=CARTESIAN_POINT('Ctrl Pts',(-26.5869597499704,24.6293877266076,22.2397711843011));
#51462=CARTESIAN_POINT('Ctrl Pts',(-26.5843808965873,24.6366273187334,22.2392953579153));
#51463=CARTESIAN_POINT('Ctrl Pts',(-26.582607505501,24.641567530361,22.2389710991441));
#51464=CARTESIAN_POINT('Ctrl Pts',(-26.5679018994689,24.6822209622872,22.2363061969817));
#51465=CARTESIAN_POINT('Ctrl Pts',(-26.5543506365233,24.7177092208651,22.2340018412618));
#51466=CARTESIAN_POINT('Ctrl Pts',(-26.5375922744891,24.759370680268,22.2313134539935));
#51467=CARTESIAN_POINT('Ctrl Pts',(-26.5349894552735,24.7657816077551,22.2309002362025));
#51468=CARTESIAN_POINT('Ctrl Pts',(-26.4200259315163,25.0463490829511,22.2128349712719));
#51469=CARTESIAN_POINT('Ctrl Pts',(-26.2704015828963,25.3037473879628,22.1969372140797));
#51470=CARTESIAN_POINT('Ctrl Pts',(-26.0468996287055,25.5891854542539,22.1763516665697));
#51471=CARTESIAN_POINT('Ctrl Pts',(-26.0045214351048,25.6400031597028,22.1725600827292));
#51472=CARTESIAN_POINT('Ctrl Pts',(-25.8916453247069,25.7671855340542,22.1626787989449));
#51473=CARTESIAN_POINT('Ctrl Pts',(-25.8189688593733,25.8415043470074,22.1565164668457));
#51474=CARTESIAN_POINT('Ctrl Pts',(-25.7356932462003,25.9188093557424,22.1495976288782));
#51475=CARTESIAN_POINT('Ctrl Pts',(-25.7285205692205,25.9254074526995,22.1490028155607));
#51476=CARTESIAN_POINT('Ctrl Pts',(-25.7186909424206,25.9343676838472,22.1481891427955));
#51477=CARTESIAN_POINT('Ctrl Pts',(-25.7160597971692,25.9367581546699,22.1479714861979));
#51478=CARTESIAN_POINT('Ctrl Pts',(-25.7111028751142,25.9412467113325,22.147561700278));
#51479=CARTESIAN_POINT('Ctrl Pts',(-25.7087779824436,25.9433457710143,22.1473696124448));
#51480=CARTESIAN_POINT('Ctrl Pts',(-25.7039281465232,25.9477116914328,22.146969134353));
#51481=CARTESIAN_POINT('Ctrl Pts',(-25.7014026770027,25.9499779594717,22.1467607194577));
#51482=CARTESIAN_POINT('Ctrl Pts',(-25.6955711712917,25.9551943460036,22.1462797634256));
#51483=CARTESIAN_POINT('Ctrl Pts',(-25.6922626262953,25.9581416383459,22.146007103989));
#51484=CARTESIAN_POINT('Ctrl Pts',(-25.6819471750358,25.9672926830953,22.1451576581534));
#51485=CARTESIAN_POINT('Ctrl Pts',(-25.6749193639823,25.9734727022002,22.1445798800348));
#51486=CARTESIAN_POINT('Ctrl Pts',(-25.6150691058854,26.0256424703571,22.1396671598498));
#51487=CARTESIAN_POINT('Ctrl Pts',(-25.5607909471644,26.0699264928203,22.1352621883468));
#51488=CARTESIAN_POINT('Ctrl Pts',(-25.4983860074865,26.1175400489098,22.1302467216276));
#51489=CARTESIAN_POINT('Ctrl Pts',(-25.491635210435,26.1226487935692,22.1297047946656));
#51490=CARTESIAN_POINT('Ctrl Pts',(-25.4406261694151,26.1609353220647,22.1256147324813));
#51491=CARTESIAN_POINT('Ctrl Pts',(-25.3955425824739,26.1929937582597,22.1220263236932));
#51492=CARTESIAN_POINT('Ctrl Pts',(-25.2653797843378,26.2805961476516,22.1117435424544));
#51493=CARTESIAN_POINT('Ctrl Pts',(-25.1784720266675,26.3332969913784,22.1049664811489));
#51494=CARTESIAN_POINT('Ctrl Pts',(-25.0188393391407,26.420058829961,22.0927325718472));
#51495=CARTESIAN_POINT('Ctrl Pts',(-24.9470512685393,26.4556764865226,22.0873041555619));
#51496=CARTESIAN_POINT('Ctrl Pts',(-24.7076038378035,26.5635509810317,22.0695337636006));
#51497=CARTESIAN_POINT('Ctrl Pts',(-24.5351064127702,26.6242578645162,22.0572397142614));
#51498=CARTESIAN_POINT('Ctrl Pts',(-24.3429870226977,26.6740230712446,22.0446866660121));
#51499=CARTESIAN_POINT('Ctrl Pts',(-24.327565822985,26.6778961221649,22.0436869416211));
#51500=CARTESIAN_POINT('Ctrl Pts',(-24.3084697326305,26.6825421611258,22.0424592612208));
#51501=CARTESIAN_POINT('Ctrl Pts',(-24.3048216792032,26.6834229784477,22.0422251917254));
#51502=CARTESIAN_POINT('Ctrl Pts',(-24.299079549773,26.6847987970287,22.041857496811));
#51503=CARTESIAN_POINT('Ctrl Pts',(-24.2969865171199,26.6852980732459,22.0417236241302));
#51504=CARTESIAN_POINT('Ctrl Pts',(-24.2930770145456,26.6862265165814,22.0414738572342));
#51505=CARTESIAN_POINT('Ctrl Pts',(-24.2912606839137,26.686656199047,22.0413579338199));
#51506=CARTESIAN_POINT('Ctrl Pts',(-24.2871867342965,26.6876162214126,22.0410981836099));
#51507=CARTESIAN_POINT('Ctrl Pts',(-24.2849289205212,26.6881457013736,22.0409544074057));
#51508=CARTESIAN_POINT('Ctrl Pts',(-24.2791973384445,26.6894832895775,22.0405898742143));
#51509=CARTESIAN_POINT('Ctrl Pts',(-24.2757227863422,26.690288071689,22.0403693096189));
#51510=CARTESIAN_POINT('Ctrl Pts',(-24.2566864008831,26.6946640305572,22.0391631416016));
#51511=CARTESIAN_POINT('Ctrl Pts',(-24.2410991703837,26.6981253741572,22.0381837897782));
#51512=CARTESIAN_POINT('Ctrl Pts',(-23.9414990950949,26.7623228128117,22.0195070594619));
#51513=CARTESIAN_POINT('Ctrl Pts',(-23.6505361469162,26.7845184406953,22.003818444791));
#51514=CARTESIAN_POINT('Ctrl Pts',(-23.2366850760106,26.7601085720148,21.9804890889904));
#51515=CARTESIAN_POINT('Ctrl Pts',(-23.1134062222116,26.7456651514575,21.9734238939847));
#51516=CARTESIAN_POINT('Ctrl Pts',(-22.9355066728671,26.7143340014971,21.9628353624472));
#51517=CARTESIAN_POINT('Ctrl Pts',(-22.8800106240596,26.7030448227496,21.9594763885099));
#51518=CARTESIAN_POINT('Ctrl Pts',(-22.8050670341939,26.6857314588107,21.9548507690711));
#51519=CARTESIAN_POINT('Ctrl Pts',(-22.7853349179991,26.6809761770409,21.9536243836975));
#51520=CARTESIAN_POINT('Ctrl Pts',(-22.7520677239213,26.6726257730871,21.9515417922851));
#51521=CARTESIAN_POINT('Ctrl Pts',(-22.7385086078025,26.6691282006269,21.950688737525));
#51522=CARTESIAN_POINT('Ctrl Pts',(-22.7199581736282,26.6642139562409,21.9495157190235));
#51523=CARTESIAN_POINT('Ctrl Pts',(-22.7149467039351,26.6628733965306,21.9491982277253));
#51524=CARTESIAN_POINT('Ctrl Pts',(-22.7069145331746,26.6607040092595,21.9486884022618));
#51525=CARTESIAN_POINT('Ctrl Pts',(-22.7038917512611,26.6598828639475,21.9484963181619));
#51526=CARTESIAN_POINT('Ctrl Pts',(-22.6976040867666,26.6581649589556,21.9480963070609));
#51527=CARTESIAN_POINT('Ctrl Pts',(-22.694339412041,26.6572674588597,21.9478883561636));
#51528=CARTESIAN_POINT('Ctrl Pts',(-22.6868502574631,26.6551958967247,21.9474107232927));
#51529=CARTESIAN_POINT('Ctrl Pts',(-22.6826267540049,26.6540183567493,21.9471409282481));
#51530=CARTESIAN_POINT('Ctrl Pts',(-22.6692905905609,26.650270800429,21.9462876405822));
#51531=CARTESIAN_POINT('Ctrl Pts',(-22.6601869089148,26.6476692605655,21.9457031201806));
#51532=CARTESIAN_POINT('Ctrl Pts',(-22.5841290690265,26.6255713748685,21.9408023910844));
#51533=CARTESIAN_POINT('Ctrl Pts',(-22.5178170233325,26.6039480348988,21.9364167986947));
#51534=CARTESIAN_POINT('Ctrl Pts',(-22.4455299461476,26.5777526307021,21.9315047403781));
#51535=CARTESIAN_POINT('Ctrl Pts',(-22.4388056917508,26.5752905085064,21.9310465493669));
#51536=CARTESIAN_POINT('Ctrl Pts',(-22.4063475737677,26.5632829592691,21.9288287311217));
#51537=CARTESIAN_POINT('Ctrl Pts',(-22.380728739186,26.553431670277,21.9270595885942));
#51538=CARTESIAN_POINT('Ctrl Pts',(-22.2598109093321,26.505152923231,21.9186208491186));
#51539=CARTESIAN_POINT('Ctrl Pts',(-22.1663048046482,26.4625273153929,21.9118293256875));
#51540=CARTESIAN_POINT('Ctrl Pts',(-22.0750357484432,26.415536637139,21.9049549578222));
#51541=CARTESIAN_POINT('Ctrl Pts',(-22.075036015355,26.4155367745608,21.6601868380444));
#51542=CARTESIAN_POINT('Ctrl Pts',(-22.0764463957423,26.4162629211716,21.6602862264009));
#51543=CARTESIAN_POINT('Ctrl Pts',(-22.0778573206843,26.4169880307625,21.6603855517639));
#51544=CARTESIAN_POINT('Ctrl Pts',(-22.0836622160409,26.4199658954842,21.6607937824192));
#51545=CARTESIAN_POINT('Ctrl Pts',(-22.0880608519347,26.4222096060075,21.6611021319279));
#51546=CARTESIAN_POINT('Ctrl Pts',(-22.0946247348677,26.4255388036736,21.6615607807606));
#51547=CARTESIAN_POINT('Ctrl Pts',(-22.0967860507001,26.4266319603244,21.6617115621373));
#51548=CARTESIAN_POINT('Ctrl Pts',(-22.1004690787101,26.4284895618734,21.6619680930338));
#51549=CARTESIAN_POINT('Ctrl Pts',(-22.1019901646428,26.4292552372642,21.6620739207706));
#51550=CARTESIAN_POINT('Ctrl Pts',(-22.1051081026874,26.4308216304759,21.6622906026426));
#51551=CARTESIAN_POINT('Ctrl Pts',(-22.1067050103529,26.4316222246031,21.6624014488298));
#51552=CARTESIAN_POINT('Ctrl Pts',(-22.1105396657435,26.4335407037762,21.662667310779));
#51553=CARTESIAN_POINT('Ctrl Pts',(-22.1127780551258,26.4346573141347,21.6628222457602));
#51554=CARTESIAN_POINT('Ctrl Pts',(-22.1208909778117,26.4386926192767,21.6633828819819));
#51555=CARTESIAN_POINT('Ctrl Pts',(-22.1267731707987,26.4415960087239,21.6637876251807));
#51556=CARTESIAN_POINT('Ctrl Pts',(-22.2222988582826,26.4883843241016,21.6703330560544));
#51557=CARTESIAN_POINT('Ctrl Pts',(-22.3139353039589,26.5281047299056,21.6762200766067));
#51558=CARTESIAN_POINT('Ctrl Pts',(-22.620989974494,26.6445752253522,21.6951494157109));
#51559=CARTESIAN_POINT('Ctrl Pts',(-22.8427289817234,26.7026778028909,21.7076145565472));
#51560=CARTESIAN_POINT('Ctrl Pts',(-23.2295927045337,26.7611328033801,21.7297671697963));
#51561=CARTESIAN_POINT('Ctrl Pts',(-23.3920115749825,26.7732207244189,21.7391768018782));
#51562=CARTESIAN_POINT('Ctrl Pts',(-23.5783271758149,26.7729673299021,21.7504254247219));
#51563=CARTESIAN_POINT('Ctrl Pts',(-23.6020172087237,26.7726738616832,21.751863735977));
#51564=CARTESIAN_POINT('Ctrl Pts',(-23.6320087835959,26.7719715267369,21.753695485374));
#51565=CARTESIAN_POINT('Ctrl Pts',(-23.6383157110017,26.7718053006707,21.7540812910625));
#51566=CARTESIAN_POINT('Ctrl Pts',(-23.6484193885904,26.7715093147956,21.754700337127));
#51567=CARTESIAN_POINT('Ctrl Pts',(-23.6522164901239,26.7713913591052,21.7549332064639));
#51568=CARTESIAN_POINT('Ctrl Pts',(-23.659362594924,26.7711567193504,21.7553718877046));
#51569=CARTESIAN_POINT('Ctrl Pts',(-23.6627116448107,26.7710415250468,21.7555776525232));
#51570=CARTESIAN_POINT('Ctrl Pts',(-23.6702323417442,26.7707710977727,21.7560401183406));
#51571=CARTESIAN_POINT('Ctrl Pts',(-23.6744038734137,26.7706129825387,21.7562969095734));
#51572=CARTESIAN_POINT('Ctrl Pts',(-23.6849974750038,26.7701908347571,21.7569497314156));
#51573=CARTESIAN_POINT('Ctrl Pts',(-23.6914190618763,26.7699156949888,21.7573461104819));
#51574=CARTESIAN_POINT('Ctrl Pts',(-23.7267928537196,26.7682940356877,21.7595332403863));
#51575=CARTESIAN_POINT('Ctrl Pts',(-23.7557259436035,26.7665762397858,21.7613356246155));
#51576=CARTESIAN_POINT('Ctrl Pts',(-24.1039121620295,26.7411867143453,21.7831950315176));
#51577=CARTESIAN_POINT('Ctrl Pts',(-24.4178817536088,26.6704642075102,21.8048908056952));
#51578=CARTESIAN_POINT('Ctrl Pts',(-24.7931749678692,26.5248250988597,21.8320557341972));
#51579=CARTESIAN_POINT('Ctrl Pts',(-24.8689946044561,26.4919967141221,21.8375958184617));
#51580=CARTESIAN_POINT('Ctrl Pts',(-25.0116412155515,26.4236087082552,21.8480249947163));
#51581=CARTESIAN_POINT('Ctrl Pts',(-25.0786452988882,26.3885355095655,21.8529262326549));
#51582=CARTESIAN_POINT('Ctrl Pts',(-25.1510769983085,26.3473114039068,21.8581780833967));
#51583=CARTESIAN_POINT('Ctrl Pts',(-25.1577809798753,26.3434638732673,21.8586637204735));
#51584=CARTESIAN_POINT('Ctrl Pts',(-25.169324016705,26.3367838031091,21.859499029815));
#51585=CARTESIAN_POINT('Ctrl Pts',(-25.1741696056248,26.333962706671,21.8598494141207));
#51586=CARTESIAN_POINT('Ctrl Pts',(-25.181267489776,26.3298054861363,21.8603622431474));
#51587=CARTESIAN_POINT('Ctrl Pts',(-25.1835255245471,26.3284792594774,21.8605253260132));
#51588=CARTESIAN_POINT('Ctrl Pts',(-25.1874251810291,26.326182450778,21.8608068610967));
#51589=CARTESIAN_POINT('Ctrl Pts',(-25.1890675599506,26.3252131625194,21.8609253982015));
#51590=CARTESIAN_POINT('Ctrl Pts',(-25.1922267036798,26.3233449372324,21.8611533392096));
#51591=CARTESIAN_POINT('Ctrl Pts',(-25.1937435881581,26.3224462151301,21.8612627569666));
#51592=CARTESIAN_POINT('Ctrl Pts',(-25.1973351823327,26.3203142872611,21.86152176174));
#51593=CARTESIAN_POINT('Ctrl Pts',(-25.1994092492966,26.319079992654,21.8616712771367));
#51594=CARTESIAN_POINT('Ctrl Pts',(-25.2066647924874,26.3147511135016,21.8621941322118));
#51595=CARTESIAN_POINT('Ctrl Pts',(-25.2118390024339,26.3116442801015,21.8625666738927));
#51596=CARTESIAN_POINT('Ctrl Pts',(-25.276409863679,26.2726257663442,21.8672120642953));
#51597=CARTESIAN_POINT('Ctrl Pts',(-25.334645386931,26.2348156267273,21.8713625910134));
#51598=CARTESIAN_POINT('Ctrl Pts',(-25.4469352331633,26.1566399255117,21.8793814423341));
#51599=CARTESIAN_POINT('Ctrl Pts',(-25.5010325856955,26.1164011350829,21.8832524784931));
#51600=CARTESIAN_POINT('Ctrl Pts',(-25.6139967911004,26.026737493405,21.8914431122713));
#51601=CARTESIAN_POINT('Ctrl Pts',(-25.6724377510352,25.976844511764,21.895747409662));
#51602=CARTESIAN_POINT('Ctrl Pts',(-25.846438005017,25.8171962918457,21.9089509044041));
#51603=CARTESIAN_POINT('Ctrl Pts',(-25.9556824584759,25.7009281309257,21.9178122560498));
#51604=CARTESIAN_POINT('Ctrl Pts',(-26.1411737756435,25.4716165068541,21.9347404042038));
#51605=CARTESIAN_POINT('Ctrl Pts',(-26.2197192339311,25.360902340441,21.9427102115787));
#51606=CARTESIAN_POINT('Ctrl Pts',(-26.2965810997774,25.2366414030097,21.9516028868877));
#51607=CARTESIAN_POINT('Ctrl Pts',(-26.3020662368156,25.2276759598599,21.9522441632564));
#51608=CARTESIAN_POINT('Ctrl Pts',(-26.3099024106677,25.2147258749448,21.9531700353776));
#51609=CARTESIAN_POINT('Ctrl Pts',(-26.3122889169085,25.2107626856255,21.953453329523));
#51610=CARTESIAN_POINT('Ctrl Pts',(-26.3164212021051,25.2038667847388,21.9539461666776));
#51611=CARTESIAN_POINT('Ctrl Pts',(-26.3181708756185,25.2009364058075,21.9541555668586));
#51612=CARTESIAN_POINT('Ctrl Pts',(-26.3215299043653,25.1952902976599,21.9545589762894));
#51613=CARTESIAN_POINT('Ctrl Pts',(-26.3231399317027,25.1925749709514,21.9547529607105));
#51614=CARTESIAN_POINT('Ctrl Pts',(-26.3269290013617,25.1861632129859,21.9552109676479));
#51615=CARTESIAN_POINT('Ctrl Pts',(-26.3291046522654,25.1824647930407,21.9554751133619));
#51616=CARTESIAN_POINT('Ctrl Pts',(-26.3366292032537,25.1696150495754,21.9563927235673));
#51617=CARTESIAN_POINT('Ctrl Pts',(-26.3419402915647,25.1604417650476,21.9570475593227));
#51618=CARTESIAN_POINT('Ctrl Pts',(-26.4051572237718,25.0500008402285,21.9649289668725));
#51619=CARTESIAN_POINT('Ctrl Pts',(-26.457561940388,24.9456994672812,21.9723527171089));
#51620=CARTESIAN_POINT('Ctrl Pts',(-26.6106377890003,24.5947787639318,21.9973047179695));
#51621=CARTESIAN_POINT('Ctrl Pts',(-26.6864262812096,24.3385247782045,22.0155850818417));
#51622=CARTESIAN_POINT('Ctrl Pts',(-26.7434208645225,23.99378934334,22.0389717183269));
#51623=CARTESIAN_POINT('Ctrl Pts',(-26.753813932362,23.9111477523414,22.0444796083276));
#51624=CARTESIAN_POINT('Ctrl Pts',(-26.7648017569625,23.7842163582056,22.0527043200266));
#51625=CARTESIAN_POINT('Ctrl Pts',(-26.7677048295803,23.7401656530567,22.0555154931734));
#51626=CARTESIAN_POINT('Ctrl Pts',(-26.7699243108141,23.6911613928198,22.0585846933093));
#51627=CARTESIAN_POINT('Ctrl Pts',(-26.7701352643545,23.6862556973999,22.058891296807));
#51628=CARTESIAN_POINT('Ctrl Pts',(-26.7704324939789,23.6789549648665,22.0593466076058));
#51629=CARTESIAN_POINT('Ctrl Pts',(-26.7705273104283,23.6765603119111,22.0594957932674));
#51630=CARTESIAN_POINT('Ctrl Pts',(-26.7706847786253,23.6724678816208,22.059750478599));
#51631=CARTESIAN_POINT('Ctrl Pts',(-26.7707487589792,23.6707701608151,22.0598560535757));
#51632=CARTESIAN_POINT('Ctrl Pts',(-26.7708775871916,23.6672783296955,22.0600730329025));
#51633=CARTESIAN_POINT('Ctrl Pts',(-26.770942278251,23.6654842198546,22.0601844280769));
#51634=CARTESIAN_POINT('Ctrl Pts',(-26.7711127108691,23.6606452445706,22.060484638638));
#51635=CARTESIAN_POINT('Ctrl Pts',(-26.7712156342006,23.6576002718945,22.0606732944818));
#51636=CARTESIAN_POINT('Ctrl Pts',(-26.771578787329,23.646385417128,22.0613672049864));
#51637=CARTESIAN_POINT('Ctrl Pts',(-26.7718122553643,23.6382146096634,22.0618709643138));
#51638=CARTESIAN_POINT('Ctrl Pts',(-26.7722333698154,23.6212109205243,22.0629157143172));
#51639=CARTESIAN_POINT('Ctrl Pts',(-26.7724157877892,23.6123779642503,22.0634564197166));
#51640=CARTESIAN_POINT('Ctrl Pts',(-26.7726931806226,23.5956052742367,22.0644795172046));
#51641=CARTESIAN_POINT('Ctrl Pts',(-26.7727951398391,23.5876657472716,22.0649622648359));
#51642=CARTESIAN_POINT('Ctrl Pts',(-26.7729146745632,23.5745958028931,22.0657545310933));
#51643=CARTESIAN_POINT('Ctrl Pts',(-26.7729493432903,23.5694656308423,22.0660648935312));
#51644=CARTESIAN_POINT('Ctrl Pts',(-26.7729909304081,23.5599488226589,22.0666395309106));
#51645=CARTESIAN_POINT('Ctrl Pts',(-26.7730011430885,23.5555622220122,22.0669039639632));
#51646=CARTESIAN_POINT('Ctrl Pts',(-26.7730295122418,23.4565144897036,22.0728651960129));
#51647=CARTESIAN_POINT('Ctrl Pts',(-26.768885907985,23.3618891241273,22.0783635827235));
#51648=CARTESIAN_POINT('Ctrl Pts',(-26.7342660432386,22.968715485987,22.1008848756491));
#51649=CARTESIAN_POINT('Ctrl Pts',(-26.6663520468112,22.6750025033421,22.1170727569472));
#51650=CARTESIAN_POINT('Ctrl Pts',(-26.5512600840379,22.3753004133235,22.1358665854907));
#51651=CARTESIAN_POINT('Ctrl Pts',(-26.5435381406761,22.3557651751386,22.1371017100258));
#51652=CARTESIAN_POINT('Ctrl Pts',(-26.5298601922505,22.3221279270264,22.1392469360055));
#51653=CARTESIAN_POINT('Ctrl Pts',(-26.5239936182054,22.3079901622655,22.1401542789479));
#51654=CARTESIAN_POINT('Ctrl Pts',(-26.5153525377084,22.287578160092,22.1414728608592));
#51655=CARTESIAN_POINT('Ctrl Pts',(-26.5126583080729,22.2812700143222,22.1418815481744));
#51656=CARTESIAN_POINT('Ctrl Pts',(-26.4920611999013,22.2334679706731,22.1449876893229));
#51657=CARTESIAN_POINT('Ctrl Pts',(-26.4733081822191,22.1923478333727,22.1477123276043));
#51658=CARTESIAN_POINT('Ctrl Pts',(-26.4504517596974,22.1448992187652,22.1509229178505));
#51659=CARTESIAN_POINT('Ctrl Pts',(-26.4471826340804,22.1381726909365,22.1513796441832));
#51660=CARTESIAN_POINT('Ctrl Pts',(-26.4419325875747,22.1274652009284,22.1521092198527));
#51661=CARTESIAN_POINT('Ctrl Pts',(-26.4399667768313,22.1234768256693,22.1523815406841));
#51662=CARTESIAN_POINT('Ctrl Pts',(-26.4364850672209,22.116449600351,22.1528623529357));
#51663=CARTESIAN_POINT('Ctrl Pts',(-26.434972604284,22.1134090476228,22.1530707236677));
#51664=CARTESIAN_POINT('Ctrl Pts',(-26.4318379943147,22.1071323398165,22.1535015588974));
#51665=CARTESIAN_POINT('Ctrl Pts',(-26.4302151956256,22.1038965171593,22.1537240460665));
#51666=CARTESIAN_POINT('Ctrl Pts',(-26.4260517117564,22.0956294164649,22.1542934458337));
#51667=CARTESIAN_POINT('Ctrl Pts',(-26.4235032807951,22.09060207232,22.1546406307176));
#51668=CARTESIAN_POINT('Ctrl Pts',(-26.4130917608197,22.0701959632868,22.1560536467266));
#51669=CARTESIAN_POINT('Ctrl Pts',(-26.4051183990443,22.054874065133,22.1571233653697));
#51670=CARTESIAN_POINT('Ctrl Pts',(-26.3523250843868,21.9553858452228,22.1641274728358));
#51671=CARTESIAN_POINT('Ctrl Pts',(-26.303915742813,21.8731877842,22.1701896900044));
#51672=CARTESIAN_POINT('Ctrl Pts',(-26.1736907060326,21.6729435324092,22.1856814210099));
#51673=CARTESIAN_POINT('Ctrl Pts',(-26.0875011981096,21.5579979234275,22.1952531613907));
#51674=CARTESIAN_POINT('Ctrl Pts',(-25.8311015538655,21.2597858334105,22.2217891022904));
#51675=CARTESIAN_POINT('Ctrl Pts',(-25.6467759527366,21.0899435887018,22.2389369743643));
#51676=CARTESIAN_POINT('Ctrl Pts',(-25.4430266605609,20.9418952352266,22.2548551913077));
#51677=CARTESIAN_POINT('Ctrl Pts',(-25.4413821789678,20.9407026957653,22.2549834827015));
#51678=CARTESIAN_POINT('Ctrl Pts',(-25.4292130626363,20.9318954825739,22.2559314527651));
#51679=CARTESIAN_POINT('Ctrl Pts',(-25.4186433916031,20.9243427994723,22.2567471864274));
#51680=CARTESIAN_POINT('Ctrl Pts',(-25.4050658896473,20.9147643204457,22.257785019326));
#51681=CARTESIAN_POINT('Ctrl Pts',(-25.4021001084835,20.9126795455725,22.2580111084077));
#51682=CARTESIAN_POINT('Ctrl Pts',(-25.3973743609445,20.9093695147847,22.2583703887834));
#51683=CARTESIAN_POINT('Ctrl Pts',(-25.3956166896726,20.908141011412,22.2585038035544));
#51684=CARTESIAN_POINT('Ctrl Pts',(-25.3923261746684,20.9058460305471,22.258753165245));
#51685=CARTESIAN_POINT('Ctrl Pts',(-25.3907936406341,20.9047791381826,22.2588691404284));
#51686=CARTESIAN_POINT('Ctrl Pts',(-25.3873472344706,20.9023843246763,22.2591295829135));
#51687=CARTESIAN_POINT('Ctrl Pts',(-25.385432853435,20.9010571490387,22.25927399844));
#51688=CARTESIAN_POINT('Ctrl Pts',(-25.3797503594922,20.8971267834943,22.259701925648));
#51689=CARTESIAN_POINT('Ctrl Pts',(-25.3759781142735,20.894529534955,22.2599850301324));
#51690=CARTESIAN_POINT('Ctrl Pts',(-25.3457506897403,20.8738123336755,22.2622459460249));
#51691=CARTESIAN_POINT('Ctrl Pts',(-25.3190307501819,20.8560792682073,22.2641978257712));
#51692=CARTESIAN_POINT('Ctrl Pts',(-25.2238382042374,20.7949301824093,22.2710052571156));
#51693=CARTESIAN_POINT('Ctrl Pts',(-25.1539921504694,20.7536990013019,22.2757378331628));
#51694=CARTESIAN_POINT('Ctrl Pts',(-24.7428921853354,20.5314950188285,22.3025486803452));
#51695=CARTESIAN_POINT('Ctrl Pts',(-24.3729023624256,20.4104169822941,22.3230909516774));
#51696=CARTESIAN_POINT('Ctrl Pts',(-23.9707885972029,20.3549977687582,22.3476492421347));
#51697=CARTESIAN_POINT('Ctrl Pts',(-23.9513014058937,20.3524934168825,22.3488434309341));
#51698=CARTESIAN_POINT('Ctrl Pts',(-23.9256729575317,20.3494377835366,22.3504196515478));
#51699=CARTESIAN_POINT('Ctrl Pts',(-23.9195510050214,20.348725679562,22.3507965941183));
#51700=CARTESIAN_POINT('Ctrl Pts',(-23.910084729048,20.3476520778044,22.3513801241917));
#51701=CARTESIAN_POINT('Ctrl Pts',(-23.9067417958936,20.3472782448974,22.3515863218109));
#51702=CARTESIAN_POINT('Ctrl Pts',(-23.9000738679614,20.3465431532836,22.351997870356));
#51703=CARTESIAN_POINT('Ctrl Pts',(-23.8967488837817,20.3461818354579,22.3522032191456));
#51704=CARTESIAN_POINT('Ctrl Pts',(-23.8894444222316,20.3453995807216,22.352654623136));
#51705=CARTESIAN_POINT('Ctrl Pts',(-23.8854647155961,20.3449808790105,22.3529007485635));
#51706=CARTESIAN_POINT('Ctrl Pts',(-23.874064582173,20.3438029441067,22.3536063291968));
#51707=CARTESIAN_POINT('Ctrl Pts',(-23.8666423218697,20.3430620632392,22.3540663627267));
#51708=CARTESIAN_POINT('Ctrl Pts',(-23.8499599849756,20.3414553265864,22.3551018306533));
#51709=CARTESIAN_POINT('Ctrl Pts',(-23.8406986267633,20.3406037777024,22.3556777130099));
#51710=CARTESIAN_POINT('Ctrl Pts',(-23.6115287247441,20.3205324242405,22.3699538155614));
#51711=CARTESIAN_POINT('Ctrl Pts',(-23.3902729610331,20.3239206420583,22.3843927214189));
#51712=CARTESIAN_POINT('Ctrl Pts',(-22.9177362731837,20.3798968808219,22.4163855404536));
#51713=CARTESIAN_POINT('Ctrl Pts',(-22.6687886155403,20.4399045165147,22.4339703003795));
#51714=CARTESIAN_POINT('Ctrl Pts',(-22.4265410283983,20.5297558656829,22.4505030017711));
#51715=CARTESIAN_POINT('Ctrl Pts',(-22.4235645046418,20.5308648881647,22.450706036401));
#51716=CARTESIAN_POINT('Ctrl Pts',(-22.4147919680841,20.5341482244502,22.4513041101213));
#51717=CARTESIAN_POINT('Ctrl Pts',(-22.4090005361102,20.5363348540477,22.4516985345263));
#51718=CARTESIAN_POINT('Ctrl Pts',(-22.3829131339263,20.5462704640352,22.4534732452903));
#51719=CARTESIAN_POINT('Ctrl Pts',(-22.3626889078704,20.5542081004693,22.4548437116512));
#51720=CARTESIAN_POINT('Ctrl Pts',(-22.3388628863324,20.5638385500347,22.4564505521771));
#51721=CARTESIAN_POINT('Ctrl Pts',(-22.3351826613638,20.5653340146556,22.4566985301896));
#51722=CARTESIAN_POINT('Ctrl Pts',(-22.3292671729498,20.5677505349162,22.4570967602308));
#51723=CARTESIAN_POINT('Ctrl Pts',(-22.327030179076,20.568667301787,22.4572472708386));
#51724=CARTESIAN_POINT('Ctrl Pts',(-22.323054038676,20.5703020352439,22.4575146441724));
#51725=CARTESIAN_POINT('Ctrl Pts',(-22.3213144889652,20.5710190078216,22.4576315675245));
#51726=CARTESIAN_POINT('Ctrl Pts',(-22.3176647016531,20.5725270442687,22.457876777482));
#51727=CARTESIAN_POINT('Ctrl Pts',(-22.3157546015942,20.5733184212602,22.4580050443085));
#51728=CARTESIAN_POINT('Ctrl Pts',(-22.3107279646035,20.5754066861511,22.4583424306366));
#51729=CARTESIAN_POINT('Ctrl Pts',(-22.3076126908925,20.5767066377375,22.4585513629225));
#51730=CARTESIAN_POINT('Ctrl Pts',(-22.2937098885428,20.5825337085041,22.4594830753684));
#51731=CARTESIAN_POINT('Ctrl Pts',(-22.2829448372896,20.5871147277434,22.460202602816));
#51732=CARTESIAN_POINT('Ctrl Pts',(-22.20265050817,20.621801241231,22.4655568614164));
#51733=CARTESIAN_POINT('Ctrl Pts',(-22.1341710248566,20.6542944127737,22.4700528257604));
#51734=CARTESIAN_POINT('Ctrl Pts',(-21.9935433494579,20.7272043907029,22.4792657272348));
#51735=CARTESIAN_POINT('Ctrl Pts',(-21.9216773645678,20.7680432170251,22.4839626674951));
#51736=CARTESIAN_POINT('Ctrl Pts',(-21.5793422268877,20.9803949539836,22.5066513606238));
#51737=CARTESIAN_POINT('Ctrl Pts',(-21.3339326999549,21.1887762136587,22.5241234346838));
#51738=CARTESIAN_POINT('Ctrl Pts',(-21.104402099322,21.4515016581899,22.5451230954145));
#51739=CARTESIAN_POINT('Ctrl Pts',(-21.0858283122358,21.4733431087205,22.5468604336561));
#51740=CARTESIAN_POINT('Ctrl Pts',(-21.0634670352489,21.5003607196851,22.5490004411722));
#51741=CARTESIAN_POINT('Ctrl Pts',(-21.0593999425179,21.5053046290978,22.5493916717176));
#51742=CARTESIAN_POINT('Ctrl Pts',(-21.0527102191427,21.5134861436145,22.5500385186929));
#51743=CARTESIAN_POINT('Ctrl Pts',(-21.0500790751915,21.5167167907402,22.5502937897018));
#51744=CARTESIAN_POINT('Ctrl Pts',(-21.0453435231106,21.5225544165647,22.5507547856067));
#51745=CARTESIAN_POINT('Ctrl Pts',(-21.0432368978333,21.5251595958453,22.5509604205573));
#51746=CARTESIAN_POINT('Ctrl Pts',(-21.0387952470279,21.5306699604002,22.5513951720596));
#51747=CARTESIAN_POINT('Ctrl Pts',(-21.0364611928579,21.5335759191499,22.5516243272984));
#51748=CARTESIAN_POINT('Ctrl Pts',(-21.030277491015,21.5413022057085,22.5522332949957));
#51749=CARTESIAN_POINT('Ctrl Pts',(-21.0264366474953,21.5461295315411,22.5526134600353));
#51750=CARTESIAN_POINT('Ctrl Pts',(-21.0180051220917,21.5567892863216,22.5534522708849));
#51751=CARTESIAN_POINT('Ctrl Pts',(-21.0134206914014,21.5626265943797,22.5539111640394));
#51752=CARTESIAN_POINT('Ctrl Pts',(-20.9998741074977,21.5799985318516,22.5552755638564));
#51753=CARTESIAN_POINT('Ctrl Pts',(-20.9909702570987,21.5915781947735,22.5561833777106));
#51754=CARTESIAN_POINT('Ctrl Pts',(-20.895514836192,21.7174823367168,22.5660368682417));
#51755=CARTESIAN_POINT('Ctrl Pts',(-20.8166189757819,21.8373846882711,22.575280703499));
#51756=CARTESIAN_POINT('Ctrl Pts',(-20.6608902327134,22.1123670395073,22.5961746626137));
#51757=CARTESIAN_POINT('Ctrl Pts',(-20.5880219296622,22.2691939063896,22.6079032353554));
#51758=CARTESIAN_POINT('Ctrl Pts',(-20.4766736586584,22.5698777183794,22.6295715035838));
#51759=CARTESIAN_POINT('Ctrl Pts',(-20.434893406036,22.71205890173,22.6394965467774));
#51760=CARTESIAN_POINT('Ctrl Pts',(-20.4020508637683,22.8610757589922,22.6492677469313));
#51761=CARTESIAN_POINT('Ctrl Pts',(-20.4010786351739,22.8655320515275,22.6495593719663));
#51762=CARTESIAN_POINT('Ctrl Pts',(-20.3990084568063,22.8751185692532,22.6501854589494));
#51763=CARTESIAN_POINT('Ctrl Pts',(-20.3979135647258,22.8802494533953,22.6505197738264));
#51764=CARTESIAN_POINT('Ctrl Pts',(-20.3950184359607,22.8939808108006,22.6514123500677));
#51765=CARTESIAN_POINT('Ctrl Pts',(-20.3932408202013,22.9025860836173,22.6519694917124));
#51766=CARTESIAN_POINT('Ctrl Pts',(-20.3886044940821,22.9255027956907,22.6534471070079));
#51767=CARTESIAN_POINT('Ctrl Pts',(-20.3858077197839,22.939826780268,22.654364355876));
#51768=CARTESIAN_POINT('Ctrl Pts',(-20.3824077114731,22.957891911815,22.6555127870491));
#51769=CARTESIAN_POINT('Ctrl Pts',(-20.3817136978569,22.9616154891958,22.6557490533613));
#51770=CARTESIAN_POINT('Ctrl Pts',(-20.3806301746523,22.9674863362381,22.6561208519729));
#51771=CARTESIAN_POINT('Ctrl Pts',(-20.3802362815485,22.9696327777189,22.6562566347933));
#51772=CARTESIAN_POINT('Ctrl Pts',(-20.3795131302459,22.9735961174427,22.65650707372));
#51773=CARTESIAN_POINT('Ctrl Pts',(-20.3791832552723,22.9754128878277,22.6566217646017));
#51774=CARTESIAN_POINT('Ctrl Pts',(-20.3784508956791,22.9794661372953,22.6568774001009));
#51775=CARTESIAN_POINT('Ctrl Pts',(-20.3780492159598,22.9817027537687,22.6570182978256));
#51776=CARTESIAN_POINT('Ctrl Pts',(-20.3768929560307,22.9881803642793,22.6574258908427));
#51777=CARTESIAN_POINT('Ctrl Pts',(-20.3761445089144,22.9924224696903,22.6576922351657));
#51778=CARTESIAN_POINT('Ctrl Pts',(-20.3710763432167,23.0214886722149,22.6595132678774));
#51779=CARTESIAN_POINT('Ctrl Pts',(-20.36703922293,23.0463620852628,22.6610520704653));
#51780=CARTESIAN_POINT('Ctrl Pts',(-20.3555033210215,23.123119164438,22.6657476755412));
#51781=CARTESIAN_POINT('Ctrl Pts',(-20.3489779833575,23.175142717168,22.6688559198228));
#51782=CARTESIAN_POINT('Ctrl Pts',(-20.3361058115589,23.3029499503053,22.6763609012535));
#51783=CARTESIAN_POINT('Ctrl Pts',(-20.3311659639058,23.3788447157707,22.6807055600794));
#51784=CARTESIAN_POINT('Ctrl Pts',(-20.3212907589536,23.7122777360982,22.6995662649293));
#51785=CARTESIAN_POINT('Ctrl Pts',(-20.3445505529016,23.9696824809969,22.7136162244674));
#51786=CARTESIAN_POINT('Ctrl Pts',(-20.419144898918,24.3199234134494,22.734445428303));
#51787=CARTESIAN_POINT('Ctrl Pts',(-20.4446799202941,24.4172264943357,22.7404122811215));
#51788=CARTESIAN_POINT('Ctrl Pts',(-20.4775246203374,24.5221316003617,22.7471030288081));
#51789=CARTESIAN_POINT('Ctrl Pts',(-20.4803694731801,24.5310806233909,22.7476758517431));
#51790=CARTESIAN_POINT('Ctrl Pts',(-20.4846463683445,24.5443335074221,22.7485272701483));
#51791=CARTESIAN_POINT('Ctrl Pts',(-20.4860484686196,24.548647040176,22.7488048782838));
#51792=CARTESIAN_POINT('Ctrl Pts',(-20.4884619394352,24.5560190597004,22.749280166026));
#51793=CARTESIAN_POINT('Ctrl Pts',(-20.489468801106,24.5590790252782,22.7494776965033));
#51794=CARTESIAN_POINT('Ctrl Pts',(-20.4914346141601,24.5650233180399,22.7498619054075));
#51795=CARTESIAN_POINT('Ctrl Pts',(-20.49239306167,24.5679078087575,22.7500485669665));
#51796=CARTESIAN_POINT('Ctrl Pts',(-20.4946652427661,24.5747138470729,22.7504895283489));
#51797=CARTESIAN_POINT('Ctrl Pts',(-20.4959824448376,24.5786342231123,22.7507439428185));
#51798=CARTESIAN_POINT('Ctrl Pts',(-20.4997391659437,24.5897444330355,22.7514661264956));
#51799=CARTESIAN_POINT('Ctrl Pts',(-20.502196539379,24.5969281613456,22.7519344873749));
#51800=CARTESIAN_POINT('Ctrl Pts',(-20.507884945275,24.6133673583722,22.7530095341188));
#51801=CARTESIAN_POINT('Ctrl Pts',(-20.5111328577622,24.6226168679614,22.7536167787485));
#51802=CARTESIAN_POINT('Ctrl Pts',(-20.5215667874341,24.6519028036563,22.7555470498871));
#51803=CARTESIAN_POINT('Ctrl Pts',(-20.5289090218194,24.6718826041495,22.7568752701931));
#51804=CARTESIAN_POINT('Ctrl Pts',(-20.5578279811451,24.7482324784138,22.7619952357672));
#51805=CARTESIAN_POINT('Ctrl Pts',(-20.5807876865711,24.8040620834945,22.7658327958149));
#51806=CARTESIAN_POINT('Ctrl Pts',(-20.6730908106924,25.0117296688887,22.7804700538646));
#51807=CARTESIAN_POINT('Ctrl Pts',(-20.7526188622951,25.1587326170157,22.7915949987556));
#51808=CARTESIAN_POINT('Ctrl Pts',(-20.9757766503871,25.5042045166071,22.8193662535487));
#51809=CARTESIAN_POINT('Ctrl Pts',(-21.1313280487672,25.6937730264392,22.8361182237649));
#51810=CARTESIAN_POINT('Ctrl Pts',(-21.3168358779287,25.8736470160998,22.8524385549815));
#51811=CARTESIAN_POINT('Ctrl Pts',(-21.3269066450529,25.8832859572276,22.8533143698741));
#51812=CARTESIAN_POINT('Ctrl Pts',(-21.3397462274164,25.8954163433241,22.854417789897));
#51813=CARTESIAN_POINT('Ctrl Pts',(-21.3424570464667,25.8979685537831,22.8546500169291));
#51814=CARTESIAN_POINT('Ctrl Pts',(-21.3467528481071,25.901998989989,22.8550168498008));
#51815=CARTESIAN_POINT('Ctrl Pts',(-21.3483348987208,25.9034803144084,22.8551516952708));
#51816=CARTESIAN_POINT('Ctrl Pts',(-21.3512813120622,25.906233562384,22.8554023627709));
#51817=CARTESIAN_POINT('Ctrl Pts',(-21.3526452761006,25.9075058892977,22.8555182159344));
#51818=CARTESIAN_POINT('Ctrl Pts',(-21.3556928342781,25.9103437549952,22.8557766553673));
#51819=CARTESIAN_POINT('Ctrl Pts',(-21.3573769954886,25.9119086731795,22.8559191933721));
#51820=CARTESIAN_POINT('Ctrl Pts',(-21.3623139940557,25.9164862849827,22.8563362121294));
#51821=CARTESIAN_POINT('Ctrl Pts',(-21.3655713923204,25.9194940853371,22.8566103163586));
#51822=CARTESIAN_POINT('Ctrl Pts',(-21.3895337715024,25.9415289113025,22.8586191640723));
#51823=CARTESIAN_POINT('Ctrl Pts',(-21.4104816159046,25.9602917103261,22.8603340449385));
#51824=CARTESIAN_POINT('Ctrl Pts',(-21.4799155573067,26.0208639680878,22.865895127633));
#51825=CARTESIAN_POINT('Ctrl Pts',(-21.5294046982868,26.0615054560786,22.8696664466894));
#51826=CARTESIAN_POINT('Ctrl Pts',(-21.6887799156698,26.1846226042972,22.8813388058313));
#51827=CARTESIAN_POINT('Ctrl Pts',(-21.8027496179665,26.2615666863508,22.8890142787548));
#51828=CARTESIAN_POINT('Ctrl Pts',(-21.9717777561264,26.3605832795733,22.8999608046169));
#51829=CARTESIAN_POINT('Ctrl Pts',(-22.0230465680281,26.3887695579674,22.903226880509));
#51830=CARTESIAN_POINT('Ctrl Pts',(-22.0750361284943,26.4155368328116,22.9065074728514));
#51831=CARTESIAN_POINT('Origin',(-23.5502525316942,23.5502525316942,-77.3107734492734));
#51832=CARTESIAN_POINT('',(-22.0750358518511,26.4155366903795,24.4018187331506));
#51833=CARTESIAN_POINT('',(-22.0750361722079,26.4155368553179,24.1541632309577));
#51834=CARTESIAN_POINT('',(-22.0750360153461,26.4155367745563,-77.3107734492734));
#51835=CARTESIAN_POINT('Ctrl Pts',(-22.0750358518511,26.4155366903795,24.4018187331506));
#51836=CARTESIAN_POINT('Ctrl Pts',(-22.0079631752057,26.3810037345297,24.3975360295522));
#51837=CARTESIAN_POINT('Ctrl Pts',(-21.9420832190341,26.3441054453173,24.3933062394776));
#51838=CARTESIAN_POINT('Ctrl Pts',(-21.7531360000098,26.2293693195608,24.3809461951244));
#51839=CARTESIAN_POINT('Ctrl Pts',(-21.6340112926944,26.1455004915822,24.3728500554956));
#51840=CARTESIAN_POINT('Ctrl Pts',(-21.4157812792204,25.968616138674,24.356803351267));
#51841=CARTESIAN_POINT('Ctrl Pts',(-21.3160859431602,25.8768257411961,24.3488984148019));
#51842=CARTESIAN_POINT('Ctrl Pts',(-21.2076234686032,25.7635458186562,24.3394175410384));
#51843=CARTESIAN_POINT('Ctrl Pts',(-21.192937500504,25.7478976146072,24.3381136787245));
#51844=CARTESIAN_POINT('Ctrl Pts',(-21.1742742557907,25.7276092083621,24.3364300723115));
#51845=CARTESIAN_POINT('Ctrl Pts',(-21.1701521406752,25.7231025018612,24.3360565203686));
#51846=CARTESIAN_POINT('Ctrl Pts',(-21.1635366867497,25.7158284165264,24.3354542655788));
#51847=CARTESIAN_POINT('Ctrl Pts',(-21.1610352777147,25.7130683700349,24.3352259053523));
#51848=CARTESIAN_POINT('Ctrl Pts',(-21.1562843036885,25.7078078609216,24.3347909567144));
#51849=CARTESIAN_POINT('Ctrl Pts',(-21.1540338555843,25.7053081995376,24.3345844060294));
#51850=CARTESIAN_POINT('Ctrl Pts',(-21.148918054092,25.6996079567441,24.3341136702865));
#51851=CARTESIAN_POINT('Ctrl Pts',(-21.1460551830693,25.6964051649177,24.333849381212));
#51852=CARTESIAN_POINT('Ctrl Pts',(-21.1373664027058,25.6866455256547,24.3330446407902));
#51853=CARTESIAN_POINT('Ctrl Pts',(-21.131560886047,25.6800706499723,24.3325033359555));
#51854=CARTESIAN_POINT('Ctrl Pts',(-21.0904037976176,25.6330740364424,24.3286399130351));
#51855=CARTESIAN_POINT('Ctrl Pts',(-21.0560423604432,25.5918000512558,24.3252769939978));
#51856=CARTESIAN_POINT('Ctrl Pts',(-21.0159431835523,25.5411099709902,24.3211788947711));
#51857=CARTESIAN_POINT('Ctrl Pts',(-21.0092005157125,25.5324966798922,24.3204836340995));
#51858=CARTESIAN_POINT('Ctrl Pts',(-20.9853873198502,25.5017558084376,24.3180060720846));
#51859=CARTESIAN_POINT('Ctrl Pts',(-20.9685612876402,25.4794411793467,24.3162146077592));
#51860=CARTESIAN_POINT('Ctrl Pts',(-20.7751902269879,25.2159323113474,24.2951400308635));
#51861=CARTESIAN_POINT('Ctrl Pts',(-20.6327546317516,24.9515405885001,24.2745770975018));
#51862=CARTESIAN_POINT('Ctrl Pts',(-20.4979973178576,24.5883748060967,24.2486904013394));
#51863=CARTESIAN_POINT('Ctrl Pts',(-20.4706223654047,24.5041081209628,24.2428502438269));
#51864=CARTESIAN_POINT('Ctrl Pts',(-20.4406723933143,24.3970923722866,24.2357246382108));
#51865=CARTESIAN_POINT('Ctrl Pts',(-20.4348212558161,24.3753067016134,24.2342889737222));
#51866=CARTESIAN_POINT('Ctrl Pts',(-20.427022506253,24.3450028346687,24.2323143129177));
#51867=CARTESIAN_POINT('Ctrl Pts',(-20.4248802191216,24.3365360351508,24.2317650078408));
#51868=CARTESIAN_POINT('Ctrl Pts',(-20.42172488314,24.3238487769547,24.2309456000024));
#51869=CARTESIAN_POINT('Ctrl Pts',(-20.4206859197852,24.3196348947578,24.2306740574281));
#51870=CARTESIAN_POINT('Ctrl Pts',(-20.4190301628392,24.312860540749,24.2302385143871));
#51871=CARTESIAN_POINT('Ctrl Pts',(-20.4184079944704,24.310301407407,24.2300742084321));
#51872=CARTESIAN_POINT('Ctrl Pts',(-20.4172533017819,24.3055263771203,24.2297680628927));
#51873=CARTESIAN_POINT('Ctrl Pts',(-20.4167199901274,24.3033106750237,24.2296261779976));
#51874=CARTESIAN_POINT('Ctrl Pts',(-20.4157570256761,24.299291197865,24.2293691011349));
#51875=CARTESIAN_POINT('Ctrl Pts',(-20.4153265787939,24.2974876155665,24.2292538629038));
#51876=CARTESIAN_POINT('Ctrl Pts',(-20.4144844931047,24.2939457223215,24.2290277834884));
#51877=CARTESIAN_POINT('Ctrl Pts',(-20.4140727441406,24.2922074452866,24.2289169359829));
#51878=CARTESIAN_POINT('Ctrl Pts',(-20.4130878261693,24.2880339570874,24.2286510530411));
#51879=CARTESIAN_POINT('Ctrl Pts',(-20.4125160459627,24.2855984145647,24.2284960984256));
#51880=CARTESIAN_POINT('Ctrl Pts',(-20.4104547671604,24.2767720574443,24.227935291115));
#51881=CARTESIAN_POINT('Ctrl Pts',(-20.4089819393871,24.2703773064123,24.2275303972549));
#51882=CARTESIAN_POINT('Ctrl Pts',(-20.3853819170214,24.166460108823,24.220973008481));
#51883=CARTESIAN_POINT('Ctrl Pts',(-20.3677835048837,24.0679525574876,24.215075162204));
#51884=CARTESIAN_POINT('Ctrl Pts',(-20.3359322652538,23.8247654970151,24.2009392795981));
#51885=CARTESIAN_POINT('Ctrl Pts',(-20.3268263135013,23.6796371019528,24.1928604504361));
#51886=CARTESIAN_POINT('Ctrl Pts',(-20.3282805640026,23.3843225230612,24.1763558200481));
#51887=CARTESIAN_POINT('Ctrl Pts',(-20.3394994951309,23.2345045387215,24.1679448463602));
#51888=CARTESIAN_POINT('Ctrl Pts',(-20.3716359015178,23.0137361645292,24.1550303038649));
#51889=CARTESIAN_POINT('Ctrl Pts',(-20.3846122069129,22.9418335279393,24.1507424535152));
#51890=CARTESIAN_POINT('Ctrl Pts',(-20.4092800108476,22.82752401855,24.1437563605225));
#51891=CARTESIAN_POINT('Ctrl Pts',(-20.4194161751385,22.7848060610108,24.1411073069936));
#51892=CARTESIAN_POINT('Ctrl Pts',(-20.4323425579423,22.7348914558426,24.1379625067953));
#51893=CARTESIAN_POINT('Ctrl Pts',(-20.4342901825287,22.7274798258884,24.1374942601693));
#51894=CARTESIAN_POINT('Ctrl Pts',(-20.4373118555928,22.7161455542953,24.1367761956621));
#51895=CARTESIAN_POINT('Ctrl Pts',(-20.4383669346938,22.7122178464856,24.1365269944512));
#51896=CARTESIAN_POINT('Ctrl Pts',(-20.4403029550873,22.705064758111,24.136072478375));
#51897=CARTESIAN_POINT('Ctrl Pts',(-20.4411814876348,22.7018387266974,24.1358672421408));
#51898=CARTESIAN_POINT('Ctrl Pts',(-20.442956521802,22.6953604623846,24.1354545975078));
#51899=CARTESIAN_POINT('Ctrl Pts',(-20.443853112825,22.6921082585257,24.135247186418));
#51900=CARTESIAN_POINT('Ctrl Pts',(-20.4464152554957,22.6828712328369,24.1346573585358));
#51901=CARTESIAN_POINT('Ctrl Pts',(-20.4480930010358,22.6768898348684,24.1342745445432));
#51902=CARTESIAN_POINT('Ctrl Pts',(-20.4552580204885,22.6516266722458,24.1326539587713));
#51903=CARTESIAN_POINT('Ctrl Pts',(-20.4609077596964,22.6323918068861,24.1314108904882));
#51904=CARTESIAN_POINT('Ctrl Pts',(-20.579037814021,22.2436619568108,24.1060981712028));
#51905=CARTESIAN_POINT('Ctrl Pts',(-20.7568533496482,21.8973641530626,24.0794799751109));
#51906=CARTESIAN_POINT('Ctrl Pts',(-21.0580049383886,21.5040922930838,24.0464784186985));
#51907=CARTESIAN_POINT('Ctrl Pts',(-21.1288552356862,21.4207195381369,24.0393274148467));
#51908=CARTESIAN_POINT('Ctrl Pts',(-21.207017762038,21.3376996614197,24.0321765704504));
#51909=CARTESIAN_POINT('Ctrl Pts',(-21.2102277273648,21.3343050356429,24.0318841254644));
#51910=CARTESIAN_POINT('Ctrl Pts',(-21.2153531969917,21.3289082682564,24.0314191321018));
#51911=CARTESIAN_POINT('Ctrl Pts',(-21.2172639058891,21.3269016120452,24.0312462212755));
#51912=CARTESIAN_POINT('Ctrl Pts',(-21.2208977280138,21.3230951575097,24.030918201333));
#51913=CARTESIAN_POINT('Ctrl Pts',(-21.2226203436965,21.321294890035,24.0307630541035));
#51914=CARTESIAN_POINT('Ctrl Pts',(-21.2256323831372,21.3181543738495,24.0304923899652));
#51915=CARTESIAN_POINT('Ctrl Pts',(-21.2269208806809,21.3168132419883,24.0303768005737));
#51916=CARTESIAN_POINT('Ctrl Pts',(-21.229442314416,21.3141933524269,24.0301509900592));
#51917=CARTESIAN_POINT('Ctrl Pts',(-21.2306751439847,21.3129145017412,24.0300407610879));
#51918=CARTESIAN_POINT('Ctrl Pts',(-21.2336206654936,21.3098640763665,24.0297778225378));
#51919=CARTESIAN_POINT('Ctrl Pts',(-21.2353343362327,21.308093442183,24.0296251898184));
#51920=CARTESIAN_POINT('Ctrl Pts',(-21.2405215403746,21.3027460982412,24.029164203487));
#51921=CARTESIAN_POINT('Ctrl Pts',(-21.2440013654985,21.2991754606271,24.0288563394914));
#51922=CARTESIAN_POINT('Ctrl Pts',(-21.2796475405569,21.262768447828,24.0257166485799));
#51923=CARTESIAN_POINT('Ctrl Pts',(-21.3125066541611,21.230613684264,24.0229383125195));
#51924=CARTESIAN_POINT('Ctrl Pts',(-21.3478602393354,21.1974686598157,24.0200539227875));
#51925=CARTESIAN_POINT('Ctrl Pts',(-21.3496779478041,21.1957684569927,24.0199059072776));
#51926=CARTESIAN_POINT('Ctrl Pts',(-21.5687857356509,20.9913002593508,24.00209811902));
#51927=CARTESIAN_POINT('Ctrl Pts',(-21.8131028881281,20.819536931826,23.9861602636745));
#51928=CARTESIAN_POINT('Ctrl Pts',(-22.1683941379893,20.6370035107918,23.9634465376667));
#51929=CARTESIAN_POINT('Ctrl Pts',(-22.2614169239764,20.5946726194036,23.9575507063536));
#51930=CARTESIAN_POINT('Ctrl Pts',(-22.4168138936112,20.5326904840661,23.9476581122768));
#51931=CARTESIAN_POINT('Ctrl Pts',(-22.4780551433208,20.5103914005395,23.9437495198142));
#51932=CARTESIAN_POINT('Ctrl Pts',(-22.547945110198,20.4873178782211,23.9392632779311));
#51933=CARTESIAN_POINT('Ctrl Pts',(-22.5559734687301,20.4847023361426,23.9387475671025));
#51934=CARTESIAN_POINT('Ctrl Pts',(-22.5680386949508,20.4808240129829,23.9379719572683));
#51935=CARTESIAN_POINT('Ctrl Pts',(-22.5720679652259,20.4795375650744,23.9377128388575));
#51936=CARTESIAN_POINT('Ctrl Pts',(-22.5789982108657,20.4773399308067,23.937266989186));
#51937=CARTESIAN_POINT('Ctrl Pts',(-22.5818979718701,20.4764249088786,23.9370803844784));
#51938=CARTESIAN_POINT('Ctrl Pts',(-22.5878689346973,20.4745500544841,23.9366960341396));
#51939=CARTESIAN_POINT('Ctrl Pts',(-22.5909402870981,20.4735907151589,23.9364982725071));
#51940=CARTESIAN_POINT('Ctrl Pts',(-22.5983319461898,20.4712940690194,23.936022185967));
#51941=CARTESIAN_POINT('Ctrl Pts',(-22.6026536328475,20.4699612560899,23.9357437137106));
#51942=CARTESIAN_POINT('Ctrl Pts',(-22.6159064614918,20.4659045992508,23.9348893832668));
#51943=CARTESIAN_POINT('Ctrl Pts',(-22.6248465879802,20.4632104873314,23.9343125510196));
#51944=CARTESIAN_POINT('Ctrl Pts',(-22.6580599892546,20.4533588538683,23.9321675711633));
#51945=CARTESIAN_POINT('Ctrl Pts',(-22.6824051009921,20.4464486134971,23.930591368066));
#51946=CARTESIAN_POINT('Ctrl Pts',(-22.7126467914289,20.4382482695302,23.9286280782575));
#51947=CARTESIAN_POINT('Ctrl Pts',(-22.7184694446759,20.4366869230702,23.9282498293846));
#51948=CARTESIAN_POINT('Ctrl Pts',(-22.7309281087085,20.4333835701199,23.9274399688955));
#51949=CARTESIAN_POINT('Ctrl Pts',(-22.7375653611147,20.4316464014928,23.9270082040032));
#51950=CARTESIAN_POINT('Ctrl Pts',(-22.7458004291177,20.4295191111709,23.9264720982249));
#51951=CARTESIAN_POINT('Ctrl Pts',(-22.7473931014676,20.4291089908439,23.9263683961725));
#51952=CARTESIAN_POINT('Ctrl Pts',(-22.7556086698187,20.4270001493663,23.925833368378));
#51953=CARTESIAN_POINT('Ctrl Pts',(-22.7622366066637,20.4253212985825,23.9254014116947));
#51954=CARTESIAN_POINT('Ctrl Pts',(-22.7723405604248,20.4227961649249,23.9247424207801));
#51955=CARTESIAN_POINT('Ctrl Pts',(-22.7758127563559,20.4219345498868,23.9245158715041));
#51956=CARTESIAN_POINT('Ctrl Pts',(-22.7833158127943,20.4200859460753,23.9240261290462));
#51957=CARTESIAN_POINT('Ctrl Pts',(-22.7873471557163,20.4191009589386,23.9237628735203));
#51958=CARTESIAN_POINT('Ctrl Pts',(-22.7952959548634,20.417175073127,23.9232435615939));
#51959=CARTESIAN_POINT('Ctrl Pts',(-22.799213296126,20.4162337281952,23.9229875196409));
#51960=CARTESIAN_POINT('Ctrl Pts',(-22.8089984399459,20.4139017383293,23.9223476662059));
#51961=CARTESIAN_POINT('Ctrl Pts',(-22.814868382238,20.4125202168652,23.9219635732011));
#51962=CARTESIAN_POINT('Ctrl Pts',(-22.8364318467683,20.4075089764329,23.9205516490563));
#51963=CARTESIAN_POINT('Ctrl Pts',(-22.8521484465184,20.4039805002535,23.9195207298533));
#51964=CARTESIAN_POINT('Ctrl Pts',(-22.8975508445778,20.394144312824,23.9165372789906));
#51965=CARTESIAN_POINT('Ctrl Pts',(-22.927299567814,20.3881380346806,23.9145759066279));
#51966=CARTESIAN_POINT('Ctrl Pts',(-23.2082670368598,20.3355292846434,23.8959911274453));
#51967=CARTESIAN_POINT('Ctrl Pts',(-23.4640869132482,20.3185436469362,23.8785127485977));
#51968=CARTESIAN_POINT('Ctrl Pts',(-23.7879343040884,20.3355416915318,23.8567171755437));
#51969=CARTESIAN_POINT('Ctrl Pts',(-23.8565637541417,20.3413535308889,23.8521242672328));
#51970=CARTESIAN_POINT('Ctrl Pts',(-23.9919860830327,20.3572064253177,23.8431721891027));
#51971=CARTESIAN_POINT('Ctrl Pts',(-24.0587576333294,20.3671571698106,23.8388123171702));
#51972=CARTESIAN_POINT('Ctrl Pts',(-24.1322871931553,20.3804882668886,23.834106666341));
#51973=CARTESIAN_POINT('Ctrl Pts',(-24.1393973572563,20.3818020873211,23.8336526369049));
#51974=CARTESIAN_POINT('Ctrl Pts',(-24.1502194975346,20.3838394974567,23.8329631572826));
#51975=CARTESIAN_POINT('Ctrl Pts',(-24.1539346640711,20.3845456995818,23.8327267481913));
#51976=CARTESIAN_POINT('Ctrl Pts',(-24.1600060322178,20.3857108597834,23.8323408806923));
#51977=CARTESIAN_POINT('Ctrl Pts',(-24.1623629662189,20.3861659114043,23.8321912021973));
#51978=CARTESIAN_POINT('Ctrl Pts',(-24.1668293928583,20.3870334187009,23.8319077840035));
#51979=CARTESIAN_POINT('Ctrl Pts',(-24.1689389837203,20.3874453518819,23.8317740145482));
#51980=CARTESIAN_POINT('Ctrl Pts',(-24.1728438980564,20.3882119086248,23.831526581589));
#51981=CARTESIAN_POINT('Ctrl Pts',(-24.1746393272552,20.3885659499798,23.8314128850436));
#51982=CARTESIAN_POINT('Ctrl Pts',(-24.1782688065368,20.3892848605778,23.8311831879552));
#51983=CARTESIAN_POINT('Ctrl Pts',(-24.1801028336594,20.3896497954321,23.8310671917254));
#51984=CARTESIAN_POINT('Ctrl Pts',(-24.1852901459752,20.3906866616866,23.8307393148959));
#51985=CARTESIAN_POINT('Ctrl Pts',(-24.1886426935298,20.3913623373382,23.8305276498244));
#51986=CARTESIAN_POINT('Ctrl Pts',(-24.2026294356373,20.394204414728,23.8296455704051));
#51987=CARTESIAN_POINT('Ctrl Pts',(-24.2132538888759,20.3964192213056,23.8289779048477));
#51988=CARTESIAN_POINT('Ctrl Pts',(-24.406097133411,20.4376374831104,23.8168989428429));
#51989=CARTESIAN_POINT('Ctrl Pts',(-24.5846366945477,20.4923260876322,23.8063519688607));
#51990=CARTESIAN_POINT('Ctrl Pts',(-24.9130389012636,20.6250033620222,23.7865051127374));
#51991=CARTESIAN_POINT('Ctrl Pts',(-25.0634562250204,20.6999048394407,23.7772124034418));
#51992=CARTESIAN_POINT('Ctrl Pts',(-25.2830197201155,20.8315362892584,23.7625818756211));
#51993=CARTESIAN_POINT('Ctrl Pts',(-25.3567835329952,20.8799821174058,23.7574678848823));
#51994=CARTESIAN_POINT('Ctrl Pts',(-25.4797660129378,20.9681834011257,23.7485105406967));
#51995=CARTESIAN_POINT('Ctrl Pts',(-25.5299733442888,21.0064742525585,23.74472164056));
#51996=CARTESIAN_POINT('Ctrl Pts',(-25.5855362037797,21.0514911904804,23.740362577383));
#51997=CARTESIAN_POINT('Ctrl Pts',(-25.5920303696722,21.056794867235,23.7398504523469));
#51998=CARTESIAN_POINT('Ctrl Pts',(-25.601759934384,21.0648043372006,23.7390791756531));
#51999=CARTESIAN_POINT('Ctrl Pts',(-25.6050108749186,21.0674912661906,23.7388207915778));
#52000=CARTESIAN_POINT('Ctrl Pts',(-25.6105951664282,21.0721252094221,23.7383757817806));
#52001=CARTESIAN_POINT('Ctrl Pts',(-25.6129310608601,21.0740691614432,23.7381892812769));
#52002=CARTESIAN_POINT('Ctrl Pts',(-25.6177380816398,21.0780811285662,23.7378047509909));
#52003=CARTESIAN_POINT('Ctrl Pts',(-25.6202088624547,21.0801495511901,23.7376067046239));
#52004=CARTESIAN_POINT('Ctrl Pts',(-25.6261529768523,21.0851408685647,23.7371292846229));
#52005=CARTESIAN_POINT('Ctrl Pts',(-25.6296232381547,21.0880673975723,23.7368497618239));
#52006=CARTESIAN_POINT('Ctrl Pts',(-25.640265349037,21.0970806116783,23.7359900961001));
#52007=CARTESIAN_POINT('Ctrl Pts',(-25.6474166942058,21.1031913313406,23.7354089624116));
#52008=CARTESIAN_POINT('Ctrl Pts',(-25.7312437946933,21.1754577149339,23.7285559719345));
#52009=CARTESIAN_POINT('Ctrl Pts',(-25.8047791752259,21.245154007265,23.7221359461539));
#52010=CARTESIAN_POINT('Ctrl Pts',(-26.0445149325752,21.4948345416373,23.699715663462));
#52011=CARTESIAN_POINT('Ctrl Pts',(-26.1934186683054,21.6902178902584,23.6830417012337));
#52012=CARTESIAN_POINT('Ctrl Pts',(-26.3564504928827,21.9638110536724,23.6615584173974));
#52013=CARTESIAN_POINT('Ctrl Pts',(-26.3919787330574,22.0283666292493,23.6566172964087));
#52014=CARTESIAN_POINT('Ctrl Pts',(-26.4540121568934,22.1508435559601,23.6475420414925));
#52015=CARTESIAN_POINT('Ctrl Pts',(-26.4810746203063,22.2084446127116,23.6433917371907));
#52016=CARTESIAN_POINT('Ctrl Pts',(-26.5175866582589,22.2925432732204,23.6375371242707));
#52017=CARTESIAN_POINT('Ctrl Pts',(-26.5284216876515,22.3184193418411,23.635763045413));
#52018=CARTESIAN_POINT('Ctrl Pts',(-26.5405756839597,22.3485434827571,23.6337319238414));
#52019=CARTESIAN_POINT('Ctrl Pts',(-26.5422249889197,22.3526557677388,23.6334553859522));
#52020=CARTESIAN_POINT('Ctrl Pts',(-26.5447169420629,22.358906343708,23.6330361818604));
#52021=CARTESIAN_POINT('Ctrl Pts',(-26.545565783641,22.3610421350927,23.632893141357));
#52022=CARTESIAN_POINT('Ctrl Pts',(-26.5470993477564,22.3649128325947,23.6326342725226));
#52023=CARTESIAN_POINT('Ctrl Pts',(-26.5477848468397,22.3666474197936,23.632518397177));
#52024=CARTESIAN_POINT('Ctrl Pts',(-26.5492637708638,22.3703992152115,23.6322680527949));
#52025=CARTESIAN_POINT('Ctrl Pts',(-26.5500566643844,22.3724166234955,23.6321336164919));
#52026=CARTESIAN_POINT('Ctrl Pts',(-26.5522065531198,22.3779029717671,23.6317684973335));
#52027=CARTESIAN_POINT('Ctrl Pts',(-26.5535595758579,22.3813734805415,23.6315380553496));
#52028=CARTESIAN_POINT('Ctrl Pts',(-26.5599541403618,22.3978599677737,23.6304457930726));
#52029=CARTESIAN_POINT('Ctrl Pts',(-26.5649172029267,22.4109065213433,23.6295886497327));
#52030=CARTESIAN_POINT('Ctrl Pts',(-26.6506865970382,22.6408558026825,23.6146009360132));
#52031=CARTESIAN_POINT('Ctrl Pts',(-26.7079927262532,22.8658494421183,23.60177480645));
#52032=CARTESIAN_POINT('Ctrl Pts',(-26.7621191517465,23.245232674654,23.580360255278));
#52033=CARTESIAN_POINT('Ctrl Pts',(-26.7729136765701,23.396710145265,23.5718685391151));
#52034=CARTESIAN_POINT('Ctrl Pts',(-26.7730337244058,23.6028861875044,23.5599467049804));
#52035=CARTESIAN_POINT('Ctrl Pts',(-26.7716824729589,23.6573860561336,23.5567621264744));
#52036=CARTESIAN_POINT('Ctrl Pts',(-26.7684163199079,23.7224519651731,23.5529079856937));
#52037=CARTESIAN_POINT('Ctrl Pts',(-26.7678301562474,23.7330776909892,23.5522769197587));
#52038=CARTESIAN_POINT('Ctrl Pts',(-26.7640140907488,23.7965369586755,23.5484977530617));
#52039=CARTESIAN_POINT('Ctrl Pts',(-26.7595357163768,23.8492848328829,23.5453136282492));
#52040=CARTESIAN_POINT('Ctrl Pts',(-26.7528078681871,23.910576174877,23.5415560497455));
#52041=CARTESIAN_POINT('Ctrl Pts',(-26.7518198229835,23.9192521090897,23.5410228087823));
#52042=CARTESIAN_POINT('Ctrl Pts',(-26.7502940335703,23.9321822837499,23.5402260493789));
#52043=CARTESIAN_POINT('Ctrl Pts',(-26.749783032834,23.9364396899857,23.5399633766331));
#52044=CARTESIAN_POINT('Ctrl Pts',(-26.7488561600969,23.9440338129979,23.5394942408712));
#52045=CARTESIAN_POINT('Ctrl Pts',(-26.7484435590836,23.9473709288078,23.5392878816092));
#52046=CARTESIAN_POINT('Ctrl Pts',(-26.7475623473083,23.9544077155919,23.5388523084232));
#52047=CARTESIAN_POINT('Ctrl Pts',(-26.7470925363722,23.9581072288567,23.5386230567963));
#52048=CARTESIAN_POINT('Ctrl Pts',(-26.7458338894795,23.9678826154407,23.5380166199728));
#52049=CARTESIAN_POINT('Ctrl Pts',(-26.7450341492029,23.9739570474523,23.5376390899753));
#52050=CARTESIAN_POINT('Ctrl Pts',(-26.7413299466234,24.0014855165775,23.5359250187717));
#52051=CARTESIAN_POINT('Ctrl Pts',(-26.7382267197819,24.0229118317863,23.5345821927953));
#52052=CARTESIAN_POINT('Ctrl Pts',(-26.7138403689159,24.1801059625506,23.5246646377594));
#52053=CARTESIAN_POINT('Ctrl Pts',(-26.6841112165263,24.3144018043241,23.5158204466399));
#52054=CARTESIAN_POINT('Ctrl Pts',(-26.5987161015817,24.6093987748373,23.495558382615));
#52055=CARTESIAN_POINT('Ctrl Pts',(-26.5387238363553,24.7684282110944,23.4840491819084));
#52056=CARTESIAN_POINT('Ctrl Pts',(-26.4120338920182,25.0377663994039,23.4639181694639));
#52057=CARTESIAN_POINT('Ctrl Pts',(-26.350719678137,25.1502146047646,23.4553054722273));
#52058=CARTESIAN_POINT('Ctrl Pts',(-26.2807743243951,25.262088982482,23.4467060406426));
#52059=CARTESIAN_POINT('Ctrl Pts',(-26.2786654153686,25.2654482730443,23.4464477975108));
#52060=CARTESIAN_POINT('Ctrl Pts',(-26.2749494112357,25.271343316555,23.4459945872238));
#52061=CARTESIAN_POINT('Ctrl Pts',(-26.2733449685139,25.2738807270362,23.4457995006479));
#52062=CARTESIAN_POINT('Ctrl Pts',(-26.2434950715683,25.3209423387497,23.4421810616369));
#52063=CARTESIAN_POINT('Ctrl Pts',(-26.2141625571307,25.3647722906092,23.4388085414191));
#52064=CARTESIAN_POINT('Ctrl Pts',(-26.1804541774281,25.412560204773,23.4351458251695));
#52065=CARTESIAN_POINT('Ctrl Pts',(-26.1771302012833,25.4172459105409,23.4347868452795));
#52066=CARTESIAN_POINT('Ctrl Pts',(-26.1724575334191,25.4237956415432,23.4342853088049));
#52067=CARTESIAN_POINT('Ctrl Pts',(-26.1711193736686,25.4256671131279,23.4341420321235));
#52068=CARTESIAN_POINT('Ctrl Pts',(-26.1686677119342,25.429088114516,23.4338801809408));
#52069=CARTESIAN_POINT('Ctrl Pts',(-26.1675548363527,25.4306380904229,23.4337615629291));
#52070=CARTESIAN_POINT('Ctrl Pts',(-26.1652920937829,25.4337836621232,23.4335208791497));
#52071=CARTESIAN_POINT('Ctrl Pts',(-26.1641421423972,25.4353791942007,23.4333988195092));
#52072=CARTESIAN_POINT('Ctrl Pts',(-26.161281865988,25.4393401152093,23.4330958591404));
#52073=CARTESIAN_POINT('Ctrl Pts',(-26.1595697821979,25.4417042411277,23.4329150810102));
#52074=CARTESIAN_POINT('Ctrl Pts',(-26.1531645303461,25.4505236666209,23.4322408486565));
#52075=CARTESIAN_POINT('Ctrl Pts',(-26.1484505492332,25.4569639214481,23.431748830262));
#52076=CARTESIAN_POINT('Ctrl Pts',(-26.0676479113083,25.5665006300306,23.423384906643));
#52077=CARTESIAN_POINT('Ctrl Pts',(-25.9854905246638,25.6650008999539,23.415928755296));
#52078=CARTESIAN_POINT('Ctrl Pts',(-25.7809629251301,25.8824328170575,23.3989388119674));
#52079=CARTESIAN_POINT('Ctrl Pts',(-25.6545953285815,25.9970624735601,23.3895461567267));
#52080=CARTESIAN_POINT('Ctrl Pts',(-25.3587610343776,26.2254692212081,23.3685210633742));
#52081=CARTESIAN_POINT('Ctrl Pts',(-25.1863876927914,26.3342299611382,23.3568378700138));
#52082=CARTESIAN_POINT('Ctrl Pts',(-24.9930187205028,26.4320439080216,23.3436762714391));
#52083=CARTESIAN_POINT('Ctrl Pts',(-24.9810679790176,26.4379961074888,23.3428628169562));
#52084=CARTESIAN_POINT('Ctrl Pts',(-24.9648306322879,26.4459577594516,23.3417574249243));
#52085=CARTESIAN_POINT('Ctrl Pts',(-24.9605759600465,26.4480323362677,23.3414677643208));
#52086=CARTESIAN_POINT('Ctrl Pts',(-24.9533693527638,26.4515266446439,23.3409771033074));
#52087=CARTESIAN_POINT('Ctrl Pts',(-24.9504197860793,26.4529512676414,23.340776273665));
#52088=CARTESIAN_POINT('Ctrl Pts',(-24.9447437487876,26.4556820950769,23.3403897855184));
#52089=CARTESIAN_POINT('Ctrl Pts',(-24.942017601317,26.4569889650862,23.3402041504798));
#52090=CARTESIAN_POINT('Ctrl Pts',(-24.9356691372612,26.4600213352388,23.3397718348371));
#52091=CARTESIAN_POINT('Ctrl Pts',(-24.9320454350061,26.4617439078086,23.3395250528141));
#52092=CARTESIAN_POINT('Ctrl Pts',(-24.9216296197132,26.4666713715025,23.3388156606069));
#52093=CARTESIAN_POINT('Ctrl Pts',(-24.9148295417498,26.4698592772731,23.338352462181));
#52094=CARTESIAN_POINT('Ctrl Pts',(-24.8995137383653,26.4769741955195,23.3373090302286));
#52095=CARTESIAN_POINT('Ctrl Pts',(-24.8909919178829,26.4808878547364,23.3367283389426));
#52096=CARTESIAN_POINT('Ctrl Pts',(-24.8210116240697,26.5126572952353,23.3319586195421));
#52097=CARTESIAN_POINT('Ctrl Pts',(-24.758713284732,26.538611973336,23.3277047335592));
#52098=CARTESIAN_POINT('Ctrl Pts',(-24.579411373383,26.6067888874818,23.3154279353687));
#52099=CARTESIAN_POINT('Ctrl Pts',(-24.4607245844803,26.6442171624869,23.3072573148523));
#52100=CARTESIAN_POINT('Ctrl Pts',(-24.049573260902,26.7481657449141,23.2789171562144));
#52101=CARTESIAN_POINT('Ctrl Pts',(-23.7501395105374,26.7807356974758,23.258080567559));
#52102=CARTESIAN_POINT('Ctrl Pts',(-23.4344913771458,26.7709627075555,23.2380978145809));
#52103=CARTESIAN_POINT('Ctrl Pts',(-23.4184676449365,26.7703468549784,23.2370892152386));
#52104=CARTESIAN_POINT('Ctrl Pts',(-23.3988804525591,26.7694475888472,23.2358639784014));
#52105=CARTESIAN_POINT('Ctrl Pts',(-23.3953123729465,26.7692778298011,23.2356410954923));
#52106=CARTESIAN_POINT('Ctrl Pts',(-23.3894265749547,26.7689879915044,23.2352739558622));
#52107=CARTESIAN_POINT('Ctrl Pts',(-23.3871087037833,26.7688713410729,23.235129506952));
#52108=CARTESIAN_POINT('Ctrl Pts',(-23.3829268239884,26.7686563525653,23.2348691368994));
#52109=CARTESIAN_POINT('Ctrl Pts',(-23.3810627794657,26.7685588990956,23.2347531660722));
#52110=CARTESIAN_POINT('Ctrl Pts',(-23.3770513672059,26.7683456850442,23.2345037859032));
#52111=CARTESIAN_POINT('Ctrl Pts',(-23.3749040363296,26.7682293949201,23.234370407178));
#52112=CARTESIAN_POINT('Ctrl Pts',(-23.369015418782,26.7679045812555,23.2340049569704));
#52113=CARTESIAN_POINT('Ctrl Pts',(-23.3652743618624,26.7676916811059,23.2337731327197));
#52114=CARTESIAN_POINT('Ctrl Pts',(-23.3457357164493,26.7665455638401,23.2325641452823));
#52115=CARTESIAN_POINT('Ctrl Pts',(-23.3299444289777,26.765502500269,23.2315930943731));
#52116=CARTESIAN_POINT('Ctrl Pts',(-23.1721618368714,26.7539125593274,23.2219455239268));
#52117=CARTESIAN_POINT('Ctrl Pts',(-23.0309897994891,26.7340815556433,23.2137557014296));
#52118=CARTESIAN_POINT('Ctrl Pts',(-22.6073671109249,26.6456330650418,23.189312105101));
#52119=CARTESIAN_POINT('Ctrl Pts',(-22.3327375190274,26.5482166443642,23.1735174004987));
#52120=CARTESIAN_POINT('Ctrl Pts',(-22.0750359362473,26.4155367338316,23.1563971075561));
#52121=CARTESIAN_POINT('',(-26.7730015390511,23.5527819743835,23.3126472226381));
#52122=CARTESIAN_POINT('Ctrl Pts',(-22.0750361284943,26.4155368328116,22.9065074728514));
#52123=CARTESIAN_POINT('Ctrl Pts',(-22.16486243135,26.4617846817109,22.9121756008112));
#52124=CARTESIAN_POINT('Ctrl Pts',(-22.2568402343458,26.503796477144,22.9178886654819));
#52125=CARTESIAN_POINT('Ctrl Pts',(-22.4634598636861,26.5866595062593,22.930728433918));
#52126=CARTESIAN_POINT('Ctrl Pts',(-22.5787072220492,26.6254728442691,22.9378960149764));
#52127=CARTESIAN_POINT('Ctrl Pts',(-22.7061805969438,26.6605217590922,22.9459399633442));
#52128=CARTESIAN_POINT('Ctrl Pts',(-22.7165137408078,26.6633075781343,22.94659278619));
#52129=CARTESIAN_POINT('Ctrl Pts',(-22.731026096484,26.6671426764694,22.9475107827341));
#52130=CARTESIAN_POINT('Ctrl Pts',(-22.7351939080936,26.668235143343,22.9477745543495));
#52131=CARTESIAN_POINT('Ctrl Pts',(-22.7424234913705,26.6701146757686,22.9482323315499));
#52132=CARTESIAN_POINT('Ctrl Pts',(-22.7454842612207,26.670905602311,22.9484262117402));
#52133=CARTESIAN_POINT('Ctrl Pts',(-22.7518487756404,26.6725402556949,22.9488295152566));
#52134=CARTESIAN_POINT('Ctrl Pts',(-22.755152703572,26.673383244986,22.9490389621639));
#52135=CARTESIAN_POINT('Ctrl Pts',(-22.7617100578641,26.6750452584321,22.9494548258914));
#52136=CARTESIAN_POINT('Ctrl Pts',(-22.7649634377647,26.6758644488918,22.9496612370104));
#52137=CARTESIAN_POINT('Ctrl Pts',(-22.7758569297536,26.6785893129885,22.9503526595473));
#52138=CARTESIAN_POINT('Ctrl Pts',(-22.7835027006515,26.6804720544012,22.9508384119548));
#52139=CARTESIAN_POINT('Ctrl Pts',(-22.8397413044736,26.6941021822103,22.9544148994032));
#52140=CARTESIAN_POINT('Ctrl Pts',(-22.8885924204813,26.7047449270611,22.9575410713065));
#52141=CARTESIAN_POINT('Ctrl Pts',(-23.0486486025913,26.7357335275974,22.9678547127887));
#52142=CARTESIAN_POINT('Ctrl Pts',(-23.160669796055,26.7513642361478,22.9751874512787));
#52143=CARTESIAN_POINT('Ctrl Pts',(-23.3562780135944,26.7682383857494,22.9881710696797));
#52144=CARTESIAN_POINT('Ctrl Pts',(-23.439527952971,26.7721770962261,22.993751550224));
#52145=CARTESIAN_POINT('Ctrl Pts',(-23.7778558200211,26.7750557104828,23.0165633111645));
#52146=CARTESIAN_POINT('Ctrl Pts',(-24.0322509006624,26.7469471236772,23.0340964832569));
#52147=CARTESIAN_POINT('Ctrl Pts',(-24.2840444306947,26.6883536956621,23.0504393210503));
#52148=CARTESIAN_POINT('Ctrl Pts',(-24.2874035980655,26.6875663145234,23.0506571495124));
#52149=CARTESIAN_POINT('Ctrl Pts',(-24.3024872406425,26.6840051801437,23.0516343411892));
#52150=CARTESIAN_POINT('Ctrl Pts',(-24.3141975750192,26.6811710392117,23.0523904906597));
#52151=CARTESIAN_POINT('Ctrl Pts',(-24.3293505191172,26.677413638132,23.0533654389536));
#52152=CARTESIAN_POINT('Ctrl Pts',(-24.3328076750557,26.6765502954261,23.0535876379502));
#52153=CARTESIAN_POINT('Ctrl Pts',(-24.3381050207881,26.6752180713369,23.0539277401309));
#52154=CARTESIAN_POINT('Ctrl Pts',(-24.339946225556,26.6747532979678,23.0540458813019));
#52155=CARTESIAN_POINT('Ctrl Pts',(-24.3435767155369,26.6738334431553,23.0542786955077));
#52156=CARTESIAN_POINT('Ctrl Pts',(-24.3453660111084,26.6733784539079,23.0543933727857));
#52157=CARTESIAN_POINT('Ctrl Pts',(-24.3493515075746,26.6723613588228,23.054648660191));
#52158=CARTESIAN_POINT('Ctrl Pts',(-24.3515475015713,26.6717984744945,23.0547892240513));
#52159=CARTESIAN_POINT('Ctrl Pts',(-24.3578898036611,26.6701656612485,23.0551949098688));
#52160=CARTESIAN_POINT('Ctrl Pts',(-24.3620345959232,26.66908977973,23.0554596859208));
#52161=CARTESIAN_POINT('Ctrl Pts',(-24.3900264793534,26.6617642253519,23.0572455908411));
#52162=CARTESIAN_POINT('Ctrl Pts',(-24.413804170551,26.6552491434057,23.0587515262944));
#52163=CARTESIAN_POINT('Ctrl Pts',(-24.4871265250587,26.6342513722177,23.0633675489862));
#52164=CARTESIAN_POINT('Ctrl Pts',(-24.5364019439207,26.6188502101736,23.066430245394));
#52165=CARTESIAN_POINT('Ctrl Pts',(-24.7188282838925,26.5569836408599,23.0776938290128));
#52166=CARTESIAN_POINT('Ctrl Pts',(-24.8492622942659,26.5029768943138,23.0856005256094));
#52167=CARTESIAN_POINT('Ctrl Pts',(-25.0331190976727,26.4123001257836,23.0970622360891));
#52168=CARTESIAN_POINT('Ctrl Pts',(-25.0896353729596,26.382303043671,23.1006308854553));
#52169=CARTESIAN_POINT('Ctrl Pts',(-25.2166588277112,26.3099565791244,23.1088236462832));
#52170=CARTESIAN_POINT('Ctrl Pts',(-25.2865111857637,26.2665517522373,23.1134558703007));
#52171=CARTESIAN_POINT('Ctrl Pts',(-25.4073953590702,26.1848671586225,23.1217943080966));
#52172=CARTESIAN_POINT('Ctrl Pts',(-25.4590943008135,26.147654342409,23.1254719169986));
#52173=CARTESIAN_POINT('Ctrl Pts',(-25.526167127659,26.0962909478847,23.1304189774858));
#52174=CARTESIAN_POINT('Ctrl Pts',(-25.5425562905233,26.0834867910561,23.1316422022653));
#52175=CARTESIAN_POINT('Ctrl Pts',(-25.6098745947229,26.0298364970527,23.1367289408539));
#52176=CARTESIAN_POINT('Ctrl Pts',(-25.6596778609204,25.9876083818812,23.1406422195937));
#52177=CARTESIAN_POINT('Ctrl Pts',(-25.71437272165,25.938300121158,23.1451280259904));
#52178=CARTESIAN_POINT('Ctrl Pts',(-25.7205616286409,25.9326769077774,23.1456384140811));
#52179=CARTESIAN_POINT('Ctrl Pts',(-25.7298832660995,25.9241408445732,23.146411437476));
#52180=CARTESIAN_POINT('Ctrl Pts',(-25.7330322302026,25.9212457092213,23.1466733187197));
#52181=CARTESIAN_POINT('Ctrl Pts',(-25.7384925288226,25.9162054520383,23.1471287204361));
#52182=CARTESIAN_POINT('Ctrl Pts',(-25.7408065019421,25.914063186049,23.1473221186728));
#52183=CARTESIAN_POINT('Ctrl Pts',(-25.7456202204641,25.9095935284785,23.1477252937206));
#52184=CARTESIAN_POINT('Ctrl Pts',(-25.7481194162172,25.9072655536732,23.147935095414));
#52185=CARTESIAN_POINT('Ctrl Pts',(-25.7530736494305,25.9026360060083,23.1483519495873));
#52186=CARTESIAN_POINT('Ctrl Pts',(-25.7555287921281,25.9003345519652,23.1485589968027));
#52187=CARTESIAN_POINT('Ctrl Pts',(-25.7612413370506,25.8949627702342,23.1490418446381));
#52188=CARTESIAN_POINT('Ctrl Pts',(-25.7644959501454,25.8918894983581,23.1493177723483));
#52189=CARTESIAN_POINT('Ctrl Pts',(-25.7829183069544,25.8744208530877,23.1508843851844));
#52190=CARTESIAN_POINT('Ctrl Pts',(-25.7979517762224,25.8598851698296,23.1521811543268));
#52191=CARTESIAN_POINT('Ctrl Pts',(-25.8859572903002,25.7731206569214,23.1598831617822));
#52192=CARTESIAN_POINT('Ctrl Pts',(-25.9555781207076,25.6975914440227,23.1664351755683));
#52193=CARTESIAN_POINT('Ctrl Pts',(-26.0645119790878,25.5674568890809,23.1774925544216));
#52194=CARTESIAN_POINT('Ctrl Pts',(-26.1059360892757,25.5147103901443,23.1819162875233));
#52195=CARTESIAN_POINT('Ctrl Pts',(-26.3313749991614,25.2084433406552,23.2072436915733));
#52196=CARTESIAN_POINT('Ctrl Pts',(-26.4792894316959,24.9304628184962,23.2290824280089));
#52197=CARTESIAN_POINT('Ctrl Pts',(-26.5895313036946,24.6222141476893,23.2497945203404));
#52198=CARTESIAN_POINT('Ctrl Pts',(-26.5942014665338,24.6088799730136,23.2506836771023));
#52199=CARTESIAN_POINT('Ctrl Pts',(-26.6004108189609,24.5907702618418,23.2518816654788));
#52200=CARTESIAN_POINT('Ctrl Pts',(-26.6020266793993,24.5860214616891,23.2521949144694));
#52201=CARTESIAN_POINT('Ctrl Pts',(-26.6044048770155,24.5789783739944,23.2526581616786));
#52202=CARTESIAN_POINT('Ctrl Pts',(-26.6051757207206,24.5766869992998,23.2528086628511));
#52203=CARTESIAN_POINT('Ctrl Pts',(-26.6065402190788,24.5726158010817,23.2530756898644));
#52204=CARTESIAN_POINT('Ctrl Pts',(-26.6071348975369,24.5708363274313,23.2531922767807));
#52205=CARTESIAN_POINT('Ctrl Pts',(-26.6083884109482,24.5670744779233,23.2534384741102));
#52206=CARTESIAN_POINT('Ctrl Pts',(-26.6090468708566,24.5650919855395,23.2535680618269));
#52207=CARTESIAN_POINT('Ctrl Pts',(-26.6107943509794,24.5598135176032,23.2539126772276));
#52208=CARTESIAN_POINT('Ctrl Pts',(-26.6118799783023,24.5565164087705,23.254127502904));
#52209=CARTESIAN_POINT('Ctrl Pts',(-26.6168965153639,24.5411976420071,23.2551236286644));
#52210=CARTESIAN_POINT('Ctrl Pts',(-26.6207620311532,24.5291544473418,23.2559010967138));
#52211=CARTESIAN_POINT('Ctrl Pts',(-26.7131163522605,24.2354901084055,23.2747287003191));
#52212=CARTESIAN_POINT('Ctrl Pts',(-26.7625838218202,23.9430043432626,23.2906579280122));
#52213=CARTESIAN_POINT('Ctrl Pts',(-26.7724844617027,23.6161547217701,23.3090613006868));
#52214=CARTESIAN_POINT('Ctrl Pts',(-26.7729766687258,23.5844691188605,23.3108502788934));
#52215=CARTESIAN_POINT('Ctrl Pts',(-26.7730015390511,23.5527819743835,23.3126472226381));
#52216=CARTESIAN_POINT('Ctrl Pts',(-26.7730015419314,23.5527783018455,23.3126474309038));
#52217=CARTESIAN_POINT('Ctrl Pts',(-26.7731347774501,23.3827768328784,23.3222880338827));
#52218=CARTESIAN_POINT('Ctrl Pts',(-26.7598169813681,23.2130497545595,23.332159750487));
#52219=CARTESIAN_POINT('Ctrl Pts',(-26.7317837701308,23.0363890775716,23.3430267767076));
#52220=CARTESIAN_POINT('Ctrl Pts',(-26.7303534844098,23.0276105905061,23.3435682729724));
#52221=CARTESIAN_POINT('Ctrl Pts',(-26.7280309523797,23.0137184544939,23.3444276207531));
#52222=CARTESIAN_POINT('Ctrl Pts',(-26.7271626518509,23.0086008032555,23.3447447119607));
#52223=CARTESIAN_POINT('Ctrl Pts',(-26.7256636102518,22.9998932583048,23.34528512884));
#52224=CARTESIAN_POINT('Ctrl Pts',(-26.7250391341262,22.9963022844,23.3455082549574));
#52225=CARTESIAN_POINT('Ctrl Pts',(-26.7238659845492,22.9896233755115,23.3459237362949));
#52226=CARTESIAN_POINT('Ctrl Pts',(-26.723318892227,22.9865351641692,23.3461160409375));
#52227=CARTESIAN_POINT('Ctrl Pts',(-26.7221753701466,22.9801346522211,23.3465150072844));
#52228=CARTESIAN_POINT('Ctrl Pts',(-26.7215782582394,22.9768224787617,23.3467216905264));
#52229=CARTESIAN_POINT('Ctrl Pts',(-26.7202043038506,22.9692689542262,23.3471935522447));
#52230=CARTESIAN_POINT('Ctrl Pts',(-26.7194241365904,22.9650282212664,23.3474588365537));
#52231=CARTESIAN_POINT('Ctrl Pts',(-26.717070682939,22.95237834043,23.3482512761457));
#52232=CARTESIAN_POINT('Ctrl Pts',(-26.7154724298395,22.9439739276224,23.3487792282389));
#52233=CARTESIAN_POINT('Ctrl Pts',(-26.7085800061031,22.9085003234153,23.3510138951074));
#52234=CARTESIAN_POINT('Ctrl Pts',(-26.7029720296144,22.8814939627236,23.352730622724));
#52235=CARTESIAN_POINT('Ctrl Pts',(-26.6956565670161,22.848404395219,23.3548536603124));
#52236=CARTESIAN_POINT('Ctrl Pts',(-26.6942768204619,22.842249266999,23.355249412015));
#52237=CARTESIAN_POINT('Ctrl Pts',(-26.6914492003773,22.829806361898,23.3560511463732));
#52238=CARTESIAN_POINT('Ctrl Pts',(-26.6900004967742,22.8235188048581,23.3564571538825));
#52239=CARTESIAN_POINT('Ctrl Pts',(-26.6874628508522,22.812654328269,23.3571602389735));
#52240=CARTESIAN_POINT('Ctrl Pts',(-26.6863827463318,22.8080753474668,23.3574570348753));
#52241=CARTESIAN_POINT('Ctrl Pts',(-26.6821369703648,22.7902506259615,23.3586142215895));
#52242=CARTESIAN_POINT('Ctrl Pts',(-26.6788974116509,22.7770227857997,23.3594769418447));
#52243=CARTESIAN_POINT('Ctrl Pts',(-26.673552638265,22.7557825001647,23.3608686612183));
#52244=CARTESIAN_POINT('Ctrl Pts',(-26.6715001768699,22.7477568481155,23.3613960038698));
#52245=CARTESIAN_POINT('Ctrl Pts',(-26.6653133948758,22.7239477508347,23.3629648445309));
#52246=CARTESIAN_POINT('Ctrl Pts',(-26.6610901767673,22.7081878650457,23.3640090746905));
#52247=CARTESIAN_POINT('Ctrl Pts',(-26.6486937537505,22.6632941787523,23.3670002166191));
#52248=CARTESIAN_POINT('Ctrl Pts',(-26.6402298238597,22.6342430519495,23.3689558027433));
#52249=CARTESIAN_POINT('Ctrl Pts',(-26.6171216119529,22.5588952877054,23.3740797923215));
#52250=CARTESIAN_POINT('Ctrl Pts',(-26.6018382137583,22.5128039213031,23.3772658662748));
#52251=CARTESIAN_POINT('Ctrl Pts',(-26.5788097365262,22.4482736689212,23.3817971389169));
#52252=CARTESIAN_POINT('Ctrl Pts',(-26.5719250045436,22.4295332969381,23.3831215828238));
#52253=CARTESIAN_POINT('Ctrl Pts',(-26.505686457019,22.2542790569056,23.3955853758218));
#52254=CARTESIAN_POINT('Ctrl Pts',(-26.4343989368746,22.1025539560604,23.4069810383859));
#52255=CARTESIAN_POINT('Ctrl Pts',(-26.2715837909986,21.8162660860202,23.4291944643353));
#52256=CARTESIAN_POINT('Ctrl Pts',(-26.1809985326333,21.6816853966507,23.4399837514184));
#52257=CARTESIAN_POINT('Ctrl Pts',(-26.076854025858,21.5496425501844,23.4505216025554));
#52258=CARTESIAN_POINT('Ctrl Pts',(-26.0730304233628,21.544823121512,23.4509061385287));
#52259=CARTESIAN_POINT('Ctrl Pts',(-26.067553470687,21.5379601936359,23.4514535650238));
#52260=CARTESIAN_POINT('Ctrl Pts',(-26.0659114148823,21.5359077611007,23.4516172586076));
#52261=CARTESIAN_POINT('Ctrl Pts',(-26.0630725444527,21.5323682957789,23.4518995134574));
#52262=CARTESIAN_POINT('Ctrl Pts',(-26.0618769180231,21.5308803153493,23.4520181607812));
#52263=CARTESIAN_POINT('Ctrl Pts',(-26.0595758186541,21.5280217573925,23.4522460701185));
#52264=CARTESIAN_POINT('Ctrl Pts',(-26.0584705465304,21.5266510261847,23.4523553463859));
#52265=CARTESIAN_POINT('Ctrl Pts',(-26.0558532241869,21.523410526361,23.4526136598583));
#52266=CARTESIAN_POINT('Ctrl Pts',(-26.0543402010283,21.5215415396651,23.4527626263555));
#52267=CARTESIAN_POINT('Ctrl Pts',(-26.0498323169783,21.5159858283025,23.4532053932629));
#52268=CARTESIAN_POINT('Ctrl Pts',(-26.0468313790559,21.5123040085176,23.4534987560811));
#52269=CARTESIAN_POINT('Ctrl Pts',(-26.0193306965118,21.4787156104459,23.4561746041087));
#52270=CARTESIAN_POINT('Ctrl Pts',(-25.9943014801422,21.4492439016129,23.4585193456803));
#52271=CARTESIAN_POINT('Ctrl Pts',(-25.7888925638333,21.2160164049705,23.4771158766059));
#52272=CARTESIAN_POINT('Ctrl Pts',(-25.58387347536,21.035377384812,23.4918497832071));
#52273=CARTESIAN_POINT('Ctrl Pts',(-25.2848088565358,20.832648678494,23.5122093894683));
#52274=CARTESIAN_POINT('Ctrl Pts',(-25.2090189625916,20.7857364989744,23.5172777257283));
#52275=CARTESIAN_POINT('Ctrl Pts',(-25.0786805971855,20.7123512445099,23.5259442326767));
#52276=CARTESIAN_POINT('Ctrl Pts',(-25.0251525071944,20.6841671377927,23.5294897792611));
#52277=CARTESIAN_POINT('Ctrl Pts',(-24.9228930822792,20.6339480478768,23.5362636539576));
#52278=CARTESIAN_POINT('Ctrl Pts',(-24.8743445586016,20.6115872374527,23.5394797628008));
#52279=CARTESIAN_POINT('Ctrl Pts',(-24.8178844524073,20.5872656181398,23.5432279750036));
#52280=CARTESIAN_POINT('Ctrl Pts',(-24.8104924927464,20.5841140698167,23.5437188552156));
#52281=CARTESIAN_POINT('Ctrl Pts',(-24.799989186852,20.579682355138,23.5444165909233));
#52282=CARTESIAN_POINT('Ctrl Pts',(-24.7968874611815,20.578379345716,23.544622668393));
#52283=CARTESIAN_POINT('Ctrl Pts',(-24.7906331856786,20.5757634902144,23.5450382620369));
#52284=CARTESIAN_POINT('Ctrl Pts',(-24.7874805784183,20.5744507935207,23.5452477829605));
#52285=CARTESIAN_POINT('Ctrl Pts',(-24.781412261389,20.5719353507241,23.5456511440275));
#52286=CARTESIAN_POINT('Ctrl Pts',(-24.7784968591937,20.5707318685117,23.545844958891));
#52287=CARTESIAN_POINT('Ctrl Pts',(-24.7716209536145,20.5679052915997,23.5463021349591));
#52288=CARTESIAN_POINT('Ctrl Pts',(-24.7676589808756,20.5662858060453,23.5465656182724));
#52289=CARTESIAN_POINT('Ctrl Pts',(-24.755937820288,20.5615219249464,23.5473452760056));
#52290=CARTESIAN_POINT('Ctrl Pts',(-24.7481696373871,20.55839988482,23.547862206157));
#52291=CARTESIAN_POINT('Ctrl Pts',(-24.6794642475673,20.5310976013259,23.5524361974753));
#52292=CARTESIAN_POINT('Ctrl Pts',(-24.6178184471994,20.5087532980522,23.5565547133044));
#52293=CARTESIAN_POINT('Ctrl Pts',(-24.4944530175027,20.4682504971379,23.5648340144744));
#52294=CARTESIAN_POINT('Ctrl Pts',(-24.4327855324364,20.4500290390643,23.5689905725245));
#52295=CARTESIAN_POINT('Ctrl Pts',(-24.341211121178,20.4259243273271,23.5751872207995));
#52296=CARTESIAN_POINT('Ctrl Pts',(-24.3116972498808,20.4186005590658,23.5771879417176));
#52297=CARTESIAN_POINT('Ctrl Pts',(-24.1269003131287,20.3755105755429,23.5897339345976));
#52298=CARTESIAN_POINT('Ctrl Pts',(-23.9692549817492,20.3508870366001,23.6005343974073));
#52299=CARTESIAN_POINT('Ctrl Pts',(-23.7902861271128,20.3363902738309,23.612681391724));
#52300=CARTESIAN_POINT('Ctrl Pts',(-23.7701090261057,20.3349469679697,23.6140489804413));
#52301=CARTESIAN_POINT('Ctrl Pts',(-23.7259120492649,20.3322034519652,23.6170391689943));
#52302=CARTESIAN_POINT('Ctrl Pts',(-23.7018883572936,20.3309820021721,23.6186609989363));
#52303=CARTESIAN_POINT('Ctrl Pts',(-23.5933689287527,20.3266819474953,23.6259662012804));
#52304=CARTESIAN_POINT('Ctrl Pts',(-23.5087801657619,20.3266600955778,23.6316041235454));
#52305=CARTESIAN_POINT('Ctrl Pts',(-23.3860665938423,20.3314603176345,23.6396202134002));
#52306=CARTESIAN_POINT('Ctrl Pts',(-23.3478773246794,20.3336355363346,23.6420917550492));
#52307=CARTESIAN_POINT('Ctrl Pts',(-23.2833826691573,20.3384623261021,23.6462167992901));
#52308=CARTESIAN_POINT('Ctrl Pts',(-23.2570554628451,20.3407585781832,23.6478868361096));
#52309=CARTESIAN_POINT('Ctrl Pts',(-23.2264173098206,20.3438109925084,23.6498118728137));
#52310=CARTESIAN_POINT('Ctrl Pts',(-23.2220770116411,20.3442523096551,23.6500841472256));
#52311=CARTESIAN_POINT('Ctrl Pts',(-23.2154657382807,20.344938103699,23.6504982110415));
#52312=CARTESIAN_POINT('Ctrl Pts',(-23.2131941266648,20.3451761814281,23.6506403609315));
#52313=CARTESIAN_POINT('Ctrl Pts',(-23.2090686415916,20.3456129900398,23.6508982977542));
#52314=CARTESIAN_POINT('Ctrl Pts',(-23.2072146938266,20.3458109140884,23.6510141299973));
#52315=CARTESIAN_POINT('Ctrl Pts',(-23.2031940589487,20.3462436789276,23.651265156621));
#52316=CARTESIAN_POINT('Ctrl Pts',(-23.201027443981,20.3464791080123,23.6514003168471));
#52317=CARTESIAN_POINT('Ctrl Pts',(-23.195108462519,20.3471283530118,23.6517692609623));
#52318=CARTESIAN_POINT('Ctrl Pts',(-23.1913565666232,20.3475465663374,23.6520027954816));
#52319=CARTESIAN_POINT('Ctrl Pts',(-23.1732309428666,20.3495992298281,23.653129456525));
#52320=CARTESIAN_POINT('Ctrl Pts',(-23.1588672995124,20.3513238898273,23.6540175443053));
#52321=CARTESIAN_POINT('Ctrl Pts',(-22.8989446196282,20.3843100435371,23.6700103538845));
#52322=CARTESIAN_POINT('Ctrl Pts',(-22.657736849038,20.4436703441888,23.6836305656529));
#52323=CARTESIAN_POINT('Ctrl Pts',(-22.3252827499329,20.5674614776992,23.703470536442));
#52324=CARTESIAN_POINT('Ctrl Pts',(-22.2268208200252,20.6098239239812,23.7094847320403));
#52325=CARTESIAN_POINT('Ctrl Pts',(-22.0405370583965,20.7012258394838,23.7213625775057));
#52326=CARTESIAN_POINT('Ctrl Pts',(-21.9525416825125,20.7496256008681,23.7272050633022));
#52327=CARTESIAN_POINT('Ctrl Pts',(-21.8268398293974,20.8266191141364,23.7359972331346));
#52328=CARTESIAN_POINT('Ctrl Pts',(-21.7872707908356,20.8520632569423,23.7388330501406));
#52329=CARTESIAN_POINT('Ctrl Pts',(-21.7418213928554,20.8827152857721,23.7421760966142));
#52330=CARTESIAN_POINT('Ctrl Pts',(-21.7353843126754,20.8870905974095,23.7426516202695));
#52331=CARTESIAN_POINT('Ctrl Pts',(-21.7262098007181,20.8933752638041,23.7433323131262));
#52332=CARTESIAN_POINT('Ctrl Pts',(-21.7234593515955,20.8952656432011,23.7435367599973));
#52333=CARTESIAN_POINT('Ctrl Pts',(-21.7179126052756,20.8990906131201,23.7439498328076));
#52334=CARTESIAN_POINT('Ctrl Pts',(-21.715116423812,20.9010253632829,23.7441584646665));
#52335=CARTESIAN_POINT('Ctrl Pts',(-21.7097144998507,20.9047757500363,23.7445622899962));
#52336=CARTESIAN_POINT('Ctrl Pts',(-21.7071083677678,20.9065908211465,23.7447574616739));
#52337=CARTESIAN_POINT('Ctrl Pts',(-21.7009267472671,20.9109096667752,23.7452212292737));
#52338=CARTESIAN_POINT('Ctrl Pts',(-21.6973536606085,20.9134168544508,23.745489955989));
#52339=CARTESIAN_POINT('Ctrl Pts',(-21.6847686440322,20.9222858054068,23.7464387997708));
#52340=CARTESIAN_POINT('Ctrl Pts',(-21.6757843732346,20.9286865173327,23.7471204148647));
#52341=CARTESIAN_POINT('Ctrl Pts',(-21.5535299786202,21.0167346154464,23.756454298491));
#52342=CARTESIAN_POINT('Ctrl Pts',(-21.4456657828931,21.1056014229899,23.7653911747509));
#52343=CARTESIAN_POINT('Ctrl Pts',(-21.1534028885981,21.3801047661281,23.791746768356));
#52344=CARTESIAN_POINT('Ctrl Pts',(-20.9853920717037,21.5815229763983,23.8097444451733));
#52345=CARTESIAN_POINT('Ctrl Pts',(-20.818013299452,21.840515637433,23.8302651934157));
#52346=CARTESIAN_POINT('Ctrl Pts',(-20.7933415156972,21.8805898388672,23.8333709171742));
#52347=CARTESIAN_POINT('Ctrl Pts',(-20.7483236270243,21.9574323460465,23.839177392827));
#52348=CARTESIAN_POINT('Ctrl Pts',(-20.7278014726324,21.9940866891688,23.8418852827158));
#52349=CARTESIAN_POINT('Ctrl Pts',(-20.6981274285326,22.0496064428178,23.8458836531076));
#52350=CARTESIAN_POINT('Ctrl Pts',(-20.6884341524419,22.0681756415642,23.8472040005109));
#52351=CARTESIAN_POINT('Ctrl Pts',(-20.6770655663065,22.0904816784908,23.8487687038613));
#52352=CARTESIAN_POINT('Ctrl Pts',(-20.6752157478452,22.094128301454,23.849023826549));
#52353=CARTESIAN_POINT('Ctrl Pts',(-20.6723698355491,22.0997651299382,23.8494171302534));
#52354=CARTESIAN_POINT('Ctrl Pts',(-20.6713688630932,22.1017528464478,23.8495556185961));
#52355=CARTESIAN_POINT('Ctrl Pts',(-20.6696162227746,22.1052422071154,23.8497983724419));
#52356=CARTESIAN_POINT('Ctrl Pts',(-20.668863672581,22.1067433959352,23.8499026937576));
#52357=CARTESIAN_POINT('Ctrl Pts',(-20.6672718684488,22.1099249350251,23.8501235411501));
#52358=CARTESIAN_POINT('Ctrl Pts',(-20.6664329125861,22.1116054259506,23.8502400481008));
#52359=CARTESIAN_POINT('Ctrl Pts',(-20.6640523730453,22.116384273115,23.8505709527065));
#52360=CARTESIAN_POINT('Ctrl Pts',(-20.6625143042087,22.1194843923606,23.8507851283171));
#52361=CARTESIAN_POINT('Ctrl Pts',(-20.6560277947913,22.1326116165875,23.8516900018728));
#52362=CARTESIAN_POINT('Ctrl Pts',(-20.651126486011,22.1426621183294,23.8523777713307));
#52363=CARTESIAN_POINT('Ctrl Pts',(-20.562146759046,22.3275581733677,23.8649422237144));
#52364=CARTESIAN_POINT('Ctrl Pts',(-20.4939597164943,22.5096486669378,23.8758840789047));
#52365=CARTESIAN_POINT('Ctrl Pts',(-20.4050022469722,22.8335681701034,23.8946876630477));
#52366=CARTESIAN_POINT('Ctrl Pts',(-20.3765109827375,22.9726721133462,23.9025639437096));
#52367=CARTESIAN_POINT('Ctrl Pts',(-20.3412183565413,23.2305073460493,23.917354402804));
#52368=CARTESIAN_POINT('Ctrl Pts',(-20.3316393381261,23.3486036678032,23.9241997599347));
#52369=CARTESIAN_POINT('Ctrl Pts',(-20.3277034743309,23.5008236176375,23.9332625908732));
#52370=CARTESIAN_POINT('Ctrl Pts',(-20.3273619299407,23.5347063536578,23.93529475094));
#52371=CARTESIAN_POINT('Ctrl Pts',(-20.3276335067348,23.5824414824083,23.9381812226157));
#52372=CARTESIAN_POINT('Ctrl Pts',(-20.3278016631737,23.596294895558,23.9390217017117));
#52373=CARTESIAN_POINT('Ctrl Pts',(-20.328250771991,23.6204561324949,23.9404925900669));
#52374=CARTESIAN_POINT('Ctrl Pts',(-20.3284918804015,23.6307645618137,23.9411217471603));
#52375=CARTESIAN_POINT('Ctrl Pts',(-20.3289114426044,23.645646983032,23.9420324372125));
#52376=CARTESIAN_POINT('Ctrl Pts',(-20.3290501788638,23.6502221039739,23.942312722607));
#52377=CARTESIAN_POINT('Ctrl Pts',(-20.3293096299157,23.6582158951931,23.9428030159618));
#52378=CARTESIAN_POINT('Ctrl Pts',(-20.3294260421854,23.6616347057942,23.943012888473));
#52379=CARTESIAN_POINT('Ctrl Pts',(-20.3296599799454,23.6681977658456,23.9434161312249));
#52380=CARTESIAN_POINT('Ctrl Pts',(-20.3297766673575,23.6713420429934,23.9436094749067));
#52381=CARTESIAN_POINT('Ctrl Pts',(-20.3300618009526,23.6787332097376,23.9440643299999));
#52382=CARTESIAN_POINT('Ctrl Pts',(-20.3302340438858,23.6829799398966,23.9443259604852));
#52383=CARTESIAN_POINT('Ctrl Pts',(-20.3308553244439,23.6975843613215,23.9452266912823));
#52384=CARTESIAN_POINT('Ctrl Pts',(-20.3313459376159,23.7079401362737,23.9458670968083));
#52385=CARTESIAN_POINT('Ctrl Pts',(-20.3374300734454,23.8244653107288,23.9530926681313));
#52386=CARTESIAN_POINT('Ctrl Pts',(-20.3482233794895,23.9302864949458,23.9598411103387));
#52387=CARTESIAN_POINT('Ctrl Pts',(-20.4100764883942,24.3365077697871,23.986511281385));
#52388=CARTESIAN_POINT('Ctrl Pts',(-20.4983943960213,24.629609982848,24.0075733636155));
#52389=CARTESIAN_POINT('Ctrl Pts',(-20.6563287677979,24.9702367166931,24.0324797284));
#52390=CARTESIAN_POINT('Ctrl Pts',(-20.6882877534216,25.0335963876198,24.037122198929));
#52391=CARTESIAN_POINT('Ctrl Pts',(-20.7365061926084,25.1218201403493,24.043549625663));
#52392=CARTESIAN_POINT('Ctrl Pts',(-20.751055515842,25.14759076436,24.0454224511347));
#52393=CARTESIAN_POINT('Ctrl Pts',(-20.7682199751146,25.1770384999244,24.0475538796328));
#52394=CARTESIAN_POINT('Ctrl Pts',(-20.770489708622,25.1809138638992,24.0478342047037));
#52395=CARTESIAN_POINT('Ctrl Pts',(-20.7739396541395,25.1867761976131,24.0482579787291));
#52396=CARTESIAN_POINT('Ctrl Pts',(-20.7751139026096,25.1887666429034,24.0484018144353));
#52397=CARTESIAN_POINT('Ctrl Pts',(-20.7771491719011,25.1922081234281,24.0486504195823));
#52398=CARTESIAN_POINT('Ctrl Pts',(-20.7780091897232,25.1936597430291,24.0487552545951));
#52399=CARTESIAN_POINT('Ctrl Pts',(-20.7798048258241,25.1966851673447,24.0489736922917));
#52400=CARTESIAN_POINT('Ctrl Pts',(-20.7807406426868,25.1982588458151,24.0490872812649));
#52401=CARTESIAN_POINT('Ctrl Pts',(-20.7833288643433,25.2026027930929,24.0494007446474));
#52402=CARTESIAN_POINT('Ctrl Pts',(-20.784984093795,25.2053713896216,24.0496004335171));
#52403=CARTESIAN_POINT('Ctrl Pts',(-20.7914713718626,25.2161853487183,24.0503800497664));
#52404=CARTESIAN_POINT('Ctrl Pts',(-20.7963344595317,25.2242121774625,24.0509579614318));
#52405=CARTESIAN_POINT('Ctrl Pts',(-20.8823241903912,25.364754608552,24.0610651932127));
#52406=CARTESIAN_POINT('Ctrl Pts',(-20.9729073110434,25.4912742656986,24.0699882979585));
#52407=CARTESIAN_POINT('Ctrl Pts',(-21.1933294000038,25.7563521572139,24.0894320316263));
#52408=CARTESIAN_POINT('Ctrl Pts',(-21.3269694692907,25.8909736204585,24.0998531585584));
#52409=CARTESIAN_POINT('Ctrl Pts',(-21.5267954118918,26.0596239943845,24.1147436687288));
#52410=CARTESIAN_POINT('Ctrl Pts',(-21.5834808218823,26.1042948161991,24.1188974046921));
#52411=CARTESIAN_POINT('Ctrl Pts',(-21.7063662386689,26.1946160858944,24.1278169050986));
#52412=CARTESIAN_POINT('Ctrl Pts',(-21.7728699245907,26.2397663697276,24.1325955088226));
#52413=CARTESIAN_POINT('Ctrl Pts',(-21.8497801360932,26.2878826687771,24.1380990118875));
#52414=CARTESIAN_POINT('Ctrl Pts',(-21.8585993466416,26.2933410525492,24.1387297456947));
#52415=CARTESIAN_POINT('Ctrl Pts',(-21.8743988748986,26.3030145216435,24.1398591568115));
#52416=CARTESIAN_POINT('Ctrl Pts',(-21.881369160575,26.3072458838771,24.1403572325108));
#52417=CARTESIAN_POINT('Ctrl Pts',(-21.8919113215309,26.3135909507984,24.1411102905615));
#52418=CARTESIAN_POINT('Ctrl Pts',(-21.8954713811887,26.3157243054611,24.1413645528743));
#52419=CARTESIAN_POINT('Ctrl Pts',(-21.9016476354321,26.3194092102352,24.1418055949037));
#52420=CARTESIAN_POINT('Ctrl Pts',(-21.9042619298394,26.3209639480615,24.1419922578709));
#52421=CARTESIAN_POINT('Ctrl Pts',(-21.9096447327773,26.3241548288673,24.1423765514942));
#52422=CARTESIAN_POINT('Ctrl Pts',(-21.9124134965096,26.3257905333864,24.1425741978904));
#52423=CARTESIAN_POINT('Ctrl Pts',(-21.9198579987277,26.3301735088906,24.1431055584493));
#52424=CARTESIAN_POINT('Ctrl Pts',(-21.9245382158995,26.3329131174339,24.1434395508876));
#52425=CARTESIAN_POINT('Ctrl Pts',(-21.9416374542388,26.3428644518291,24.1446595814824));
#52426=CARTESIAN_POINT('Ctrl Pts',(-21.9540975859397,26.3500048747246,24.1455481993334));
#52427=CARTESIAN_POINT('Ctrl Pts',(-22.0023892250627,26.3772518079234,24.1489909243063));
#52428=CARTESIAN_POINT('Ctrl Pts',(-22.0385399192203,26.3967464445293,24.1515654718717));
#52429=CARTESIAN_POINT('Ctrl Pts',(-22.0750361722079,26.4155368553179,24.1541632309577));
#52430=CARTESIAN_POINT('Origin',(-23.5502525316942,23.5502525316942,-77.3107734492734));
#52431=CARTESIAN_POINT('',(-22.0750360153461,26.4155367745563,25.653793035611));
#52432=CARTESIAN_POINT('',(-22.0750361607755,26.4155368494319,25.4084140214669));
#52433=CARTESIAN_POINT('',(-22.0750360153461,26.4155367745563,-77.3107734492734));
#52434=CARTESIAN_POINT('',(-26.7730020784469,23.5485433198117,24.8107734492728));
#52435=CARTESIAN_POINT('Ctrl Pts',(-26.7730020784469,23.5485433198117,24.8107734492728));
#52436=CARTESIAN_POINT('Ctrl Pts',(-26.7729503115416,23.450935894898,24.8168290675995));
#52437=CARTESIAN_POINT('Ctrl Pts',(-26.7684646036353,23.3534486965496,24.8228846859262));
#52438=CARTESIAN_POINT('Ctrl Pts',(-26.7595750669373,23.2563708764643,24.8289403042529));
#52439=CARTESIAN_POINT('Ctrl Pts',(-26.7505145500469,23.1574258742166,24.8351123955547));
#52440=CARTESIAN_POINT('Ctrl Pts',(-26.736858003116,23.0587260119028,24.8412844868565));
#52441=CARTESIAN_POINT('Ctrl Pts',(-26.7186249230167,22.9607324282157,24.8474565781583));
#52442=CARTESIAN_POINT('Ctrl Pts',(-26.7004165469383,22.8628716161464,24.8536203068866));
#52443=CARTESIAN_POINT('Ctrl Pts',(-26.6776440411043,22.765715603996,24.8597840356149));
#52444=CARTESIAN_POINT('Ctrl Pts',(-26.6503787403315,22.6697214118465,24.8659477643432));
#52445=CARTESIAN_POINT('Ctrl Pts',(-26.6231423245858,22.5738289165339,24.8721049631794));
#52446=CARTESIAN_POINT('Ctrl Pts',(-26.5914226946394,22.4790962097682,24.8782621620156));
#52447=CARTESIAN_POINT('Ctrl Pts',(-26.5553422294784,22.3859701472311,24.8844193608518));
#52448=CARTESIAN_POINT('Ctrl Pts',(-26.519288136949,22.2929121541969,24.8905720591492));
#52449=CARTESIAN_POINT('Ctrl Pts',(-26.4788797029659,22.2014588744071,24.8967247574465));
#52450=CARTESIAN_POINT('Ctrl Pts',(-26.4342888589272,22.112041133568,24.9028774557439));
#52451=CARTESIAN_POINT('Ctrl Pts',(-26.3897149237996,22.0226573000625,24.9090278209293));
#52452=CARTESIAN_POINT('Ctrl Pts',(-26.3409619235781,21.9353078601051,24.9151781861148));
#52453=CARTESIAN_POINT('Ctrl Pts',(-26.2882491878679,21.8504019872987,24.9213285513003));
#52454=CARTESIAN_POINT('Ctrl Pts',(-26.2355423386933,21.7655055960994,24.9274782296622));
#52455=CARTESIAN_POINT('Ctrl Pts',(-26.1788768622937,21.6830525985938,24.9336279080242));
#52456=CARTESIAN_POINT('Ctrl Pts',(-26.1185166255224,21.6034250850896,24.9397775863862));
#52457=CARTESIAN_POINT('Ctrl Pts',(-26.0581469812845,21.5237851612106,24.9459282232086));
#52458=CARTESIAN_POINT('Ctrl Pts',(-25.9940816953355,21.4469719422293,24.9520788600309));
#52459=CARTESIAN_POINT('Ctrl Pts',(-25.926625675243,21.3733353892379,24.9582294968532));
#52460=CARTESIAN_POINT('Ctrl Pts',(-25.8590974913771,21.299620060601,24.9643867135651));
#52461=CARTESIAN_POINT('Ctrl Pts',(-25.7881716238659,21.229088505097,24.9705439302769));
#52462=CARTESIAN_POINT('Ctrl Pts',(-25.7141906149643,21.1620545637122,24.9767011469888));
#52463=CARTESIAN_POINT('Ctrl Pts',(-25.6401683323597,21.0949832243651,24.9828617987868));
#52464=CARTESIAN_POINT('Ctrl Pts',(-25.5630878491221,21.0314136615306,24.9890224505847));
#52465=CARTESIAN_POINT('Ctrl Pts',(-25.4833239940354,20.9716187298561,24.9951831023827));
#52466=CARTESIAN_POINT('Ctrl Pts',(-25.4034266656512,20.9117237399949,25.0013540631421));
#52467=CARTESIAN_POINT('Ctrl Pts',(-25.3208373557785,20.8556162421793,25.0075250239016));
#52468=CARTESIAN_POINT('Ctrl Pts',(-25.2359591145877,20.8035252283585,25.013695984661));
#52469=CARTESIAN_POINT('Ctrl Pts',(-25.1711699579192,20.7637631785316,25.0184063949833));
#52470=CARTESIAN_POINT('Ctrl Pts',(-25.1050477273011,20.7263404488991,25.0231168053055));
#52471=CARTESIAN_POINT('Ctrl Pts',(-25.037779847147,20.691340142641,25.0278272156278));
#52472=CARTESIAN_POINT('Ctrl Pts',(-24.9496381631259,20.645478939229,25.0339993069332));
#52473=CARTESIAN_POINT('Ctrl Pts',(-24.8592183703656,20.6036169615311,25.0401713982386));
#52474=CARTESIAN_POINT('Ctrl Pts',(-24.7669189714713,20.5659870715147,25.046343489544));
#52475=CARTESIAN_POINT('Ctrl Pts',(-24.6747446291396,20.5284081662799,25.0525072182757));
#52476=CARTESIAN_POINT('Ctrl Pts',(-24.5806961411827,20.4950501142229,25.0586709470075));
#52477=CARTESIAN_POINT('Ctrl Pts',(-24.4851965657563,20.4660999388947,25.0648346757392));
#52478=CARTESIAN_POINT('Ctrl Pts',(-24.3897981631688,20.4371804335608,25.0709918745787));
#52479=CARTESIAN_POINT('Ctrl Pts',(-24.2929521428106,20.4126596464327,25.0771490734183));
#52480=CARTESIAN_POINT('Ctrl Pts',(-24.1951006028942,20.3926761624563,25.0833062722578));
#52481=CARTESIAN_POINT('Ctrl Pts',(-24.0973205865218,20.3727072851953,25.0894589705582));
#52482=CARTESIAN_POINT('Ctrl Pts',(-23.9985369361751,20.3572692039967,25.0956116688586));
#52483=CARTESIAN_POINT('Ctrl Pts',(-23.8992050489584,20.3464501496496,25.101764367159));
#52484=CARTESIAN_POINT('Ctrl Pts',(-23.7999108285361,20.3356351979034,25.1079147323474));
#52485=CARTESIAN_POINT('Ctrl Pts',(-23.7000692156912,20.3294358396973,25.1140650975358));
#52486=CARTESIAN_POINT('Ctrl Pts',(-23.6001430119909,20.3278887250337,25.1202154627242));
#52487=CARTESIAN_POINT('Ctrl Pts',(-23.5002279672502,20.3263417831394,25.126365141089));
#52488=CARTESIAN_POINT('Ctrl Pts',(-23.400228784785,20.3294460586256,25.1325148194537));
#52489=CARTESIAN_POINT('Ctrl Pts',(-23.3006095548028,20.3371860918911,25.1386644978185));
#52490=CARTESIAN_POINT('Ctrl Pts',(-23.2009747986322,20.3449273314821,25.1448151346435));
#52491=CARTESIAN_POINT('Ctrl Pts',(-23.1017205457037,20.3573057302842,25.1509657714684));
#52492=CARTESIAN_POINT('Ctrl Pts',(-23.0033060396225,20.3742539332514,25.1571164082933));
#52493=CARTESIAN_POINT('Ctrl Pts',(-22.9047862506941,20.3912202672355,25.1632736250076));
#52494=CARTESIAN_POINT('Ctrl Pts',(-22.8071084314714,20.412766093829,25.1694308417219));
#52495=CARTESIAN_POINT('Ctrl Pts',(-22.7107217802524,20.4387728708441,25.1755880584361));
#52496=CARTESIAN_POINT('Ctrl Pts',(-22.614281355316,20.4647941569335,25.1817487102363));
#52497=CARTESIAN_POINT('Ctrl Pts',(-22.5191339466243,20.4952812171865,25.1879093620365));
#52498=CARTESIAN_POINT('Ctrl Pts',(-22.4257117222186,20.5300661913629,25.1940700138367));
#52499=CARTESIAN_POINT('Ctrl Pts',(-22.3321331692098,20.5649093731708,25.2002409745982));
#52500=CARTESIAN_POINT('Ctrl Pts',(-22.2402859666905,20.6040646641897,25.2064119353597));
#52501=CARTESIAN_POINT('Ctrl Pts',(-22.150580635134,20.6473167514056,25.2125828961211));
#52502=CARTESIAN_POINT('Ctrl Pts',(-22.0821068701068,20.6803318822298,25.2172933064149));
#52503=CARTESIAN_POINT('Ctrl Pts',(-22.0148806314104,20.7157330522426,25.2220037167087));
#52504=CARTESIAN_POINT('Ctrl Pts',(-21.9490731459827,20.7534074989345,25.2267141270025));
#52505=CARTESIAN_POINT('Ctrl Pts',(-21.862845028446,20.8027726524025,25.232886218366));
#52506=CARTESIAN_POINT('Ctrl Pts',(-21.7787501123152,20.8562161680798,25.2390583097295));
#52507=CARTESIAN_POINT('Ctrl Pts',(-21.6971997158266,20.9135286507948,25.245230401093));
#52508=CARTESIAN_POINT('Ctrl Pts',(-21.6157598120601,20.9707634807638,25.251394129883));
#52509=CARTESIAN_POINT('Ctrl Pts',(-21.5368579277957,21.0318566110277,25.2575578586731));
#52510=CARTESIAN_POINT('Ctrl Pts',(-21.4608800899563,21.0965532098118,25.2637215874632));
#52511=CARTESIAN_POINT('Ctrl Pts',(-21.3849827435036,21.1611812686229,25.2698787863612));
#52512=CARTESIAN_POINT('Ctrl Pts',(-21.3120036137762,21.2294049262685,25.2760359852593));
#52513=CARTESIAN_POINT('Ctrl Pts',(-21.2422982674428,21.3009271491353,25.2821931841574));
#52514=CARTESIAN_POINT('Ctrl Pts',(-21.1726438714911,21.3723970935938,25.2883458825164));
#52515=CARTESIAN_POINT('Ctrl Pts',(-21.1062588036481,21.4471604995426,25.2944985808754));
#52516=CARTESIAN_POINT('Ctrl Pts',(-21.0434634554003,21.5248819262312,25.3006512792344));
#52517=CARTESIAN_POINT('Ctrl Pts',(-20.9806919192384,21.6025738808436,25.3068016444814));
#52518=CARTESIAN_POINT('Ctrl Pts',(-20.9215076706287,21.6832212898979,25.3129520097284));
#52519=CARTESIAN_POINT('Ctrl Pts',(-20.8661917077021,21.7664546015432,25.3191023749753));
#52520=CARTESIAN_POINT('Ctrl Pts',(-20.8108819220205,21.8496786183571,25.3252520533987));
#52521=CARTESIAN_POINT('Ctrl Pts',(-20.759439803631,21.9354876018513,25.331401731822));
#52522=CARTESIAN_POINT('Ctrl Pts',(-20.7121032065455,22.023482748571,25.3375514102453));
#52523=CARTESIAN_POINT('Ctrl Pts',(-20.6647592317998,22.1114916098019,25.3437020471287));
#52524=CARTESIAN_POINT('Ctrl Pts',(-20.6215222551146,22.2016869284285,25.349852684012));
#52525=CARTESIAN_POINT('Ctrl Pts',(-20.5825838501992,22.2936459268358,25.3560033208954));
#52526=CARTESIAN_POINT('Ctrl Pts',(-20.5436037893743,22.3857033020442,25.3621605376676));
#52527=CARTESIAN_POINT('Ctrl Pts',(-20.5089316529185,22.4795277239199,25.3683177544397));
#52528=CARTESIAN_POINT('Ctrl Pts',(-20.4787105200252,22.5746771973133,25.3744749712119));
#52529=CARTESIAN_POINT('Ctrl Pts',(-20.4484725268871,22.6698797542037,25.3806356230698));
#52530=CARTESIAN_POINT('Ctrl Pts',(-20.422690594659,22.7664084150925,25.3867962749276));
#52531=CARTESIAN_POINT('Ctrl Pts',(-20.4014571048539,22.8638088541726,25.3929569267855));
#52532=CARTESIAN_POINT('Ctrl Pts',(-20.3801880838731,22.9613722788071,25.3991278876037));
#52533=CARTESIAN_POINT('Ctrl Pts',(-20.3634827811419,23.0598099670568,25.4052988484219));
#52534=CARTESIAN_POINT('Ctrl Pts',(-20.3513819539305,23.1586601553409,25.41146980924));
#52535=CARTESIAN_POINT('Ctrl Pts',(-20.3421451663856,23.2341143513231,25.4161802189525));
#52536=CARTESIAN_POINT('Ctrl Pts',(-20.3355901338506,23.3098087377366,25.420890628665));
#52537=CARTESIAN_POINT('Ctrl Pts',(-20.3317145427561,23.385538305647,25.4256010383775));
#52538=CARTESIAN_POINT('Ctrl Pts',(-20.3266363216934,23.4847674238516,25.4317731296101));
#52539=CARTESIAN_POINT('Ctrl Pts',(-20.326142380789,23.584406371618,25.4379452208428));
#52540=CARTESIAN_POINT('Ctrl Pts',(-20.3302788873238,23.6839959130626,25.4441173120754));
#52541=CARTESIAN_POINT('Ctrl Pts',(-20.3344097893012,23.7834505205247,25.4502810407347));
#52542=CARTESIAN_POINT('Ctrl Pts',(-20.3431586510069,23.8828554245149,25.4564447693939));
#52543=CARTESIAN_POINT('Ctrl Pts',(-20.3565197421183,23.9817481067446,25.4626084980532));
#52544=CARTESIAN_POINT('Ctrl Pts',(-20.369866678408,24.0805360214613,25.4687656968205));
#52545=CARTESIAN_POINT('Ctrl Pts',(-20.3878160720054,24.1788123651428,25.4749228955879));
#52546=CARTESIAN_POINT('Ctrl Pts',(-20.410310222414,24.2761174343394,25.4810800943553));
#52547=CARTESIAN_POINT('Ctrl Pts',(-20.4327879309649,24.3733513794407,25.4872327925843));
#52548=CARTESIAN_POINT('Ctrl Pts',(-20.4598036942034,24.4696150395802,25.4933854908134));
#52549=CARTESIAN_POINT('Ctrl Pts',(-20.4912484853867,24.5644575440928,25.4995381890424));
#52550=CARTESIAN_POINT('Ctrl Pts',(-20.5226813526625,24.6592640841989,25.50568855416));
#52551=CARTESIAN_POINT('Ctrl Pts',(-20.5585397741922,24.7526501276034,25.5118389192775));
#52552=CARTESIAN_POINT('Ctrl Pts',(-20.5986647312134,24.8441795074362,25.517989284395));
#52553=CARTESIAN_POINT('Ctrl Pts',(-20.6387852074039,24.9356986660081,25.5241389626895));
#52554=CARTESIAN_POINT('Ctrl Pts',(-20.6831710974228,25.0253611753709,25.530288640984));
#52555=CARTESIAN_POINT('Ctrl Pts',(-20.731615451417,25.1127513547935,25.5364383192785));
#52556=CARTESIAN_POINT('Ctrl Pts',(-20.7800673557275,25.2001551544512,25.5425889560338));
#52557=CARTESIAN_POINT('Ctrl Pts',(-20.8325787697541,25.2852855407593,25.5487395927892));
#52558=CARTESIAN_POINT('Ctrl Pts',(-20.8888975573152,25.367752810332,25.5548902295445));
#52559=CARTESIAN_POINT('Ctrl Pts',(-20.9452765941619,25.4503083025793,25.5610474461906));
#52560=CARTESIAN_POINT('Ctrl Pts',(-21.00547089264,25.5301946295357,25.5672046628367));
#52561=CARTESIAN_POINT('Ctrl Pts',(-21.0691859351917,25.6070524991727,25.5733618794828));
#52562=CARTESIAN_POINT('Ctrl Pts',(-21.1329365241119,25.6839532475091,25.5795225312156));
#52563=CARTESIAN_POINT('Ctrl Pts',(-21.2002114762874,25.7578218526046,25.5856831829483));
#52564=CARTESIAN_POINT('Ctrl Pts',(-21.2706784959261,25.8283350099974,25.591843834681));
#52565=CARTESIAN_POINT('Ctrl Pts',(-21.3412634319697,25.898966161,25.5980147953769));
#52566=CARTESIAN_POINT('Ctrl Pts',(-21.4150507837403,25.9662303559649,25.6041857560727));
#52567=CARTESIAN_POINT('Ctrl Pts',(-21.4916740928308,26.0298437023404,25.6103567167685));
#52568=CARTESIAN_POINT('Ctrl Pts',(-21.5501621136388,26.0784009725842,25.6150671277631));
#52569=CARTESIAN_POINT('Ctrl Pts',(-21.6103018138662,26.1248318693068,25.6197775387578));
#52570=CARTESIAN_POINT('Ctrl Pts',(-21.6719194653256,26.1690275228468,25.6244879497524));
#52571=CARTESIAN_POINT('Ctrl Pts',(-21.7526486331184,26.2269310333805,25.6306593560061));
#52572=CARTESIAN_POINT('Ctrl Pts',(-21.836199967998,26.2812000499403,25.6368307622599));
#52573=CARTESIAN_POINT('Ctrl Pts',(-21.9222121847103,26.3315475881549,25.6430021685136));
#52574=CARTESIAN_POINT('Ctrl Pts',(-21.9723437301601,26.360892255654,25.6465991242127));
#52575=CARTESIAN_POINT('Ctrl Pts',(-22.0233105772739,26.3889054828269,25.6501960799119));
#52576=CARTESIAN_POINT('Ctrl Pts',(-22.0750360153461,26.4155367745563,25.653793035611));
#52577=CARTESIAN_POINT('Ctrl Pts',(-26.7730020009422,23.5484029475698,24.8083546326523));
#52578=CARTESIAN_POINT('Ctrl Pts',(-26.7731829229496,23.8636447879474,24.7900599457156));
#52579=CARTESIAN_POINT('Ctrl Pts',(-26.7271130127483,24.1772373733017,24.7732082235204));
#52580=CARTESIAN_POINT('Ctrl Pts',(-26.6081560899502,24.5724184315231,24.7492635678694));
#52581=CARTESIAN_POINT('Ctrl Pts',(-26.5758835712151,24.6643222259386,24.7435064575939));
#52582=CARTESIAN_POINT('Ctrl Pts',(-26.5329639705256,24.7708492053277,24.7365476269339));
#52583=CARTESIAN_POINT('Ctrl Pts',(-26.5262925927927,24.7870262793587,24.7354829744732));
#52584=CARTESIAN_POINT('Ctrl Pts',(-26.5172878862852,24.8083665366096,24.7340677738117));
#52585=CARTESIAN_POINT('Ctrl Pts',(-26.5150721265288,24.813579256732,24.7337212336612));
#52586=CARTESIAN_POINT('Ctrl Pts',(-26.5114154033842,24.8221193318752,24.7331520805999));
#52587=CARTESIAN_POINT('Ctrl Pts',(-26.5099825396466,24.8254501594891,24.7329297446674));
#52588=CARTESIAN_POINT('Ctrl Pts',(-26.5071979000963,24.8318933413037,24.732498969244));
#52589=CARTESIAN_POINT('Ctrl Pts',(-26.5058468234619,24.8350059939978,24.7322905539096));
#52590=CARTESIAN_POINT('Ctrl Pts',(-26.5027201488775,24.8421782901962,24.7318095947986));
#52591=CARTESIAN_POINT('Ctrl Pts',(-26.5009410923502,24.8462364103354,24.7315369327176));
#52592=CARTESIAN_POINT('Ctrl Pts',(-26.4953783888303,24.8588543945781,24.7306874711052));
#52593=CARTESIAN_POINT('Ctrl Pts',(-26.491565845879,24.8674013975213,24.7301096798018));
#52594=CARTESIAN_POINT('Ctrl Pts',(-26.4589039024724,24.9397743217212,24.7251966063665));
#52595=CARTESIAN_POINT('Ctrl Pts',(-26.4280199961365,25.0026563250545,24.7207912836801));
#52596=CARTESIAN_POINT('Ctrl Pts',(-26.3911499023996,25.0719262395936,24.71577731142));
#52597=CARTESIAN_POINT('Ctrl Pts',(-26.3871565679271,25.0793582282664,24.7152372472884));
#52598=CARTESIAN_POINT('Ctrl Pts',(-26.3567766719616,25.1353695679733,24.7111510342131));
#52599=CARTESIAN_POINT('Ctrl Pts',(-26.3291744805024,25.1832761114008,24.7075646483272));
#52600=CARTESIAN_POINT('Ctrl Pts',(-26.1644291442531,25.4529273856814,24.6868551744497));
#52601=CARTESIAN_POINT('Ctrl Pts',(-26.002011043197,25.6580817296413,24.6689254480265));
#52602=CARTESIAN_POINT('Ctrl Pts',(-25.7715222255063,25.8860856273245,24.6472869898608));
#52603=CARTESIAN_POINT('Ctrl Pts',(-25.7250329927821,25.9294301611663,24.643087990581));
#52604=CARTESIAN_POINT('Ctrl Pts',(-25.6496876396391,25.9956236121448,24.6365755393889));
#52605=CARTESIAN_POINT('Ctrl Pts',(-25.6216712691363,26.0194005971973,24.6342144210437));
#52606=CARTESIAN_POINT('Ctrl Pts',(-25.583593513431,26.0506121083367,24.6310921866857));
#52607=CARTESIAN_POINT('Ctrl Pts',(-25.5738878101214,26.0584737803422,24.6303037378344));
#52608=CARTESIAN_POINT('Ctrl Pts',(-25.5576061972556,26.0715059480572,24.6289937119343));
#52609=CARTESIAN_POINT('Ctrl Pts',(-25.5510555165781,26.0767075476308,24.6284700153822));
#52610=CARTESIAN_POINT('Ctrl Pts',(-25.5421490689468,26.0837233893494,24.6277626322869));
#52611=CARTESIAN_POINT('Ctrl Pts',(-25.5398110097781,26.0855599024408,24.6275773666569));
#52612=CARTESIAN_POINT('Ctrl Pts',(-25.5360948401269,26.0884705959114,24.6272835900863));
#52613=CARTESIAN_POINT('Ctrl Pts',(-25.5347183990394,26.0895468897506,24.6271749272451));
#52614=CARTESIAN_POINT('Ctrl Pts',(-25.5318555171133,26.0917817411305,24.6269492300012));
#52615=CARTESIAN_POINT('Ctrl Pts',(-25.5303689392054,26.0929401111973,24.6268322095589));
#52616=CARTESIAN_POINT('Ctrl Pts',(-25.5269558502869,26.0955948472363,24.6265639374704));
#52617=CARTESIAN_POINT('Ctrl Pts',(-25.5250286514086,26.0970903337783,24.6264127491369));
#52618=CARTESIAN_POINT('Ctrl Pts',(-25.5189367888999,26.1018064846637,24.6259357566268));
#52619=CARTESIAN_POINT('Ctrl Pts',(-25.5147659030678,26.1050191539337,24.6256105215025));
#52620=CARTESIAN_POINT('Ctrl Pts',(-25.4801134198738,26.1315755584305,24.6229193670571));
#52621=CARTESIAN_POINT('Ctrl Pts',(-25.4492231531455,26.154384347586,24.6205905337262));
#52622=CARTESIAN_POINT('Ctrl Pts',(-25.4083916698818,26.1834204948443,24.6175919183136));
#52623=CARTESIAN_POINT('Ctrl Pts',(-25.3988153110416,26.190152195999,24.6168942450292));
#52624=CARTESIAN_POINT('Ctrl Pts',(-25.3831371613361,26.2010460061342,24.6157607632035));
#52625=CARTESIAN_POINT('Ctrl Pts',(-25.3770574492587,26.205239519366,24.6153233414309));
#52626=CARTESIAN_POINT('Ctrl Pts',(-25.2872292634605,26.26674434496,24.6088907718959));
#52627=CARTESIAN_POINT('Ctrl Pts',(-25.2008271021701,26.3200941762613,24.603090576683));
#52628=CARTESIAN_POINT('Ctrl Pts',(-25.0500311775264,26.4036378361574,24.5933620074062));
#52629=CARTESIAN_POINT('Ctrl Pts',(-24.9868994038662,26.43593958656,24.5893994834452));
#52630=CARTESIAN_POINT('Ctrl Pts',(-24.783229503671,26.5318066703035,24.5768211899159));
#52631=CARTESIAN_POINT('Ctrl Pts',(-24.639177555762,26.5873787958498,24.5682156958418));
#52632=CARTESIAN_POINT('Ctrl Pts',(-24.3825066355611,26.6657795148598,24.5527578007421));
#52633=CARTESIAN_POINT('Ctrl Pts',(-24.2716200106518,26.6933051675425,24.5460439215414));
#52634=CARTESIAN_POINT('Ctrl Pts',(-24.1405303566504,26.7185428319792,24.5379638604057));
#52635=CARTESIAN_POINT('Ctrl Pts',(-24.1215135510899,26.7220268237688,24.5367883612839));
#52636=CARTESIAN_POINT('Ctrl Pts',(-24.0966742280309,26.7263469040183,24.5352482350452));
#52637=CARTESIAN_POINT('Ctrl Pts',(-24.0908788742407,26.7273385061615,24.5348885689008));
#52638=CARTESIAN_POINT('Ctrl Pts',(-24.0814579094915,26.7289239375919,24.5343033402141));
#52639=CARTESIAN_POINT('Ctrl Pts',(-24.0778339214935,26.7295274391271,24.5340780858782));
#52640=CARTESIAN_POINT('Ctrl Pts',(-24.0708772729198,26.7306737054647,24.533645427159));
#52641=CARTESIAN_POINT('Ctrl Pts',(-24.0675447739702,26.7312174324258,24.5334380536958));
#52642=CARTESIAN_POINT('Ctrl Pts',(-24.0599433036526,26.7324454189734,24.5329647708083));
#52643=CARTESIAN_POINT('Ctrl Pts',(-24.0556738041121,26.7331263262337,24.5326987551748));
#52644=CARTESIAN_POINT('Ctrl Pts',(-24.042365958612,26.7352212330773,24.5318690028271));
#52645=CARTESIAN_POINT('Ctrl Pts',(-24.0333230126722,26.7366053309589,24.5313043174583));
#52646=CARTESIAN_POINT('Ctrl Pts',(-23.9630465829505,26.7470556805904,24.5269091364839));
#52647=CARTESIAN_POINT('Ctrl Pts',(-23.9015729284183,26.7543939799702,24.5230241643808));
#52648=CARTESIAN_POINT('Ctrl Pts',(-23.8348940360998,26.7604117703565,24.5187625207856));
#52649=CARTESIAN_POINT('Ctrl Pts',(-23.8298576630376,26.7608543590255,24.5184403404906));
#52650=CARTESIAN_POINT('Ctrl Pts',(-23.802907893282,26.7631587697666,24.5167147847664));
#52651=CARTESIAN_POINT('Ctrl Pts',(-23.7809773232093,26.7648080623732,24.5153050783406));
#52652=CARTESIAN_POINT('Ctrl Pts',(-23.5035062614069,26.7828213143613,24.497399136189));
#52653=CARTESIAN_POINT('Ctrl Pts',(-23.246944905116,26.7688937132499,24.4799839898157));
#52654=CARTESIAN_POINT('Ctrl Pts',(-22.8890453021343,26.7062700769006,24.4554642681914));
#52655=CARTESIAN_POINT('Ctrl Pts',(-22.7842835862117,26.6824940069301,24.448274714745));
#52656=CARTESIAN_POINT('Ctrl Pts',(-22.6413059934595,26.6424401479014,24.4386003177503));
#52657=CARTESIAN_POINT('Ctrl Pts',(-22.6019282340121,26.6305917090377,24.4359509820921));
#52658=CARTESIAN_POINT('Ctrl Pts',(-22.5498718007017,26.6138354034694,24.4324784842278));
#52659=CARTESIAN_POINT('Ctrl Pts',(-22.5369837087975,26.6095968939198,24.4316212278387));
#52660=CARTESIAN_POINT('Ctrl Pts',(-22.5184326885527,26.6033659262793,24.4303912470133));
#52661=CARTESIAN_POINT('Ctrl Pts',(-22.5127481654279,26.6014389042765,24.4300148851612));
#52662=CARTESIAN_POINT('Ctrl Pts',(-22.5026546478469,26.597985788319,24.4293476087184));
#52663=CARTESIAN_POINT('Ctrl Pts',(-22.4982435413587,26.5964659869013,24.4290563322886));
#52664=CARTESIAN_POINT('Ctrl Pts',(-22.4916298657739,26.5941712338393,24.4286201407113));
#52665=CARTESIAN_POINT('Ctrl Pts',(-22.4894248377134,26.5934034674573,24.428474800416));
#52666=CARTESIAN_POINT('Ctrl Pts',(-22.4854981444806,26.5920314497977,24.4282161388622));
#52667=CARTESIAN_POINT('Ctrl Pts',(-22.48377615948,26.5914281332143,24.4281027618608));
#52668=CARTESIAN_POINT('Ctrl Pts',(-22.4803287604498,26.5902170105416,24.4278758921971));
#52669=CARTESIAN_POINT('Ctrl Pts',(-22.4786033575071,26.5896091998778,24.4277624003191));
#52670=CARTESIAN_POINT('Ctrl Pts',(-22.4738440777874,26.587928083693,24.4274494985629));
#52671=CARTESIAN_POINT('Ctrl Pts',(-22.4708112790477,26.5868516987154,24.4272502731076));
#52672=CARTESIAN_POINT('Ctrl Pts',(-22.4589889621292,26.5826358346145,24.4264742974844));
#52673=CARTESIAN_POINT('Ctrl Pts',(-22.450211374184,26.5794626813791,24.4258995393776));
#52674=CARTESIAN_POINT('Ctrl Pts',(-22.3160453566838,26.5303007507336,24.4171335696966));
#52675=CARTESIAN_POINT('Ctrl Pts',(-22.1936747191441,26.4766189517593,24.4093940250471));
#52676=CARTESIAN_POINT('Ctrl Pts',(-22.0750358518511,26.4155366903795,24.4018187331506));
#52677=CARTESIAN_POINT('Ctrl Pts',(-22.0750361722079,26.4155368553179,24.1541632309577));
#52678=CARTESIAN_POINT('Ctrl Pts',(-22.2447100853409,26.5028949336658,24.1662404145976));
#52679=CARTESIAN_POINT('Ctrl Pts',(-22.4218508058323,26.5750313572462,24.1788526081293));
#52680=CARTESIAN_POINT('Ctrl Pts',(-22.72466923503,26.6680019667534,24.2001947943061));
#52681=CARTESIAN_POINT('Ctrl Pts',(-22.8470106117513,26.6978547808728,24.2087525403761));
#52682=CARTESIAN_POINT('Ctrl Pts',(-23.0398027584921,26.7330942509945,24.2219317630653));
#52683=CARTESIAN_POINT('Ctrl Pts',(-23.1092192415935,26.7434532776121,24.2266152637563));
#52684=CARTESIAN_POINT('Ctrl Pts',(-23.2470672325462,26.759442854602,24.2357319232465));
#52685=CARTESIAN_POINT('Ctrl Pts',(-23.3154538668281,26.7651701146984,24.2401660867381));
#52686=CARTESIAN_POINT('Ctrl Pts',(-23.3949764318985,26.7692785041857,24.2451808350332));
#52687=CARTESIAN_POINT('Ctrl Pts',(-23.4059791595261,26.7697903993414,24.2458715332543));
#52688=CARTESIAN_POINT('Ctrl Pts',(-23.4202837255786,26.770382432114,24.246765233302));
#52689=CARTESIAN_POINT('Ctrl Pts',(-23.4235831928683,26.7705139100571,24.2469710773621));
#52690=CARTESIAN_POINT('Ctrl Pts',(-23.428932444153,26.7707188342289,24.2473043163164));
#52691=CARTESIAN_POINT('Ctrl Pts',(-23.4309820956735,26.7707953947145,24.2474318867301));
#52692=CARTESIAN_POINT('Ctrl Pts',(-23.4349170636705,26.7709386156126,24.2476765759008));
#52693=CARTESIAN_POINT('Ctrl Pts',(-23.4368023600201,26.7710055771622,24.2477937111044));
#52694=CARTESIAN_POINT('Ctrl Pts',(-23.441137449412,26.7711557388236,24.2480628290084));
#52695=CARTESIAN_POINT('Ctrl Pts',(-23.4435872853156,26.7712377996191,24.2482147470742));
#52696=CARTESIAN_POINT('Ctrl Pts',(-23.4513613076727,26.7714893227218,24.2486963084999));
#52697=CARTESIAN_POINT('Ctrl Pts',(-23.4566858572178,26.7716483807711,24.2490253671839));
#52698=CARTESIAN_POINT('Ctrl Pts',(-23.5020002689835,26.7728895943084,24.2518194415279));
#52699=CARTESIAN_POINT('Ctrl Pts',(-23.5420089029944,26.7732403257166,24.254244158474));
#52700=CARTESIAN_POINT('Ctrl Pts',(-23.5894453648174,26.7727727700537,24.2570799273101));
#52701=CARTESIAN_POINT('Ctrl Pts',(-23.5968746210305,26.7726738492105,24.2575229132003));
#52702=CARTESIAN_POINT('Ctrl Pts',(-23.6065794133295,26.7725110604257,24.2581001732299));
#52703=CARTESIAN_POINT('Ctrl Pts',(-23.608855256234,26.7724704734712,24.2582354435308));
#52704=CARTESIAN_POINT('Ctrl Pts',(-23.6170346415687,26.7723159353245,24.2587212473545));
#52705=CARTESIAN_POINT('Ctrl Pts',(-23.6229379451371,26.7721881702241,24.2590711960261));
#52706=CARTESIAN_POINT('Ctrl Pts',(-23.6326697540266,26.7719507846003,24.2596470422848));
#52707=CARTESIAN_POINT('Ctrl Pts',(-23.6364984508115,26.771850562641,24.2598733225294));
#52708=CARTESIAN_POINT('Ctrl Pts',(-23.6622200022581,26.7711313756353,24.261391736511));
#52709=CARTESIAN_POINT('Ctrl Pts',(-23.6841067098141,26.7702960629841,24.2626752118637));
#52710=CARTESIAN_POINT('Ctrl Pts',(-23.7409124127531,26.7675478622886,24.2659880224285));
#52711=CARTESIAN_POINT('Ctrl Pts',(-23.7758123407182,26.7652895992896,24.2680052869893));
#52712=CARTESIAN_POINT('Ctrl Pts',(-23.9444726084568,26.7516161506131,24.2776953423726));
#52713=CARTESIAN_POINT('Ctrl Pts',(-24.0774731362469,26.7324184848717,24.2851622028118));
#52714=CARTESIAN_POINT('Ctrl Pts',(-24.3545482966431,26.6745710077587,24.3009834459309));
#52715=CARTESIAN_POINT('Ctrl Pts',(-24.4979148720412,26.6341120261508,24.3093308043312));
#52716=CARTESIAN_POINT('Ctrl Pts',(-24.7326848571957,26.5499352669083,24.3237800651477));
#52717=CARTESIAN_POINT('Ctrl Pts',(-24.8257532540196,26.5115592580394,24.3297234804835));
#52718=CARTESIAN_POINT('Ctrl Pts',(-24.9275987789843,26.4638714622227,24.3365359669732));
#52719=CARTESIAN_POINT('Ctrl Pts',(-24.9383016191099,26.4587878473393,24.3372557592595));
#52720=CARTESIAN_POINT('Ctrl Pts',(-24.9547161777229,26.4508800543719,24.3383657515743));
#52721=CARTESIAN_POINT('Ctrl Pts',(-24.9604480375965,26.4480977298627,24.3387544987821));
#52722=CARTESIAN_POINT('Ctrl Pts',(-24.9710873564993,26.4428942150551,24.339478228975));
#52723=CARTESIAN_POINT('Ctrl Pts',(-24.9759969805754,26.4404774837691,24.3398130555789));
#52724=CARTESIAN_POINT('Ctrl Pts',(-24.9840841354077,26.43647101244,24.3403660025021));
#52725=CARTESIAN_POINT('Ctrl Pts',(-24.9872652483703,26.4348884945769,24.3405838694409));
#52726=CARTESIAN_POINT('Ctrl Pts',(-24.9934794996717,26.4317842419193,24.3410101823424));
#52727=CARTESIAN_POINT('Ctrl Pts',(-24.9965128651859,26.430262970175,24.3412186118303));
#52728=CARTESIAN_POINT('Ctrl Pts',(-25.0035018748681,26.4267440659708,24.3416996143388));
#52729=CARTESIAN_POINT('Ctrl Pts',(-25.0074558061545,26.4247430633865,24.3419723057027));
#52730=CARTESIAN_POINT('Ctrl Pts',(-25.0197486811314,26.4184900126817,24.3428218977587));
#52731=CARTESIAN_POINT('Ctrl Pts',(-25.0280731794824,26.4142098132466,24.3433997906087));
#52732=CARTESIAN_POINT('Ctrl Pts',(-25.0985592178828,26.3775789356495,24.3483149972469));
#52733=CARTESIAN_POINT('Ctrl Pts',(-25.1596647473001,26.3432472084175,24.3527224178789));
#52734=CARTESIAN_POINT('Ctrl Pts',(-25.2262875569993,26.3029031261272,24.3576990825772));
#52735=CARTESIAN_POINT('Ctrl Pts',(-25.2329611246031,26.2988286159157,24.3581995407796));
#52736=CARTESIAN_POINT('Ctrl Pts',(-25.3392779846162,26.2333851106255,24.3662035614789));
#52737=CARTESIAN_POINT('Ctrl Pts',(-25.4355109429511,26.1666638742353,24.3738920895116));
#52738=CARTESIAN_POINT('Ctrl Pts',(-25.5893679031738,26.047088034922,24.3869034538945));
#52739=CARTESIAN_POINT('Ctrl Pts',(-25.6490874218692,25.9971016075127,24.392151655686));
#52740=CARTESIAN_POINT('Ctrl Pts',(-25.8277435836705,25.8362060101559,24.4084118474589));
#52741=CARTESIAN_POINT('Ctrl Pts',(-25.9401502971111,25.7184182410306,24.4194691482687));
#52742=CARTESIAN_POINT('Ctrl Pts',(-26.0865598898561,25.5397111010809,24.4346449286161));
#52743=CARTESIAN_POINT('Ctrl Pts',(-26.1282346035031,25.4854038087505,24.4390677021774));
#52744=CARTESIAN_POINT('Ctrl Pts',(-26.1745655922208,25.4208726081644,24.4440705412725));
#52745=CARTESIAN_POINT('Ctrl Pts',(-26.1809339011975,25.4119061113493,24.4447601826025));
#52746=CARTESIAN_POINT('Ctrl Pts',(-26.1891534818622,25.4002066471059,24.4456527190623));
#52747=CARTESIAN_POINT('Ctrl Pts',(-26.1910465301905,25.3975033299523,24.4458584473119));
#52748=CARTESIAN_POINT('Ctrl Pts',(-26.1941091300579,25.3931155366388,24.4461915448068));
#52749=CARTESIAN_POINT('Ctrl Pts',(-26.1952812260625,25.391432852502,24.4463190892971));
#52750=CARTESIAN_POINT('Ctrl Pts',(-26.1975285744576,25.3881999398796,24.4465637609153));
#52751=CARTESIAN_POINT('Ctrl Pts',(-26.1986040684866,25.3866498904999,24.4466809044325));
#52752=CARTESIAN_POINT('Ctrl Pts',(-26.2010742788195,25.3830830312749,24.4469500854416));
#52753=CARTESIAN_POINT('Ctrl Pts',(-26.2024680583072,25.3810655684935,24.4471020581985));
#52754=CARTESIAN_POINT('Ctrl Pts',(-26.206179773632,25.375679814866,24.4475070202332));
#52755=CARTESIAN_POINT('Ctrl Pts',(-26.2084936138016,25.372308686276,24.4477597296647));
#52756=CARTESIAN_POINT('Ctrl Pts',(-26.2241744231407,25.3493692246748,24.4494741764484));
#52757=CARTESIAN_POINT('Ctrl Pts',(-26.2373320724234,25.3296577068003,24.4509218975529));
#52758=CARTESIAN_POINT('Ctrl Pts',(-26.4264526356753,25.0394532647605,24.4718944784099));
#52759=CARTESIAN_POINT('Ctrl Pts',(-26.5610622265451,24.7441320491174,24.48908181635));
#52760=CARTESIAN_POINT('Ctrl Pts',(-26.6777387859486,24.3348033696304,24.5132784037033));
#52761=CARTESIAN_POINT('Ctrl Pts',(-26.70117466175,24.2346335213793,24.5192113911714));
#52762=CARTESIAN_POINT('Ctrl Pts',(-26.7316214122632,24.0691832416836,24.5291575731653));
#52763=CARTESIAN_POINT('Ctrl Pts',(-26.7414986148808,24.0045041589202,24.5330811276687));
#52764=CARTESIAN_POINT('Ctrl Pts',(-26.7504213975063,23.9311832561042,24.5375832887968));
#52765=CARTESIAN_POINT('Ctrl Pts',(-26.7514093305785,23.9227899570974,24.5380994598241));
#52766=CARTESIAN_POINT('Ctrl Pts',(-26.752842333348,23.9101886776667,24.5388756343341));
#52767=CARTESIAN_POINT('Ctrl Pts',(-26.7533121538779,23.9059835020947,24.5391348555624));
#52768=CARTESIAN_POINT('Ctrl Pts',(-26.7541054000862,23.8987544806794,24.5395808314792));
#52769=CARTESIAN_POINT('Ctrl Pts',(-26.7544328306971,23.8957310724557,24.5397674594396));
#52770=CARTESIAN_POINT('Ctrl Pts',(-26.7550978600462,23.8895080918584,24.5401518106526));
#52771=CARTESIAN_POINT('Ctrl Pts',(-26.7554349478226,23.8863084689684,24.5403495498385));
#52772=CARTESIAN_POINT('Ctrl Pts',(-26.7562341647953,23.8786117379118,24.540825505401));
#52773=CARTESIAN_POINT('Ctrl Pts',(-26.7566916228442,23.8741141603431,24.5411038689284));
#52774=CARTESIAN_POINT('Ctrl Pts',(-26.7580641451004,23.8603319682164,24.5419576162046));
#52775=CARTESIAN_POINT('Ctrl Pts',(-26.7589483505287,23.8510443921432,24.5425339721548));
#52776=CARTESIAN_POINT('Ctrl Pts',(-26.7686540843315,23.7441803514128,24.5491777037408));
#52777=CARTESIAN_POINT('Ctrl Pts',(-26.7730610902647,23.6462638720254,24.5553836380815));
#52778=CARTESIAN_POINT('Ctrl Pts',(-26.7729532790423,23.4677077078081,24.5669332623744));
#52779=CARTESIAN_POINT('Ctrl Pts',(-26.7698810632503,23.3871442905677,24.5722302431843));
#52780=CARTESIAN_POINT('Ctrl Pts',(-26.7397931034448,22.9900111221567,24.598718681482));
#52781=CARTESIAN_POINT('Ctrl Pts',(-26.6690921232823,22.6785448539725,24.6208881486241));
#52782=CARTESIAN_POINT('Ctrl Pts',(-26.5480385604194,22.3671780095951,24.6420336191901));
#52783=CARTESIAN_POINT('Ctrl Pts',(-26.541980549888,22.3519412653005,24.6430651416269));
#52784=CARTESIAN_POINT('Ctrl Pts',(-26.5344503637869,22.3334148966652,24.6443148333827));
#52785=CARTESIAN_POINT('Ctrl Pts',(-26.5330887635058,22.330081008672,24.6445395399804));
#52786=CARTESIAN_POINT('Ctrl Pts',(-26.5308370263427,22.3245939082232,24.644909069626));
#52787=CARTESIAN_POINT('Ctrl Pts',(-26.5299501425287,22.3224393785286,24.64505408917));
#52788=CARTESIAN_POINT('Ctrl Pts',(-26.5283482354139,22.3185597822403,24.6453150791071));
#52789=CARTESIAN_POINT('Ctrl Pts',(-26.5276340509093,22.3168343792954,24.6454311002531));
#52790=CARTESIAN_POINT('Ctrl Pts',(-26.526096627323,22.3131292241444,24.6456801359081));
#52791=CARTESIAN_POINT('Ctrl Pts',(-26.525272914391,22.3111496779428,24.6458131206096));
#52792=CARTESIAN_POINT('Ctrl Pts',(-26.5230154365776,22.3057397366306,24.6461763774884));
#52793=CARTESIAN_POINT('Ctrl Pts',(-26.5215777042952,22.3023109846952,24.6464064073956));
#52794=CARTESIAN_POINT('Ctrl Pts',(-26.5141336189494,22.2846438759967,24.6475906857598));
#52795=CARTESIAN_POINT('Ctrl Pts',(-26.5080307117073,22.2704460505562,24.6485391158548));
#52796=CARTESIAN_POINT('Ctrl Pts',(-26.4694082632743,22.1823467520432,24.6544069993));
#52797=CARTESIAN_POINT('Ctrl Pts',(-26.4342202860548,22.1096384905802,24.6591740889681));
#52798=CARTESIAN_POINT('Ctrl Pts',(-26.3220131426054,21.8984178762582,24.6730164145676));
#52799=CARTESIAN_POINT('Ctrl Pts',(-26.2374716622895,21.7641745519564,24.6818136922495));
#52800=CARTESIAN_POINT('Ctrl Pts',(-26.1166529820714,21.600448800247,24.6931880214801));
#52801=CARTESIAN_POINT('Ctrl Pts',(-26.0891552004595,21.5647755019798,24.6957083210066));
#52802=CARTESIAN_POINT('Ctrl Pts',(-25.9297076738589,21.3666526189152,24.7100007969063));
#52803=CARTESIAN_POINT('Ctrl Pts',(-25.7829501076783,21.2168093748268,24.7220024714878));
#52804=CARTESIAN_POINT('Ctrl Pts',(-25.6128848020216,21.0739991900047,24.7354949374918));
#52805=CARTESIAN_POINT('Ctrl Pts',(-25.6030007251963,21.0657994044616,24.7362775821494));
#52806=CARTESIAN_POINT('Ctrl Pts',(-25.5894661413546,21.0547070794872,24.7373473163125));
#52807=CARTESIAN_POINT('Ctrl Pts',(-25.5858578912978,21.0517629740937,24.7376323130007));
#52808=CARTESIAN_POINT('Ctrl Pts',(-25.5797172095469,21.0467746956253,24.7381170185827));
#52809=CARTESIAN_POINT('Ctrl Pts',(-25.5771880316916,21.0447265124571,24.7383165651992));
#52810=CARTESIAN_POINT('Ctrl Pts',(-25.5722990961098,21.0407795935046,24.7387021196412));
#52811=CARTESIAN_POINT('Ctrl Pts',(-25.5699397551325,21.0388803459056,24.738888106507));
#52812=CARTESIAN_POINT('Ctrl Pts',(-25.564348694931,21.0343925689252,24.739328669771));
#52813=CARTESIAN_POINT('Ctrl Pts',(-25.5611146633544,21.0318069408129,24.7395833623625));
#52814=CARTESIAN_POINT('Ctrl Pts',(-25.5516084950091,21.0242366851615,24.7403316004087));
#52815=CARTESIAN_POINT('Ctrl Pts',(-25.5453227772385,21.0192692322004,24.7408258324094));
#52816=CARTESIAN_POINT('Ctrl Pts',(-25.4980521271458,20.982197873776,24.7445388269298));
#52817=CARTESIAN_POINT('Ctrl Pts',(-25.456315207615,20.9510694767509,24.7477960612853));
#52818=CARTESIAN_POINT('Ctrl Pts',(-25.3154040511981,20.8511940906729,24.7587331851646));
#52819=CARTESIAN_POINT('Ctrl Pts',(-25.2131339680768,20.7870124252903,24.7665804253408));
#52820=CARTESIAN_POINT('Ctrl Pts',(-24.83639151254,20.5790801916629,24.7951218745607));
#52821=CARTESIAN_POINT('Ctrl Pts',(-24.5451386335911,20.4693099927126,24.8167011456358));
#52822=CARTESIAN_POINT('Ctrl Pts',(-24.2360699690346,20.4013133005574,24.8369786526742));
#52823=CARTESIAN_POINT('Ctrl Pts',(-24.2294215172514,20.3998726610214,24.8374135655674));
#52824=CARTESIAN_POINT('Ctrl Pts',(-24.197400640427,20.3930401988073,24.8395019080729));
#52825=CARTESIAN_POINT('Ctrl Pts',(-24.1719673667614,20.3879335791155,24.8411415318508));
#52826=CARTESIAN_POINT('Ctrl Pts',(-24.1423364936593,20.3823554575764,24.8430274432683));
#52827=CARTESIAN_POINT('Ctrl Pts',(-24.1381971945408,20.3815846153403,24.8432903465017));
#52828=CARTESIAN_POINT('Ctrl Pts',(-24.1316096872305,20.3803712074859,24.8437078573127));
#52829=CARTESIAN_POINT('Ctrl Pts',(-24.1291624747587,20.3799233642765,24.8438627648723));
#52830=CARTESIAN_POINT('Ctrl Pts',(-24.1248529395932,20.3791398697725,24.8441352108989));
#52831=CARTESIAN_POINT('Ctrl Pts',(-24.1229908379986,20.3788030246195,24.8442528180959));
#52832=CARTESIAN_POINT('Ctrl Pts',(-24.1191663189272,20.3781146658715,24.8444941337254));
#52833=CARTESIAN_POINT('Ctrl Pts',(-24.1172038756575,20.3777633338055,24.8446178314743));
#52834=CARTESIAN_POINT('Ctrl Pts',(-24.1121679294303,20.3768665809872,24.8449349382581));
#52835=CARTESIAN_POINT('Ctrl Pts',(-24.1090939486703,20.3763238026226,24.8451281954669));
#52836=CARTESIAN_POINT('Ctrl Pts',(-24.1024078575175,20.375153241913,24.845547882996));
#52837=CARTESIAN_POINT('Ctrl Pts',(-24.0987954491213,20.3745271544209,24.8457742171639));
#52838=CARTESIAN_POINT('Ctrl Pts',(-24.0883541735169,20.3727358635519,24.8464272258668));
#52839=CARTESIAN_POINT('Ctrl Pts',(-24.0815225557165,20.3715865038012,24.846853018013));
#52840=CARTESIAN_POINT('Ctrl Pts',(-24.0127774721639,20.360248563938,24.8511234306534));
#52841=CARTESIAN_POINT('Ctrl Pts',(-23.9505777715584,20.3518473693978,24.8548711967023));
#52842=CARTESIAN_POINT('Ctrl Pts',(-23.8454976721986,20.3407683302316,24.8610676541603));
#52843=CARTESIAN_POINT('Ctrl Pts',(-23.8027404482539,20.3371218685373,24.8635516411557));
#52844=CARTESIAN_POINT('Ctrl Pts',(-23.3754786246961,20.3092655974738,24.8881110827195));
#52845=CARTESIAN_POINT('Ctrl Pts',(-22.9896769918236,20.3533274079918,24.9086083127863));
#52846=CARTESIAN_POINT('Ctrl Pts',(-22.6016145333458,20.4702196020796,24.9331236884112));
#52847=CARTESIAN_POINT('Ctrl Pts',(-22.5825346962012,20.4761609484275,24.9343381554212));
#52848=CARTESIAN_POINT('Ctrl Pts',(-22.5576050008768,20.4841789937812,24.9359373636615));
#52849=CARTESIAN_POINT('Ctrl Pts',(-22.5517038574818,20.4860957790613,24.9363168281429));
#52850=CARTESIAN_POINT('Ctrl Pts',(-22.5426041594643,20.4890805842725,24.9369033951151));
#52851=CARTESIAN_POINT('Ctrl Pts',(-22.5394016615432,20.4901366103742,24.9371101010624));
#52852=CARTESIAN_POINT('Ctrl Pts',(-22.5330268401287,20.4922498115842,24.9375221113758));
#52853=CARTESIAN_POINT('Ctrl Pts',(-22.5298544926599,20.4933069015623,24.9377274127124));
#52854=CARTESIAN_POINT('Ctrl Pts',(-22.5228246993689,20.4956615320021,24.9381829530888));
#52855=CARTESIAN_POINT('Ctrl Pts',(-22.5189680593784,20.4969614445303,24.9384332704571));
#52856=CARTESIAN_POINT('Ctrl Pts',(-22.5078445224066,20.500734204556,24.9391564159176));
#52857=CARTESIAN_POINT('Ctrl Pts',(-22.5005840217141,20.5032257016678,24.939629862212));
#52858=CARTESIAN_POINT('Ctrl Pts',(-22.4516090163294,20.5202276730268,24.9428332612695));
#52859=CARTESIAN_POINT('Ctrl Pts',(-22.4101894378261,20.5355677974494,24.9455907277039));
#52860=CARTESIAN_POINT('Ctrl Pts',(-22.3117588115538,20.574341067129,24.9522642590641));
#52861=CARTESIAN_POINT('Ctrl Pts',(-22.2550809416906,20.598567340342,24.9562060089334));
#52862=CARTESIAN_POINT('Ctrl Pts',(-22.0789744392539,20.6798908879159,24.9687713324372));
#52863=CARTESIAN_POINT('Ctrl Pts',(-21.9623576921053,20.7427235660855,24.9775699975659));
#52864=CARTESIAN_POINT('Ctrl Pts',(-21.6451297509722,20.9397441156922,25.0027143190638));
#52865=CARTESIAN_POINT('Ctrl Pts',(-21.4552298247767,21.0895334345474,25.0192873671481));
#52866=CARTESIAN_POINT('Ctrl Pts',(-21.2586248342316,21.2840189178179,25.0370468952579));
#52867=CARTESIAN_POINT('Ctrl Pts',(-21.2338532677246,21.3093449020208,25.0392957069507));
#52868=CARTESIAN_POINT('Ctrl Pts',(-21.2063197868229,21.3384391810442,25.0418027066979));
#52869=CARTESIAN_POINT('Ctrl Pts',(-21.2031437277352,21.3418098057879,25.0420920100669));
#52870=CARTESIAN_POINT('Ctrl Pts',(-21.1983504121396,21.3469187803925,25.0425287843651));
#52871=CARTESIAN_POINT('Ctrl Pts',(-21.1967278098213,21.3486520722073,25.0426766657259));
#52872=CARTESIAN_POINT('Ctrl Pts',(-21.193910474493,21.3516682724116,25.0429334781585));
#52873=CARTESIAN_POINT('Ctrl Pts',(-21.1927148730194,21.3529503622909,25.0430424765985));
#52874=CARTESIAN_POINT('Ctrl Pts',(-21.1902419150939,21.3556065529986,25.043267954839));
#52875=CARTESIAN_POINT('Ctrl Pts',(-21.1889647132758,21.3569807927435,25.043384422373));
#52876=CARTESIAN_POINT('Ctrl Pts',(-21.1859312665289,21.3602504324938,25.0436610799906));
#52877=CARTESIAN_POINT('Ctrl Pts',(-21.1841760947002,21.3621468363885,25.0438211868869));
#52878=CARTESIAN_POINT('Ctrl Pts',(-21.1804560861729,21.3661758897255,25.0441605975087));
#52879=CARTESIAN_POINT('Ctrl Pts',(-21.1784918414152,21.3683090861846,25.0443398559366));
#52880=CARTESIAN_POINT('Ctrl Pts',(-21.1731574306548,21.3741180431605,25.0448268029681));
#52881=CARTESIAN_POINT('Ctrl Pts',(-21.1697928957499,21.3777989984767,25.04513406747));
#52882=CARTESIAN_POINT('Ctrl Pts',(-21.0693595185165,21.4881911721281,25.0543107079177));
#52883=CARTESIAN_POINT('Ctrl Pts',(-20.9795412084919,21.6013085658299,25.062649323268));
#52884=CARTESIAN_POINT('Ctrl Pts',(-20.6988727174088,22.0081102138774,25.0906341108799));
#52885=CARTESIAN_POINT('Ctrl Pts',(-20.5484005595743,22.3265478018212,25.1095574545639));
#52886=CARTESIAN_POINT('Ctrl Pts',(-20.446453899504,22.6825165602709,25.1319505526884));
#52887=CARTESIAN_POINT('Ctrl Pts',(-20.4410367181624,22.7021318677329,25.1331871081912));
#52888=CARTESIAN_POINT('Ctrl Pts',(-20.4341993272694,22.7278359454309,25.1348113212676));
#52889=CARTESIAN_POINT('Ctrl Pts',(-20.432610472652,22.7338796971452,25.1351934939566));
#52890=CARTESIAN_POINT('Ctrl Pts',(-20.4301890779167,22.7432004648039,25.1357833221574));
#52891=CARTESIAN_POINT('Ctrl Pts',(-20.4293440935351,22.7464742570694,25.1359905739199));
#52892=CARTESIAN_POINT('Ctrl Pts',(-20.4276738500891,22.7529877598102,25.1364030867017));
#52893=CARTESIAN_POINT('Ctrl Pts',(-20.4268484771296,22.7562274369412,25.1366083437398));
#52894=CARTESIAN_POINT('Ctrl Pts',(-20.4250330891775,22.7633996587312,25.1370629399854));
#52895=CARTESIAN_POINT('Ctrl Pts',(-20.4240454539403,22.7673327948525,25.1373123558582));
#52896=CARTESIAN_POINT('Ctrl Pts',(-20.4212263519589,22.778649909517,25.1380303766606));
#52897=CARTESIAN_POINT('Ctrl Pts',(-20.4194136137085,22.7860384857256,25.1384995862627));
#52898=CARTESIAN_POINT('Ctrl Pts',(-20.4075895282158,22.8349807334184,25.1416106249113));
#52899=CARTESIAN_POINT('Ctrl Pts',(-20.3983799463952,22.8767219673827,25.1442781858845));
#52900=CARTESIAN_POINT('Ctrl Pts',(-20.3738615614906,22.999397295641,25.1521642389251));
#52901=CARTESIAN_POINT('Ctrl Pts',(-20.3608228523623,23.0807448471439,25.1574528943659));
#52902=CARTESIAN_POINT('Ctrl Pts',(-20.3149321040827,23.4593854792597,25.1823434440813));
#52903=CARTESIAN_POINT('Ctrl Pts',(-20.3204521299649,23.7597799160756,25.2030439281942));
#52904=CARTESIAN_POINT('Ctrl Pts',(-20.3812016216365,24.1428099604202,25.2286830214828));
#52905=CARTESIAN_POINT('Ctrl Pts',(-20.39873887127,24.2299385119705,25.2344477288169));
#52906=CARTESIAN_POINT('Ctrl Pts',(-20.4213760974434,24.3224511558062,25.2404183219073));
#52907=CARTESIAN_POINT('Ctrl Pts',(-20.4229145198483,24.328658221047,25.2408181769383));
#52908=CARTESIAN_POINT('Ctrl Pts',(-20.4250739235547,24.3372610158356,25.241371300147));
#52909=CARTESIAN_POINT('Ctrl Pts',(-20.4256791911111,24.3396606177319,25.241525469492));
#52910=CARTESIAN_POINT('Ctrl Pts',(-20.4267243647189,24.3437842060544,25.2417902009331));
#52911=CARTESIAN_POINT('Ctrl Pts',(-20.4271629342986,24.3455085249292,25.2419008407081));
#52912=CARTESIAN_POINT('Ctrl Pts',(-20.4280454516656,24.3489663189318,25.2421225856057));
#52913=CARTESIAN_POINT('Ctrl Pts',(-20.4284894143094,24.3506997838299,25.2422336891917));
#52914=CARTESIAN_POINT('Ctrl Pts',(-20.4295424603684,24.3547972306367,25.2424961638094));
#52915=CARTESIAN_POINT('Ctrl Pts',(-20.430152787981,24.357160897772,25.2426474621104));
#52916=CARTESIAN_POINT('Ctrl Pts',(-20.4320677089244,24.3645423162451,25.2431195978627));
#52917=CARTESIAN_POINT('Ctrl Pts',(-20.4333817336143,24.3695576464969,25.2434398884316));
#52918=CARTESIAN_POINT('Ctrl Pts',(-20.4364583153547,24.3811857269735,25.2441813617453));
#52919=CARTESIAN_POINT('Ctrl Pts',(-20.4382298518671,24.3877961060512,25.2446020338253));
#52920=CARTESIAN_POINT('Ctrl Pts',(-20.4442667959811,24.4100389803399,25.2460148400851));
#52921=CARTESIAN_POINT('Ctrl Pts',(-20.448629122822,24.4256452332248,25.2470016274361));
#52922=CARTESIAN_POINT('Ctrl Pts',(-20.4673307877551,24.4906552957092,25.2510960504461));
#52923=CARTESIAN_POINT('Ctrl Pts',(-20.4827350188909,24.5397477507378,25.2541488470215));
#52924=CARTESIAN_POINT('Ctrl Pts',(-20.5460188343804,24.7257188774601,25.2656371221783));
#52925=CARTESIAN_POINT('Ctrl Pts',(-20.6019430438989,24.8596871939321,25.2737582007767));
#52926=CARTESIAN_POINT('Ctrl Pts',(-20.7918160437981,25.24011510201,25.2975249315984));
#52927=CARTESIAN_POINT('Ctrl Pts',(-20.9490563559416,25.4733646062996,25.3131401889811));
#52928=CARTESIAN_POINT('Ctrl Pts',(-21.1464787723451,25.6969520974813,25.3312020212581));
#52929=CARTESIAN_POINT('Ctrl Pts',(-21.1586125674031,25.7104621446849,25.3323063414239));
#52930=CARTESIAN_POINT('Ctrl Pts',(-21.1748877385455,25.7282780893167,25.3337802703979));
#52931=CARTESIAN_POINT('Ctrl Pts',(-21.1789280054581,25.7326762349881,25.3341455797796));
#52932=CARTESIAN_POINT('Ctrl Pts',(-21.1852368393966,25.7395056909266,25.3347151029217));
#52933=CARTESIAN_POINT('Ctrl Pts',(-21.1874969981602,25.7419447793979,25.3349189568964));
#52934=CARTESIAN_POINT('Ctrl Pts',(-21.1920194678573,25.7468101530787,25.3353265035709));
#52935=CARTESIAN_POINT('Ctrl Pts',(-21.1942817582284,25.7492364520269,25.3355301952603));
#52936=CARTESIAN_POINT('Ctrl Pts',(-21.199374551669,25.7546815758282,25.3359883452474));
#52937=CARTESIAN_POINT('Ctrl Pts',(-21.2022071272738,25.7576984463462,25.3362428926513));
#52938=CARTESIAN_POINT('Ctrl Pts',(-21.2105329061001,25.7665317655877,25.3369902919019));
#52939=CARTESIAN_POINT('Ctrl Pts',(-21.2160419370033,25.7723331933175,25.3374838279577));
#52940=CARTESIAN_POINT('Ctrl Pts',(-21.257360581219,25.8155216518161,25.3411780548802));
#52941=CARTESIAN_POINT('Ctrl Pts',(-21.2940430476527,25.8520596355479,25.3444167800098));
#52942=CARTESIAN_POINT('Ctrl Pts',(-21.4183058517872,25.9700079021186,25.3552644042781));
#52943=CARTESIAN_POINT('Ctrl Pts',(-21.5095273206934,26.0474204597432,25.363037371445));
#52944=CARTESIAN_POINT('Ctrl Pts',(-21.7077729659232,26.1975265358039,25.3795235101272));
#52945=CARTESIAN_POINT('Ctrl Pts',(-21.8153028012303,26.2692112433931,25.3882482032679));
#52946=CARTESIAN_POINT('Ctrl Pts',(-21.9755324628609,26.362645105302,25.4008038841439));
#52947=CARTESIAN_POINT('Ctrl Pts',(-22.0249500916317,26.3897496042714,25.4046182645467));
#52948=CARTESIAN_POINT('Ctrl Pts',(-22.0750361607755,26.4155368494319,25.4084140214669));
#52949=CARTESIAN_POINT('Origin',(-23.5502525316942,23.5502525316942,-77.3107734492734));
#52950=CARTESIAN_POINT('',(-22.0750359502314,26.4155367410314,26.9066135500179));
#52951=CARTESIAN_POINT('',(-22.0750360239718,26.4155367789973,26.65912344949));
#52952=CARTESIAN_POINT('',(-22.0750360153461,26.4155367745563,-77.3107734492734));
#52953=CARTESIAN_POINT('',(-26.7730012737579,23.5530999914162,26.0607734492728));
#52954=CARTESIAN_POINT('Ctrl Pts',(-22.0750359502314,26.4155367410314,26.9066135500179));
#52955=CARTESIAN_POINT('Ctrl Pts',(-21.9929580785884,26.3732782324952,26.9007492253846));
#52956=CARTESIAN_POINT('Ctrl Pts',(-21.9127240473899,26.3275074705045,26.8947643953227));
#52957=CARTESIAN_POINT('Ctrl Pts',(-21.6109491453685,26.1377214829904,26.8712772276802));
#52958=CARTESIAN_POINT('Ctrl Pts',(-21.4055080510349,25.9701579434784,26.8530612011559));
#52959=CARTESIAN_POINT('Ctrl Pts',(-21.2053313937181,25.7611577773525,26.8338699128938));
#52960=CARTESIAN_POINT('Ctrl Pts',(-21.1880535021463,25.7426879249033,26.8322008762093));
#52961=CARTESIAN_POINT('Ctrl Pts',(-21.1513291836319,25.7024919116327,26.8286292740379));
#52962=CARTESIAN_POINT('Ctrl Pts',(-21.1319562669122,25.6807010448331,26.8267301350214));
#52963=CARTESIAN_POINT('Ctrl Pts',(-21.1113016857495,25.6568237177462,26.8246915435628));
#52964=CARTESIAN_POINT('Ctrl Pts',(-21.1097243110865,25.6549960779077,26.8245357691453));
#52965=CARTESIAN_POINT('Ctrl Pts',(-21.0806070557029,25.6211823564755,26.8216586648387));
#52966=CARTESIAN_POINT('Ctrl Pts',(-21.0536944342395,25.5886580881064,26.8189726210674));
#52967=CARTESIAN_POINT('Ctrl Pts',(-21.0243990343653,25.5518032684836,26.8160271449043));
#52968=CARTESIAN_POINT('Ctrl Pts',(-21.021379674926,25.5479870778619,26.8157233030136));
#52969=CARTESIAN_POINT('Ctrl Pts',(-21.0168917286336,25.5422882504382,26.8152713003195));
#52970=CARTESIAN_POINT('Ctrl Pts',(-21.0154165894096,25.5404108191244,26.8151226711923));
#52971=CARTESIAN_POINT('Ctrl Pts',(-21.0127881859765,25.5370579483385,26.8148577378918));
#52972=CARTESIAN_POINT('Ctrl Pts',(-21.0116341225899,25.5355831445693,26.8147413761529));
#52973=CARTESIAN_POINT('Ctrl Pts',(-21.009184919501,25.532447625034,26.8144943514059));
#52974=CARTESIAN_POINT('Ctrl Pts',(-21.0078901254244,25.5307866498161,26.8143637133598));
#52975=CARTESIAN_POINT('Ctrl Pts',(-21.0044622465206,25.5263804305846,26.8140177321108));
#52976=CARTESIAN_POINT('Ctrl Pts',(-21.0023319665997,25.5236329925017,26.8138025899507));
#52977=CARTESIAN_POINT('Ctrl Pts',(-20.9924273492387,25.5108161575393,26.8128016650482));
#52978=CARTESIAN_POINT('Ctrl Pts',(-20.9847080900109,25.5007040500474,26.812019760336));
#52979=CARTESIAN_POINT('Ctrl Pts',(-20.7995041246043,25.2550878707824,26.7932083176412));
#52980=CARTESIAN_POINT('Ctrl Pts',(-20.6550822945767,24.9963291544905,26.7772938720883));
#52981=CARTESIAN_POINT('Ctrl Pts',(-20.4743189284497,24.5329555553363,26.749302234164));
#52982=CARTESIAN_POINT('Ctrl Pts',(-20.418703522984,24.3379421294129,26.7376682853775));
#52983=CARTESIAN_POINT('Ctrl Pts',(-20.3794399493201,24.1266409828942,26.7246084225434));
#52984=CARTESIAN_POINT('Ctrl Pts',(-20.3772123934014,24.1142492984843,26.7238410681121));
#52985=CARTESIAN_POINT('Ctrl Pts',(-20.3742671200533,24.0972950841248,26.7227890822467));
#52986=CARTESIAN_POINT('Ctrl Pts',(-20.3734864933887,24.0927434778248,26.7225064551499));
#52987=CARTESIAN_POINT('Ctrl Pts',(-20.3721742213014,24.0849920356542,26.7220247812454));
#52988=CARTESIAN_POINT('Ctrl Pts',(-20.3716376170277,24.081793036481,26.7218258924725));
#52989=CARTESIAN_POINT('Ctrl Pts',(-20.3706088181759,24.0756025188826,26.7214408125975));
#52990=CARTESIAN_POINT('Ctrl Pts',(-20.3701160133923,24.0726111047257,26.7212546411682));
#52991=CARTESIAN_POINT('Ctrl Pts',(-20.3689562580605,24.0655087076917,26.7208124033243));
#52992=CARTESIAN_POINT('Ctrl Pts',(-20.3682930550723,24.0613971261251,26.7205562180498));
#52993=CARTESIAN_POINT('Ctrl Pts',(-20.3663590197998,24.0492572767993,26.7197992872649));
#52994=CARTESIAN_POINT('Ctrl Pts',(-20.3651105952358,24.0412255181145,26.7192978306633));
#52995=CARTESIAN_POINT('Ctrl Pts',(-20.3557603508492,23.9795336910117,26.7154408996367));
#52996=CARTESIAN_POINT('Ctrl Pts',(-20.3489851130133,23.9256842046718,26.7120435728685));
#52997=CARTESIAN_POINT('Ctrl Pts',(-20.3306847416764,23.7431196538725,26.7004123636756));
#52998=CARTESIAN_POINT('Ctrl Pts',(-20.3255423204574,23.6139040441732,26.691984346246));
#52999=CARTESIAN_POINT('Ctrl Pts',(-20.3322283547432,23.2850599754964,26.6701001880548));
#53000=CARTESIAN_POINT('Ctrl Pts',(-20.3548422769434,23.0861911286024,26.6564362419457));
#53001=CARTESIAN_POINT('Ctrl Pts',(-20.4154147502456,22.7964764885113,26.636607079519));
#53002=CARTESIAN_POINT('Ctrl Pts',(-20.4393320327008,22.7031615121302,26.6302395293287));
#53003=CARTESIAN_POINT('Ctrl Pts',(-20.4774241329454,22.5781271704303,26.621851422128));
#53004=CARTESIAN_POINT('Ctrl Pts',(-20.4879814775342,22.545365316744,26.6196674153321));
#53005=CARTESIAN_POINT('Ctrl Pts',(-20.5005403941846,22.5084298374257,26.6172259407769));
#53006=CARTESIAN_POINT('Ctrl Pts',(-20.5020279274436,22.5040855227381,26.6169391048877));
#53007=CARTESIAN_POINT('Ctrl Pts',(-20.5042953516082,22.4975094441835,26.6165054286955));
#53008=CARTESIAN_POINT('Ctrl Pts',(-20.5050684134697,22.4952753578083,26.6163581860571));
#53009=CARTESIAN_POINT('Ctrl Pts',(-20.5064181496661,22.4913885738573,26.6161021775316));
#53010=CARTESIAN_POINT('Ctrl Pts',(-20.5069937121586,22.489735495633,26.6159933452904));
#53011=CARTESIAN_POINT('Ctrl Pts',(-20.5082025576762,22.4862726473117,26.6157654710598));
#53012=CARTESIAN_POINT('Ctrl Pts',(-20.5088361087086,22.4844629742256,26.6156464457261));
#53013=CARTESIAN_POINT('Ctrl Pts',(-20.5101025638427,22.4808558012765,26.6154093154137));
#53014=CARTESIAN_POINT('Ctrl Pts',(-20.5107354488026,22.4790582930473,26.61529120914));
#53015=CARTESIAN_POINT('Ctrl Pts',(-20.5129530680002,22.4727776409226,26.6148787392868));
#53016=CARTESIAN_POINT('Ctrl Pts',(-20.5145461395474,22.4682974153582,26.6145848722831));
#53017=CARTESIAN_POINT('Ctrl Pts',(-20.5291066868773,22.4276338368715,26.6119208280811));
#53018=CARTESIAN_POINT('Ctrl Pts',(-20.5427112982238,22.391679702484,26.6095880784015));
#53019=CARTESIAN_POINT('Ctrl Pts',(-20.589402146365,22.2746553121679,26.6020436972514));
#53020=CARTESIAN_POINT('Ctrl Pts',(-20.6251508737185,22.1946839801035,26.5969646629299));
#53021=CARTESIAN_POINT('Ctrl Pts',(-20.7267077887733,21.9902843190817,26.5839413803056));
#53022=CARTESIAN_POINT('Ctrl Pts',(-20.7974836718896,21.8685354363971,26.5761371601335));
#53023=CARTESIAN_POINT('Ctrl Pts',(-21.0087951290877,21.5543201850005,26.5549485094532));
#53024=CARTESIAN_POINT('Ctrl Pts',(-21.1630395322912,21.3721934311609,26.5414497116441));
#53025=CARTESIAN_POINT('Ctrl Pts',(-21.3465977419816,21.1986064023514,26.5261187780233));
#53026=CARTESIAN_POINT('Ctrl Pts',(-21.3573545353437,21.1885725541662,26.5252230144161));
#53027=CARTESIAN_POINT('Ctrl Pts',(-21.3722104315065,21.1749040992886,26.5239893564097));
#53028=CARTESIAN_POINT('Ctrl Pts',(-21.3762507841995,21.1712056706959,26.5236541859428));
#53029=CARTESIAN_POINT('Ctrl Pts',(-21.3826859585977,21.1653451701098,26.5231208926016));
#53030=CARTESIAN_POINT('Ctrl Pts',(-21.3850746448399,21.1631763514479,26.5229230562298));
#53031=CARTESIAN_POINT('Ctrl Pts',(-21.3897184776807,21.1589726672003,26.5225386700682));
#53032=CARTESIAN_POINT('Ctrl Pts',(-21.391973253086,21.1569373948351,26.52235213776));
#53033=CARTESIAN_POINT('Ctrl Pts',(-21.3973578747523,21.1520907651917,26.5219069244765));
#53034=CARTESIAN_POINT('Ctrl Pts',(-21.4004903493642,21.1492823483394,26.5216481199777));
#53035=CARTESIAN_POINT('Ctrl Pts',(-21.4098439790663,21.1409293413111,26.5208759010017));
#53036=CARTESIAN_POINT('Ctrl Pts',(-21.4160811146663,21.1354027706262,26.5203617313163));
#53037=CARTESIAN_POINT('Ctrl Pts',(-21.4675926406325,21.0901151256205,26.5161213592833));
#53038=CARTESIAN_POINT('Ctrl Pts',(-21.5139499108582,21.0516090754381,26.5123433922128));
#53039=CARTESIAN_POINT('Ctrl Pts',(-21.6313654016923,20.9595178955684,26.5028571202663));
#53040=CARTESIAN_POINT('Ctrl Pts',(-21.7036120563247,20.9075360553845,26.4970904530061));
#53041=CARTESIAN_POINT('Ctrl Pts',(-21.9423581700751,20.750330919305,26.4782675546142));
#53042=CARTESIAN_POINT('Ctrl Pts',(-22.1163721542714,20.6573543243392,26.4648652542607));
#53043=CARTESIAN_POINT('Ctrl Pts',(-22.4463253771609,20.5181805077695,26.4406986617962));
#53044=CARTESIAN_POINT('Ctrl Pts',(-22.5994050352915,20.4667449448191,26.4299403539007));
#53045=CARTESIAN_POINT('Ctrl Pts',(-22.7648687209819,20.4246519273755,26.4192023010467));
#53046=CARTESIAN_POINT('Ctrl Pts',(-22.7740375066119,20.4223623309353,26.4186101397418));
#53047=CARTESIAN_POINT('Ctrl Pts',(-22.7863588439786,20.4193430049712,26.4178183351114));
#53048=CARTESIAN_POINT('Ctrl Pts',(-22.7895024959003,20.4185776740635,26.4176166606129));
#53049=CARTESIAN_POINT('Ctrl Pts',(-22.7944287538752,20.4173862181472,26.417301173751));
#53050=CARTESIAN_POINT('Ctrl Pts',(-22.7962105688713,20.416956880145,26.4171871749746));
#53051=CARTESIAN_POINT('Ctrl Pts',(-22.7996328374256,20.4161353542496,26.4169684379536));
#53052=CARTESIAN_POINT('Ctrl Pts',(-22.8012732219503,20.4157429367227,26.4168636870527));
#53053=CARTESIAN_POINT('Ctrl Pts',(-22.8046603373505,20.4149354718866,26.4166475907927));
#53054=CARTESIAN_POINT('Ctrl Pts',(-22.806407101814,20.4145205976362,26.4165362558449));
#53055=CARTESIAN_POINT('Ctrl Pts',(-22.8103506211426,20.4135874524147,26.4162851458211));
#53056=CARTESIAN_POINT('Ctrl Pts',(-22.8125475785152,20.4130700284056,26.4161454198842));
#53057=CARTESIAN_POINT('Ctrl Pts',(-22.8228763173456,20.4106488695705,26.4154893006147));
#53058=CARTESIAN_POINT('Ctrl Pts',(-22.8310150339363,20.4087744181468,26.4149745883705));
#53059=CARTESIAN_POINT('Ctrl Pts',(-22.9198829470903,20.3886704525339,26.4093783977253));
#53060=CARTESIAN_POINT('Ctrl Pts',(-23.0012865531326,20.373523688671,26.4044682024706));
#53061=CARTESIAN_POINT('Ctrl Pts',(-23.2164576959292,20.3420069567183,26.3918396630189));
#53062=CARTESIAN_POINT('Ctrl Pts',(-23.3508265510868,20.3308592929678,26.3843007720226));
#53063=CARTESIAN_POINT('Ctrl Pts',(-23.7633768062159,20.3225693458991,26.3612379940522));
#53064=CARTESIAN_POINT('Ctrl Pts',(-24.0407564939307,20.3529504402609,26.3457327227698));
#53065=CARTESIAN_POINT('Ctrl Pts',(-24.3282978166272,20.4227794657512,26.3278131684815));
#53066=CARTESIAN_POINT('Ctrl Pts',(-24.3457715376222,20.4271784476771,26.3267173110875));
#53067=CARTESIAN_POINT('Ctrl Pts',(-24.3689680703198,20.4332254428591,26.3252530622308));
#53068=CARTESIAN_POINT('Ctrl Pts',(-24.3747247589748,20.4347431750384,26.324888899305));
#53069=CARTESIAN_POINT('Ctrl Pts',(-24.3836864500191,20.4371324733262,26.3243207636741));
#53070=CARTESIAN_POINT('Ctrl Pts',(-24.3868943870748,20.4379930631215,26.3241171478555));
#53071=CARTESIAN_POINT('Ctrl Pts',(-24.393304109499,20.4397232186575,26.3237098136718));
#53072=CARTESIAN_POINT('Ctrl Pts',(-24.3965058939394,20.4405927726757,26.3235060958981));
#53073=CARTESIAN_POINT('Ctrl Pts',(-24.4037049024312,20.442559851299,26.3230474928176));
#53074=CARTESIAN_POINT('Ctrl Pts',(-24.4077013576639,20.4436601452545,26.3227925176064));
#53075=CARTESIAN_POINT('Ctrl Pts',(-24.4194375208071,20.4469156879891,26.3220426039857));
#53076=CARTESIAN_POINT('Ctrl Pts',(-24.4271712629328,20.4490921605225,26.3215469742951));
#53077=CARTESIAN_POINT('Ctrl Pts',(-24.484599635823,20.4654859695957,26.3178555970315));
#53078=CARTESIAN_POINT('Ctrl Pts',(-24.5339514967645,20.4808673981169,26.3146219455358));
#53079=CARTESIAN_POINT('Ctrl Pts',(-24.6960868671618,20.5357117892988,26.3037850313776));
#53080=CARTESIAN_POINT('Ctrl Pts',(-24.8070346801265,20.5802550226636,26.2960178664573));
#53081=CARTESIAN_POINT('Ctrl Pts',(-24.9894401422818,20.6655402183768,26.2826683935778));
#53082=CARTESIAN_POINT('Ctrl Pts',(-25.062283644121,20.7030456688475,26.2771728916489));
#53083=CARTESIAN_POINT('Ctrl Pts',(-25.2044124806302,20.7832181463539,26.2661606963856));
#53084=CARTESIAN_POINT('Ctrl Pts',(-25.2736720646164,20.8258169203984,26.2606483207847));
#53085=CARTESIAN_POINT('Ctrl Pts',(-25.4652580335461,20.9538853888959,26.24507414678));
#53086=CARTESIAN_POINT('Ctrl Pts',(-25.5833783245481,21.0453019704712,26.2350697739671));
#53087=CARTESIAN_POINT('Ctrl Pts',(-25.6978602503146,21.1473551116283,26.2252534180174));
#53088=CARTESIAN_POINT('Ctrl Pts',(-25.7009652328373,21.1501338258846,26.2249870881038));
#53089=CARTESIAN_POINT('Ctrl Pts',(-25.707790833634,21.1562660808022,26.2244014395974));
#53090=CARTESIAN_POINT('Ctrl Pts',(-25.7115090501165,21.1596222981147,26.2240822901335));
#53091=CARTESIAN_POINT('Ctrl Pts',(-25.7220667018086,21.1691968377854,26.2231757804333));
#53092=CARTESIAN_POINT('Ctrl Pts',(-25.7288872954969,21.1754359961367,26.2225897803661));
#53093=CARTESIAN_POINT('Ctrl Pts',(-25.746106009399,21.1913234798342,26.2211096994371));
#53094=CARTESIAN_POINT('Ctrl Pts',(-25.7564675882277,21.2010113969258,26.2202183767931));
#53095=CARTESIAN_POINT('Ctrl Pts',(-25.7694854376405,21.2133449779553,26.2190981025864));
#53096=CARTESIAN_POINT('Ctrl Pts',(-25.7722013046289,21.2159270924396,26.2188643586138));
#53097=CARTESIAN_POINT('Ctrl Pts',(-25.7764847900753,21.2200138710563,26.2184956651177));
#53098=CARTESIAN_POINT('Ctrl Pts',(-25.7780553904031,21.2215153832414,26.2183604718891));
#53099=CARTESIAN_POINT('Ctrl Pts',(-25.7809710768147,21.2243084626499,26.2181094870075));
#53100=CARTESIAN_POINT('Ctrl Pts',(-25.7823165521092,21.2255996008963,26.2179936635171));
#53101=CARTESIAN_POINT('Ctrl Pts',(-25.7849524194104,21.228133416825,26.2177667503164));
#53102=CARTESIAN_POINT('Ctrl Pts',(-25.7862428899571,21.2293759969358,26.2176556540014));
#53103=CARTESIAN_POINT('Ctrl Pts',(-25.7891471434974,21.232177141822,26.2174056167674));
#53104=CARTESIAN_POINT('Ctrl Pts',(-25.7907603385318,21.2337363190449,26.2172667237632));
#53105=CARTESIAN_POINT('Ctrl Pts',(-25.7948198819631,21.2376681361355,26.2169171819277));
#53106=CARTESIAN_POINT('Ctrl Pts',(-25.7972641048379,21.2400429812672,26.2167067042058));
#53107=CARTESIAN_POINT('Ctrl Pts',(-25.8288304974965,21.2708108719084,26.2139881026536));
#53108=CARTESIAN_POINT('Ctrl Pts',(-25.8574180644152,21.2997504965842,26.2115222281589));
#53109=CARTESIAN_POINT('Ctrl Pts',(-25.9492087658228,21.3962596959981,26.2035601964081));
#53110=CARTESIAN_POINT('Ctrl Pts',(-26.0100553949186,21.4660143221509,26.198210151161));
#53111=CARTESIAN_POINT('Ctrl Pts',(-26.1111589222809,21.5925255183622,26.1889948487992));
#53112=CARTESIAN_POINT('Ctrl Pts',(-26.1527349483438,21.6481425484671,26.1850950506388));
#53113=CARTESIAN_POINT('Ctrl Pts',(-26.254611860594,21.7940256160188,26.1751346025429));
#53114=CARTESIAN_POINT('Ctrl Pts',(-26.3122073117956,21.8860717009852,26.1690984212877));
#53115=CARTESIAN_POINT('Ctrl Pts',(-26.4604574783865,22.1519646583804,26.1519436513561));
#53116=CARTESIAN_POINT('Ctrl Pts',(-26.540048547062,22.3313989015759,26.1406583979027));
#53117=CARTESIAN_POINT('Ctrl Pts',(-26.606945467091,22.5290234585465,26.1279815015744));
#53118=CARTESIAN_POINT('Ctrl Pts',(-26.6109665920806,22.5411390820017,26.127203528246));
#53119=CARTESIAN_POINT('Ctrl Pts',(-26.6163525516445,22.5576953260091,26.126139219398));
#53120=CARTESIAN_POINT('Ctrl Pts',(-26.6177799612247,22.5621155940141,26.1258549494743));
#53121=CARTESIAN_POINT('Ctrl Pts',(-26.6201901744655,22.5696348683179,26.1253711788046));
#53122=CARTESIAN_POINT('Ctrl Pts',(-26.6211778572934,22.5727323136388,26.1251718390381));
#53123=CARTESIAN_POINT('Ctrl Pts',(-26.6230768532445,22.5787189864511,26.124786445186));
#53124=CARTESIAN_POINT('Ctrl Pts',(-26.623988782861,22.5816080154713,26.1246004116717));
#53125=CARTESIAN_POINT('Ctrl Pts',(-26.6261395423733,22.5884553270966,26.1241593682908));
#53126=CARTESIAN_POINT('Ctrl Pts',(-26.627374805036,22.5924147166732,26.1239042414472));
#53127=CARTESIAN_POINT('Ctrl Pts',(-26.6309838726525,22.6040619036301,26.123153450393));
#53128=CARTESIAN_POINT('Ctrl Pts',(-26.6333365218117,22.6117561769875,26.1226570924428));
#53129=CARTESIAN_POINT('Ctrl Pts',(-26.6385768769098,22.6291269837464,26.1215356200054));
#53130=CARTESIAN_POINT('Ctrl Pts',(-26.6414479545181,22.6388084080591,26.120909965218));
#53131=CARTESIAN_POINT('Ctrl Pts',(-26.6504721290202,22.6697715371631,26.1189069518365));
#53132=CARTESIAN_POINT('Ctrl Pts',(-26.6564512067717,22.6911029028437,26.1175239382748));
#53133=CARTESIAN_POINT('Ctrl Pts',(-26.736013732696,22.9866476313332,26.0983168638294));
#53134=CARTESIAN_POINT('Ctrl Pts',(-26.7732476569941,23.2692853830247,26.0792408559392));
#53135=CARTESIAN_POINT('Ctrl Pts',(-26.7730013173331,23.5530502384158,26.0600382396916));
#53136=CARTESIAN_POINT('Ctrl Pts',(-22.0750360153461,26.4155367745563,25.653793035611));
#53137=CARTESIAN_POINT('Ctrl Pts',(-22.1636145467195,26.4611422019415,25.6599527331432));
#53138=CARTESIAN_POINT('Ctrl Pts',(-22.2544190940411,26.5026924933022,25.6661124306754));
#53139=CARTESIAN_POINT('Ctrl Pts',(-22.3470417866287,26.5399684823254,25.6722721282076));
#53140=CARTESIAN_POINT('Ctrl Pts',(-22.4417132505225,26.5780689990598,25.6785680754125));
#53141=CARTESIAN_POINT('Ctrl Pts',(-22.5382838620969,26.6117036240226,25.6848640226175));
#53142=CARTESIAN_POINT('Ctrl Pts',(-22.6362924949834,26.6406885225854,25.6911599698225));
#53143=CARTESIAN_POINT('Ctrl Pts',(-22.7320460985457,26.6690065227915,25.6973110568743));
#53144=CARTESIAN_POINT('Ctrl Pts',(-22.8291718214375,26.6928863357309,25.7034621439261));
#53145=CARTESIAN_POINT('Ctrl Pts',(-22.9272218171399,26.7122060878398,25.709613230978));
#53146=CARTESIAN_POINT('Ctrl Pts',(-23.025250537181,26.7315216477965,25.7157629833184));
#53147=CARTESIAN_POINT('Ctrl Pts',(-23.1242027053701,26.7462790294842,25.7219127356589));
#53148=CARTESIAN_POINT('Ctrl Pts',(-23.2236194282402,26.7564072968651,25.7280624879993));
#53149=CARTESIAN_POINT('Ctrl Pts',(-23.3230411756617,26.7665360761317,25.7342125511501));
#53150=CARTESIAN_POINT('Ctrl Pts',(-23.4229270921102,26.7720352328171,25.7403626143009));
#53151=CARTESIAN_POINT('Ctrl Pts',(-23.5228133023489,26.7728857176452,25.7465126774517));
#53152=CARTESIAN_POINT('Ctrl Pts',(-23.6268430232608,26.7737714825481,25.7529178594247));
#53153=CARTESIAN_POINT('Ctrl Pts',(-23.7308725498221,26.7696145252937,25.7593230413976));
#53154=CARTESIAN_POINT('Ctrl Pts',(-23.8343797818175,26.7604533460106,25.7657282233706));
#53155=CARTESIAN_POINT('Ctrl Pts',(-23.9339131021665,26.7516438882096,25.7718874937609));
#53156=CARTESIAN_POINT('Ctrl Pts',(-24.032963063677,26.7382075168608,25.7780467641512));
#53157=CARTESIAN_POINT('Ctrl Pts',(-24.1310738740573,26.7202311011416,25.7842060345414));
#53158=CARTESIAN_POINT('Ctrl Pts',(-24.2292546594097,26.7022418642135,25.7903696978704));
#53159=CARTESIAN_POINT('Ctrl Pts',(-24.3264945383187,26.6797062357736,25.7965333611993));
#53160=CARTESIAN_POINT('Ctrl Pts',(-24.4223514623728,26.652761358049,25.8026970245283));
#53161=CARTESIAN_POINT('Ctrl Pts',(-24.5183509782933,26.6257763984999,25.8088698566081));
#53162=CARTESIAN_POINT('Ctrl Pts',(-24.6129630252629,26.5943692422234,25.815042688688));
#53163=CARTESIAN_POINT('Ctrl Pts',(-24.7057644460702,26.5587255294515,25.8212155207679));
#53164=CARTESIAN_POINT('Ctrl Pts',(-24.7165855111701,26.5545693114438,25.8219353008877));
#53165=CARTESIAN_POINT('Ctrl Pts',(-24.7273819850634,26.5503555421446,25.8226550810075));
#53166=CARTESIAN_POINT('Ctrl Pts',(-24.7381532190843,26.5460845562573,25.8233748611273));
#53167=CARTESIAN_POINT('Ctrl Pts',(-24.8305162082613,26.5094609881022,25.8295469527638));
#53168=CARTESIAN_POINT('Ctrl Pts',(-24.9213465968592,26.468497520667,25.8357190444003));
#53169=CARTESIAN_POINT('Ctrl Pts',(-25.0102075054303,26.4233430344739,25.8418911360368));
#53170=CARTESIAN_POINT('Ctrl Pts',(-25.0989480162784,26.3782497281339,25.8480548651009));
#53171=CARTESIAN_POINT('Ctrl Pts',(-25.1857239670718,26.3289768845462,25.854218594165));
#53172=CARTESIAN_POINT('Ctrl Pts',(-25.2701170629948,26.2757219511656,25.8603823232291));
#53173=CARTESIAN_POINT('Ctrl Pts',(-25.3544207523686,26.2225234363792,25.8665395224019));
#53174=CARTESIAN_POINT('Ctrl Pts',(-25.4363462402853,26.1653514494029,25.8726967215746));
#53175=CARTESIAN_POINT('Ctrl Pts',(-25.5154993923776,26.1044495364442,25.8788539207474));
#53176=CARTESIAN_POINT('Ctrl Pts',(-25.594594688316,26.0435921390905,25.885006619381));
#53177=CARTESIAN_POINT('Ctrl Pts',(-25.6709213340261,25.9790105002969,25.8911593180145));
#53178=CARTESIAN_POINT('Ctrl Pts',(-25.7441145614843,25.9109911781236,25.8973120166481));
#53179=CARTESIAN_POINT('Ctrl Pts',(-25.8172800339653,25.8429976489752,25.9034623821695));
#53180=CARTESIAN_POINT('Ctrl Pts',(-25.8873141312736,25.771569322023,25.909612747691));
#53181=CARTESIAN_POINT('Ctrl Pts',(-25.9538862370753,25.6970321134995,25.9157631132124));
#53182=CARTESIAN_POINT('Ctrl Pts',(-26.020450908631,25.6225032287015,25.9219127919096));
#53183=CARTESIAN_POINT('Ctrl Pts',(-26.0835540679393,25.5448664765553,25.9280624706069));
#53184=CARTESIAN_POINT('Ctrl Pts',(-26.1429036530184,25.4644828536765,25.9342121493041));
#53185=CARTESIAN_POINT('Ctrl Pts',(-26.2022624880375,25.384086702594,25.9403627864606));
#53186=CARTESIAN_POINT('Ctrl Pts',(-26.257866328792,25.3009431799375,25.9465134236172));
#53187=CARTESIAN_POINT('Ctrl Pts',(-26.3094655212953,25.2154435839512,25.9526640607737));
#53188=CARTESIAN_POINT('Ctrl Pts',(-26.361119914063,25.1298525214112,25.9588212778161));
#53189=CARTESIAN_POINT('Ctrl Pts',(-26.4087608787012,25.0419007249948,25.9649784948585));
#53190=CARTESIAN_POINT('Ctrl Pts',(-26.4521840362903,24.952005400474,25.9711357119009));
#53191=CARTESIAN_POINT('Ctrl Pts',(-26.4956314194697,24.8620599237436,25.9772963640278));
#53192=CARTESIAN_POINT('Ctrl Pts',(-26.5348561388962,24.7701691591104,25.9834570161547));
#53193=CARTESIAN_POINT('Ctrl Pts',(-26.5697022492787,24.6767697155308,25.9896176682817));
#53194=CARTESIAN_POINT('Ctrl Pts',(-26.60460666956,24.5832139815631,25.9957886293641));
#53195=CARTESIAN_POINT('Ctrl Pts',(-26.6351177125498,24.4881449397316,26.0019595904466));
#53196=CARTESIAN_POINT('Ctrl Pts',(-26.6611294783929,24.3920138903929,26.0081305515291));
#53197=CARTESIAN_POINT('Ctrl Pts',(-26.6809847330347,24.3186353095189,26.0128409585201));
#53198=CARTESIAN_POINT('Ctrl Pts',(-26.6982194975119,24.2446382499281,26.0175513655111));
#53199=CARTESIAN_POINT('Ctrl Pts',(-26.7128069574075,24.1702259721747,26.0222617725022));
#53200=CARTESIAN_POINT('Ctrl Pts',(-26.7407090601528,24.027894199937,26.031271583722));
#53201=CARTESIAN_POINT('Ctrl Pts',(-26.7590096370179,23.8836232293146,26.0402813949418));
#53202=CARTESIAN_POINT('Ctrl Pts',(-26.7675014364373,23.7384732729247,26.0492912061617));
#53203=CARTESIAN_POINT('Ctrl Pts',(-26.7711087967177,23.6768128212911,26.0531186205321));
#53204=CARTESIAN_POINT('Ctrl Pts',(-26.7729465872607,23.614994050472,26.0569460349024));
#53205=CARTESIAN_POINT('Ctrl Pts',(-26.7730012737579,23.5530999914162,26.0607734492728));
#53206=CARTESIAN_POINT('',(-26.7730026521799,23.5484313703039,25.8164188470677));
#53207=CARTESIAN_POINT('Ctrl Pts',(-22.0750361607755,26.4155368494318,25.4084140214669));
#53208=CARTESIAN_POINT('Ctrl Pts',(-22.1782012019014,26.4686522616209,25.4162323515028));
#53209=CARTESIAN_POINT('Ctrl Pts',(-22.2842020110658,26.5161790568714,25.4239739883152));
#53210=CARTESIAN_POINT('Ctrl Pts',(-22.4005170944886,26.5609498395686,25.4320063618042));
#53211=CARTESIAN_POINT('Ctrl Pts',(-22.4084642392242,26.5639727167167,25.4325528924445));
#53212=CARTESIAN_POINT('Ctrl Pts',(-22.4470690419364,26.578482307905,25.4351964379665));
#53213=CARTESIAN_POINT('Ctrl Pts',(-22.4778899708359,26.5895333896195,25.4372723875315));
#53214=CARTESIAN_POINT('Ctrl Pts',(-22.5136306701617,26.6017370765861,25.4396356913983));
#53215=CARTESIAN_POINT('Ctrl Pts',(-22.5183897750248,26.6033496581765,25.439949486294));
#53216=CARTESIAN_POINT('Ctrl Pts',(-22.5254457836472,26.6057221428194,25.4404133847563));
#53217=CARTESIAN_POINT('Ctrl Pts',(-22.5277397735785,26.606490590965,25.4405639933222));
#53218=CARTESIAN_POINT('Ctrl Pts',(-22.5318145470433,26.6078504704126,25.4408311408059));
#53219=CARTESIAN_POINT('Ctrl Pts',(-22.5335949809529,26.6084429293028,25.4409477410013));
#53220=CARTESIAN_POINT('Ctrl Pts',(-22.537317802918,26.609678128708,25.441191280742));
#53221=CARTESIAN_POINT('Ctrl Pts',(-22.5392602806046,26.6103205728849,25.4413182023298));
#53222=CARTESIAN_POINT('Ctrl Pts',(-22.5443879424781,26.6120110516273,25.4416528475676));
#53223=CARTESIAN_POINT('Ctrl Pts',(-22.5475741635347,26.6130559691499,25.4418603856741));
#53224=CARTESIAN_POINT('Ctrl Pts',(-22.5617158009588,26.6176692703367,25.4427797526757));
#53225=CARTESIAN_POINT('Ctrl Pts',(-22.5726888549657,26.6211839187399,25.4434884318982));
#53226=CARTESIAN_POINT('Ctrl Pts',(-22.6016788638739,26.6302982312593,25.4453489329733));
#53227=CARTESIAN_POINT('Ctrl Pts',(-22.6197268368355,26.6357987530522,25.4464952512587));
#53228=CARTESIAN_POINT('Ctrl Pts',(-22.7011298730619,26.659828924516,25.4516162941497));
#53229=CARTESIAN_POINT('Ctrl Pts',(-22.7650010829774,26.6765692228039,25.4555007957022));
#53230=CARTESIAN_POINT('Ctrl Pts',(-22.9192179937474,26.7119633715666,25.4646601615215));
#53231=CARTESIAN_POINT('Ctrl Pts',(-23.0099389049544,26.7287243312666,25.4698714113415));
#53232=CARTESIAN_POINT('Ctrl Pts',(-23.4117502720847,26.7852561583849,25.4926386317475));
#53233=CARTESIAN_POINT('Ctrl Pts',(-23.7269098273122,26.7833939247232,25.5098773080211));
#53234=CARTESIAN_POINT('Ctrl Pts',(-24.0553628773759,26.7332279385035,25.5299902788652));
#53235=CARTESIAN_POINT('Ctrl Pts',(-24.0738666893163,26.7302363512263,25.5311299332376));
#53236=CARTESIAN_POINT('Ctrl Pts',(-24.098305665065,26.7260661146142,25.5326441616666));
#53237=CARTESIAN_POINT('Ctrl Pts',(-24.1042653687441,26.7250318824605,25.5330141337573));
#53238=CARTESIAN_POINT('Ctrl Pts',(-24.1135119849006,26.7234004184462,25.5335892704376));
#53239=CARTESIAN_POINT('Ctrl Pts',(-24.1168009618476,26.7228148398264,25.5337940633004));
#53240=CARTESIAN_POINT('Ctrl Pts',(-24.1233833800959,26.7216323254471,25.534204368993));
#53241=CARTESIAN_POINT('Ctrl Pts',(-24.1266768138055,26.7210353707535,25.5344098821989));
#53242=CARTESIAN_POINT('Ctrl Pts',(-24.1340264653712,26.7196913728574,25.5348690046711));
#53243=CARTESIAN_POINT('Ctrl Pts',(-24.1380821858119,26.7189416724907,25.5351226984782));
#53244=CARTESIAN_POINT('Ctrl Pts',(-24.149935983983,26.7167269553963,25.535865174975));
#53245=CARTESIAN_POINT('Ctrl Pts',(-24.1577300622579,26.7152409308774,25.5363546282118));
#53246=CARTESIAN_POINT('Ctrl Pts',(-24.2146960346144,26.7041615828578,25.5399413233347));
#53247=CARTESIAN_POINT('Ctrl Pts',(-24.2636414370363,26.6934520615622,25.5430741426074));
#53248=CARTESIAN_POINT('Ctrl Pts',(-24.4223347989986,26.6548316156612,25.5534068045175));
#53249=CARTESIAN_POINT('Ctrl Pts',(-24.5308550985955,26.6222799612034,25.560752369686));
#53250=CARTESIAN_POINT('Ctrl Pts',(-24.7567814515174,26.5413192307102,25.576624419732));
#53251=CARTESIAN_POINT('Ctrl Pts',(-24.8734996539564,26.491545677167,25.5851744107897));
#53252=CARTESIAN_POINT('Ctrl Pts',(-25.0424115468596,26.4074214870876,25.5979458933017));
#53253=CARTESIAN_POINT('Ctrl Pts',(-25.097040522891,26.378219998058,25.6021408588672));
#53254=CARTESIAN_POINT('Ctrl Pts',(-25.2251595773539,26.3049112614838,25.6120944940392));
#53255=CARTESIAN_POINT('Ctrl Pts',(-25.2978025412706,26.2594090276105,25.6178326945842));
#53256=CARTESIAN_POINT('Ctrl Pts',(-25.3770751519917,26.2052371480579,25.6241399427837));
#53257=CARTESIAN_POINT('Ctrl Pts',(-25.3855731016868,26.199369858123,25.6248166637968));
#53258=CARTESIAN_POINT('Ctrl Pts',(-25.4002707129897,26.1891174300168,25.6259879225723));
#53259=CARTESIAN_POINT('Ctrl Pts',(-25.4064833100331,26.1847510650331,25.6264832687521));
#53260=CARTESIAN_POINT('Ctrl Pts',(-25.4134175068567,26.1798408366279,25.6270363940962));
#53261=CARTESIAN_POINT('Ctrl Pts',(-25.4141543272033,26.179318615843,25.6270951716979));
#53262=CARTESIAN_POINT('Ctrl Pts',(-25.4173055060694,26.177083229976,25.6273465603261));
#53263=CARTESIAN_POINT('Ctrl Pts',(-25.4197177300441,26.1753670432597,25.6275390305066));
#53264=CARTESIAN_POINT('Ctrl Pts',(-25.426080558524,26.1708269644805,25.6280467963155));
#53265=CARTESIAN_POINT('Ctrl Pts',(-25.4300271657867,26.167997452343,25.6283618234762));
#53266=CARTESIAN_POINT('Ctrl Pts',(-25.4371436187509,26.162870933195,25.6289299991719));
#53267=CARTESIAN_POINT('Ctrl Pts',(-25.4403156960136,26.1605770558581,25.6291833017423));
#53268=CARTESIAN_POINT('Ctrl Pts',(-25.4800553960131,26.1317290046662,25.6323571544011));
#53269=CARTESIAN_POINT('Ctrl Pts',(-25.5160671063167,26.1044125608642,25.63523846938));
#53270=CARTESIAN_POINT('Ctrl Pts',(-25.5557593159857,26.0729672806974,25.6384091669173));
#53271=CARTESIAN_POINT('Ctrl Pts',(-25.5600155961446,26.0695777573212,25.6387490999583));
#53272=CARTESIAN_POINT('Ctrl Pts',(-25.56604804123,26.0647487541318,25.6392307673663));
#53273=CARTESIAN_POINT('Ctrl Pts',(-25.5678312597824,26.063318162545,25.6393731353698));
#53274=CARTESIAN_POINT('Ctrl Pts',(-25.571097159376,26.0606923696666,25.6396338470576));
#53275=CARTESIAN_POINT('Ctrl Pts',(-25.5725803054489,26.0594977498564,25.6397522328894));
#53276=CARTESIAN_POINT('Ctrl Pts',(-25.575424061759,26.057203049299,25.6399792003166));
#53277=CARTESIAN_POINT('Ctrl Pts',(-25.5767848340962,26.0561031759387,25.6400877968286));
#53278=CARTESIAN_POINT('Ctrl Pts',(-25.5796492185803,26.0537841166751,25.6403163693369));
#53279=CARTESIAN_POINT('Ctrl Pts',(-25.5811526301685,26.052564682447,25.6404363272161));
#53280=CARTESIAN_POINT('Ctrl Pts',(-25.5865619176092,26.0481690617834,25.6408678988277));
#53281=CARTESIAN_POINT('Ctrl Pts',(-25.5904614752363,26.0449850572294,25.6411789478602));
#53282=CARTESIAN_POINT('Ctrl Pts',(-25.6341933784183,26.0091066639358,25.6446666381402));
#53283=CARTESIAN_POINT('Ctrl Pts',(-25.6732462992263,25.9754682549462,25.6477756331427));
#53284=CARTESIAN_POINT('Ctrl Pts',(-25.7656509124129,25.8919315624595,25.655165822624));
#53285=CARTESIAN_POINT('Ctrl Pts',(-25.8181469271391,25.8411272723573,25.6593931983228));
#53286=CARTESIAN_POINT('Ctrl Pts',(-26.0792168655783,25.5706920896179,25.6808496932107));
#53287=CARTESIAN_POINT('Ctrl Pts',(-26.2577930040983,25.3242517755272,25.6971805666352));
#53288=CARTESIAN_POINT('Ctrl Pts',(-26.4088533530779,25.0385174521646,25.7161160433643));
#53289=CARTESIAN_POINT('Ctrl Pts',(-26.4181875845009,25.020449673942,25.7173125935699));
#53290=CARTESIAN_POINT('Ctrl Pts',(-26.4294071580061,24.9982190525818,25.7187844820835));
#53291=CARTESIAN_POINT('Ctrl Pts',(-26.4314555944326,24.9941387179275,25.7190546263805));
#53292=CARTESIAN_POINT('Ctrl Pts',(-26.4352951885162,24.9864498234203,25.7195636632746));
#53293=CARTESIAN_POINT('Ctrl Pts',(-26.437088265474,24.9828422281563,25.7198024940292));
#53294=CARTESIAN_POINT('Ctrl Pts',(-26.4407208614247,24.9754990842243,25.7202886191982));
#53295=CARTESIAN_POINT('Ctrl Pts',(-26.4425599141645,24.9717633145413,25.7205359280052));
#53296=CARTESIAN_POINT('Ctrl Pts',(-26.4676050521694,24.9206379274791,25.723920442057));
#53297=CARTESIAN_POINT('Ctrl Pts',(-26.4896499872633,24.8726911743882,25.7270947500384));
#53298=CARTESIAN_POINT('Ctrl Pts',(-26.5139557150827,24.816213475613,25.730841764078));
#53299=CARTESIAN_POINT('Ctrl Pts',(-26.5173717918601,24.8081861405744,25.731374516148));
#53300=CARTESIAN_POINT('Ctrl Pts',(-26.5224176604426,24.7961940969756,25.7321706953239));
#53301=CARTESIAN_POINT('Ctrl Pts',(-26.5240722236245,24.7922398006507,25.7324332786025));
#53302=CARTESIAN_POINT('Ctrl Pts',(-26.5270106111623,24.7851777137988,25.732902324462));
#53303=CARTESIAN_POINT('Ctrl Pts',(-26.5282974724468,24.782071187096,25.7331086834715));
#53304=CARTESIAN_POINT('Ctrl Pts',(-26.5310017230855,24.7755140288462,25.7335443282901));
#53305=CARTESIAN_POINT('Ctrl Pts',(-26.5324179868285,24.7720629410458,25.7337736519299));
#53306=CARTESIAN_POINT('Ctrl Pts',(-26.5361462471653,24.7629329831652,25.7343804447327));
#53307=CARTESIAN_POINT('Ctrl Pts',(-26.5384480263752,24.7572499808242,25.7347582593922));
#53308=CARTESIAN_POINT('Ctrl Pts',(-26.5488198081606,24.7314309418125,25.7364752888727));
#53309=CARTESIAN_POINT('Ctrl Pts',(-26.5567024411274,24.7112206850176,25.7378208149143));
#53310=CARTESIAN_POINT('Ctrl Pts',(-26.6131846603531,24.5619723526261,25.7477700388037));
#53311=CARTESIAN_POINT('Ctrl Pts',(-26.6536557769766,24.4300306002522,25.7566450565172));
#53312=CARTESIAN_POINT('Ctrl Pts',(-26.7438013880824,24.0509953044662,25.7823544411515));
#53313=CARTESIAN_POINT('Ctrl Pts',(-26.7731438782448,23.8001313092259,25.7996825319716));
#53314=CARTESIAN_POINT('Ctrl Pts',(-26.7730020198273,23.548436151331,25.8164196296698));
#53315=CARTESIAN_POINT('Ctrl Pts',(-26.7730020171705,23.5484314435376,25.8164199427262));
#53316=CARTESIAN_POINT('Ctrl Pts',(-26.7729508853726,23.4579443493913,25.8224371045826));
#53317=CARTESIAN_POINT('Ctrl Pts',(-26.7690887550542,23.3674885436758,25.8283579034823));
#53318=CARTESIAN_POINT('Ctrl Pts',(-26.7601466049889,23.2622858317644,25.8350467304567));
#53319=CARTESIAN_POINT('Ctrl Pts',(-26.7587645555835,23.2472749821746,25.8359963976571));
#53320=CARTESIAN_POINT('Ctrl Pts',(-26.7568975818284,23.2284453095156,25.8371812592684));
#53321=CARTESIAN_POINT('Ctrl Pts',(-26.7565111022516,23.2246172374036,25.8374218089649));
#53322=CARTESIAN_POINT('Ctrl Pts',(-26.7558695388139,23.2183744487913,25.8378135425975));
#53323=CARTESIAN_POINT('Ctrl Pts',(-26.7556185811685,23.215959326234,25.8379649560027));
#53324=CARTESIAN_POINT('Ctrl Pts',(-26.7551715203555,23.2117037697322,25.8382315126332));
#53325=CARTESIAN_POINT('Ctrl Pts',(-26.7549765611708,23.209863220692,25.8383467203063));
#53326=CARTESIAN_POINT('Ctrl Pts',(-26.7545902212932,23.2062456598311,25.8385730011819));
#53327=CARTESIAN_POINT('Ctrl Pts',(-26.7543989475674,23.2044686359091,25.8386840805099));
#53328=CARTESIAN_POINT('Ctrl Pts',(-26.7540146535614,23.2009260606441,25.8389053720425));
#53329=CARTESIAN_POINT('Ctrl Pts',(-26.753821652477,23.1991605134247,25.8390155851057));
#53330=CARTESIAN_POINT('Ctrl Pts',(-26.7533575324538,23.1949470541703,25.8392784323874));
#53331=CARTESIAN_POINT('Ctrl Pts',(-26.7530850662469,23.1924992871875,25.8394309898803));
#53332=CARTESIAN_POINT('Ctrl Pts',(-26.7522531170804,23.1851023976257,25.8398915825659));
#53333=CARTESIAN_POINT('Ctrl Pts',(-26.7516849635077,23.1801542278042,25.8401991293191));
#53334=CARTESIAN_POINT('Ctrl Pts',(-26.7457771444037,23.1297334770029,25.8433273527712));
#53335=CARTESIAN_POINT('Ctrl Pts',(-26.7394801605924,23.0843754169231,25.8460949625909));
#53336=CARTESIAN_POINT('Ctrl Pts',(-26.7299435750956,23.0250019500297,25.8496746154563));
#53337=CARTESIAN_POINT('Ctrl Pts',(-26.7275742756882,23.0108548549804,25.8505243159767));
#53338=CARTESIAN_POINT('Ctrl Pts',(-26.7186564954646,22.9597054103027,25.8535862476331));
#53339=CARTESIAN_POINT('Ctrl Pts',(-26.7115552407843,22.9228013674714,25.855776071186));
#53340=CARTESIAN_POINT('Ctrl Pts',(-26.7010859111894,22.8730957865562,25.858709353206));
#53341=CARTESIAN_POINT('Ctrl Pts',(-26.6982823340377,22.8601796272125,25.8594700902017));
#53342=CARTESIAN_POINT('Ctrl Pts',(-26.634697175194,22.5756949260541,25.8761998852543));
#53343=CARTESIAN_POINT('Ctrl Pts',(-26.5390753079627,22.3131125466077,25.8912303861599));
#53344=CARTESIAN_POINT('Ctrl Pts',(-26.3729198947162,21.9928609820453,25.9120516557774));
#53345=CARTESIAN_POINT('Ctrl Pts',(-26.3321443967014,21.921143722296,25.9168842439819));
#53346=CARTESIAN_POINT('Ctrl Pts',(-26.2661969957937,21.8148622900479,25.9243613402459));
#53347=CARTESIAN_POINT('Ctrl Pts',(-26.2430131545674,21.7791021750985,25.9269337495212));
#53348=CARTESIAN_POINT('Ctrl Pts',(-26.2148670523715,21.7375184637387,25.9299965108269));
#53349=CARTESIAN_POINT('Ctrl Pts',(-26.2105839889066,21.7312385457294,25.9304609971542));
#53350=CARTESIAN_POINT('Ctrl Pts',(-26.2039827469513,21.7216328496996,25.9311744941909));
#53351=CARTESIAN_POINT('Ctrl Pts',(-26.2016804238545,21.7182961650793,25.9314229004665));
#53352=CARTESIAN_POINT('Ctrl Pts',(-26.1976525415448,21.7124821801752,25.9318567204163));
#53353=CARTESIAN_POINT('Ctrl Pts',(-26.1959297819071,21.710002938653,25.9320420269041));
#53354=CARTESIAN_POINT('Ctrl Pts',(-26.1920452790639,21.704429438859,25.9324593170946));
#53355=CARTESIAN_POINT('Ctrl Pts',(-26.1898815810993,21.7013365543057,25.932691375537));
#53356=CARTESIAN_POINT('Ctrl Pts',(-26.1840754730514,21.6930680145503,25.9333130876674));
#53357=CARTESIAN_POINT('Ctrl Pts',(-26.1804232559083,21.6878992951381,25.9337031179205));
#53358=CARTESIAN_POINT('Ctrl Pts',(-26.1645753422939,21.6656104867645,25.9353910931808));
#53359=CARTESIAN_POINT('Ctrl Pts',(-26.1522277577916,21.6485994916803,25.9366948948896));
#53360=CARTESIAN_POINT('Ctrl Pts',(-25.9284107165336,21.3465128610276,25.9601319614637));
#53361=CARTESIAN_POINT('Ctrl Pts',(-25.6714746131869,21.0982360920666,25.9843574315045));
#53362=CARTESIAN_POINT('Ctrl Pts',(-25.3215930923605,20.8570389379362,26.0129041989637));
#53363=CARTESIAN_POINT('Ctrl Pts',(-25.262498594258,20.8190877059489,26.0175830382128));
#53364=CARTESIAN_POINT('Ctrl Pts',(-25.1598770501091,20.757824004178,26.0254161594825));
#53365=CARTESIAN_POINT('Ctrl Pts',(-25.116968479097,20.7335257255886,26.0286083576628));
#53366=CARTESIAN_POINT('Ctrl Pts',(-25.0527088621478,20.6990597879695,26.0332495058558));
#53367=CARTESIAN_POINT('Ctrl Pts',(-25.0317781726435,20.6881279813832,26.0347398539775));
#53368=CARTESIAN_POINT('Ctrl Pts',(-25.006966932198,20.6755145394527,26.0364797891443));
#53369=CARTESIAN_POINT('Ctrl Pts',(-25.0032015948466,20.6736096291008,26.0367431205578));
#53370=CARTESIAN_POINT('Ctrl Pts',(-24.997781423168,20.6708808836015,26.0371211377086));
#53371=CARTESIAN_POINT('Ctrl Pts',(-24.9961296250947,20.6700510786162,26.0372361990192));
#53372=CARTESIAN_POINT('Ctrl Pts',(-24.9928776025667,20.6684208799986,26.0374624534011));
#53373=CARTESIAN_POINT('Ctrl Pts',(-24.9912774225979,20.667620396356,26.0375736521762));
#53374=CARTESIAN_POINT('Ctrl Pts',(-24.9880849262335,20.6660266854137,26.0377952406598));
#53375=CARTESIAN_POINT('Ctrl Pts',(-24.986492623176,20.6652334456572,26.0379056311315));
#53376=CARTESIAN_POINT('Ctrl Pts',(-24.9826845529548,20.6633403081693,26.0381693267425));
#53377=CARTESIAN_POINT('Ctrl Pts',(-24.9804681705585,20.6622416403862,26.0383225540196));
#53378=CARTESIAN_POINT('Ctrl Pts',(-24.9725232307422,20.65831469756,26.0388709336001));
#53379=CARTESIAN_POINT('Ctrl Pts',(-24.966787481921,20.6555008818441,26.0392651816654));
#53380=CARTESIAN_POINT('Ctrl Pts',(-24.8815195804946,20.6139846913807,26.0451022255994));
#53381=CARTESIAN_POINT('Ctrl Pts',(-24.8004268548213,20.5785512889499,26.0503459803637));
#53382=CARTESIAN_POINT('Ctrl Pts',(-24.5866808818096,20.4954569826156,26.0636413162355));
#53383=CARTESIAN_POINT('Ctrl Pts',(-24.4521771527532,20.4530769175625,26.0715059635698));
#53384=CARTESIAN_POINT('Ctrl Pts',(-24.2990708004479,20.4156602589407,26.080312777012));
#53385=CARTESIAN_POINT('Ctrl Pts',(-24.2827866248665,20.4118148123829,26.0812475719305));
#53386=CARTESIAN_POINT('Ctrl Pts',(-24.2476428875576,20.4038041753138,26.0832620936102));
#53387=CARTESIAN_POINT('Ctrl Pts',(-24.2287743622989,20.3996813628218,26.0843418869993));
#53388=CARTESIAN_POINT('Ctrl Pts',(-24.1877018276741,20.3910930120451,26.0866901734016));
#53389=CARTESIAN_POINT('Ctrl Pts',(-24.1654855533632,20.3866914377482,26.087958993486));
#53390=CARTESIAN_POINT('Ctrl Pts',(-24.1164953718931,20.3775208840379,26.0907565717696));
#53391=CARTESIAN_POINT('Ctrl Pts',(-24.0897038804668,20.372855911909,26.0922862662849));
#53392=CARTESIAN_POINT('Ctrl Pts',(-24.0292965634924,20.3631237453181,26.0957392088235));
#53393=CARTESIAN_POINT('Ctrl Pts',(-23.9956534046897,20.3582482898633,26.0976650064516));
#53394=CARTESIAN_POINT('Ctrl Pts',(-23.8500453583177,20.3394940669868,26.106026815534));
#53395=CARTESIAN_POINT('Ctrl Pts',(-23.7374810321793,20.3309688461738,26.1125632030665));
#53396=CARTESIAN_POINT('Ctrl Pts',(-23.5747295719455,20.3272077474001,26.1222593671421));
#53397=CARTESIAN_POINT('Ctrl Pts',(-23.524732648307,20.3272159016937,26.1252707345463));
#53398=CARTESIAN_POINT('Ctrl Pts',(-23.4668301252195,20.3285726666372,26.1288025168985));
#53399=CARTESIAN_POINT('Ctrl Pts',(-23.4589028552326,20.3287876963043,26.1292870008526));
#53400=CARTESIAN_POINT('Ctrl Pts',(-23.446854931912,20.3291590058179,26.1300248052801));
#53401=CARTESIAN_POINT('Ctrl Pts',(-23.4427336116098,20.329293940272,26.1302774550432));
#53402=CARTESIAN_POINT('Ctrl Pts',(-23.4352675432404,20.3295527292253,26.1307356301612));
#53403=CARTESIAN_POINT('Ctrl Pts',(-23.4319227024627,20.3296738854614,26.1309410704571));
#53404=CARTESIAN_POINT('Ctrl Pts',(-23.4252392494024,20.3299263983091,26.1313519210974));
#53405=CARTESIAN_POINT('Ctrl Pts',(-23.4219006404829,20.3300577366543,26.1315573306216));
#53406=CARTESIAN_POINT('Ctrl Pts',(-23.4125160651701,20.33044153634,26.1321352187284));
#53407=CARTESIAN_POINT('Ctrl Pts',(-23.4064706203145,20.3307058336053,26.1325080688415));
#53408=CARTESIAN_POINT('Ctrl Pts',(-23.3816833132228,20.3318594497573,26.1340392228559));
#53409=CARTESIAN_POINT('Ctrl Pts',(-23.3629489410805,20.3328953938795,26.1352021260462));
#53410=CARTESIAN_POINT('Ctrl Pts',(-23.0328407098786,20.3540421758558,26.1557955897981));
#53411=CARTESIAN_POINT('Ctrl Pts',(-22.7260704502414,20.419101869334,26.1767891579853));
#53412=CARTESIAN_POINT('Ctrl Pts',(-22.3291076746122,20.5657403549522,26.2054076519512));
#53413=CARTESIAN_POINT('Ctrl Pts',(-22.2267549729426,20.6096973362167,26.212902006021));
#53414=CARTESIAN_POINT('Ctrl Pts',(-22.080044480779,20.6819201472966,26.2236416928645));
#53415=CARTESIAN_POINT('Ctrl Pts',(-22.033775885001,20.7061108957067,26.2270277861206));
#53416=CARTESIAN_POINT('Ctrl Pts',(-21.973682145234,20.7394135871053,26.2314051842126));
#53417=CARTESIAN_POINT('Ctrl Pts',(-21.9593128938971,20.7475215686462,26.2324502988225));
#53418=CARTESIAN_POINT('Ctrl Pts',(-21.9389925914881,20.7591941188688,26.2339253063251));
#53419=CARTESIAN_POINT('Ctrl Pts',(-21.9329900867101,20.7626679419748,26.2343606475492));
#53420=CARTESIAN_POINT('Ctrl Pts',(-21.9224717266498,20.768800631288,26.235122797681));
#53421=CARTESIAN_POINT('Ctrl Pts',(-21.9179510820558,20.7714511710396,26.2354501276282));
#53422=CARTESIAN_POINT('Ctrl Pts',(-21.9113244313939,20.7753582529353,26.2359295853252));
#53423=CARTESIAN_POINT('Ctrl Pts',(-21.9092133918809,20.7766061739298,26.2360822709452));
#53424=CARTESIAN_POINT('Ctrl Pts',(-21.9055668368967,20.7787674208277,26.2363459193962));
#53425=CARTESIAN_POINT('Ctrl Pts',(-21.9040306551724,20.7796796148139,26.2364569566381));
#53426=CARTESIAN_POINT('Ctrl Pts',(-21.9009697398967,20.7815006493575,26.2366781432636));
#53427=CARTESIAN_POINT('Ctrl Pts',(-21.8994450017755,20.7824094703078,26.23678829354));
#53428=CARTESIAN_POINT('Ctrl Pts',(-21.8958097904295,20.7845803122976,26.2370508397822));
#53429=CARTESIAN_POINT('Ctrl Pts',(-21.8937000054565,20.7858434922836,26.237203159424));
#53430=CARTESIAN_POINT('Ctrl Pts',(-21.887334559195,20.7896645449613,26.2376625625859));
#53431=CARTESIAN_POINT('Ctrl Pts',(-21.8830833360512,20.7922298541891,26.237969161151));
#53432=CARTESIAN_POINT('Ctrl Pts',(-21.8401342756492,20.8182821312639,26.2410646191982));
#53433=CARTESIAN_POINT('Ctrl Pts',(-21.8019270363729,20.8425736007255,26.2438016120632));
#53434=CARTESIAN_POINT('Ctrl Pts',(-21.7587193739858,20.871340341008,26.2468926952176));
#53435=CARTESIAN_POINT('Ctrl Pts',(-21.7532081049598,20.875034239612,26.2472868939016));
#53436=CARTESIAN_POINT('Ctrl Pts',(-21.7429709576011,20.8819415428572,26.2480190468523));
#53437=CARTESIAN_POINT('Ctrl Pts',(-21.7382421554303,20.8851505414584,26.2483572197616));
#53438=CARTESIAN_POINT('Ctrl Pts',(-21.7287239888428,20.891646680387,26.2490378948187));
#53439=CARTESIAN_POINT('Ctrl Pts',(-21.7239349257831,20.8949342253009,26.2493803753845));
#53440=CARTESIAN_POINT('Ctrl Pts',(-21.7106782230547,20.9040873761319,26.2503284774512));
#53441=CARTESIAN_POINT('Ctrl Pts',(-21.7022297191454,20.9099806979159,26.2509327882723));
#53442=CARTESIAN_POINT('Ctrl Pts',(-21.471097318003,21.0728618928778,26.267471975173));
#53443=CARTESIAN_POINT('Ctrl Pts',(-21.2691691651441,21.2574291729343,26.2821763424851));
#53444=CARTESIAN_POINT('Ctrl Pts',(-21.0636437686147,21.4996589771405,26.3002437269313));
#53445=CARTESIAN_POINT('Ctrl Pts',(-21.0351537744921,21.5347041933496,26.3028292636445));
#53446=CARTESIAN_POINT('Ctrl Pts',(-20.9572621302943,21.6347418075215,26.3101520601756));
#53447=CARTESIAN_POINT('Ctrl Pts',(-20.909582384188,21.7010256262659,26.3149388155384));
#53448=CARTESIAN_POINT('Ctrl Pts',(-20.8415811627579,21.8035606909281,26.3222981495056));
#53449=CARTESIAN_POINT('Ctrl Pts',(-20.8193581632005,21.8385140365042,26.3247991245502));
#53450=CARTESIAN_POINT('Ctrl Pts',(-20.7938928180428,21.8803257169855,26.3277853293147));
#53451=CARTESIAN_POINT('Ctrl Pts',(-20.7899925993808,21.8867803972526,26.3282461699932));
#53452=CARTESIAN_POINT('Ctrl Pts',(-20.7840373339764,21.8967146963561,26.3289552283832));
#53453=CARTESIAN_POINT('Ctrl Pts',(-20.7819660978303,21.9001846201139,26.3292028534018));
#53454=CARTESIAN_POINT('Ctrl Pts',(-20.7783595289985,21.9062525769688,26.3296358164609));
#53455=CARTESIAN_POINT('Ctrl Pts',(-20.776821305579,21.908848893511,26.3298210487214));
#53456=CARTESIAN_POINT('Ctrl Pts',(-20.7736069030334,21.9142917962262,26.3302093262963));
#53457=CARTESIAN_POINT('Ctrl Pts',(-20.7719314502176,21.9171388053268,26.3304123977856));
#53458=CARTESIAN_POINT('Ctrl Pts',(-20.7672942192439,21.925046398501,26.3309763667922));
#53459=CARTESIAN_POINT('Ctrl Pts',(-20.7643418813443,21.9301124785677,26.3313376068516));
#53460=CARTESIAN_POINT('Ctrl Pts',(-20.7527043721091,21.9502077923815,26.3327702530183));
#53461=CARTESIAN_POINT('Ctrl Pts',(-20.7441269858956,21.9652988177824,26.3338455518609));
#53462=CARTESIAN_POINT('Ctrl Pts',(-20.604211203519,22.2161623937189,26.3517133179768));
#53463=CARTESIAN_POINT('Ctrl Pts',(-20.5029078199641,22.4673937076515,26.3696398798604));
#53464=CARTESIAN_POINT('Ctrl Pts',(-20.3947658789947,22.8773471990841,26.3983271450534));
#53465=CARTESIAN_POINT('Ctrl Pts',(-20.3661836330995,23.0290925691655,26.4087996564778));
#53466=CARTESIAN_POINT('Ctrl Pts',(-20.3425919101127,23.2343762220688,26.4223761162917));
#53467=CARTESIAN_POINT('Ctrl Pts',(-20.3378787413927,23.2865864023653,26.4257774236067));
#53468=CARTESIAN_POINT('Ctrl Pts',(-20.3333326568256,23.3557540542404,26.4301957996883));
#53469=CARTESIAN_POINT('Ctrl Pts',(-20.3323569729912,23.3726255610273,26.4312666528582));
#53470=CARTESIAN_POINT('Ctrl Pts',(-20.3311619197704,23.3965546928009,26.4327749678696));
#53471=CARTESIAN_POINT('Ctrl Pts',(-20.3308329789276,23.4036062262066,26.4332181532725));
#53472=CARTESIAN_POINT('Ctrl Pts',(-20.3303662246702,23.4143719041332,26.4338927419989));
#53473=CARTESIAN_POINT('Ctrl Pts',(-20.3302116648933,23.4180852453961,26.4341250555352));
#53474=CARTESIAN_POINT('Ctrl Pts',(-20.3299376401443,23.4249547379125,26.4345541320549));
#53475=CARTESIAN_POINT('Ctrl Pts',(-20.3298163908399,23.4281108076669,26.434750993828));
#53476=CARTESIAN_POINT('Ctrl Pts',(-20.3296259007067,23.4332667611471,26.4350721528332));
#53477=CARTESIAN_POINT('Ctrl Pts',(-20.329553882903,23.4352665305314,26.4351966066318));
#53478=CARTESIAN_POINT('Ctrl Pts',(-20.3294174855085,23.439154656967,26.435438365469));
#53479=CARTESIAN_POINT('Ctrl Pts',(-20.3293529042015,23.4410429985073,26.4355556813166));
#53480=CARTESIAN_POINT('Ctrl Pts',(-20.3292077262896,23.4454001331403,26.4358261480431));
#53481=CARTESIAN_POINT('Ctrl Pts',(-20.3291283071146,23.4478689693839,26.4359792321525));
#53482=CARTESIAN_POINT('Ctrl Pts',(-20.3289230664606,23.4544858319803,26.436389078038));
#53483=CARTESIAN_POINT('Ctrl Pts',(-20.3288024179608,23.4586340317031,26.4366455491805));
#53484=CARTESIAN_POINT('Ctrl Pts',(-20.3280166577791,23.4875739453529,26.4384316359929));
#53485=CARTESIAN_POINT('Ctrl Pts',(-20.3276297049508,23.5123732634944,26.4399458782074));
#53486=CARTESIAN_POINT('Ctrl Pts',(-20.3274949192065,23.545590006885,26.4419552038689));
#53487=CARTESIAN_POINT('Ctrl Pts',(-20.3274937302696,23.5540047335916,26.4424625993338));
#53488=CARTESIAN_POINT('Ctrl Pts',(-20.3287910921516,23.897644647954,26.4631207995232));
#53489=CARTESIAN_POINT('Ctrl Pts',(-20.3823499015367,24.230669251405,26.4808845516421));
#53490=CARTESIAN_POINT('Ctrl Pts',(-20.5306399230803,24.6853666129075,26.5082645827915));
#53491=CARTESIAN_POINT('Ctrl Pts',(-20.5839377275395,24.8181296907315,26.5166449296376));
#53492=CARTESIAN_POINT('Ctrl Pts',(-20.6504526389001,24.9564496240396,26.525985672453));
#53493=CARTESIAN_POINT('Ctrl Pts',(-20.6550884118073,24.9659694509557,26.5266317015572));
#53494=CARTESIAN_POINT('Ctrl Pts',(-20.6618230931939,24.9796280855771,26.52756320589));
#53495=CARTESIAN_POINT('Ctrl Pts',(-20.6638841920089,24.9837855458026,26.5278473572804));
#53496=CARTESIAN_POINT('Ctrl Pts',(-20.6674778999292,24.9909952742325,26.52834120121));
#53497=CARTESIAN_POINT('Ctrl Pts',(-20.6690063992213,24.9940495921184,26.5285507492604));
#53498=CARTESIAN_POINT('Ctrl Pts',(-20.671955476274,24.9999192407727,26.5289540998495));
#53499=CARTESIAN_POINT('Ctrl Pts',(-20.6733753372938,25.0027349291338,26.5291478770076));
#53500=CARTESIAN_POINT('Ctrl Pts',(-20.676731053913,25.0093653370977,26.5296048681879));
#53501=CARTESIAN_POINT('Ctrl Pts',(-20.6786703734999,25.0131782887401,26.5298682040771));
#53502=CARTESIAN_POINT('Ctrl Pts',(-20.6844233627734,25.0244338890179,26.5306471412632));
#53503=CARTESIAN_POINT('Ctrl Pts',(-20.6882583951468,25.031865524338,26.5311634963251));
#53504=CARTESIAN_POINT('Ctrl Pts',(-20.7222966830311,25.0972006008343,26.5357212872539));
#53505=CARTESIAN_POINT('Ctrl Pts',(-20.7542226796643,25.1541847834394,26.539823700541));
#53506=CARTESIAN_POINT('Ctrl Pts',(-20.7968742523831,25.2251651263367,26.5451032752371));
#53507=CARTESIAN_POINT('Ctrl Pts',(-20.8060147407314,25.2400995888116,26.5462238669561));
#53508=CARTESIAN_POINT('Ctrl Pts',(-20.827624559586,25.2747696948877,26.5488482074975));
#53509=CARTESIAN_POINT('Ctrl Pts',(-20.8401874214789,25.2944456333662,26.5503551129478));
#53510=CARTESIAN_POINT('Ctrl Pts',(-21.009939759627,25.5540495088953,26.5704712282139));
#53511=CARTESIAN_POINT('Ctrl Pts',(-21.1982566725404,25.7720672581973,26.5902098732285));
#53512=CARTESIAN_POINT('Ctrl Pts',(-21.500121990606,26.0395642895927,26.61714482083));
#53513=CARTESIAN_POINT('Ctrl Pts',(-21.5915157639048,26.1121005769147,26.6247910373325));
#53514=CARTESIAN_POINT('Ctrl Pts',(-21.6905218161546,26.182274898733,26.6324024396636));
#53515=CARTESIAN_POINT('Ctrl Pts',(-21.6943988807157,26.1850100730518,26.632699470715));
#53516=CARTESIAN_POINT('Ctrl Pts',(-21.7005741331281,26.1893461694144,26.6331709165183));
#53517=CARTESIAN_POINT('Ctrl Pts',(-21.7028683732334,26.1909526619607,26.6333457068405));
#53518=CARTESIAN_POINT('Ctrl Pts',(-21.707184314151,26.1939664299064,26.6336738393385));
#53519=CARTESIAN_POINT('Ctrl Pts',(-21.7092055374242,26.1953743805137,26.6338272276013));
#53520=CARTESIAN_POINT('Ctrl Pts',(-21.7127632412056,26.1978465646149,26.6340967202118));
#53521=CARTESIAN_POINT('Ctrl Pts',(-21.7142990355046,26.1989117803926,26.6342128924386));
#53522=CARTESIAN_POINT('Ctrl Pts',(-21.7172848148989,26.2009788506142,26.6344384288426));
#53523=CARTESIAN_POINT('Ctrl Pts',(-21.7187346924914,26.2019808498573,26.6345478031317));
#53524=CARTESIAN_POINT('Ctrl Pts',(-21.7221698010991,26.2043506656441,26.6348065960362));
#53525=CARTESIAN_POINT('Ctrl Pts',(-21.7241557498159,26.2057174472671,26.6349559433114));
#53526=CARTESIAN_POINT('Ctrl Pts',(-21.7300790025364,26.2097841969204,26.6354005874578));
#53527=CARTESIAN_POINT('Ctrl Pts',(-21.7340207966459,26.2124776611459,26.6356954415186));
#53528=CARTESIAN_POINT('Ctrl Pts',(-21.7705143757065,26.2372952839188,26.6384157165108));
#53529=CARTESIAN_POINT('Ctrl Pts',(-21.8034646952323,26.2588313571608,26.640802007203));
#53530=CARTESIAN_POINT('Ctrl Pts',(-21.8436192101301,26.2840383748532,26.6436374568762));
#53531=CARTESIAN_POINT('Ctrl Pts',(-21.8504514119529,26.2882916998571,26.6441174127544));
#53532=CARTESIAN_POINT('Ctrl Pts',(-21.9282636129354,26.3363294741816,26.6495562721621));
#53533=CARTESIAN_POINT('Ctrl Pts',(-22.0008974377762,26.3773658832763,26.6543754537399));
#53534=CARTESIAN_POINT('Ctrl Pts',(-22.0750360239718,26.4155367789973,26.65912344949));
#53535=CARTESIAN_POINT('Origin',(-23.5502525316942,23.5502525316942,-77.3107734492734));
#53536=CARTESIAN_POINT('',(-22.0750359096863,26.4155367201564,28.1544576001758));
#53537=CARTESIAN_POINT('',(-22.0750363456406,26.4155369446113,27.9044917472066));
#53538=CARTESIAN_POINT('',(-22.0750360153461,26.4155367745563,-77.3107734492734));
#53539=CARTESIAN_POINT('Ctrl Pts',(-22.0750359096863,26.4155367201564,28.1544576001758));
#53540=CARTESIAN_POINT('Ctrl Pts',(-22.0173610161786,26.3858422968536,28.1508130336123));
#53541=CARTESIAN_POINT('Ctrl Pts',(-21.9605783308166,26.3544042342411,28.147146887933));
#53542=CARTESIAN_POINT('Ctrl Pts',(-21.8139335814481,26.2673234195051,28.1374047791776));
#53543=CARTESIAN_POINT('Ctrl Pts',(-21.725814651594,26.2089554106126,28.1312676286439));
#53544=CARTESIAN_POINT('Ctrl Pts',(-21.6151963563925,26.1275921543532,28.1230816475099));
#53545=CARTESIAN_POINT('Ctrl Pts',(-21.5899458145721,26.1084392723183,28.1211787550168));
#53546=CARTESIAN_POINT('Ctrl Pts',(-21.5493190360085,26.0766685882533,28.1180582775673));
#53547=CARTESIAN_POINT('Ctrl Pts',(-21.5337695635216,26.064275076638,28.116849559606));
#53548=CARTESIAN_POINT('Ctrl Pts',(-21.5149129043682,26.0489581192546,28.1153656889653));
#53549=CARTESIAN_POINT('Ctrl Pts',(-21.5114954922939,26.0461705483487,28.1150960325726));
#53550=CARTESIAN_POINT('Ctrl Pts',(-21.5048860999888,26.0407566591471,28.1145730798338));
#53551=CARTESIAN_POINT('Ctrl Pts',(-21.5016934280596,26.0381311958314,28.1143198184589));
#53552=CARTESIAN_POINT('Ctrl Pts',(-21.4961708627039,26.0335719287158,28.1138806067314));
#53553=CARTESIAN_POINT('Ctrl Pts',(-21.4938386217162,26.0316409658685,28.1136947723112));
#53554=CARTESIAN_POINT('Ctrl Pts',(-21.4890028942939,26.0276257587959,28.1133087284619));
#53555=CARTESIAN_POINT('Ctrl Pts',(-21.4864998406915,26.0255410005985,28.1131084981407));
#53556=CARTESIAN_POINT('Ctrl Pts',(-21.4804175589649,26.020459514816,28.1126209541279));
#53557=CARTESIAN_POINT('Ctrl Pts',(-21.4768416802161,26.0174588048731,28.1123334773196));
#53558=CARTESIAN_POINT('Ctrl Pts',(-21.4633962231729,26.0061261319661,28.1112493662718));
#53559=CARTESIAN_POINT('Ctrl Pts',(-21.4535703483005,25.9977427169577,28.1104506155047));
#53560=CARTESIAN_POINT('Ctrl Pts',(-21.2931250632783,25.8591758927199,28.097299958417));
#53561=CARTESIAN_POINT('Ctrl Pts',(-21.1548655263839,25.7153959273152,28.0843552146197));
#53562=CARTESIAN_POINT('Ctrl Pts',(-20.9439116789241,25.4509123084033,28.0617143503197));
#53563=CARTESIAN_POINT('Ctrl Pts',(-20.8642081442081,25.3365009864723,28.052243409155));
#53564=CARTESIAN_POINT('Ctrl Pts',(-20.7059727727865,25.0747037153209,28.0315968215798));
#53565=CARTESIAN_POINT('Ctrl Pts',(-20.6309612746357,24.9256190392759,28.0204799171011));
#53566=CARTESIAN_POINT('Ctrl Pts',(-20.5654721316602,24.7656708210194,28.0096487939715));
#53567=CARTESIAN_POINT('Ctrl Pts',(-20.5631499427657,24.7599524032211,28.0092629792111));
#53568=CARTESIAN_POINT('Ctrl Pts',(-20.5598499533574,24.7517586966472,28.0087122209064));
#53569=CARTESIAN_POINT('Ctrl Pts',(-20.5588587876135,24.7492888584753,28.0085464726686));
#53570=CARTESIAN_POINT('Ctrl Pts',(-20.5571598152388,24.7450400520763,28.0082618029513));
#53571=CARTESIAN_POINT('Ctrl Pts',(-20.5564505335901,24.7432616785064,28.0081427914274));
#53572=CARTESIAN_POINT('Ctrl Pts',(-20.5550948643458,24.7398538024068,28.0079149993422));
#53573=CARTESIAN_POINT('Ctrl Pts',(-20.5544482224511,24.7382244069143,28.0078062031804));
#53574=CARTESIAN_POINT('Ctrl Pts',(-20.5529286098187,24.7343861858119,28.0075501959818));
#53575=CARTESIAN_POINT('Ctrl Pts',(-20.5520567492775,24.7321769175348,28.0074030526787));
#53576=CARTESIAN_POINT('Ctrl Pts',(-20.5494905172452,24.7256530513864,28.0069691700418));
#53577=CARTESIAN_POINT('Ctrl Pts',(-20.5478030019938,24.72133573595,28.0066828441839));
#53578=CARTESIAN_POINT('Ctrl Pts',(-20.533254790345,24.6838776446877,28.0042054654805));
#53579=CARTESIAN_POINT('Ctrl Pts',(-20.5209332921916,24.6505281650556,28.002046283905));
#53580=CARTESIAN_POINT('Ctrl Pts',(-20.4622774570331,24.4833087876907,27.99141776957));
#53581=CARTESIAN_POINT('Ctrl Pts',(-20.4242481289722,24.3466755483813,27.9833565032334));
#53582=CARTESIAN_POINT('Ctrl Pts',(-20.3544882634718,24.0120530095176,27.9641479484535));
#53583=CARTESIAN_POINT('Ctrl Pts',(-20.3319837974126,23.8127659183084,27.9531200035869));
#53584=CARTESIAN_POINT('Ctrl Pts',(-20.3270751115492,23.559408322583,27.9385617576426));
#53585=CARTESIAN_POINT('Ctrl Pts',(-20.3273643030219,23.5061211762853,27.9354720028141));
#53586=CARTESIAN_POINT('Ctrl Pts',(-20.3314137106725,23.3721758928065,27.9276089674043));
#53587=CARTESIAN_POINT('Ctrl Pts',(-20.3368840182894,23.2916104316228,27.9227907573503));
#53588=CARTESIAN_POINT('Ctrl Pts',(-20.34638380226,23.2017769897238,27.9172896845966));
#53589=CARTESIAN_POINT('Ctrl Pts',(-20.3474378828565,23.1922185097991,27.916702736562));
#53590=CARTESIAN_POINT('Ctrl Pts',(-20.349049137874,23.1781843463816,27.9158385252525));
#53591=CARTESIAN_POINT('Ctrl Pts',(-20.3495729590479,23.1737048241652,27.9155623163305));
#53592=CARTESIAN_POINT('Ctrl Pts',(-20.3505073497667,23.1658571017385,27.9150777797798));
#53593=CARTESIAN_POINT('Ctrl Pts',(-20.3509138397677,23.1624884152029,27.9148695814567));
#53594=CARTESIAN_POINT('Ctrl Pts',(-20.3517123552837,23.1559576485855,27.9144655484549));
#53595=CARTESIAN_POINT('Ctrl Pts',(-20.3521037518254,23.1527954941931,27.9142697338976));
#53596=CARTESIAN_POINT('Ctrl Pts',(-20.3530475624256,23.1452619625111,27.9138027824446));
#53597=CARTESIAN_POINT('Ctrl Pts',(-20.3536042520764,23.1408911354199,27.913531510425));
#53598=CARTESIAN_POINT('Ctrl Pts',(-20.3556178021786,23.1253364109476,27.912564846354));
#53599=CARTESIAN_POINT('Ctrl Pts',(-20.3571243931712,23.114159135202,27.9118678808545));
#53600=CARTESIAN_POINT('Ctrl Pts',(-20.3804019490563,22.948055789844,27.9014749709444));
#53601=CARTESIAN_POINT('Ctrl Pts',(-20.4133635458321,22.794932862244,27.891419448734));
#53602=CARTESIAN_POINT('Ctrl Pts',(-20.509851285762,22.4653294160291,27.8687168338023));
#53603=CARTESIAN_POINT('Ctrl Pts',(-20.577920443092,22.2907564304879,27.8559823817404));
#53604=CARTESIAN_POINT('Ctrl Pts',(-20.7333658911343,21.9760328111633,27.8323004933322));
#53605=CARTESIAN_POINT('Ctrl Pts',(-20.8171289436563,21.8347150689012,27.8213683440384));
#53606=CARTESIAN_POINT('Ctrl Pts',(-20.9147367392574,21.6954722464665,27.8107145290983));
#53607=CARTESIAN_POINT('Ctrl Pts',(-20.9181866143207,21.690579870545,27.810340374378));
#53608=CARTESIAN_POINT('Ctrl Pts',(-20.9231663215389,21.6835596071443,27.809803768147));
#53609=CARTESIAN_POINT('Ctrl Pts',(-20.9246851219391,21.6814239662281,27.809640564478));
#53610=CARTESIAN_POINT('Ctrl Pts',(-20.9273137239916,21.6777373219396,27.8093589033964));
#53611=CARTESIAN_POINT('Ctrl Pts',(-20.9284222989055,21.676185449057,27.8092403608338));
#53612=CARTESIAN_POINT('Ctrl Pts',(-20.9305580127126,21.6732013080775,27.8090124539186));
#53613=CARTESIAN_POINT('Ctrl Pts',(-20.9315849467733,21.6717689015858,27.808903075653));
#53614=CARTESIAN_POINT('Ctrl Pts',(-20.9340195629084,21.6683788830866,27.808644256483));
#53615=CARTESIAN_POINT('Ctrl Pts',(-20.9354282702975,21.6664220036515,27.808494886956));
#53616=CARTESIAN_POINT('Ctrl Pts',(-20.939633637727,21.6605940017594,27.8080501257668));
#53617=CARTESIAN_POINT('Ctrl Pts',(-20.9424367235006,21.6567274907922,27.8077551772338));
#53618=CARTESIAN_POINT('Ctrl Pts',(-20.9684482954551,21.62101505498,27.8050319194333));
#53619=CARTESIAN_POINT('Ctrl Pts',(-20.9922317156465,21.5895893263304,27.8026428331372));
#53620=CARTESIAN_POINT('Ctrl Pts',(-21.0181911685565,21.5565651050934,27.8001307140675));
#53621=CARTESIAN_POINT('Ctrl Pts',(-21.019797952492,21.5545261164855,27.7999756040536));
#53622=CARTESIAN_POINT('Ctrl Pts',(-21.0222103552994,21.5514724048369,27.7997432889105));
#53623=CARTESIAN_POINT('Ctrl Pts',(-21.0230141213529,21.5504562274523,27.7996659796996));
#53624=CARTESIAN_POINT('Ctrl Pts',(-21.02942089581,21.542366365425,27.7990504956335));
#53625=CARTESIAN_POINT('Ctrl Pts',(-21.0350530374656,21.5353156838306,27.7985139525816));
#53626=CARTESIAN_POINT('Ctrl Pts',(-21.044248001028,21.5239034579703,27.7976451372829));
#53627=CARTESIAN_POINT('Ctrl Pts',(-21.0477927336282,21.5195274798543,27.7973119047323));
#53628=CARTESIAN_POINT('Ctrl Pts',(-21.0550098561774,21.5106655238709,27.7966368317887));
#53629=CARTESIAN_POINT('Ctrl Pts',(-21.0586829178077,21.5061801180543,27.7962950281465));
#53630=CARTESIAN_POINT('Ctrl Pts',(-21.0725631402396,21.4893231095868,27.7950099038778));
#53631=CARTESIAN_POINT('Ctrl Pts',(-21.082850646771,21.4770176780729,27.7940706340535));
#53632=CARTESIAN_POINT('Ctrl Pts',(-21.1163761966167,21.4375189993406,27.7910501156446));
#53633=CARTESIAN_POINT('Ctrl Pts',(-21.1399757378193,21.4106350611374,27.7889855802773));
#53634=CARTESIAN_POINT('Ctrl Pts',(-21.3045125206393,21.229377234183,27.7749623369691));
#53635=CARTESIAN_POINT('Ctrl Pts',(-21.4597350517808,21.0886361698423,27.7635171374815));
#53636=CARTESIAN_POINT('Ctrl Pts',(-21.7346811458177,20.8842340241497,27.7441479573197));
#53637=CARTESIAN_POINT('Ctrl Pts',(-21.8467000964658,20.8113005957623,27.7364715979163));
#53638=CARTESIAN_POINT('Ctrl Pts',(-22.0086697586828,20.7196334306843,27.7254160127077));
#53639=CARTESIAN_POINT('Ctrl Pts',(-22.0550519189111,20.6948617389377,27.7222558005086));
#53640=CARTESIAN_POINT('Ctrl Pts',(-22.1108373437503,20.6667999211204,27.71845375986));
#53641=CARTESIAN_POINT('Ctrl Pts',(-22.1196776606154,20.6624037518002,27.7178512236386));
#53642=CARTESIAN_POINT('Ctrl Pts',(-22.1326360896558,20.6560338048784,27.716967916939));
#53643=CARTESIAN_POINT('Ctrl Pts',(-22.1367384772796,20.6540280181212,27.7166882661768));
#53644=CARTESIAN_POINT('Ctrl Pts',(-22.1439053449168,20.6505427647349,27.7161996883916));
#53645=CARTESIAN_POINT('Ctrl Pts',(-22.1469679381495,20.6490594164859,27.7159908971604));
#53646=CARTESIAN_POINT('Ctrl Pts',(-22.152889720223,20.6462028082142,27.7155871620169));
#53647=CARTESIAN_POINT('Ctrl Pts',(-22.1557485997197,20.6448289125099,27.7153922405319));
#53648=CARTESIAN_POINT('Ctrl Pts',(-22.1625323940824,20.6415811342,27.7149296907984));
#53649=CARTESIAN_POINT('Ctrl Pts',(-22.1664590763048,20.6397109753052,27.7146619333871));
#53650=CARTESIAN_POINT('Ctrl Pts',(-22.1802749010383,20.6331651982858,27.7137197694954));
#53651=CARTESIAN_POINT('Ctrl Pts',(-22.1901839669419,20.6285320259545,27.7130438927294));
#53652=CARTESIAN_POINT('Ctrl Pts',(-22.3219820388685,20.5677231000673,27.704051991083));
#53653=CARTESIAN_POINT('Ctrl Pts',(-22.4472241929496,20.5191718358914,27.6954735262335));
#53654=CARTESIAN_POINT('Ctrl Pts',(-22.8247606641092,20.399318754444,27.6694875057864));
#53655=CARTESIAN_POINT('Ctrl Pts',(-23.0831311363232,20.3508005047192,27.6514620661094));
#53656=CARTESIAN_POINT('Ctrl Pts',(-23.3873861614961,20.3313332468641,27.631140633707));
#53657=CARTESIAN_POINT('Ctrl Pts',(-23.4303536942529,20.3294465200179,27.6282943878418));
#53658=CARTESIAN_POINT('Ctrl Pts',(-23.5185065593216,20.327342318137,27.6225188607451));
#53659=CARTESIAN_POINT('Ctrl Pts',(-23.5636857014011,20.3272138952396,27.6195932056216));
#53660=CARTESIAN_POINT('Ctrl Pts',(-23.6350151184828,20.3285111632754,27.6150434005071));
#53661=CARTESIAN_POINT('Ctrl Pts',(-23.6611695195116,20.329305517197,27.6133898474699));
#53662=CARTESIAN_POINT('Ctrl Pts',(-23.6917163189335,20.3306058135741,27.6114780686054));
#53663=CARTESIAN_POINT('Ctrl Pts',(-23.6961199317306,20.3308023154679,27.6112029407094));
#53664=CARTESIAN_POINT('Ctrl Pts',(-23.7028331974419,20.331115682965,27.6107842468134));
#53665=CARTESIAN_POINT('Ctrl Pts',(-23.705143128232,20.3312259997142,27.6106403135962));
#53666=CARTESIAN_POINT('Ctrl Pts',(-23.7093168767647,20.3314298309001,27.6103804873017));
#53667=CARTESIAN_POINT('Ctrl Pts',(-23.7111807271371,20.3315224776218,27.6102645455232));
#53668=CARTESIAN_POINT('Ctrl Pts',(-23.7149187095161,20.3317115370841,27.6100321983214));
#53669=CARTESIAN_POINT('Ctrl Pts',(-23.7167928302724,20.3318079674524,27.60991579434));
#53670=CARTESIAN_POINT('Ctrl Pts',(-23.7221147324871,20.3320864597307,27.6095854928809));
#53671=CARTESIAN_POINT('Ctrl Pts',(-23.7255623204566,20.3322724259403,27.6093718161414));
#53672=CARTESIAN_POINT('Ctrl Pts',(-23.7401085142803,20.3330805073928,27.6084714883252));
#53673=CARTESIAN_POINT('Ctrl Pts',(-23.751204333428,20.3337545121117,27.6077877293596));
#53674=CARTESIAN_POINT('Ctrl Pts',(-23.7760449367015,20.3353924740859,27.6062632739094));
#53675=CARTESIAN_POINT('Ctrl Pts',(-23.7897875589025,20.3363871975429,27.6054242190391));
#53676=CARTESIAN_POINT('Ctrl Pts',(-23.8073107995806,20.3377685953849,27.6043593759402));
#53677=CARTESIAN_POINT('Ctrl Pts',(-23.811097436386,20.338073842688,27.6041295718724));
#53678=CARTESIAN_POINT('Ctrl Pts',(-23.8206767815296,20.3388631007708,27.6035489588744));
#53679=CARTESIAN_POINT('Ctrl Pts',(-23.8264687634227,20.3393560920179,27.6031985862971));
#53680=CARTESIAN_POINT('Ctrl Pts',(-23.8415725377017,20.3406828378047,27.6022866313876));
#53681=CARTESIAN_POINT('Ctrl Pts',(-23.8508821581294,20.3415414512581,27.601726222468));
#53682=CARTESIAN_POINT('Ctrl Pts',(-23.8691327926678,20.3433048087797,27.6006306976187));
#53683=CARTESIAN_POINT('Ctrl Pts',(-23.8780740075283,20.3442064618725,27.6000954491404));
#53684=CARTESIAN_POINT('Ctrl Pts',(-23.9005681872112,20.3465699134277,27.598752301149));
#53685=CARTESIAN_POINT('Ctrl Pts',(-23.91411597796,20.3480803344396,27.5979464801079));
#53686=CARTESIAN_POINT('Ctrl Pts',(-23.9605332906161,20.3535537123479,27.5951950874469));
#53687=CARTESIAN_POINT('Ctrl Pts',(-23.9933519492917,20.3579372768804,27.5932661104233));
#53688=CARTESIAN_POINT('Ctrl Pts',(-24.3133225590691,20.4057051647797,27.5745696029612));
#53689=CARTESIAN_POINT('Ctrl Pts',(-24.5934418118021,20.4872092651833,27.5589488049468));
#53690=CARTESIAN_POINT('Ctrl Pts',(-24.9611632059889,20.6506009992864,27.5357504841367));
#53691=CARTESIAN_POINT('Ctrl Pts',(-25.0610109701451,20.7013487525684,27.5291635944778));
#53692=CARTESIAN_POINT('Ctrl Pts',(-25.1689566023336,20.763484827109,27.5216239000751));
#53693=CARTESIAN_POINT('Ctrl Pts',(-25.1798663815724,20.7698504383164,27.5208570016011));
#53694=CARTESIAN_POINT('Ctrl Pts',(-25.1989729464373,20.7811497743986,27.5195051678481));
#53695=CARTESIAN_POINT('Ctrl Pts',(-25.2071857585042,20.7860561990795,27.5189212277312));
#53696=CARTESIAN_POINT('Ctrl Pts',(-25.2192241587753,20.7933210007991,27.5180610171292));
#53697=CARTESIAN_POINT('Ctrl Pts',(-25.2230669076351,20.7956509595305,27.5177857890578));
#53698=CARTESIAN_POINT('Ctrl Pts',(-25.2298007130102,20.7997531282996,27.517302362016));
#53699=CARTESIAN_POINT('Ctrl Pts',(-25.2326938757643,20.8015218819111,27.5170942904235));
#53700=CARTESIAN_POINT('Ctrl Pts',(-25.2383046755696,20.804964257461,27.5166900525897));
#53701=CARTESIAN_POINT('Ctrl Pts',(-25.2410226297742,20.8066373574395,27.5164939057583));
#53702=CARTESIAN_POINT('Ctrl Pts',(-25.2475030898378,20.8106398422967,27.5160254438246));
#53703=CARTESIAN_POINT('Ctrl Pts',(-25.2512632851853,20.8129729403424,27.5157529916559));
#53704=CARTESIAN_POINT('Ctrl Pts',(-25.2646853450385,20.8213392968954,27.5147781933944));
#53705=CARTESIAN_POINT('Ctrl Pts',(-25.274319926005,20.8274159723217,27.514074239335));
#53706=CARTESIAN_POINT('Ctrl Pts',(-25.4232505523995,20.9224561399968,27.5031261631887));
#53707=CARTESIAN_POINT('Ctrl Pts',(-25.5555095637881,21.0219400358619,27.4924793441141));
#53708=CARTESIAN_POINT('Ctrl Pts',(-25.7467908793405,21.190302752394,27.4755879542881));
#53709=CARTESIAN_POINT('Ctrl Pts',(-25.8115395459572,21.2522700899586,27.4695708734129));
#53710=CARTESIAN_POINT('Ctrl Pts',(-25.9969384902576,21.445137295342,27.4515018220242));
#53711=CARTESIAN_POINT('Ctrl Pts',(-26.1094244266201,21.5834208997825,27.4393662821745));
#53712=CARTESIAN_POINT('Ctrl Pts',(-26.2393756517925,21.7733297800473,27.4242536878808));
#53713=CARTESIAN_POINT('Ctrl Pts',(-26.2677811100163,21.8170829698717,27.420870665215));
#53714=CARTESIAN_POINT('Ctrl Pts',(-26.3081984171674,21.8827767203016,27.4159564904869));
#53715=CARTESIAN_POINT('Ctrl Pts',(-26.3210360135567,21.9041966155463,27.414379439218));
#53716=CARTESIAN_POINT('Ctrl Pts',(-26.3357897125286,21.9294753602753,27.4125496386335));
#53717=CARTESIAN_POINT('Ctrl Pts',(-26.3379481996208,21.9331907243602,27.4122814890254));
#53718=CARTESIAN_POINT('Ctrl Pts',(-26.341235647428,21.9388754923069,27.4118724157007));
#53719=CARTESIAN_POINT('Ctrl Pts',(-26.3423699580268,21.9408417721234,27.4117311446076));
#53720=CARTESIAN_POINT('Ctrl Pts',(-26.3444230565874,21.9444094357225,27.4114752228268));
#53721=CARTESIAN_POINT('Ctrl Pts',(-26.3453425425081,21.946010404533,27.4113605267506));
#53722=CARTESIAN_POINT('Ctrl Pts',(-26.3472038953457,21.9492577691987,27.4111281788129));
#53723=CARTESIAN_POINT('Ctrl Pts',(-26.3481456808386,21.9509041999708,27.4110105323902));
#53724=CARTESIAN_POINT('Ctrl Pts',(-26.3508473638997,21.9556369758184,27.4106727926805));
#53725=CARTESIAN_POINT('Ctrl Pts',(-26.3526036191034,21.9587254133571,27.4104529365187));
#53726=CARTESIAN_POINT('Ctrl Pts',(-26.3602491030745,21.9722221623054,27.4094944748164));
#53727=CARTESIAN_POINT('Ctrl Pts',(-26.3660855778112,21.982660478623,27.4087592446812));
#53728=CARTESIAN_POINT('Ctrl Pts',(-26.4667435424267,22.1650596659597,27.396012417811));
#53729=CARTESIAN_POINT('Ctrl Pts',(-26.5457268264232,22.3453301348107,27.3849536534753));
#53730=CARTESIAN_POINT('Ctrl Pts',(-26.6596609686117,22.6873438388451,27.3647813075165));
#53731=CARTESIAN_POINT('Ctrl Pts',(-26.6995496853667,22.8467207464071,27.3556752076593));
#53732=CARTESIAN_POINT('Ctrl Pts',(-26.7509715464855,23.1482258749894,27.33815015481));
#53733=CARTESIAN_POINT('Ctrl Pts',(-26.765557540103,23.2894207899487,27.3298267829904));
#53734=CARTESIAN_POINT('Ctrl Pts',(-26.77115519982,23.4407251969664,27.3206059653181));
#53735=CARTESIAN_POINT('Ctrl Pts',(-26.7714679946659,23.4503467133426,27.3200183593341));
#53736=CARTESIAN_POINT('Ctrl Pts',(-26.7718626896692,23.464430231942,27.3191563742683));
#53737=CARTESIAN_POINT('Ctrl Pts',(-26.7719784396549,23.4688912954683,27.318883058537));
#53738=CARTESIAN_POINT('Ctrl Pts',(-26.7721657216574,23.4767377389219,27.3184018415892));
#53739=CARTESIAN_POINT('Ctrl Pts',(-26.7722411847821,23.4801230254457,27.3181940641295));
#53740=CARTESIAN_POINT('Ctrl Pts',(-26.7723776054423,23.4867087052414,27.3177895433338));
#53741=CARTESIAN_POINT('Ctrl Pts',(-26.7724391304131,23.4899090840198,27.317592818056));
#53742=CARTESIAN_POINT('Ctrl Pts',(-26.7725907084634,23.4984564378133,27.3170670296649));
#53743=CARTESIAN_POINT('Ctrl Pts',(-26.7726722205565,23.5038035372304,27.316737698733));
#53744=CARTESIAN_POINT('Ctrl Pts',(-26.7729175804141,23.5230404143155,27.3155514137426));
#53745=CARTESIAN_POINT('Ctrl Pts',(-26.7730049328194,23.5369308613233,27.314692061835));
#53746=CARTESIAN_POINT('Ctrl Pts',(-26.7729902628023,23.6200588915252,27.3095322508042));
#53747=CARTESIAN_POINT('Ctrl Pts',(-26.7707468127409,23.6892733894291,27.3051649806394));
#53748=CARTESIAN_POINT('Ctrl Pts',(-26.7614124245131,23.8335254060318,27.2959054392696));
#53749=CARTESIAN_POINT('Ctrl Pts',(-26.7539149434557,23.9084942640823,27.291003542779));
#53750=CARTESIAN_POINT('Ctrl Pts',(-26.7211484207959,24.1502302494961,27.2749201630473));
#53751=CARTESIAN_POINT('Ctrl Pts',(-26.6854189927194,24.3152865231714,27.2634913702863));
#53752=CARTESIAN_POINT('Ctrl Pts',(-26.5840181879805,24.6531015103468,27.2396312858963));
#53753=CARTESIAN_POINT('Ctrl Pts',(-26.5160718575201,24.824592907168,27.2272485170435));
#53754=CARTESIAN_POINT('Ctrl Pts',(-26.429043892908,24.9989737949812,27.2149755206588));
#53755=CARTESIAN_POINT('Ctrl Pts',(-26.4241979864778,25.0085633801799,27.2143017286782));
#53756=CARTESIAN_POINT('Ctrl Pts',(-26.4177524192232,25.0211616260647,27.2134182054145));
#53757=CARTESIAN_POINT('Ctrl Pts',(-26.4161958900738,25.024192094803,27.2132058041464));
#53758=CARTESIAN_POINT('Ctrl Pts',(-26.4137787751932,25.0288797673819,27.2128774560556));
#53759=CARTESIAN_POINT('Ctrl Pts',(-26.4129215556488,25.0305386893874,27.2127612965089));
#53760=CARTESIAN_POINT('Ctrl Pts',(-26.4112042771354,25.033854957963,27.2125291685302));
#53761=CARTESIAN_POINT('Ctrl Pts',(-26.4103442250899,25.035512291591,27.2124132012404));
#53762=CARTESIAN_POINT('Ctrl Pts',(-26.4084081121296,25.0392352936305,27.2121527850952));
#53763=CARTESIAN_POINT('Ctrl Pts',(-26.407331254245,25.0413005391533,27.2120083879907));
#53764=CARTESIAN_POINT('Ctrl Pts',(-26.4041307961566,25.0474223213986,27.2115805473663));
#53765=CARTESIAN_POINT('Ctrl Pts',(-26.4020007773195,25.0514755237118,27.211297510813));
#53766=CARTESIAN_POINT('Ctrl Pts',(-26.3848977006121,25.0838531284887,27.2090383392424));
#53767=CARTESIAN_POINT('Ctrl Pts',(-26.3695109845738,25.1119586469161,27.207088091149));
#53768=CARTESIAN_POINT('Ctrl Pts',(-26.3137732135825,25.2102603505334,27.2002887383748));
#53769=CARTESIAN_POINT('Ctrl Pts',(-26.271196233903,25.2791654968496,27.195562271471));
#53770=CARTESIAN_POINT('Ctrl Pts',(-26.0581104338111,25.5966105380004,27.1736255207598));
#53771=CARTESIAN_POINT('Ctrl Pts',(-25.8558943945743,25.8220285277798,27.1574130288819));
#53772=CARTESIAN_POINT('Ctrl Pts',(-25.5508969995853,26.0786895964007,27.134194091959));
#53773=CARTESIAN_POINT('Ctrl Pts',(-25.4737104300391,26.1378922087295,27.128418552256));
#53774=CARTESIAN_POINT('Ctrl Pts',(-25.3863341453027,26.1988386784496,27.1219340124906));
#53775=CARTESIAN_POINT('Ctrl Pts',(-25.3786738902483,26.2041326347396,27.1213659687162));
#53776=CARTESIAN_POINT('Ctrl Pts',(-25.3672644135931,26.2119448092281,27.1205205318743));
#53777=CARTESIAN_POINT('Ctrl Pts',(-25.3635326206346,26.2144884968369,27.1202441071993));
#53778=CARTESIAN_POINT('Ctrl Pts',(-25.3571342981806,26.2188300904842,27.1197703296585));
#53779=CARTESIAN_POINT('Ctrl Pts',(-25.3544703940264,26.2206318700031,27.1195731238541));
#53780=CARTESIAN_POINT('Ctrl Pts',(-25.3492819864506,26.2241298350871,27.1191891244928));
#53781=CARTESIAN_POINT('Ctrl Pts',(-25.3467577697609,26.2258264406309,27.1190023471373));
#53782=CARTESIAN_POINT('Ctrl Pts',(-25.3407135827587,26.22987651953,27.1185552119227));
#53783=CARTESIAN_POINT('Ctrl Pts',(-25.3371913754047,26.2322266292812,27.1182947275467));
#53784=CARTESIAN_POINT('Ctrl Pts',(-25.3266128682736,26.2392547988692,27.1175126297482));
#53785=CARTESIAN_POINT('Ctrl Pts',(-25.3195427970398,26.2439119743493,27.1169902319159));
#53786=CARTESIAN_POINT('Ctrl Pts',(-25.2599330235087,26.2828420050913,27.1125882183764));
#53787=CARTESIAN_POINT('Ctrl Pts',(-25.2064245119428,26.3155999043005,27.108652448068));
#53788=CARTESIAN_POINT('Ctrl Pts',(-25.0686461137499,26.3945143045002,27.0985466777094));
#53789=CARTESIAN_POINT('Ctrl Pts',(-24.9832097687096,26.4385002248896,27.092304654803));
#53790=CARTESIAN_POINT('Ctrl Pts',(-24.5989328247726,26.6150904433102,27.0643679070284));
#53791=CARTESIAN_POINT('Ctrl Pts',(-24.2829231040249,26.70558639212,27.0415193935694));
#53792=CARTESIAN_POINT('Ctrl Pts',(-23.9303606208478,26.7506358029833,27.0188044626008));
#53793=CARTESIAN_POINT('Ctrl Pts',(-23.9019479288539,26.7538826178576,27.0169946942335));
#53794=CARTESIAN_POINT('Ctrl Pts',(-23.8687573883957,26.7572285041729,27.0149077710829));
#53795=CARTESIAN_POINT('Ctrl Pts',(-23.8640190807496,26.7576955608353,27.014610485272));
#53796=CARTESIAN_POINT('Ctrl Pts',(-23.8569168585411,26.7583797405284,27.0141658693321));
#53797=CARTESIAN_POINT('Ctrl Pts',(-23.8545537378389,26.758604752609,27.0140180955647));
#53798=CARTESIAN_POINT('Ctrl Pts',(-23.8503229984115,26.7590028796378,27.0137538281405));
#53799=CARTESIAN_POINT('Ctrl Pts',(-23.8484554780954,26.7591769750633,27.0136372788856));
#53800=CARTESIAN_POINT('Ctrl Pts',(-23.8445054264257,26.7595417317612,27.0133909801908));
#53801=CARTESIAN_POINT('Ctrl Pts',(-23.8424228664763,26.7597319959154,27.0132612537576));
#53802=CARTESIAN_POINT('Ctrl Pts',(-23.8369422067294,26.7602273342159,27.0129201869163));
#53803=CARTESIAN_POINT('Ctrl Pts',(-23.8335437935575,26.7605290406268,27.012709037505));
#53804=CARTESIAN_POINT('Ctrl Pts',(-23.8180641847547,26.7618785269774,27.0117487714541));
#53805=CARTESIAN_POINT('Ctrl Pts',(-23.805977405847,26.7628635281993,27.0110031633054));
#53806=CARTESIAN_POINT('Ctrl Pts',(-23.618824813142,26.7770524431776,26.9995188975899));
#53807=CARTESIAN_POINT('Ctrl Pts',(-23.4429438948042,26.7759995369787,26.9895416721648));
#53808=CARTESIAN_POINT('Ctrl Pts',(-23.0261258103459,26.7393534901486,26.9660607821395));
#53809=CARTESIAN_POINT('Ctrl Pts',(-22.7874472796697,26.6908248460841,26.9526936196271));
#53810=CARTESIAN_POINT('Ctrl Pts',(-22.5374643231404,26.6097912895227,26.9372947586525));
#53811=CARTESIAN_POINT('Ctrl Pts',(-22.5185016901403,26.603448814755,26.936118128442));
#53812=CARTESIAN_POINT('Ctrl Pts',(-22.4947877294154,26.5952710080177,26.9346353341244));
#53813=CARTESIAN_POINT('Ctrl Pts',(-22.4899798299442,26.5936002389918,26.9343341165775));
#53814=CARTESIAN_POINT('Ctrl Pts',(-22.4813158115808,26.5905664264087,26.9337902370704));
#53815=CARTESIAN_POINT('Ctrl Pts',(-22.4774582845578,26.5892074166991,26.9335476978937));
#53816=CARTESIAN_POINT('Ctrl Pts',(-22.4704504416563,26.5867235423681,26.9331063781281));
#53817=CARTESIAN_POINT('Ctrl Pts',(-22.4672992662039,26.5856011075513,26.9329076722053));
#53818=CARTESIAN_POINT('Ctrl Pts',(-22.4143817481995,26.5666592264092,26.9295664054233));
#53819=CARTESIAN_POINT('Ctrl Pts',(-22.3650618775877,26.5476237798608,26.9263865334187));
#53820=CARTESIAN_POINT('Ctrl Pts',(-22.308170626901,26.524042420502,26.9226334945939));
#53821=CARTESIAN_POINT('Ctrl Pts',(-22.300120411541,26.5206672234149,26.9221004281876));
#53822=CARTESIAN_POINT('Ctrl Pts',(-22.2881369025134,26.5155855792361,26.9213038793064));
#53823=CARTESIAN_POINT('Ctrl Pts',(-22.2841930943073,26.5139039020461,26.9210412418666));
#53824=CARTESIAN_POINT('Ctrl Pts',(-22.2771623002621,26.5108893097006,26.9205721457793));
#53825=CARTESIAN_POINT('Ctrl Pts',(-22.2740740168574,26.5095594212859,26.9203657908202));
#53826=CARTESIAN_POINT('Ctrl Pts',(-22.267564697252,26.5067442687712,26.9199302025796));
#53827=CARTESIAN_POINT('Ctrl Pts',(-22.2641441488214,26.5052578953692,26.9197009315541));
#53828=CARTESIAN_POINT('Ctrl Pts',(-22.2551098863997,26.5013134674819,26.9190943880917));
#53829=CARTESIAN_POINT('Ctrl Pts',(-22.2495006102249,26.4988453412148,26.918716770635));
#53830=CARTESIAN_POINT('Ctrl Pts',(-22.2245072635091,26.4877628714342,26.9170296228426));
#53831=CARTESIAN_POINT('Ctrl Pts',(-22.2052018370598,26.4789734310645,26.9157140811468));
#53832=CARTESIAN_POINT('Ctrl Pts',(-22.148648067492,26.4525483281695,26.9118231005602));
#53833=CARTESIAN_POINT('Ctrl Pts',(-22.1116584725339,26.4343921662557,26.9092301670837));
#53834=CARTESIAN_POINT('Ctrl Pts',(-22.0750359502314,26.4155367410314,26.9066135500179));
#53835=CARTESIAN_POINT('Ctrl Pts',(-22.0750360239718,26.4155367789973,26.65912344949));
#53836=CARTESIAN_POINT('Ctrl Pts',(-22.1002035109265,26.4284944784815,26.6607352299033));
#53837=CARTESIAN_POINT('Ctrl Pts',(-22.1255444033382,26.4411219678302,26.662338762767));
#53838=CARTESIAN_POINT('Ctrl Pts',(-22.318005719262,26.5338800785094,26.6743948788536));
#53839=CARTESIAN_POINT('Ctrl Pts',(-22.4915870603914,26.5997924768428,26.6845988913205));
#53840=CARTESIAN_POINT('Ctrl Pts',(-22.7833682994856,26.6826519796707,26.7018404289965));
#53841=CARTESIAN_POINT('Ctrl Pts',(-22.8985383847735,26.70862272329,26.7086625340796));
#53842=CARTESIAN_POINT('Ctrl Pts',(-23.0655028963066,26.7367509679445,26.7187404833921));
#53843=CARTESIAN_POINT('Ctrl Pts',(-23.1163346709547,26.7440698909521,26.7218325006049));
#53844=CARTESIAN_POINT('Ctrl Pts',(-23.1752450752332,26.7511197136806,26.7254502496706));
#53845=CARTESIAN_POINT('Ctrl Pts',(-23.1831761009048,26.7520389395093,26.7259380139693));
#53846=CARTESIAN_POINT('Ctrl Pts',(-23.1952194946412,26.7533894632106,26.7266797989716));
#53847=CARTESIAN_POINT('Ctrl Pts',(-23.1993294522773,26.7538423386956,26.7269331377892));
#53848=CARTESIAN_POINT('Ctrl Pts',(-23.2067686647732,26.7546475765935,26.7273920505936));
#53849=CARTESIAN_POINT('Ctrl Pts',(-23.2100976239146,26.755002663793,26.7275975382357));
#53850=CARTESIAN_POINT('Ctrl Pts',(-23.2167439333816,26.7557011274602,26.728008058016));
#53851=CARTESIAN_POINT('Ctrl Pts',(-23.2200612755955,26.7560445429623,26.7282130886588));
#53852=CARTESIAN_POINT('Ctrl Pts',(-23.2293689523761,26.7569934850396,26.7287887232825));
#53853=CARTESIAN_POINT('Ctrl Pts',(-23.2353604364257,26.7575873724753,26.7291596940361));
#53854=CARTESIAN_POINT('Ctrl Pts',(-23.2597971155129,26.7599404501934,26.7306744884708));
#53855=CARTESIAN_POINT('Ctrl Pts',(-23.2782553686142,26.7615573137323,26.7318227896483));
#53856=CARTESIAN_POINT('Ctrl Pts',(-23.6010348871531,26.7870285710069,26.7519775486845));
#53857=CARTESIAN_POINT('Ctrl Pts',(-23.907145919701,26.7676794194904,26.7724722575359));
#53858=CARTESIAN_POINT('Ctrl Pts',(-24.3923106645748,26.6668716828463,26.8059986069167));
#53859=CARTESIAN_POINT('Ctrl Pts',(-24.5749737445106,26.6116807711367,26.8188149936768));
#53860=CARTESIAN_POINT('Ctrl Pts',(-24.7566209284287,26.5387004286289,26.8311046322034));
#53861=CARTESIAN_POINT('Ctrl Pts',(-24.7615242857119,26.5367163737968,26.831436007984));
#53862=CARTESIAN_POINT('Ctrl Pts',(-24.7703200395528,26.5331321051258,26.8320297453242));
#53863=CARTESIAN_POINT('Ctrl Pts',(-24.774214214319,26.5315363278589,26.8322923685132));
#53864=CARTESIAN_POINT('Ctrl Pts',(-24.7800692257252,26.5291236221627,26.8326868504849));
#53865=CARTESIAN_POINT('Ctrl Pts',(-24.7820323792746,26.5283123836286,26.8328190537518));
#53866=CARTESIAN_POINT('Ctrl Pts',(-24.7856880139195,26.5267975240134,26.8330651106059));
#53867=CARTESIAN_POINT('Ctrl Pts',(-24.7873806942676,26.5260944010596,26.833178994207));
#53868=CARTESIAN_POINT('Ctrl Pts',(-24.7907828867047,26.5246777589073,26.83340779506));
#53869=CARTESIAN_POINT('Ctrl Pts',(-24.7924923770923,26.5239642124949,26.8335227100362));
#53870=CARTESIAN_POINT('Ctrl Pts',(-24.7972755919546,26.5219628399031,26.8338441088757));
#53871=CARTESIAN_POINT('Ctrl Pts',(-24.8003479468294,26.5206717145762,26.834050390926));
#53872=CARTESIAN_POINT('Ctrl Pts',(-24.8127906126895,26.5154200892518,26.8348851856375));
#53873=CARTESIAN_POINT('Ctrl Pts',(-24.8221442813769,26.5114199423619,26.8355113029031));
#53874=CARTESIAN_POINT('Ctrl Pts',(-24.9825994218186,26.441899880304,26.8462298049572));
#53875=CARTESIAN_POINT('Ctrl Pts',(-25.1285027578106,26.3649256424062,26.8556443693302));
#53876=CARTESIAN_POINT('Ctrl Pts',(-25.3542985523088,26.2226975422164,26.8706580084505));
#53877=CARTESIAN_POINT('Ctrl Pts',(-25.4380638258682,26.1641984615646,26.8763371310586));
#53878=CARTESIAN_POINT('Ctrl Pts',(-25.6105116033297,26.0311466486744,26.8885350775715));
#53879=CARTESIAN_POINT('Ctrl Pts',(-25.6982355750633,25.9555944076823,26.8950573080001));
#53880=CARTESIAN_POINT('Ctrl Pts',(-25.8412359759228,25.8183619840093,26.9064954835451));
#53881=CARTESIAN_POINT('Ctrl Pts',(-25.8985483084863,25.7589695692253,26.9113303768721));
#53882=CARTESIAN_POINT('Ctrl Pts',(-25.981860334445,25.665721971269,26.9188056440167));
#53883=CARTESIAN_POINT('Ctrl Pts',(-26.009572927011,25.6334400857977,26.921373735971));
#53884=CARTESIAN_POINT('Ctrl Pts',(-26.0414713526595,25.5947583587771,26.9244318731567));
#53885=CARTESIAN_POINT('Ctrl Pts',(-26.0462844998661,25.5888794478346,26.9248961432663));
#53886=CARTESIAN_POINT('Ctrl Pts',(-26.053633289723,25.579838393628,26.9256093774157));
#53887=CARTESIAN_POINT('Ctrl Pts',(-26.0561838539742,25.5766883679369,26.9258577377227));
#53888=CARTESIAN_POINT('Ctrl Pts',(-26.060827291813,25.5709314058864,26.9263113877445));
#53889=CARTESIAN_POINT('Ctrl Pts',(-26.0629220672863,25.5683260049665,26.9265166004236));
#53890=CARTESIAN_POINT('Ctrl Pts',(-26.067128091261,25.5630780136564,26.926929769404));
#53891=CARTESIAN_POINT('Ctrl Pts',(-26.069239240876,25.5604353497501,26.9271377293122));
#53892=CARTESIAN_POINT('Ctrl Pts',(-26.0752430314933,25.5528957030038,26.9277307838726));
#53893=CARTESIAN_POINT('Ctrl Pts',(-26.0791255640723,25.5479907229734,26.9281162827488));
#53894=CARTESIAN_POINT('Ctrl Pts',(-26.0956105400957,25.5270394391697,26.9297615941946));
#53895=CARTESIAN_POINT('Ctrl Pts',(-26.1080745064524,25.5108852313878,26.9310269051937));
#53896=CARTESIAN_POINT('Ctrl Pts',(-26.3373474263915,25.2078235103166,26.9547080494624));
#53897=CARTESIAN_POINT('Ctrl Pts',(-26.5047361887244,24.88678646575,26.9792812596588));
#53898=CARTESIAN_POINT('Ctrl Pts',(-26.6436713915966,24.4586087445473,27.0094934229028));
#53899=CARTESIAN_POINT('Ctrl Pts',(-26.6680217453622,24.3711477301968,27.0155171421788));
#53900=CARTESIAN_POINT('Ctrl Pts',(-26.699409123468,24.23667157406,27.024449247208));
#53901=CARTESIAN_POINT('Ctrl Pts',(-26.7091523593242,24.190339102167,27.0274681427176));
#53902=CARTESIAN_POINT('Ctrl Pts',(-26.7187884775357,24.1389139732259,27.0307419454235));
#53903=CARTESIAN_POINT('Ctrl Pts',(-26.719693792244,24.1340199764464,27.0310527383684));
#53904=CARTESIAN_POINT('Ctrl Pts',(-26.7210206236057,24.1267532489419,27.0315130543606));
#53905=CARTESIAN_POINT('Ctrl Pts',(-26.7214508165439,24.1243821406925,27.0316630712046));
#53906=CARTESIAN_POINT('Ctrl Pts',(-26.7221801271835,24.1203365472595,27.0319187162889));
#53907=CARTESIAN_POINT('Ctrl Pts',(-26.7224805787188,24.1186623077846,27.0320244213522));
#53908=CARTESIAN_POINT('Ctrl Pts',(-26.7230945802085,24.1152251891701,27.0322412386783));
#53909=CARTESIAN_POINT('Ctrl Pts',(-26.7234079858506,24.1134622904095,27.0323523424115));
#53910=CARTESIAN_POINT('Ctrl Pts',(-26.7241584136641,24.1092206435285,27.0326194219322));
#53911=CARTESIAN_POINT('Ctrl Pts',(-26.7245940023249,24.1067416381333,27.0327753152882));
#53912=CARTESIAN_POINT('Ctrl Pts',(-26.7261706111393,24.0977068180355,27.0333427548533));
#53913=CARTESIAN_POINT('Ctrl Pts',(-26.7272942403617,24.0911479247513,27.0337533126045));
#53914=CARTESIAN_POINT('Ctrl Pts',(-26.7291805479057,24.0799284062761,27.0344533208118));
#53915=CARTESIAN_POINT('Ctrl Pts',(-26.7299533057075,24.0752695340414,27.0347433246901));
#53916=CARTESIAN_POINT('Ctrl Pts',(-26.758704891206,23.8995373632741,27.0456574646504));
#53917=CARTESIAN_POINT('Ctrl Pts',(-26.7728503665737,23.7264580187519,27.055528652753));
#53918=CARTESIAN_POINT('Ctrl Pts',(-26.7732154882093,23.3070170739045,27.0790849247666));
#53919=CARTESIAN_POINT('Ctrl Pts',(-26.7452551395816,23.0617801032081,27.0926117794247));
#53920=CARTESIAN_POINT('Ctrl Pts',(-26.6850037036113,22.8020019501826,27.1082309318386));
#53921=CARTESIAN_POINT('Ctrl Pts',(-26.6801457921284,22.781934892698,27.1094454763104));
#53922=CARTESIAN_POINT('Ctrl Pts',(-26.673966630763,22.7574416553488,27.1109383850029));
#53923=CARTESIAN_POINT('Ctrl Pts',(-26.6728281846266,22.7529695519551,27.1112113965384));
#53924=CARTESIAN_POINT('Ctrl Pts',(-26.6706819518144,22.7446137196177,27.1117223124583));
#53925=CARTESIAN_POINT('Ctrl Pts',(-26.6696765090945,22.7407293939822,27.1119601473094));
#53926=CARTESIAN_POINT('Ctrl Pts',(-26.667404338373,22.7320184100123,27.1124942606677));
#53927=CARTESIAN_POINT('Ctrl Pts',(-26.6661336504255,22.7271928028153,27.1127906564237));
#53928=CARTESIAN_POINT('Ctrl Pts',(-26.6630711588772,22.7156713180635,27.1134995672237));
#53929=CARTESIAN_POINT('Ctrl Pts',(-26.6612689557792,22.7089782506919,27.1139123938956));
#53930=CARTESIAN_POINT('Ctrl Pts',(-26.6589095236445,22.7003269976165,27.1144473255561));
#53931=CARTESIAN_POINT('Ctrl Pts',(-26.6583720029826,22.6983634196324,27.1145688275838));
#53932=CARTESIAN_POINT('Ctrl Pts',(-26.6565839608661,22.6918558715591,27.1149717953353));
#53933=CARTESIAN_POINT('Ctrl Pts',(-26.6553253364479,22.6873141498702,27.115253509239));
#53934=CARTESIAN_POINT('Ctrl Pts',(-26.6535525573608,22.680971206753,27.1156476224777));
#53935=CARTESIAN_POINT('Ctrl Pts',(-26.6530467838057,22.6791676332855,27.115759762084));
#53936=CARTESIAN_POINT('Ctrl Pts',(-26.6510969700594,22.6722378994951,27.116190921518));
#53937=CARTESIAN_POINT('Ctrl Pts',(-26.6496418021535,22.6671149008844,27.116510286515));
#53938=CARTESIAN_POINT('Ctrl Pts',(-26.644749645636,22.6500528154092,27.1175760139364));
#53939=CARTESIAN_POINT('Ctrl Pts',(-26.6412563476154,22.6381301052484,27.1183241364571));
#53940=CARTESIAN_POINT('Ctrl Pts',(-26.6311913943934,22.6045000924015,27.1204442316431));
#53941=CARTESIAN_POINT('Ctrl Pts',(-26.6244595045691,22.582841864368,27.1218212939463));
#53942=CARTESIAN_POINT('Ctrl Pts',(-26.6154995748848,22.5550537543438,27.1236037830363));
#53943=CARTESIAN_POINT('Ctrl Pts',(-26.613480641613,22.5488567119275,27.124002305748));
#53944=CARTESIAN_POINT('Ctrl Pts',(-26.6102496316203,22.5390404477968,27.124635191442));
#53945=CARTESIAN_POINT('Ctrl Pts',(-26.6090498926251,22.5354171584736,27.1248691462837));
#53946=CARTESIAN_POINT('Ctrl Pts',(-26.6067954898645,22.5286490324378,27.1253068201278));
#53947=CARTESIAN_POINT('Ctrl Pts',(-26.6057424010411,22.5255036731826,27.125510486748));
#53948=CARTESIAN_POINT('Ctrl Pts',(-26.6033660899418,22.5184423511547,27.1259683179138));
#53949=CARTESIAN_POINT('Ctrl Pts',(-26.602040187684,22.5145273023432,27.1262225710365));
#53950=CARTESIAN_POINT('Ctrl Pts',(-26.5981332111613,22.5030636424175,27.1269682735413));
#53951=CARTESIAN_POINT('Ctrl Pts',(-26.5955316493111,22.4955220921668,27.1274604024123));
#53952=CARTESIAN_POINT('Ctrl Pts',(-26.5760303630848,22.4396643380187,27.1311171033311));
#53953=CARTESIAN_POINT('Ctrl Pts',(-26.5580105050036,22.3917495719368,27.1343188426746));
#53954=CARTESIAN_POINT('Ctrl Pts',(-26.4949394301051,22.2354478697928,27.1449874608855));
#53955=CARTESIAN_POINT('Ctrl Pts',(-26.4451130206286,22.1291017253764,27.152611931003));
#53956=CARTESIAN_POINT('Ctrl Pts',(-26.2409640086401,21.7488866174755,27.1811994800256));
#53957=CARTESIAN_POINT('Ctrl Pts',(-26.0526558250693,21.4953051377525,27.2031124456538));
#53958=CARTESIAN_POINT('Ctrl Pts',(-25.8264313261303,21.2687698535442,27.2236225025693));
#53959=CARTESIAN_POINT('Ctrl Pts',(-25.8222063003646,21.2645624413434,27.2240037393628));
#53960=CARTESIAN_POINT('Ctrl Pts',(-25.8156028846158,21.2580229542619,27.2245967305327));
#53961=CARTESIAN_POINT('Ctrl Pts',(-25.8132325368919,21.2556828218254,27.2248090193358));
#53962=CARTESIAN_POINT('Ctrl Pts',(-25.8074681233114,21.2500095086516,27.2253238897863));
#53963=CARTESIAN_POINT('Ctrl Pts',(-25.8040702859314,21.2466801487692,27.2256262134075));
#53964=CARTESIAN_POINT('Ctrl Pts',(-25.7961954063491,21.2389980767049,27.2263241633312));
#53965=CARTESIAN_POINT('Ctrl Pts',(-25.7917130421661,21.2346508100302,27.2267194129556));
#53966=CARTESIAN_POINT('Ctrl Pts',(-25.7773228895002,21.2207753085499,27.2279817809126));
#53967=CARTESIAN_POINT('Ctrl Pts',(-25.7673665936322,21.2112972597313,27.2288453213514));
#53968=CARTESIAN_POINT('Ctrl Pts',(-25.7546509633859,21.1993465714761,27.2299353752249));
#53969=CARTESIAN_POINT('Ctrl Pts',(-25.7519477914895,21.1968147775232,27.2301663777779));
#53970=CARTESIAN_POINT('Ctrl Pts',(-25.7476591923194,21.1928119263383,27.2305317043135));
#53971=CARTESIAN_POINT('Ctrl Pts',(-25.7460766489504,21.1913378053671,27.2306662646679));
#53972=CARTESIAN_POINT('Ctrl Pts',(-25.7432629046183,21.1887221199188,27.2309050668521));
#53973=CARTESIAN_POINT('Ctrl Pts',(-25.742032302393,21.1875799309568,27.2310093570647));
#53974=CARTESIAN_POINT('Ctrl Pts',(-25.7391715037881,21.1849288264872,27.2312514521635));
#53975=CARTESIAN_POINT('Ctrl Pts',(-25.7375406422634,21.1834206368945,27.2313892006504));
#53976=CARTESIAN_POINT('Ctrl Pts',(-25.7329175121721,21.1791541137674,27.2317789468384));
#53977=CARTESIAN_POINT('Ctrl Pts',(-25.7299215627231,21.176399747694,27.2320306395743));
#53978=CARTESIAN_POINT('Ctrl Pts',(-25.7117197351977,21.1597291644794,27.2335545463208));
#53979=CARTESIAN_POINT('Ctrl Pts',(-25.6963853993515,21.145953006266,27.2348162232521));
#53980=CARTESIAN_POINT('Ctrl Pts',(-25.6500887074748,21.1051565766362,27.2385634401385));
#53981=CARTESIAN_POINT('Ctrl Pts',(-25.618739539945,21.078579406316,27.2410192488098));
#53982=CARTESIAN_POINT('Ctrl Pts',(-25.5263522252921,21.0032446822363,27.2480526939295));
#53983=CARTESIAN_POINT('Ctrl Pts',(-25.464036723143,20.9560955162728,27.2525470872287));
#53984=CARTESIAN_POINT('Ctrl Pts',(-25.1058498441037,20.7050233856249,27.2773907496014));
#53985=CARTESIAN_POINT('Ctrl Pts',(-24.7792507677546,20.5494557495119,27.2967378105584));
#53986=CARTESIAN_POINT('Ctrl Pts',(-24.4140977229529,20.4453684886603,27.3196999507841));
#53987=CARTESIAN_POINT('Ctrl Pts',(-24.3944337164012,20.4399645172474,27.3209391269503));
#53988=CARTESIAN_POINT('Ctrl Pts',(-24.3686738602927,20.4331475914606,27.3225663040356));
#53989=CARTESIAN_POINT('Ctrl Pts',(-24.362623017741,20.4315651680647,27.3229487950949));
#53990=CARTESIAN_POINT('Ctrl Pts',(-24.3532930672447,20.4291541834139,27.3235390065003));
#53991=CARTESIAN_POINT('Ctrl Pts',(-24.3500171737522,20.4283131475052,27.3237463222452));
#53992=CARTESIAN_POINT('Ctrl Pts',(-24.3435654315749,20.4266675818825,27.3241547885204));
#53993=CARTESIAN_POINT('Ctrl Pts',(-24.3403896674157,20.4258627348802,27.3243559284966));
#53994=CARTESIAN_POINT('Ctrl Pts',(-24.333388687487,20.424099804423,27.3247995188891));
#53995=CARTESIAN_POINT('Ctrl Pts',(-24.3295629336645,20.423143897525,27.3250420393965));
#53996=CARTESIAN_POINT('Ctrl Pts',(-24.3216346509618,20.4211783812999,27.3255448700825));
#53997=CARTESIAN_POINT('Ctrl Pts',(-24.3175318738928,20.4201698134016,27.325805213452));
#53998=CARTESIAN_POINT('Ctrl Pts',(-24.3070366382876,20.4176116899691,27.326471544544));
#53999=CARTESIAN_POINT('Ctrl Pts',(-24.3006414202909,20.4160736372982,27.3268779032427));
#54000=CARTESIAN_POINT('Ctrl Pts',(-24.2821957166974,20.4116971302992,27.3280509444554));
#54001=CARTESIAN_POINT('Ctrl Pts',(-24.2701336260797,20.4089085459533,27.32881923142));
#54002=CARTESIAN_POINT('Ctrl Pts',(-24.1524395267564,20.3824128043248,27.336327877405));
#54003=CARTESIAN_POINT('Ctrl Pts',(-24.0457037103836,20.363975494389,27.343236621469));
#54004=CARTESIAN_POINT('Ctrl Pts',(-23.6481260920866,20.3157588418114,27.3693579170136));
#54005=CARTESIAN_POINT('Ctrl Pts',(-23.3546184897718,20.3202038204604,27.38955007316));
#54006=CARTESIAN_POINT('Ctrl Pts',(-23.0375823867764,20.3684135808812,27.410819513959));
#54007=CARTESIAN_POINT('Ctrl Pts',(-23.0094640476387,20.3730717548855,27.4126995840299));
#54008=CARTESIAN_POINT('Ctrl Pts',(-22.971415572815,20.3798947525046,27.4152319490993));
#54009=CARTESIAN_POINT('Ctrl Pts',(-22.9614290834225,20.3817343252777,27.4158955176354));
#54010=CARTESIAN_POINT('Ctrl Pts',(-22.9475756134337,20.3843539778636,27.4168143663633));
#54011=CARTESIAN_POINT('Ctrl Pts',(-22.9437012138919,20.3850939858912,27.4170711593587));
#54012=CARTESIAN_POINT('Ctrl Pts',(-22.9372451691874,20.3863393760984,27.4174987494476));
#54013=CARTESIAN_POINT('Ctrl Pts',(-22.9346627761465,20.3868408076865,27.4176697003247));
#54014=CARTESIAN_POINT('Ctrl Pts',(-22.9227430016417,20.3891704572956,27.4184583788062));
#54015=CARTESIAN_POINT('Ctrl Pts',(-22.9134130305478,20.3910368781875,27.4190745842761));
#54016=CARTESIAN_POINT('Ctrl Pts',(-22.9011913622054,20.3935381127195,27.4198801917714));
#54017=CARTESIAN_POINT('Ctrl Pts',(-22.8982921773616,20.3941356103474,27.4200711784609));
#54018=CARTESIAN_POINT('Ctrl Pts',(-22.889751807307,20.3959079787457,27.4206334312569));
#54019=CARTESIAN_POINT('Ctrl Pts',(-22.8841129136074,20.3970939920961,27.4210042126531));
#54020=CARTESIAN_POINT('Ctrl Pts',(-22.8436380890675,20.4057203742661,27.4236622027573));
#54021=CARTESIAN_POINT('Ctrl Pts',(-22.8089226567796,20.4137231218494,27.4259238714752));
#54022=CARTESIAN_POINT('Ctrl Pts',(-22.7698429148051,20.4234170849069,27.4284438554017));
#54023=CARTESIAN_POINT('Ctrl Pts',(-22.7653429015337,20.4245436593678,27.4287336382437));
#54024=CARTESIAN_POINT('Ctrl Pts',(-22.7585414664707,20.4262620070365,27.4291710136679));
#54025=CARTESIAN_POINT('Ctrl Pts',(-22.7562382652036,20.4268466096842,27.4293190182633));
#54026=CARTESIAN_POINT('Ctrl Pts',(-22.7522365205823,20.427867052053,27.4295759853162));
#54027=CARTESIAN_POINT('Ctrl Pts',(-22.750537686657,20.4283017306523,27.429685015341));
#54028=CARTESIAN_POINT('Ctrl Pts',(-22.7469845438922,20.4292139595574,27.4299129300571));
#54029=CARTESIAN_POINT('Ctrl Pts',(-22.7451303069942,20.4296917756266,27.4300317986192));
#54030=CARTESIAN_POINT('Ctrl Pts',(-22.7407002393559,20.4308375657849,27.430315628073));
#54031=CARTESIAN_POINT('Ctrl Pts',(-22.73812480031,20.4315070801371,27.4304804990021));
#54032=CARTESIAN_POINT('Ctrl Pts',(-22.7294158161583,20.4337825978779,27.4310375726947));
#54033=CARTESIAN_POINT('Ctrl Pts',(-22.7232861316412,20.435403524639,27.4314289114891));
#54034=CARTESIAN_POINT('Ctrl Pts',(-22.7087399555581,20.4392960642139,27.4323558932674));
#54035=CARTESIAN_POINT('Ctrl Pts',(-22.7003277686039,20.4415837716827,27.4328906267321));
#54036=CARTESIAN_POINT('Ctrl Pts',(-22.6019444893796,20.4687684659821,27.4391298196486));
#54037=CARTESIAN_POINT('Ctrl Pts',(-22.5130771912219,20.4975319163713,27.4446218654016));
#54038=CARTESIAN_POINT('Ctrl Pts',(-22.0544632491773,20.6683164457409,27.4728067033159));
#54039=CARTESIAN_POINT('Ctrl Pts',(-21.7120096517425,20.8737155778351,27.49377945799));
#54040=CARTESIAN_POINT('Ctrl Pts',(-21.4013826009653,21.1484154122913,27.5188828837749));
#54041=CARTESIAN_POINT('Ctrl Pts',(-21.3875564295565,21.1608574043582,27.5200138478056));
#54042=CARTESIAN_POINT('Ctrl Pts',(-21.3693915874165,21.1774905403839,27.521518177171));
#54043=CARTESIAN_POINT('Ctrl Pts',(-21.3649556803542,21.1815753488715,27.521887015983));
#54044=CARTESIAN_POINT('Ctrl Pts',(-21.358082892052,21.1879399001831,27.5224607898686));
#54045=CARTESIAN_POINT('Ctrl Pts',(-21.3556380268463,21.1902110335542,27.5226653561409));
#54046=CARTESIAN_POINT('Ctrl Pts',(-21.3507974749491,21.1947216423938,27.5230712836476));
#54047=CARTESIAN_POINT('Ctrl Pts',(-21.3484016700882,21.1969609857506,27.5232726390792));
#54048=CARTESIAN_POINT('Ctrl Pts',(-21.3430790086122,21.2019512870067,27.5237209734844));
#54049=CARTESIAN_POINT('Ctrl Pts',(-21.3401538723117,21.2047040644147,27.5239680307618));
#54050=CARTESIAN_POINT('Ctrl Pts',(-21.3340882117308,21.2104337365192,27.5244817340694));
#54051=CARTESIAN_POINT('Ctrl Pts',(-21.3309485231067,21.2134115006209,27.5247484175147));
#54052=CARTESIAN_POINT('Ctrl Pts',(-21.3228758352996,21.2210987950105,27.5254361314042));
#54053=CARTESIAN_POINT('Ctrl Pts',(-21.3179517900819,21.2258176596019,27.5258575674866));
#54054=CARTESIAN_POINT('Ctrl Pts',(-21.3036771980047,21.2395846339333,27.5270850213888));
#54055=CARTESIAN_POINT('Ctrl Pts',(-21.2943665057809,21.2486737053734,27.5278928297702));
#54056=CARTESIAN_POINT('Ctrl Pts',(-21.2014485395632,21.3404854430537,27.536027696977));
#54057=CARTESIAN_POINT('Ctrl Pts',(-21.1223838088231,21.4276601242072,27.5435539274481));
#54058=CARTESIAN_POINT('Ctrl Pts',(-20.8397993811679,21.7757239019829,27.5729094889668));
#54059=CARTESIAN_POINT('Ctrl Pts',(-20.6721349275666,22.0630063860666,27.5960029633228));
#54060=CARTESIAN_POINT('Ctrl Pts',(-20.5472706802057,22.380497178921,27.6181112965073));
#54061=CARTESIAN_POINT('Ctrl Pts',(-20.5434792949456,22.3902774051277,27.6187889734273));
#54062=CARTESIAN_POINT('Ctrl Pts',(-20.5256350809092,22.4369835498124,27.6220086871245));
#54063=CARTESIAN_POINT('Ctrl Pts',(-20.512213561853,22.4741493203482,27.624521500742));
#54064=CARTESIAN_POINT('Ctrl Pts',(-20.4977673924332,22.5165793663981,27.6273272823384));
#54065=CARTESIAN_POINT('Ctrl Pts',(-20.496068995794,22.5216084396691,27.6276588455048));
#54066=CARTESIAN_POINT('Ctrl Pts',(-20.4936055899177,22.5289626478279,27.6281422257942));
#54067=CARTESIAN_POINT('Ctrl Pts',(-20.4928308033975,22.5312844610493,27.6282946200396));
#54068=CARTESIAN_POINT('Ctrl Pts',(-20.4914637244077,22.5353968022075,27.6285641541264));
#54069=CARTESIAN_POINT('Ctrl Pts',(-20.4908703581276,22.5371869684705,27.6286813580655));
#54070=CARTESIAN_POINT('Ctrl Pts',(-20.4896344374464,22.5409266887467,27.6289259319619));
#54071=CARTESIAN_POINT('Ctrl Pts',(-20.4889921755184,22.5428763319349,27.6290532842275));
#54072=CARTESIAN_POINT('Ctrl Pts',(-20.4873192994737,22.547970869718,27.62938566878));
#54073=CARTESIAN_POINT('Ctrl Pts',(-20.4862916627405,22.5511167507667,27.6295905238155));
#54074=CARTESIAN_POINT('Ctrl Pts',(-20.4818440391499,22.5648035516745,27.6304801036122));
#54075=CARTESIAN_POINT('Ctrl Pts',(-20.4784735350793,22.5753606537141,27.6311619271138));
#54076=CARTESIAN_POINT('Ctrl Pts',(-20.4544231268978,22.6520545818143,27.6360851488371));
#54077=CARTESIAN_POINT('Ctrl Pts',(-20.4358248696428,22.7188313181952,27.6402103518796));
#54078=CARTESIAN_POINT('Ctrl Pts',(-20.3739100262168,22.9725270442527,27.6554594332074));
#54079=CARTESIAN_POINT('Ctrl Pts',(-20.3451543045787,23.1625974644635,27.6660486351879));
#54080=CARTESIAN_POINT('Ctrl Pts',(-20.3191572901728,23.5889542391757,27.6899572850673));
#54081=CARTESIAN_POINT('Ctrl Pts',(-20.3305983639806,23.8246197288227,27.7033167957185));
#54082=CARTESIAN_POINT('Ctrl Pts',(-20.3698698738081,24.0713051023975,27.718476399373));
#54083=CARTESIAN_POINT('Ctrl Pts',(-20.3722567850523,24.0856707378248,27.7193632324363));
#54084=CARTESIAN_POINT('Ctrl Pts',(-20.3756714690803,24.1053943096399,27.7205865136477));
#54085=CARTESIAN_POINT('Ctrl Pts',(-20.3766156303009,24.1107667012417,27.7209202972989));
#54086=CARTESIAN_POINT('Ctrl Pts',(-20.3781391738528,24.1193085823367,27.7214519328993));
#54087=CARTESIAN_POINT('Ctrl Pts',(-20.3787096806937,24.1224796613499,27.7216495015595));
#54088=CARTESIAN_POINT('Ctrl Pts',(-20.3798753041776,24.1289033168727,27.7220501337541));
#54089=CARTESIAN_POINT('Ctrl Pts',(-20.3804706730015,24.1321558433523,27.7222532051284));
#54090=CARTESIAN_POINT('Ctrl Pts',(-20.3818466485864,24.1396080859988,27.7227189856311));
#54091=CARTESIAN_POINT('Ctrl Pts',(-20.3826306004717,24.1438071711841,27.7229818013035));
#54092=CARTESIAN_POINT('Ctrl Pts',(-20.3842908795108,24.1526031595796,27.723533100004));
#54093=CARTESIAN_POINT('Ctrl Pts',(-20.3851688748428,24.1571997343158,27.7238216358814));
#54094=CARTESIAN_POINT('Ctrl Pts',(-20.3875103833517,24.1693149988796,27.7245833035799));
#54095=CARTESIAN_POINT('Ctrl Pts',(-20.3889906893279,24.1768303780561,27.7250569721817));
#54096=CARTESIAN_POINT('Ctrl Pts',(-20.3934976711492,24.1992893446802,27.7264760765324));
#54097=CARTESIAN_POINT('Ctrl Pts',(-20.3966035849002,24.2142166434354,27.7274240453669));
#54098=CARTESIAN_POINT('Ctrl Pts',(-20.4079331102722,24.2667937676483,27.7307801134687));
#54099=CARTESIAN_POINT('Ctrl Pts',(-20.4167257314593,24.3043163710793,27.7332063342722));
#54100=CARTESIAN_POINT('Ctrl Pts',(-20.4623139241014,24.4842722630159,27.7449967493157));
#54101=CARTESIAN_POINT('Ctrl Pts',(-20.5081554938185,24.6242140151136,27.7546463011361));
#54102=CARTESIAN_POINT('Ctrl Pts',(-20.6741517893392,25.033882329867,27.7842219637196));
#54103=CARTESIAN_POINT('Ctrl Pts',(-20.8219167530609,25.2907425579738,27.8047015212794));
#54104=CARTESIAN_POINT('Ctrl Pts',(-21.0121190377125,25.5362635201789,27.8243465830336));
#54105=CARTESIAN_POINT('Ctrl Pts',(-21.021769544954,25.548535566931,27.8253283232041));
#54106=CARTESIAN_POINT('Ctrl Pts',(-21.0337159365839,25.5635020547531,27.8265248689699));
#54107=CARTESIAN_POINT('Ctrl Pts',(-21.035927358597,25.5662631965599,27.8267455862883));
#54108=CARTESIAN_POINT('Ctrl Pts',(-21.0395903844625,25.5708213826238,27.8271098939513));
#54109=CARTESIAN_POINT('Ctrl Pts',(-21.0410393742911,25.572620507527,27.827253671413));
#54110=CARTESIAN_POINT('Ctrl Pts',(-21.0435451037207,25.5757248848473,27.8275017293103));
#54111=CARTESIAN_POINT('Ctrl Pts',(-21.0446009272821,25.5770308669344,27.8276060759109));
#54112=CARTESIAN_POINT('Ctrl Pts',(-21.0469750606858,25.579962818239,27.82784031506));
#54113=CARTESIAN_POINT('Ctrl Pts',(-21.0482939317837,25.581588325835,27.827970165904));
#54114=CARTESIAN_POINT('Ctrl Pts',(-21.0518161929987,25.5859208757361,27.8283162301519));
#54115=CARTESIAN_POINT('Ctrl Pts',(-21.0540224066314,25.5886256350419,27.8285322385175));
#54116=CARTESIAN_POINT('Ctrl Pts',(-21.0643698071359,25.6012692800458,27.8295418520452));
#54117=CARTESIAN_POINT('Ctrl Pts',(-21.0725661340474,25.6111631921255,27.8303314972888));
#54118=CARTESIAN_POINT('Ctrl Pts',(-21.2701981508566,25.8468446253154,27.8491392604071));
#54119=CARTESIAN_POINT('Ctrl Pts',(-21.4896959486678,26.0456798741573,27.8650455520782));
#54120=CARTESIAN_POINT('Ctrl Pts',(-21.8429133622767,26.2868114479692,27.8891137015016));
#54121=CARTESIAN_POINT('Ctrl Pts',(-21.9570772617629,26.3548047014022,27.8966842956439));
#54122=CARTESIAN_POINT('Ctrl Pts',(-22.0750363456406,26.4155369446113,27.9044917472066));
#54123=CARTESIAN_POINT('Origin',(-23.5502525316942,23.5502525316942,-77.3107734492734));
#54124=CARTESIAN_POINT('',(-22.0750360153459,26.4155367745562,29.4036987823186));
#54125=CARTESIAN_POINT('',(-22.0750360153802,26.4155367745738,29.1557101328919));
#54126=CARTESIAN_POINT('',(-22.0750360153461,26.4155367745563,-77.3107734492734));
#54127=CARTESIAN_POINT('',(-26.7730011212944,23.5472374479352,28.5607734493046));
#54128=CARTESIAN_POINT('Ctrl Pts',(-26.7730011212944,23.5472374479352,28.5607734493046));
#54129=CARTESIAN_POINT('Ctrl Pts',(-26.7728770430253,23.4146132495376,28.5689619155671));
#54130=CARTESIAN_POINT('Ctrl Pts',(-26.7645626120231,23.2823550477187,28.5771503818296));
#54131=CARTESIAN_POINT('Ctrl Pts',(-26.7482144162662,23.1513072380455,28.5853388480921));
#54132=CARTESIAN_POINT('Ctrl Pts',(-26.733272166814,23.0315295517846,28.59282310552));
#54133=CARTESIAN_POINT('Ctrl Pts',(-26.7116191815025,22.9127623390399,28.6003073629479));
#54134=CARTESIAN_POINT('Ctrl Pts',(-26.6834084421646,22.7956323602277,28.6077916203757));
#54135=CARTESIAN_POINT('Ctrl Pts',(-26.6601379603629,22.6990141536737,28.6139652365362));
#54136=CARTESIAN_POINT('Ctrl Pts',(-26.6323532111562,22.6033035052964,28.6201388526966));
#54137=CARTESIAN_POINT('Ctrl Pts',(-26.6001402414619,22.5089540536834,28.6263124688571));
#54138=CARTESIAN_POINT('Ctrl Pts',(-26.5679709395546,22.4147325018507,28.6324777160854));
#54139=CARTESIAN_POINT('Ctrl Pts',(-26.5313854877104,22.3218688864176,28.6386429633138));
#54140=CARTESIAN_POINT('Ctrl Pts',(-26.4905206292591,22.2308052697916,28.6448082105422));
#54141=CARTESIAN_POINT('Ctrl Pts',(-26.4496991068733,22.1398382236423,28.6509669196944));
#54142=CARTESIAN_POINT('Ctrl Pts',(-26.4046073770992,22.0506677752294,28.6571256288465));
#54143=CARTESIAN_POINT('Ctrl Pts',(-26.3554312203936,21.9637185462508,28.6632843379987));
#54144=CARTESIAN_POINT('Ctrl Pts',(-26.3062911453097,21.8768331138232,28.6694385283713));
#54145=CARTESIAN_POINT('Ctrl Pts',(-26.2530728147334,21.7921660373047,28.6755927187439));
#54146=CARTESIAN_POINT('Ctrl Pts',(-26.196008722109,21.710118910627,28.6817469091165));
#54147=CARTESIAN_POINT('Ctrl Pts',(-26.1389663707552,21.6281030436909,28.6878987547585));
#54148=CARTESIAN_POINT('Ctrl Pts',(-26.0780814164171,21.5487054992064,28.6940506004006));
#54149=CARTESIAN_POINT('Ctrl Pts',(-26.0136301234778,21.4722995960389,28.7002024460427));
#54150=CARTESIAN_POINT('Ctrl Pts',(-25.9491861651483,21.3959023879257,28.7063535915997));
#54151=CARTESIAN_POINT('Ctrl Pts',(-25.8811769550647,21.3224964761269,28.7125047371567));
#54152=CARTESIAN_POINT('Ctrl Pts',(-25.8099189146665,21.2524219460842,28.7186558827137));
#54153=CARTESIAN_POINT('Ctrl Pts',(-25.7386499437626,21.1823366670784,28.7248079718152));
#54154=CARTESIAN_POINT('Ctrl Pts',(-25.6641314623008,21.1155840892799,28.7309600609167));
#54155=CARTESIAN_POINT('Ctrl Pts',(-25.5867158622222,21.0524665789123,28.7371121500182));
#54156=CARTESIAN_POINT('Ctrl Pts',(-25.509217864773,20.9892818893599,28.7432707871018));
#54157=CARTESIAN_POINT('Ctrl Pts',(-25.4288169282932,20.9297402681568,28.7494294241854));
#54158=CARTESIAN_POINT('Ctrl Pts',(-25.3458974682944,20.8741029050549,28.755588061269));
#54159=CARTESIAN_POINT('Ctrl Pts',(-25.2629319668925,20.8184346490568,28.7617501179636));
#54160=CARTESIAN_POINT('Ctrl Pts',(-25.1774455283915,20.7666751934139,28.7679121746582));
#54161=CARTESIAN_POINT('Ctrl Pts',(-25.0898486030466,20.7190405121562,28.7740742313527));
#54162=CARTESIAN_POINT('Ctrl Pts',(-25.0021056968023,20.6713264473633,28.7802465571586));
#54163=CARTESIAN_POINT('Ctrl Pts',(-24.9122456691325,20.6277510771515,28.7864188829645));
#54164=CARTESIAN_POINT('Ctrl Pts',(-24.8207005657972,20.5884828993386,28.7925912087704));
#54165=CARTESIAN_POINT('Ctrl Pts',(-24.7510549962827,20.5586085040085,28.7972869830972));
#54166=CARTESIAN_POINT('Ctrl Pts',(-24.6804345781804,20.5312260596704,28.801982757424));
#54167=CARTESIAN_POINT('Ctrl Pts',(-24.6090348746265,20.5063902626691,28.8066785317507));
#54168=CARTESIAN_POINT('Ctrl Pts',(-24.5151585414876,20.4737361557608,28.8128525360266));
#54169=CARTESIAN_POINT('Ctrl Pts',(-24.4196057560507,20.4453718170294,28.8190265403026));
#54170=CARTESIAN_POINT('Ctrl Pts',(-24.3228048326036,20.4214699401964,28.8252005445785));
#54171=CARTESIAN_POINT('Ctrl Pts',(-24.2261346830957,20.3976003537846,28.8313662080367));
#54172=CARTESIAN_POINT('Ctrl Pts',(-24.12822016485,20.3781813497186,28.8375318714949));
#54173=CARTESIAN_POINT('Ctrl Pts',(-24.0295072351286,20.3633367041682,28.8436975349531));
#54174=CARTESIAN_POINT('Ctrl Pts',(-23.9308985456846,20.3485077344767,28.8498566875067));
#54175=CARTESIAN_POINT('Ctrl Pts',(-23.8314935478987,20.33824358386,28.8560158400603));
#54176=CARTESIAN_POINT('Ctrl Pts',(-23.7317500115561,20.3326173399262,28.8621749926138));
#54177=CARTESIAN_POINT('Ctrl Pts',(-23.6320790295015,20.3269951885697,28.868329664948));
#54178=CARTESIAN_POINT('Ctrl Pts',(-23.5320704305932,20.3260042607985,28.8744843372822));
#54179=CARTESIAN_POINT('Ctrl Pts',(-23.4321878439339,20.3296658938277,28.8806390096164));
#54180=CARTESIAN_POINT('Ctrl Pts',(-23.3323429288885,20.3333261458392,28.8867913606606));
#54181=CARTESIAN_POINT('Ctrl Pts',(-23.2326243649712,20.3416354560159,28.8929437117048));
#54182=CARTESIAN_POINT('Ctrl Pts',(-23.1334956335591,20.3545630520425,28.8990960627491));
#54183=CARTESIAN_POINT('Ctrl Pts',(-23.0343778166042,20.3674892246907,28.9052477363957));
#54184=CARTESIAN_POINT('Ctrl Pts',(-22.9358501334765,20.3850326160794,28.9113994100423));
#54185=CARTESIAN_POINT('Ctrl Pts',(-22.8383697942054,20.4071107069326,28.9175510836889));
#54186=CARTESIAN_POINT('Ctrl Pts',(-22.7408741555218,20.4291922629135,28.9237037228327));
#54187=CARTESIAN_POINT('Ctrl Pts',(-22.644426610603,20.4558098361482,28.9298563619764));
#54188=CARTESIAN_POINT('Ctrl Pts',(-22.5494720627858,20.486830259863,28.9360090011202));
#54189=CARTESIAN_POINT('Ctrl Pts',(-22.4544159917333,20.5178838499068,28.9421682185253));
#54190=CARTESIAN_POINT('Ctrl Pts',(-22.3608565188245,20.5533495556489,28.9483274359304));
#54191=CARTESIAN_POINT('Ctrl Pts',(-22.2692212022268,20.5930450152316,28.9544866533355));
#54192=CARTESIAN_POINT('Ctrl Pts',(-22.1775347462838,20.6327626278431,28.9606493080436));
#54193=CARTESIAN_POINT('Ctrl Pts',(-22.0877749750697,20.6767145044222,28.9668119627517));
#54194=CARTESIAN_POINT('Ctrl Pts',(-22.0003454654848,20.724671945582,28.9729746174598));
#54195=CARTESIAN_POINT('Ctrl Pts',(-21.9127699496478,20.7727094751042,28.9791475637287));
#54196=CARTESIAN_POINT('Ctrl Pts',(-21.827532839302,20.8247657045023,28.9853205099976));
#54197=CARTESIAN_POINT('Ctrl Pts',(-21.7450094316521,20.8805681098476,28.9914934562665));
#54198=CARTESIAN_POINT('Ctrl Pts',(-21.6823020275795,20.9229709150621,28.9961841185529));
#54199=CARTESIAN_POINT('Ctrl Pts',(-21.6211609510266,20.9675358869179,29.0008747808392));
#54200=CARTESIAN_POINT('Ctrl Pts',(-21.5617373904308,21.0141285017094,29.0055654431255));
#54201=CARTESIAN_POINT('Ctrl Pts',(-21.4836644003982,21.0753436950391,29.0117282180629));
#54202=CARTESIAN_POINT('Ctrl Pts',(-21.4082807768226,21.1402771855626,29.0178909930002));
#54203=CARTESIAN_POINT('Ctrl Pts',(-21.3359627690922,21.2086636673254,29.0240537679376));
#54204=CARTESIAN_POINT('Ctrl Pts',(-21.2637431363746,21.2769571221751,29.0302081595817));
#54205=CARTESIAN_POINT('Ctrl Pts',(-21.1945811452636,21.3486939361772,29.0363625512258));
#54206=CARTESIAN_POINT('Ctrl Pts',(-21.1288215339032,21.4235674385417,29.0425169428699));
#54207=CARTESIAN_POINT('Ctrl Pts',(-21.0631317896435,21.498361390641,29.0486647957057));
#54208=CARTESIAN_POINT('Ctrl Pts',(-21.0008375249201,21.5762850804529,29.0548126485414));
#54209=CARTESIAN_POINT('Ctrl Pts',(-20.9422472978569,21.6569944238872,29.0609605013771));
#54210=CARTESIAN_POINT('Ctrl Pts',(-20.8836997349241,21.737644996531,29.06710387748));
#54211=CARTESIAN_POINT('Ctrl Pts',(-20.8288511029882,21.8210768387006,29.0732472535828));
#54212=CARTESIAN_POINT('Ctrl Pts',(-20.777969646471,21.9069128933971,29.0793906296856));
#54213=CARTESIAN_POINT('Ctrl Pts',(-20.7271073720606,21.9927165882423,29.0855316897601));
#54214=CARTESIAN_POINT('Ctrl Pts',(-20.6802095235959,22.0809223203237,29.0916727498346));
#54215=CARTESIAN_POINT('Ctrl Pts',(-20.6375004593718,22.1711249351021,29.097813809909));
#54216=CARTESIAN_POINT('Ctrl Pts',(-20.5947959805517,22.2613178653924,29.1039542106565));
#54217=CARTESIAN_POINT('Ctrl Pts',(-20.5562795784705,22.35350685826,29.1100946114039));
#54218=CARTESIAN_POINT('Ctrl Pts',(-20.5221287030737,22.4472640272027,29.1162350121513));
#54219=CARTESIAN_POINT('Ctrl Pts',(-20.4879722860564,22.5410364100055,29.122376409294));
#54220=CARTESIAN_POINT('Ctrl Pts',(-20.4581829518959,22.6363770647411,29.1285178064367));
#54221=CARTESIAN_POINT('Ctrl Pts',(-20.4328888926931,22.7328410657029,29.1346592035794));
#54222=CARTESIAN_POINT('Ctrl Pts',(-20.4075672588473,22.8294102281326,29.1408072958449));
#54223=CARTESIAN_POINT('Ctrl Pts',(-20.3867507965031,22.9271047597847,29.1469553881104));
#54224=CARTESIAN_POINT('Ctrl Pts',(-20.3705169339306,23.0254677274028,29.153103480376));
#54225=CARTESIAN_POINT('Ctrl Pts',(-20.3542738710606,23.1238864407539,29.1592550569804));
#54226=CARTESIAN_POINT('Ctrl Pts',(-20.3426186303105,23.2229739115664,29.1654066335848));
#54227=CARTESIAN_POINT('Ctrl Pts',(-20.335576687458,23.322268367805,29.1715582101892));
#54228=CARTESIAN_POINT('Ctrl Pts',(-20.3285227426266,23.4217320571646,29.1777202712713));
#54229=CARTESIAN_POINT('Ctrl Pts',(-20.3260978114541,23.5214030007143,29.1838823323533));
#54230=CARTESIAN_POINT('Ctrl Pts',(-20.3282752106598,23.6208195582726,29.1900443934354));
#54231=CARTESIAN_POINT('Ctrl Pts',(-20.3299722555587,23.6983039081485,29.1948470471237));
#54232=CARTESIAN_POINT('Ctrl Pts',(-20.3344639246531,23.7756337186087,29.1996497008121));
#54233=CARTESIAN_POINT('Ctrl Pts',(-20.3417159218685,23.8525940371284,29.2044523545004));
#54234=CARTESIAN_POINT('Ctrl Pts',(-20.3510543363531,23.9516960268091,29.2106367433571));
#54235=CARTESIAN_POINT('Ctrl Pts',(-20.3650046499201,24.0505365678241,29.2168211322138));
#54236=CARTESIAN_POINT('Ctrl Pts',(-20.3835453683844,24.1486531536376,29.2230055210705));
#54237=CARTESIAN_POINT('Ctrl Pts',(-20.4020609124087,24.2466365175319,29.2291815128132));
#54238=CARTESIAN_POINT('Ctrl Pts',(-20.4251543921595,24.343897458819,29.2353575045559));
#54239=CARTESIAN_POINT('Ctrl Pts',(-20.4527524934316,24.4399778125889,29.2415334962986));
#54240=CARTESIAN_POINT('Ctrl Pts',(-20.4803211919858,24.5359558033916,29.2477029082067));
#54241=CARTESIAN_POINT('Ctrl Pts',(-20.5123848512336,24.6307552940067,29.2538723201149));
#54242=CARTESIAN_POINT('Ctrl Pts',(-20.5488191522555,24.7239284798551,29.260041732023));
#54243=CARTESIAN_POINT('Ctrl Pts',(-20.5852261414904,24.8170318214594,29.2662065192324));
#54244=CARTESIAN_POINT('Ctrl Pts',(-20.625997100487,24.9085108808592,29.2723713064417));
#54245=CARTESIAN_POINT('Ctrl Pts',(-20.6709582176269,24.9979340627913,29.2785360936511));
#54246=CARTESIAN_POINT('Ctrl Pts',(-20.7159017341586,25.0873222388674,29.2846984675752));
#54247=CARTESIAN_POINT('Ctrl Pts',(-20.7650319550941,25.1746557508006,29.2908608414993));
#54248=CARTESIAN_POINT('Ctrl Pts',(-20.8181277354351,25.2595247920922,29.2970232154234));
#54249=CARTESIAN_POINT('Ctrl Pts',(-20.8712167881162,25.3443830797978,29.3031848085254));
#54250=CARTESIAN_POINT('Ctrl Pts',(-20.9282701716987,25.4267771510795,29.3093464016274));
#54251=CARTESIAN_POINT('Ctrl Pts',(-20.9890222710729,25.506324389929,29.3155079947294));
#54252=CARTESIAN_POINT('Ctrl Pts',(-21.0497827567766,25.5858826096227,29.3216704383889));
#54253=CARTESIAN_POINT('Ctrl Pts',(-21.1142427097965,25.6625928725552,29.3278328820483));
#54254=CARTESIAN_POINT('Ctrl Pts',(-21.1820955375943,25.7361047713928,29.3339953257078));
#54255=CARTESIAN_POINT('Ctrl Pts',(-21.2500181805297,25.8096923081,29.3401641100293));
#54256=CARTESIAN_POINT('Ctrl Pts',(-21.3213403757397,25.8800745904679,29.3463328943509));
#54257=CARTESIAN_POINT('Ctrl Pts',(-21.395717967883,25.9469374037295,29.3525016786724));
#54258=CARTESIAN_POINT('Ctrl Pts',(-21.4701355884634,26.0138362011342,29.3586737829024));
#54259=CARTESIAN_POINT('Ctrl Pts',(-21.5476115464694,26.0772114826441,29.3648458871323));
#54260=CARTESIAN_POINT('Ctrl Pts',(-21.6277694384365,26.1367900471071,29.3710179913623));
#54261=CARTESIAN_POINT('Ctrl Pts',(-21.7080572364831,26.1964651662266,29.3772000982737));
#54262=CARTESIAN_POINT('Ctrl Pts',(-21.7910352916877,26.2523310354384,29.3833822051852));
#54263=CARTESIAN_POINT('Ctrl Pts',(-21.8762990308253,26.3041583469734,29.3895643120967));
#54264=CARTESIAN_POINT('Ctrl Pts',(-21.9396271745814,26.3426521717644,29.3941559633562));
#54265=CARTESIAN_POINT('Ctrl Pts',(-22.0042156407435,26.3789190481311,29.3987476146158));
#54266=CARTESIAN_POINT('Ctrl Pts',(-22.0698912045492,26.4128820752422,29.4033392658753));
#54267=CARTESIAN_POINT('Ctrl Pts',(-22.0716052898007,26.4137684859632,29.4034591046898));
#54268=CARTESIAN_POINT('Ctrl Pts',(-22.0733202276715,26.4146533863471,29.4035789435042));
#54269=CARTESIAN_POINT('Ctrl Pts',(-22.0750360153459,26.4155367745562,29.4036987823186));
#54270=CARTESIAN_POINT('Ctrl Pts',(-26.7730011251471,23.5472415688628,28.5608472020237));
#54271=CARTESIAN_POINT('Ctrl Pts',(-26.7732052327801,23.7657057692041,28.5486405204165));
#54272=CARTESIAN_POINT('Ctrl Pts',(-26.7511964717817,23.9836060593955,28.5363786813096));
#54273=CARTESIAN_POINT('Ctrl Pts',(-26.6975842485767,24.2450678492038,28.5204949993101));
#54274=CARTESIAN_POINT('Ctrl Pts',(-26.6867827696282,24.2923057258727,28.517579823793));
#54275=CARTESIAN_POINT('Ctrl Pts',(-26.6732345673099,24.3459586406051,28.5142107461922));
#54276=CARTESIAN_POINT('Ctrl Pts',(-26.6715267876305,24.3526315098634,28.5137907009532));
#54277=CARTESIAN_POINT('Ctrl Pts',(-26.6687045815779,24.3635134572781,28.5131040008554));
#54278=CARTESIAN_POINT('Ctrl Pts',(-26.6676029880457,24.3677258661197,28.5128377620448));
#54279=CARTESIAN_POINT('Ctrl Pts',(-26.6654495553398,24.3758927746728,28.5123207708302));
#54280=CARTESIAN_POINT('Ctrl Pts',(-26.6643987139196,24.379847530739,28.5120700512362));
#54281=CARTESIAN_POINT('Ctrl Pts',(-26.662559223334,24.3867175581329,28.5116338632029));
#54282=CARTESIAN_POINT('Ctrl Pts',(-26.6617740012806,24.3896337487135,28.5114485065059));
#54283=CARTESIAN_POINT('Ctrl Pts',(-26.6601297659965,24.3957061671889,28.5110621101178));
#54284=CARTESIAN_POINT('Ctrl Pts',(-26.6592700446441,24.398862198296,28.5108610475363));
#54285=CARTESIAN_POINT('Ctrl Pts',(-26.656895218863,24.4075281182112,28.5103083018023));
#54286=CARTESIAN_POINT('Ctrl Pts',(-26.6553702676289,24.4130352750817,28.5099562978897));
#54287=CARTESIAN_POINT('Ctrl Pts',(-26.6494321890629,24.4342601887979,28.5085967908123));
#54288=CARTESIAN_POINT('Ctrl Pts',(-26.6449143593179,24.4499481709622,28.5075858730496));
#54289=CARTESIAN_POINT('Ctrl Pts',(-26.5682243849988,24.7088375135347,28.4908009274684));
#54290=CARTESIAN_POINT('Ctrl Pts',(-26.4677199651157,24.9426619677442,28.4740341061042));
#54291=CARTESIAN_POINT('Ctrl Pts',(-26.3181482739264,25.2015963512007,28.4538243368009));
#54292=CARTESIAN_POINT('Ctrl Pts',(-26.2945847993518,25.2404666075435,28.4507462420151));
#54293=CARTESIAN_POINT('Ctrl Pts',(-26.2468732310488,25.3155420147868,28.4447248746834));
#54294=CARTESIAN_POINT('Ctrl Pts',(-26.2227979264607,25.3517828079685,28.441782062865));
#54295=CARTESIAN_POINT('Ctrl Pts',(-26.1340127413415,25.4797335394188,28.4312832000252));
#54296=CARTESIAN_POINT('Ctrl Pts',(-26.0652505777227,25.5685445966407,28.4237880085619));
#54297=CARTESIAN_POINT('Ctrl Pts',(-25.9617489097634,25.6886981409627,28.4135279749305));
#54298=CARTESIAN_POINT('Ctrl Pts',(-25.9307532497951,25.7231495138557,28.4105714585326));
#54299=CARTESIAN_POINT('Ctrl Pts',(-25.8962741622837,25.7598489186474,28.4074172765493));
#54300=CARTESIAN_POINT('Ctrl Pts',(-25.8935193960734,25.7627701219398,28.4071661765245));
#54301=CARTESIAN_POINT('Ctrl Pts',(-25.8890424176267,25.7674998495487,28.4067595775438));
#54302=CARTESIAN_POINT('Ctrl Pts',(-25.8873235607179,25.7693115224541,28.4066038239335));
#54303=CARTESIAN_POINT('Ctrl Pts',(-25.8839997423051,25.7728066771356,28.4063033213533));
#54304=CARTESIAN_POINT('Ctrl Pts',(-25.8823950615293,25.7744904220894,28.4061585508721));
#54305=CARTESIAN_POINT('Ctrl Pts',(-25.8794997381004,25.7775218229659,28.4058978965794));
#54306=CARTESIAN_POINT('Ctrl Pts',(-25.8782097531349,25.7788700896399,28.4057819625563));
#54307=CARTESIAN_POINT('Ctrl Pts',(-25.8754343976114,25.7817657971123,28.4055329601953));
#54308=CARTESIAN_POINT('Ctrl Pts',(-25.8739486573939,25.7833128709595,28.4053999219466));
#54309=CARTESIAN_POINT('Ctrl Pts',(-25.8699464878757,25.7874719368959,28.4050422518339));
#54310=CARTESIAN_POINT('Ctrl Pts',(-25.8674271824342,25.7900811759505,28.4048178445526));
#54311=CARTESIAN_POINT('Ctrl Pts',(-25.855854113568,25.8020269540329,28.4037903318898));
#54312=CARTESIAN_POINT('Ctrl Pts',(-25.8467481239361,25.8113130598078,28.4029912601999));
#54313=CARTESIAN_POINT('Ctrl Pts',(-25.6830586238193,25.9762313004227,28.3887884107199));
#54314=CARTESIAN_POINT('Ctrl Pts',(-25.5130117965697,26.1157629175801,28.3765642749067));
#54315=CARTESIAN_POINT('Ctrl Pts',(-25.2325058369869,26.3015867985429,28.3577627383615));
#54316=CARTESIAN_POINT('Ctrl Pts',(-25.1314851885689,26.3608607272297,28.351230950272));
#54317=CARTESIAN_POINT('Ctrl Pts',(-24.9240760554497,26.467830237088,28.337956983082));
#54318=CARTESIAN_POINT('Ctrl Pts',(-24.8178824683506,26.5155115583233,28.3312259744154));
#54319=CARTESIAN_POINT('Ctrl Pts',(-24.6780767387035,26.5694003436548,28.3223058079386));
#54320=CARTESIAN_POINT('Ctrl Pts',(-24.6466173586655,26.5809661427991,28.3202952161408));
#54321=CARTESIAN_POINT('Ctrl Pts',(-24.5953835567667,26.5988997659439,28.3170125701837));
#54322=CARTESIAN_POINT('Ctrl Pts',(-24.5757174545188,26.6055709241279,28.3157505872963));
#54323=CARTESIAN_POINT('Ctrl Pts',(-24.5517423539163,26.6134462367334,28.3142093292167));
#54324=CARTESIAN_POINT('Ctrl Pts',(-24.5474932248197,26.6148321991631,28.3139360657904));
#54325=CARTESIAN_POINT('Ctrl Pts',(-24.5392675926891,26.6174962810254,28.3134068630366));
#54326=CARTESIAN_POINT('Ctrl Pts',(-24.5352914589502,26.6187755184446,28.3131509611152));
#54327=CARTESIAN_POINT('Ctrl Pts',(-24.5284223217407,26.6209707917981,28.3127087004477));
#54328=CARTESIAN_POINT('Ctrl Pts',(-24.5255304837352,26.6218904802903,28.3125224622548));
#54329=CARTESIAN_POINT('Ctrl Pts',(-24.5195473490813,26.623783989798,28.3121370334584));
#54330=CARTESIAN_POINT('Ctrl Pts',(-24.5164558746813,26.6247572343818,28.3119378241248));
#54331=CARTESIAN_POINT('Ctrl Pts',(-24.5080699203258,26.6273833667659,28.311397284801));
#54332=CARTESIAN_POINT('Ctrl Pts',(-24.5027726508505,26.6290272470804,28.3110556592819));
#54333=CARTESIAN_POINT('Ctrl Pts',(-24.4829904286147,26.6351102428535,28.3097792126744));
#54334=CARTESIAN_POINT('Ctrl Pts',(-24.46847865157,26.6394608222807,28.3088414936667));
#54335=CARTESIAN_POINT('Ctrl Pts',(-24.2209512445699,26.7117704440484,28.2928223847464));
#54336=CARTESIAN_POINT('Ctrl Pts',(-23.9810734928331,26.7532790394524,28.2768391948932));
#54337=CARTESIAN_POINT('Ctrl Pts',(-23.581482004816,26.7767050619091,28.2498291584829));
#54338=CARTESIAN_POINT('Ctrl Pts',(-23.4236347819836,26.7743711998989,28.2390866274553));
#54339=CARTESIAN_POINT('Ctrl Pts',(-23.1711705404608,26.7520630098291,28.2222540672274));
#54340=CARTESIAN_POINT('Ctrl Pts',(-23.0761636222282,26.7393805031465,28.2160038763618));
#54341=CARTESIAN_POINT('Ctrl Pts',(-22.9716579381135,26.7206552105916,28.2093216273621));
#54342=CARTESIAN_POINT('Ctrl Pts',(-22.9614710397305,26.7187791943223,28.2086723231425));
#54343=CARTESIAN_POINT('Ctrl Pts',(-22.9489223992816,26.7164056322464,28.2078751765298));
#54344=CARTESIAN_POINT('Ctrl Pts',(-22.946552094915,26.7159545339374,28.207724722662));
#54345=CARTESIAN_POINT('Ctrl Pts',(-22.9419564599334,26.7150745784358,28.2074332501457));
#54346=CARTESIAN_POINT('Ctrl Pts',(-22.9397310716364,26.71464603525,28.207292213675));
#54347=CARTESIAN_POINT('Ctrl Pts',(-22.9356928001506,26.713863966487,28.207036478556));
#54348=CARTESIAN_POINT('Ctrl Pts',(-22.9338797745739,26.7135112309343,28.206921734999));
#54349=CARTESIAN_POINT('Ctrl Pts',(-22.9302015623798,26.7127923292127,28.2066890919444));
#54350=CARTESIAN_POINT('Ctrl Pts',(-22.9283364036013,26.7124260729631,28.2065711981951));
#54351=CARTESIAN_POINT('Ctrl Pts',(-22.922967651316,26.7113668916332,28.2062320626084));
#54352=CARTESIAN_POINT('Ctrl Pts',(-22.919464870047,26.7106697895845,28.2060110608988));
#54353=CARTESIAN_POINT('Ctrl Pts',(-22.9040839224942,26.7075821780507,28.205041756317));
#54354=CARTESIAN_POINT('Ctrl Pts',(-22.8922179307233,26.7051304757975,28.2042969221138));
#54355=CARTESIAN_POINT('Ctrl Pts',(-22.6882694481591,26.6617907538697,28.1915415353527));
#54356=CARTESIAN_POINT('Ctrl Pts',(-22.500273182098,26.6034890787997,28.1804827253851));
#54357=CARTESIAN_POINT('Ctrl Pts',(-22.2359402074733,26.4941831285167,28.1644763297204));
#54358=CARTESIAN_POINT('Ctrl Pts',(-22.1546382446509,26.4565206784539,28.1594877959985));
#54359=CARTESIAN_POINT('Ctrl Pts',(-22.0750359096863,26.4155367201564,28.1544576001758));
#54360=CARTESIAN_POINT('',(-26.7730024951077,23.5507381430868,28.3112187782627));
#54361=CARTESIAN_POINT('Ctrl Pts',(-22.0750363456406,26.4155369446113,27.9044917472066));
#54362=CARTESIAN_POINT('Ctrl Pts',(-22.1370108204797,26.4474450330344,27.9085937009903));
#54363=CARTESIAN_POINT('Ctrl Pts',(-22.2000329815414,26.477348858093,27.9127595589773));
#54364=CARTESIAN_POINT('Ctrl Pts',(-22.2754514881685,26.510177471065,27.9177582064902));
#54365=CARTESIAN_POINT('Ctrl Pts',(-22.2869243926363,26.5150923846166,27.9185189556714));
#54366=CARTESIAN_POINT('Ctrl Pts',(-22.3026654277518,26.5217277802182,27.9195632770429));
#54367=CARTESIAN_POINT('Ctrl Pts',(-22.3069092276057,26.5235059958872,27.9198448825534));
#54368=CARTESIAN_POINT('Ctrl Pts',(-22.3141470301014,26.5265205377674,27.920325260705));
#54369=CARTESIAN_POINT('Ctrl Pts',(-22.3171391241759,26.5277614534486,27.9205238771448));
#54370=CARTESIAN_POINT('Ctrl Pts',(-22.3231860273209,26.5302586166514,27.9209253338485));
#54371=CARTESIAN_POINT('Ctrl Pts',(-22.3262409061166,26.5315146826734,27.9211281799381));
#54372=CARTESIAN_POINT('Ctrl Pts',(-22.33320981648,26.5343675531553,27.9215909942883));
#54373=CARTESIAN_POINT('Ctrl Pts',(-22.3371250635236,26.5359613550164,27.9218510639175));
#54374=CARTESIAN_POINT('Ctrl Pts',(-22.3453239613838,26.5392801374906,27.9223957899415));
#54375=CARTESIAN_POINT('Ctrl Pts',(-22.3496082038766,26.5410036222208,27.9226804963259));
#54376=CARTESIAN_POINT('Ctrl Pts',(-22.3608714063266,26.5455065329968,27.9234291650558));
#54377=CARTESIAN_POINT('Ctrl Pts',(-22.3678563755703,26.548270764152,27.9238936398385));
#54378=CARTESIAN_POINT('Ctrl Pts',(-22.388676247457,26.5564259407559,27.925278658544));
#54379=CARTESIAN_POINT('Ctrl Pts',(-22.4025386661893,26.561745666416,27.9262015934575));
#54380=CARTESIAN_POINT('Ctrl Pts',(-22.4512479136405,26.580052752147,27.9294474670952));
#54381=CARTESIAN_POINT('Ctrl Pts',(-22.4862812751604,26.5925321876661,27.9317872303062));
#54382=CARTESIAN_POINT('Ctrl Pts',(-22.6514537013537,26.6481673081038,27.942846478607));
#54383=CARTESIAN_POINT('Ctrl Pts',(-22.7840299422326,26.6835910023773,27.9518124347171));
#54384=CARTESIAN_POINT('Ctrl Pts',(-23.17559622144,26.7618752160113,27.9784517532854));
#54385=CARTESIAN_POINT('Ctrl Pts',(-23.4380487111231,26.7817064112265,27.9965756940932));
#54386=CARTESIAN_POINT('Ctrl Pts',(-23.7007834385039,26.7694851460926,28.0136968013963));
#54387=CARTESIAN_POINT('Ctrl Pts',(-23.7015680801068,26.7694483605199,28.0137479225244));
#54388=CARTESIAN_POINT('Ctrl Pts',(-23.705411549764,26.7692667626366,28.0139982836235));
#54389=CARTESIAN_POINT('Ctrl Pts',(-23.7084701935041,26.7691178770476,28.0141973683649));
#54390=CARTESIAN_POINT('Ctrl Pts',(-23.7185649763606,26.7686120700184,28.0148539142029));
#54391=CARTESIAN_POINT('Ctrl Pts',(-23.7256002064051,26.7682364333955,28.0153106453887));
#54392=CARTESIAN_POINT('Ctrl Pts',(-23.7399359132502,26.7674238456701,28.0162395686254));
#54393=CARTESIAN_POINT('Ctrl Pts',(-23.7472362567654,26.7669851072643,28.0167116850798));
#54394=CARTESIAN_POINT('Ctrl Pts',(-23.7942434687685,26.7639994258681,28.0197454083601));
#54395=CARTESIAN_POINT('Ctrl Pts',(-23.8339040276543,26.76074203758,28.0222762763525));
#54396=CARTESIAN_POINT('Ctrl Pts',(-23.8787882269132,26.756217308299,28.0251002356253));
#54397=CARTESIAN_POINT('Ctrl Pts',(-23.8840788964053,26.7556707276637,28.0254324705672));
#54398=CARTESIAN_POINT('Ctrl Pts',(-23.8918043452103,26.7548532747308,28.0259166479695));
#54399=CARTESIAN_POINT('Ctrl Pts',(-23.8942401720074,26.754592723839,28.0260691702243));
#54400=CARTESIAN_POINT('Ctrl Pts',(-23.8985511100151,26.7541266273919,28.0263388569363));
#54401=CARTESIAN_POINT('Ctrl Pts',(-23.9004263388629,26.7539222127928,28.0264560857029));
#54402=CARTESIAN_POINT('Ctrl Pts',(-23.9043411688434,26.7534919873775,28.0267006442483));
#54403=CARTESIAN_POINT('Ctrl Pts',(-23.9063807296153,26.7532658754233,28.0268279564431));
#54404=CARTESIAN_POINT('Ctrl Pts',(-23.9117053255158,26.7526704257474,28.0271600705618));
#54405=CARTESIAN_POINT('Ctrl Pts',(-23.9149900214695,26.7522979801692,28.0273646958347));
#54406=CARTESIAN_POINT('Ctrl Pts',(-23.9292471857311,26.7506591641407,28.0282517923214));
#54407=CARTESIAN_POINT('Ctrl Pts',(-23.9402138468028,26.7493414241583,28.0289313829262));
#54408=CARTESIAN_POINT('Ctrl Pts',(-24.0195531153669,26.7393940727527,28.0338293012803));
#54409=CARTESIAN_POINT('Ctrl Pts',(-24.0876458425578,26.7286289800014,28.0379327139359));
#54410=CARTESIAN_POINT('Ctrl Pts',(-24.3309593280151,26.6821179906193,28.0524016189829));
#54411=CARTESIAN_POINT('Ctrl Pts',(-24.503489002333,26.6339897746306,28.0623096760968));
#54412=CARTESIAN_POINT('Ctrl Pts',(-24.7565693948789,26.5401050906481,28.0774020635333));
#54413=CARTESIAN_POINT('Ctrl Pts',(-24.8406071326346,26.5048088218857,28.0825098420656));
#54414=CARTESIAN_POINT('Ctrl Pts',(-25.0694713882489,26.3970558008127,28.0968979991911));
#54415=CARTESIAN_POINT('Ctrl Pts',(-25.2104861373816,26.3171872738515,28.106329339487));
#54416=CARTESIAN_POINT('Ctrl Pts',(-25.3543227497192,26.2207538054779,28.1168612304858));
#54417=CARTESIAN_POINT('Ctrl Pts',(-25.3637172506223,26.2143831803063,28.1175534212066));
#54418=CARTESIAN_POINT('Ctrl Pts',(-25.3767219573451,26.205463733545,28.1185177012015));
#54419=CARTESIAN_POINT('Ctrl Pts',(-25.3803609488482,26.2029568632052,28.1187881935831));
#54420=CARTESIAN_POINT('Ctrl Pts',(-25.3866182268595,26.1986272736532,28.1192544618639));
#54421=CARTESIAN_POINT('Ctrl Pts',(-25.3892389910645,26.1968081314066,28.1194501010067));
#54422=CARTESIAN_POINT('Ctrl Pts',(-25.3945853837571,26.1930852820729,28.1198499247448));
#54423=CARTESIAN_POINT('Ctrl Pts',(-25.3973107751573,26.1911812434922,28.1200541218613));
#54424=CARTESIAN_POINT('Ctrl Pts',(-25.4036130570688,26.1867637562282,28.1205272014696));
#54425=CARTESIAN_POINT('Ctrl Pts',(-25.4071877831266,26.1842472442549,28.1207962013687));
#54426=CARTESIAN_POINT('Ctrl Pts',(-25.4146910594564,26.1789422714237,28.1213622290977));
#54427=CARTESIAN_POINT('Ctrl Pts',(-25.418618496742,26.1761522616551,28.1216593162361));
#54428=CARTESIAN_POINT('Ctrl Pts',(-25.429043132077,26.1687114841615,28.1224500467262));
#54429=CARTESIAN_POINT('Ctrl Pts',(-25.4355292843739,26.1640453639212,28.1229442831443));
#54430=CARTESIAN_POINT('Ctrl Pts',(-25.4550701198176,26.1498771647519,28.1244401197117));
#54431=CARTESIAN_POINT('Ctrl Pts',(-25.4680706576172,26.1403011600784,28.1254445882186));
#54432=CARTESIAN_POINT('Ctrl Pts',(-25.5143256003552,26.1056912573388,28.1290521635529));
#54433=CARTESIAN_POINT('Ctrl Pts',(-25.54716513671,26.0801121891812,28.1316765383227));
#54434=CARTESIAN_POINT('Ctrl Pts',(-25.6539921234378,25.9935273870365,28.1404284164067));
#54435=CARTESIAN_POINT('Ctrl Pts',(-25.7257470106641,25.9298603046134,28.1466592813762));
#54436=CARTESIAN_POINT('Ctrl Pts',(-26.0405039909782,25.624431322755,28.1756295020245));
#54437=CARTESIAN_POINT('Ctrl Pts',(-26.2467880640397,25.3480961729768,28.1996663752747));
#54438=CARTESIAN_POINT('Ctrl Pts',(-26.406729441681,25.04245306913,28.2214696359326));
#54439=CARTESIAN_POINT('Ctrl Pts',(-26.4077864740024,25.0404278736668,28.2216139004194));
#54440=CARTESIAN_POINT('Ctrl Pts',(-26.4147549113325,25.0270421865883,28.2225660709243));
#54441=CARTESIAN_POINT('Ctrl Pts',(-26.42060082395,25.0156474484278,28.2233701672264));
#54442=CARTESIAN_POINT('Ctrl Pts',(-26.4280054483736,25.0010001710707,28.2243952512185));
#54443=CARTESIAN_POINT('Ctrl Pts',(-26.4296267326283,24.9977796554166,28.2246201114467));
#54444=CARTESIAN_POINT('Ctrl Pts',(-26.4322016269598,24.9926434474689,28.2249778814319));
#54445=CARTESIAN_POINT('Ctrl Pts',(-26.4331587335785,24.9907295265862,28.2251110114785));
#54446=CARTESIAN_POINT('Ctrl Pts',(-26.4349396884712,24.9871592761091,28.2253590035628));
#54447=CARTESIAN_POINT('Ctrl Pts',(-26.4357640113947,24.9855032014946,28.2254738951025));
#54448=CARTESIAN_POINT('Ctrl Pts',(-26.4376219591748,24.9817624917573,28.2257330935293));
#54449=CARTESIAN_POINT('Ctrl Pts',(-26.4386547504618,24.9796774507473,28.2258773472474));
#54450=CARTESIAN_POINT('Ctrl Pts',(-26.4417085436379,24.9734955054955,28.2263043953378));
#54451=CARTESIAN_POINT('Ctrl Pts',(-26.4437231044671,24.969395398564,28.2265867848962));
#54452=CARTESIAN_POINT('Ctrl Pts',(-26.4596666624731,24.9367714115786,28.2288271163122));
#54453=CARTESIAN_POINT('Ctrl Pts',(-26.4731828875898,24.9080461494892,28.2307596483457));
#54454=CARTESIAN_POINT('Ctrl Pts',(-26.5264544089083,24.7903476218444,28.2385347905647));
#54455=CARTESIAN_POINT('Ctrl Pts',(-26.5625924098078,24.6997852490306,28.2441886538635));
#54456=CARTESIAN_POINT('Ctrl Pts',(-26.7126483907092,24.2677907903654,28.2702539828218));
#54457=CARTESIAN_POINT('Ctrl Pts',(-26.7729482783921,23.910546254642,28.2895550119449));
#54458=CARTESIAN_POINT('Ctrl Pts',(-26.7730024951077,23.5507381430868,28.3112187782627));
#54459=CARTESIAN_POINT('Ctrl Pts',(-22.0750360153802,26.4155367745738,29.1557101328919));
#54460=CARTESIAN_POINT('Ctrl Pts',(-21.903523834291,26.3272322362299,29.1428205289804));
#54461=CARTESIAN_POINT('Ctrl Pts',(-21.7402616852622,26.2236941082807,29.1302936435899));
#54462=CARTESIAN_POINT('Ctrl Pts',(-21.5770994734328,26.0983787718882,29.117532731908));
#54463=CARTESIAN_POINT('Ctrl Pts',(-21.5670275385601,26.0905475857023,29.1167437886155));
#54464=CARTESIAN_POINT('Ctrl Pts',(-21.5533519097916,26.0797835255595,29.1156708205667));
#54465=CARTESIAN_POINT('Ctrl Pts',(-21.5497077664611,26.0769024451824,29.1153847364847));
#54466=CARTESIAN_POINT('Ctrl Pts',(-21.5435228987184,26.0719908845966,29.1148988971793));
#54467=CARTESIAN_POINT('Ctrl Pts',(-21.5409790027695,26.0699644252359,29.114698981506));
#54468=CARTESIAN_POINT('Ctrl Pts',(-21.5358594045649,26.0658734864667,29.1142964764718));
#54469=CARTESIAN_POINT('Ctrl Pts',(-21.5332837974685,26.0638088935059,29.1140938919889));
#54470=CARTESIAN_POINT('Ctrl Pts',(-21.5274384342904,26.0591085116993,29.1136339193165));
#54471=CARTESIAN_POINT('Ctrl Pts',(-21.5241706447973,26.0564702774051,29.1133766298839));
#54472=CARTESIAN_POINT('Ctrl Pts',(-21.5173501630926,26.0509417361898,29.1128393073652));
#54473=CARTESIAN_POINT('Ctrl Pts',(-21.5137984538577,26.0480502270551,29.1125593234604));
#54474=CARTESIAN_POINT('Ctrl Pts',(-21.5045092149839,26.0404547104572,29.1118265708541));
#54475=CARTESIAN_POINT('Ctrl Pts',(-21.4987817218802,26.0357384252181,29.111374298945));
#54476=CARTESIAN_POINT('Ctrl Pts',(-21.4818351742594,26.0216853626285,29.1100346517203));
#54477=CARTESIAN_POINT('Ctrl Pts',(-21.4706631048166,26.0122920173259,29.109149573495));
#54478=CARTESIAN_POINT('Ctrl Pts',(-21.3506622089354,25.9099970694466,29.0996207145988));
#54479=CARTESIAN_POINT('Ctrl Pts',(-21.2480643489262,25.8100156362744,29.0912864711653));
#54480=CARTESIAN_POINT('Ctrl Pts',(-21.0312821028377,25.5686152585135,29.0728030485355));
#54481=CARTESIAN_POINT('Ctrl Pts',(-20.9217277054565,25.4237139561571,29.0628036964094));
#54482=CARTESIAN_POINT('Ctrl Pts',(-20.760844296867,25.1688138446026,29.0458442317717));
#54483=CARTESIAN_POINT('Ctrl Pts',(-20.7024796284295,25.0637660794743,29.0390054648641));
#54484=CARTESIAN_POINT('Ctrl Pts',(-20.6281524228337,24.9103941499232,29.0288923486045));
#54485=CARTESIAN_POINT('Ctrl Pts',(-20.6072545609322,24.864564715976,29.02585461993));
#54486=CARTESIAN_POINT('Ctrl Pts',(-20.5854302267779,24.8135705309798,29.022437150822));
#54487=CARTESIAN_POINT('Ctrl Pts',(-20.5834311389967,24.8088686328279,29.0221216983338));
#54488=CARTESIAN_POINT('Ctrl Pts',(-20.5804726977639,24.8018641020228,29.0216512180069));
#54489=CARTESIAN_POINT('Ctrl Pts',(-20.5795048107722,24.7995650480557,29.0214967082355));
#54490=CARTESIAN_POINT('Ctrl Pts',(-20.5778492254366,24.7956196786666,29.0212314036766));
#54491=CARTESIAN_POINT('Ctrl Pts',(-20.5771602214079,24.7939739073594,29.0211206889759));
#54492=CARTESIAN_POINT('Ctrl Pts',(-20.5758165103108,24.7907567900429,29.0209041757315));
#54493=CARTESIAN_POINT('Ctrl Pts',(-20.5751616831767,24.7891855013489,29.0207983850234));
#54494=CARTESIAN_POINT('Ctrl Pts',(-20.5735772191261,24.7853750051121,29.0205417325251));
#54495=CARTESIAN_POINT('Ctrl Pts',(-20.572648865471,24.7831352704797,29.0203907921514));
#54496=CARTESIAN_POINT('Ctrl Pts',(-20.5697912283803,24.7762189157929,29.0199244269508));
#54497=CARTESIAN_POINT('Ctrl Pts',(-20.5678704406278,24.7715388280006,29.0196084884382));
#54498=CARTESIAN_POINT('Ctrl Pts',(-20.5463318034568,24.7187051218155,29.0160379120575));
#54499=CARTESIAN_POINT('Ctrl Pts',(-20.5278724415341,24.670091362248,29.0127157923183));
#54500=CARTESIAN_POINT('Ctrl Pts',(-20.4826350647755,24.5416775352006,29.0038842426427));
#54501=CARTESIAN_POINT('Ctrl Pts',(-20.4577937627476,24.4612394751727,28.9982970890804));
#54502=CARTESIAN_POINT('Ctrl Pts',(-20.4127050062616,24.2920023094964,28.9865466057507));
#54503=CARTESIAN_POINT('Ctrl Pts',(-20.393014293255,24.2031256870088,28.9803787235144));
#54504=CARTESIAN_POINT('Ctrl Pts',(-20.3600394111265,24.0173687267186,28.9676101963295));
#54505=CARTESIAN_POINT('Ctrl Pts',(-20.3473480346287,23.9204707371898,28.9610177853943));
#54506=CARTESIAN_POINT('Ctrl Pts',(-20.3235423274876,23.6403421778372,28.9422828299221));
#54507=CARTESIAN_POINT('Ctrl Pts',(-20.3236426732886,23.4565248657216,28.9304058818221));
#54508=CARTESIAN_POINT('Ctrl Pts',(-20.3403899451264,23.2620944636847,28.9183109226904));
#54509=CARTESIAN_POINT('Ctrl Pts',(-20.3414510464762,23.2505094233887,28.9175919064636));
#54510=CARTESIAN_POINT('Ctrl Pts',(-20.3430059568645,23.234488560877,28.9165998177692));
#54511=CARTESIAN_POINT('Ctrl Pts',(-20.3434462743388,23.2300477454694,28.9163250587344));
#54512=CARTESIAN_POINT('Ctrl Pts',(-20.34421811424,23.2224246605355,28.9158538119853));
#54513=CARTESIAN_POINT('Ctrl Pts',(-20.3445451533826,23.2192419521463,28.9156571829187));
#54514=CARTESIAN_POINT('Ctrl Pts',(-20.3452205942789,23.2127635308989,28.9152571872378));
#54515=CARTESIAN_POINT('Ctrl Pts',(-20.3455693412412,23.2094678570523,28.9150538317693));
#54516=CARTESIAN_POINT('Ctrl Pts',(-20.346384134712,23.2018798889987,28.9145859190452));
#54517=CARTESIAN_POINT('Ctrl Pts',(-20.3468537250986,23.1975879749979,28.9143214740985));
#54518=CARTESIAN_POINT('Ctrl Pts',(-20.3478581222631,23.188575635692,28.9137666304346));
#54519=CARTESIAN_POINT('Ctrl Pts',(-20.3483947448019,23.1838554198682,28.9134762896437));
#54520=CARTESIAN_POINT('Ctrl Pts',(-20.3498438792451,23.1713549406675,28.9127080601571));
#54521=CARTESIAN_POINT('Ctrl Pts',(-20.350774328509,23.1635767551045,28.9122307379048));
#54522=CARTESIAN_POINT('Ctrl Pts',(-20.3536577931424,23.1401953258242,28.9107979297246));
#54523=CARTESIAN_POINT('Ctrl Pts',(-20.3556966760933,23.124602753586,28.9098451497913));
#54524=CARTESIAN_POINT('Ctrl Pts',(-20.363351001329,23.0692215348088,28.9064702502806));
#54525=CARTESIAN_POINT('Ctrl Pts',(-20.3695964940952,23.0295226892218,28.9040679124913));
#54526=CARTESIAN_POINT('Ctrl Pts',(-20.3922646563213,22.9011256034451,28.8963427179516));
#54527=CARTESIAN_POINT('Ctrl Pts',(-20.4116691199122,22.812994580749,28.8911110161058));
#54528=CARTESIAN_POINT('Ctrl Pts',(-20.4775906594915,22.5638887167067,28.8763834340805));
#54529=CARTESIAN_POINT('Ctrl Pts',(-20.5329888601922,22.4055750358515,28.8671078768767));
#54530=CARTESIAN_POINT('Ctrl Pts',(-20.6756630740369,22.0813292410139,28.8472642605691));
#54531=CARTESIAN_POINT('Ctrl Pts',(-20.7655918131333,21.9172667594246,28.836703385407));
#54532=CARTESIAN_POINT('Ctrl Pts',(-20.8755459019558,21.7524224762358,28.8245734898339));
#54533=CARTESIAN_POINT('Ctrl Pts',(-20.8819451783495,21.7429384133756,28.8238699021014));
#54534=CARTESIAN_POINT('Ctrl Pts',(-20.8903618471657,21.7306066085806,28.8229472878342));
#54535=CARTESIAN_POINT('Ctrl Pts',(-20.8923336576871,21.7277276352751,28.8227313396326));
#54536=CARTESIAN_POINT('Ctrl Pts',(-20.8953764826729,21.7233003508187,28.8223983891156));
#54537=CARTESIAN_POINT('Ctrl Pts',(-20.896444192349,21.721749754871,28.822281613928));
#54538=CARTESIAN_POINT('Ctrl Pts',(-20.8985720327129,21.7186653592511,28.822049000321));
#54539=CARTESIAN_POINT('Ctrl Pts',(-20.8996321318709,21.7171315496222,28.8219331640678));
#54540=CARTESIAN_POINT('Ctrl Pts',(-20.9020019416855,21.7137091324778,28.8216743351153));
#54541=CARTESIAN_POINT('Ctrl Pts',(-20.9033123392048,21.7118210094471,28.8215312951069));
#54542=CARTESIAN_POINT('Ctrl Pts',(-20.9071541521064,21.7062980478469,28.8211121712726));
#54543=CARTESIAN_POINT('Ctrl Pts',(-20.9096910298006,21.7026670433236,28.8208357134777));
#54544=CARTESIAN_POINT('Ctrl Pts',(-20.9283225649299,21.6761166914224,28.8188076175202));
#54545=CARTESIAN_POINT('Ctrl Pts',(-20.9447072428868,21.6534036933718,28.8170365525425));
#54546=CARTESIAN_POINT('Ctrl Pts',(-20.9991043040542,21.580031361701,28.8112042151842));
#54547=CARTESIAN_POINT('Ctrl Pts',(-21.0383124309599,21.530281116342,28.807073907356));
#54548=CARTESIAN_POINT('Ctrl Pts',(-21.233359575192,21.2972562751459,28.7869896314095));
#54549=CARTESIAN_POINT('Ctrl Pts',(-21.4079290619932,21.1306567553353,28.7704254561559));
#54550=CARTESIAN_POINT('Ctrl Pts',(-21.7409514727248,20.8773957308274,28.74259042454));
#54551=CARTESIAN_POINT('Ctrl Pts',(-21.8911660006027,20.7816454824267,28.7310968101406));
#54552=CARTESIAN_POINT('Ctrl Pts',(-22.0587419710486,20.6933929337504,28.7193592112775));
#54553=CARTESIAN_POINT('Ctrl Pts',(-22.0689730128347,20.6880747756077,28.7186465676134));
#54554=CARTESIAN_POINT('Ctrl Pts',(-22.0831916387644,20.6807805072414,28.7176616028229));
#54555=CARTESIAN_POINT('Ctrl Pts',(-22.0871550108788,20.6787576235368,28.7173876309787));
#54556=CARTESIAN_POINT('Ctrl Pts',(-22.0939751372373,20.6752944540647,28.7169171786178));
#54557=CARTESIAN_POINT('Ctrl Pts',(-22.0968298625359,20.6738502054134,28.716720558636));
#54558=CARTESIAN_POINT('Ctrl Pts',(-22.1026531368747,20.6709150055017,28.7163200859506));
#54559=CARTESIAN_POINT('Ctrl Pts',(-22.1056218508138,20.6694243879801,28.7161162451546));
#54560=CARTESIAN_POINT('Ctrl Pts',(-22.1124810333354,20.665993600724,28.715646010426));
#54561=CARTESIAN_POINT('Ctrl Pts',(-22.1163731397596,20.664056704649,28.7153797316374));
#54562=CARTESIAN_POINT('Ctrl Pts',(-22.1245568069852,20.6600047648638,28.7148209864917));
#54563=CARTESIAN_POINT('Ctrl Pts',(-22.1288491854022,20.6578913888459,28.7145285788996));
#54564=CARTESIAN_POINT('Ctrl Pts',(-22.1402496684181,20.6523098060472,28.7137536813049));
#54565=CARTESIAN_POINT('Ctrl Pts',(-22.1473658916364,20.6488581785474,28.7132717693729));
#54566=CARTESIAN_POINT('Ctrl Pts',(-22.1688461923039,20.6385369544802,28.7118224247145));
#54567=CARTESIAN_POINT('Ctrl Pts',(-22.1832486855846,20.6317475075697,28.7108577665009));
#54568=CARTESIAN_POINT('Ctrl Pts',(-22.2347717001149,20.6079242396428,28.7074315572543));
#54569=CARTESIAN_POINT('Ctrl Pts',(-22.2721659447374,20.5914891925991,28.7049904304417));
#54570=CARTESIAN_POINT('Ctrl Pts',(-22.395497582566,20.5400586959942,28.6970759881295));
#54571=CARTESIAN_POINT('Ctrl Pts',(-22.482637844172,20.5080614020839,28.6916994293299));
#54572=CARTESIAN_POINT('Ctrl Pts',(-22.7323780904471,20.4284140801791,28.6767321366502));
#54573=CARTESIAN_POINT('Ctrl Pts',(-22.8975169296546,20.3897570278578,28.6673595754364));
#54574=CARTESIAN_POINT('Ctrl Pts',(-23.173533396809,20.3477116210626,28.6517015382719));
#54575=CARTESIAN_POINT('Ctrl Pts',(-23.2829031045341,20.336733173535,28.6454940292578));
#54576=CARTESIAN_POINT('Ctrl Pts',(-23.4031759185237,20.330842973238,28.6384708234775));
#54577=CARTESIAN_POINT('Ctrl Pts',(-23.413742622887,20.3303776155765,28.6378521161621));
#54578=CARTESIAN_POINT('Ctrl Pts',(-23.4416478732878,20.3292862781204,28.6362133299423));
#54579=CARTESIAN_POINT('Ctrl Pts',(-23.4589892964726,20.3287482902693,28.6351899687757));
#54580=CARTESIAN_POINT('Ctrl Pts',(-23.4835473303668,20.3281848663916,28.6337326745831));
#54581=CARTESIAN_POINT('Ctrl Pts',(-23.4907612490409,20.3280435984958,28.6333036098166));
#54582=CARTESIAN_POINT('Ctrl Pts',(-23.5007481657472,20.327881576971,28.6327081770578));
#54583=CARTESIAN_POINT('Ctrl Pts',(-23.5035208595915,20.3278401740327,28.6325427121346));
#54584=CARTESIAN_POINT('Ctrl Pts',(-23.5118229809335,20.3277269209445,28.6320468014854));
#54585=CARTESIAN_POINT('Ctrl Pts',(-23.5173525145251,20.3276657244335,28.6317158838186));
#54586=CARTESIAN_POINT('Ctrl Pts',(-23.5588418223804,20.3273133484892,28.6292280872079));
#54587=CARTESIAN_POINT('Ctrl Pts',(-23.5948022662794,20.3276098566029,28.6270444895093));
#54588=CARTESIAN_POINT('Ctrl Pts',(-23.6354010396643,20.3286242236627,28.6245408345939));
#54589=CARTESIAN_POINT('Ctrl Pts',(-23.6400534359174,20.3287505496246,28.6242533595278));
#54590=CARTESIAN_POINT('Ctrl Pts',(-23.64708555455,20.3289567368816,28.6238179560723));
#54591=CARTESIAN_POINT('Ctrl Pts',(-23.6494655143603,20.3290291591263,28.6236704445302));
#54592=CARTESIAN_POINT('Ctrl Pts',(-23.6536001914156,20.3291595640591,28.6234139052064));
#54593=CARTESIAN_POINT('Ctrl Pts',(-23.6553549495317,20.3292163433464,28.6233049455962));
#54594=CARTESIAN_POINT('Ctrl Pts',(-23.6590232801263,20.3293380415569,28.6230769872293));
#54595=CARTESIAN_POINT('Ctrl Pts',(-23.6609368369518,20.3294032317447,28.6229579731648));
#54596=CARTESIAN_POINT('Ctrl Pts',(-23.6655068015381,20.3295629966305,28.6226735029309));
#54597=CARTESIAN_POINT('Ctrl Pts',(-23.6681631495431,20.3296591525073,28.6225079572129));
#54598=CARTESIAN_POINT('Ctrl Pts',(-23.6771363786964,20.3299950866329,28.6219480903426));
#54599=CARTESIAN_POINT('Ctrl Pts',(-23.6834526203049,20.3302501624584,28.6215529158448));
#54600=CARTESIAN_POINT('Ctrl Pts',(-23.69844443881,20.3308997795109,28.6206124449374));
#54601=CARTESIAN_POINT('Ctrl Pts',(-23.7071192002536,20.331310806751,28.6200662610029));
#54602=CARTESIAN_POINT('Ctrl Pts',(-23.8083774813217,20.3365189075832,28.6136683136895));
#54603=CARTESIAN_POINT('Ctrl Pts',(-23.900705019942,20.3452733203515,28.6076161065517));
#54604=CARTESIAN_POINT('Ctrl Pts',(-24.0779979398687,20.3698359415566,28.5957272710955));
#54605=CARTESIAN_POINT('Ctrl Pts',(-24.1629661174933,20.385107063928,28.5899091368595));
#54606=CARTESIAN_POINT('Ctrl Pts',(-24.2746459259265,20.4098447362447,28.5821724059398));
#54607=CARTESIAN_POINT('Ctrl Pts',(-24.3019957300885,20.4162791639482,28.5802703940746));
#54608=CARTESIAN_POINT('Ctrl Pts',(-24.4234252096127,20.4465281885524,28.5717997830398));
#54609=CARTESIAN_POINT('Ctrl Pts',(-24.5164880137386,20.4742282232915,28.5652402726388));
#54610=CARTESIAN_POINT('Ctrl Pts',(-24.7905098614222,20.5694563368348,28.5458600719231));
#54611=CARTESIAN_POINT('Ctrl Pts',(-24.9668212259242,20.6490903843892,28.5333300852608));
#54612=CARTESIAN_POINT('Ctrl Pts',(-25.1453912938353,20.7499323514752,28.5206168217921));
#54613=CARTESIAN_POINT('Ctrl Pts',(-25.1557791801157,20.7558751467224,28.5198770302077));
#54614=CARTESIAN_POINT('Ctrl Pts',(-25.1700441836802,20.7641418029993,28.5188607440423));
#54615=CARTESIAN_POINT('Ctrl Pts',(-25.1739497755004,20.7664161052546,28.5185824573165));
#54616=CARTESIAN_POINT('Ctrl Pts',(-25.1806272135395,20.7703233403922,28.5181065948648));
#54617=CARTESIAN_POINT('Ctrl Pts',(-25.1834014150319,20.7719522173232,28.517908872133));
#54618=CARTESIAN_POINT('Ctrl Pts',(-25.1890264565541,20.7752663059936,28.5175079189169));
#54619=CARTESIAN_POINT('Ctrl Pts',(-25.1918771479565,20.7769517638287,28.5173046976849));
#54620=CARTESIAN_POINT('Ctrl Pts',(-25.1984113926356,20.7808287102722,28.5168388244732));
#54621=CARTESIAN_POINT('Ctrl Pts',(-25.2020931876752,20.783023162616,28.5165762809616));
#54622=CARTESIAN_POINT('Ctrl Pts',(-25.2098041424527,20.7876399791569,28.5160263304025));
#54623=CARTESIAN_POINT('Ctrl Pts',(-25.2138324043022,20.790063829444,28.5157389783342));
#54624=CARTESIAN_POINT('Ctrl Pts',(-25.2244539619891,20.7964866382278,28.514981148636));
#54625=CARTESIAN_POINT('Ctrl Pts',(-25.2310382613092,20.8005004777874,28.5145112158891));
#54626=CARTESIAN_POINT('Ctrl Pts',(-25.2507165486983,20.8125936023207,28.5131062290394));
#54627=CARTESIAN_POINT('Ctrl Pts',(-25.2637672765258,20.820743140133,28.5121737523546));
#54628=CARTESIAN_POINT('Ctrl Pts',(-25.30969697711,20.8498832251091,28.5088891248205));
#54629=CARTESIAN_POINT('Ctrl Pts',(-25.3422535152869,20.8713774283177,28.5065555449449));
#54630=CARTESIAN_POINT('Ctrl Pts',(-25.4444341715162,20.9415348712261,28.4992051808918));
#54631=CARTESIAN_POINT('Ctrl Pts',(-25.5125308931006,20.9923633248121,28.4942679563359));
#54632=CARTESIAN_POINT('Ctrl Pts',(-25.706029638216,21.1490745983631,28.4800010846273));
#54633=CARTESIAN_POINT('Ctrl Pts',(-25.8254496385929,21.2619100678056,28.4708949956884));
#54634=CARTESIAN_POINT('Ctrl Pts',(-26.0678445978434,21.5287584565743,28.4507224526013));
#54635=CARTESIAN_POINT('Ctrl Pts',(-26.1863370045312,21.6859184357703,28.4396635085306));
#54636=CARTESIAN_POINT('Ctrl Pts',(-26.2960923857667,21.8630580610241,28.4269138152973));
#54637=CARTESIAN_POINT('Ctrl Pts',(-26.3023582224796,21.8732981667442,28.4261757877939));
#54638=CARTESIAN_POINT('Ctrl Pts',(-26.3104067073467,21.8866182120766,28.4252141775191));
#54639=CARTESIAN_POINT('Ctrl Pts',(-26.3122417765848,21.8896666008855,28.4249939976785));
#54640=CARTESIAN_POINT('Ctrl Pts',(-26.3150478628767,21.8943455473509,28.4246558695367));
#54641=CARTESIAN_POINT('Ctrl Pts',(-26.3160225016005,21.8959739464359,28.424538159247));
#54642=CARTESIAN_POINT('Ctrl Pts',(-26.317942377159,21.8991880599697,28.4243057579234));
#54643=CARTESIAN_POINT('Ctrl Pts',(-26.3188876861248,21.9007737194376,28.4241910724519));
#54644=CARTESIAN_POINT('Ctrl Pts',(-26.3209914087059,21.9043094031452,28.4239352770239));
#54645=CARTESIAN_POINT('Ctrl Pts',(-26.3221491216886,21.9062598305841,28.4237941218961));
#54646=CARTESIAN_POINT('Ctrl Pts',(-26.3254898856854,21.911901658492,28.4233856802544));
#54647=CARTESIAN_POINT('Ctrl Pts',(-26.3276676177528,21.9155961782255,28.4231180479484));
#54648=CARTESIAN_POINT('Ctrl Pts',(-26.3423891219573,21.9406855370152,28.421299496154));
#54649=CARTESIAN_POINT('Ctrl Pts',(-26.3546924900912,21.9622194473466,28.4197333885703));
#54650=CARTESIAN_POINT('Ctrl Pts',(-26.3919649537566,22.029239562356,28.4148481064973));
#54651=CARTESIAN_POINT('Ctrl Pts',(-26.4160838760334,22.0751864403287,28.4114834061322));
#54652=CARTESIAN_POINT('Ctrl Pts',(-26.4589273314549,22.1618243229434,28.4051371508418));
#54653=CARTESIAN_POINT('Ctrl Pts',(-26.4779338747275,22.2023639469,28.4021669150757));
#54654=CARTESIAN_POINT('Ctrl Pts',(-26.642684599646,22.5737033947311,28.3750302911328));
#54655=CARTESIAN_POINT('Ctrl Pts',(-26.7326952720963,22.926570046644,28.3501549653898));
#54656=CARTESIAN_POINT('Ctrl Pts',(-26.7638871041612,23.307189710949,28.326181623642));
#54657=CARTESIAN_POINT('Ctrl Pts',(-26.7653493835414,23.3273647492704,28.32491783057));
#54658=CARTESIAN_POINT('Ctrl Pts',(-26.7676781248179,23.3643163718506,28.3226155081313));
#54659=CARTESIAN_POINT('Ctrl Pts',(-26.7686035406181,23.3810884002205,28.3215751632675));
#54660=CARTESIAN_POINT('Ctrl Pts',(-26.7696713833718,23.4036466079819,28.3201820081312));
#54661=CARTESIAN_POINT('Ctrl Pts',(-26.769929403328,23.4094268154008,28.3198255704294));
#54662=CARTESIAN_POINT('Ctrl Pts',(-26.7703096151641,23.4184923351576,28.3192673774902));
#54663=CARTESIAN_POINT('Ctrl Pts',(-26.7704423478823,23.4217771720332,28.3190652913293));
#54664=CARTESIAN_POINT('Ctrl Pts',(-26.770697704254,23.4283457999143,28.318661524494));
#54665=CARTESIAN_POINT('Ctrl Pts',(-26.7708203322258,23.4316295869276,28.3184598439135));
#54666=CARTESIAN_POINT('Ctrl Pts',(-26.7710536577081,23.4381448870054,28.318060029171));
#54667=CARTESIAN_POINT('Ctrl Pts',(-26.7711645148531,23.441376390166,28.3178618902309));
#54668=CARTESIAN_POINT('Ctrl Pts',(-26.7714045286842,23.4486942259397,28.3174135673003));
#54669=CARTESIAN_POINT('Ctrl Pts',(-26.7715307733969,23.4527806539243,28.3171634749366));
#54670=CARTESIAN_POINT('Ctrl Pts',(-26.7718304723853,23.4631190081454,28.316531412623));
#54671=CARTESIAN_POINT('Ctrl Pts',(-26.7719935045567,23.4693712389252,28.3161497697238));
#54672=CARTESIAN_POINT('Ctrl Pts',(-26.7727181990729,23.5006579469635,28.3142429716697));
#54673=CARTESIAN_POINT('Ctrl Pts',(-26.7730062814916,23.5256982728467,28.3127264089526));
#54674=CARTESIAN_POINT('Ctrl Pts',(-26.7730024948489,23.5507398571939,28.3112186750576));
#54675=CARTESIAN_POINT('Origin',(-23.5502525316942,23.5502525316942,0.));
#54676=CARTESIAN_POINT('',(-27.4844229589094,23.5526670019077,-74.5958360648399));
#54677=CARTESIAN_POINT('',(-21.8015553287927,27.0731131722198,-74.9999401439847));
#54678=CARTESIAN_POINT('Ctrl Pts',(-27.4832517860125,23.5526744176369,-74.5958364779651));
#54679=CARTESIAN_POINT('Ctrl Pts',(-27.483176366467,23.6751512902655,-74.6020627797075));
#54680=CARTESIAN_POINT('Ctrl Pts',(-27.4773804143339,23.7974636017587,-74.6082890814499));
#54681=CARTESIAN_POINT('Ctrl Pts',(-27.4659067048209,23.9192259676967,-74.6145153831923));
#54682=CARTESIAN_POINT('Ctrl Pts',(-27.4550637875768,24.0342941813215,-74.620399380382));
#54683=CARTESIAN_POINT('Ctrl Pts',(-27.4391265096654,24.149073567767,-74.6262833775717));
#54684=CARTESIAN_POINT('Ctrl Pts',(-27.4181161321085,24.2630780142565,-74.6321673747614));
#54685=CARTESIAN_POINT('Ctrl Pts',(-27.3971330386182,24.3769344146246,-74.638043730995));
#54686=CARTESIAN_POINT('Ctrl Pts',(-27.3710900215547,24.4900174753001,-74.6439200872287));
#54687=CARTESIAN_POINT('Ctrl Pts',(-27.3400601821272,24.6018451204468,-74.6497964434623));
#54688=CARTESIAN_POINT('Ctrl Pts',(-27.3090624249359,24.7135571452428,-74.6556667240394));
#54689=CARTESIAN_POINT('Ctrl Pts',(-27.2730882110991,24.8240159422074,-74.6615370046165));
#54690=CARTESIAN_POINT('Ctrl Pts',(-27.2322617585231,24.9327492056673,-74.6674072851936));
#54691=CARTESIAN_POINT('Ctrl Pts',(-27.1899550191757,25.0454249231332,-74.6734904105842));
#54692=CARTESIAN_POINT('Ctrl Pts',(-27.142437582367,25.1562471619655,-74.6795735359748));
#54693=CARTESIAN_POINT('Ctrl Pts',(-27.0899044923739,25.2647066714297,-74.6856566613653));
#54694=CARTESIAN_POINT('Ctrl Pts',(-27.039269673959,25.3692470205281,-74.6915199743665));
#54695=CARTESIAN_POINT('Ctrl Pts',(-26.9839755999771,25.4715920343096,-74.6973832873676));
#54696=CARTESIAN_POINT('Ctrl Pts',(-26.9242457874241,25.5713063435184,-74.7032466003688));
#54697=CARTESIAN_POINT('Ctrl Pts',(-26.864525935161,25.6710040247924,-74.7091089356287));
#54698=CARTESIAN_POINT('Ctrl Pts',(-26.8003720267301,25.7680715208646,-74.7149712708887));
#54699=CARTESIAN_POINT('Ctrl Pts',(-26.7320527052678,25.8620995541953,-74.7208336061487));
#54700=CARTESIAN_POINT('Ctrl Pts',(-26.6637284033848,25.95613444209,-74.7266963687679));
#54701=CARTESIAN_POINT('Ctrl Pts',(-26.591238326868,26.0471290938028,-74.7325591313872));
#54702=CARTESIAN_POINT('Ctrl Pts',(-26.5148930582176,26.1347051910584,-74.7384218940064));
#54703=CARTESIAN_POINT('Ctrl Pts',(-26.4385239277329,26.2223086603617,-74.7442864890414));
#54704=CARTESIAN_POINT('Ctrl Pts',(-26.3582974793948,26.306491140376,-74.7501510840764));
#54705=CARTESIAN_POINT('Ctrl Pts',(-26.2745625120793,26.3869097423515,-74.7560156791114));
#54706=CARTESIAN_POINT('Ctrl Pts',(-26.1907356370096,26.4674166120286,-74.7618867111437));
#54707=CARTESIAN_POINT('Ctrl Pts',(-26.1033928533998,26.5441510722657,-74.7677577431759));
#54708=CARTESIAN_POINT('Ctrl Pts',(-26.0129176017944,26.6168091922678,-74.7736287752082));
#54709=CARTESIAN_POINT('Ctrl Pts',(-25.922383302987,26.6895147314106,-74.7795036388741));
#54710=CARTESIAN_POINT('Ctrl Pts',(-25.828712796173,26.7581383894547,-74.78537850254));
#54711=CARTESIAN_POINT('Ctrl Pts',(-25.7323187762878,26.8224193832171,-74.7912533662059));
#54712=CARTESIAN_POINT('Ctrl Pts',(-25.6357870685638,26.8867921950312,-74.797136621443));
#54713=CARTESIAN_POINT('Ctrl Pts',(-25.5365244343096,26.9468097497519,-74.80301987668));
#54714=CARTESIAN_POINT('Ctrl Pts',(-25.4349684871045,27.0022569881545,-74.8089031319171));
#54715=CARTESIAN_POINT('Ctrl Pts',(-25.409080510343,27.0163912349294,-74.8104028528005));
#54716=CARTESIAN_POINT('Ctrl Pts',(-25.3830436130049,27.0302287427077,-74.811902573684));
#54717=CARTESIAN_POINT('Ctrl Pts',(-25.3568652381275,27.0437664545166,-74.8134022945674));
#54718=CARTESIAN_POINT('Ctrl Pts',(-25.2551946978962,27.0963436858972,-74.8192268514059));
#54719=CARTESIAN_POINT('Ctrl Pts',(-25.1510459488802,27.1445723874773,-74.8250514082445));
#54720=CARTESIAN_POINT('Ctrl Pts',(-25.0448307679798,27.1882086743135,-74.830875965083));
#54721=CARTESIAN_POINT('Ctrl Pts',(-24.9387513096792,27.2317892023566,-74.8366930792566));
#54722=CARTESIAN_POINT('Ctrl Pts',(-24.8306110542562,27.2707888232278,-74.8425101934303));
#54723=CARTESIAN_POINT('Ctrl Pts',(-24.720846744442,27.3050092733595,-74.848327307604));
#54724=CARTESIAN_POINT('Ctrl Pts',(-24.6111921317371,27.3391955239917,-74.8541386082248));
#54725=CARTESIAN_POINT('Ctrl Pts',(-24.4999170912857,27.3686119767027,-74.8599499088456));
#54726=CARTESIAN_POINT('Ctrl Pts',(-24.3874780220788,27.393108563118,-74.8657612094665));
#54727=CARTESIAN_POINT('Ctrl Pts',(-24.275117106024,27.417588122663,-74.87156847082));
#54728=CARTESIAN_POINT('Ctrl Pts',(-24.1615941799012,27.4371545269804,-74.8773757321735));
#54729=CARTESIAN_POINT('Ctrl Pts',(-24.0473797635603,27.4517078390554,-74.883182993527));
#54730=CARTESIAN_POINT('Ctrl Pts',(-23.9332063326367,27.4662559287287,-74.8889881709664));
#54731=CARTESIAN_POINT('Ctrl Pts',(-23.818342321467,27.4757944482308,-74.8947933484058));
#54732=CARTESIAN_POINT('Ctrl Pts',(-23.7032666959445,27.4802748809358,-74.9005985258453));
#54733=CARTESIAN_POINT('Ctrl Pts',(-23.5882033789001,27.4847548344142,-74.9064030823634));
#54734=CARTESIAN_POINT('Ctrl Pts',(-23.4729289128697,27.4841777605835,-74.9122076388816));
#54735=CARTESIAN_POINT('Ctrl Pts',(-23.3579248026403,27.4785472055491,-74.9180121953998));
#54736=CARTESIAN_POINT('Ctrl Pts',(-23.2429040244642,27.4729158344588,-74.9238175931926));
#54737=CARTESIAN_POINT('Ctrl Pts',(-23.1281541001282,27.4622295477948,-74.9296229909855));
#54738=CARTESIAN_POINT('Ctrl Pts',(-23.01415313124,27.4465439007826,-74.9354283887783));
#54739=CARTESIAN_POINT('Ctrl Pts',(-22.90003966309,27.4308427747466,-74.9412395154958));
#54740=CARTESIAN_POINT('Ctrl Pts',(-22.7866770436019,27.4101324947738,-74.9470506422132));
#54741=CARTESIAN_POINT('Ctrl Pts',(-22.674534903303,27.3845200804347,-74.9528617689307));
#54742=CARTESIAN_POINT('Ctrl Pts',(-22.5623338906578,27.3588942200983,-74.9586759463717));
#54743=CARTESIAN_POINT('Ctrl Pts',(-22.451355038326,27.3283612127694,-74.9644901238128));
#54744=CARTESIAN_POINT('Ctrl Pts',(-22.342052709662,27.2930779604367,-74.9703043012538));
#54745=CARTESIAN_POINT('Ctrl Pts',(-22.2325830393214,27.2577406895055,-74.9761273801904));
#54746=CARTESIAN_POINT('Ctrl Pts',(-22.1247954125246,27.2176387965384,-74.981950459127));
#54747=CARTESIAN_POINT('Ctrl Pts',(-22.0191243475635,27.1729774017003,-74.9877735380637));
#54748=CARTESIAN_POINT('Ctrl Pts',(-21.9455287910648,27.1418725745811,-74.9918290733707));
#54749=CARTESIAN_POINT('Ctrl Pts',(-21.8729594269255,27.1085571364925,-74.9958846086777));
#54750=CARTESIAN_POINT('Ctrl Pts',(-21.8015553287927,27.0731131722198,-74.9999401439847));
#54751=CARTESIAN_POINT('',(-25.2989470070244,27.0731145261455,-75.));
#54752=CARTESIAN_POINT('Origin',(-23.5502525316942,23.5502525316942,-75.));
#54753=CARTESIAN_POINT('',(-27.4851692780616,23.554414982299,-74.7791635220347));
#54754=CARTESIAN_POINT('Ctrl Pts',(-25.2989470070244,27.0731145261455,-75.0000000000001));
#54755=CARTESIAN_POINT('Ctrl Pts',(-26.4728992620448,26.4903826945015,-74.9337043628751));
#54756=CARTESIAN_POINT('Ctrl Pts',(-27.4161416976464,25.1461349635273,-74.8600922035533));
#54757=CARTESIAN_POINT('Ctrl Pts',(-27.4883708345099,23.69846686772,-74.7864800442315));
#54758=CARTESIAN_POINT('Ctrl Pts',(-27.4872905609711,23.5544172262436,-74.7791635220347));
#54759=CARTESIAN_POINT('',(-27.4817157848272,23.5524277069527,-73.5291635548767));
#54760=CARTESIAN_POINT('Ctrl Pts',(-27.4832503311977,23.5544129523903,-74.7791635220347));
#54761=CARTESIAN_POINT('Ctrl Pts',(-27.4833696199972,23.4416448887938,-74.7734299077509));
#54762=CARTESIAN_POINT('Ctrl Pts',(-27.4786348720723,23.3286475420881,-74.7676962934671));
#54763=CARTESIAN_POINT('Ctrl Pts',(-27.4690136201014,23.2158866662325,-74.7619626791833));
#54764=CARTESIAN_POINT('Ctrl Pts',(-27.4594043197065,23.1032658626041,-74.7562361872291));
#54765=CARTESIAN_POINT('Ctrl Pts',(-27.4449206105733,22.9908813736366,-74.750509695275));
#54766=CARTESIAN_POINT('Ctrl Pts',(-27.4255820071538,22.8792007776292,-74.7447832033208));
#54767=CARTESIAN_POINT('Ctrl Pts',(-27.4055227965739,22.7633586692614,-74.7388433272345));
#54768=CARTESIAN_POINT('Ctrl Pts',(-27.3802397965917,22.6482744033037,-74.7329034511482));
#54769=CARTESIAN_POINT('Ctrl Pts',(-27.34981401959,22.5344663830884,-74.7269635750619));
#54770=CARTESIAN_POINT('Ctrl Pts',(-27.3205268577506,22.424917367907,-74.7212459852618));
#54771=CARTESIAN_POINT('Ctrl Pts',(-27.2864750423102,22.3165512540446,-74.7155283954617));
#54772=CARTESIAN_POINT('Ctrl Pts',(-27.2477829838819,22.2098206777215,-74.7098108056617));
#54773=CARTESIAN_POINT('Ctrl Pts',(-27.2091014823529,22.1031192222049,-74.7040947758721));
#54774=CARTESIAN_POINT('Ctrl Pts',(-27.1657823998924,21.9980528251032,-74.6983787460826));
#54775=CARTESIAN_POINT('Ctrl Pts',(-27.1179996559044,21.895057842937,-74.6926627162931));
#54776=CARTESIAN_POINT('Ctrl Pts',(-27.0702172636805,21.7920636189931,-74.6869467285835));
#54777=CARTESIAN_POINT('Ctrl Pts',(-27.0179714584404,21.6911411725022,-74.6812307408739));
#54778=CARTESIAN_POINT('Ctrl Pts',(-26.9614834250078,21.5927048841252,-74.6755147531643));
#54779=CARTESIAN_POINT('Ctrl Pts',(-26.9049808073633,21.4942431812382,-74.6697972896877));
#54780=CARTESIAN_POINT('Ctrl Pts',(-26.8442340028997,21.3982692864339,-74.6640798262111));
#54781=CARTESIAN_POINT('Ctrl Pts',(-26.7795085478587,21.3051702209391,-74.6583623627345));
#54782=CARTESIAN_POINT('Ctrl Pts',(-26.7147125334941,21.2119696651252,-74.652638666465));
#54783=CARTESIAN_POINT('Ctrl Pts',(-26.6459294636619,21.1216505464843,-74.6469149701956));
#54784=CARTESIAN_POINT('Ctrl Pts',(-26.5734662165351,21.0345681286359,-74.6411912739261));
#54785=CARTESIAN_POINT('Ctrl Pts',(-26.5009559978528,20.9474292629083,-74.6354638674873));
#54786=CARTESIAN_POINT('Ctrl Pts',(-26.424761149098,20.8635315891097,-74.6297364610485));
#54787=CARTESIAN_POINT('Ctrl Pts',(-26.3452251776108,20.7831932788812,-74.6240090546097));
#54788=CARTESIAN_POINT('Ctrl Pts',(-26.2655711448374,20.7027357163942,-74.6182731465463));
#54789=CARTESIAN_POINT('Ctrl Pts',(-26.1825664154429,20.6258483459862,-74.6125372384829));
#54790=CARTESIAN_POINT('Ctrl Pts',(-26.0965871078452,20.5528087496863,-74.6068013304195));
#54791=CARTESIAN_POINT('Ctrl Pts',(-26.0737271121074,20.5333891369124,-74.6052762793631));
#54792=CARTESIAN_POINT('Ctrl Pts',(-26.0506569937147,20.5142412863503,-74.6037512283067));
#54793=CARTESIAN_POINT('Ctrl Pts',(-26.0273841403122,20.4953698836068,-74.6022261772503));
#54794=CARTESIAN_POINT('Ctrl Pts',(-25.9376229399062,20.4225846632343,-74.5963441991732));
#54795=CARTESIAN_POINT('Ctrl Pts',(-25.8445036587257,20.3536394154685,-74.5904622210961));
#54796=CARTESIAN_POINT('Ctrl Pts',(-25.7483883828409,20.2888589982635,-74.5845802430191));
#54797=CARTESIAN_POINT('Ctrl Pts',(-25.6523972122015,20.2241622263428,-74.5787058598256));
#54798=CARTESIAN_POINT('Ctrl Pts',(-25.5534180788839,20.1636198179255,-74.5728314766321));
#54799=CARTESIAN_POINT('Ctrl Pts',(-25.4518464541428,20.1075167657507,-74.5669570934387));
#54800=CARTESIAN_POINT('Ctrl Pts',(-25.3503790679149,20.0514712896829,-74.5610887388676));
#54801=CARTESIAN_POINT('Ctrl Pts',(-25.2463248410248,19.9998563051262,-74.5552203842965));
#54802=CARTESIAN_POINT('Ctrl Pts',(-25.1401080253617,19.952913444361,-74.5493520297255));
#54803=CARTESIAN_POINT('Ctrl Pts',(-25.0299904827973,19.9042466448892,-74.543268164565));
#54804=CARTESIAN_POINT('Ctrl Pts',(-24.9175488362501,19.8606019713076,-74.5371842994046));
#54805=CARTESIAN_POINT('Ctrl Pts',(-24.8032839381334,19.8221965645074,-74.5311004342442));
#54806=CARTESIAN_POINT('Ctrl Pts',(-24.6931952093274,19.7851948038303,-74.5252389230297));
#54807=CARTESIAN_POINT('Ctrl Pts',(-24.5814145914695,19.753056191361,-74.5193774118151));
#54808=CARTESIAN_POINT('Ctrl Pts',(-24.4684094216106,19.7259255418175,-74.5135159006006));
#54809=CARTESIAN_POINT('Ctrl Pts',(-24.3554221781225,19.6987991960956,-74.5076553192163));
#54810=CARTESIAN_POINT('Ctrl Pts',(-24.2412111692231,19.6766793296322,-74.501794737832));
#54811=CARTESIAN_POINT('Ctrl Pts',(-24.1262566493561,19.6596602559042,-74.4959341564477));
#54812=CARTESIAN_POINT('Ctrl Pts',(-24.0112927871526,19.6426397990387,-74.4900730987749));
#54813=CARTESIAN_POINT('Ctrl Pts',(-23.895585701244,19.6307210192758,-74.484212041102));
#54814=CARTESIAN_POINT('Ctrl Pts',(-23.7796228533173,19.6239466017445,-74.4783509834292));
#54815=CARTESIAN_POINT('Ctrl Pts',(-23.663622761514,19.6171700084682,-74.4724880433559));
#54816=CARTESIAN_POINT('Ctrl Pts',(-23.5473671552413,19.6155410869641,-74.4666251032827));
#54817=CARTESIAN_POINT('Ctrl Pts',(-23.431344902167,19.6190504285659,-74.4607621632094));
#54818=CARTESIAN_POINT('Ctrl Pts',(-23.3151936817199,19.6225636710622,-74.4548927060418));
#54819=CARTESIAN_POINT('Ctrl Pts',(-23.1992767440886,19.631226564613,-74.4490232488741));
#54820=CARTESIAN_POINT('Ctrl Pts',(-23.0840793457134,19.6449776936485,-74.4431537917065));
#54821=CARTESIAN_POINT('Ctrl Pts',(-22.9688058692284,19.6587379041384,-74.4372804582603));
#54822=CARTESIAN_POINT('Ctrl Pts',(-22.8542532837516,19.6775929753553,-74.431407124814));
#54823=CARTESIAN_POINT('Ctrl Pts',(-22.7408964607948,19.7014304066151,-74.4255337913678));
#54824=CARTESIAN_POINT('Ctrl Pts',(-22.6273762254666,19.7253022013219,-74.4196519910704));
#54825=CARTESIAN_POINT('Ctrl Pts',(-22.515055590567,19.7541705892566,-74.4137701907731));
#54826=CARTESIAN_POINT('Ctrl Pts',(-22.4043941737707,19.7878732813292,-74.4078883904757));
#54827=CARTESIAN_POINT('Ctrl Pts',(-22.375864780954,19.7965621032236,-74.406372015609));
#54828=CARTESIAN_POINT('Ctrl Pts',(-22.3474455617636,19.8055719888764,-74.4048556407421));
#54829=CARTESIAN_POINT('Ctrl Pts',(-22.319144157869,19.8148996471735,-74.4033392658754));
#54830=CARTESIAN_POINT('Ctrl Pts',(-22.2093479792547,19.8510865882965,-74.3974564423116));
#54831=CARTESIAN_POINT('Ctrl Pts',(-22.1009722265775,19.8921767568183,-74.3915736187478));
#54832=CARTESIAN_POINT('Ctrl Pts',(-21.9944858986412,19.9380400263896,-74.385690795184));
#54833=CARTESIAN_POINT('Ctrl Pts',(-21.8881338225866,19.9838454741695,-74.3798153883482));
#54834=CARTESIAN_POINT('Ctrl Pts',(-21.7836668084796,20.0344118933758,-74.3739399815124));
#54835=CARTESIAN_POINT('Ctrl Pts',(-21.6815382297402,20.0895595580728,-74.3680645746766));
#54836=CARTESIAN_POINT('Ctrl Pts',(-21.5795113788949,20.1446522914679,-74.3621950201965));
#54837=CARTESIAN_POINT('Ctrl Pts',(-21.4798186900967,20.2043169983498,-74.3563254657164));
#54838=CARTESIAN_POINT('Ctrl Pts',(-21.3828924895577,20.2683263521846,-74.3504559112363));
#54839=CARTESIAN_POINT('Ctrl Pts',(-21.2824336297223,20.334668648378,-74.3443724297056));
#54840=CARTESIAN_POINT('Ctrl Pts',(-21.184947175876,20.4056781465189,-74.3382889481749));
#54841=CARTESIAN_POINT('Ctrl Pts',(-21.0908856904151,20.481050071768,-74.3322054666443));
#54842=CARTESIAN_POINT('Ctrl Pts',(-21.0002309680286,20.5536921412156,-74.326342319506));
#54843=CARTESIAN_POINT('Ctrl Pts',(-20.9127577730638,20.6303858405778,-74.3204791723677));
#54844=CARTESIAN_POINT('Ctrl Pts',(-20.8288400685972,20.710815403371,-74.3146160252294));
#54845=CARTESIAN_POINT('Ctrl Pts',(-20.7449333931878,20.7912343955432,-74.3087536486673));
#54846=CARTESIAN_POINT('Ctrl Pts',(-20.6645815762154,20.8753879900511,-74.3028912721052));
#54847=CARTESIAN_POINT('Ctrl Pts',(-20.5881229799605,20.9629223404071,-74.2970288955431));
#54848=CARTESIAN_POINT('Ctrl Pts',(-20.511656108692,21.050466164491,-74.2911658845036));
#54849=CARTESIAN_POINT('Ctrl Pts',(-20.4390835667527,21.1413911618974,-74.2853028734642));
#54850=CARTESIAN_POINT('Ctrl Pts',(-20.3707040935097,21.2353096103161,-74.2794398624247));
#54851=CARTESIAN_POINT('Ctrl Pts',(-20.3023008322258,21.3292607313452,-74.2735748117448));
#54852=CARTESIAN_POINT('Ctrl Pts',(-20.2380937826937,21.4262070417607,-74.2677097610648));
#54853=CARTESIAN_POINT('Ctrl Pts',(-20.1783385474773,21.5257315801991,-74.2618447103848));
#54854=CARTESIAN_POINT('Ctrl Pts',(-20.1185146289072,21.6253705132851,-74.2559729183482));
#54855=CARTESIAN_POINT('Ctrl Pts',(-20.0631529501736,21.7275932363411,-74.2501011263116));
#54856=CARTESIAN_POINT('Ctrl Pts',(-20.0124633577918,21.8319578069689,-74.244229334275));
#54857=CARTESIAN_POINT('Ctrl Pts',(-19.9617391481416,21.9363936509325,-74.2383535322357));
#54858=CARTESIAN_POINT('Ctrl Pts',(-19.9156935415742,22.0429738783499,-74.2324777301965));
#54859=CARTESIAN_POINT('Ctrl Pts',(-19.8744877478804,22.1512377876424,-74.2266019281572));
#54860=CARTESIAN_POINT('Ctrl Pts',(-19.8332213284705,22.2596609846572,-74.2207174811029));
#54861=CARTESIAN_POINT('Ctrl Pts',(-19.7968090627029,22.3697724182824,-74.2148330340487));
#54862=CARTESIAN_POINT('Ctrl Pts',(-19.7653619995541,22.4810974167946,-74.2089485869944));
#54863=CARTESIAN_POINT('Ctrl Pts',(-19.7573525635011,22.5094514304097,-74.2074498428297));
#54864=CARTESIAN_POINT('Ctrl Pts',(-19.7496649597729,22.5378841250592,-74.2059510986651));
#54865=CARTESIAN_POINT('Ctrl Pts',(-19.7423004883812,22.5663875837321,-74.2044523545005));
#54866=CARTESIAN_POINT('Ctrl Pts',(-19.7134867755638,22.6779082114623,-74.1985884734901));
#54867=CARTESIAN_POINT('Ctrl Pts',(-19.6895266558515,22.7908876659337,-74.1927245924796));
#54868=CARTESIAN_POINT('Ctrl Pts',(-19.6705664942649,22.9048648567452,-74.1868607114692));
#54869=CARTESIAN_POINT('Ctrl Pts',(-19.6516312761111,23.0186921025053,-74.1810045448088));
#54870=CARTESIAN_POINT('Ctrl Pts',(-19.6376830036379,23.1335140693503,-74.1751483781483));
#54871=CARTESIAN_POINT('Ctrl Pts',(-19.6288179866241,23.2488556028265,-74.1692922114879));
#54872=CARTESIAN_POINT('Ctrl Pts',(-19.6199622419566,23.3640764950626,-74.1634421700729));
#54873=CARTESIAN_POINT('Ctrl Pts',(-19.6161792097235,23.4798154621531,-74.1575921286579));
#54874=CARTESIAN_POINT('Ctrl Pts',(-19.6175138410972,23.5955889572455,-74.151742087243));
#54875=CARTESIAN_POINT('Ctrl Pts',(-19.6189033749591,23.7161250055534,-74.1456513937381));
#54876=CARTESIAN_POINT('Ctrl Pts',(-19.6258407228482,23.8366980322504,-74.1395607002332));
#54877=CARTESIAN_POINT('Ctrl Pts',(-19.6383166657902,23.9567581049082,-74.1334700067283));
#54878=CARTESIAN_POINT('Ctrl Pts',(-19.650285395133,24.0719370954819,-74.1276269323885));
#54879=CARTESIAN_POINT('Ctrl Pts',(-19.6673511371457,24.1866435710266,-74.1217838580486));
#54880=CARTESIAN_POINT('Ctrl Pts',(-19.6894526486738,24.3003946937339,-74.1159407837087));
#54881=CARTESIAN_POINT('Ctrl Pts',(-19.7115505912792,24.4141274480615,-74.1100986529007));
#54882=CARTESIAN_POINT('Ctrl Pts',(-19.7386826076022,24.5269047492561,-74.1042565220927));
#54883=CARTESIAN_POINT('Ctrl Pts',(-19.7707361355208,24.6382529044222,-74.0984143912847));
#54884=CARTESIAN_POINT('Ctrl Pts',(-19.8027923108917,24.7496102563587,-74.0925717779475));
#54885=CARTESIAN_POINT('Ctrl Pts',(-19.8397706910818,24.8595378290581,-74.0867291646104));
#54886=CARTESIAN_POINT('Ctrl Pts',(-19.8815087436497,24.9675767774775,-74.0808865512732));
#54887=CARTESIAN_POINT('Ctrl Pts',(-19.9232604307852,25.0756510189747,-74.0750420293298));
#54888=CARTESIAN_POINT('Ctrl Pts',(-19.9697747323456,25.1818350228425,-74.0691975073864));
#54889=CARTESIAN_POINT('Ctrl Pts',(-20.0208411431113,25.2856903007142,-74.063352985443));
#54890=CARTESIAN_POINT('Ctrl Pts',(-20.0719656566824,25.3896637439887,-74.0575018136662));
#54891=CARTESIAN_POINT('Ctrl Pts',(-20.1276524339694,25.4913028004289,-74.0516506418895));
#54892=CARTESIAN_POINT('Ctrl Pts',(-20.187645168696,25.5901938843587,-74.0457994701128));
#54893=CARTESIAN_POINT('Ctrl Pts',(-20.2476782100473,25.6891514090969,-74.0399443671769));
#54894=CARTESIAN_POINT('Ctrl Pts',(-20.3120227388763,25.7853569415034,-74.0340892642411));
#54895=CARTESIAN_POINT('Ctrl Pts',(-20.3803803378345,25.8784276270414,-74.0282341613053));
#54896=CARTESIAN_POINT('Ctrl Pts',(-20.4488393836399,25.9716364351548,-74.0223703690395));
#54897=CARTESIAN_POINT('Ctrl Pts',(-20.5213231265793,26.0617007896389,-74.0165065767737));
#54898=CARTESIAN_POINT('Ctrl Pts',(-20.5974942498583,26.1482724563772,-74.0106427845079));
#54899=CARTESIAN_POINT('Ctrl Pts',(-20.6194792713164,26.1732593525784,-74.0089503373805));
#54900=CARTESIAN_POINT('Ctrl Pts',(-20.6417712484578,26.1979555352059,-74.007257890253));
#54901=CARTESIAN_POINT('Ctrl Pts',(-20.6643615458576,26.2223532442174,-74.0055654431255));
#54902=CARTESIAN_POINT('Ctrl Pts',(-20.7427683912889,26.3070332891714,-73.99969126458));
#54903=CARTESIAN_POINT('Ctrl Pts',(-20.8250362932512,26.3884006391815,-73.9938170860344));
#54904=CARTESIAN_POINT('Ctrl Pts',(-20.9108542445527,26.4660827191082,-73.9879429074889));
#54905=CARTESIAN_POINT('Ctrl Pts',(-20.9965611353252,26.5436642674705,-73.9820763309586));
#54906=CARTESIAN_POINT('Ctrl Pts',(-21.0858086355093,26.6175697555757,-73.9762097544284));
#54907=CARTESIAN_POINT('Ctrl Pts',(-21.1782469736425,26.687461264401,-73.9703431778981));
#54908=CARTESIAN_POINT('Ctrl Pts',(-21.2705903648361,26.7572809849944,-73.9644826271521));
#54909=CARTESIAN_POINT('Ctrl Pts',(-21.3661177473683,26.8230946794785,-73.9586220764062));
#54910=CARTESIAN_POINT('Ctrl Pts',(-21.4644446524362,26.884603216734,-73.9527615256602));
#54911=CARTESIAN_POINT('Ctrl Pts',(-21.5665673687757,26.9484862292041,-73.9466747342473));
#54912=CARTESIAN_POINT('Ctrl Pts',(-21.6717097729922,27.0077246879211,-73.9405879428344));
#54913=CARTESIAN_POINT('Ctrl Pts',(-21.7794056283828,27.0620313181545,-73.9345011514215));
#54914=CARTESIAN_POINT('Ctrl Pts',(-21.8829785022079,27.1142588968355,-73.9286473840995));
#54915=CARTESIAN_POINT('Ctrl Pts',(-21.9889125080763,27.1619251180764,-73.9227936167774));
#54916=CARTESIAN_POINT('Ctrl Pts',(-22.096766657896,27.204820606675,-73.9169398494553));
#54917=CARTESIAN_POINT('Ctrl Pts',(-22.2046043441469,27.2477095474234,-73.9110869756909));
#54918=CARTESIAN_POINT('Ctrl Pts',(-22.3143612078228,27.2858290509121,-73.9052341019265));
#54919=CARTESIAN_POINT('Ctrl Pts',(-22.4255762965451,27.3190178953234,-73.8993812281621));
#54920=CARTESIAN_POINT('Ctrl Pts',(-22.5368012936864,27.3522096966084,-73.8935278329511));
#54921=CARTESIAN_POINT('Ctrl Pts',(-22.6494843782854,27.3804698474238,-73.8876744377401));
#54922=CARTESIAN_POINT('Ctrl Pts',(-22.7631501424009,27.4036872111417,-73.8818210425292));
#54923=CARTESIAN_POINT('Ctrl Pts',(-22.8768535106594,27.4269122558802,-73.8759657108344));
#54924=CARTESIAN_POINT('Ctrl Pts',(-22.9915398003756,27.4450911135209,-73.8701103791396));
#54925=CARTESIAN_POINT('Ctrl Pts',(-23.1067248418525,27.4581640184533,-73.8642550474449));
#54926=CARTESIAN_POINT('Ctrl Pts',(-23.2220404474327,27.4712517417344,-73.8583930786371));
#54927=CARTESIAN_POINT('Ctrl Pts',(-23.3378555224973,27.4792219136071,-73.8525311098294));
#54928=CARTESIAN_POINT('Ctrl Pts',(-23.4536821185467,27.4820667637383,-73.8466691410216));
#54929=CARTESIAN_POINT('Ctrl Pts',(-23.5695865123549,27.4849135246825,-73.8408032348796));
#54930=CARTESIAN_POINT('Ctrl Pts',(-23.6855020305534,27.4826281170552,-73.8349373287375));
#54931=CARTESIAN_POINT('Ctrl Pts',(-23.8009438151018,27.4752548094545,-73.8290714225954));
#54932=CARTESIAN_POINT('Ctrl Pts',(-23.9165551367192,27.4678706734613,-73.8231969018209));
#54933=CARTESIAN_POINT('Ctrl Pts',(-24.0316909270041,27.4553837689823,-73.8173223810464));
#54934=CARTESIAN_POINT('Ctrl Pts',(-24.1458744202636,27.4378898046219,-73.811447860272));
#54935=CARTESIAN_POINT('Ctrl Pts',(-24.1767750169227,27.4331555481963,-73.8098580840982));
#54936=CARTESIAN_POINT('Ctrl Pts',(-24.2076059476972,27.4280548775577,-73.8082683079245));
#54937=CARTESIAN_POINT('Ctrl Pts',(-24.2383579509695,27.422590318092,-73.8066785317508));
#54938=CARTESIAN_POINT('Ctrl Pts',(-24.3519742737502,27.4024009617558,-73.8008049461731));
#54939=CARTESIAN_POINT('Ctrl Pts',(-24.4648906384944,27.3771733823538,-73.7949313605954));
#54940=CARTESIAN_POINT('Ctrl Pts',(-24.5766255530572,27.346967878019,-73.7890577750178));
#54941=CARTESIAN_POINT('Ctrl Pts',(-24.6882161795882,27.3168013793324,-73.7831917742502));
#54942=CARTESIAN_POINT('Ctrl Pts',(-24.7986279947573,27.2816698461074,-73.7773257734825));
#54943=CARTESIAN_POINT('Ctrl Pts',(-24.9073877158074,27.2416849219788,-73.7714597727149));
#54944=CARTESIAN_POINT('Ctrl Pts',(-25.0160360453782,27.201740950326,-73.765599779893));
#54945=CARTESIAN_POINT('Ctrl Pts',(-25.123035261007,27.1569536168588,-73.7597397870712));
#54946=CARTESIAN_POINT('Ctrl Pts',(-25.2279259647884,27.1074847214578,-73.7538797942493));
#54947=CARTESIAN_POINT('Ctrl Pts',(-25.3368801040218,27.0560994153921,-73.7477927870045));
#54948=CARTESIAN_POINT('Ctrl Pts',(-25.4435586228252,26.999662605872,-73.7417057797598));
#54949=CARTESIAN_POINT('Ctrl Pts',(-25.5474677321391,26.9384113891139,-73.7356187725151));
#54950=CARTESIAN_POINT('Ctrl Pts',(-25.6473865916651,26.8795123015993,-73.7297655145492));
#54951=CARTESIAN_POINT('Ctrl Pts',(-25.7447444286019,26.8161619765703,-73.7239122565833));
#54952=CARTESIAN_POINT('Ctrl Pts',(-25.8391268258036,26.7486182809113,-73.7180589986174));
#54953=CARTESIAN_POINT('Ctrl Pts',(-25.9334951195196,26.6810846782524,-73.7122066152992));
#54954=CARTESIAN_POINT('Ctrl Pts',(-26.0248885216434,26.6093591912674,-73.7063542319809));
#54955=CARTESIAN_POINT('Ctrl Pts',(-26.1129223459199,26.5337425054089,-73.7005018486627));
#54956=CARTESIAN_POINT('Ctrl Pts',(-26.2009643078742,26.4581188296892,-73.6946489243613));
#54957=CARTESIAN_POINT('Ctrl Pts',(-26.2856457611703,26.3786035092642,-73.68879600006));
#54958=CARTESIAN_POINT('Ctrl Pts',(-26.366616353408,26.2955364557614,-73.6829430757587));
#54959=CARTESIAN_POINT('Ctrl Pts',(-26.4476140145222,26.2124416325245,-73.6770881947953));
#54960=CARTESIAN_POINT('Ctrl Pts',(-26.5248980595177,26.1257930108825,-73.6712333138319));
#54961=CARTESIAN_POINT('Ctrl Pts',(-26.5981566290412,26.0359656312644,-73.6653784328685));
#54962=CARTESIAN_POINT('Ctrl Pts',(-26.6714986507999,25.9460359251111,-73.6595168823386));
#54963=CARTESIAN_POINT('Ctrl Pts',(-26.7408057830521,25.852920553796,-73.6536553318087));
#54964=CARTESIAN_POINT('Ctrl Pts',(-26.8058078761404,25.7570258320692,-73.6477937812787));
#54965=CARTESIAN_POINT('Ctrl Pts',(-26.8708538366292,25.6610663947006,-73.6419282750149));
#54966=CARTESIAN_POINT('Ctrl Pts',(-26.9315887569188,25.5623242231031,-73.636062768751));
#54967=CARTESIAN_POINT('Ctrl Pts',(-26.9877879478463,25.4612311455724,-73.6301972624872));
#54968=CARTESIAN_POINT('Ctrl Pts',(-27.0440699684829,25.3599890710533,-73.6243231112915));
#54969=CARTESIAN_POINT('Ctrl Pts',(-27.0958027338074,25.25638954356,-73.6184489600958));
#54970=CARTESIAN_POINT('Ctrl Pts',(-27.14280921265,25.1508853734538,-73.6125748089));
#54971=CARTESIAN_POINT('Ctrl Pts',(-27.155567983672,25.1222488199109,-73.6109804127253));
#54972=CARTESIAN_POINT('Ctrl Pts',(-27.1679788427514,25.0934720372478,-73.6093860165506));
#54973=CARTESIAN_POINT('Ctrl Pts',(-27.1800388861824,25.0645642633964,-73.6077916203759));
#54974=CARTESIAN_POINT('Ctrl Pts',(-27.2296008949614,24.945764745833,-73.6012392826782));
#54975=CARTESIAN_POINT('Ctrl Pts',(-27.2733751995325,24.8244139971785,-73.5946869449805));
#54976=CARTESIAN_POINT('Ctrl Pts',(-27.3111208139817,24.7010604058781,-73.5881346072828));
#54977=CARTESIAN_POINT('Ctrl Pts',(-27.3487184499471,24.5781904118824,-73.5816079574699));
#54978=CARTESIAN_POINT('Ctrl Pts',(-27.3803344475293,24.4533334638435,-73.5750813076571));
#54979=CARTESIAN_POINT('Ctrl Pts',(-27.4057768105741,24.3270546525509,-73.5685546578443));
#54980=CARTESIAN_POINT('Ctrl Pts',(-27.4313693794316,24.200030320434,-73.5619894762041));
#54981=CARTESIAN_POINT('Ctrl Pts',(-27.4507150012671,24.0715674845368,-73.555424294564));
#54982=CARTESIAN_POINT('Ctrl Pts',(-27.4636676401974,23.9422617006414,-73.5488591129239));
#54983=CARTESIAN_POINT('Ctrl Pts',(-27.4766202791278,23.812955916746,-73.5422939312838));
#54984=CARTESIAN_POINT('Ctrl Pts',(-27.4831797858945,23.6828074206673,-73.5357287496436));
#54985=CARTESIAN_POINT('Ctrl Pts',(-27.4832519295814,23.5524288172932,-73.5291635680035));
#54986=CARTESIAN_POINT('',(-27.4799905867943,23.5470322484969,-72.2791635220347));
#54987=CARTESIAN_POINT('Ctrl Pts',(-27.4778725016352,23.55242492899,-73.5291635220347));
#54988=CARTESIAN_POINT('Ctrl Pts',(-27.4739703607174,22.7574340764279,-73.4890772510234));
#54989=CARTESIAN_POINT('Ctrl Pts',(-26.8529990368603,20.6420195649947,-73.3826953428873));
#54990=CARTESIAN_POINT('Ctrl Pts',(-23.3948704418965,18.9009230350336,-73.210017797626));
#54991=CARTESIAN_POINT('Ctrl Pts',(-19.554684473212,21.167768508944,-73.0111308862512));
#54992=CARTESIAN_POINT('Ctrl Pts',(-19.3860646478423,25.6239837848511,-72.8122439748762));
#54993=CARTESIAN_POINT('Ctrl Pts',(-23.0439921451409,28.174579327054,-72.6133570635014));
#54994=CARTESIAN_POINT('Ctrl Pts',(-26.7277621119337,26.656849026205,-72.4356635792209));
#54995=CARTESIAN_POINT('Ctrl Pts',(-27.4731413038454,24.4402793233453,-72.3242657320653));
#54996=CARTESIAN_POINT('Ctrl Pts',(-27.4799905867943,23.5470322484969,-72.2791635220347));
#54997=CARTESIAN_POINT('',(-27.4856295271234,23.5494159766936,-71.0291638765219));
#54998=CARTESIAN_POINT('Ctrl Pts',(-27.4799905867943,23.5470322484969,-72.2791635220347));
#54999=CARTESIAN_POINT('Ctrl Pts',(-27.4832090494534,23.1272974562284,-72.2579700949403));
#55000=CARTESIAN_POINT('Ctrl Pts',(-27.2276593103525,21.398397011866,-72.1704810307208));
#55001=CARTESIAN_POINT('Ctrl Pts',(-24.7078912105456,19.0446320962057,-72.0166963293769));
#55002=CARTESIAN_POINT('Ctrl Pts',(-20.3853508355522,20.14083173501,-71.8178094180018));
#55003=CARTESIAN_POINT('Ctrl Pts',(-18.9710862915074,24.3700015369503,-71.618922506627));
#55004=CARTESIAN_POINT('Ctrl Pts',(-21.7646875315776,27.8458907001526,-71.420035595252));
#55005=CARTESIAN_POINT('Ctrl Pts',(-26.1477706968028,27.3799070216123,-71.2234495793812));
#55006=CARTESIAN_POINT('Ctrl Pts',(-27.4858620735673,24.8089282503745,-71.0931592006353));
#55007=CARTESIAN_POINT('Ctrl Pts',(-27.4895355474849,23.5494266036718,-71.0291644590143));
#55008=CARTESIAN_POINT('',(-27.4832508538687,23.5538854055544,-69.7791635439327));
#55009=CARTESIAN_POINT('Ctrl Pts',(-27.483252441345,23.5494095094363,-71.0291635220347));
#55010=CARTESIAN_POINT('Ctrl Pts',(-27.4832427515645,23.5042032228065,-71.0268629388572));
#55011=CARTESIAN_POINT('Ctrl Pts',(-27.4824536810313,23.4590061945149,-71.0245623556797));
#55012=CARTESIAN_POINT('Ctrl Pts',(-27.4808860205748,23.41383634464,-71.0222617725022));
#55013=CARTESIAN_POINT('Ctrl Pts',(-27.4768845272569,23.2985391502213,-71.0163894752369));
#55014=CARTESIAN_POINT('Ctrl Pts',(-27.4677990137816,23.1832250148259,-71.0105171779717));
#55015=CARTESIAN_POINT('Ctrl Pts',(-27.4536211817208,23.0683789154942,-71.0046448807064));
#55016=CARTESIAN_POINT('Ctrl Pts',(-27.4394617229954,22.9536816475135,-70.9987801934683));
#55017=CARTESIAN_POINT('Ctrl Pts',(-27.420223119379,22.8394516158931,-70.9929155062302));
#55018=CARTESIAN_POINT('Ctrl Pts',(-27.3959490620305,22.7261729259768,-70.9870508189921));
#55019=CARTESIAN_POINT('Ctrl Pts',(-27.3716999690168,22.6130107360384,-70.9811921632145));
#55020=CARTESIAN_POINT('Ctrl Pts',(-27.3424258089596,22.5007983435031,-70.9753335074368));
#55021=CARTESIAN_POINT('Ctrl Pts',(-27.3082218870988,22.3900131926612,-70.9694748516592));
#55022=CARTESIAN_POINT('Ctrl Pts',(-27.2726819324168,22.2749006843241,-70.9633873520537));
#55023=CARTESIAN_POINT('Ctrl Pts',(-27.2318192995848,22.161329640374,-70.9572998524482));
#55024=CARTESIAN_POINT('Ctrl Pts',(-27.1857991426444,22.0498226467585,-70.9512123528427));
#55025=CARTESIAN_POINT('Ctrl Pts',(-27.1415602906898,21.9426317610592,-70.945360482451));
#55026=CARTESIAN_POINT('Ctrl Pts',(-27.0925559282324,21.837348527908,-70.9395086120592));
#55027=CARTESIAN_POINT('Ctrl Pts',(-27.0389828294276,21.7344194144511,-70.9336567416675));
#55028=CARTESIAN_POINT('Ctrl Pts',(-26.9854178876001,21.6315059728603,-70.9278057622747));
#55029=CARTESIAN_POINT('Ctrl Pts',(-26.9272857833643,21.5309463048658,-70.921954782882));
#55030=CARTESIAN_POINT('Ctrl Pts',(-26.8648298748244,21.4331634838721,-70.9161038034892));
#55031=CARTESIAN_POINT('Ctrl Pts',(-26.8023683508848,21.3353718712423,-70.9102522980359));
#55032=CARTESIAN_POINT('Ctrl Pts',(-26.7355824723696,21.2403579503292,-70.9044007925826));
#55033=CARTESIAN_POINT('Ctrl Pts',(-26.6647592727034,21.1485163346467,-70.8985492871293));
#55034=CARTESIAN_POINT('Ctrl Pts',(-26.5939125541853,21.0566442203512,-70.8926958385177));
#55035=CARTESIAN_POINT('Ctrl Pts',(-26.5190261009088,20.9679468331937,-70.8868423899061));
#55036=CARTESIAN_POINT('Ctrl Pts',(-26.4404271499071,20.8827856291371,-70.8809889412945));
#55037=CARTESIAN_POINT('Ctrl Pts',(-26.3617388148394,20.7975275783083,-70.8751288360414));
#55038=CARTESIAN_POINT('Ctrl Pts',(-26.2793298357643,20.7158140411441,-70.8692687307883));
#55039=CARTESIAN_POINT('Ctrl Pts',(-26.1935642885217,20.6379695859251,-70.8634086255352));
#55040=CARTESIAN_POINT('Ctrl Pts',(-26.1077409835509,20.5600727073376,-70.857544573868));
#55041=CARTESIAN_POINT('Ctrl Pts',(-26.0185569267443,20.4860503623003,-70.8516805222007));
#55042=CARTESIAN_POINT('Ctrl Pts',(-25.9264078561718,20.4161857050364,-70.8458164705335));
#55043=CARTESIAN_POINT('Ctrl Pts',(-25.8341229763041,20.3462180812444,-70.8399437764272));
#55044=CARTESIAN_POINT('Ctrl Pts',(-25.738864700173,20.2804206087893,-70.834071082321));
#55045=CARTESIAN_POINT('Ctrl Pts',(-25.6410562499928,20.2190322130198,-70.8281983882147));
#55046=CARTESIAN_POINT('Ctrl Pts',(-25.614277983195,20.2022251289982,-70.8265905458523));
#55047=CARTESIAN_POINT('Ctrl Pts',(-25.5873086936766,20.1857482644168,-70.8249827034899));
#55048=CARTESIAN_POINT('Ctrl Pts',(-25.5601573454409,20.1696059012879,-70.8233748611275));
#55049=CARTESIAN_POINT('Ctrl Pts',(-25.4609929105405,20.1106494066143,-70.8175025641833));
#55050=CARTESIAN_POINT('Ctrl Pts',(-25.359066094642,20.0559610254743,-70.8116302672392));
#55051=CARTESIAN_POINT('Ctrl Pts',(-25.2547804313492,20.0058098901358,-70.8057579702949));
#55052=CARTESIAN_POINT('Ctrl Pts',(-25.1506299139877,19.9557237466827,-70.7998932833808));
#55053=CARTESIAN_POINT('Ctrl Pts',(-25.0441269973708,19.9101633335037,-70.7940285964668));
#55054=CARTESIAN_POINT('Ctrl Pts',(-24.9357025843097,19.8693535719688,-70.7881639095527));
#55055=CARTESIAN_POINT('Ctrl Pts',(-24.827389678963,19.8285857807163,-70.7823052541015));
#55056=CARTESIAN_POINT('Ctrl Pts',(-24.7171595923729,19.7925590678489,-70.7764465986504));
#55057=CARTESIAN_POINT('Ctrl Pts',(-24.6054655228979,19.7614513303648,-70.7705879431993));
#55058=CARTESIAN_POINT('Ctrl Pts',(-24.4894085840485,19.7291284970765,-70.7645004434723));
#55059=CARTESIAN_POINT('Ctrl Pts',(-24.3717713715992,19.7021169492531,-70.7584129437454));
#55060=CARTESIAN_POINT('Ctrl Pts',(-24.2530828186991,19.6805602199375,-70.7523254440185));
#55061=CARTESIAN_POINT('Ctrl Pts',(-24.1389883594895,19.6598378898266,-70.7464735739576));
#55062=CARTESIAN_POINT('Ctrl Pts',(-24.0239228798842,19.6441560301766,-70.7406217038967));
#55063=CARTESIAN_POINT('Ctrl Pts',(-23.9083683649091,19.633590426023,-70.7347698338358));
#55064=CARTESIAN_POINT('Ctrl Pts',(-23.7928314441503,19.6230264305778,-70.7289188547749));
#55065=CARTESIAN_POINT('Ctrl Pts',(-23.6768060476247,19.6175771793654,-70.7230678757139));
#55066=CARTESIAN_POINT('Ctrl Pts',(-23.5607796594119,19.6172666202546,-70.717216896653));
#55067=CARTESIAN_POINT('Ctrl Pts',(-23.4447428393001,19.6169560332216,-70.7113653915323));
#55068=CARTESIAN_POINT('Ctrl Pts',(-23.3287054407299,19.6217850578465,-70.7055138864115));
#55069=CARTESIAN_POINT('Ctrl Pts',(-23.2131546123612,19.6317255134409,-70.6996623812907));
#55070=CARTESIAN_POINT('Ctrl Pts',(-23.0975654120675,19.641669270045,-70.693808933012));
#55071=CARTESIAN_POINT('Ctrl Pts',(-22.9824635149095,19.6567277973703,-70.6879554847332));
#55072=CARTESIAN_POINT('Ctrl Pts',(-22.868329905299,19.6768211676953,-70.6821020364545));
#55073=CARTESIAN_POINT('Ctrl Pts',(-22.7540665009729,19.6969373885488,-70.6762419315331));
#55074=CARTESIAN_POINT('Ctrl Pts',(-22.6407739894265,19.7220998090305,-70.6703818266116));
#55075=CARTESIAN_POINT('Ctrl Pts',(-22.528922233783,19.7521775689573,-70.6645217216902));
#55076=CARTESIAN_POINT('Ctrl Pts',(-22.4169951529728,19.7822755843756,-70.6586576703544));
#55077=CARTESIAN_POINT('Ctrl Pts',(-22.3065111531423,19.8172954058531,-70.6527936190186));
#55078=CARTESIAN_POINT('Ctrl Pts',(-22.1979223698499,19.8570571491879,-70.6469295676827));
#55079=CARTESIAN_POINT('Ctrl Pts',(-22.0891735483504,19.8968774934013,-70.6410568739049));
#55080=CARTESIAN_POINT('Ctrl Pts',(-21.9823258981003,19.9414535488962,-70.6351841801271));
#55081=CARTESIAN_POINT('Ctrl Pts',(-21.8778092005089,19.9905584010175,-70.6293114863492));
#55082=CARTESIAN_POINT('Ctrl Pts',(-21.8491942732487,20.0040024898948,-70.6277036408169));
#55083=CARTESIAN_POINT('Ctrl Pts',(-21.8207539099472,20.01778578834,-70.6260957952846));
#55084=CARTESIAN_POINT('Ctrl Pts',(-21.7924965586072,20.0319030693643,-70.6244879497523));
#55085=CARTESIAN_POINT('Ctrl Pts',(-21.6892928905123,20.083463287012,-70.6186156528528));
#55086=CARTESIAN_POINT('Ctrl Pts',(-21.5881868738218,20.1396546383768,-70.6127433559532));
#55087=CARTESIAN_POINT('Ctrl Pts',(-21.4896230610458,20.2002831012821,-70.6068710590536));
#55088=CARTESIAN_POINT('Ctrl Pts',(-21.3911869791644,20.2608329945016,-70.6010063721857));
#55089=CARTESIAN_POINT('Ctrl Pts',(-21.2952868984824,20.3258083497012,-70.5951416853178));
#55090=CARTESIAN_POINT('Ctrl Pts',(-21.2023449703586,20.3949682206656,-70.5892769984499));
#55091=CARTESIAN_POINT('Ctrl Pts',(-21.1094986272077,20.4640569650188,-70.5834183430464));
#55092=CARTESIAN_POINT('Ctrl Pts',(-21.0196047150193,20.5373214199315,-70.577559687643));
#55093=CARTESIAN_POINT('Ctrl Pts',(-20.9330578744486,20.6144764629033,-70.5717010322395));
#55094=CARTESIAN_POINT('Ctrl Pts',(-20.8431304365711,20.6946452511344,-70.5656135324952));
#55095=CARTESIAN_POINT('Ctrl Pts',(-20.756817267376,20.7790145250746,-70.559526032751));
#55096=CARTESIAN_POINT('Ctrl Pts',(-20.6745250344264,20.8672168700866,-70.5534385330068));
#55097=CARTESIAN_POINT('Ctrl Pts',(-20.5954180988584,20.9520051541534,-70.5475866629969));
#55098=CARTESIAN_POINT('Ctrl Pts',(-20.520026917881,21.0403349619105,-70.5417347929872));
#55099=CARTESIAN_POINT('Ctrl Pts',(-20.4486757840577,21.1318417563046,-70.5358829229773));
#55100=CARTESIAN_POINT('Ctrl Pts',(-20.3773355141019,21.223334617946,-70.5300319439687));
#55101=CARTESIAN_POINT('Ctrl Pts',(-20.3100343223364,21.3180031785176,-70.5241809649599));
#55102=CARTESIAN_POINT('Ctrl Pts',(-20.2470558623188,21.4154502543328,-70.5183299859513));
#55103=CARTESIAN_POINT('Ctrl Pts',(-20.1840717399382,21.5129060915677,-70.5124784808839));
#55104=CARTESIAN_POINT('Ctrl Pts',(-20.1254113463097,21.613140593448,-70.5066269758165));
#55105=CARTESIAN_POINT('Ctrl Pts',(-20.0713142970534,21.715728680785,-70.5007754707491));
#55106=CARTESIAN_POINT('Ctrl Pts',(-20.0171992833495,21.8183508353835,-70.4949220225247));
#55107=CARTESIAN_POINT('Ctrl Pts',(-19.9676508199871,21.9233277640855,-70.4890685743004));
#55108=CARTESIAN_POINT('Ctrl Pts',(-19.9228616549023,22.030211602322,-70.4832151260761));
#55109=CARTESIAN_POINT('Ctrl Pts',(-19.8780215548136,22.1372169906856,-70.4773550212104));
#55110=CARTESIAN_POINT('Ctrl Pts',(-19.8379517157607,22.2461332354966,-70.4714949163448));
#55111=CARTESIAN_POINT('Ctrl Pts',(-19.8027960238171,22.3564942975573,-70.4656348114791));
#55112=CARTESIAN_POINT('Ctrl Pts',(-19.767616656717,22.4669296808805,-70.4597707601999));
#55113=CARTESIAN_POINT('Ctrl Pts',(-19.7373581339983,22.5788114208061,-70.4539067089207));
#55114=CARTESIAN_POINT('Ctrl Pts',(-19.7121135145048,22.6916618930725,-70.4480426576414));
#55115=CARTESIAN_POINT('Ctrl Pts',(-19.6868316894807,22.8046786844118,-70.442169963921));
#55116=CARTESIAN_POINT('Ctrl Pts',(-19.6665785877282,22.9186666520617,-70.4362972702006));
#55117=CARTESIAN_POINT('Ctrl Pts',(-19.6513956172167,23.0331415567276,-70.4304245764801));
#55118=CARTESIAN_POINT('Ctrl Pts',(-19.647238771979,23.0644828849565,-70.428816730446));
#55119=CARTESIAN_POINT('Ctrl Pts',(-19.6434616689011,23.0958607067755,-70.4272088844118));
#55120=CARTESIAN_POINT('Ctrl Pts',(-19.6400644769335,23.1272650893196,-70.4256010383776));
#55121=CARTESIAN_POINT('Ctrl Pts',(-19.6276569952297,23.2419625528554,-70.4197287413624));
#55122=CARTESIAN_POINT('Ctrl Pts',(-19.6202796337672,23.3573985511179,-70.4138564443473));
#55123=CARTESIAN_POINT('Ctrl Pts',(-19.6180094578943,23.4730941973888,-70.4079841473321));
#55124=CARTESIAN_POINT('Ctrl Pts',(-19.6157422239888,23.5886399113025,-70.4021194603469));
#55125=CARTESIAN_POINT('Ctrl Pts',(-19.6185690218743,23.7044441945922,-70.3962547733617));
#55126=CARTESIAN_POINT('Ctrl Pts',(-19.6265153301458,23.8200216425744,-70.3903900863765));
#55127=CARTESIAN_POINT('Ctrl Pts',(-19.6344534661374,23.9354802263973,-70.3845314308542));
#55128=CARTESIAN_POINT('Ctrl Pts',(-19.6475006117855,24.0507120290006,-70.3786727753319));
#55129=CARTESIAN_POINT('Ctrl Pts',(-19.6656302087334,24.1652309117649,-70.3728141198095));
#55130=CARTESIAN_POINT('Ctrl Pts',(-19.6844679634991,24.2842230016476,-70.3667266201092));
#55131=CARTESIAN_POINT('Ctrl Pts',(-19.7087933227104,24.4024448871687,-70.360639120409));
#55132=CARTESIAN_POINT('Ctrl Pts',(-19.7385169953152,24.5193558289259,-70.3545516207087));
#55133=CARTESIAN_POINT('Ctrl Pts',(-19.7670901502209,24.6317414850802,-70.3486997505768));
#55134=CARTESIAN_POINT('Ctrl Pts',(-19.8006513714833,24.7429153581334,-70.342847880445));
#55135=CARTESIAN_POINT('Ctrl Pts',(-19.8390692618257,24.8524075675668,-70.3369960103131));
#55136=CARTESIAN_POINT('Ctrl Pts',(-19.8774813026968,24.9618831058207,-70.3311450311815));
#55137=CARTESIAN_POINT('Ctrl Pts',(-19.9207484055142,25.0696770995997,-70.3252940520498));
#55138=CARTESIAN_POINT('Ctrl Pts',(-19.9686897397363,25.1753362117743,-70.3194430729181));
#55139=CARTESIAN_POINT('Ctrl Pts',(-20.0166353843474,25.2810048237237,-70.3135915677269));
#55140=CARTESIAN_POINT('Ctrl Pts',(-20.0692559249819,25.3845377960297,-70.3077400625357));
#55141=CARTESIAN_POINT('Ctrl Pts',(-20.1263232577722,25.4855037627183,-70.3018885573444));
#55142=CARTESIAN_POINT('Ctrl Pts',(-20.183409541383,25.586503258009,-70.2960351089956));
#55143=CARTESIAN_POINT('Ctrl Pts',(-20.2449453501414,25.6849336929597,-70.2901816606467));
#55144=CARTESIAN_POINT('Ctrl Pts',(-20.310658076488,25.780390815702,-70.2843282122979));
#55145=CARTESIAN_POINT('Ctrl Pts',(-20.376445532473,25.87595649392,-70.2784681073072));
#55146=CARTESIAN_POINT('Ctrl Pts',(-20.4464191524863,25.9685417702502,-70.2726080023166));
#55147=CARTESIAN_POINT('Ctrl Pts',(-20.5202646264403,26.0577736769719,-70.266747897326));
#55148=CARTESIAN_POINT('Ctrl Pts',(-20.5941598306995,26.1470656757985,-70.2608838459214));
#55149=CARTESIAN_POINT('Ctrl Pts',(-20.6719318041427,26.232999502574,-70.2550197945168));
#55150=CARTESIAN_POINT('Ctrl Pts',(-20.7532290157016,26.3152386891612,-70.2491557431122));
#55151=CARTESIAN_POINT('Ctrl Pts',(-20.8346460431168,26.3975990798878,-70.2432830492668));
#55152=CARTESIAN_POINT('Ctrl Pts',(-20.9195983756635,26.4762536831418,-70.2374103554213));
#55153=CARTESIAN_POINT('Ctrl Pts',(-21.0077009974478,26.5509059098273,-70.2315376615759));
#55154=CARTESIAN_POINT('Ctrl Pts',(-21.0318220143301,26.5713444346261,-70.2299298167182));
#55155=CARTESIAN_POINT('Ctrl Pts',(-21.0561790002685,26.5914832027443,-70.2283219718605));
#55156=CARTESIAN_POINT('Ctrl Pts',(-21.0807636899205,26.6113167029188,-70.2267141270027));
#55157=CARTESIAN_POINT('Ctrl Pts',(-21.1705538196383,26.6837541661788,-70.2208418300412));
#55158=CARTESIAN_POINT('Ctrl Pts',(-21.2636842842061,26.7523589143102,-70.2149695330797));
#55159=CARTESIAN_POINT('Ctrl Pts',(-21.359793845292,26.8168072523694,-70.2090972361182));
#55160=CARTESIAN_POINT('Ctrl Pts',(-21.4557788560196,26.8811720705008,-70.2032325491872));
#55161=CARTESIAN_POINT('Ctrl Pts',(-21.5547349456072,26.9413909620253,-70.1973678622562));
#55162=CARTESIAN_POINT('Ctrl Pts',(-21.6562675072221,26.9971801095634,-70.1915031753252));
#55163=CARTESIAN_POINT('Ctrl Pts',(-21.7576956489535,27.0529118814558,-70.1856445198576));
#55164=CARTESIAN_POINT('Ctrl Pts',(-21.8616946321271,27.104222773039,-70.1797858643899));
#55165=CARTESIAN_POINT('Ctrl Pts',(-21.967841104258,27.1508723497699,-70.1739272089223));
#55166=CARTESIAN_POINT('Ctrl Pts',(-22.0781337512672,27.1993441001372,-70.1678397092017));
#55167=CARTESIAN_POINT('Ctrl Pts',(-22.1907446953129,27.2427827086799,-70.1617522094811));
#55168=CARTESIAN_POINT('Ctrl Pts',(-22.3051707376551,27.2809710048777,-70.1556647097605));
#55169=CARTESIAN_POINT('Ctrl Pts',(-22.4151676762777,27.3176811417222,-70.1498128396842));
#55170=CARTESIAN_POINT('Ctrl Pts',(-22.5268413827651,27.3495397146062,-70.1439609696079));
#55171=CARTESIAN_POINT('Ctrl Pts',(-22.6397255129632,27.3764032799216,-70.1381090995316));
#55172=CARTESIAN_POINT('Ctrl Pts',(-22.7525924555269,27.403262755015,-70.1322581204557));
#55173=CARTESIAN_POINT('Ctrl Pts',(-22.8666690533158,27.4251286390516,-70.1264071413798));
#55174=CARTESIAN_POINT('Ctrl Pts',(-22.981476159631,27.4419080198615,-70.1205561623039));
#55175=CARTESIAN_POINT('Ctrl Pts',(-23.0962935882111,27.4586889092994,-70.1147046571686));
#55176=CARTESIAN_POINT('Ctrl Pts',(-23.2118412468211,27.470382326604,-70.1088531520333));
#55177=CARTESIAN_POINT('Ctrl Pts',(-23.3276329202268,27.4769470077886,-70.103001646898));
#55178=CARTESIAN_POINT('Ctrl Pts',(-23.4434630455278,27.4835138689609,-70.0971481986052));
#55179=CARTESIAN_POINT('Ctrl Pts',(-23.55953693425,27.4849485840369,-70.0912947503124));
#55180=CARTESIAN_POINT('Ctrl Pts',(-23.6753671265787,27.4812619870564,-70.0854413020195));
#55181=CARTESIAN_POINT('Ctrl Pts',(-23.7913290429907,27.4775711976145,-70.0795811970848));
#55182=CARTESIAN_POINT('Ctrl Pts',(-23.9070462964358,27.4687474846583,-70.0737210921501));
#55183=CARTESIAN_POINT('Ctrl Pts',(-24.0220352049937,27.4548536776724,-70.0678609872154));
#55184=CARTESIAN_POINT('Ctrl Pts',(-24.1371015513859,27.4409505140769,-70.0619969358667));
#55185=CARTESIAN_POINT('Ctrl Pts',(-24.2514381694125,27.4219705252512,-70.056132884518));
#55186=CARTESIAN_POINT('Ctrl Pts',(-24.364571965347,27.3980275848873,-70.0502688331694));
#55187=CARTESIAN_POINT('Ctrl Pts',(-24.477872497916,27.3740493574082,-70.0443961393794));
#55188=CARTESIAN_POINT('Ctrl Pts',(-24.5899662716441,27.3450936832612,-70.0385234455895));
#55189=CARTESIAN_POINT('Ctrl Pts',(-24.7003956437437,27.3113241637965,-70.0326507517995));
#55190=CARTESIAN_POINT('Ctrl Pts',(-24.7306293598649,27.3020786338652,-70.031042906409));
#55191=CARTESIAN_POINT('Ctrl Pts',(-24.7607384368583,27.2924725477748,-70.0294350610184));
#55192=CARTESIAN_POINT('Ctrl Pts',(-24.7907137702284,27.2825098802293,-70.0278272156279));
#55193=CARTESIAN_POINT('Ctrl Pts',(-24.9001919949714,27.2461234573288,-70.021954918668));
#55194=CARTESIAN_POINT('Ctrl Pts',(-25.0082512847691,27.2048550096705,-70.0160826217083));
#55195=CARTESIAN_POINT('Ctrl Pts',(-25.1144240450024,27.1588334822834,-70.0102103247485));
#55196=CARTESIAN_POINT('Ctrl Pts',(-25.2204592137675,27.1128715951421,-70.0043456378193));
#55197=CARTESIAN_POINT('Ctrl Pts',(-25.3246123389994,27.0621690404198,-69.9984809508901));
#55198=CARTESIAN_POINT('Ctrl Pts',(-25.426431338653,27.0069043921393,-69.992616263961));
#55199=CARTESIAN_POINT('Ctrl Pts',(-25.5281456238366,26.9516965800915,-69.9867576084954));
#55200=CARTESIAN_POINT('Ctrl Pts',(-25.6275301970324,26.8919362027846,-69.9808989530298));
#55201=CARTESIAN_POINT('Ctrl Pts',(-25.7241539366599,26.8278494687028,-69.9750402975642));
#55202=CARTESIAN_POINT('Ctrl Pts',(-25.8245518848761,26.7612594501992,-69.9689527978429));
#55203=CARTESIAN_POINT('Ctrl Pts',(-25.921968504259,26.6899983829722,-69.9628652981216));
#55204=CARTESIAN_POINT('Ctrl Pts',(-26.0159490853543,26.6143722266913,-69.9567777984003));
#55205=CARTESIAN_POINT('Ctrl Pts',(-26.1062919478126,26.5416733419268,-69.9509259283264));
#55206=CARTESIAN_POINT('Ctrl Pts',(-26.1934594722299,26.4649412882319,-69.9450740582525));
#55207=CARTESIAN_POINT('Ctrl Pts',(-26.2770788983064,26.3844908714159,-69.9392221881787));
#55208=CARTESIAN_POINT('Ctrl Pts',(-26.3606855925636,26.3040527039087,-69.9333712091053));
#55209=CARTESIAN_POINT('Ctrl Pts',(-26.4407449648164,26.2198975855049,-69.9275202300319));
#55210=CARTESIAN_POINT('Ctrl Pts',(-26.5169198473938,26.1323784073942,-69.9216692509586));
#55211=CARTESIAN_POINT('Ctrl Pts',(-26.5931015788251,26.0448513604684,-69.915817745826));
#55212=CARTESIAN_POINT('Ctrl Pts',(-26.6653978548847,25.9539599644044,-69.9099662406934));
#55213=CARTESIAN_POINT('Ctrl Pts',(-26.7335111395414,25.8600909753016,-69.9041147355608));
#55214=CARTESIAN_POINT('Ctrl Pts',(-26.8016470431362,25.7661908143523,-69.8982612872708));
#55215=CARTESIAN_POINT('Ctrl Pts',(-26.8655969505795,25.6693114286132,-69.8924078389809));
#55216=CARTESIAN_POINT('Ctrl Pts',(-26.9251064840354,25.5698687824624,-69.8865543906909));
#55217=CARTESIAN_POINT('Ctrl Pts',(-26.9846836927524,25.4703130484304,-69.8806942857592));
#55218=CARTESIAN_POINT('Ctrl Pts',(-27.0398102360944,25.368188590696,-69.8748341808275));
#55219=CARTESIAN_POINT('Ctrl Pts',(-27.0902775229772,25.2639363009736,-69.8689740758958));
#55220=CARTESIAN_POINT('Ctrl Pts',(-27.1407787964188,25.1596138038597,-69.8631100245503));
#55221=CARTESIAN_POINT('Ctrl Pts',(-27.186614402501,25.0531610002021,-69.8572459732048));
#55222=CARTESIAN_POINT('Ctrl Pts',(-27.2276244178556,24.9450374652483,-69.8513819218592));
#55223=CARTESIAN_POINT('Ctrl Pts',(-27.2686948737866,24.8367545777872,-69.8455092280726));
#55224=CARTESIAN_POINT('Ctrl Pts',(-27.3049254160151,24.7267964358507,-69.8396365342859));
#55225=CARTESIAN_POINT('Ctrl Pts',(-27.3362063097734,24.6156364954592,-69.8337638404993));
#55226=CARTESIAN_POINT('Ctrl Pts',(-27.3447704957242,24.5852027614637,-69.8321559950838));
#55227=CARTESIAN_POINT('Ctrl Pts',(-27.3529639669847,24.5546789925653,-69.8305481496684));
#55228=CARTESIAN_POINT('Ctrl Pts',(-27.3607851461743,24.5240749970254,-69.8289403042529));
#55229=CARTESIAN_POINT('Ctrl Pts',(-27.3982292934994,24.3775573824872,-69.8212426925305));
#55230=CARTESIAN_POINT('Ctrl Pts',(-27.4272382874208,24.2288027131749,-69.8135450808082));
#55231=CARTESIAN_POINT('Ctrl Pts',(-27.4475957085458,24.0786512086875,-69.8058474690858));
#55232=CARTESIAN_POINT('Ctrl Pts',(-27.4674978941642,23.9318574132038,-69.7983219924365));
#55233=CARTESIAN_POINT('Ctrl Pts',(-27.4791311547766,23.7837282753288,-69.7907965157872));
#55234=CARTESIAN_POINT('Ctrl Pts',(-27.4823378263443,23.6350713715633,-69.7832710391378));
#55235=CARTESIAN_POINT('Ctrl Pts',(-27.4829212395818,23.6080251325948,-69.7819018740694));
#55236=CARTESIAN_POINT('Ctrl Pts',(-27.4832258439406,23.5809614915974,-69.780532709001));
#55237=CARTESIAN_POINT('Ctrl Pts',(-27.4832508538687,23.5538854055544,-69.7791635439327));
#55238=CARTESIAN_POINT('',(-27.48082193576,23.5494884268893,-68.5291634982728));
#55239=CARTESIAN_POINT('Ctrl Pts',(-27.4825506534957,23.5538843258169,-69.7791635220347));
#55240=CARTESIAN_POINT('Ctrl Pts',(-27.4736068510643,22.571135203937,-69.7294601456491));
#55241=CARTESIAN_POINT('Ctrl Pts',(-26.6026245505,20.2634339527826,-69.6134611321385));
#55242=CARTESIAN_POINT('Ctrl Pts',(-22.7246114047614,18.9721451101221,-69.4311664815032));
#55243=CARTESIAN_POINT('Ctrl Pts',(-19.252319914895,21.7702171237683,-69.2322795701282));
#55244=CARTESIAN_POINT('Ctrl Pts',(-19.7294640953999,26.2039907547912,-69.0333926587533));
#55245=CARTESIAN_POINT('Ctrl Pts',(-23.7175888993554,28.1992039588933,-68.8345057473784));
#55246=CARTESIAN_POINT('Ctrl Pts',(-26.9579470188054,26.275131802411,-68.6664293684722));
#55247=CARTESIAN_POINT('Ctrl Pts',(-27.4756470504516,24.2536744838534,-68.564648626691));
#55248=CARTESIAN_POINT('Ctrl Pts',(-27.4768626123758,23.549489668419,-68.5291635220347));
#55249=CARTESIAN_POINT('',(-27.4835405418261,23.5468852840711,-67.2791635220347));
#55250=CARTESIAN_POINT('Ctrl Pts',(-27.4832524573208,23.5494876647477,-68.529163483686));
#55251=CARTESIAN_POINT('Ctrl Pts',(-27.4832283862113,23.425712317898,-68.5229363586002));
#55252=CARTESIAN_POINT('Ctrl Pts',(-27.4773570697139,23.302085006948,-68.5167092335144));
#55253=CARTESIAN_POINT('Ctrl Pts',(-27.4657057254873,23.1791524276579,-68.5104821084287));
#55254=CARTESIAN_POINT('Ctrl Pts',(-27.4540152803793,23.0558072974982,-68.5042340856616));
#55255=CARTESIAN_POINT('Ctrl Pts',(-27.4365060316608,22.9331618903031,-68.4979860628945));
#55256=CARTESIAN_POINT('Ctrl Pts',(-27.4132968556742,22.8117557131729,-68.4917380401273));
#55257=CARTESIAN_POINT('Ctrl Pts',(-27.3900487592371,22.6901459448813,-68.4854795397862));
#55258=CARTESIAN_POINT('Ctrl Pts',(-27.361081730058,22.5697798724058,-68.479221039445));
#55259=CARTESIAN_POINT('Ctrl Pts',(-27.3265646982176,22.4511822787225,-68.4729625391039));
#55260=CARTESIAN_POINT('Ctrl Pts',(-27.2919438843206,22.3322280986956,-68.4666852213847));
#55261=CARTESIAN_POINT('Ctrl Pts',(-27.2517397888736,22.2150533457786,-68.4604079036655));
#55262=CARTESIAN_POINT('Ctrl Pts',(-27.2061705425266,22.1001654660076,-68.4541305859463));
#55263=CARTESIAN_POINT('Ctrl Pts',(-27.1640695518829,21.9940216532599,-68.4483310321738));
#55264=CARTESIAN_POINT('Ctrl Pts',(-27.1173896272137,21.8898297857102,-68.4425314784013));
#55265=CARTESIAN_POINT('Ctrl Pts',(-27.0663369843744,21.7879701702037,-68.4367319246287));
#55266=CARTESIAN_POINT('Ctrl Pts',(-27.014643993578,21.6848329401982,-68.4308596276601));
#55267=CARTESIAN_POINT('Ctrl Pts',(-26.9583225723137,21.583799319875,-68.4249873306915));
#55268=CARTESIAN_POINT('Ctrl Pts',(-26.897567314718,21.4853136116894,-68.4191150337228));
#55269=CARTESIAN_POINT('Ctrl Pts',(-26.836890791111,21.3869555331601,-68.4132503467847));
#55270=CARTESIAN_POINT('Ctrl Pts',(-26.7717920727394,21.2911391490672,-68.4073856598465));
#55271=CARTESIAN_POINT('Ctrl Pts',(-26.70251264891,21.1982863003442,-68.4015209729084));
#55272=CARTESIAN_POINT('Ctrl Pts',(-26.633304474631,21.1055289449634,-68.3956623174336));
#55273=CARTESIAN_POINT('Ctrl Pts',(-26.5599243927277,21.0157293920309,-68.3898036619588));
#55274=CARTESIAN_POINT('Ctrl Pts',(-26.4826580333507,20.9292819149465,-68.3839450064841));
#55275=CARTESIAN_POINT('Ctrl Pts',(-26.4023735819201,20.8394577232641,-68.3778575067661));
#55276=CARTESIAN_POINT('Ctrl Pts',(-26.3178932996183,20.7532532029775,-68.3717700070482));
#55277=CARTESIAN_POINT('Ctrl Pts',(-26.2295851241246,20.6710745484601,-68.3656825073303));
#55278=CARTESIAN_POINT('Ctrl Pts',(-26.1446951045384,20.5920767936933,-68.3598306372469));
#55279=CARTESIAN_POINT('Ctrl Pts',(-26.05626834603,20.5167993482214,-68.3539787671636));
#55280=CARTESIAN_POINT('Ctrl Pts',(-25.9646698027029,20.4455660352094,-68.3481268970802));
#55281=CARTESIAN_POINT('Ctrl Pts',(-25.873085206087,20.3743435681171,-68.3422759179973));
#55282=CARTESIAN_POINT('Ctrl Pts',(-25.7783301111103,20.3071642628654,-68.3364249389144));
#55283=CARTESIAN_POINT('Ctrl Pts',(-25.6808020661824,20.2443112616332,-68.3305739598315));
#55284=CARTESIAN_POINT('Ctrl Pts',(-25.5832652525447,20.1814526093114,-68.3247224546892));
#55285=CARTESIAN_POINT('Ctrl Pts',(-25.4829553408366,20.1229212582056,-68.318870949547));
#55286=CARTESIAN_POINT('Ctrl Pts',(-25.3802977182725,20.0689562766935,-68.3130194444048));
#55287=CARTESIAN_POINT('Ctrl Pts',(-25.2776060053466,20.0149733745859,-68.3071659961051));
#55288=CARTESIAN_POINT('Ctrl Pts',(-25.1725653970445,19.9655600495693,-68.3013125478053));
#55289=CARTESIAN_POINT('Ctrl Pts',(-25.0656240056263,19.9209084730532,-68.2954590995056));
#55290=CARTESIAN_POINT('Ctrl Pts',(-24.9585609986243,19.8762061179987,-68.2895989945641));
#55291=CARTESIAN_POINT('Ctrl Pts',(-24.8495932757046,19.836276479274,-68.2837388896226));
#55292=CARTESIAN_POINT('Ctrl Pts',(-24.7391870608596,19.801262843077,-68.2778787846811));
#55293=CARTESIAN_POINT('Ctrl Pts',(-24.6287064943391,19.7662256273874,-68.2720147333258));
#55294=CARTESIAN_POINT('Ctrl Pts',(-24.5167859051605,19.7361111134737,-68.2661506819704));
#55295=CARTESIAN_POINT('Ctrl Pts',(-24.4039030369592,19.711011745437,-68.260286630615));
#55296=CARTESIAN_POINT('Ctrl Pts',(-24.2908538019437,19.6858753859421,-68.2544139368185));
#55297=CARTESIAN_POINT('Ctrl Pts',(-24.1768398630102,19.6657689955036,-68.2485412430219));
#55298=CARTESIAN_POINT('Ctrl Pts',(-24.0623455123509,19.6507333588779,-68.2426685492254));
#55299=CARTESIAN_POINT('Ctrl Pts',(-24.0309988743857,19.6466168530837,-68.2410607039015));
#55300=CARTESIAN_POINT('Ctrl Pts',(-23.9996162315936,19.6428801357629,-68.2394528585776));
#55301=CARTESIAN_POINT('Ctrl Pts',(-23.9682075170356,19.6395233630828,-68.2378450132537));
#55302=CARTESIAN_POINT('Ctrl Pts',(-23.8534941820222,19.627263498442,-68.2319727162851));
#55303=CARTESIAN_POINT('Ctrl Pts',(-23.7380487862485,19.6200347002225,-68.2261004193164));
#55304=CARTESIAN_POINT('Ctrl Pts',(-23.6223503152049,19.6179134174248,-68.2202281223477));
#55305=CARTESIAN_POINT('Ctrl Pts',(-23.5068017801913,19.6157948836412,-68.2143634354095));
#55306=CARTESIAN_POINT('Ctrl Pts',(-23.3910012316118,19.6187707101027,-68.2084987484713));
#55307=CARTESIAN_POINT('Ctrl Pts',(-23.2754341065293,19.6268657507115,-68.2026340615331));
#55308=CARTESIAN_POINT('Ctrl Pts',(-23.1599858350003,19.6349524660778,-68.1967754060583));
#55309=CARTESIAN_POINT('Ctrl Pts',(-23.044770919367,19.6481478949392,-68.1909167505835));
#55310=CARTESIAN_POINT('Ctrl Pts',(-22.9302754636613,19.6664248533447,-68.1850580951087));
#55311=CARTESIAN_POINT('Ctrl Pts',(-22.8113077146091,19.6854157258438,-68.1789705953908));
#55312=CARTESIAN_POINT('Ctrl Pts',(-22.6931172313741,19.7098932070916,-68.1728830956729));
#55313=CARTESIAN_POINT('Ctrl Pts',(-22.5762446380117,19.7397673102238,-68.166795595955));
#55314=CARTESIAN_POINT('Ctrl Pts',(-22.4638958471521,19.7684850726039,-68.1609437258716));
#55315=CARTESIAN_POINT('Ctrl Pts',(-22.3527652576022,19.8021893376685,-68.1550918557882));
#55316=CARTESIAN_POINT('Ctrl Pts',(-22.2433225803882,19.8407481035557,-68.1492399857048));
#55317=CARTESIAN_POINT('Ctrl Pts',(-22.1338965668171,19.8793009985201,-68.1433890066219));
#55318=CARTESIAN_POINT('Ctrl Pts',(-22.0261583443687,19.9227067873276,-68.1375380275389));
#55319=CARTESIAN_POINT('Ctrl Pts',(-21.9205610170775,19.9707840561819,-68.131687048456));
#55320=CARTESIAN_POINT('Ctrl Pts',(-21.8149541955703,20.0188656476454,-68.1258355433137));
#55321=CARTESIAN_POINT('Ctrl Pts',(-21.7114890281137,20.0716193827978,-68.1199840381714));
#55322=CARTESIAN_POINT('Ctrl Pts',(-21.6105965867679,20.1288166028316,-68.1141325330291));
#55323=CARTESIAN_POINT('Ctrl Pts',(-21.5096706412387,20.1860328168169,-68.1082790847294));
#55324=CARTESIAN_POINT('Ctrl Pts',(-21.4113194800582,20.2476952460285,-68.1024256364296));
#55325=CARTESIAN_POINT('Ctrl Pts',(-21.3159470039309,20.3135307628969,-68.0965721881299));
#55326=CARTESIAN_POINT('Ctrl Pts',(-21.2204660685884,20.3794411490438,-68.0907120831884));
#55327=CARTESIAN_POINT('Ctrl Pts',(-21.127970919872,20.4495338601562,-68.0848519782468));
#55328=CARTESIAN_POINT('Ctrl Pts',(-21.0388341206963,20.5234941064311,-68.0789918733053));
#55329=CARTESIAN_POINT('Ctrl Pts',(-20.9496372934653,20.5975041603029,-68.0731278219499));
#55330=CARTESIAN_POINT('Ctrl Pts',(-20.8638036245391,20.675386658396,-68.0672637705945));
#55331=CARTESIAN_POINT('Ctrl Pts',(-20.7816691293789,20.75678963693,-68.0613997192391));
#55332=CARTESIAN_POINT('Ctrl Pts',(-20.6994135843686,20.8383125872047,-68.0555270254425));
#55333=CARTESIAN_POINT('Ctrl Pts',(-20.620868373355,20.9233660705823,-68.0496543316459));
#55334=CARTESIAN_POINT('Ctrl Pts',(-20.5463295896988,21.0115646898055,-68.0437816378494));
#55335=CARTESIAN_POINT('Ctrl Pts',(-20.5259221176133,21.0357119963684,-68.0421737925259));
#55336=CARTESIAN_POINT('Ctrl Pts',(-20.5058147058072,21.0600948861663,-68.0405659472024));
#55337=CARTESIAN_POINT('Ctrl Pts',(-20.4860128549072,21.0847050867635,-68.0389581018789));
#55338=CARTESIAN_POINT('Ctrl Pts',(-20.4136910044672,21.1745883636287,-68.0330858049102));
#55339=CARTESIAN_POINT('Ctrl Pts',(-20.3452061647447,21.2678070401771,-68.0272135079415));
#55340=CARTESIAN_POINT('Ctrl Pts',(-20.2808815655298,21.3639994618046,-68.0213412109727));
#55341=CARTESIAN_POINT('Ctrl Pts',(-20.216640325887,21.4600672256932,-68.0154765240345));
#55342=CARTESIAN_POINT('Ctrl Pts',(-20.156548832977,21.5591007305008,-68.0096118370963));
#55343=CARTESIAN_POINT('Ctrl Pts',(-20.1008903961162,21.6607050044695,-68.003747150158));
#55344=CARTESIAN_POINT('Ctrl Pts',(-20.0452892004735,21.7622047848029,-67.9978884946832));
#55345=CARTESIAN_POINT('Ctrl Pts',(-19.994112189964,21.8662697151237,-67.9920298392084));
#55346=CARTESIAN_POINT('Ctrl Pts',(-19.94759925411,21.9724761338761,-67.9861711837335));
#55347=CARTESIAN_POINT('Ctrl Pts',(-19.8992694820138,22.0828310688898,-67.9800836840156));
#55348=CARTESIAN_POINT('Ctrl Pts',(-19.8559758310383,22.1954978217528,-67.9739961842977));
#55349=CARTESIAN_POINT('Ctrl Pts',(-19.8179348239456,22.3099729146617,-67.9679086845798));
#55350=CARTESIAN_POINT('Ctrl Pts',(-19.7813662750067,22.4200170054272,-67.9620568144964));
#55351=CARTESIAN_POINT('Ctrl Pts',(-19.7496514438923,22.5317316190854,-67.9562049444129));
#55352=CARTESIAN_POINT('Ctrl Pts',(-19.7229331739432,22.6446502272666,-67.9503530743295));
#55353=CARTESIAN_POINT('Ctrl Pts',(-19.6962189720937,22.757551642563,-67.9445020952465));
#55354=CARTESIAN_POINT('Ctrl Pts',(-19.6744999139099,22.8716562857205,-67.9386511161635));
#55355=CARTESIAN_POINT('Ctrl Pts',(-19.6578682948601,22.9864848908653,-67.9328001370805));
#55356=CARTESIAN_POINT('Ctrl Pts',(-19.6412351804678,23.1013238202067,-67.9269486319382));
#55357=CARTESIAN_POINT('Ctrl Pts',(-19.629690473757,23.2168864317923,-67.9210971267959));
#55358=CARTESIAN_POINT('Ctrl Pts',(-19.6232748129593,23.332686457686,-67.9152456216535));
#55359=CARTESIAN_POINT('Ctrl Pts',(-19.6168570216602,23.4485249382475,-67.9093921733537));
#55360=CARTESIAN_POINT('Ctrl Pts',(-19.6155716859241,23.5646005773543,-67.903538725054));
#55361=CARTESIAN_POINT('Ctrl Pts',(-19.6194073443974,23.6804259295369,-67.8976852767542));
#55362=CARTESIAN_POINT('Ctrl Pts',(-19.6232473648473,23.796383000296,-67.8918251718126));
#55363=CARTESIAN_POINT('Ctrl Pts',(-19.6322199897106,23.9120888026154,-67.885965066871));
#55364=CARTESIAN_POINT('Ctrl Pts',(-19.646261767094,24.0270597358308,-67.8801049619294));
#55365=CARTESIAN_POINT('Ctrl Pts',(-19.6603130007356,24.1421080947738,-67.874240910574));
#55366=CARTESIAN_POINT('Ctrl Pts',(-19.6794401163117,24.2564201924733,-67.8683768592185));
#55367=CARTESIAN_POINT('Ctrl Pts',(-19.7035286313899,24.3695230821397,-67.862512807863));
#55368=CARTESIAN_POINT('Ctrl Pts',(-19.7276526481307,24.482792662888,-67.8566401140664));
#55369=CARTESIAN_POINT('Ctrl Pts',(-19.7567525544247,24.5948490802039,-67.8507674202698));
#55370=CARTESIAN_POINT('Ctrl Pts',(-19.7906641601067,24.7052349022195,-67.8448947264732));
#55371=CARTESIAN_POINT('Ctrl Pts',(-19.7999485904692,24.7354566937536,-67.8432868811501));
#55372=CARTESIAN_POINT('Ctrl Pts',(-19.8095934162612,24.7655533822659,-67.841679035827));
#55373=CARTESIAN_POINT('Ctrl Pts',(-19.8195946510658,24.7955158683845,-67.8400711905039));
#55374=CARTESIAN_POINT('Ctrl Pts',(-19.8561219338723,24.9049471761611,-67.8341988935352));
#55375=CARTESIAN_POINT('Ctrl Pts',(-19.8975294113498,25.0129532673691,-67.8283265965665));
#55376=CARTESIAN_POINT('Ctrl Pts',(-19.9436875368159,25.1190667137178,-67.8224542995978));
#55377=CARTESIAN_POINT('Ctrl Pts',(-19.9897858450172,25.2250426454674,-67.8165896126596));
#55378=CARTESIAN_POINT('Ctrl Pts',(-20.040622394843,25.3291304343588,-67.8107249257215));
#55379=CARTESIAN_POINT('Ctrl Pts',(-20.0960180306221,25.4308782285311,-67.8048602387833));
#55380=CARTESIAN_POINT('Ctrl Pts',(-20.1513566954577,25.5325213814667,-67.7990015833085));
#55381=CARTESIAN_POINT('Ctrl Pts',(-20.2112449236353,25.6318289655324,-67.7931429278336));
#55382=CARTESIAN_POINT('Ctrl Pts',(-20.2754559520363,25.7283701506168,-67.7872842723588));
#55383=CARTESIAN_POINT('Ctrl Pts',(-20.3421751197632,25.8286823194232,-67.7811967726409));
#55384=CARTESIAN_POINT('Ctrl Pts',(-20.4135614955971,25.9260071505859,-67.775109272923));
#55385=CARTESIAN_POINT('Ctrl Pts',(-20.4893085349464,26.0198903287757,-67.7690217732051));
#55386=CARTESIAN_POINT('Ctrl Pts',(-20.5621236239015,26.1101395587127,-67.7631699031217));
#55387=CARTESIAN_POINT('Ctrl Pts',(-20.6389677920425,26.1972082628491,-67.7573180330384));
#55388=CARTESIAN_POINT('Ctrl Pts',(-20.7195257541058,26.2807240863242,-67.751466162955));
#55389=CARTESIAN_POINT('Ctrl Pts',(-20.8000714504867,26.3642271937558,-67.745615183872));
#55390=CARTESIAN_POINT('Ctrl Pts',(-20.8843295295658,26.4441781986792,-67.7397642047891));
#55391=CARTESIAN_POINT('Ctrl Pts',(-20.9719466665354,26.5202403878457,-67.7339132257061));
#55392=CARTESIAN_POINT('Ctrl Pts',(-21.0595716811287,26.5963094157351,-67.7280617205638));
#55393=CARTESIAN_POINT('Ctrl Pts',(-21.150556041801,26.6684886617996,-67.7222102154216));
#55394=CARTESIAN_POINT('Ctrl Pts',(-21.2445126098657,26.7364810879793,-67.7163587102793));
#55395=CARTESIAN_POINT('Ctrl Pts',(-21.3385003788614,26.8044960929636,-67.7105052619795));
#55396=CARTESIAN_POINT('Ctrl Pts',(-21.4354619831323,26.8683212712168,-67.7046518136798));
#55397=CARTESIAN_POINT('Ctrl Pts',(-21.5349811312791,26.9277027804276,-67.69879836538));
#55398=CARTESIAN_POINT('Ctrl Pts',(-21.6346134543076,26.9871518193087,-67.6929382604385));
#55399=CARTESIAN_POINT('Ctrl Pts',(-21.7368087712538,27.0421468907372,-67.687078155497));
#55400=CARTESIAN_POINT('Ctrl Pts',(-21.8411259223268,27.092479971195,-67.6812180505554));
#55401=CARTESIAN_POINT('Ctrl Pts',(-21.945513324472,27.1428469478322,-67.6753539992));
#55402=CARTESIAN_POINT('Ctrl Pts',(-22.0520250270473,27.1885455194192,-67.6694899478446));
#55403=CARTESIAN_POINT('Ctrl Pts',(-22.1602012493755,27.2294163541577,-67.6636258964892));
#55404=CARTESIAN_POINT('Ctrl Pts',(-22.2685369018614,27.270347424348,-67.6577532026926));
#55405=CARTESIAN_POINT('Ctrl Pts',(-22.3785415788432,27.3064364289057,-67.651880508896));
#55406=CARTESIAN_POINT('Ctrl Pts',(-22.4897416834709,27.3375742424551,-67.6460078150995));
#55407=CARTESIAN_POINT('Ctrl Pts',(-22.5201864119694,27.3460992549335,-67.644399969776));
#55408=CARTESIAN_POINT('Ctrl Pts',(-22.5507206982046,27.3542534372032,-67.6427921244526));
#55409=CARTESIAN_POINT('Ctrl Pts',(-22.5813347318949,27.3620352245077,-67.6411842791292));
#55410=CARTESIAN_POINT('Ctrl Pts',(-22.6931456720514,27.3904564695944,-67.6353119821605));
#55411=CARTESIAN_POINT('Ctrl Pts',(-22.8063955057018,27.4140015350489,-67.6294396851918));
#55412=CARTESIAN_POINT('Ctrl Pts',(-22.920620952109,27.4325267458616,-67.6235673882231));
#55413=CARTESIAN_POINT('Ctrl Pts',(-23.0346983714093,27.4510279494723,-67.6177027012849));
#55414=CARTESIAN_POINT('Ctrl Pts',(-23.1497484849095,27.464522169646,-67.6118380143466));
#55415=CARTESIAN_POINT('Ctrl Pts',(-23.2652943008228,27.4729158879687,-67.6059733274084));
#55416=CARTESIAN_POINT('Ctrl Pts',(-23.3807212850978,27.4813009738775,-67.6001146719336));
#55417=CARTESIAN_POINT('Ctrl Pts',(-23.4966425479518,27.484595961827,-67.5942560164588));
#55418=CARTESIAN_POINT('Ctrl Pts',(-23.6125730497049,27.4827587494941,-67.588397360984));
#55419=CARTESIAN_POINT('Ctrl Pts',(-23.7330318989666,27.4808497740293,-67.5823098612661));
#55420=CARTESIAN_POINT('Ctrl Pts',(-23.8535002747853,27.4733994154378,-67.5762223615482));
#55421=CARTESIAN_POINT('Ctrl Pts',(-23.9734302537047,27.4604199981327,-67.5701348618303));
#55422=CARTESIAN_POINT('Ctrl Pts',(-24.0887180875057,27.4479429768025,-67.5642829917469));
#55423=CARTESIAN_POINT('Ctrl Pts',(-24.2035079796918,27.430357014525,-67.5584311216635));
#55424=CARTESIAN_POINT('Ctrl Pts',(-24.3173162368203,27.4077260924951,-67.5525792515801));
#55425=CARTESIAN_POINT('Ctrl Pts',(-24.4311071656067,27.3850986162289,-67.5467282724971));
#55426=CARTESIAN_POINT('Ctrl Pts',(-24.5439163511823,27.3574277881214,-67.5408772934141));
#55427=CARTESIAN_POINT('Ctrl Pts',(-24.6552695240046,27.3248288584765,-67.5350263143312));
#55428=CARTESIAN_POINT('Ctrl Pts',(-24.7666327085487,27.292226997874,-67.5291748091889));
#55429=CARTESIAN_POINT('Ctrl Pts',(-24.8765392233482,27.2546962710756,-67.5233233040466));
#55430=CARTESIAN_POINT('Ctrl Pts',(-24.9845299004276,27.2124018226897,-67.5174717989043));
#55431=CARTESIAN_POINT('Ctrl Pts',(-25.09255643886,27.1700933292383,-67.5116183506045));
#55432=CARTESIAN_POINT('Ctrl Pts',(-25.1986654898017,27.1230181193066,-67.5057649023047));
#55433=CARTESIAN_POINT('Ctrl Pts',(-25.3024184683078,27.071389213303,-67.499911454005));
#55434=CARTESIAN_POINT('Ctrl Pts',(-25.4062894364801,27.0197015940222,-67.4940513490635));
#55435=CARTESIAN_POINT('Ctrl Pts',(-25.5077986139703,26.9634501267305,-67.4881912441219));
#55436=CARTESIAN_POINT('Ctrl Pts',(-25.6065325215332,26.9028935210319,-67.4823311391804));
#55437=CARTESIAN_POINT('Ctrl Pts',(-25.7053329202034,26.8422961342495,-67.476467087825));
#55438=CARTESIAN_POINT('Ctrl Pts',(-25.801353985815,26.7773880670358,-67.4706030364695));
#55439=CARTESIAN_POINT('Ctrl Pts',(-25.8942131389054,26.7084700149974,-67.4647389851141));
#55440=CARTESIAN_POINT('Ctrl Pts',(-25.9872091478511,26.6394503915076,-67.4588662913175));
#55441=CARTESIAN_POINT('Ctrl Pts',(-26.0770336242338,26.5664092479619,-67.4529935975209));
#55442=CARTESIAN_POINT('Ctrl Pts',(-26.1633387598692,26.4896860424446,-67.4471209037243));
#55443=CARTESIAN_POINT('Ctrl Pts',(-26.1869676622981,26.4686805121959,-67.445513058401));
#55444=CARTESIAN_POINT('Ctrl Pts',(-26.2103329888039,26.4473991860725,-67.4439052130776));
#55445=CARTESIAN_POINT('Ctrl Pts',(-26.2334281200576,26.4258494718113,-67.4422973677542));
#55446=CARTESIAN_POINT('Ctrl Pts',(-26.316523802111,26.3483141599345,-67.4365123820655));
#55447=CARTESIAN_POINT('Ctrl Pts',(-26.3964150326815,26.2670252898223,-67.4307273963768));
#55448=CARTESIAN_POINT('Ctrl Pts',(-26.4727356899813,26.1822823927573,-67.424942410688));
#55449=CARTESIAN_POINT('Ctrl Pts',(-26.552870868075,26.0933040297723,-67.4188682903275));
#55450=CARTESIAN_POINT('Ctrl Pts',(-26.629068918564,26.0005176697059,-67.4127941699669));
#55451=CARTESIAN_POINT('Ctrl Pts',(-26.7009452846778,25.9043179887911,-67.4067200496064));
#55452=CARTESIAN_POINT('Ctrl Pts',(-26.7692293025233,25.8129263244166,-67.4009495110341));
#55453=CARTESIAN_POINT('Ctrl Pts',(-26.8336128432904,25.7184546498319,-67.3951789724618));
#55454=CARTESIAN_POINT('Ctrl Pts',(-26.8938048520551,25.6212780943102,-67.3894084338895));
#55455=CARTESIAN_POINT('Ctrl Pts',(-26.953959458448,25.5241619227786,-67.3836414810395));
#55456=CARTESIAN_POINT('Ctrl Pts',(-27.0099274837551,25.4243445712755,-67.3778745281896));
#55457=CARTESIAN_POINT('Ctrl Pts',(-27.0614603196305,25.3222313323392,-67.3721075753396));
#55458=CARTESIAN_POINT('Ctrl Pts',(-27.1129744756948,25.2201551077839,-67.3663427129158));
#55459=CARTESIAN_POINT('Ctrl Pts',(-27.1600564460019,25.1157850305423,-67.360577850492));
#55460=CARTESIAN_POINT('Ctrl Pts',(-27.202503292056,25.0095514672919,-67.3548129880683));
#55461=CARTESIAN_POINT('Ctrl Pts',(-27.2449457395983,24.903328912388,-67.3490487230226));
#55462=CARTESIAN_POINT('Ctrl Pts',(-27.2827538613391,24.7952436522743,-67.3432844579769));
#55463=CARTESIAN_POINT('Ctrl Pts',(-27.3157729852035,24.6857456907238,-67.3375201929312));
#55464=CARTESIAN_POINT('Ctrl Pts',(-27.3488106043595,24.5761863951192,-67.3317526990971));
#55465=CARTESIAN_POINT('Ctrl Pts',(-27.3770537451572,24.4652132267656,-67.3259852052631));
#55466=CARTESIAN_POINT('Ctrl Pts',(-27.4003978176522,24.353290685841,-67.320217711429));
#55467=CARTESIAN_POINT('Ctrl Pts',(-27.4237495032394,24.2413316441459,-67.3144483366694));
#55468=CARTESIAN_POINT('Ctrl Pts',(-27.442198868346,24.1284230341177,-67.3086789619098));
#55469=CARTESIAN_POINT('Ctrl Pts',(-27.4556928575527,24.0150372788176,-67.3029095871502));
#55470=CARTESIAN_POINT('Ctrl Pts',(-27.4692011758476,23.9015311206873,-67.297134085968));
#55471=CARTESIAN_POINT('Ctrl Pts',(-27.4777435827243,23.7875472309409,-67.2913585847858));
#55472=CARTESIAN_POINT('Ctrl Pts',(-27.4813190681306,23.6735606259547,-67.2855830836036));
#55473=CARTESIAN_POINT('Ctrl Pts',(-27.4826438044597,23.6313279835306,-67.2834432297473));
#55474=CARTESIAN_POINT('Ctrl Pts',(-27.4832872255155,23.5890949466114,-67.281303375891));
#55475=CARTESIAN_POINT('Ctrl Pts',(-27.4832510904674,23.5468855318674,-67.2791635220347));
#55476=CARTESIAN_POINT('',(-27.4879913355201,23.552603565581,-66.0291635220347));
#55477=CARTESIAN_POINT('Ctrl Pts',(-27.4853590703307,23.5468837272474,-67.2791635220347));
#55478=CARTESIAN_POINT('Ctrl Pts',(-27.4874959140799,23.3116748807435,-67.2672458334829));
#55479=CARTESIAN_POINT('Ctrl Pts',(-27.3610477196202,21.7703416614824,-67.189032507806));
#55480=CARTESIAN_POINT('Ctrl Pts',(-25.3247553604629,19.2500327067552,-67.0445235450044));
#55481=CARTESIAN_POINT('Ctrl Pts',(-20.8915994482856,19.7328824141667,-66.8456366336297));
#55482=CARTESIAN_POINT('Ctrl Pts',(-18.9015203031529,23.7235715999746,-66.6467497222545));
#55483=CARTESIAN_POINT('Ctrl Pts',(-21.1832319285545,27.554995257066,-66.4478628108798));
#55484=CARTESIAN_POINT('Ctrl Pts',(-25.6400347979899,27.7063998957303,-66.2489758995048));
#55485=CARTESIAN_POINT('Ctrl Pts',(-27.4199713476433,25.1326070363992,-66.1094094698899));
#55486=CARTESIAN_POINT('Ctrl Pts',(-27.4889610422656,23.6900265544838,-66.0361386773998));
#55487=CARTESIAN_POINT('Ctrl Pts',(-27.4879913355201,23.552603565581,-66.0291635220347));
#55488=CARTESIAN_POINT('',(-27.4779966819508,23.5524812139231,-64.7791635220347));
#55489=CARTESIAN_POINT('Ctrl Pts',(-27.4879913355201,23.552603565581,-66.0291635220347));
#55490=CARTESIAN_POINT('Ctrl Pts',(-27.4797444265551,22.3838843787112,-65.9698430402749));
#55491=CARTESIAN_POINT('Ctrl Pts',(-26.3078739937543,19.894666085494,-65.8442269213898));
#55492=CARTESIAN_POINT('Ctrl Pts',(-22.0716745106532,19.1395204079076,-65.6523151653804));
#55493=CARTESIAN_POINT('Ctrl Pts',(-19.0401954898553,22.4100173316296,-65.4534282540051));
#55494=CARTESIAN_POINT('Ctrl Pts',(-20.153076500729,26.7282937282087,-65.2545413426305));
#55495=CARTESIAN_POINT('Ctrl Pts',(-24.3876742510315,28.1262197186492,-65.0556544312555));
#55496=CARTESIAN_POINT('Ctrl Pts',(-27.1484078217908,25.8897972304457,-64.8971951577236));
#55497=CARTESIAN_POINT('Ctrl Pts',(-27.4806287621626,24.0654490020844,-64.8050315213167));
#55498=CARTESIAN_POINT('Ctrl Pts',(-27.4779966819508,23.5524812139231,-64.7791635220347));
#55499=CARTESIAN_POINT('',(-27.4798202215753,23.5470868039979,-63.5291635220347));
#55500=CARTESIAN_POINT('Ctrl Pts',(-27.4779966819508,23.5524812139231,-64.7791635220347));
#55501=CARTESIAN_POINT('Ctrl Pts',(-27.4738831521638,22.7507927749053,-64.7387358841917));
#55502=CARTESIAN_POINT('Ctrl Pts',(-26.8448208971909,20.6285198012337,-64.6320126092237));
#55503=CARTESIAN_POINT('Ctrl Pts',(-23.3709510498503,18.9017472008681,-64.4589936971309));
#55504=CARTESIAN_POINT('Ctrl Pts',(-19.5424669510336,21.1883876812941,-64.2601067857559));
#55505=CARTESIAN_POINT('Ctrl Pts',(-19.3967979966629,25.6453817061212,-64.061219874381));
#55506=CARTESIAN_POINT('Ctrl Pts',(-23.0678016051148,28.1771296573105,-63.8623329630061));
#55507=CARTESIAN_POINT('Ctrl Pts',(-26.7366505891984,26.6434011874026,-63.6849808455575));
#55508=CARTESIAN_POINT('Ctrl Pts',(-27.473158079598,24.4336695320874,-63.5739243652336));
#55509=CARTESIAN_POINT('Ctrl Pts',(-27.4798202215753,23.5470868039979,-63.5291635220347));
#55510=CARTESIAN_POINT('',(-27.4855958674576,23.5492949760936,-62.2791639176179));
#55511=CARTESIAN_POINT('Ctrl Pts',(-27.4798202215753,23.5470868039979,-63.5291635220347));
#55512=CARTESIAN_POINT('Ctrl Pts',(-27.4830254305109,23.1205448762016,-63.5076287281086));
#55513=CARTESIAN_POINT('Ctrl Pts',(-27.2221533585443,21.3846924303558,-63.4197982970575));
#55514=CARTESIAN_POINT('Ctrl Pts',(-24.6846826946482,19.0387318304793,-63.2656722288816));
#55515=CARTESIAN_POINT('Ctrl Pts',(-20.3678420653385,20.157169205907,-63.0667853175066));
#55516=CARTESIAN_POINT('Ctrl Pts',(-18.9753668306978,24.393562471708,-62.8678984061318));
#55517=CARTESIAN_POINT('Ctrl Pts',(-21.786823668931,27.8550254035288,-62.6690114947568));
#55518=CARTESIAN_POINT('Ctrl Pts',(-26.1598424050956,27.3673334894723,-62.4727668831467));
#55519=CARTESIAN_POINT('Ctrl Pts',(-27.4853352952305,24.8021464490294,-62.3428179086613));
#55520=CARTESIAN_POINT('Ctrl Pts',(-27.4894683157168,23.5493068921072,-62.2791645713009));
#55521=CARTESIAN_POINT('',(-27.4832508498222,23.5538897837606,-61.0291635375734));
#55522=CARTESIAN_POINT('Ctrl Pts',(-27.4832524133653,23.5492877649886,-62.2791635220346));
#55523=CARTESIAN_POINT('Ctrl Pts',(-27.4832396780116,23.4973704005476,-62.2765215720254));
#55524=CARTESIAN_POINT('Ctrl Pts',(-27.4821989889277,23.445466886612,-62.2738796220162));
#55525=CARTESIAN_POINT('Ctrl Pts',(-27.480131717455,23.393604565465,-62.271237672007));
#55526=CARTESIAN_POINT('Ctrl Pts',(-27.4755367660139,23.2783295034084,-62.2653653750383));
#55527=CARTESIAN_POINT('Ctrl Pts',(-27.4658577751254,23.1630636712445,-62.2594930780696));
#55528=CARTESIAN_POINT('Ctrl Pts',(-27.4510889429275,23.0482920822599,-62.2536207811009));
#55529=CARTESIAN_POINT('Ctrl Pts',(-27.4363392499632,22.9336692281397,-62.2477560941628));
#55530=CARTESIAN_POINT('Ctrl Pts',(-27.4165128850979,22.8195397496921,-62.2418914072246));
#55531=CARTESIAN_POINT('Ctrl Pts',(-27.39165603088,22.7063875208997,-62.2360267202864));
#55532=CARTESIAN_POINT('Ctrl Pts',(-27.3668247403806,22.5933516620911,-62.2301680648116));
#55533=CARTESIAN_POINT('Ctrl Pts',(-27.3369733391347,22.4812914551893,-62.2243094093368));
#55534=CARTESIAN_POINT('Ctrl Pts',(-27.3021995888,22.3706838475238,-62.218450753862));
#55535=CARTESIAN_POINT('Ctrl Pts',(-27.2660675451487,22.2557558092808,-62.2123632541441));
#55536=CARTESIAN_POINT('Ctrl Pts',(-27.2246208285365,22.1423966142518,-62.2062757544262));
#55537=CARTESIAN_POINT('Ctrl Pts',(-27.1780272809046,22.0311279913778,-62.2001882547082));
#55538=CARTESIAN_POINT('Ctrl Pts',(-27.1332372357135,21.9241662574001,-62.1943363846249));
#55539=CARTESIAN_POINT('Ctrl Pts',(-27.0836915635299,21.8191366816362,-62.1884845145415));
#55540=CARTESIAN_POINT('Ctrl Pts',(-27.0295893341285,21.7164847123599,-62.1826326444581));
#55541=CARTESIAN_POINT('Ctrl Pts',(-26.9754953422835,21.6138483727794,-62.1767816653751));
#55542=CARTESIAN_POINT('Ctrl Pts',(-26.9168463653594,21.51358928549,-62.1709306862922));
#55543=CARTESIAN_POINT('Ctrl Pts',(-26.8538879360401,21.4161292655373,-62.1650797072092));
#55544=CARTESIAN_POINT('Ctrl Pts',(-26.7909238461521,21.3186604829907,-62.1592282020669));
#55545=CARTESIAN_POINT('Ctrl Pts',(-26.7236497579546,21.2239916153172,-62.1533766969246));
#55546=CARTESIAN_POINT('Ctrl Pts',(-26.6523547323724,21.1325157932243,-62.1475251917823));
#55547=CARTESIAN_POINT('Ctrl Pts',(-26.5810360312643,21.0410095940021,-62.1416717434826));
#55548=CARTESIAN_POINT('Ctrl Pts',(-26.5056939916643,20.9526988746596,-62.1358182951828));
#55549=CARTESIAN_POINT('Ctrl Pts',(-26.42665770689,20.8679434018386,-62.129964846883));
#55550=CARTESIAN_POINT('Ctrl Pts',(-26.3475315406976,20.7830915436407,-62.1241047419415));
#55551=CARTESIAN_POINT('Ctrl Pts',(-26.2647030260392,20.701803304352,-62.118244637));
#55552=CARTESIAN_POINT('Ctrl Pts',(-26.178537904666,20.6244013737877,-62.1123845320584));
#55553=CARTESIAN_POINT('Ctrl Pts',(-26.0923147564763,20.5469473178676,-62.106520480703));
#55554=CARTESIAN_POINT('Ctrl Pts',(-26.0027508460223,20.4733850437404,-62.1006564293475));
#55555=CARTESIAN_POINT('Ctrl Pts',(-25.9102433636795,20.4039956647259,-62.0947923779921));
#55556=CARTESIAN_POINT('Ctrl Pts',(-25.8175995437741,20.3345040196182,-62.0889196841955));
#55557=CARTESIAN_POINT('Ctrl Pts',(-25.7220038337499,20.2691977761741,-62.083046990399));
#55558=CARTESIAN_POINT('Ctrl Pts',(-25.6238806800869,20.2083136779458,-62.0771742966024));
#55559=CARTESIAN_POINT('Ctrl Pts',(-25.5970162020123,20.1916446303164,-62.075566451279));
#55560=CARTESIAN_POINT('Ctrl Pts',(-25.5699624029027,20.1753067822909,-62.0739586059556));
#55561=CARTESIAN_POINT('Ctrl Pts',(-25.5427282687353,20.1593043697043,-62.0723507606321));
#55562=CARTESIAN_POINT('Ctrl Pts',(-25.443261658866,20.1008591215487,-62.0664784636635));
#55563=CARTESIAN_POINT('Ctrl Pts',(-25.3410546754112,20.0466961502296,-62.0606061666948));
#55564=CARTESIAN_POINT('Ctrl Pts',(-25.2365122320342,19.9970825071936,-62.0547338697261));
#55565=CARTESIAN_POINT('Ctrl Pts',(-25.1321052673613,19.9475331594989,-62.0488691827879));
#55566=CARTESIAN_POINT('Ctrl Pts',(-25.025369231542,19.9025215915189,-62.0430044958497));
#55567=CARTESIAN_POINT('Ctrl Pts',(-24.9167361795013,19.862270503501,-62.0371398089115));
#55568=CARTESIAN_POINT('Ctrl Pts',(-24.8082148497541,19.8220608112075,-62.0312811534367));
#55569=CARTESIAN_POINT('Ctrl Pts',(-24.6978007696496,19.7866020035299,-62.0254224979619));
#55570=CARTESIAN_POINT('Ctrl Pts',(-24.585948047299,19.7560696421966,-62.0195638424871));
#55571=CARTESIAN_POINT('Ctrl Pts',(-24.4697262590945,19.724344659937,-62.0134763427692));
#55572=CARTESIAN_POINT('Ctrl Pts',(-24.3519515589681,19.6979390274756,-62.0073888430513));
#55573=CARTESIAN_POINT('Ctrl Pts',(-24.233153611916,19.6769935531812,-62.0013013433334));
#55574=CARTESIAN_POINT('Ctrl Pts',(-24.1189539922797,19.6568588180542,-61.99544947325));
#55575=CARTESIAN_POINT('Ctrl Pts',(-24.0038093117721,19.6417694851315,-61.9895976031666));
#55576=CARTESIAN_POINT('Ctrl Pts',(-23.8882019391522,19.6317988573478,-61.9837457330832));
#55577=CARTESIAN_POINT('Ctrl Pts',(-23.772612168806,19.6218297476828,-61.9778947540003));
#55578=CARTESIAN_POINT('Ctrl Pts',(-23.6565602581637,19.6169778290317,-61.9720437749174));
#55579=CARTESIAN_POINT('Ctrl Pts',(-23.5405338081249,19.6172645395422,-61.9661927958344));
#55580=CARTESIAN_POINT('Ctrl Pts',(-23.4244969261917,19.6175512758306,-61.9603412906921));
#55581=CARTESIAN_POINT('Ctrl Pts',(-23.3084859228187,19.6229775586966,-61.9544897855499));
#55582=CARTESIAN_POINT('Ctrl Pts',(-23.1929877951504,19.6335127001478,-61.9486382804076));
#55583=CARTESIAN_POINT('Ctrl Pts',(-23.0774513130683,19.6440513400901,-61.9427848321078));
#55584=CARTESIAN_POINT('Ctrl Pts',(-22.9624284568071,19.659702174551,-61.9369313838081));
#55585=CARTESIAN_POINT('Ctrl Pts',(-22.8483997929683,19.6803828009225,-61.9310779355084));
#55586=CARTESIAN_POINT('Ctrl Pts',(-22.7342414537779,19.7010869456569,-61.9252178305668));
#55587=CARTESIAN_POINT('Ctrl Pts',(-22.6210799706674,19.7268322253675,-61.9193577256253));
#55588=CARTESIAN_POINT('Ctrl Pts',(-22.509384526914,19.7574853629077,-61.9134976206838));
#55589=CARTESIAN_POINT('Ctrl Pts',(-22.3976138632701,19.7881591434174,-61.9076335693284));
#55590=CARTESIAN_POINT('Ctrl Pts',(-22.287311597317,19.8237472363157,-61.9017695179729));
#55591=CARTESIAN_POINT('Ctrl Pts',(-22.1789289326433,19.864067432342,-61.8959054666175));
#55592=CARTESIAN_POINT('Ctrl Pts',(-22.070386533557,19.9044470522886,-61.890032772821));
#55593=CARTESIAN_POINT('Ctrl Pts',(-21.9637697613652,19.9495725339506,-61.8841600790244));
#55594=CARTESIAN_POINT('Ctrl Pts',(-21.8595072237068,19.9992147533091,-61.8782873852279));
#55595=CARTESIAN_POINT('Ctrl Pts',(-21.8309618849919,20.012805962558,-61.8766795399044));
#55596=CARTESIAN_POINT('Ctrl Pts',(-21.8025928540155,20.0267354781966,-61.8750716945809));
#55597=CARTESIAN_POINT('Ctrl Pts',(-21.7744085517583,20.0409980298199,-61.8734638492574));
#55598=CARTESIAN_POINT('Ctrl Pts',(-21.6714716645523,20.0930888232805,-61.8675915522886));
#55599=CARTESIAN_POINT('Ctrl Pts',(-21.5706562406025,20.1497998911861,-61.8617192553199));
#55600=CARTESIAN_POINT('Ctrl Pts',(-21.472405827772,20.2109349255058,-61.8558469583512));
#55601=CARTESIAN_POINT('Ctrl Pts',(-21.3742827396737,20.2719907336763,-61.849982271413));
#55602=CARTESIAN_POINT('Ctrl Pts',(-21.2787184000945,20.337458890786,-61.8441175844748));
#55603=CARTESIAN_POINT('Ctrl Pts',(-21.1861337144921,20.407096280702,-61.8382528975366));
#55604=CARTESIAN_POINT('Ctrl Pts',(-21.093644246443,20.4766620529219,-61.8323942420617));
#55605=CARTESIAN_POINT('Ctrl Pts',(-21.0041286655255,20.5503882823135,-61.8265355865869));
#55606=CARTESIAN_POINT('Ctrl Pts',(-20.9179801394522,20.6279878186607,-61.8206769311121));
#55607=CARTESIAN_POINT('Ctrl Pts',(-20.828466576072,20.7086184612463,-61.8145894313942));
#55608=CARTESIAN_POINT('Ctrl Pts',(-20.7425888561999,20.7934309287559,-61.8085019316763));
#55609=CARTESIAN_POINT('Ctrl Pts',(-20.6607517506638,20.8820557180343,-61.8024144319584));
#55610=CARTESIAN_POINT('Ctrl Pts',(-20.5820823244967,20.9672500961961,-61.796562561875));
#55611=CARTESIAN_POINT('Ctrl Pts',(-20.5071468343922,21.0559668237066,-61.7907106917916));
#55612=CARTESIAN_POINT('Ctrl Pts',(-20.4362676921025,21.1478396989793,-61.7848588217081));
#55613=CARTESIAN_POINT('Ctrl Pts',(-20.3653993418067,21.2396985857713,-61.7790078426252));
#55614=CARTESIAN_POINT('Ctrl Pts',(-20.2985863637469,21.3347123376244,-61.7731568635422));
#55615=CARTESIAN_POINT('Ctrl Pts',(-20.2361103631534,21.4324823159484,-61.7673058844592));
#55616=CARTESIAN_POINT('Ctrl Pts',(-20.1736287453662,21.5302610847344,-61.7614543793169));
#55617=CARTESIAN_POINT('Ctrl Pts',(-20.1154851028063,21.6307962242594,-61.7556028741746));
#55618=CARTESIAN_POINT('Ctrl Pts',(-20.0619168597525,21.7336614274942,-61.7497513690323));
#55619=CARTESIAN_POINT('Ctrl Pts',(-20.0083308278512,21.8365607900236,-61.7438979207325));
#55620=CARTESIAN_POINT('Ctrl Pts',(-19.9593234075026,21.9417913883908,-61.7380444724327));
#55621=CARTESIAN_POINT('Ctrl Pts',(-19.9150850386307,22.0489043717478,-61.732191024133));
#55622=CARTESIAN_POINT('Ctrl Pts',(-19.8707963611272,22.156139165826,-61.7263309191914));
#55623=CARTESIAN_POINT('Ctrl Pts',(-19.8312877180315,22.2652602353222,-61.7204708142499));
#55624=CARTESIAN_POINT('Ctrl Pts',(-19.7967005944955,22.3758008065254,-61.7146107093083));
#55625=CARTESIAN_POINT('Ctrl Pts',(-19.7620901786965,22.4864158198849,-61.7087466579529));
#55626=CARTESIAN_POINT('Ctrl Pts',(-19.7324079875653,22.5984518398084,-61.7028826065974));
#55627=CARTESIAN_POINT('Ctrl Pts',(-19.7077446200612,22.7114307693167,-61.6970185552419));
#55628=CARTESIAN_POINT('Ctrl Pts',(-19.6830449036768,22.8245762072145,-61.6911458614454));
#55629=CARTESIAN_POINT('Ctrl Pts',(-19.6633788433503,22.9386669223457,-61.6852731676488));
#55630=CARTESIAN_POINT('Ctrl Pts',(-19.6487853537993,23.0532184686673,-61.6794004738522));
#55631=CARTESIAN_POINT('Ctrl Pts',(-19.6447899004797,23.0845807658353,-61.6777926285289));
#55632=CARTESIAN_POINT('Ctrl Pts',(-19.6411743718086,23.1159776012902,-61.6761847832057));
#55633=CARTESIAN_POINT('Ctrl Pts',(-19.6379388856029,23.1473990414423,-61.6745769378824));
#55634=CARTESIAN_POINT('Ctrl Pts',(-19.6261219927944,23.2621588539,-61.6687046409137));
#55635=CARTESIAN_POINT('Ctrl Pts',(-19.6193389552216,23.3776312979306,-61.662832343945));
#55636=CARTESIAN_POINT('Ctrl Pts',(-19.617664372068,23.4933370964622,-61.6569600469763));
#55637=CARTESIAN_POINT('Ctrl Pts',(-19.6159919590411,23.6088929494682,-61.6510953600381));
#55638=CARTESIAN_POINT('Ctrl Pts',(-19.6194148412559,23.7246811460681,-61.6452306730999));
#55639=CARTESIAN_POINT('Ctrl Pts',(-19.6279559982741,23.840216156862,-61.6393659861617));
#55640=CARTESIAN_POINT('Ctrl Pts',(-19.6364883712469,23.9556323471299,-61.6335073306869));
#55641=CARTESIAN_POINT('Ctrl Pts',(-19.6501285187102,24.070795459733,-61.6276486752121));
#55642=CARTESIAN_POINT('Ctrl Pts',(-19.6688473801853,24.1852194992131,-61.6217900197373));
#55643=CARTESIAN_POINT('Ctrl Pts',(-19.688297416877,24.3041130424587,-61.6157025200194));
#55644=CARTESIAN_POINT('Ctrl Pts',(-19.7132310205916,24.4222081432094,-61.6096150203014));
#55645=CARTESIAN_POINT('Ctrl Pts',(-19.7435561179166,24.5389645288567,-61.6035275205835));
#55646=CARTESIAN_POINT('Ctrl Pts',(-19.7727074177994,24.6512016100684,-61.5976756505001));
#55647=CARTESIAN_POINT('Ctrl Pts',(-19.8068404800227,24.7622012473678,-61.5918237804167));
#55648=CARTESIAN_POINT('Ctrl Pts',(-19.8458214902675,24.8714942428562,-61.5859719103333));
#55649=CARTESIAN_POINT('Ctrl Pts',(-19.8847965652991,24.9807705974923,-61.5801209312504));
#55650=CARTESIAN_POINT('Ctrl Pts',(-19.9286179818527,25.088340437734,-61.5742699521674));
#55651=CARTESIAN_POINT('Ctrl Pts',(-19.9771025781589,25.1937513633187,-61.5684189730844));
#55652=CARTESIAN_POINT('Ctrl Pts',(-20.025591533697,25.29917176636,-61.5625674679421));
#55653=CARTESIAN_POINT('Ctrl Pts',(-20.0787443296951,25.4024324932943,-61.5567159627998));
#55654=CARTESIAN_POINT('Ctrl Pts',(-20.1363306447845,25.5031033580705,-61.5508644576575));
#55655=CARTESIAN_POINT('Ctrl Pts',(-20.1939360830355,25.6038076534493,-61.5450110093578));
#55656=CARTESIAN_POINT('Ctrl Pts',(-20.2559777627562,25.7019200179063,-61.539157561058));
#55657=CARTESIAN_POINT('Ctrl Pts',(-20.3221809990495,25.7970376082266,-61.5333041127582));
#55658=CARTESIAN_POINT('Ctrl Pts',(-20.3884595227982,25.8922633679015,-61.5274440078167));
#55659=CARTESIAN_POINT('Ctrl Pts',(-20.458908812942,25.9844872162568,-61.5215839028751));
#55660=CARTESIAN_POINT('Ctrl Pts',(-20.5332126436486,26.0733378084817,-61.5157237979336));
#55661=CARTESIAN_POINT('Ctrl Pts',(-20.6075665133347,26.1622482360195,-61.5098597465782));
#55662=CARTESIAN_POINT('Ctrl Pts',(-20.6857798140403,26.2477805797459,-61.5039956952227));
#55663=CARTESIAN_POINT('Ctrl Pts',(-20.7674992873335,26.3296001855512,-61.4981316438673));
#55664=CARTESIAN_POINT('Ctrl Pts',(-20.8493391988177,26.4115403771226,-61.4922589500707));
#55665=CARTESIAN_POINT('Ctrl Pts',(-20.9346952923896,26.4897566318144,-61.4863862562741));
#55666=CARTESIAN_POINT('Ctrl Pts',(-21.0231810305196,26.5639543463983,-61.4805135624776));
#55667=CARTESIAN_POINT('Ctrl Pts',(-21.0474069454341,26.5842684394754,-61.4789057171542));
#55668=CARTESIAN_POINT('Ctrl Pts',(-21.0718672833677,26.6042815649795,-61.4772978718309));
#55669=CARTESIAN_POINT('Ctrl Pts',(-21.0965537507095,26.6239882542628,-61.4756900265075));
#55670=CARTESIAN_POINT('Ctrl Pts',(-21.186715574882,26.6959625480965,-61.4698177295388));
#55671=CARTESIAN_POINT('Ctrl Pts',(-21.2801979601086,26.7640869826368,-61.4639454325701));
#55672=CARTESIAN_POINT('Ctrl Pts',(-21.3766380065686,26.8280397267639,-61.4580731356014));
#55673=CARTESIAN_POINT('Ctrl Pts',(-21.4729530743875,26.8919095932136,-61.4522084486632));
#55674=CARTESIAN_POINT('Ctrl Pts',(-21.5722178398534,26.9516182938486,-61.446343761725));
#55675=CARTESIAN_POINT('Ctrl Pts',(-21.6740362403629,27.0068840463545,-61.4404790747868));
#55676=CARTESIAN_POINT('Ctrl Pts',(-21.7757499270213,27.0620929614936,-61.434620419312));
#55677=CARTESIAN_POINT('Ctrl Pts',(-21.8800116638402,27.1128678210478,-61.4287617638371));
#55678=CARTESIAN_POINT('Ctrl Pts',(-21.9863968662657,27.1589703729374,-61.4229031083623));
#55679=CARTESIAN_POINT('Ctrl Pts',(-22.0969375684009,27.2068737311105,-61.4168156086444));
#55680=CARTESIAN_POINT('Ctrl Pts',(-22.2097706279095,27.2497320803257,-61.4107281089265));
#55681=CARTESIAN_POINT('Ctrl Pts',(-22.3243917347984,27.2873308432411,-61.4046406092086));
#55682=CARTESIAN_POINT('Ctrl Pts',(-22.4345761877612,27.3234742660046,-61.3987887391252));
#55683=CARTESIAN_POINT('Ctrl Pts',(-22.5464124121354,27.3547575576321,-61.3929368690418));
#55684=CARTESIAN_POINT('Ctrl Pts',(-22.6594333315443,27.3810396770005,-61.3870849989584));
#55685=CARTESIAN_POINT('Ctrl Pts',(-22.7724370424906,27.4073177946773,-61.3812340198754));
#55686=CARTESIAN_POINT('Ctrl Pts',(-22.8866246872882,27.4285961605441,-61.3753830407925));
#55687=CARTESIAN_POINT('Ctrl Pts',(-23.0015166473045,27.44478433015,-61.3695320617095));
#55688=CARTESIAN_POINT('Ctrl Pts',(-23.1164189372138,27.4609739552281,-61.3636805565672));
#55689=CARTESIAN_POINT('Ctrl Pts',(-23.2320252588615,27.4720724165851,-61.3578290514249));
#55690=CARTESIAN_POINT('Ctrl Pts',(-23.3478491910413,27.4780409536554,-61.3519775462826));
#55691=CARTESIAN_POINT('Ctrl Pts',(-23.4637115858275,27.4840114727469,-61.3461240979828));
#55692=CARTESIAN_POINT('Ctrl Pts',(-23.5797913222211,27.4848486589147,-61.3402706496831));
#55693=CARTESIAN_POINT('Ctrl Pts',(-23.6956010026349,27.4805658553359,-61.3344172013833));
#55694=CARTESIAN_POINT('Ctrl Pts',(-23.8115423838029,27.4762781812794,-61.3285570964417));
#55695=CARTESIAN_POINT('Ctrl Pts',(-23.9272126826588,27.4668589111484,-61.3226969915002));
#55696=CARTESIAN_POINT('Ctrl Pts',(-24.0421285471146,27.4523733634284,-61.3168368865587));
#55697=CARTESIAN_POINT('Ctrl Pts',(-24.1571218002129,27.4378780605987,-61.3109728352032));
#55698=CARTESIAN_POINT('Ctrl Pts',(-24.2713592008013,27.4183097561906,-61.3051087838478));
#55699=CARTESIAN_POINT('Ctrl Pts',(-24.3843682476043,27.3937847577165,-61.2992447324923));
#55700=CARTESIAN_POINT('Ctrl Pts',(-24.4975438471834,27.3692236142903,-61.2933720386958));
#55701=CARTESIAN_POINT('Ctrl Pts',(-24.6094870816644,27.3396913021259,-61.2874993448992));
#55702=CARTESIAN_POINT('Ctrl Pts',(-24.7197411564874,27.3053537761987,-61.2816266511026));
#55703=CARTESIAN_POINT('Ctrl Pts',(-24.7499268778493,27.2959527359962,-61.2800188057793));
#55704=CARTESIAN_POINT('Ctrl Pts',(-24.7799861057219,27.2861917860426,-61.2784109604559));
#55705=CARTESIAN_POINT('Ctrl Pts',(-24.8099097561921,27.2760749478555,-61.2768031151325));
#55706=CARTESIAN_POINT('Ctrl Pts',(-24.9191992253931,27.2391254494459,-61.2709308181638));
#55707=CARTESIAN_POINT('Ctrl Pts',(-25.0270446473952,27.1973012951529,-61.2650585211951));
#55708=CARTESIAN_POINT('Ctrl Pts',(-25.1329790975397,27.1507338353211,-61.2591862242264));
#55709=CARTESIAN_POINT('Ctrl Pts',(-25.2387762650499,27.1042267232189,-61.2533215372882));
#55710=CARTESIAN_POINT('Ctrl Pts',(-25.3426670105679,27.0529886944684,-61.24745685035));
#55711=CARTESIAN_POINT('Ctrl Pts',(-25.4442001772773,26.9972006478964,-61.2415921634118));
#55712=CARTESIAN_POINT('Ctrl Pts',(-25.545628923481,26.9414699758379,-61.235733507937));
#55713=CARTESIAN_POINT('Ctrl Pts',(-25.6447045534566,26.881198791411,-61.2298748524622));
#55714=CARTESIAN_POINT('Ctrl Pts',(-25.7409971157814,26.8166155193753,-61.2240161969873));
#55715=CARTESIAN_POINT('Ctrl Pts',(-25.8410509504038,26.7495095678497,-61.2179286972694));
#55716=CARTESIAN_POINT('Ctrl Pts',(-25.9380994506838,26.6777479763894,-61.2118411975515));
#55717=CARTESIAN_POINT('Ctrl Pts',(-26.0316894881728,26.601639041303,-61.2057536978336));
#55718=CARTESIAN_POINT('Ctrl Pts',(-26.1216569240439,26.5284760645554,-61.1999018277502));
#55719=CARTESIAN_POINT('Ctrl Pts',(-26.2084283025172,26.4512963178911,-61.1940499576668));
#55720=CARTESIAN_POINT('Ctrl Pts',(-26.2916324887472,26.3704165217962,-61.1881980875835));
#55721=CARTESIAN_POINT('Ctrl Pts',(-26.3748240063832,26.2895490403857,-61.1823471085005));
#55722=CARTESIAN_POINT('Ctrl Pts',(-26.4544491153716,26.2049829177538,-61.1764961294175));
#55723=CARTESIAN_POINT('Ctrl Pts',(-26.5301724690748,26.1170727760435,-61.1706451503346));
#55724=CARTESIAN_POINT('Ctrl Pts',(-26.6059026310362,26.0291547303655,-61.1647936451923));
#55725=CARTESIAN_POINT('Ctrl Pts',(-26.677730070539,25.9378923811526,-61.15894214005));
#55726=CARTESIAN_POINT('Ctrl Pts',(-26.7453592463859,25.843674010998,-61.1530906349077));
#55727=CARTESIAN_POINT('Ctrl Pts',(-26.81301088041,25.7494243529736,-61.1472371866079));
#55728=CARTESIAN_POINT('Ctrl Pts',(-26.8764612376695,25.6522170577456,-61.1413837383082));
#55729=CARTESIAN_POINT('Ctrl Pts',(-26.9354580849452,25.5524693936347,-61.1355302900084));
#55730=CARTESIAN_POINT('Ctrl Pts',(-26.9945220244471,25.4526082947699,-61.1296701850669));
#55731=CARTESIAN_POINT('Ctrl Pts',(-27.0491221345907,25.3502014167806,-61.1238100801253));
#55732=CARTESIAN_POINT('Ctrl Pts',(-27.0990520966194,25.2456907192984,-61.1179499751838));
#55733=CARTESIAN_POINT('Ctrl Pts',(-27.1490156833525,25.1411096404028,-61.1120859238284));
#55734=CARTESIAN_POINT('Ctrl Pts',(-27.1943026984173,25.0344223004926,-61.1062218724729));
#55735=CARTESIAN_POINT('Ctrl Pts',(-27.234755586305,24.92608909196,-61.1003578211175));
#55736=CARTESIAN_POINT('Ctrl Pts',(-27.2752680936743,24.8175962219032,-61.0944851273209));
#55737=CARTESIAN_POINT('Ctrl Pts',(-27.3109321277976,24.7074530338344,-61.0886124335244));
#55738=CARTESIAN_POINT('Ctrl Pts',(-27.3416403925553,24.5961335423809,-61.0827397397278));
#55739=CARTESIAN_POINT('Ctrl Pts',(-27.3500478017595,24.5656561277684,-61.0811318944044));
#55740=CARTESIAN_POINT('Ctrl Pts',(-27.358084037758,24.5350905877725,-61.0795240490811));
#55741=CARTESIAN_POINT('Ctrl Pts',(-27.365747573681,24.5044467386427,-61.0779162037578));
#55742=CARTESIAN_POINT('Ctrl Pts',(-27.4044761963103,24.3495842729633,-61.0697907593937));
#55743=CARTESIAN_POINT('Ctrl Pts',(-27.4337921536769,24.1922805254554,-61.0616653150297));
#55744=CARTESIAN_POINT('Ctrl Pts',(-27.4534487225508,24.0335210861051,-61.0535398706656));
#55745=CARTESIAN_POINT('Ctrl Pts',(-27.4717796892775,23.8854680856582,-61.0459623910336));
#55746=CARTESIAN_POINT('Ctrl Pts',(-27.4817105553438,23.736148950333,-61.0383849114016));
#55747=CARTESIAN_POINT('Ctrl Pts',(-27.4830865394795,23.586386549012,-61.0308074317696));
#55748=CARTESIAN_POINT('Ctrl Pts',(-27.4831860436438,23.575556494944,-61.0302594670376));
#55749=CARTESIAN_POINT('Ctrl Pts',(-27.4832408301729,23.564724134297,-61.0297115023055));
#55750=CARTESIAN_POINT('Ctrl Pts',(-27.4832508498222,23.5538897837606,-61.0291635375734));
#55751=CARTESIAN_POINT('',(-27.4768264258044,23.5495998111571,-59.7791635220347));
#55752=CARTESIAN_POINT('Ctrl Pts',(-27.4827541867016,23.5538890172514,-61.0291635220347));
#55753=CARTESIAN_POINT('Ctrl Pts',(-27.4736971142189,22.5645208266935,-60.9791187788174));
#55754=CARTESIAN_POINT('Ctrl Pts',(-26.5929390169561,20.2501455696673,-60.8627783984751));
#55755=CARTESIAN_POINT('Ctrl Pts',(-22.7010557676678,18.9764558934434,-60.680142381008));
#55756=CARTESIAN_POINT('Ctrl Pts',(-19.2432138286812,21.7923650373258,-60.481255469633));
#55757=CARTESIAN_POINT('Ctrl Pts',(-19.7431752811021,26.223623744252,-60.2823685582583));
#55758=CARTESIAN_POINT('Ctrl Pts',(-23.7415179398966,28.1982809713375,-60.0834816468832));
#55759=CARTESIAN_POINT('Ctrl Pts',(-26.9653676070822,26.2614956795997,-59.9157466348087));
#55760=CARTESIAN_POINT('Ctrl Pts',(-27.4757968990708,24.247026390915,-59.8143072598592));
#55761=CARTESIAN_POINT('Ctrl Pts',(-27.4768264258044,23.5495998111571,-59.7791635220347));
#55762=CARTESIAN_POINT('',(-27.4834398043345,23.546843952154,-58.5291636146978));
#55763=CARTESIAN_POINT('Ctrl Pts',(-27.4768264258044,23.5495998111571,-59.7791635220347));
#55764=CARTESIAN_POINT('Ctrl Pts',(-27.4777390126582,22.9313911649828,-59.7480116227343));
#55765=CARTESIAN_POINT('Ctrl Pts',(-27.0484773771044,20.9987458094278,-59.6505640863089));
#55766=CARTESIAN_POINT('Ctrl Pts',(-24.0207930075597,18.9221489791923,-59.4868209127587));
#55767=CARTESIAN_POINT('Ctrl Pts',(-19.9108984363416,20.6526927651409,-59.2879340013836));
#55768=CARTESIAN_POINT('Ctrl Pts',(-19.1452617124101,25.0458483039971,-59.0890470900089));
#55769=CARTESIAN_POINT('Ctrl Pts',(-22.4274380697694,28.0646781337172,-58.8901601786339));
#55770=CARTESIAN_POINT('Ctrl Pts',(-26.4754744607769,27.0047585962735,-58.7035326345686));
#55771=CARTESIAN_POINT('Ctrl Pts',(-27.475398742621,24.6134662246994,-58.5832007276283));
#55772=CARTESIAN_POINT('Ctrl Pts',(-27.4851571966465,23.5468591049139,-58.5291644578129));
#55773=CARTESIAN_POINT('',(-27.4849330916743,23.5524945914181,-57.2791629100328));
#55774=CARTESIAN_POINT('Ctrl Pts',(-27.483251053208,23.54684228678,-58.5291635220347));
#55775=CARTESIAN_POINT('Ctrl Pts',(-27.4831007264043,23.3734720123943,-58.5203759322785));
#55776=CARTESIAN_POINT('Ctrl Pts',(-27.4714837675545,23.2005800536994,-58.5115883425223));
#55777=CARTESIAN_POINT('Ctrl Pts',(-27.4486073494167,23.0293699008261,-58.502800752766));
#55778=CARTESIAN_POINT('Ctrl Pts',(-27.4395702071008,22.9617347269926,-58.4993292871387));
#55779=CARTESIAN_POINT('Ctrl Pts',(-27.4287763948297,22.8943616140389,-58.4958578215115));
#55780=CARTESIAN_POINT('Ctrl Pts',(-27.4162404617435,22.827323541604,-58.4923863558842));
#55781=CARTESIAN_POINT('Ctrl Pts',(-27.3950348011478,22.7139226003837,-58.4865140589155));
#55782=CARTESIAN_POINT('Ctrl Pts',(-27.3687998039024,22.6012655107326,-58.4806417619468));
#55783=CARTESIAN_POINT('Ctrl Pts',(-27.3375998206115,22.4898330330376,-58.4747694649781));
#55784=CARTESIAN_POINT('Ctrl Pts',(-27.306440270021,22.378544962984,-58.4689047780399));
#55785=CARTESIAN_POINT('Ctrl Pts',(-27.2703286391819,22.268478743313,-58.4630400911017));
#55786=CARTESIAN_POINT('Ctrl Pts',(-27.2293805527643,22.1601064945539,-58.4571754041635));
#55787=CARTESIAN_POINT('Ctrl Pts',(-27.1884745788902,22.0518456998686,-58.4513167486887));
#55788=CARTESIAN_POINT('Ctrl Pts',(-27.1427421881976,21.9452757952577,-58.4454580932138));
#55789=CARTESIAN_POINT('Ctrl Pts',(-27.092349042018,21.8408545933686,-58.439599437739));
#55790=CARTESIAN_POINT('Ctrl Pts',(-27.0399874951629,21.7323546073606,-58.4335119380211));
#55791=CARTESIAN_POINT('Ctrl Pts',(-26.9825937862766,21.626175044375,-58.4274244383032));
#55792=CARTESIAN_POINT('Ctrl Pts',(-26.9204093929195,21.5228079009493,-58.4213369385853));
#55793=CARTESIAN_POINT('Ctrl Pts',(-26.8606319788736,21.4234418028384,-58.4154850685019));
#55794=CARTESIAN_POINT('Ctrl Pts',(-26.7964280846312,21.3266748385302,-58.4096331984185));
#55795=CARTESIAN_POINT('Ctrl Pts',(-26.7280590640968,21.2329190117581,-58.4037813283351));
#55796=CARTESIAN_POINT('Ctrl Pts',(-26.6597004533674,21.1391774601632,-58.3979303492521));
#55797=CARTESIAN_POINT('Ctrl Pts',(-26.587178220795,21.0484464684288,-58.3920793701691));
#55798=CARTESIAN_POINT('Ctrl Pts',(-26.5107962801063,20.9611079405718,-58.3862283910862));
#55799=CARTESIAN_POINT('Ctrl Pts',(-26.434407471946,20.8737615601406,-58.3803768859439));
#55800=CARTESIAN_POINT('Ctrl Pts',(-26.3541585379674,20.7898085611189,-58.3745253808016));
#55801=CARTESIAN_POINT('Ctrl Pts',(-26.2703923178979,20.7095961738234,-58.3686738756593));
#55802=CARTESIAN_POINT('Ctrl Pts',(-26.1865982808901,20.6293571497402,-58.3628204273595));
#55803=CARTESIAN_POINT('Ctrl Pts',(-26.0992849336816,20.5528614931237,-58.3569669790597));
#55804=CARTESIAN_POINT('Ctrl Pts',(-26.0088299065595,20.4804176351891,-58.3511135307599));
#55805=CARTESIAN_POINT('Ctrl Pts',(-25.9182720124298,20.4078913928573,-58.3452534258184));
#55806=CARTESIAN_POINT('Ctrl Pts',(-25.8245656300914,20.3394264047519,-58.3393933208768));
#55807=CARTESIAN_POINT('Ctrl Pts',(-25.7281192954062,20.2752891182316,-58.3335332159353));
#55808=CARTESIAN_POINT('Ctrl Pts',(-25.631608010151,20.2111086392631,-58.3276691645798));
#55809=CARTESIAN_POINT('Ctrl Pts',(-25.5323534515609,20.1512618780335,-58.3218051132244));
#55810=CARTESIAN_POINT('Ctrl Pts',(-25.4307892655792,20.0959695970594,-58.3159410618689));
#55811=CARTESIAN_POINT('Ctrl Pts',(-25.3290753942615,20.0405958263006,-58.3100683680724));
#55812=CARTESIAN_POINT('Ctrl Pts',(-25.2250454720223,19.9897901131692,-58.3041956742758));
#55813=CARTESIAN_POINT('Ctrl Pts',(-25.1191537027079,19.943725377271,-58.2983229804792));
#55814=CARTESIAN_POINT('Ctrl Pts',(-25.0901623076226,19.931113623151,-58.2967151351559));
#55815=CARTESIAN_POINT('Ctrl Pts',(-25.0610314420914,19.918856951594,-58.2951072898326));
#55816=CARTESIAN_POINT('Ctrl Pts',(-25.0317706099032,19.9069582553641,-58.2934994445092));
#55817=CARTESIAN_POINT('Ctrl Pts',(-24.9249019368617,19.8635009172803,-58.2876271475405));
#55818=CARTESIAN_POINT('Ctrl Pts',(-24.8159405089581,19.8246769278107,-58.2817548505718));
#55819=CARTESIAN_POINT('Ctrl Pts',(-24.7053255822017,19.7906920190822,-58.2758825536031));
#55820=CARTESIAN_POINT('Ctrl Pts',(-24.5948540036055,19.7567511520964,-58.2700178666649));
#55821=CARTESIAN_POINT('Ctrl Pts',(-24.4827335789287,19.7276370152407,-58.2641531797267));
#55822=CARTESIAN_POINT('Ctrl Pts',(-24.36942401113,19.703507532701,-58.2582884927885));
#55823=CARTESIAN_POINT('Ctrl Pts',(-24.2562309751285,19.6794028658236,-58.2524298373136));
#55824=CARTESIAN_POINT('Ctrl Pts',(-24.14185163042,19.6602727421615,-58.2465711818388));
#55825=CARTESIAN_POINT('Ctrl Pts',(-24.0267606894386,19.646225255201,-58.240712526364));
#55826=CARTESIAN_POINT('Ctrl Pts',(-23.9071741949318,19.6316290610269,-58.2346250266461));
#55827=CARTESIAN_POINT('Ctrl Pts',(-23.7868198143401,19.6225207962139,-58.2285375269282));
#55828=CARTESIAN_POINT('Ctrl Pts',(-23.6662420014635,19.6189632466247,-58.2224500272103));
#55829=CARTESIAN_POINT('Ctrl Pts',(-23.5503314094976,19.6155433995648,-58.2165981571269));
#55830=CARTESIAN_POINT('Ctrl Pts',(-23.4342148122107,19.6172525665684,-58.2107462870435));
#55831=CARTESIAN_POINT('Ctrl Pts',(-23.3183801081215,19.6240935716944,-58.2048944169601));
#55832=CARTESIAN_POINT('Ctrl Pts',(-23.2025630409193,19.6309335352152,-58.1990434378771));
#55833=CARTESIAN_POINT('Ctrl Pts',(-23.087028194125,19.6429037588822,-58.1931924587941));
#55834=CARTESIAN_POINT('Ctrl Pts',(-22.9722611482489,19.659954990289,-58.1873414797112));
#55835=CARTESIAN_POINT('Ctrl Pts',(-22.8574837837109,19.6770077547657,-58.1814899745689));
#55836=CARTESIAN_POINT('Ctrl Pts',(-22.7434747662406,19.6991423743668,-58.1756384694266));
#55837=CARTESIAN_POINT('Ctrl Pts',(-22.630711545936,19.726258104984,-58.1697869642843));
#55838=CARTESIAN_POINT('Ctrl Pts',(-22.5179108794207,19.753382840145,-58.1639335159845));
#55839=CARTESIAN_POINT('Ctrl Pts',(-22.4063572344046,19.7854918788342,-58.1580800676848));
#55840=CARTESIAN_POINT('Ctrl Pts',(-22.2965142244232,19.822434234502,-58.152226619385));
#55841=CARTESIAN_POINT('Ctrl Pts',(-22.1865462990875,19.85941860165,-58.1463665144434));
#55842=CARTESIAN_POINT('Ctrl Pts',(-22.0782932837225,19.9012471248324,-58.1405064095019));
#55843=CARTESIAN_POINT('Ctrl Pts',(-21.972200175914,19.9477201220667,-58.1346463045604));
#55844=CARTESIAN_POINT('Ctrl Pts',(-21.8660356210376,19.994224415956,-58.1287822532049));
#55845=CARTESIAN_POINT('Ctrl Pts',(-21.7620342400739,20.0453792298865,-58.1229182018495));
#55846=CARTESIAN_POINT('Ctrl Pts',(-21.6606161682483,20.1009390617494,-58.117054150494));
#55847=CARTESIAN_POINT('Ctrl Pts',(-21.5590486264297,20.1565807777136,-58.1111814566974));
#55848=CARTESIAN_POINT('Ctrl Pts',(-21.4600723444297,20.2166402549786,-58.1053087629009));
#55849=CARTESIAN_POINT('Ctrl Pts',(-21.3640783188479,20.2808288346054,-58.0994360691043));
#55850=CARTESIAN_POINT('Ctrl Pts',(-21.3377967604277,20.2984025939633,-58.097828223781));
#55851=CARTESIAN_POINT('Ctrl Pts',(-21.311738549237,20.3162856293256,-58.0962203784577));
#55852=CARTESIAN_POINT('Ctrl Pts',(-21.2859112562073,20.334471508657,-58.0946125331343));
#55853=CARTESIAN_POINT('Ctrl Pts',(-21.191582820276,20.4008913828341,-58.0887402361656));
#55854=CARTESIAN_POINT('Ctrl Pts',(-21.1000212755521,20.471576448137,-58.0828679391969));
#55855=CARTESIAN_POINT('Ctrl Pts',(-21.0116371444203,20.5462683580514,-58.0769956422282));
#55856=CARTESIAN_POINT('Ctrl Pts',(-20.9233675521031,20.6208634731825,-58.07113095529));
#55857=CARTESIAN_POINT('Ctrl Pts',(-20.8382674976224,20.6994548424408,-58.0652662683518));
#55858=CARTESIAN_POINT('Ctrl Pts',(-20.7567183341826,20.7817410747316,-58.0594015814136));
#55859=CARTESIAN_POINT('Ctrl Pts',(-20.6752530389524,20.8639426807837,-58.0535429259388));
#55860=CARTESIAN_POINT('Ctrl Pts',(-20.597331660246,20.949831299749,-58.047684270464));
#55861=CARTESIAN_POINT('Ctrl Pts',(-20.5233017411223,21.0390659772033,-58.0418256149892));
#55862=CARTESIAN_POINT('Ctrl Pts',(-20.4463801481528,21.1317862397559,-58.0357381152713));
#55863=CARTESIAN_POINT('Ctrl Pts',(-20.3736605672507,21.2281189962251,-58.0296506155534));
#55864=CARTESIAN_POINT('Ctrl Pts',(-20.3054901215756,21.3276401269143,-58.0235631158355));
#55865=CARTESIAN_POINT('Ctrl Pts',(-20.2399583581088,21.4233090803983,-58.0177112457521));
#55866=CARTESIAN_POINT('Ctrl Pts',(-20.1786303656202,21.5219237991508,-58.0118593756687));
#55867=CARTESIAN_POINT('Ctrl Pts',(-20.121772249871,21.6230753324856,-58.0060075055853));
#55868=CARTESIAN_POINT('Ctrl Pts',(-20.0649227912869,21.7242114645798,-58.0001565265023));
#55869=CARTESIAN_POINT('Ctrl Pts',(-20.0125420587352,21.8278832830057,-57.9943055474193));
#55870=CARTESIAN_POINT('Ctrl Pts',(-19.9648510921911,21.9336556377194,-57.9884545683363));
#55871=CARTESIAN_POINT('Ctrl Pts',(-19.9171558377701,22.0394375023857,-57.982603063194));
#55872=CARTESIAN_POINT('Ctrl Pts',(-19.8741513574927,22.1473199019024,-57.9767515580518));
#55873=CARTESIAN_POINT('Ctrl Pts',(-19.8360109756684,22.2568466930297,-57.9709000529095));
#55874=CARTESIAN_POINT('Ctrl Pts',(-19.7978579282537,22.3664098556201,-57.9650466046097));
#55875=CARTESIAN_POINT('Ctrl Pts',(-19.7645723270104,22.4776181054569,-57.9591931563099));
#55876=CARTESIAN_POINT('Ctrl Pts',(-19.736277747191,22.5899997820634,-57.9533397080102));
#55877=CARTESIAN_POINT('Ctrl Pts',(-19.7079509902902,22.7025092610394,-57.9474796030686));
#55878=CARTESIAN_POINT('Ctrl Pts',(-19.6846266846769,22.8161944291788,-57.9416194981271));
#55879=CARTESIAN_POINT('Ctrl Pts',(-19.666377374609,22.9305729659697,-57.9357593931855));
#55880=CARTESIAN_POINT('Ctrl Pts',(-19.6481157747729,23.0450285295464,-57.9298953418301));
#55881=CARTESIAN_POINT('Ctrl Pts',(-19.6349360226784,23.1601779818479,-57.9240312904746));
#55882=CARTESIAN_POINT('Ctrl Pts',(-19.6268586741821,23.2755351517625,-57.9181672391192));
#55883=CARTESIAN_POINT('Ctrl Pts',(-19.6187694212866,23.3910623351181,-57.9122945453226));
#55884=CARTESIAN_POINT('Ctrl Pts',(-19.6157975908789,23.5067974353769,-57.9064218515261));
#55885=CARTESIAN_POINT('Ctrl Pts',(-19.6179116795881,23.6222554681455,-57.9005491577295));
#55886=CARTESIAN_POINT('Ctrl Pts',(-19.6184904817123,23.6538659461412,-57.8989413124061));
#55887=CARTESIAN_POINT('Ctrl Pts',(-19.619450211574,23.6854556951569,-57.8973334670828));
#55888=CARTESIAN_POINT('Ctrl Pts',(-19.6207895502036,23.717014868853,-57.8957256217594));
#55889=CARTESIAN_POINT('Ctrl Pts',(-19.6256811862707,23.8322777223989,-57.8898533247907));
#55890=CARTESIAN_POINT('Ctrl Pts',(-19.6356568211889,23.9475182605663,-57.883981027822));
#55891=CARTESIAN_POINT('Ctrl Pts',(-19.6507210084532,24.0622514567418,-57.8781087308533));
#55892=CARTESIAN_POINT('Ctrl Pts',(-19.6657656737272,24.176835967807,-57.8722440439151));
#55893=CARTESIAN_POINT('Ctrl Pts',(-19.6858857242154,24.2909140382802,-57.8663793569769));
#55894=CARTESIAN_POINT('Ctrl Pts',(-19.7110337321068,24.4040019146483,-57.8605146700387));
#55895=CARTESIAN_POINT('Ctrl Pts',(-19.7361558768464,24.5169734872149,-57.8546560145639));
#55896=CARTESIAN_POINT('Ctrl Pts',(-19.7662956045298,24.6289564901325,-57.8487973590891));
#55897=CARTESIAN_POINT('Ctrl Pts',(-19.8013539262362,24.7394742292742,-57.8429387036143));
#55898=CARTESIAN_POINT('Ctrl Pts',(-19.8377816568674,24.8543088886495,-57.8368512038963));
#55899=CARTESIAN_POINT('Ctrl Pts',(-19.8795200049003,24.9675610308765,-57.8307637041784));
#55900=CARTESIAN_POINT('Ctrl Pts',(-19.9263997861015,25.0787093607413,-57.8246762044605));
#55901=CARTESIAN_POINT('Ctrl Pts',(-19.9714649855825,25.1855554579069,-57.8188243343771));
#55902=CARTESIAN_POINT('Ctrl Pts',(-20.0212808232329,25.2904571630241,-57.8129724642937));
#55903=CARTESIAN_POINT('Ctrl Pts',(-20.0756470834238,25.3929695416689,-57.8071205942103));
#55904=CARTESIAN_POINT('Ctrl Pts',(-20.1300050658573,25.4954663118718,-57.8012696151274));
#55905=CARTESIAN_POINT('Ctrl Pts',(-20.1889118996094,25.5955741138439,-57.7954186360444));
#55906=CARTESIAN_POINT('Ctrl Pts',(-20.2521209671241,25.6928717658994,-57.7895676569614));
#55907=CARTESIAN_POINT('Ctrl Pts',(-20.3153357177422,25.7901781659503,-57.7837161518191));
#55908=CARTESIAN_POINT('Ctrl Pts',(-20.3828532458539,25.8846735671458,-57.7778646466768));
#55909=CARTESIAN_POINT('Ctrl Pts',(-20.4543834796354,25.9759655840778,-57.7720131415346));
#55910=CARTESIAN_POINT('Ctrl Pts',(-20.5259374670503,26.0672879171014,-57.7661596932348));
#55911=CARTESIAN_POINT('Ctrl Pts',(-20.6015065549688,26.1554044253906,-57.760306244935));
#55912=CARTESIAN_POINT('Ctrl Pts',(-20.6807607251806,26.2399561905294,-57.7544527966352));
#55913=CARTESIAN_POINT('Ctrl Pts',(-20.7601050245937,26.3246041093852,-57.7485926916937));
#55914=CARTESIAN_POINT('Ctrl Pts',(-20.8431424880157,26.4056788918743,-57.7427325867522));
#55915=CARTESIAN_POINT('Ctrl Pts',(-20.9295065443544,26.4828587906117,-57.7368724818106));
#55916=CARTESIAN_POINT('Ctrl Pts',(-21.0159287614796,26.5600906651804,-57.7310084304552));
#55917=CARTESIAN_POINT('Ctrl Pts',(-21.1056817129704,26.6334221722514,-57.7251443790997));
#55918=CARTESIAN_POINT('Ctrl Pts',(-21.1983674862254,26.7025732217415,-57.7192803277443));
#55919=CARTESIAN_POINT('Ctrl Pts',(-21.2911898598083,26.7718261860747,-57.7134076339477));
#55920=CARTESIAN_POINT('Ctrl Pts',(-21.386953341168,26.8368861649078,-57.7075349401512));
#55921=CARTESIAN_POINT('Ctrl Pts',(-21.4852328758897,26.8975175079309,-57.7016622463546));
#55922=CARTESIAN_POINT('Ctrl Pts',(-21.5121401684809,26.9141173554123,-57.7000544010312));
#55923=CARTESIAN_POINT('Ctrl Pts',(-21.5392359290243,26.9303855171045,-57.6984465557079));
#55924=CARTESIAN_POINT('Ctrl Pts',(-21.5665111606702,26.9463177803147,-57.6968387103845));
#55925=CARTESIAN_POINT('Ctrl Pts',(-21.6661278699325,27.004506823499,-57.6909664134158));
#55926=CARTESIAN_POINT('Ctrl Pts',(-21.7684739217973,27.0584065507413,-57.6850941164471));
#55927=CARTESIAN_POINT('Ctrl Pts',(-21.8731437165943,27.1077509536635,-57.6792218194784));
#55928=CARTESIAN_POINT('Ctrl Pts',(-21.97767786765,27.1570314101584,-57.6733571325402));
#55929=CARTESIAN_POINT('Ctrl Pts',(-22.0845294026075,27.201768107307,-57.667492445602));
#55930=CARTESIAN_POINT('Ctrl Pts',(-22.1932656947774,27.2417394576408,-57.6616277586638));
#55931=CARTESIAN_POINT('Ctrl Pts',(-22.3018901584778,27.281669699943,-57.655769103189));
#55932=CARTESIAN_POINT('Ctrl Pts',(-22.4123951382376,27.3168442017246,-57.6499104477142));
#55933=CARTESIAN_POINT('Ctrl Pts',(-22.5243260755816,27.3470885706414,-57.6440517922393));
#55934=CARTESIAN_POINT('Ctrl Pts',(-22.6406291339257,27.378514311247,-57.6379642925214));
#55935=CARTESIAN_POINT('Ctrl Pts',(-22.7584714078796,27.4046167227234,-57.6318767928035));
#55936=CARTESIAN_POINT('Ctrl Pts',(-22.8773228717832,27.4252563604422,-57.6257892930856));
#55937=CARTESIAN_POINT('Ctrl Pts',(-22.9915739367877,27.4450970970494,-57.6199374230022));
#55938=CARTESIAN_POINT('Ctrl Pts',(-23.1067570734629,27.4598900157265,-57.6140855529188));
#55939=CARTESIAN_POINT('Ctrl Pts',(-23.2223897259773,27.469563055323,-57.6082336828354));
#55940=CARTESIAN_POINT('Ctrl Pts',(-23.338004772369,27.4792346221112,-57.6023827037524));
#55941=CARTESIAN_POINT('Ctrl Pts',(-23.4540687866825,27.4837878253591,-57.5965317246695));
#55942=CARTESIAN_POINT('Ctrl Pts',(-23.5700941144552,27.4832024819979,-57.5906807455865));
#55943=CARTESIAN_POINT('Ctrl Pts',(-23.6861298740214,27.4826170860086,-57.5848292404442));
#55944=CARTESIAN_POINT('Ctrl Pts',(-23.8021265267299,27.4768922270731,-57.5789777353019));
#55945=CARTESIAN_POINT('Ctrl Pts',(-23.9175971560356,27.4660598465359,-57.5731262301596));
#55946=CARTESIAN_POINT('Ctrl Pts',(-24.0331061306234,27.4552238688009,-57.5672727818599));
#55947=CARTESIAN_POINT('Ctrl Pts',(-24.1480883231084,27.4392770354725,-57.5614193335601));
#55948=CARTESIAN_POINT('Ctrl Pts',(-24.2620633805721,27.4183029857886,-57.5555658852604));
#55949=CARTESIAN_POINT('Ctrl Pts',(-24.3761680524256,27.3973050840557,-57.5497057803188));
#55950=CARTESIAN_POINT('Ctrl Pts',(-24.489262896414,27.371268629795,-57.5438456753773));
#55951=CARTESIAN_POINT('Ctrl Pts',(-24.6008790738485,27.3403281073155,-57.5379855704357));
#55952=CARTESIAN_POINT('Ctrl Pts',(-24.7125704177926,27.3093667483306,-57.5321215190803));
#55953=CARTESIAN_POINT('Ctrl Pts',(-24.822780720244,27.2734948726593,-57.5262574677248));
#55954=CARTESIAN_POINT('Ctrl Pts',(-24.9310592480865,27.2328958502856,-57.5203934163694));
#55955=CARTESIAN_POINT('Ctrl Pts',(-25.0394973568647,27.1922369930572,-57.5145207225728));
#55956=CARTESIAN_POINT('Ctrl Pts',(-25.1459976300264,27.1468372460935,-57.5086480287763));
#55957=CARTESIAN_POINT('Ctrl Pts',(-25.2501320510816,27.0969268358229,-57.5027753349797));
#55958=CARTESIAN_POINT('Ctrl Pts',(-25.2786423136107,27.0832622003899,-57.5011674896564));
#55959=CARTESIAN_POINT('Ctrl Pts',(-25.3069753982381,27.0692597134763,-57.499559644333));
#55960=CARTESIAN_POINT('Ctrl Pts',(-25.335122897576,27.0549246671438,-57.4979517990097));
#55961=CARTESIAN_POINT('Ctrl Pts',(-25.4379253703254,27.0025691028975,-57.492079502041));
#55962=CARTESIAN_POINT('Ctrl Pts',(-25.5385944949873,26.9455987398224,-57.4862072050723));
#55963=CARTESIAN_POINT('Ctrl Pts',(-25.6366872304336,26.8842110269212,-57.4803349081036));
#55964=CARTESIAN_POINT('Ctrl Pts',(-25.7346528454852,26.8229028676205,-57.4744702211654));
#55965=CARTESIAN_POINT('Ctrl Pts',(-25.8300483638023,26.7571889598113,-57.4686055342272));
#55966=CARTESIAN_POINT('Ctrl Pts',(-25.9224535070639,26.6873135021656,-57.462740847289));
#55967=CARTESIAN_POINT('Ctrl Pts',(-26.01476361742,26.617509907054,-57.4568821918142));
#55968=CARTESIAN_POINT('Ctrl Pts',(-26.1040891421339,26.5435535228683,-57.4510235363393));
#55969=CARTESIAN_POINT('Ctrl Pts',(-26.1900376538747,26.4657325108253,-57.4451648808645));
#55970=CARTESIAN_POINT('Ctrl Pts',(-26.2793433901867,26.3848717415081,-57.4390773811466));
#55971=CARTESIAN_POINT('Ctrl Pts',(-26.3650025316752,26.2998385192065,-57.4329898814287));
#55972=CARTESIAN_POINT('Ctrl Pts',(-26.4466112598961,26.2110033876686,-57.4269023817108));
#55973=CARTESIAN_POINT('Ctrl Pts',(-26.5250611485779,26.1256068089924,-57.4210505116274));
#55974=CARTESIAN_POINT('Ctrl Pts',(-26.5997680475929,26.0366975031978,-57.415198641544));
#55975=CARTESIAN_POINT('Ctrl Pts',(-26.6704104888022,25.9446425004954,-57.4093467714606));
#55976=CARTESIAN_POINT('Ctrl Pts',(-26.7410421740574,25.8526015140042,-57.4034957923776));
#55977=CARTESIAN_POINT('Ctrl Pts',(-26.8076103803839,25.757416110791,-57.3976448132947));
#55978=CARTESIAN_POINT('Ctrl Pts',(-26.869834529517,25.6594856529331,-57.3917938342117));
#55979=CARTESIAN_POINT('Ctrl Pts',(-26.9320642731998,25.5615463901846,-57.3859423290694));
#55980=CARTESIAN_POINT('Ctrl Pts',(-26.9899489615603,25.4608619310919,-57.3800908239272));
#55981=CARTESIAN_POINT('Ctrl Pts',(-27.0432522683531,25.3578591923647,-57.3742393187849));
#55982=CARTESIAN_POINT('Ctrl Pts',(-27.0965732760138,25.2548222486705,-57.3683858704851));
#55983=CARTESIAN_POINT('Ctrl Pts',(-27.145309687054,25.149465861485,-57.3625324221853));
#55984=CARTESIAN_POINT('Ctrl Pts',(-27.1892722174519,25.0422393703318,-57.3566789738856));
#55985=CARTESIAN_POINT('Ctrl Pts',(-27.2332847427933,24.9348909393742,-57.3508188689441));
#55986=CARTESIAN_POINT('Ctrl Pts',(-27.2725123945841,24.8256685423021,-57.3449587640025));
#55987=CARTESIAN_POINT('Ctrl Pts',(-27.3068148895434,24.7150393154407,-57.339098659061));
#55988=CARTESIAN_POINT('Ctrl Pts',(-27.3411404850861,24.604335586719,-57.3332346077055));
#55989=CARTESIAN_POINT('Ctrl Pts',(-27.3705342148381,24.4922235406138,-57.3273705563501));
#55990=CARTESIAN_POINT('Ctrl Pts',(-27.3949067106861,24.3791815057082,-57.3215065049947));
#55991=CARTESIAN_POINT('Ctrl Pts',(-27.4193151267278,24.2659728694086,-57.3156338111981));
#55992=CARTESIAN_POINT('Ctrl Pts',(-27.4386874703901,24.1518319148441,-57.3097611174015));
#55993=CARTESIAN_POINT('Ctrl Pts',(-27.4529860739721,24.0372431866136,-57.303888423605));
#55994=CARTESIAN_POINT('Ctrl Pts',(-27.4569007924465,24.0058707096587,-57.3022805782816));
#55995=CARTESIAN_POINT('Ctrl Pts',(-27.4604354986348,23.9744646723974,-57.3006727329582));
#55996=CARTESIAN_POINT('Ctrl Pts',(-27.4635901002877,23.9430350086899,-57.2990648876349));
#55997=CARTESIAN_POINT('Ctrl Pts',(-27.4766056310531,23.8133597596587,-57.2924310991015));
#55998=CARTESIAN_POINT('Ctrl Pts',(-27.4831771127117,23.6830269945391,-57.2857973105681));
#55999=CARTESIAN_POINT('Ctrl Pts',(-27.4832518862965,23.5525056845392,-57.2791635220347));
#56000=CARTESIAN_POINT('',(-27.4814477670606,23.552581764037,-56.0291640430588));
#56001=CARTESIAN_POINT('Ctrl Pts',(-27.4881430614576,23.5524734110292,-57.2791617415215));
#56002=CARTESIAN_POINT('Ctrl Pts',(-27.4801041554848,22.3771595256381,-57.2195004864343));
#56003=CARTESIAN_POINT('Ctrl Pts',(-26.2965486380378,19.8818213561216,-57.0935435942221));
#56004=CARTESIAN_POINT('Ctrl Pts',(-22.0489891170354,19.1471900756399,-56.9012910648851));
#56005=CARTESIAN_POINT('Ctrl Pts',(-19.0343856930495,22.433248714451,-56.7024041535101));
#56006=CARTESIAN_POINT('Ctrl Pts',(-20.1694810114101,26.7457391550027,-56.5035172421352));
#56007=CARTESIAN_POINT('Ctrl Pts',(-24.411218714757,28.1218483213208,-56.3046303307603));
#56008=CARTESIAN_POINT('Ctrl Pts',(-27.1544722338234,25.8760995970628,-56.1465129185815));
#56009=CARTESIAN_POINT('Ctrl Pts',(-27.4808162851497,24.0587493601289,-56.0546911435275));
#56010=CARTESIAN_POINT('Ctrl Pts',(-27.4781149091143,23.5525988839457,-56.0291650055986));
#56011=CARTESIAN_POINT('',(-27.4822168486201,23.5471344304972,-54.7791631113927));
#56012=CARTESIAN_POINT('Ctrl Pts',(-27.4832518474532,23.5525724970079,-56.0291635220347));
#56013=CARTESIAN_POINT('Ctrl Pts',(-27.4833210457297,23.4352617887352,-56.0232550255369));
#56014=CARTESIAN_POINT('Ctrl Pts',(-27.4781373133555,23.3179395204581,-56.0173465290391));
#56015=CARTESIAN_POINT('Ctrl Pts',(-27.4677241201152,23.2011030595281,-56.0114380325413));
#56016=CARTESIAN_POINT('Ctrl Pts',(-27.4573091591171,23.0842467642809,-56.0055285330091));
#56017=CARTESIAN_POINT('Ctrl Pts',(-27.4416630057699,22.9678768410211,-55.9996190334769));
#56018=CARTESIAN_POINT('Ctrl Pts',(-27.420861003246,22.8524853355955,-55.9937095339447));
#56019=CARTESIAN_POINT('Ctrl Pts',(-27.4000508088788,22.7370483889136,-55.9877977072474));
#56020=CARTESIAN_POINT('Ctrl Pts',(-27.3740807956718,22.6225910223746,-55.9818858805501));
#56021=CARTESIAN_POINT('Ctrl Pts',(-27.3430772746285,22.5095943412275,-55.9759740538528));
#56022=CARTESIAN_POINT('Ctrl Pts',(-27.3120322330754,22.3964463327587,-55.9700543099239));
#56023=CARTESIAN_POINT('Ctrl Pts',(-27.2759403254324,22.2847633054023,-55.9641345659949));
#56024=CARTESIAN_POINT('Ctrl Pts',(-27.2349777000081,22.1750109405568,-55.958214822066));
#56025=CARTESIAN_POINT('Ctrl Pts',(-27.1939868338899,22.0651829095912,-55.9522909969124));
#56026=CARTESIAN_POINT('Ctrl Pts',(-27.1481187161183,21.9572885630109,-55.9463671717588));
#56027=CARTESIAN_POINT('Ctrl Pts',(-27.0975968319451,21.8517716176191,-55.9404433466052));
#56028=CARTESIAN_POINT('Ctrl Pts',(-27.0469818102325,21.746060150807,-55.9345086008277));
#56029=CARTESIAN_POINT('Ctrl Pts',(-26.9916960677777,21.6427351980163,-55.9285738550501));
#56030=CARTESIAN_POINT('Ctrl Pts',(-26.932008429644,21.5422146718217,-55.9226391092726));
#56031=CARTESIAN_POINT('Ctrl Pts',(-26.8790982052221,21.4531080533279,-55.9173782421853));
#56032=CARTESIAN_POINT('Ctrl Pts',(-26.8227297304176,21.3662048814533,-55.9121173750979));
#56033=CARTESIAN_POINT('Ctrl Pts',(-26.7631168605512,21.2817746710224,-55.9068565080106));
#56034=CARTESIAN_POINT('Ctrl Pts',(-26.6965756480093,21.187531790419,-55.9009842110419));
#56035=CARTESIAN_POINT('Ctrl Pts',(-26.6257728086476,21.0960612877013,-55.8951119140732));
#56036=CARTESIAN_POINT('Ctrl Pts',(-26.5509672170767,21.0077733524422,-55.8892396171045));
#56037=CARTESIAN_POINT('Ctrl Pts',(-26.4762585676116,20.9195998313355,-55.8833749301663));
#56038=CARTESIAN_POINT('Ctrl Pts',(-26.3975577462774,20.8346009883091,-55.8775102432281));
#56039=CARTESIAN_POINT('Ctrl Pts',(-26.3151666346911,20.7531577883848,-55.8716455562899));
#56040=CARTESIAN_POINT('Ctrl Pts',(-26.2328602572054,20.6717983476934,-55.8657869008151));
#56041=CARTESIAN_POINT('Ctrl Pts',(-26.1468714306049,20.5939875654901,-55.8599282453403));
#56042=CARTESIAN_POINT('Ctrl Pts',(-26.0575415562922,20.5200725457643,-55.8540695898655));
#56043=CARTESIAN_POINT('Ctrl Pts',(-25.9647223784078,20.4432703402642,-55.8479820901476));
#56044=CARTESIAN_POINT('Ctrl Pts',(-25.8682961172614,20.3706747923508,-55.8418945904297));
#56045=CARTESIAN_POINT('Ctrl Pts',(-25.7686873389186,20.3026324790872,-55.8358070907118));
#56046=CARTESIAN_POINT('Ctrl Pts',(-25.67293413037,20.2372238883941,-55.8299552206284));
#56047=CARTESIAN_POINT('Ctrl Pts',(-25.5742405689188,20.1760228561691,-55.824103350545));
#56048=CARTESIAN_POINT('Ctrl Pts',(-25.4730159473699,20.1192949616652,-55.8182514804616));
#56049=CARTESIAN_POINT('Ctrl Pts',(-25.3718067381901,20.0625757044991,-55.8124005013786));
#56050=CARTESIAN_POINT('Ctrl Pts',(-25.2680675956813,20.0103284328963,-55.8065495222956));
#56051=CARTESIAN_POINT('Ctrl Pts',(-25.1622339539886,19.9627736266443,-55.8006985432127));
#56052=CARTESIAN_POINT('Ctrl Pts',(-25.0563907968331,19.9152145447578,-55.7948470380704));
#56053=CARTESIAN_POINT('Ctrl Pts',(-24.9484531432285,19.8723489363555,-55.7889955329281));
#56054=CARTESIAN_POINT('Ctrl Pts',(-24.8388773590915,19.8343495385827,-55.7831440277858));
#56055=CARTESIAN_POINT('Ctrl Pts',(-24.7292651872215,19.7963375220369,-55.777290579486));
#56056=CARTESIAN_POINT('Ctrl Pts',(-24.6180141934921,19.7631950647314,-55.7714371311862));
#56057=CARTESIAN_POINT('Ctrl Pts',(-24.5055961970215,19.7350451348258,-55.7655836828864));
#56058=CARTESIAN_POINT('Ctrl Pts',(-24.3930503568783,19.7068631923375,-55.7597235779449));
#56059=CARTESIAN_POINT('Ctrl Pts',(-24.2793352663113,19.6836852100147,-55.7538634730033));
#56060=CARTESIAN_POINT('Ctrl Pts',(-24.1649333387917,19.6655831113463,-55.7480033680618));
#56061=CARTESIAN_POINT('Ctrl Pts',(-24.0504543687342,19.6474688220474,-55.7421393167063));
#56062=CARTESIAN_POINT('Ctrl Pts',(-23.9352880504695,19.6344372692628,-55.7362752653509));
#56063=CARTESIAN_POINT('Ctrl Pts',(-23.8199205811606,19.6265083831676,-55.7304112139954));
#56064=CARTESIAN_POINT('Ctrl Pts',(-23.7043830832316,19.618567811477,-55.7245385201989));
#56065=CARTESIAN_POINT('Ctrl Pts',(-23.5886442542966,19.6157449256096,-55.7186658264023));
#56066=CARTESIAN_POINT('Ctrl Pts',(-23.4731890378049,19.6180075980832,-55.7127931326057));
#56067=CARTESIAN_POINT('Ctrl Pts',(-23.4415793308591,19.6186270799566,-55.7111852872824));
#56068=CARTESIAN_POINT('Ctrl Pts',(-23.4099908431004,19.6196274625754,-55.7095774419591));
#56069=CARTESIAN_POINT('Ctrl Pts',(-23.3784334191629,19.6210074142996,-55.7079695966357));
#56070=CARTESIAN_POINT('Ctrl Pts',(-23.2631769562199,19.6260473806506,-55.702097299667));
#56071=CARTESIAN_POINT('Ctrl Pts',(-23.1479493513484,19.6361713129244,-55.6962250026983));
#56072=CARTESIAN_POINT('Ctrl Pts',(-23.0332356366199,19.6513831404209,-55.6903527057296));
#56073=CARTESIAN_POINT('Ctrl Pts',(-22.9186705817551,19.6665752545971,-55.6844880187914));
#56074=CARTESIAN_POINT('Ctrl Pts',(-22.8046184986894,19.6868420980349,-55.6786233318532));
#56075=CARTESIAN_POINT('Ctrl Pts',(-22.6915630794992,19.7121356204096,-55.6727586449149));
#56076=CARTESIAN_POINT('Ctrl Pts',(-22.5786239307304,19.7374031299798,-55.6668999894401));
#56077=CARTESIAN_POINT('Ctrl Pts',(-22.4666798080314,19.7676869461267,-55.6610413339653));
#56078=CARTESIAN_POINT('Ctrl Pts',(-22.3562072777432,19.8028874665428,-55.6551826784905));
#56079=CARTESIAN_POINT('Ctrl Pts',(-22.2414195931189,19.8394629502906,-55.6490951787726));
#56080=CARTESIAN_POINT('Ctrl Pts',(-22.1282212586844,19.8813470104659,-55.6430076790547));
#56081=CARTESIAN_POINT('Ctrl Pts',(-22.0171333514949,19.928369792109,-55.6369201793368));
#56082=CARTESIAN_POINT('Ctrl Pts',(-21.9103453382162,19.9735724568954,-55.6310683092534));
#56083=CARTESIAN_POINT('Ctrl Pts',(-21.8055078290779,20.0235232536357,-55.62521643917));
#56084=CARTESIAN_POINT('Ctrl Pts',(-21.7030655004737,20.0780213942711,-55.6193645690865));
#56085=CARTESIAN_POINT('Ctrl Pts',(-21.6006387696455,20.1325112370689,-55.6135135900036));
#56086=CARTESIAN_POINT('Ctrl Pts',(-21.500606859088,20.1915468530021,-55.6076626109206));
#56087=CARTESIAN_POINT('Ctrl Pts',(-21.4033906327606,20.2548810826908,-55.6018116318376));
#56088=CARTESIAN_POINT('Ctrl Pts',(-21.3061656657588,20.3182210067362,-55.5959601266953));
#56089=CARTESIAN_POINT('Ctrl Pts',(-21.2117572326247,20.385860087175,-55.590108621553));
#56090=CARTESIAN_POINT('Ctrl Pts',(-21.1205573451418,20.4575077474541,-55.5842571164107));
#56091=CARTESIAN_POINT('Ctrl Pts',(-21.0293271721614,20.5291792003617,-55.5784036681109));
#56092=CARTESIAN_POINT('Ctrl Pts',(-20.9413079883829,20.6048616248008,-55.5725502198111));
#56093=CARTESIAN_POINT('Ctrl Pts',(-20.8568582872175,20.6842245409342,-55.5666967715114));
#56094=CARTESIAN_POINT('Ctrl Pts',(-20.7723125484041,20.7636777099364,-55.5608366665698));
#56095=CARTESIAN_POINT('Ctrl Pts',(-20.6913446958137,20.8468194415406,-55.5549765616283));
#56096=CARTESIAN_POINT('Ctrl Pts',(-20.6142760048163,20.9332827508939,-55.5491164566867));
#56097=CARTESIAN_POINT('Ctrl Pts',(-20.5371554128789,21.0198042878746,-55.5432524053313));
#56098=CARTESIAN_POINT('Ctrl Pts',(-20.4639394716058,21.1096515369929,-55.5373883539758));
#56099=CARTESIAN_POINT('Ctrl Pts',(-20.3949077587654,21.2024262255227,-55.5315243026204));
#56100=CARTESIAN_POINT('Ctrl Pts',(-20.3257743069605,21.2953376454236,-55.5256516088238));
#56101=CARTESIAN_POINT('Ctrl Pts',(-20.2608376221606,21.3911847746194,-55.5197789150272));
#56102=CARTESIAN_POINT('Ctrl Pts',(-20.2003328074686,21.4895422557835,-55.5139062212307));
#56103=CARTESIAN_POINT('Ctrl Pts',(-20.183767601328,21.5164708888062,-55.5122983759074));
#56104=CARTESIAN_POINT('Ctrl Pts',(-20.1675343232456,21.5435875627712,-55.5106905305841));
#56105=CARTESIAN_POINT('Ctrl Pts',(-20.1516371743323,21.5708832754148,-55.5090826852607));
#56106=CARTESIAN_POINT('Ctrl Pts',(-20.0935763782963,21.6705747869621,-55.503210388292));
#56107=CARTESIAN_POINT('Ctrl Pts',(-20.0398084071022,21.7729901188356,-55.4973380913233));
#56108=CARTESIAN_POINT('Ctrl Pts',(-19.9905987469325,21.8777233293686,-55.4914657943546));
#56109=CARTESIAN_POINT('Ctrl Pts',(-19.9414528585742,21.9823208139786,-55.4856011074164));
#56110=CARTESIAN_POINT('Ctrl Pts',(-19.8968537080926,22.0892298331064,-55.4797364204782));
#56111=CARTESIAN_POINT('Ctrl Pts',(-19.8570223260157,22.1980174752548,-55.47387173354));
#56112=CARTESIAN_POINT('Ctrl Pts',(-19.8172319080216,22.3066932361237,-55.4680130780652));
#56113=CARTESIAN_POINT('Ctrl Pts',(-19.7821996466882,22.4172433912263,-55.4621544225904));
#56114=CARTESIAN_POINT('Ctrl Pts',(-19.7520993492335,22.5292131580345,-55.4562957671155));
#56115=CARTESIAN_POINT('Ctrl Pts',(-19.7208233076483,22.6455565625555,-55.4502082673976));
#56116=CARTESIAN_POINT('Ctrl Pts',(-19.694872571635,22.763432330701,-55.4441207676797));
#56117=CARTESIAN_POINT('Ctrl Pts',(-19.6743859036046,22.8823102577951,-55.4380332679618));
#56118=CARTESIAN_POINT('Ctrl Pts',(-19.6546922156685,22.9965867616761,-55.4321813978784));
#56119=CARTESIAN_POINT('Ctrl Pts',(-19.6400475409863,23.1117888403065,-55.426329527795));
#56120=CARTESIAN_POINT('Ctrl Pts',(-19.6305233196369,23.2274338455175,-55.4204776577117));
#56121=CARTESIAN_POINT('Ctrl Pts',(-19.6210005484369,23.3430612427248,-55.4146266786287));
#56122=CARTESIAN_POINT('Ctrl Pts',(-19.6165967143256,23.4591310205462,-55.4087756995457));
#56123=CARTESIAN_POINT('Ctrl Pts',(-19.6173313727817,23.5751554989486,-55.4029247204628));
#56124=CARTESIAN_POINT('Ctrl Pts',(-19.6180660972906,23.6911904090681,-55.3970732153205));
#56125=CARTESIAN_POINT('Ctrl Pts',(-19.6239402301624,23.8071795982729,-55.3912217101782));
#56126=CARTESIAN_POINT('Ctrl Pts',(-19.6349212034552,23.9226361915271,-55.3853702050359));
#56127=CARTESIAN_POINT('Ctrl Pts',(-19.6459058232902,24.0381311254019,-55.3795167567362));
#56128=CARTESIAN_POINT('Ctrl Pts',(-19.6620006165586,24.1530927003363,-55.3736633084365));
#56129=CARTESIAN_POINT('Ctrl Pts',(-19.6831213259151,24.2670406714466,-55.3678098601367));
#56130=CARTESIAN_POINT('Ctrl Pts',(-19.7042660541046,24.3811182261442,-55.3619497551952));
#56131=CARTESIAN_POINT('Ctrl Pts',(-19.7304480310795,24.4941794695873,-55.3560896502537));
#56132=CARTESIAN_POINT('Ctrl Pts',(-19.7615321692833,24.6057557365463,-55.3502295453121));
#56133=CARTESIAN_POINT('Ctrl Pts',(-19.7926372407087,24.7174071431378,-55.3443654939567));
#56134=CARTESIAN_POINT('Ctrl Pts',(-19.8286509187688,24.8275711900096,-55.3385014426012));
#56135=CARTESIAN_POINT('Ctrl Pts',(-19.8693892535732,24.9357973804018,-55.3326373912458));
#56136=CARTESIAN_POINT('Ctrl Pts',(-19.910187628551,25.0441830745949,-55.3267646974492));
#56137=CARTESIAN_POINT('Ctrl Pts',(-19.9557243954944,25.1506248336195,-55.3208920036526));
#56138=CARTESIAN_POINT('Ctrl Pts',(-20.0057687773416,25.2546949376237,-55.3150193098561));
#56139=CARTESIAN_POINT('Ctrl Pts',(-20.0194700919515,25.2831875912205,-55.3134114645327));
#56140=CARTESIAN_POINT('Ctrl Pts',(-20.033509029748,25.3115026322737,-55.3118036192093));
#56141=CARTESIAN_POINT('Ctrl Pts',(-20.0478802878541,25.339631660213,-55.310195773886));
#56142=CARTESIAN_POINT('Ctrl Pts',(-20.1003681075384,25.4423666702912,-55.3043234769172));
#56143=CARTESIAN_POINT('Ctrl Pts',(-20.157467976777,25.5429623951609,-55.2984511799485));
#56144=CARTESIAN_POINT('Ctrl Pts',(-20.2189818765709,25.6409760481627,-55.2925788829798));
#56145=CARTESIAN_POINT('Ctrl Pts',(-20.280416059236,25.7388626832542,-55.2867141960416));
#56146=CARTESIAN_POINT('Ctrl Pts',(-20.3462526792466,25.8341735538834,-55.2808495091034));
#56147=CARTESIAN_POINT('Ctrl Pts',(-20.4162469972672,25.9264886963422,-55.2749848221652));
#56148=CARTESIAN_POINT('Ctrl Pts',(-20.4861693305134,26.0187088984558,-55.2691261666904));
#56149=CARTESIAN_POINT('Ctrl Pts',(-20.560240608465,26.1079391730819,-55.2632675112156));
#56150=CARTESIAN_POINT('Ctrl Pts',(-20.6381721651203,26.1937874640556,-55.2574088557408));
#56151=CARTESIAN_POINT('Ctrl Pts',(-20.71914779702,26.2829890648891,-55.2513213560229));
#56152=CARTESIAN_POINT('Ctrl Pts',(-20.8042911855645,26.3685387042961,-55.245233856305));
#56153=CARTESIAN_POINT('Ctrl Pts',(-20.8932312676302,26.4500330410279,-55.2391463565871));
#56154=CARTESIAN_POINT('Ctrl Pts',(-20.9787287345005,26.5283729659867,-55.2332944865037));
#56155=CARTESIAN_POINT('Ctrl Pts',(-21.0677341086437,26.6029653837714,-55.2274426164202));
#56156=CARTESIAN_POINT('Ctrl Pts',(-21.1598799464485,26.6734892988487,-55.2215907463368));
#56157=CARTESIAN_POINT('Ctrl Pts',(-21.2520117542115,26.7440024760186,-55.2157397672539));
#56158=CARTESIAN_POINT('Ctrl Pts',(-21.3472827467111,26.8104481310046,-55.2098887881709));
#56159=CARTESIAN_POINT('Ctrl Pts',(-21.4452932011183,26.8725461997226,-55.2040378090879));
#56160=CARTESIAN_POINT('Ctrl Pts',(-21.5433124676084,26.9346498516544,-55.1981863039456));
#56161=CARTESIAN_POINT('Ctrl Pts',(-21.644071336421,26.9924049190076,-55.1923347988034));
#56162=CARTESIAN_POINT('Ctrl Pts',(-21.7471425870662,27.0455756251412,-55.1864832936611));
#56163=CARTESIAN_POINT('Ctrl Pts',(-21.8502480654299,27.0987639881087,-55.1806298453613));
#56164=CARTESIAN_POINT('Ctrl Pts',(-21.9556670853445,27.1473647733088,-55.1747763970616));
#56165=CARTESIAN_POINT('Ctrl Pts',(-22.0629500640649,27.1911892751414,-55.1689229487618));
#56166=CARTESIAN_POINT('Ctrl Pts',(-22.1703550468282,27.2350636149489,-55.1630628438203));
#56167=CARTESIAN_POINT('Ctrl Pts',(-22.279627836394,27.2741506735195,-55.1572027388788));
#56168=CARTESIAN_POINT('Ctrl Pts',(-22.3903011162899,27.3083107688563,-55.1513426339372));
#56169=CARTESIAN_POINT('Ctrl Pts',(-22.501048927713,27.3424938688792,-55.1454785825818));
#56170=CARTESIAN_POINT('Ctrl Pts',(-22.6131987084253,27.3717432948005,-55.1396145312263));
#56171=CARTESIAN_POINT('Ctrl Pts',(-22.7262720152301,27.3959702941525,-55.1337504798709));
#56172=CARTESIAN_POINT('Ctrl Pts',(-22.8395119695179,27.4202329992656,-55.1278777860744));
#56173=CARTESIAN_POINT('Ctrl Pts',(-22.9536777602647,27.4394584363482,-55.1220050922778));
#56174=CARTESIAN_POINT('Ctrl Pts',(-23.0682847947976,27.4536095613023,-55.1161323984812));
#56175=CARTESIAN_POINT('Ctrl Pts',(-23.0996622837125,27.4574839025954,-55.1145245531578));
#56176=CARTESIAN_POINT('Ctrl Pts',(-23.1310728438597,27.4609781887276,-55.1129167078344));
#56177=CARTESIAN_POINT('Ctrl Pts',(-23.1625065412686,27.4640923402337,-55.111308862511));
#56178=CARTESIAN_POINT('Ctrl Pts',(-23.2773111206166,27.4754660850732,-55.1054365655423));
#56179=CARTESIAN_POINT('Ctrl Pts',(-23.392808891728,27.4818032608947,-55.0995642685736));
#56180=CARTESIAN_POINT('Ctrl Pts',(-23.5085202930935,27.4830311194438,-55.0936919716049));
#56181=CARTESIAN_POINT('Ctrl Pts',(-23.6240817416724,27.4842573867857,-55.0878272846667));
#56182=CARTESIAN_POINT('Ctrl Pts',(-23.7398558604101,27.4803874998374,-55.0819625977285));
#56183=CARTESIAN_POINT('Ctrl Pts',(-23.8553570348068,27.4714003537203,-55.0760979107903));
#56184=CARTESIAN_POINT('Ctrl Pts',(-23.9707394234761,27.4624224503204,-55.0702392553155));
#56185=CARTESIAN_POINT('Ctrl Pts',(-24.0858490164839,27.4483377875688,-55.0643805998407));
#56186=CARTESIAN_POINT('Ctrl Pts',(-24.2001999341894,27.4291773020384,-55.0585219443659));
#56187=CARTESIAN_POINT('Ctrl Pts',(-24.3190174994595,27.4092683910668,-55.052434444648));
#56188=CARTESIAN_POINT('Ctrl Pts',(-24.4370154574585,27.3838790365336,-55.0463469449301));
#56189=CARTESIAN_POINT('Ctrl Pts',(-24.5536538950772,27.3531033970268,-55.0402594452122));
#56190=CARTESIAN_POINT('Ctrl Pts',(-24.66577759369,27.3235189941566,-55.0344075751288));
#56191=CARTESIAN_POINT('Ctrl Pts',(-24.7766446242322,27.2889576435455,-55.0285557050453));
#56192=CARTESIAN_POINT('Ctrl Pts',(-24.8857863089272,27.2495549699749,-55.0227038349619));
#56193=CARTESIAN_POINT('Ctrl Pts',(-24.9949113758078,27.2101582958199,-55.016852855879));
#56194=CARTESIAN_POINT('Ctrl Pts',(-25.1023112304589,27.1659219047011,-55.0110018767961));
#56195=CARTESIAN_POINT('Ctrl Pts',(-25.2075341831328,27.117030703631,-55.0051508977131));
#56196=CARTESIAN_POINT('Ctrl Pts',(-25.3127665963632,27.0681351067712,-54.9992993925708));
#56197=CARTESIAN_POINT('Ctrl Pts',(-25.4158213436214,27.0145840421973,-54.9934478874285));
#56198=CARTESIAN_POINT('Ctrl Pts',(-25.5162691312773,26.9566094904059,-54.9875963822862));
#56199=CARTESIAN_POINT('Ctrl Pts',(-25.616750275457,26.8986156865278,-54.9817429339864));
#56200=CARTESIAN_POINT('Ctrl Pts',(-25.7146223807757,26.8361956810611,-54.9758894856866));
#56201=CARTESIAN_POINT('Ctrl Pts',(-25.8094836675129,26.7696257121359,-54.9700360373868));
#56202=CARTESIAN_POINT('Ctrl Pts',(-25.9044528321315,26.7029800387009,-54.9641759324453));
#56203=CARTESIAN_POINT('Ctrl Pts',(-25.996404005482,26.6321752196087,-54.9583158275038));
#56204=CARTESIAN_POINT('Ctrl Pts',(-26.0849670663925,26.5575289120073,-54.9524557225622));
#56205=CARTESIAN_POINT('Ctrl Pts',(-26.1735897689815,26.4828323347897,-54.9465916712068));
#56206=CARTESIAN_POINT('Ctrl Pts',(-26.2588195126049,26.4042893972812,-54.9407276198514));
#56207=CARTESIAN_POINT('Ctrl Pts',(-26.3403230094922,26.3222546472995,-54.9348635684959));
#56208=CARTESIAN_POINT('Ctrl Pts',(-26.4219466262642,26.240098994472,-54.9289908746994));
#56209=CARTESIAN_POINT('Ctrl Pts',(-26.4998327587808,26.1544415629824,-54.9231181809028));
#56210=CARTESIAN_POINT('Ctrl Pts',(-26.5736882983376,26.0656700248713,-54.9172454871063));
#56211=CARTESIAN_POINT('Ctrl Pts',(-26.5939087096164,26.0413658627024,-54.9156376417829));
#56212=CARTESIAN_POINT('Ctrl Pts',(-26.6138272505147,26.0168284412247,-54.9140297964595));
#56213=CARTESIAN_POINT('Ctrl Pts',(-26.633438484445,25.9920660751001,-54.9124219511362));
#56214=CARTESIAN_POINT('Ctrl Pts',(-26.7049732138191,25.9017418677765,-54.9065571095616));
#56215=CARTESIAN_POINT('Ctrl Pts',(-26.7726603804216,25.8081136964325,-54.9006922679871));
#56216=CARTESIAN_POINT('Ctrl Pts',(-26.8361786611447,25.7115434588474,-54.8948274264125));
#56217=CARTESIAN_POINT('Ctrl Pts',(-26.8996168611287,25.6150949722905,-54.8889699789431));
#56218=CARTESIAN_POINT('Ctrl Pts',(-26.9588963977614,25.5157121346701,-54.8831125314737));
#56219=CARTESIAN_POINT('Ctrl Pts',(-27.0137358333513,25.4137901404218,-54.8772550840044));
#56220=CARTESIAN_POINT('Ctrl Pts',(-27.0685194668807,25.3119718572574,-54.8714035968013));
#56221=CARTESIAN_POINT('Ctrl Pts',(-27.1188717875628,25.2076199165718,-54.8655521095982));
#56222=CARTESIAN_POINT('Ctrl Pts',(-27.1645547795137,25.1011581579034,-54.8597006223951));
#56223=CARTESIAN_POINT('Ctrl Pts',(-27.2102023940815,24.9947788443254,-54.8538536666443));
#56224=CARTESIAN_POINT('Ctrl Pts',(-27.2511877090005,24.8862933411769,-54.8480067108936));
#56225=CARTESIAN_POINT('Ctrl Pts',(-27.2873191081256,24.7761491029104,-54.8421597551429));
#56226=CARTESIAN_POINT('Ctrl Pts',(-27.3234340270074,24.6660551036019,-54.836315466304));
#56227=CARTESIAN_POINT('Ctrl Pts',(-27.3546993026387,24.5543042658531,-54.8304711774651));
#56228=CARTESIAN_POINT('Ctrl Pts',(-27.3809720672344,24.4413624239244,-54.8246268886261));
#56229=CARTESIAN_POINT('Ctrl Pts',(-27.4072375689592,24.3284518037582,-54.8187842153886));
#56230=CARTESIAN_POINT('Ctrl Pts',(-27.4285132143907,24.2143512380285,-54.812941542151));
#56231=CARTESIAN_POINT('Ctrl Pts',(-27.4447066747234,24.0995392763389,-54.8070988689135));
#56232=CARTESIAN_POINT('Ctrl Pts',(-27.4609036343248,23.9847025047637,-54.8012549331241));
#56233=CARTESIAN_POINT('Ctrl Pts',(-27.4720161551831,23.8691544399423,-54.7954109973347));
#56234=CARTESIAN_POINT('Ctrl Pts',(-27.4780035216107,23.7533809669516,-54.7895670615453));
#56235=CARTESIAN_POINT('Ctrl Pts',(-27.481556481205,23.6846798983596,-54.7860992150418));
#56236=CARTESIAN_POINT('Ctrl Pts',(-27.4833056850997,23.6158995597262,-54.7826313685382));
#56237=CARTESIAN_POINT('Ctrl Pts',(-27.4832513014648,23.5471417467537,-54.7791635220347));
#56238=CARTESIAN_POINT('',(-27.4893929762737,23.5491656528098,-53.5291635220347));
#56239=CARTESIAN_POINT('Ctrl Pts',(-27.4796534495588,23.5471163006375,-54.7791620938121));
#56240=CARTESIAN_POINT('Ctrl Pts',(-27.4828378583424,23.1137759715362,-54.7572864091285));
#56241=CARTESIAN_POINT('Ctrl Pts',(-27.216596050397,21.3709791532061,-54.6691150873199));
#56242=CARTESIAN_POINT('Ctrl Pts',(-24.6614438543076,19.0329519354699,-54.5146481283863));
#56243=CARTESIAN_POINT('Ctrl Pts',(-20.3504177643223,20.1735961539112,-54.3157612170115));
#56244=CARTESIAN_POINT('Ctrl Pts',(-18.9797685243006,24.4171012902892,-54.1168743056365));
#56245=CARTESIAN_POINT('Ctrl Pts',(-21.809006573937,27.8640459141707,-53.9179873942616));
#56246=CARTESIAN_POINT('Ctrl Pts',(-26.1718623003577,27.3547361893404,-53.7220837997278));
#56247=CARTESIAN_POINT('Ctrl Pts',(-27.4848291776058,24.7953569349182,-53.5924758423187));
#56248=CARTESIAN_POINT('Ctrl Pts',(-27.4893929762737,23.5491656528098,-53.5291635220347));
#56249=CARTESIAN_POINT('',(-27.482958713852,23.5538899792342,-52.2791635220347));
#56250=CARTESIAN_POINT('Ctrl Pts',(-27.4893929762737,23.5491656528098,-53.5291635220347));
#56251=CARTESIAN_POINT('Ctrl Pts',(-27.4896080253726,23.4904443261825,-53.5261802051937));
#56252=CARTESIAN_POINT('Ctrl Pts',(-27.4884091334729,23.431731975206,-53.5231968883528));
#56253=CARTESIAN_POINT('Ctrl Pts',(-27.4270986390246,22.0698132025148,-53.4539179343869));
#56254=CARTESIAN_POINT('Ctrl Pts',(-25.8862801146668,19.5273523385874,-53.3213266601369));
#56255=CARTESIAN_POINT('Ctrl Pts',(-21.4284410418566,19.4103652344728,-53.1224397487623));
#56256=CARTESIAN_POINT('Ctrl Pts',(-18.920366828257,23.097583551946,-52.9235528373871));
#56257=CARTESIAN_POINT('Ctrl Pts',(-20.6667650265468,27.2007662818071,-52.7246659260124));
#56258=CARTESIAN_POINT('Ctrl Pts',(-25.0628437626404,27.9494363878393,-52.5257790146374));
#56259=CARTESIAN_POINT('Ctrl Pts',(-27.3074034903904,25.4900842062352,-52.3772782133115));
#56260=CARTESIAN_POINT('Ctrl Pts',(-27.4858519506129,23.8683743917818,-52.2950730491106));
#56261=CARTESIAN_POINT('Ctrl Pts',(-27.482958713852,23.5538899792342,-52.2791635220347));
#56262=CARTESIAN_POINT('',(-27.476795898706,23.5497105560713,-51.0291635220347));
#56263=CARTESIAN_POINT('Ctrl Pts',(-27.482958713852,23.5538899792342,-52.2791635220347));
#56264=CARTESIAN_POINT('Ctrl Pts',(-27.4737957170429,22.557905237283,-52.2287774119857));
#56265=CARTESIAN_POINT('Ctrl Pts',(-26.5831973659458,20.2368697433501,-52.1120956648117));
#56266=CARTESIAN_POINT('Ctrl Pts',(-22.677522633219,18.9808878760329,-51.9291182805128));
#56267=CARTESIAN_POINT('Ctrl Pts',(-19.2342218731823,21.8145595326581,-51.7302313691379));
#56268=CARTESIAN_POINT('Ctrl Pts',(-19.7569873492678,26.2431858929006,-51.5313444577628));
#56269=CARTESIAN_POINT('Ctrl Pts',(-23.7654419121505,28.1972348172902,-51.3324575463881));
#56270=CARTESIAN_POINT('Ctrl Pts',(-26.9727382800942,26.2478552605321,-51.1650639011454));
#56271=CARTESIAN_POINT('Ctrl Pts',(-27.4759497159671,24.2403761058591,-51.0639658930275));
#56272=CARTESIAN_POINT('Ctrl Pts',(-27.476795898706,23.5497105560713,-51.0291635220347));
#56273=CARTESIAN_POINT('',(-27.483338271532,23.546803532641,-49.7791635651174));
#56274=CARTESIAN_POINT('Ctrl Pts',(-27.476795898706,23.5497105560713,-51.0291635220347));
#56275=CARTESIAN_POINT('Ctrl Pts',(-27.4775616240699,22.9247153805349,-50.9976702559025));
#56276=CARTESIAN_POINT('Ctrl Pts',(-27.0416309458266,20.9850685926429,-50.8998813526456));
#56277=CARTESIAN_POINT('Ctrl Pts',(-23.9969628335229,18.9197881124001,-50.7357968122635));
#56278=CARTESIAN_POINT('Ctrl Pts',(-19.8960309801959,20.6714653418028,-50.5369099008885));
#56279=CARTESIAN_POINT('Ctrl Pts',(-19.1530189058048,25.0685039178133,-50.3380229895135));
#56280=CARTESIAN_POINT('Ctrl Pts',(-22.450691709674,28.0703981964692,-50.1391360781388));
#56281=CARTESIAN_POINT('Ctrl Pts',(-26.4858247139179,26.9916313974245,-49.9528498692994));
#56282=CARTESIAN_POINT('Ctrl Pts',(-27.4752038925693,24.6068284845104,-49.8328592975852));
#56283=CARTESIAN_POINT('Ctrl Pts',(-27.4849541685477,23.546817866354,-49.7791643629959));
#56284=CARTESIAN_POINT('',(-27.4850065049564,23.5523966888927,-48.5291629058911));
#56285=CARTESIAN_POINT('Ctrl Pts',(-27.4832510187351,23.5468027586706,-49.7791635220347));
#56286=CARTESIAN_POINT('Ctrl Pts',(-27.4831011760015,23.3759708690314,-49.7705061923292));
#56287=CARTESIAN_POINT('Ctrl Pts',(-27.4718178556067,23.2056082410999,-49.7618488626238));
#56288=CARTESIAN_POINT('Ctrl Pts',(-27.449602469036,23.0368724910297,-49.7531915329183));
#56289=CARTESIAN_POINT('Ctrl Pts',(-27.4394841846031,22.9600196166593,-49.7492484404086));
#56290=CARTESIAN_POINT('Ctrl Pts',(-27.4270986677299,22.8835037321968,-49.7453053478988));
#56291=CARTESIAN_POINT('Ctrl Pts',(-27.4124678417013,22.8074322982954,-49.741362255389));
#56292=CARTESIAN_POINT('Ctrl Pts',(-27.3906787116914,22.6941420192582,-49.7354899584203));
#56293=CARTESIAN_POINT('Ctrl Pts',(-27.3638641407678,22.5816214712891,-49.7296176614516));
#56294=CARTESIAN_POINT('Ctrl Pts',(-27.332090953477,22.4703510771497,-49.7237453644829));
#56295=CARTESIAN_POINT('Ctrl Pts',(-27.3003589417136,22.3592248806043,-49.7178806775447));
#56296=CARTESIAN_POINT('Ctrl Pts',(-27.2636812049932,22.2493460099168,-49.7120159906065));
#56297=CARTESIAN_POINT('Ctrl Pts',(-27.2221757967736,22.1411859841641,-49.7061513036684));
#56298=CARTESIAN_POINT('Ctrl Pts',(-27.1807130742681,22.033137194227,-49.7002926481936));
#56299=CARTESIAN_POINT('Ctrl Pts',(-27.1344327030313,21.9268041167515,-49.6944339927187));
#56300=CARTESIAN_POINT('Ctrl Pts',(-27.0835026988673,21.82264370555,-49.6885753372439));
#56301=CARTESIAN_POINT('Ctrl Pts',(-27.030583323882,21.7144146969434,-49.682487837526));
#56302=CARTESIAN_POINT('Ctrl Pts',(-26.9726437983051,21.6085319845137,-49.6764003378081));
#56303=CARTESIAN_POINT('Ctrl Pts',(-26.9099281291323,21.5054863152335,-49.6703128380902));
#56304=CARTESIAN_POINT('Ctrl Pts',(-26.8496400034323,21.4064292479272,-49.6644609680068));
#56305=CARTESIAN_POINT('Ctrl Pts',(-26.784938835661,21.3099940660363,-49.6586090979234));
#56306=CARTESIAN_POINT('Ctrl Pts',(-26.7160880971187,21.2165914224726,-49.65275722784));
#56307=CARTESIAN_POINT('Ctrl Pts',(-26.6472478417273,21.1232030003107,-49.646906248757));
#56308=CARTESIAN_POINT('Ctrl Pts',(-26.5742595170202,21.0328465310636,-49.6410552696741));
#56309=CARTESIAN_POINT('Ctrl Pts',(-26.4974289986125,20.9459023492412,-49.6352042905911));
#56310=CARTESIAN_POINT('Ctrl Pts',(-26.4205915724017,20.8589503503001,-49.6293527854488));
#56311=CARTESIAN_POINT('Ctrl Pts',(-26.339911539517,20.7754115584539,-49.6235012803065));
#56312=CARTESIAN_POINT('Ctrl Pts',(-26.2557335225697,20.6956314345937,-49.6176497751642));
#56313=CARTESIAN_POINT('Ctrl Pts',(-26.1715275519354,20.6158248174911,-49.6117963268645));
#56314=CARTESIAN_POINT('Ctrl Pts',(-26.0838215873411,20.5397796344981,-49.6059428785647));
#56315=CARTESIAN_POINT('Ctrl Pts',(-25.9929948417721,20.4678023688278,-49.6000894302649));
#56316=CARTESIAN_POINT('Ctrl Pts',(-25.9020648064708,20.3957432493769,-49.5942293253234));
#56317=CARTESIAN_POINT('Ctrl Pts',(-25.8080072306637,20.3277615377149,-49.5883692203818));
#56318=CARTESIAN_POINT('Ctrl Pts',(-25.7112320163825,20.2641215746634,-49.5825091154403));
#56319=CARTESIAN_POINT('Ctrl Pts',(-25.6143916300514,20.2004387540798,-49.5766450640848));
#56320=CARTESIAN_POINT('Ctrl Pts',(-25.5148303152712,20.1411037152761,-49.5707810127294));
#56321=CARTESIAN_POINT('Ctrl Pts',(-25.4129828486518,20.0863349855787,-49.5649169613739));
#56322=CARTESIAN_POINT('Ctrl Pts',(-25.3109852791974,20.0314855377067,-49.5590442675774));
#56323=CARTESIAN_POINT('Ctrl Pts',(-25.206695204351,19.9812160091992,-49.5531715737808));
#56324=CARTESIAN_POINT('Ctrl Pts',(-25.1005677120735,19.9356969792804,-49.5472988799842));
#56325=CARTESIAN_POINT('Ctrl Pts',(-25.0715117799823,19.9232346303283,-49.5456910346608));
#56326=CARTESIAN_POINT('Ctrl Pts',(-25.0423182071403,19.9111280771821,-49.5440831893374));
#56327=CARTESIAN_POINT('Ctrl Pts',(-25.0129965121013,19.8993801636453,-49.542475344014));
#56328=CARTESIAN_POINT('Ctrl Pts',(-24.9059055510578,19.8564735257707,-49.5366030470453));
#56329=CARTESIAN_POINT('Ctrl Pts',(-24.7967457138194,19.8182109479283,-49.5307307500766));
#56330=CARTESIAN_POINT('Ctrl Pts',(-24.685957309616,19.7847958983753,-49.5248584531079));
#56331=CARTESIAN_POINT('Ctrl Pts',(-24.5753124783859,19.7514241520727,-49.5189937661697));
#56332=CARTESIAN_POINT('Ctrl Pts',(-24.4630436693248,19.7228875596612,-49.5131290792315));
#56333=CARTESIAN_POINT('Ctrl Pts',(-24.3496113922415,19.699341676836,-49.5072643922933));
#56334=CARTESIAN_POINT('Ctrl Pts',(-24.2362957731543,19.6758200094774,-49.5014057368185));
#56335=CARTESIAN_POINT('Ctrl Pts',(-24.1218194683739,19.6572789261479,-49.4955470813437));
#56336=CARTESIAN_POINT('Ctrl Pts',(-24.0066577404742,19.6438240752396,-49.4896884258689));
#56337=CARTESIAN_POINT('Ctrl Pts',(-23.8869976940492,19.6298436660039,-49.483600926151));
#56338=CARTESIAN_POINT('Ctrl Pts',(-23.7665980217507,19.6213550662404,-49.477513426433));
#56339=CARTESIAN_POINT('Ctrl Pts',(-23.6460034933658,19.6184182583125,-49.4714259267151));
#56340=CARTESIAN_POINT('Ctrl Pts',(-23.5300768329011,19.6155951257868,-49.4655740566318));
#56341=CARTESIAN_POINT('Ctrl Pts',(-23.4139705723056,19.6179019998154,-49.4597221865484));
#56342=CARTESIAN_POINT('Ctrl Pts',(-23.2981726181708,19.6253391928805,-49.453870316465));
#56343=CARTESIAN_POINT('Ctrl Pts',(-23.1823922953274,19.6327752535653,-49.448019337382));
#56344=CARTESIAN_POINT('Ctrl Pts',(-23.0669205980278,19.6453400536469,-49.4421683582991));
#56345=CARTESIAN_POINT('Ctrl Pts',(-22.9522428468135,19.6629818417642,-49.4363173792161));
#56346=CARTESIAN_POINT('Ctrl Pts',(-22.8375547849657,19.6806252160481,-49.4304658740738));
#56347=CARTESIAN_POINT('Ctrl Pts',(-22.7236612197076,19.7033464229298,-49.4246143689316));
#56348=CARTESIAN_POINT('Ctrl Pts',(-22.611039076214,19.7310422618812,-49.4187628637893));
#56349=CARTESIAN_POINT('Ctrl Pts',(-22.4983795333581,19.7587472980178,-49.4129094154895));
#56350=CARTESIAN_POINT('Ctrl Pts',(-22.3869926530182,19.7914301523915,-49.4070559671897));
#56351=CARTESIAN_POINT('Ctrl Pts',(-22.2773412653584,19.8289374539246,-49.40120251889));
#56352=CARTESIAN_POINT('Ctrl Pts',(-22.1675651802605,19.8664874094041,-49.3953424139485));
#56353=CARTESIAN_POINT('Ctrl Pts',(-22.0595289185181,19.9088726289492,-49.3894823090069));
#56354=CARTESIAN_POINT('Ctrl Pts',(-21.9536764439244,19.9558911425234,-49.3836222040654));
#56355=CARTESIAN_POINT('Ctrl Pts',(-21.8477526843142,20.0029413201238,-49.37775815271));
#56356=CARTESIAN_POINT('Ctrl Pts',(-21.7440160092884,20.0546308208483,-49.3718941013545));
#56357=CARTESIAN_POINT('Ctrl Pts',(-21.6428852847426,20.1107119831243,-49.3660300499991));
#56358=CARTESIAN_POINT('Ctrl Pts',(-21.5416055136963,20.1668757978387,-49.3601573562026));
#56359=CARTESIAN_POINT('Ctrl Pts',(-21.4429397093039,20.2274439763767,-49.354284662406));
#56360=CARTESIAN_POINT('Ctrl Pts',(-21.347277377064,20.2921258509032,-49.3484119686095));
#56361=CARTESIAN_POINT('Ctrl Pts',(-21.3210866307305,20.309834666154,-49.346804123286));
#56362=CARTESIAN_POINT('Ctrl Pts',(-21.2951208207174,20.3278516035943,-49.3451962779626));
#56363=CARTESIAN_POINT('Ctrl Pts',(-21.269387484746,20.3461701923012,-49.3435884326392));
#56364=CARTESIAN_POINT('Ctrl Pts',(-21.1754022060517,20.4130747579131,-49.3377161356705));
#56365=CARTESIAN_POINT('Ctrl Pts',(-21.0842057376923,20.484230215103,-49.3318438387018));
#56366=CARTESIAN_POINT('Ctrl Pts',(-20.9962072667315,20.5593761075467,-49.3259715417331));
#56367=CARTESIAN_POINT('Ctrl Pts',(-20.9083228348004,20.6344246168817,-49.3201068547949));
#56368=CARTESIAN_POINT('Ctrl Pts',(-20.8236284701001,20.7134530116684,-49.3142421678567));
#56369=CARTESIAN_POINT('Ctrl Pts',(-20.7425039693215,20.7961579417257,-49.3083774809185));
#56370=CARTESIAN_POINT('Ctrl Pts',(-20.6614629000135,20.8787778149397,-49.3025188254436));
#56371=CARTESIAN_POINT('Ctrl Pts',(-20.5839846797925,20.9650664093115,-49.2966601699688));
#56372=CARTESIAN_POINT('Ctrl Pts',(-20.5104150919925,21.054680985898,-49.290801514494));
#56373=CARTESIAN_POINT('Ctrl Pts',(-20.4339718112937,21.1477959867776,-49.2847140147761));
#56374=CARTESIAN_POINT('Ctrl Pts',(-20.3617490829071,21.2445018031483,-49.2786265150582));
#56375=CARTESIAN_POINT('Ctrl Pts',(-20.2940918421659,21.3443725340582,-49.2725390153403));
#56376=CARTESIAN_POINT('Ctrl Pts',(-20.2290534189436,21.4403775557422,-49.2666871452569));
#56377=CARTESIAN_POINT('Ctrl Pts',(-20.1682338748234,21.5393066640488,-49.2608352751735));
#56378=CARTESIAN_POINT('Ctrl Pts',(-20.1118972068984,21.640749543886,-49.2549834050901));
#56379=CARTESIAN_POINT('Ctrl Pts',(-20.0555691167434,21.7421769781224,-49.2491324260071));
#56380=CARTESIAN_POINT('Ctrl Pts',(-20.0037227462841,21.8461170615773,-49.2432814469241));
#56381=CARTESIAN_POINT('Ctrl Pts',(-19.9565768925592,21.9521335121317,-49.2374304678412));
#56382=CARTESIAN_POINT('Ctrl Pts',(-19.9094267999683,22.0581594945852,-49.2315789626989));
#56383=CARTESIAN_POINT('Ctrl Pts',(-19.866978232227,22.1662618375114,-49.2257274575566));
#56384=CARTESIAN_POINT('Ctrl Pts',(-19.8294021632746,22.2759835114981,-49.2198759524143));
#56385=CARTESIAN_POINT('Ctrl Pts',(-19.7918136161277,22.3857416216642,-49.2140225041145));
#56386=CARTESIAN_POINT('Ctrl Pts',(-19.7591009190245,22.4971197412845,-49.2081690558147));
#56387=CARTESIAN_POINT('Ctrl Pts',(-19.7313852176287,22.609645580007,-49.202315607515));
#56388=CARTESIAN_POINT('Ctrl Pts',(-19.7036379974621,22.7222993850426,-49.1964555025734));
#56389=CARTESIAN_POINT('Ctrl Pts',(-19.6808992143611,22.836103112707,-49.1905953976319));
#56390=CARTESIAN_POINT('Ctrl Pts',(-19.6632389287966,22.950574075445,-49.1847352926903));
#56391=CARTESIAN_POINT('Ctrl Pts',(-19.6455667501352,23.065122127212,-49.1788712413349));
#56392=CARTESIAN_POINT('Ctrl Pts',(-19.6329799237928,23.1803378988461,-49.1730071899794));
#56393=CARTESIAN_POINT('Ctrl Pts',(-19.6254965027066,23.2957351198625,-49.167143138624));
#56394=CARTESIAN_POINT('Ctrl Pts',(-19.6180020525515,23.4113024133472,-49.1612704448274));
#56395=CARTESIAN_POINT('Ctrl Pts',(-19.6156260273691,23.5270512781892,-49.1553977510308));
#56396=CARTESIAN_POINT('Ctrl Pts',(-19.6183344276671,23.64249689859,-49.1495250572343));
#56397=CARTESIAN_POINT('Ctrl Pts',(-19.6190759423627,23.6741039782867,-49.1479172119109));
#56398=CARTESIAN_POINT('Ctrl Pts',(-19.6201982730429,23.7056883683887,-49.1463093665876));
#56399=CARTESIAN_POINT('Ctrl Pts',(-19.6217000500697,23.7372402294764,-49.1447015212642));
#56400=CARTESIAN_POINT('Ctrl Pts',(-19.6271849562072,23.8524763753493,-49.1388292242955));
#56401=CARTESIAN_POINT('Ctrl Pts',(-19.637753678964,23.9676640354022,-49.1329569273268));
#56402=CARTESIAN_POINT('Ctrl Pts',(-19.653408275019,24.082318166008,-49.1270846303581));
#56403=CARTESIAN_POINT('Ctrl Pts',(-19.6690425839608,24.1968237139662,-49.1212199434199));
#56404=CARTESIAN_POINT('Ctrl Pts',(-19.6897496038834,24.3107967016452,-49.1153552564817));
#56405=CARTESIAN_POINT('Ctrl Pts',(-19.7154794174018,24.4237536260841,-49.1094905695435));
#56406=CARTESIAN_POINT('Ctrl Pts',(-19.7411827694178,24.5365943813974,-49.1036319140686));
#56407=CARTESIAN_POINT('Ctrl Pts',(-19.7718985490698,24.6484207513093,-49.0977732585938));
#56408=CARTESIAN_POINT('Ctrl Pts',(-19.8075253148856,24.7587565575709,-49.091914603119));
#56409=CARTESIAN_POINT('Ctrl Pts',(-19.8445436935537,24.8734021776075,-49.0858271034011));
#56410=CARTESIAN_POINT('Ctrl Pts',(-19.8868644729888,24.9864379641687,-49.0797396036832));
#56411=CARTESIAN_POINT('Ctrl Pts',(-19.9343157877445,25.0973434998517,-49.0736521039653));
#56412=CARTESIAN_POINT('Ctrl Pts',(-19.9799303983572,25.2039562007014,-49.0678002338819));
#56413=CARTESIAN_POINT('Ctrl Pts',(-20.0302855751122,25.3086000805575,-49.0619483637985));
#56414=CARTESIAN_POINT('Ctrl Pts',(-20.0851788146588,25.4108312415343,-49.0560964937151));
#56415=CARTESIAN_POINT('Ctrl Pts',(-20.1400636962105,25.5130468368873,-49.0502455146321));
#56416=CARTESIAN_POINT('Ctrl Pts',(-20.1994850711967,25.6128500796862,-49.0443945355491));
#56417=CARTESIAN_POINT('Ctrl Pts',(-20.2631941572255,25.7098210633308,-49.0385435564661));
#56418=CARTESIAN_POINT('Ctrl Pts',(-20.3269089713142,25.8068007656001,-49.0326920513238));
#56419=CARTESIAN_POINT('Ctrl Pts',(-20.3949120357993,25.9009473569887,-49.0268405461815));
#56420=CARTESIAN_POINT('Ctrl Pts',(-20.4669112628304,25.9918699504807,-49.0209890410392));
#56421=CARTESIAN_POINT('Ctrl Pts',(-20.5389343992375,26.0828227373867,-49.0151355927394));
#56422=CARTESIAN_POINT('Ctrl Pts',(-20.6149560804299,26.1705490736297,-49.0092821444397));
#56423=CARTESIAN_POINT('Ctrl Pts',(-20.6946444449772,26.2546917443733,-49.0034286961399));
#56424=CARTESIAN_POINT('Ctrl Pts',(-20.774423432499,26.3389301036048,-48.9975685911984));
#56425=CARTESIAN_POINT('Ctrl Pts',(-20.8578771417787,26.4195763626296,-48.9917084862568));
#56426=CARTESIAN_POINT('Ctrl Pts',(-20.9446373503323,26.4963106653121,-48.9858483813153));
#56427=CARTESIAN_POINT('Ctrl Pts',(-21.0314559864561,26.5730966437448,-48.9799843299598));
#56428=CARTESIAN_POINT('Ctrl Pts',(-21.1215852350192,26.6459651608429,-48.9741202786043));
#56429=CARTESIAN_POINT('Ctrl Pts',(-21.2146257468817,26.7146381785562,-48.9682562272489));
#56430=CARTESIAN_POINT('Ctrl Pts',(-21.307803381886,26.7834124065892,-48.9623835334523));
#56431=CARTESIAN_POINT('Ctrl Pts',(-21.4039005016028,26.8479785648305,-48.9565108396557));
#56432=CARTESIAN_POINT('Ctrl Pts',(-21.5024908441997,26.9081031941313,-48.9506381458592));
#56433=CARTESIAN_POINT('Ctrl Pts',(-21.5294832307866,26.924564311871,-48.9490303005359));
#56434=CARTESIAN_POINT('Ctrl Pts',(-21.5566623754204,26.9406927780457,-48.9474224552126));
#56435=CARTESIAN_POINT('Ctrl Pts',(-21.5840192596848,26.9564844263313,-48.9458146098894));
#56436=CARTESIAN_POINT('Ctrl Pts',(-21.6839341869571,27.0141599048219,-48.9399423129207));
#56437=CARTESIAN_POINT('Ctrl Pts',(-21.7865563406964,27.067532074452,-48.934070015952));
#56438=CARTESIAN_POINT('Ctrl Pts',(-21.8914787572833,27.1163370182602,-48.9281977189833));
#56439=CARTESIAN_POINT('Ctrl Pts',(-21.9962652027512,27.1650787147373,-48.9223330320451));
#56440=CARTESIAN_POINT('Ctrl Pts',(-22.1033456116534,27.2092647829473,-48.9164683451069));
#56441=CARTESIAN_POINT('Ctrl Pts',(-22.2122862223738,27.2486758653762,-48.9106036581687));
#56442=CARTESIAN_POINT('Ctrl Pts',(-22.3211147944957,27.288046415974,-48.9047450026939));
#56443=CARTESIAN_POINT('Ctrl Pts',(-22.4317993767891,27.3226516087894,-48.8988863472191));
#56444=CARTESIAN_POINT('Ctrl Pts',(-22.5438845190874,27.3523193937051,-48.8930276917442));
#56445=CARTESIAN_POINT('Ctrl Pts',(-22.6603478057673,27.3831460284308,-48.8869401920263));
#56446=CARTESIAN_POINT('Ctrl Pts',(-22.7783228849336,27.4086414811871,-48.8808526923084));
#56447=CARTESIAN_POINT('Ctrl Pts',(-22.8972790201337,27.4286690375894,-48.8747651925905));
#56448=CARTESIAN_POINT('Ctrl Pts',(-23.0116307049094,27.4479213847902,-48.8689133225071));
#56449=CARTESIAN_POINT('Ctrl Pts',(-23.1268884645165,27.4621211829458,-48.8630614524237));
#56450=CARTESIAN_POINT('Ctrl Pts',(-23.2425693785703,27.4711988558975,-48.8572095823403));
#56451=CARTESIAN_POINT('Ctrl Pts',(-23.358232679153,27.480275146691,-48.8513586032574));
#56452=CARTESIAN_POINT('Ctrl Pts',(-23.474318594074,27.4842308306213,-48.8455076241744));
#56453=CARTESIAN_POINT('Ctrl Pts',(-23.5903393714356,27.4830482351702,-48.8396566450915));
#56454=CARTESIAN_POINT('Ctrl Pts',(-23.7063705801816,27.4818655333925,-48.8338051399492));
#56455=CARTESIAN_POINT('Ctrl Pts',(-23.8223362263402,27.4755436380719,-48.8279536348069));
#56456=CARTESIAN_POINT('Ctrl Pts',(-23.9377495642408,27.4641169966147,-48.8221021296646));
#56457=CARTESIAN_POINT('Ctrl Pts',(-24.0532012283986,27.4526865606186,-48.8162486813648));
#56458=CARTESIAN_POINT('Ctrl Pts',(-24.1680998084462,27.4361480484437,-48.810395233065));
#56459=CARTESIAN_POINT('Ctrl Pts',(-24.2819653883767,27.4145875709171,-48.8045417847653));
#56460=CARTESIAN_POINT('Ctrl Pts',(-24.3959604581968,27.3930025744457,-48.7986816798237));
#56461=CARTESIAN_POINT('Ctrl Pts',(-24.5089197767366,27.3663842904624,-48.7928215748822));
#56462=CARTESIAN_POINT('Ctrl Pts',(-24.6203752037998,27.3348696149201,-48.7869614699407));
#56463=CARTESIAN_POINT('Ctrl Pts',(-24.7319056891174,27.3033337162163,-48.7810974185852));
#56464=CARTESIAN_POINT('Ctrl Pts',(-24.8419298748564,27.2668949897968,-48.7752333672298));
#56465=CARTESIAN_POINT('Ctrl Pts',(-24.9499979778003,27.2257391234403,-48.7693693158743));
#56466=CARTESIAN_POINT('Ctrl Pts',(-25.0582253515555,27.1845226015523,-48.7634966220778));
#56467=CARTESIAN_POINT('Ctrl Pts',(-25.1644905108437,27.1385752280766,-48.7576239282812));
#56468=CARTESIAN_POINT('Ctrl Pts',(-25.2683666299751,27.0881294296781,-48.7517512344847));
#56469=CARTESIAN_POINT('Ctrl Pts',(-25.2968061737587,27.0743182139314,-48.7501433891613));
#56470=CARTESIAN_POINT('Ctrl Pts',(-25.3250668028408,27.0601700632334,-48.7485355438379));
#56471=CARTESIAN_POINT('Ctrl Pts',(-25.353140137187,27.0456903128542,-48.7469276985145));
#56472=CARTESIAN_POINT('Ctrl Pts',(-25.4556717388197,26.9928062493039,-48.7410554015458));
#56473=CARTESIAN_POINT('Ctrl Pts',(-25.5560462651788,26.9353184298351,-48.7351831045771));
#56474=CARTESIAN_POINT('Ctrl Pts',(-25.6538216974083,26.873426581463,-48.7293108076084));
#56475=CARTESIAN_POINT('Ctrl Pts',(-25.7514704204429,26.811614940011,-48.7234461206702));
#56476=CARTESIAN_POINT('Ctrl Pts',(-25.8465264014651,26.745410838428,-48.717581433732));
#56477=CARTESIAN_POINT('Ctrl Pts',(-25.9385706247761,26.6750606356036,-48.7117167467938));
#56478=CARTESIAN_POINT('Ctrl Pts',(-26.0305201863655,26.6047827835588,-48.705858091319));
#56479=CARTESIAN_POINT('Ctrl Pts',(-26.1194638246777,26.530367561117,-48.6999994358442));
#56480=CARTESIAN_POINT('Ctrl Pts',(-26.2050106009395,26.4521051457628,-48.6941407803694));
#56481=CARTESIAN_POINT('Ctrl Pts',(-26.2938989096307,26.3707857315322,-48.6880532806515));
#56482=CARTESIAN_POINT('Ctrl Pts',(-26.3791191934116,26.2853126910584,-48.6819657809336));
#56483=CARTESIAN_POINT('Ctrl Pts',(-26.4602695466242,26.1960586419029,-48.6758782812157));
#56484=CARTESIAN_POINT('Ctrl Pts',(-26.5382788026781,26.1102593607073,-48.6700264111323));
#56485=CARTESIAN_POINT('Ctrl Pts',(-26.6125270363051,26.0209666666019,-48.6641745410489));
#56486=CARTESIAN_POINT('Ctrl Pts',(-26.6826946729749,25.9285492397458,-48.6583226709655));
#56487=CARTESIAN_POINT('Ctrl Pts',(-26.7528516259839,25.8361458842832,-48.6524716918825));
#56488=CARTESIAN_POINT('Ctrl Pts',(-26.8189289674899,25.7406190711998,-48.6466207127995));
#56489=CARTESIAN_POINT('Ctrl Pts',(-26.8806481787288,25.6423696016052,-48.6407697337166));
#56490=CARTESIAN_POINT('Ctrl Pts',(-26.9423729391188,25.5441112984377,-48.6349182285743));
#56491=CARTESIAN_POINT('Ctrl Pts',(-26.9997385703967,25.4431302021994,-48.629066723432));
#56492=CARTESIAN_POINT('Ctrl Pts',(-27.0525109470736,25.3398544404728,-48.6232152182897));
#56493=CARTESIAN_POINT('Ctrl Pts',(-27.1053008483081,25.2365443831139,-48.6173617699899));
#56494=CARTESIAN_POINT('Ctrl Pts',(-27.1534942739404,25.1309385129752,-48.6115083216901));
#56495=CARTESIAN_POINT('Ctrl Pts',(-27.1969042555072,25.0234871379983,-48.6056548733904));
#56496=CARTESIAN_POINT('Ctrl Pts',(-27.2403636036492,24.9159135674754,-48.5997947684488));
#56497=CARTESIAN_POINT('Ctrl Pts',(-27.2790284950821,24.8064906866064,-48.5939346635073));
#56498=CARTESIAN_POINT('Ctrl Pts',(-27.3127610530459,24.695686347659,-48.5880745585658));
#56499=CARTESIAN_POINT('Ctrl Pts',(-27.3465163277763,24.5848073889242,-48.5822105072103));
#56500=CARTESIAN_POINT('Ctrl Pts',(-27.3753325525098,24.4725455190721,-48.5763464558549));
#56501=CARTESIAN_POINT('Ctrl Pts',(-27.3991228225941,24.3593795203853,-48.5704824044994));
#56502=CARTESIAN_POINT('Ctrl Pts',(-27.4229481547874,24.2460467376067,-48.5646097107029));
#56503=CARTESIAN_POINT('Ctrl Pts',(-27.4417326820611,24.1318075729435,-48.5587370169063));
#56504=CARTESIAN_POINT('Ctrl Pts',(-27.4554412314881,24.0171467584755,-48.5528643231097));
#56505=CARTESIAN_POINT('Ctrl Pts',(-27.4591944030053,23.9857545455146,-48.5512564777864));
#56506=CARTESIAN_POINT('Ctrl Pts',(-27.4625673945139,23.9543307288691,-48.549648632463));
#56507=CARTESIAN_POINT('Ctrl Pts',(-27.4655601649022,23.9228852427422,-48.5480407871396));
#56508=CARTESIAN_POINT('Ctrl Pts',(-27.4772725933714,23.7998210048773,-48.541748365438));
#56509=CARTESIAN_POINT('Ctrl Pts',(-27.4831841036996,23.6761959820669,-48.5354559437363));
#56510=CARTESIAN_POINT('Ctrl Pts',(-27.4832519411198,23.5524078640301,-48.5291635220346));
#56511=CARTESIAN_POINT('',(-27.4815091528986,23.5526679104256,-47.2791640449873));
#56512=CARTESIAN_POINT('Ctrl Pts',(-27.4882898507423,23.5523757766641,-48.5291617528909));
#56513=CARTESIAN_POINT('Ctrl Pts',(-27.4804866516216,22.3704529683091,-48.4691591271821));
#56514=CARTESIAN_POINT('Ctrl Pts',(-26.2851771232687,19.8689985368499,-48.3428608643485));
#56515=CARTESIAN_POINT('Ctrl Pts',(-22.0263435048847,19.154976418624,-48.1502669643898));
#56516=CARTESIAN_POINT('Ctrl Pts',(-19.0286955606611,22.456509696377,-47.9513800530149));
#56517=CARTESIAN_POINT('Ctrl Pts',(-20.1859751080046,26.7630999056849,-47.75249314164));
#56518=CARTESIAN_POINT('Ctrl Pts',(-24.4347403640322,28.117355782832,-47.5536062302651));
#56519=CARTESIAN_POINT('Ctrl Pts',(-27.1604995493759,25.8623944274898,-47.3958301919578));
#56520=CARTESIAN_POINT('Ctrl Pts',(-27.4810072727968,24.0520277401451,-47.3043497907753));
#56521=CARTESIAN_POINT('Ctrl Pts',(-27.4782377188801,23.5526853739332,-47.2791650267177));
#56522=CARTESIAN_POINT('',(-27.4821351592969,23.5471947449596,-46.0291630887908));
#56523=CARTESIAN_POINT('Ctrl Pts',(-27.4832517957162,23.5526586078825,-47.2791635220346));
#56524=CARTESIAN_POINT('Ctrl Pts',(-27.4833234694447,23.4354999231549,-47.273262034116));
#56525=CARTESIAN_POINT('Ctrl Pts',(-27.478155809776,23.3183245754339,-47.2673605461975));
#56526=CARTESIAN_POINT('Ctrl Pts',(-27.4677709458428,23.2016288451683,-47.2614590582789));
#56527=CARTESIAN_POINT('Ctrl Pts',(-27.4573847051595,23.0849176442282,-47.2555567879838));
#56528=CARTESIAN_POINT('Ctrl Pts',(-27.4417799191657,22.9686865891467,-47.2496545176888));
#56529=CARTESIAN_POINT('Ctrl Pts',(-27.4210306059043,22.8534268000984,-47.2437522473937));
#56530=CARTESIAN_POINT('Ctrl Pts',(-27.4002738442678,22.7381256362763,-47.2378478583623));
#56531=CARTESIAN_POINT('Ctrl Pts',(-27.3743689516746,22.6237968291915,-47.2319434693309));
#56532=CARTESIAN_POINT('Ctrl Pts',(-27.3434409454458,22.5109206993227,-47.2260390802996));
#56533=CARTESIAN_POINT('Ctrl Pts',(-27.3124724484287,22.3978967925995,-47.2201269612722));
#56534=CARTESIAN_POINT('Ctrl Pts',(-27.2764678083027,22.286329751818,-47.2142148422447));
#56535=CARTESIAN_POINT('Ctrl Pts',(-27.2356019212984,22.1766845950621,-47.2083027232173));
#56536=CARTESIAN_POINT('Ctrl Pts',(-27.1947089385844,22.066966739203,-47.2023866842196));
#56537=CARTESIAN_POINT('Ctrl Pts',(-27.1489484441694,21.9591736775379,-47.196470645222));
#56538=CARTESIAN_POINT('Ctrl Pts',(-27.0985427249335,21.8537485663107,-47.1905546062243));
#56539=CARTESIAN_POINT('Ctrl Pts',(-27.0480436648253,21.7481282297798,-47.1846276119571));
#56540=CARTESIAN_POINT('Ctrl Pts',(-26.9928823794142,21.6448849629928,-47.1787006176899));
#56541=CARTESIAN_POINT('Ctrl Pts',(-26.9333265762987,21.5444362368349,-47.1727736234227));
#56542=CARTESIAN_POINT('Ctrl Pts',(-26.876583496888,21.4487315406185,-47.1671265514536));
#56543=CARTESIAN_POINT('Ctrl Pts',(-26.8158517014826,21.3555636795958,-47.1614794794845));
#56544=CARTESIAN_POINT('Ctrl Pts',(-26.751396921784,21.2652659685397,-47.1558324075154));
#56545=CARTESIAN_POINT('Ctrl Pts',(-26.6843714598259,21.1713668686499,-47.1499601105467));
#56546=CARTESIAN_POINT('Ctrl Pts',(-26.6130986987919,21.0802620473527,-47.144087813578));
#56547=CARTESIAN_POINT('Ctrl Pts',(-26.5378396213827,20.9923603561859,-47.1382155166093));
#56548=CARTESIAN_POINT('Ctrl Pts',(-26.4626780737607,20.9045725786297,-47.1323508296712));
#56549=CARTESIAN_POINT('Ctrl Pts',(-26.3835407493514,20.8199799874659,-47.126486142733));
#56550=CARTESIAN_POINT('Ctrl Pts',(-26.3007314868534,20.7389619886826,-47.1206214557948));
#56551=CARTESIAN_POINT('Ctrl Pts',(-26.2180073884982,20.6580273118395,-47.11476280032));
#56552=CARTESIAN_POINT('Ctrl Pts',(-26.1316191571331,20.5806602024921,-47.1089041448452));
#56553=CARTESIAN_POINT('Ctrl Pts',(-26.0419099764137,20.5072060026096,-47.1030454893704));
#56554=CARTESIAN_POINT('Ctrl Pts',(-25.94869667608,20.4308826169815,-47.0969579896525));
#56555=CARTESIAN_POINT('Ctrl Pts',(-25.8518979947514,20.3587844012713,-47.0908704899346));
#56556=CARTESIAN_POINT('Ctrl Pts',(-25.7519402769323,20.2912557424248,-47.0847829902167));
#56557=CARTESIAN_POINT('Ctrl Pts',(-25.6558516353529,20.2263409240615,-47.0789311201333));
#56558=CARTESIAN_POINT('Ctrl Pts',(-25.556844338942,20.165648744379,-47.0730792500499));
#56559=CARTESIAN_POINT('Ctrl Pts',(-25.4553290421953,20.1094426722081,-47.0672273799665));
#56560=CARTESIAN_POINT('Ctrl Pts',(-25.3538292020755,20.0532451579226,-47.0613764008836));
#56561=CARTESIAN_POINT('Ctrl Pts',(-25.2498224824428,20.001532593206,-47.0555254218006));
#56562=CARTESIAN_POINT('Ctrl Pts',(-25.1437454466297,19.9545232134543,-47.0496744427177));
#56563=CARTESIAN_POINT('Ctrl Pts',(-25.0376588734705,19.907509607107,-47.0438229375754));
#56564=CARTESIAN_POINT('Ctrl Pts',(-24.9295019920551,19.8652001938305,-47.0379714324331));
#56565=CARTESIAN_POINT('Ctrl Pts',(-24.8197320514474,19.8277653592613,-47.0321199272909));
#56566=CARTESIAN_POINT('Ctrl Pts',(-24.7099256586321,19.7903180933985,-47.0262664789911));
#56567=CARTESIAN_POINT('Ctrl Pts',(-24.5985055325443,19.7577487583681,-47.0204130306914));
#56568=CARTESIAN_POINT('Ctrl Pts',(-24.4859441190497,19.7301778919323,-47.0145595823916));
#56569=CARTESIAN_POINT('Ctrl Pts',(-24.3732546987856,19.7025756714344,-47.0086994774501));
#56570=CARTESIAN_POINT('Ctrl Pts',(-24.2594218023143,19.6799833637158,-47.0028393725086));
#56571=CARTESIAN_POINT('Ctrl Pts',(-24.1449282069534,19.6624704080079,-46.9969792675671));
#56572=CARTESIAN_POINT('Ctrl Pts',(-24.030357507322,19.6449456584204,-46.9911152162117));
#56573=CARTESIAN_POINT('Ctrl Pts',(-23.9151256328295,19.6325071162445,-46.9852511648562));
#56574=CARTESIAN_POINT('Ctrl Pts',(-23.799718876791,19.6251722086098,-46.9793871135008));
#56575=CARTESIAN_POINT('Ctrl Pts',(-23.6841420342313,19.6178264907855,-46.9735144197042));
#56576=CARTESIAN_POINT('Ctrl Pts',(-23.5683902074797,19.6155994273635,-46.9676417259077));
#56577=CARTESIAN_POINT('Ctrl Pts',(-23.4529481681787,19.6184563949596,-46.9617690321111));
#56578=CARTESIAN_POINT('Ctrl Pts',(-23.4213420689235,19.6192385848963,-46.9601611867876));
#56579=CARTESIAN_POINT('Ctrl Pts',(-23.3897591493249,19.6204015613025,-46.9585533414641));
#56580=CARTESIAN_POINT('Ctrl Pts',(-23.3582092470315,19.621943941879,-46.9569454961405));
#56581=CARTESIAN_POINT('Ctrl Pts',(-23.242980255232,19.6275771434383,-46.9510731991718));
#56582=CARTESIAN_POINT('Ctrl Pts',(-23.1278062916893,19.6382940950095,-46.9452009022031));
#56583=CARTESIAN_POINT('Ctrl Pts',(-23.0131724022755,19.6540962290565,-46.9393286052344));
#56584=CARTESIAN_POINT('Ctrl Pts',(-22.898687069278,19.6698778847927,-46.9334639182962));
#56585=CARTESIAN_POINT('Ctrl Pts',(-22.7847408243035,19.6907315619455,-46.927599231358));
#56586=CARTESIAN_POINT('Ctrl Pts',(-22.6718171056727,19.7166067209404,-46.9217345444197));
#56587=CARTESIAN_POINT('Ctrl Pts',(-22.5590095220178,19.742455268954,-46.9158758889449));
#56588=CARTESIAN_POINT('Ctrl Pts',(-22.4472227735291,19.7733149350178,-46.9100172334701));
#56589=CARTESIAN_POINT('Ctrl Pts',(-22.3369329075138,19.809083664939,-46.9041585779953));
#56590=CARTESIAN_POINT('Ctrl Pts',(-22.2223350221898,19.8462495529556,-46.8980710782774));
#56591=CARTESIAN_POINT('Ctrl Pts',(-22.1093537927857,19.8887157656178,-46.8919835785595));
#56592=CARTESIAN_POINT('Ctrl Pts',(-21.998509415096,19.9363097678848,-46.8858960788416));
#56593=CARTESIAN_POINT('Ctrl Pts',(-21.8919555049896,19.9820615429849,-46.8800442087582));
#56594=CARTESIAN_POINT('Ctrl Pts',(-21.7873765149867,20.032551346582,-46.8741923386748));
#56595=CARTESIAN_POINT('Ctrl Pts',(-21.6852160819991,20.0875761042311,-46.8683404685914));
#56596=CARTESIAN_POINT('Ctrl Pts',(-21.5830712038666,20.1425924838604,-46.8624894895084));
#56597=CARTESIAN_POINT('Ctrl Pts',(-21.483344514405,20.2021422486573,-46.8566385104255));
#56598=CARTESIAN_POINT('Ctrl Pts',(-21.3864555997031,20.2659760760489,-46.8507875313425));
#56599=CARTESIAN_POINT('Ctrl Pts',(-21.2895579737555,20.3298156427158,-46.8449360262002));
#56600=CARTESIAN_POINT('Ctrl Pts',(-21.1954989749873,20.3979398102345,-46.8390845210579));
#56601=CARTESIAN_POINT('Ctrl Pts',(-21.1046691141967,20.4700559879553,-46.8332330159157));
#56602=CARTESIAN_POINT('Ctrl Pts',(-21.0138090907866,20.5421961138888,-46.8273795676159));
#56603=CARTESIAN_POINT('Ctrl Pts',(-20.926180661184,20.6183306291052,-46.8215261193161));
#56604=CARTESIAN_POINT('Ctrl Pts',(-20.8421406128498,20.6981272127412,-46.8156726710164));
#56605=CARTESIAN_POINT('Ctrl Pts',(-20.7580049927315,20.7780145424204,-46.8098125660748));
#56606=CARTESIAN_POINT('Ctrl Pts',(-20.6774661989265,20.8615719680608,-46.8039524611333));
#56607=CARTESIAN_POINT('Ctrl Pts',(-20.6008436134321,20.9484308558532,-46.7980923561918));
#56608=CARTESIAN_POINT('Ctrl Pts',(-20.524169427422,21.0353482376702,-46.7922283048363));
#56609=CARTESIAN_POINT('Ctrl Pts',(-20.4514169600033,21.1255711877167,-46.7863642534809));
#56610=CARTESIAN_POINT('Ctrl Pts',(-20.3828637350648,21.2186999993701,-46.7805002021254));
#56611=CARTESIAN_POINT('Ctrl Pts',(-20.3142094763573,21.3119660643017,-46.7746275083289));
#56612=CARTESIAN_POINT('Ctrl Pts',(-20.2497670411067,21.4081461960695,-46.7687548145323));
#56613=CARTESIAN_POINT('Ctrl Pts',(-20.1897693397026,21.5068138327502,-46.7628821207357));
#56614=CARTESIAN_POINT('Ctrl Pts',(-20.1733429726966,21.5338273811663,-46.7612742754123));
#56615=CARTESIAN_POINT('Ctrl Pts',(-20.1572494973232,21.561027259378,-46.7596664300889));
#56616=CARTESIAN_POINT('Ctrl Pts',(-20.1414930682971,21.5884044436148,-46.7580585847655));
#56617=CARTESIAN_POINT('Ctrl Pts',(-20.0839462203127,21.6883935120077,-46.7521862877968));
#56618=CARTESIAN_POINT('Ctrl Pts',(-20.0307061616155,21.7910842666017,-46.7463139908281));
#56619=CARTESIAN_POINT('Ctrl Pts',(-19.9820362852176,21.8960694044739,-46.7404416938594));
#56620=CARTESIAN_POINT('Ctrl Pts',(-19.9334294811142,22.0009184899451,-46.7345770069212));
#56621=CARTESIAN_POINT('Ctrl Pts',(-19.8893812536582,22.1080556742114,-46.728712319983));
#56622=CARTESIAN_POINT('Ctrl Pts',(-19.8501104019643,22.21704691372,-46.7228476330448));
#56623=CARTESIAN_POINT('Ctrl Pts',(-19.8108799378831,22.3259260625615,-46.71698897757));
#56624=CARTESIAN_POINT('Ctrl Pts',(-19.7764172161789,22.4366550873923,-46.7111303220952));
#56625=CARTESIAN_POINT('Ctrl Pts',(-19.7468937006977,22.5487783170081,-46.7052716666204));
#56626=CARTESIAN_POINT('Ctrl Pts',(-19.7162169706978,22.6652811787297,-46.6991841669025));
#56627=CARTESIAN_POINT('Ctrl Pts',(-19.690873363812,22.7832889708687,-46.6930966671845));
#56628=CARTESIAN_POINT('Ctrl Pts',(-19.6709989112952,22.9022707814716,-46.6870091674666));
#56629=CARTESIAN_POINT('Ctrl Pts',(-19.6518937417681,23.0166471478292,-46.6811572973832));
#56630=CARTESIAN_POINT('Ctrl Pts',(-19.6378422831501,23.13192308603,-46.6753054272999));
#56631=CARTESIAN_POINT('Ctrl Pts',(-19.6289134900614,23.24761558655,-46.6694535572164));
#56632=CARTESIAN_POINT('Ctrl Pts',(-19.6199860564626,23.3632904718349,-46.6636025781335));
#56633=CARTESIAN_POINT('Ctrl Pts',(-19.6161797693585,23.479381381285,-46.6577515990505));
#56634=CARTESIAN_POINT('Ctrl Pts',(-19.6175116735539,23.5954005406634,-46.6519006199675));
#56635=CARTESIAN_POINT('Ctrl Pts',(-19.6188436975003,23.7114301312808,-46.6460491148252));
#56636=CARTESIAN_POINT('Ctrl Pts',(-19.6253148263598,23.8273875456222,-46.6401976096829));
#56637=CARTESIAN_POINT('Ctrl Pts',(-19.6368899863511,23.9427860827516,-46.6343461045406));
#56638=CARTESIAN_POINT('Ctrl Pts',(-19.648468990201,24.058222941223,-46.6284926562408));
#56639=CARTESIAN_POINT('Ctrl Pts',(-19.6651553542235,24.1731001423452,-46.622639207941));
#56640=CARTESIAN_POINT('Ctrl Pts',(-19.6868623500484,24.2869378813265,-46.6167857596412));
#56641=CARTESIAN_POINT('Ctrl Pts',(-19.7085940314411,24.4009050785363,-46.6109256546997));
#56642=CARTESIAN_POINT('Ctrl Pts',(-19.7353576632463,24.5138300478736,-46.6050655497582));
#56643=CARTESIAN_POINT('Ctrl Pts',(-19.7670157471645,24.6252448257043,-46.5992054448166));
#56644=CARTESIAN_POINT('Ctrl Pts',(-19.7986951508208,24.7367346344149,-46.5933413934611));
#56645=CARTESIAN_POINT('Ctrl Pts',(-19.8352754396424,24.8467118352359,-46.5874773421057));
#56646=CARTESIAN_POINT('Ctrl Pts',(-19.8765703471683,24.9547268842891,-46.5816132907502));
#56647=CARTESIAN_POINT('Ctrl Pts',(-19.9179261151446,25.0629011259627,-46.5757405969536));
#56648=CARTESIAN_POINT('Ctrl Pts',(-19.9640102055735,25.1691070665559,-46.569867903157));
#56649=CARTESIAN_POINT('Ctrl Pts',(-20.0145896426912,25.2729181798473,-46.5639952093605));
#56650=CARTESIAN_POINT('Ctrl Pts',(-20.0284374464825,25.301339926117,-46.5623873640372));
#56651=CARTESIAN_POINT('Ctrl Pts',(-20.0426219546968,25.3295823242243,-46.560779518714));
#56652=CARTESIAN_POINT('Ctrl Pts',(-20.0571378212839,25.3576370010077,-46.5591716733908));
#56653=CARTESIAN_POINT('Ctrl Pts',(-20.1101537912445,25.4601004600558,-46.5532993764221));
#56654=CARTESIAN_POINT('Ctrl Pts',(-20.167770737323,25.5604009209406,-46.5474270794533));
#56655=CARTESIAN_POINT('Ctrl Pts',(-20.2297883638258,25.6580966222051,-46.5415547824846));
#56656=CARTESIAN_POINT('Ctrl Pts',(-20.2917256204098,25.7556657175995,-46.5356900955464));
#56657=CARTESIAN_POINT('Ctrl Pts',(-20.3580519968302,25.8506364203737,-46.5298254086083));
#56658=CARTESIAN_POINT('Ctrl Pts',(-20.4285205951604,25.9425900322207,-46.5239607216701));
#56659=CARTESIAN_POINT('Ctrl Pts',(-20.4989167209491,26.0344490755347,-46.5181020661952));
#56660=CARTESIAN_POINT('Ctrl Pts',(-20.5734463453189,26.1232968735865,-46.5122434107204));
#56661=CARTESIAN_POINT('Ctrl Pts',(-20.651818787918,26.2087428613625,-46.5063847552455));
#56662=CARTESIAN_POINT('Ctrl Pts',(-20.7332525271543,26.2975264446805,-46.5002972555276));
#56663=CARTESIAN_POINT('Ctrl Pts',(-20.8188351687312,26.3826366607314,-46.4942097558097));
#56664=CARTESIAN_POINT('Ctrl Pts',(-20.9081935781745,26.46367208372,-46.4881222560918));
#56665=CARTESIAN_POINT('Ctrl Pts',(-20.9940931801707,26.5415708581688,-46.4822703860084));
#56666=CARTESIAN_POINT('Ctrl Pts',(-21.0834813520403,26.6157041175541,-46.476418515925));
#56667=CARTESIAN_POINT('Ctrl Pts',(-21.1759890026619,26.6857527620732,-46.4705666458416));
#56668=CARTESIAN_POINT('Ctrl Pts',(-21.2684825681527,26.7557907410494,-46.4647156667587));
#56669=CARTESIAN_POINT('Ctrl Pts',(-21.364094338535,26.8217450922534,-46.4588646876757));
#56670=CARTESIAN_POINT('Ctrl Pts',(-21.4624231545989,26.8833378129521,-46.4530137085927));
#56671=CARTESIAN_POINT('Ctrl Pts',(-21.5607608113695,26.9449360714289,-46.4471622034505));
#56672=CARTESIAN_POINT('Ctrl Pts',(-21.6618156490959,27.0021717003803,-46.4413106983082));
#56673=CARTESIAN_POINT('Ctrl Pts',(-21.7651592392486,27.0548111254783,-46.4354591931659));
#56674=CARTESIAN_POINT('Ctrl Pts',(-21.8685371475583,27.1074680309836,-46.4296057448661));
#56675=CARTESIAN_POINT('Ctrl Pts',(-21.9742049514397,27.1555255101603,-46.4237522965663));
#56676=CARTESIAN_POINT('Ctrl Pts',(-22.0817121027105,27.1987971742113,-46.4178988482666));
#56677=CARTESIAN_POINT('Ctrl Pts',(-22.1893415129568,27.2421180475405,-46.412038743325));
#56678=CARTESIAN_POINT('Ctrl Pts',(-22.2988140619247,27.2806420882121,-46.4061786383835));
#56679=CARTESIAN_POINT('Ctrl Pts',(-22.4096617202973,27.3142320216698,-46.4003185334419));
#56680=CARTESIAN_POINT('Ctrl Pts',(-22.5205840276297,27.3478445758453,-46.3944544820865));
#56681=CARTESIAN_POINT('Ctrl Pts',(-22.6328828887608,27.3765163044147,-46.3885904307311));
#56682=CARTESIAN_POINT('Ctrl Pts',(-22.7460794099647,27.4001609189533,-46.3827263793757));
#56683=CARTESIAN_POINT('Ctrl Pts',(-22.8594427602453,27.4238403809339,-46.3768536855791));
#56684=CARTESIAN_POINT('Ctrl Pts',(-22.9737060045358,27.442477875726,-46.3709809917825));
#56685=CARTESIAN_POINT('Ctrl Pts',(-23.0883843658929,27.4560388542443,-46.3651082979859));
#56686=CARTESIAN_POINT('Ctrl Pts',(-23.1197813828984,27.4597516233152,-46.3635004526626));
#56687=CARTESIAN_POINT('Ctrl Pts',(-23.1512095143003,27.4630841720209,-46.3618926073392));
#56688=CARTESIAN_POINT('Ctrl Pts',(-23.1826588258506,27.4660364720341,-46.3602847620158));
#56689=CARTESIAN_POINT('Ctrl Pts',(-23.2975204323751,27.4768190903412,-46.3544124650471));
#56690=CARTESIAN_POINT('Ctrl Pts',(-23.4130492948945,27.4825616380405,-46.3485401680784));
#56691=CARTESIAN_POINT('Ctrl Pts',(-23.5287654837693,27.4831938364649,-46.3426678711097));
#56692=CARTESIAN_POINT('Ctrl Pts',(-23.6443317136537,27.4838252156103,-46.3368031841715));
#56693=CARTESIAN_POINT('Ctrl Pts',(-23.7600843775699,27.4793594132309,-46.3309384972333));
#56694=CARTESIAN_POINT('Ctrl Pts',(-23.8755377588109,27.4697778245096,-46.3250738102951));
#56695=CARTESIAN_POINT('Ctrl Pts',(-23.9908724034759,27.4602060898526,-46.3192151548203));
#56696=CARTESIAN_POINT('Ctrl Pts',(-24.1059079681931,27.4455290677664,-46.3133564993455));
#56697=CARTESIAN_POINT('Ctrl Pts',(-24.2201587390104,27.4257801955613,-46.3074978438707));
#56698=CARTESIAN_POINT('Ctrl Pts',(-24.3388722455673,27.4052599150131,-46.3014103441528));
#56699=CARTESIAN_POINT('Ctrl Pts',(-24.4567379442093,27.3792634825815,-46.2953228444349));
#56700=CARTESIAN_POINT('Ctrl Pts',(-24.5732164136781,27.3478878349002,-46.289235344717));
#56701=CARTESIAN_POINT('Ctrl Pts',(-24.6851863360486,27.317726648449,-46.2833834746336));
#56702=CARTESIAN_POINT('Ctrl Pts',(-24.795873987325,27.282595049108,-46.2775316045502));
#56703=CARTESIAN_POINT('Ctrl Pts',(-24.9048113940913,27.2426310724591,-46.2716797344668));
#56704=CARTESIAN_POINT('Ctrl Pts',(-25.0137322141468,27.2026731806891,-46.2658287553838));
#56705=CARTESIAN_POINT('Ctrl Pts',(-25.1209029315755,27.1578845168978,-46.2599777763009));
#56706=CARTESIAN_POINT('Ctrl Pts',(-25.225872814454,27.1084523107965,-46.2541267972179));
#56707=CARTESIAN_POINT('Ctrl Pts',(-25.3308521351355,27.0590156602641,-46.2482752920756));
#56708=CARTESIAN_POINT('Ctrl Pts',(-25.4336298538959,27.0049348136004,-46.2424237869333));
#56709=CARTESIAN_POINT('Ctrl Pts',(-25.5337778769518,26.9464439580895,-46.236572281791));
#56710=CARTESIAN_POINT('Ctrl Pts',(-25.6339591569866,26.8879336790384,-46.2307188334912));
#56711=CARTESIAN_POINT('Ctrl Pts',(-25.7315086481128,26.8250106875082,-46.2248653851914));
#56712=CARTESIAN_POINT('Ctrl Pts',(-25.8260259979156,26.7579532861977,-46.2190119368915));
#56713=CARTESIAN_POINT('Ctrl Pts',(-25.9206508344686,26.6908196260611,-46.21315183195));
#56714=CARTESIAN_POINT('Ctrl Pts',(-26.0122363098395,26.6195424109897,-46.2072917270084));
#56715=CARTESIAN_POINT('Ctrl Pts',(-26.1004139429539,26.5444411991836,-46.2014316220669));
#56716=CARTESIAN_POINT('Ctrl Pts',(-26.1886509581849,26.4692894114122,-46.1955675707115));
#56717=CARTESIAN_POINT('Ctrl Pts',(-26.2734752596195,26.3903087801372,-46.1897035193561));
#56718=CARTESIAN_POINT('Ctrl Pts',(-26.3545553889977,26.3078555641336,-46.1838394680006));
#56719=CARTESIAN_POINT('Ctrl Pts',(-26.4357550143019,26.2252808285485,-46.1779667742041));
#56720=CARTESIAN_POINT('Ctrl Pts',(-26.5131991788765,26.1392236000248,-46.1720940804075));
#56721=CARTESIAN_POINT('Ctrl Pts',(-26.5865967735075,26.0500730542932,-46.166221386611));
#56722=CARTESIAN_POINT('Ctrl Pts',(-26.6066918071259,26.0256651261781,-46.1646135412876));
#56723=CARTESIAN_POINT('Ctrl Pts',(-26.6264837736218,26.0010254957733,-46.1630056959643));
#56724=CARTESIAN_POINT('Ctrl Pts',(-26.645967279281,25.9761625056161,-46.1613978506409));
#56725=CARTESIAN_POINT('Ctrl Pts',(-26.7171035301144,25.8853852124929,-46.1555274446563));
#56726=CARTESIAN_POINT('Ctrl Pts',(-26.7843670858414,25.7913186538014,-46.1496570386717));
#56727=CARTESIAN_POINT('Ctrl Pts',(-26.847438158004,25.6943271445881,-46.1437866326871));
#56728=CARTESIAN_POINT('Ctrl Pts',(-26.9104292608357,25.5974586132444,-46.1379236699316));
#56729=CARTESIAN_POINT('Ctrl Pts',(-26.9692382243808,25.4976728461835,-46.1320607071761));
#56730=CARTESIAN_POINT('Ctrl Pts',(-27.0235853347113,25.3953672271767,-46.1261977444206));
#56731=CARTESIAN_POINT('Ctrl Pts',(-27.0778766835601,25.2931665762696,-46.1203407972101));
#56732=CARTESIAN_POINT('Ctrl Pts',(-27.1277150893714,25.1884515763986,-46.1144838499996));
#56733=CARTESIAN_POINT('Ctrl Pts',(-27.1728644158078,25.0816480185228,-46.1086269027892));
#56734=CARTESIAN_POINT('Ctrl Pts',(-27.2179783370944,24.9749282137452,-46.1027745484732));
#56735=CARTESIAN_POINT('Ctrl Pts',(-27.2584103323726,24.8661234873855,-46.0969221941572));
#56736=CARTESIAN_POINT('Ctrl Pts',(-27.2939707877688,24.7556830021626,-46.0910698398412));
#56737=CARTESIAN_POINT('Ctrl Pts',(-27.3295141448012,24.6452956195104,-46.0852202994848));
#56738=CARTESIAN_POINT('Ctrl Pts',(-27.3601904933446,24.5332744343669,-46.0793707591284));
#56739=CARTESIAN_POINT('Ctrl Pts',(-27.3858590643831,24.4200867264661,-46.073521218772));
#56740=CARTESIAN_POINT('Ctrl Pts',(-27.4115202849672,24.3069314310076,-46.0676733534905));
#56741=CARTESIAN_POINT('Ctrl Pts',(-27.4321764924474,24.1926106805289,-46.061825488209));
#56742=CARTESIAN_POINT('Ctrl Pts',(-27.4477375135206,24.0776042325897,-46.0559776229274));
#56743=CARTESIAN_POINT('Ctrl Pts',(-27.4633012898499,23.9625774214487,-46.0501287222148));
#56744=CARTESIAN_POINT('Ctrl Pts',(-27.4737680202745,23.8468650794797,-46.0442798215021));
#56745=CARTESIAN_POINT('Ctrl Pts',(-27.4790991777868,23.7309540299923,-46.0384309207894));
#56746=CARTESIAN_POINT('Ctrl Pts',(-27.4819148614464,23.6697348956372,-46.0353417878712));
#56747=CARTESIAN_POINT('Ctrl Pts',(-27.4832988550031,23.6084604087577,-46.0322526549529));
#56748=CARTESIAN_POINT('Ctrl Pts',(-27.4832513490189,23.5472024624234,-46.0291635220347));
#56749=CARTESIAN_POINT('',(-27.4893096392136,23.5490465589118,-44.7791635220347));
#56750=CARTESIAN_POINT('Ctrl Pts',(-27.4794900392396,23.5471764562959,-46.0291620620995));
#56751=CARTESIAN_POINT('Ctrl Pts',(-27.482652033486,23.1070280463571,-46.006945021155));
#56752=CARTESIAN_POINT('Ctrl Pts',(-27.2110024468889,21.3572725754213,-45.9184323430858));
#56753=CARTESIAN_POINT('Ctrl Pts',(-24.6381755688857,19.0272917428667,-45.7636240278909));
#56754=CARTESIAN_POINT('Ctrl Pts',(-20.3330782546349,20.190112578786,-45.5647371165163));
#56755=CARTESIAN_POINT('Ctrl Pts',(-18.9842913296047,24.4406171385372,-45.3658502051413));
#56756=CARTESIAN_POINT('Ctrl Pts',(-21.831235619625,27.8729521150715,-45.1669632937664));
#56757=CARTESIAN_POINT('Ctrl Pts',(-26.1838140696498,27.3421172137652,-44.9714010660644));
#56758=CARTESIAN_POINT('Ctrl Pts',(-27.4843286353731,24.7885886070499,-44.842134475487));
#56759=CARTESIAN_POINT('Ctrl Pts',(-27.4893096392136,23.5490465589118,-44.7791635220347));
#56760=CARTESIAN_POINT('',(-27.4831640504939,23.5538871935688,-43.5291635220347));
#56761=CARTESIAN_POINT('Ctrl Pts',(-27.4893096392136,23.5490465589118,-44.7791635220347));
#56762=CARTESIAN_POINT('Ctrl Pts',(-27.4895726217672,23.4836023345022,-44.775838838362));
#56763=CARTESIAN_POINT('Ctrl Pts',(-27.4880834946516,23.4181703317586,-44.7725141546893));
#56764=CARTESIAN_POINT('Ctrl Pts',(-27.4194264635282,22.0498761014208,-44.7028938338917));
#56765=CARTESIAN_POINT('Ctrl Pts',(-25.8655406100273,19.5153805453182,-44.5703025596418));
#56766=CARTESIAN_POINT('Ctrl Pts',(-21.4071583898454,19.4213424659167,-44.3714156482669));
#56767=CARTESIAN_POINT('Ctrl Pts',(-18.9180979816037,23.1214226631191,-44.1725287368921));
#56768=CARTESIAN_POINT('Ctrl Pts',(-20.685594862955,27.2155611507664,-43.9736418255171));
#56769=CARTESIAN_POINT('Ctrl Pts',(-25.0854692589609,27.9415917844081,-43.7747549141422));
#56770=CARTESIAN_POINT('Ctrl Pts',(-27.3122087991913,25.4763978711854,-43.6265954796481));
#56771=CARTESIAN_POINT('Ctrl Pts',(-27.4860063149194,23.8615827651834,-43.5447316822789));
#56772=CARTESIAN_POINT('Ctrl Pts',(-27.4831640504939,23.5538871935688,-43.5291635220347));
#56773=CARTESIAN_POINT('',(-27.4767710526401,23.5498218007742,-42.2791635220347));
#56774=CARTESIAN_POINT('Ctrl Pts',(-27.4831640504939,23.5538871935688,-43.5291635220347));
#56775=CARTESIAN_POINT('Ctrl Pts',(-27.4739027825809,22.5512883154403,-43.4784360451539));
#56776=CARTESIAN_POINT('Ctrl Pts',(-26.5733994698775,20.2236067000968,-43.3614129311482));
#56777=CARTESIAN_POINT('Ctrl Pts',(-22.6540126249395,18.9854409406596,-43.1780941800175));
#56778=CARTESIAN_POINT('Ctrl Pts',(-19.2253442867124,21.8368000215273,-42.9792072686427));
#56779=CARTESIAN_POINT('Ctrl Pts',(-19.7708999338745,26.2626766824239,-42.7803203572679));
#56780=CARTESIAN_POINT('Ctrl Pts',(-23.789360182175,28.1960655244424,-42.5814334458929));
#56781=CARTESIAN_POINT('Ctrl Pts',(-26.9800591897039,26.2342106968784,-42.414381167482));
#56782=CARTESIAN_POINT('Ctrl Pts',(-27.4761053845458,24.2337235905629,-42.3136245261958));
#56783=CARTESIAN_POINT('Ctrl Pts',(-27.4767710526401,23.5498218007742,-42.2791635220347));
#56784=CARTESIAN_POINT('',(-27.4832509871795,23.5467669685326,-41.0291635220347));
#56785=CARTESIAN_POINT('Ctrl Pts',(-27.4767710526401,23.5498218007742,-42.2791635220347));
#56786=CARTESIAN_POINT('Ctrl Pts',(-27.4773859882745,22.9180421126532,-42.2473288890708));
#56787=CARTESIAN_POINT('Ctrl Pts',(-27.0347362334315,20.9713941367988,-42.1491986189821));
#56788=CARTESIAN_POINT('Ctrl Pts',(-23.9731208222587,18.9175499467075,-41.9847727117682));
#56789=CARTESIAN_POINT('Ctrl Pts',(-19.8812603560255,20.6903142024657,-41.7858858003934));
#56790=CARTESIAN_POINT('Ctrl Pts',(-19.1608926199949,25.0911193000017,-41.5869988890184));
#56791=CARTESIAN_POINT('Ctrl Pts',(-22.4739744864657,28.0759984814201,-41.3881119776436));
#56792=CARTESIAN_POINT('Ctrl Pts',(-26.4961175464744,26.9784891217487,-41.2021671032004));
#56793=CARTESIAN_POINT('Ctrl Pts',(-27.4750186852402,24.600193314807,-41.0825178658824));
#56794=CARTESIAN_POINT('Ctrl Pts',(-27.4847500155487,23.5467803226292,-41.0291642656893));
#56795=CARTESIAN_POINT('',(-27.4850771999075,23.5522961849479,-39.7791629056863));
#56796=CARTESIAN_POINT('Ctrl Pts',(-27.4832509871795,23.5467669685326,-41.0291635220347));
#56797=CARTESIAN_POINT('Ctrl Pts',(-27.4831016864497,23.3783007803076,-41.0206276628369));
#56798=CARTESIAN_POINT('Ctrl Pts',(-27.4721249776244,23.2102952848097,-41.012091803639));
#56799=CARTESIAN_POINT('Ctrl Pts',(-27.4505169199899,23.0438666102941,-41.0035559444412));
#56800=CARTESIAN_POINT('Ctrl Pts',(-27.4393635511366,22.9579616008736,-40.9991500145921));
#56801=CARTESIAN_POINT('Ctrl Pts',(-27.4253783983837,22.8724761011641,-40.994744084743));
#56802=CARTESIAN_POINT('Ctrl Pts',(-27.4085928781309,22.7875607387275,-40.9903381548939));
#56803=CARTESIAN_POINT('Ctrl Pts',(-27.3862208560891,22.6743841239126,-40.9844658579251));
#56804=CARTESIAN_POINT('Ctrl Pts',(-27.3588274220373,22.5620030992679,-40.9785935609564));
#56805=CARTESIAN_POINT('Ctrl Pts',(-27.326481872693,22.4508977371991,-40.9727212639876));
#56806=CARTESIAN_POINT('Ctrl Pts',(-27.2941782406119,22.3399363588557,-40.9668565770494));
#56807=CARTESIAN_POINT('Ctrl Pts',(-27.2569353699205,22.2302477487934,-40.9609918901112));
#56808=CARTESIAN_POINT('Ctrl Pts',(-27.2148737397359,22.1223028121415,-40.9551272031729));
#56809=CARTESIAN_POINT('Ctrl Pts',(-27.1728553673048,22.0144688900993,-40.949268547698));
#56810=CARTESIAN_POINT('Ctrl Pts',(-27.1260282418908,21.9083754574422,-40.9434098922232));
#56811=CARTESIAN_POINT('Ctrl Pts',(-27.0745627293182,21.8044785970384,-40.9375512367483));
#56812=CARTESIAN_POINT('Ctrl Pts',(-27.0210869284949,21.6965234337574,-40.9314637370304));
#56813=CARTESIAN_POINT('Ctrl Pts',(-26.9626031215471,21.5909403776341,-40.9253762373125));
#56814=CARTESIAN_POINT('Ctrl Pts',(-26.8993578384398,21.488218913072,-40.9192887375946));
#56815=CARTESIAN_POINT('Ctrl Pts',(-26.8385605986392,21.3894735014488,-40.9134368675112));
#56816=CARTESIAN_POINT('Ctrl Pts',(-26.7733638718324,21.2933726573776,-40.9075849974277));
#56817=CARTESIAN_POINT('Ctrl Pts',(-26.7040332397333,21.2003256720664,-40.9017331273442));
#56818=CARTESIAN_POINT('Ctrl Pts',(-26.6347131638534,21.1072928540048,-40.8958821482612));
#56819=CARTESIAN_POINT('Ctrl Pts',(-26.5612606811033,21.0173133015696,-40.8900311691782));
#56820=CARTESIAN_POINT('Ctrl Pts',(-26.4839836208811,20.9307657696856,-40.8841801900952));
#56821=CARTESIAN_POINT('Ctrl Pts',(-26.4066996127076,20.8442104563456,-40.8783286849528));
#56822=CARTESIAN_POINT('Ctrl Pts',(-26.3255906188283,20.7610880853406,-40.8724771798105));
#56823=CARTESIAN_POINT('Ctrl Pts',(-26.2410030356066,20.6817423389817,-40.8666256746681));
#56824=CARTESIAN_POINT('Ctrl Pts',(-26.1563873626897,20.6023702436277,-40.8607722263683));
#56825=CARTESIAN_POINT('Ctrl Pts',(-26.0682911047986,20.526777549353,-40.8549187780685));
#56826=CARTESIAN_POINT('Ctrl Pts',(-25.977095047568,20.4552687832478,-40.8490653297686));
#56827=CARTESIAN_POINT('Ctrl Pts',(-25.8857952806177,20.3836786961478,-40.843205224827));
#56828=CARTESIAN_POINT('Ctrl Pts',(-25.7913890037402,20.3161820623535,-40.8373451198854));
#56829=CARTESIAN_POINT('Ctrl Pts',(-25.6942874742751,20.2530411091445,-40.8314850149438));
#56830=CARTESIAN_POINT('Ctrl Pts',(-25.5971205530072,20.1898576344554,-40.8256209635883));
#56831=CARTESIAN_POINT('Ctrl Pts',(-25.497255120277,20.1310358903768,-40.8197569122328));
#56832=CARTESIAN_POINT('Ctrl Pts',(-25.39512707184,20.0767921632544,-40.8138928608773));
#56833=CARTESIAN_POINT('Ctrl Pts',(-25.2928485070464,20.0224684917063,-40.8080201670807));
#56834=CARTESIAN_POINT('Ctrl Pts',(-25.1883010431383,19.9727364798982,-40.8021474732841));
#56835=CARTESIAN_POINT('Ctrl Pts',(-25.0819406401324,19.9277643621526,-40.7962747794875));
#56836=CARTESIAN_POINT('Ctrl Pts',(-25.05282094099,19.915451748609,-40.7946669341646));
#56837=CARTESIAN_POINT('Ctrl Pts',(-25.0235654344391,19.9034956346859,-40.7930590888417));
#56838=CARTESIAN_POINT('Ctrl Pts',(-24.9941836535463,19.8918988151508,-40.7914512435188));
#56839=CARTESIAN_POINT('Ctrl Pts',(-24.8868732422674,19.8495440144535,-40.7855789465501));
#56840=CARTESIAN_POINT('Ctrl Pts',(-24.7775178882831,19.8118438621452,-40.7797066495814));
#56841=CARTESIAN_POINT('Ctrl Pts',(-24.6665589423767,19.7789995572215,-40.7738343526127));
#56842=CARTESIAN_POINT('Ctrl Pts',(-24.555743790452,19.7461978159086,-40.7679696656745));
#56843=CARTESIAN_POINT('Ctrl Pts',(-24.4433295719789,19.7182395241225,-40.7621049787363));
#56844=CARTESIAN_POINT('Ctrl Pts',(-24.3297775914139,19.6952778649462,-40.7562402917981));
#56845=CARTESIAN_POINT('Ctrl Pts',(-24.2163423919526,19.6723398203989,-40.7503816363233));
#56846=CARTESIAN_POINT('Ctrl Pts',(-24.1017721605685,19.6543882687158,-40.7445229808485));
#56847=CARTESIAN_POINT('Ctrl Pts',(-23.9865426973814,19.6415264103953,-40.7386643253736));
#56848=CARTESIAN_POINT('Ctrl Pts',(-23.8668122698692,19.6281621565601,-40.7325768256557));
#56849=CARTESIAN_POINT('Ctrl Pts',(-23.7463704962939,19.6202934467827,-40.7264893259378));
#56850=CARTESIAN_POINT('Ctrl Pts',(-23.625762447994,19.6179774583378,-40.7204018262199));
#56851=CARTESIAN_POINT('Ctrl Pts',(-23.5098227909313,19.6157511151554,-40.7145499561366));
#56852=CARTESIAN_POINT('Ctrl Pts',(-23.3937299436869,19.61865563508,-40.7086980860532));
#56853=CARTESIAN_POINT('Ctrl Pts',(-23.2779718079965,19.6266888190087,-40.7028462159698));
#56854=CARTESIAN_POINT('Ctrl Pts',(-23.1622312975349,19.634720779812,-40.6969952368868));
#56855=CARTESIAN_POINT('Ctrl Pts',(-23.0468258095748,19.6478798233579,-40.6911442578039));
#56856=CARTESIAN_POINT('Ctrl Pts',(-22.9322403918285,19.6661117007023,-40.6852932787209));
#56857=CARTESIAN_POINT('Ctrl Pts',(-22.8176446717505,19.6843452172678,-40.6794417735786));
#56858=CARTESIAN_POINT('Ctrl Pts',(-22.7038695767311,19.7076524093489,-40.6735902684364));
#56859=CARTESIAN_POINT('Ctrl Pts',(-22.5913914943841,19.7359276227321,-40.6677387632941));
#56860=CARTESIAN_POINT('Ctrl Pts',(-22.4788760605146,19.7642122256982,-40.6618853149943));
#56861=CARTESIAN_POINT('Ctrl Pts',(-22.3676588964537,19.7974680297047,-40.6560318666946));
#56862=CARTESIAN_POINT('Ctrl Pts',(-22.2582020367302,19.8355392832101,-40.6501784183948));
#56863=CARTESIAN_POINT('Ctrl Pts',(-22.148620700789,19.8736538319978,-40.6443183134533));
#56864=CARTESIAN_POINT('Ctrl Pts',(-22.0408040554849,19.9165946247544,-40.6384582085118));
#56865=CARTESIAN_POINT('Ctrl Pts',(-21.9351950190544,19.9641574087414,-40.6325981035702));
#56866=CARTESIAN_POINT('Ctrl Pts',(-21.8295148615476,20.0117522232866,-40.6267340522148));
#56867=CARTESIAN_POINT('Ctrl Pts',(-21.7260456413423,20.0639750411031,-40.6208700008593));
#56868=CARTESIAN_POINT('Ctrl Pts',(-21.6252049439045,20.1205760477171,-40.6150059495039));
#56869=CARTESIAN_POINT('Ctrl Pts',(-21.5242156274085,20.1772604729163,-40.6091332557073));
#56870=CARTESIAN_POINT('Ctrl Pts',(-21.4258629151349,20.2383357477522,-40.6032605619108));
#56871=CARTESIAN_POINT('Ctrl Pts',(-21.3305348111603,20.3035092031959,-40.5973878681142));
#56872=CARTESIAN_POINT('Ctrl Pts',(-21.3044355709357,20.3213526050783,-40.5957800227908));
#56873=CARTESIAN_POINT('Ctrl Pts',(-21.2785628501617,20.3395029671702,-40.5941721774675));
#56874=CARTESIAN_POINT('Ctrl Pts',(-21.25292415315,20.3579537798329,-40.5925643321441));
#56875=CARTESIAN_POINT('Ctrl Pts',(-21.1592845221766,20.425341263998,-40.5866920351754));
#56876=CARTESIAN_POINT('Ctrl Pts',(-21.0684555467662,20.4969652275506,-40.5808197382067));
#56877=CARTESIAN_POINT('Ctrl Pts',(-20.9808450678181,20.572563111258,-40.574947441238));
#56878=CARTESIAN_POINT('Ctrl Pts',(-20.8933481250928,20.648063026112,-40.5690827542998));
#56879=CARTESIAN_POINT('Ctrl Pts',(-20.8090616944605,20.7275263522804,-40.5632180673616));
#56880=CARTESIAN_POINT('Ctrl Pts',(-20.7283640060337,20.8106477885341,-40.5573533804234));
#56881=CARTESIAN_POINT('Ctrl Pts',(-20.6477493101276,20.8936837395941,-40.5514947249486));
#56882=CARTESIAN_POINT('Ctrl Pts',(-20.5707163014611,20.9803700228401,-40.5456360694738));
#56883=CARTESIAN_POINT('Ctrl Pts',(-20.4976089944803,21.0703621238927,-40.539777413999));
#56884=CARTESIAN_POINT('Ctrl Pts',(-20.4216460516966,21.1638693956765,-40.5336899142811));
#56885=CARTESIAN_POINT('Ctrl Pts',(-20.349922089631,21.2609457093743,-40.5276024145631));
#56886=CARTESIAN_POINT('Ctrl Pts',(-20.2827798466498,21.3611633940645,-40.5215149148452));
#56887=CARTESIAN_POINT('Ctrl Pts',(-20.218236487103,21.457501939944,-40.5156630447619));
#56888=CARTESIAN_POINT('Ctrl Pts',(-20.1579270029877,21.5567428163157,-40.5098111746785));
#56889=CARTESIAN_POINT('Ctrl Pts',(-20.1021132757333,21.6584743545547,-40.5039593045951));
#56890=CARTESIAN_POINT('Ctrl Pts',(-20.0463080466263,21.7601904032421,-40.4981083255121));
#56891=CARTESIAN_POINT('Ctrl Pts',(-19.9949974121188,21.8643959974527,-40.4922573464291));
#56892=CARTESIAN_POINT('Ctrl Pts',(-19.948397920515,21.9706537345538,-40.4864063673462));
#56893=CARTESIAN_POINT('Ctrl Pts',(-19.9017942391685,22.076921025248,-40.4805548622039));
#56894=CARTESIAN_POINT('Ctrl Pts',(-19.8599027087935,22.1852404470163,-40.4747033570616));
#56895=CARTESIAN_POINT('Ctrl Pts',(-19.8228919484283,22.2951540963848,-40.4688518519193));
#56896=CARTESIAN_POINT('Ctrl Pts',(-19.7858688975954,22.4051042456837,-40.4629984036195));
#56897=CARTESIAN_POINT('Ctrl Pts',(-19.753729971475,22.5166492837163,-40.4571449553198));
#56898=CARTESIAN_POINT('Ctrl Pts',(-19.7265938829317,22.6293163027706,-40.45129150702));
#56899=CARTESIAN_POINT('Ctrl Pts',(-19.6994269347633,22.7421114486908,-40.4454314020785));
#56900=CARTESIAN_POINT('Ctrl Pts',(-19.6772742767218,22.8560307202338,-40.4395712971369));
#56901=CARTESIAN_POINT('Ctrl Pts',(-19.6602034836346,22.9705910755917,-40.4337111921954));
#56902=CARTESIAN_POINT('Ctrl Pts',(-19.6431211944367,23.0852285801789,-40.4278471408399));
#56903=CARTESIAN_POINT('Ctrl Pts',(-19.6311276273805,23.2005076180819,-40.4219830894845));
#56904=CARTESIAN_POINT('Ctrl Pts',(-19.6242383320048,23.3159418323282,-40.4161190381291));
#56905=CARTESIAN_POINT('Ctrl Pts',(-19.617338883183,23.4315461735634,-40.4102463443325));
#56906=CARTESIAN_POINT('Ctrl Pts',(-19.6155587261871,23.5473057357987,-40.4043736505359));
#56907=CARTESIAN_POINT('Ctrl Pts',(-19.6188613663048,23.6627358846772,-40.3985009567394));
#56908=CARTESIAN_POINT('Ctrl Pts',(-19.6197655739227,23.6943387285313,-40.3968931114159));
#56909=CARTESIAN_POINT('Ctrl Pts',(-19.6210504756811,23.7259169227772,-40.3952852660925));
#56910=CARTESIAN_POINT('Ctrl Pts',(-19.6227146513102,23.757460635176,-40.3936774207691));
#56911=CARTESIAN_POINT('Ctrl Pts',(-19.6287926821754,23.8726670197724,-40.3878051238004));
#56912=CARTESIAN_POINT('Ctrl Pts',(-19.6399542127138,23.9877987493919,-40.3819328268317));
#56913=CARTESIAN_POINT('Ctrl Pts',(-19.6561988027336,24.102370776247,-40.376060529863));
#56914=CARTESIAN_POINT('Ctrl Pts',(-19.6724223410549,24.2167943268545,-40.3701958429248));
#56915=CARTESIAN_POINT('Ctrl Pts',(-19.6937157817035,24.3306592116078,-40.3643311559866));
#56916=CARTESIAN_POINT('Ctrl Pts',(-19.7200267190434,24.4434821909103,-40.3584664690484));
#56917=CARTESIAN_POINT('Ctrl Pts',(-19.7463105972312,24.5561891388413,-40.3526078135735));
#56918=CARTESIAN_POINT('Ctrl Pts',(-19.7776016149248,24.6678559124983,-40.3467491580987));
#56919=CARTESIAN_POINT('Ctrl Pts',(-19.8137958807882,24.7780068621287,-40.3408905026239));
#56920=CARTESIAN_POINT('Ctrl Pts',(-19.8514039265558,24.8924604048713,-40.334803002906));
#56921=CARTESIAN_POINT('Ctrl Pts',(-19.8943060159491,25.0052768404701,-40.3287155031881));
#56922=CARTESIAN_POINT('Ctrl Pts',(-19.942327606863,25.1159366431234,-40.3226280034702));
#56923=CARTESIAN_POINT('Ctrl Pts',(-19.9884904198813,25.2223131225635,-40.3167761333868));
#56924=CARTESIAN_POINT('Ctrl Pts',(-20.0393836013961,25.3266964042356,-40.3109242633034));
#56925=CARTESIAN_POINT('Ctrl Pts',(-20.0948023657008,25.4286436385556,-40.30507239322));
#56926=CARTESIAN_POINT('Ctrl Pts',(-20.1502126919947,25.5305753504823,-40.299221414137));
#56927=CARTESIAN_POINT('Ctrl Pts',(-20.2101470336281,25.6300713894557,-40.293370435054));
#56928=CARTESIAN_POINT('Ctrl Pts',(-20.2743544499655,25.7267131350882,-40.2875194559711));
#56929=CARTESIAN_POINT('Ctrl Pts',(-20.3385676391675,25.8233635697436,-40.2816679508288));
#56930=CARTESIAN_POINT('Ctrl Pts',(-20.4070544380356,25.9171588565667,-40.2758164456865));
#56931=CARTESIAN_POINT('Ctrl Pts',(-20.4795207504331,26.0077096172917,-40.2699649405442));
#56932=CARTESIAN_POINT('Ctrl Pts',(-20.5520111273155,26.0982904479531,-40.2641114922444));
#56933=CARTESIAN_POINT('Ctrl Pts',(-20.628483387309,26.1856242875196,-40.2582580439446));
#56934=CARTESIAN_POINT('Ctrl Pts',(-20.7086038345567,26.2693556342,-40.2524045956448));
#56935=CARTESIAN_POINT('Ctrl Pts',(-20.7888153961507,26.3531822016034,-40.2465444907033));
#56936=CARTESIAN_POINT('Ctrl Pts',(-20.8726831398765,26.4333978001463,-40.2406843857618));
#56937=CARTESIAN_POINT('Ctrl Pts',(-20.9598372016155,26.5096844734177,-40.2348242808202));
#56938=CARTESIAN_POINT('Ctrl Pts',(-21.0470499561602,26.5860225209889,-40.2289602294648));
#56939=CARTESIAN_POINT('Ctrl Pts',(-21.1375531134912,26.6584261171962,-40.2230961781093));
#56940=CARTESIAN_POINT('Ctrl Pts',(-21.230945898512,26.7266192833898,-40.2172321267539));
#56941=CARTESIAN_POINT('Ctrl Pts',(-21.3244763258551,26.7949129526978,-40.2113594329573));
#56942=CARTESIAN_POINT('Ctrl Pts',(-21.420904537484,26.8589835794306,-40.2054867391607));
#56943=CARTESIAN_POINT('Ctrl Pts',(-21.5198030754438,26.9185999017872,-40.1996140453642));
#56944=CARTESIAN_POINT('Ctrl Pts',(-21.5468798407662,26.9349218535889,-40.1980062000409));
#56945=CARTESIAN_POINT('Ctrl Pts',(-21.5741416492813,26.9509101968645,-40.1963983547175));
#56946=CARTESIAN_POINT('Ctrl Pts',(-21.6015794612456,26.9665608117691,-40.1947905093942));
#56947=CARTESIAN_POINT('Ctrl Pts',(-21.7017899589164,27.0237211972432,-40.1889182124255));
#56948=CARTESIAN_POINT('Ctrl Pts',(-21.8046854951808,27.0765643949701,-40.1830459154568));
#56949=CARTESIAN_POINT('Ctrl Pts',(-21.9098577532546,27.1248285863989,-40.1771736184881));
#56950=CARTESIAN_POINT('Ctrl Pts',(-22.0148937164346,27.1730302312686,-40.1713089315499));
#56951=CARTESIAN_POINT('Ctrl Pts',(-22.1222001617944,27.2166644996686,-40.1654442446117));
#56952=CARTESIAN_POINT('Ctrl Pts',(-22.2313422042853,27.2555142698517,-40.1595795576735));
#56953=CARTESIAN_POINT('Ctrl Pts',(-22.340372001018,27.2943240854783,-40.1537209021987));
#56954=CARTESIAN_POINT('Ctrl Pts',(-22.4512332528523,27.3283590523365,-40.1478622467238));
#56955=CARTESIAN_POINT('Ctrl Pts',(-22.5634696299993,27.3574494670947,-40.142003591249));
#56956=CARTESIAN_POINT('Ctrl Pts',(-22.6800900588941,27.3876761790758,-40.1359160915311));
#56957=CARTESIAN_POINT('Ctrl Pts',(-22.7981948170911,27.4125639975166,-40.1298285918132));
#56958=CARTESIAN_POINT('Ctrl Pts',(-22.9172524714096,27.4319789418988,-40.1237410920953));
#56959=CARTESIAN_POINT('Ctrl Pts',(-23.0317017457902,27.4506423895318,-40.1178892220119));
#56960=CARTESIAN_POINT('Ctrl Pts',(-23.1470310741534,27.4642486908902,-40.1120373519285));
#56961=CARTESIAN_POINT('Ctrl Pts',(-23.2627571843576,27.4727307566509,-40.1061854818451));
#56962=CARTESIAN_POINT('Ctrl Pts',(-23.3784656742093,27.48121153094,-40.1003345027621));
#56963=CARTESIAN_POINT('Ctrl Pts',(-23.4945704136167,27.4845695907323,-40.0944835236791));
#56964=CARTESIAN_POINT('Ctrl Pts',(-23.6105835661724,27.4827897745285,-40.0886325445961));
#56965=CARTESIAN_POINT('Ctrl Pts',(-23.7266071494271,27.4810097983021,-40.0827810394538));
#56966=CARTESIAN_POINT('Ctrl Pts',(-23.8425387161017,27.4740910341182,-40.0769295343115));
#56967=CARTESIAN_POINT('Ctrl Pts',(-23.9578917042987,27.4620704345315,-40.0710780291692));
#56968=CARTESIAN_POINT('Ctrl Pts',(-24.0732829987118,27.4500458431654,-40.0652245808694));
#56969=CARTESIAN_POINT('Ctrl Pts',(-24.1880949216634,27.4329160903923,-40.0593711325697));
#56970=CARTESIAN_POINT('Ctrl Pts',(-24.301848006775,27.4107697563466,-40.0535176842699));
#56971=CARTESIAN_POINT('Ctrl Pts',(-24.4157304538454,27.3885982371101,-40.0476575793284));
#56972=CARTESIAN_POINT('Ctrl Pts',(-24.5285512536664,27.3613988287529,-40.0417974743868));
#56973=CARTESIAN_POINT('Ctrl Pts',(-24.6398429769391,27.3293108352443,-40.0359373694453));
#56974=CARTESIAN_POINT('Ctrl Pts',(-24.751209648222,27.2972012324804,-40.0300733180898));
#56975=CARTESIAN_POINT('Ctrl Pts',(-24.8610448017554,27.2601966208898,-40.0242092667343));
#56976=CARTESIAN_POINT('Ctrl Pts',(-24.968899616141,27.2184850011256,-40.0183452153789));
#56977=CARTESIAN_POINT('Ctrl Pts',(-25.0769133869931,27.1767119067603,-40.0124725215823));
#56978=CARTESIAN_POINT('Ctrl Pts',(-25.1829406165239,27.1302181243161,-40.0065998277857));
#56979=CARTESIAN_POINT('Ctrl Pts',(-25.2865556811539,27.0792382745354,-40.0007271339891));
#56980=CARTESIAN_POINT('Ctrl Pts',(-25.3149237525804,27.0652808444546,-39.9991192886659));
#56981=CARTESIAN_POINT('Ctrl Pts',(-25.3431111772467,27.0509874048801,-39.9975114433426));
#56982=CARTESIAN_POINT('Ctrl Pts',(-25.3711096026936,27.0363633341489,-39.9959035980193));
#56983=CARTESIAN_POINT('Ctrl Pts',(-25.4733676162594,26.9829521726515,-39.9900313010506));
#56984=CARTESIAN_POINT('Ctrl Pts',(-25.5734448845254,26.9249484201392,-39.9841590040819));
#56985=CARTESIAN_POINT('Ctrl Pts',(-25.6709004226202,26.8625540763473,-39.9782867071132));
#56986=CARTESIAN_POINT('Ctrl Pts',(-25.7682296660774,26.8002405906696,-39.972422020175));
#56987=CARTESIAN_POINT('Ctrl Pts',(-25.8629435909488,26.7335480496325,-39.9665573332368));
#56988=CARTESIAN_POINT('Ctrl Pts',(-25.9546244552608,26.6627249658155,-39.9606926462986));
#56989=CARTESIAN_POINT('Ctrl Pts',(-26.046211031543,26.5919747191066,-39.9548339908238));
#56990=CARTESIAN_POINT('Ctrl Pts',(-26.1347704265662,26.5171026303126,-39.948975335349));
#56991=CARTESIAN_POINT('Ctrl Pts',(-26.219913200474,26.4384008854964,-39.9431166798742));
#56992=CARTESIAN_POINT('Ctrl Pts',(-26.3083817261235,26.3566249812079,-39.9370291801563));
#56993=CARTESIAN_POINT('Ctrl Pts',(-26.3931608939733,26.2707143874827,-39.9309416804383));
#56994=CARTESIAN_POINT('Ctrl Pts',(-26.4738507218022,26.1810437858224,-39.9248541807204));
#56995=CARTESIAN_POINT('Ctrl Pts',(-26.5514172780876,26.0948440756732,-39.919002310637));
#56996=CARTESIAN_POINT('Ctrl Pts',(-26.6252048788477,26.0051703593938,-39.9131504405537));
#56997=CARTESIAN_POINT('Ctrl Pts',(-26.6948958516298,25.9123929573219,-39.9072985704703));
#56998=CARTESIAN_POINT('Ctrl Pts',(-26.7645762133275,25.819629681453,-39.9014475913873));
#56999=CARTESIAN_POINT('Ctrl Pts',(-26.830160939052,25.7237639898318,-39.8955966123043));
#57000=CARTESIAN_POINT('Ctrl Pts',(-26.8913735769205,25.6251981119796,-39.8897456332214));
#57001=CARTESIAN_POINT('Ctrl Pts',(-26.9525917183942,25.5266233721065,-39.8838941280791));
#57002=CARTESIAN_POINT('Ctrl Pts',(-27.0094367724771,25.4253483145863,-39.8780426229368));
#57003=CARTESIAN_POINT('Ctrl Pts',(-27.0616768206409,25.3218022665295,-39.8721911177945));
#57004=CARTESIAN_POINT('Ctrl Pts',(-27.1139342165874,25.2182218330845,-39.8663376694947));
#57005=CARTESIAN_POINT('Ctrl Pts',(-27.1615833797504,25.1123692784073,-39.860484221195));
#57006=CARTESIAN_POINT('Ctrl Pts',(-27.2044396621794,25.0046958669246,-39.8546307728952));
#57007=CARTESIAN_POINT('Ctrl Pts',(-27.2473446815077,24.8969000073919,-39.8487706679537));
#57008=CARTESIAN_POINT('Ctrl Pts',(-27.2854457880149,24.7872795422856,-39.8429105630122));
#57009=CARTESIAN_POINT('Ctrl Pts',(-27.3186075151159,24.6763030274185,-39.8370504580706));
#57010=CARTESIAN_POINT('Ctrl Pts',(-27.3517915745645,24.5652517768145,-39.8311864067152));
#57011=CARTESIAN_POINT('Ctrl Pts',(-27.3800295306883,24.4528430580043,-39.8253223553598));
#57012=CARTESIAN_POINT('Ctrl Pts',(-27.4032369445985,24.3395560942837,-39.8194583040043));
#57013=CARTESIAN_POINT('Ctrl Pts',(-27.4264785616041,24.2261021681927,-39.8135856102078));
#57014=CARTESIAN_POINT('Ctrl Pts',(-27.4446747747246,24.1117678206154,-39.8077129164112));
#57015=CARTESIAN_POINT('Ctrl Pts',(-27.4577929067385,23.9970379582675,-39.8018402226146));
#57016=CARTESIAN_POINT('Ctrl Pts',(-27.4613844318446,23.9656268411517,-39.8002323772912));
#57017=CARTESIAN_POINT('Ctrl Pts',(-27.4645956192938,23.9341860778103,-39.7986245319678));
#57018=CARTESIAN_POINT('Ctrl Pts',(-27.4674264791132,23.9027256025266,-39.7970166866444));
#57019=CARTESIAN_POINT('Ctrl Pts',(-27.4779042295962,23.7862821785711,-39.7910656317745));
#57020=CARTESIAN_POINT('Ctrl Pts',(-27.4831908370144,23.6693646861602,-39.7851145769046));
#57021=CARTESIAN_POINT('Ctrl Pts',(-27.4832519949075,23.5523073708991,-39.7791635220347));
#57022=CARTESIAN_POINT('',(-27.4815728590188,23.5527517371402,-38.5291640444444));
#57023=CARTESIAN_POINT('Ctrl Pts',(-27.4884312052316,23.5522756295914,-39.7791617730815));
#57024=CARTESIAN_POINT('Ctrl Pts',(-27.4808809331833,22.3637409737853,-39.7188177738108));
#57025=CARTESIAN_POINT('Ctrl Pts',(-26.273746231481,19.8561955596585,-39.5921781374153));
#57026=CARTESIAN_POINT('Ctrl Pts',(-22.0037382742824,19.1628792305343,-39.3992428638946));
#57027=CARTESIAN_POINT('Ctrl Pts',(-19.0231252434711,22.4797996610202,-39.2003559525198));
#57028=CARTESIAN_POINT('Ctrl Pts',(-20.2025583534408,26.7803755202187,-39.0014690411448));
#57029=CARTESIAN_POINT('Ctrl Pts',(-24.4582385755645,28.1127422222292,-38.80258212977));
#57030=CARTESIAN_POINT('Ctrl Pts',(-27.1664814591117,25.8486886819478,-38.6451474635765));
#57031=CARTESIAN_POINT('Ctrl Pts',(-27.4811981277005,24.0453033749675,-38.554008434508));
#57032=CARTESIAN_POINT('Ctrl Pts',(-27.4783651688805,23.5527694946165,-38.5291650425645));
#57033=CARTESIAN_POINT('',(-27.4820553179501,23.5472580460612,-37.2791630686818));
#57034=CARTESIAN_POINT('Ctrl Pts',(-27.4832517435352,23.5527424429907,-38.5291635220347));
#57035=CARTESIAN_POINT('Ctrl Pts',(-27.4833258207743,23.4357319600559,-38.523268827156));
#57036=CARTESIAN_POINT('Ctrl Pts',(-27.4781738034219,23.318699749024,-38.5173741322774));
#57037=CARTESIAN_POINT('Ctrl Pts',(-27.4678164922244,23.202141033529,-38.5114794373987));
#57038=CARTESIAN_POINT('Ctrl Pts',(-27.4574581828925,23.0855710852667,-38.5055841744481));
#57039=CARTESIAN_POINT('Ctrl Pts',(-27.4418936169437,22.9694751265147,-38.4996889114975));
#57040=CARTESIAN_POINT('Ctrl Pts',(-27.4211954988383,22.8543433816485,-38.4937936485469));
#57041=CARTESIAN_POINT('Ctrl Pts',(-27.4004906542045,22.7391742209672,-38.4878964697383));
#57042=CARTESIAN_POINT('Ctrl Pts',(-27.3746490092089,22.6249702959038,-38.4819992909298));
#57043=CARTESIAN_POINT('Ctrl Pts',(-27.3437942984983,22.5122111724446,-38.4761021121212));
#57044=CARTESIAN_POINT('Ctrl Pts',(-27.3127095232854,22.3986112739134,-38.4701609616962));
#57045=CARTESIAN_POINT('Ctrl Pts',(-27.2765367268469,22.2864782137126,-38.4642198112711));
#57046=CARTESIAN_POINT('Ctrl Pts',(-27.2354529487445,22.1762849606895,-38.458278660846));
#57047=CARTESIAN_POINT('Ctrl Pts',(-27.1945948460353,22.0666970051065,-38.4523701454784));
#57048=CARTESIAN_POINT('Ctrl Pts',(-27.1488797994331,21.9590279468057,-38.4464616301107));
#57049=CARTESIAN_POINT('Ctrl Pts',(-27.0985291928668,21.8537202638673,-38.4405531147431));
#57050=CARTESIAN_POINT('Ctrl Pts',(-27.0477614269543,21.7475400972161,-38.4345956467893));
#57051=CARTESIAN_POINT('Ctrl Pts',(-26.99228114698,21.6437609777045,-38.4286381788355));
#57052=CARTESIAN_POINT('Ctrl Pts',(-26.9323605244277,21.5428077564916,-38.4226807108817));
#57053=CARTESIAN_POINT('Ctrl Pts',(-26.8724399018754,21.4418545352787,-38.4167232429279));
#57054=CARTESIAN_POINT('Ctrl Pts',(-26.8080792180531,21.3437275234703,-38.4107657749741));
#57055=CARTESIAN_POINT('Ctrl Pts',(-26.7395921569827,21.2488178151392,-38.4048083070203));
#57056=CARTESIAN_POINT('Ctrl Pts',(-26.6720842216924,21.1552649841621,-38.3989360100516));
#57057=CARTESIAN_POINT('Ctrl Pts',(-26.6003434276182,21.0645282584402,-38.3930637130829));
#57058=CARTESIAN_POINT('Ctrl Pts',(-26.5246328586346,20.9770151406419,-38.3871914161142));
#57059=CARTESIAN_POINT('Ctrl Pts',(-26.4490204045356,20.889615432894,-38.3813267291759));
#57060=CARTESIAN_POINT('Ctrl Pts',(-26.3694486740837,20.8054313351828,-38.3754620422377));
#57061=CARTESIAN_POINT('Ctrl Pts',(-26.286223455008,20.7248406844087,-38.3695973552995));
#57062=CARTESIAN_POINT('Ctrl Pts',(-26.2030838278604,20.6443329160741,-38.3637386998247));
#57063=CARTESIAN_POINT('Ctrl Pts',(-26.1162984809027,20.567411529707,-38.3578800443499));
#57064=CARTESIAN_POINT('Ctrl Pts',(-26.026212370949,20.4944200961053,-38.3520213888751));
#57065=CARTESIAN_POINT('Ctrl Pts',(-25.9326074181935,20.418577552817,-38.3459338891572));
#57066=CARTESIAN_POINT('Ctrl Pts',(-25.8354388817183,20.3469785798161,-38.3398463894393));
#57067=CARTESIAN_POINT('Ctrl Pts',(-25.7351348731684,20.2799653648059,-38.3337588897214));
#57068=CARTESIAN_POINT('Ctrl Pts',(-25.6387133447776,20.2155460389277,-38.327907019638));
#57069=CARTESIAN_POINT('Ctrl Pts',(-25.5393949369666,20.1553643200487,-38.3220551495546));
#57070=CARTESIAN_POINT('Ctrl Pts',(-25.4375916550404,20.099681559596,-38.3162032794712));
#57071=CARTESIAN_POINT('Ctrl Pts',(-25.3358038735896,20.0440072773499,-38.3103523003882));
#57072=CARTESIAN_POINT('Ctrl Pts',(-25.2315323328709,19.992830789833,-38.3045013213052));
#57073=CARTESIAN_POINT('Ctrl Pts',(-25.1252147138359,19.946368082267,-38.2986503422222));
#57074=CARTESIAN_POINT('Ctrl Pts',(-25.0188875358238,19.8999011972564,-38.2927988370799));
#57075=CARTESIAN_POINT('Ctrl Pts',(-24.9105142926091,19.8581491002485,-38.2869473319376));
#57076=CARTESIAN_POINT('Ctrl Pts',(-24.8005531042859,19.8212798208559,-38.2810958267953));
#57077=CARTESIAN_POINT('Ctrl Pts',(-24.6905554002461,19.7843982979783,-38.2752423784956));
#57078=CARTESIAN_POINT('Ctrl Pts',(-24.5789690942821,19.7524029482666,-38.2693889301958));
#57079=CARTESIAN_POINT('Ctrl Pts',(-24.4662672464887,19.7254118758917,-38.263535481896));
#57080=CARTESIAN_POINT('Ctrl Pts',(-24.3534372322211,19.6983901088063,-38.2576753769545));
#57081=CARTESIAN_POINT('Ctrl Pts',(-24.2394895462633,19.676384074358,-38.2518152720129));
#57082=CARTESIAN_POINT('Ctrl Pts',(-24.1249073169867,19.6594607256809,-38.2459551670714));
#57083=CARTESIAN_POINT('Ctrl Pts',(-24.0102479237504,19.6425259801876,-38.2400911157159));
#57084=CARTESIAN_POINT('Ctrl Pts',(-23.8949535465194,19.6306807782257,-38.2342270643605));
#57085=CARTESIAN_POINT('Ctrl Pts',(-23.7795105618746,19.6239400434175,-38.228363013005));
#57086=CARTESIAN_POINT('Ctrl Pts',(-23.6638974373149,19.6171893741117,-38.2224903192084));
#57087=CARTESIAN_POINT('Ctrl Pts',(-23.5481356800144,19.61555819215,-38.2166176254119));
#57088=CARTESIAN_POINT('Ctrl Pts',(-23.4327098769627,19.6190093791636,-38.2107449316153));
#57089=CARTESIAN_POINT('Ctrl Pts',(-23.4011082229252,19.6199542564366,-38.209137086292));
#57090=CARTESIAN_POINT('Ctrl Pts',(-23.3695317083993,19.6212797958127,-38.2075292409686));
#57091=CARTESIAN_POINT('Ctrl Pts',(-23.337990163788,19.62298456437,-38.2059213956453));
#57092=CARTESIAN_POINT('Ctrl Pts',(-23.2227916965455,19.6292108518654,-38.2000490986766));
#57093=CARTESIAN_POINT('Ctrl Pts',(-23.1076744262871,19.6405205387493,-38.1941768017079));
#57094=CARTESIAN_POINT('Ctrl Pts',(-22.9931233998321,19.6569125606115,-38.1883045047392));
#57095=CARTESIAN_POINT('Ctrl Pts',(-22.8787208224101,19.6732833397151,-38.182439817801));
#57096=CARTESIAN_POINT('Ctrl Pts',(-22.76488343495,19.6947232979882,-38.1765751308628));
#57097=CARTESIAN_POINT('Ctrl Pts',(-22.6520944092062,19.7211794079463,-38.1707104439246));
#57098=CARTESIAN_POINT('Ctrl Pts',(-22.5394213799146,19.7476083094514,-38.1648517884498));
#57099=CARTESIAN_POINT('Ctrl Pts',(-22.4277949678349,19.7790430076925,-38.1589931329749));
#57100=CARTESIAN_POINT('Ctrl Pts',(-22.317690688626,19.8153789992955,-38.1531344775001));
#57101=CARTESIAN_POINT('Ctrl Pts',(-22.2032856392926,19.8531343067348,-38.1470469777822));
#57102=CARTESIAN_POINT('Ctrl Pts',(-22.0905245087702,19.8961815465863,-38.1409594780643));
#57103=CARTESIAN_POINT('Ctrl Pts',(-21.9799265978079,19.9443455082999,-38.1348719783464));
#57104=CARTESIAN_POINT('Ctrl Pts',(-21.8736096144094,19.9906451813531,-38.129020108263));
#57105=CARTESIAN_POINT('Ctrl Pts',(-21.7692919147448,20.041672653895,-38.1231682381796));
#57106=CARTESIAN_POINT('Ctrl Pts',(-21.6674160844884,20.0972225704756,-38.1173163680962));
#57107=CARTESIAN_POINT('Ctrl Pts',(-21.5655557657533,20.1527640290764,-38.1114653890132));
#57108=CARTESIAN_POINT('Ctrl Pts',(-21.4661369400108,20.2128263647485,-38.1056144099302));
#57109=CARTESIAN_POINT('Ctrl Pts',(-21.3695779043605,20.2771580983325,-38.0997634308473));
#57110=CARTESIAN_POINT('Ctrl Pts',(-21.2730101871237,20.3414956159585,-38.093911925705));
#57111=CARTESIAN_POINT('Ctrl Pts',(-21.1793031151586,20.4101030653583,-38.0880604205627));
#57112=CARTESIAN_POINT('Ctrl Pts',(-21.0888456879293,20.4826858495392,-38.0822089154204));
#57113=CARTESIAN_POINT('Ctrl Pts',(-20.9983582217579,20.5552927368825,-38.0763554671206));
#57114=CARTESIAN_POINT('Ctrl Pts',(-20.9111228683668,20.6318773254143,-38.0705020188208));
#57115=CARTESIAN_POINT('Ctrl Pts',(-20.8274946998121,20.712105462051,-38.0646485705211));
#57116=CARTESIAN_POINT('Ctrl Pts',(-20.7437714278701,20.7924248355003,-38.0587884655795));
#57117=CARTESIAN_POINT('Ctrl Pts',(-20.6636638270207,20.8763957410175,-38.052928360638));
#57118=CARTESIAN_POINT('Ctrl Pts',(-20.5874893774252,20.963647905605,-38.0470682556965));
#57119=CARTESIAN_POINT('Ctrl Pts',(-20.5112636291053,21.0509588290646,-38.041204204341));
#57120=CARTESIAN_POINT('Ctrl Pts',(-20.4389765633839,21.1415550892527,-38.0353401529856));
#57121=CARTESIAN_POINT('Ctrl Pts',(-20.3709036429159,21.2350355562416,-38.0294761016301));
#57122=CARTESIAN_POINT('Ctrl Pts',(-20.3027303965518,21.3286537947782,-38.0236034078335));
#57123=CARTESIAN_POINT('Ctrl Pts',(-20.238783918489,21.4251643804734,-38.017730714037));
#57124=CARTESIAN_POINT('Ctrl Pts',(-20.179294920232,21.5241395581103,-38.0118580202404));
#57125=CARTESIAN_POINT('Ctrl Pts',(-20.1630078276387,21.5512373060946,-38.0102501749171));
#57126=CARTESIAN_POINT('Ctrl Pts',(-20.1470545814315,21.57851966779,-38.0086423295938));
#57127=CARTESIAN_POINT('Ctrl Pts',(-20.1314392898184,21.6059775981587,-38.0070344842704));
#57128=CARTESIAN_POINT('Ctrl Pts',(-20.0744079148003,21.7062615738204,-38.0011621873017));
#57129=CARTESIAN_POINT('Ctrl Pts',(-20.0216971793903,21.809225029967,-37.995289890333));
#57130=CARTESIAN_POINT('Ctrl Pts',(-19.9735683764508,21.9144593132125,-37.9894175933643));
#57131=CARTESIAN_POINT('Ctrl Pts',(-19.9255019446175,22.0195572211844,-37.9835529064261));
#57132=CARTESIAN_POINT('Ctrl Pts',(-19.882005807406,22.1269197315975,-37.9776882194879));
#57133=CARTESIAN_POINT('Ctrl Pts',(-19.8432965267201,22.2361116803443,-37.9718235325497));
#57134=CARTESIAN_POINT('Ctrl Pts',(-19.8046270561062,22.3451913320073,-37.9659648770749));
#57135=CARTESIAN_POINT('Ctrl Pts',(-19.7707347872471,22.456096292396,-37.9601062216001));
#57136=CARTESIAN_POINT('Ctrl Pts',(-19.7417888360728,22.5683700137045,-37.9542475661253));
#57137=CARTESIAN_POINT('Ctrl Pts',(-19.7117122305504,22.6850292454569,-37.9481600664074));
#57138=CARTESIAN_POINT('Ctrl Pts',(-19.6869764243636,22.8031659345413,-37.9420725666895));
#57139=CARTESIAN_POINT('Ctrl Pts',(-19.6677147140067,22.9222484757945,-37.9359850669716));
#57140=CARTESIAN_POINT('Ctrl Pts',(-19.6491985691499,23.0367216738079,-37.9301331968882));
#57141=CARTESIAN_POINT('Ctrl Pts',(-19.635740698941,23.1520684169209,-37.9242813268048));
#57142=CARTESIAN_POINT('Ctrl Pts',(-19.6274075707139,23.2678053470534,-37.9184294567214));
#57143=CARTESIAN_POINT('Ctrl Pts',(-19.6190757112813,23.3835246551859,-37.9125784776384));
#57144=CARTESIAN_POINT('Ctrl Pts',(-19.615867072046,23.4996336200104,-37.9067274985554));
#57145=CARTESIAN_POINT('Ctrl Pts',(-19.6177961866868,23.6156443860121,-37.9008765194725));
#57146=CARTESIAN_POINT('Ctrl Pts',(-19.6197254747736,23.7316655824983,-37.8950250143302));
#57147=CARTESIAN_POINT('Ctrl Pts',(-19.6267934281445,23.8475881492598,-37.8891735091879));
#57148=CARTESIAN_POINT('Ctrl Pts',(-19.6389624681078,23.9629255723573,-37.8833220040456));
#57149=CARTESIAN_POINT('Ctrl Pts',(-19.6511355491443,24.078301296502,-37.8774685557458));
#57150=CARTESIAN_POINT('Ctrl Pts',(-19.6684130417542,24.1930910797191,-37.871615107446));
#57151=CARTESIAN_POINT('Ctrl Pts',(-19.6907057488406,24.3068155700227,-37.8657616591463));
#57152=CARTESIAN_POINT('Ctrl Pts',(-19.7130238075758,24.4206693897666,-37.8599015542047));
#57153=CARTESIAN_POINT('Ctrl Pts',(-19.7403683850107,24.5334550926377,-37.8540414492632));
#57154=CARTESIAN_POINT('Ctrl Pts',(-19.772599575746,24.6447054289975,-37.8481813443216));
#57155=CARTESIAN_POINT('Ctrl Pts',(-19.8048524721711,24.7560306854963,-37.8423172929662));
#57156=CARTESIAN_POINT('Ctrl Pts',(-19.8419984024251,24.8658181260177,-37.8364532416107));
#57157=CARTESIAN_POINT('Ctrl Pts',(-19.8838487884123,24.9736191714777,-37.8305891902552));
#57158=CARTESIAN_POINT('Ctrl Pts',(-19.9257608535142,25.0815790941592,-37.8247164964587));
#57159=CARTESIAN_POINT('Ctrl Pts',(-19.9723910462615,25.1875464020056,-37.8188438026621));
#57160=CARTESIAN_POINT('Ctrl Pts',(-20.0235041983619,25.2910957737288,-37.8129711088655));
#57161=CARTESIAN_POINT('Ctrl Pts',(-20.0374981243883,25.3194458595371,-37.8113632635422));
#57162=CARTESIAN_POINT('Ctrl Pts',(-20.0518278271519,25.3476148663168,-37.8097554182189));
#57163=CARTESIAN_POINT('Ctrl Pts',(-20.066487917571,25.375594448537,-37.8081475728955));
#57164=CARTESIAN_POINT('Ctrl Pts',(-20.1200306329556,25.4777836414108,-37.8022752759268));
#57165=CARTESIAN_POINT('Ctrl Pts',(-20.1781631291024,25.5777861804829,-37.7964029789581));
#57166=CARTESIAN_POINT('Ctrl Pts',(-20.24068283893,25.675161341205,-37.7905306819894));
#57167=CARTESIAN_POINT('Ctrl Pts',(-20.303121528179,25.7724103114523,-37.7846659950512));
#57168=CARTESIAN_POINT('Ctrl Pts',(-20.3699359034493,25.8670383297756,-37.778801308113));
#57169=CARTESIAN_POINT('Ctrl Pts',(-20.440876914766,25.9586279743635,-37.7729366211748));
#57170=CARTESIAN_POINT('Ctrl Pts',(-20.5117449676936,26.0501234247356,-37.7670779657));
#57171=CARTESIAN_POINT('Ctrl Pts',(-20.586730963546,26.138586391865,-37.7612193102251));
#57172=CARTESIAN_POINT('Ctrl Pts',(-20.6655422153237,26.2236278122385,-37.7553606547503));
#57173=CARTESIAN_POINT('Ctrl Pts',(-20.7474319040116,26.3119910253952,-37.7492731550324));
#57174=CARTESIAN_POINT('Ctrl Pts',(-20.8334515307957,26.3966595627834,-37.7431856553145));
#57175=CARTESIAN_POINT('Ctrl Pts',(-20.9232258997385,26.4772339246989,-37.7370981555966));
#57176=CARTESIAN_POINT('Ctrl Pts',(-21.0095253606368,26.554689484425,-37.7312462855132));
#57177=CARTESIAN_POINT('Ctrl Pts',(-21.0992939615664,26.6283616209793,-37.7253944154298));
#57178=CARTESIAN_POINT('Ctrl Pts',(-21.1921609736767,26.6979331387455,-37.7195425453464));
#57179=CARTESIAN_POINT('Ctrl Pts',(-21.2850138459401,26.7674940636155,-37.7136915662634));
#57180=CARTESIAN_POINT('Ctrl Pts',(-21.3809638606217,26.8329553633358,-37.7078405871804));
#57181=CARTESIAN_POINT('Ctrl Pts',(-21.4796084327609,26.8940411038908,-37.7019896080974));
#57182=CARTESIAN_POINT('Ctrl Pts',(-21.5782618739963,26.9551323366416,-37.6961381029551));
#57183=CARTESIAN_POINT('Ctrl Pts',(-21.6796100028192,27.0118470105239,-37.6902865978128));
#57184=CARTESIAN_POINT('Ctrl Pts',(-21.7832231940134,27.0639537597122,-37.6844350926705));
#57185=CARTESIAN_POINT('Ctrl Pts',(-21.8868707928928,27.1160778124176,-37.6785816443707));
#57186=CARTESIAN_POINT('Ctrl Pts',(-21.9927845806855,27.163590712112,-37.6727281960709));
#57187=CARTESIAN_POINT('Ctrl Pts',(-22.100513055711,27.2063083917401,-37.6668747477712));
#57188=CARTESIAN_POINT('Ctrl Pts',(-22.2083640414052,27.2490746506458,-37.6610146428296));
#57189=CARTESIAN_POINT('Ctrl Pts',(-22.3180334488997,27.2870346525829,-37.6551545378881));
#57190=CARTESIAN_POINT('Ctrl Pts',(-22.4290525484346,27.3200535340733,-37.6492944329465));
#57191=CARTESIAN_POINT('Ctrl Pts',(-22.5401464123844,27.3530946517138,-37.6434303815911));
#57192=CARTESIAN_POINT('Ctrl Pts',(-22.6525913781656,27.3811879231691,-37.6375663302356));
#57193=CARTESIAN_POINT('Ctrl Pts',(-22.7659081142131,27.4042495263435,-37.6317022788802));
#57194=CARTESIAN_POINT('Ctrl Pts',(-22.8793918565097,27.4273451177176,-37.6258295850836));
#57195=CARTESIAN_POINT('Ctrl Pts',(-22.9937495265209,27.4453941763504,-37.619956891287));
#57196=CARTESIAN_POINT('Ctrl Pts',(-23.1084961758793,27.458364649085,-37.6140841974904));
#57197=CARTESIAN_POINT('Ctrl Pts',(-23.1399118889956,27.4619157475502,-37.6124763521672));
#57198=CARTESIAN_POINT('Ctrl Pts',(-23.1713567588479,27.4650864705212,-37.6108685068439));
#57199=CARTESIAN_POINT('Ctrl Pts',(-23.202820851174,27.4678768408095,-37.6092606615206));
#57200=CARTESIAN_POINT('Ctrl Pts',(-23.3177364411962,27.4780680468591,-37.6033883645519));
#57201=CARTESIAN_POINT('Ctrl Pts',(-23.4332933337633,27.4832158142665,-37.5975160675832));
#57202=CARTESIAN_POINT('Ctrl Pts',(-23.5490112438236,27.4832523358137,-37.5916437706145));
#57203=CARTESIAN_POINT('Ctrl Pts',(-23.6645791926627,27.483288810032,-37.5857790836763));
#57204=CARTESIAN_POINT('Ctrl Pts',(-23.7803073344661,27.4782272105591,-37.5799143967381));
#57205=CARTESIAN_POINT('Ctrl Pts',(-23.895709863191,27.468051433133,-37.5740497098));
#57206=CARTESIAN_POINT('Ctrl Pts',(-24.0109937076391,27.457886120857,-37.5681910543252));
#57207=CARTESIAN_POINT('Ctrl Pts',(-24.1259521957782,27.4426171283577,-37.5623323988503));
#57208=CARTESIAN_POINT('Ctrl Pts',(-24.2400997922157,27.4222803927963,-37.5564737433755));
#57209=CARTESIAN_POINT('Ctrl Pts',(-24.3587060943105,27.4011492864314,-37.5503862436576));
#57210=CARTESIAN_POINT('Ctrl Pts',(-24.4764364103125,27.3745464649719,-37.5442987439397));
#57211=CARTESIAN_POINT('Ctrl Pts',(-24.5927518251079,27.3425716405288,-37.5382112442218));
#57212=CARTESIAN_POINT('Ctrl Pts',(-24.7045650041831,27.3118344697278,-37.5323593741384));
#57213=CARTESIAN_POINT('Ctrl Pts',(-24.8150703431188,27.2761335525973,-37.526507504055));
#57214=CARTESIAN_POINT('Ctrl Pts',(-24.923800585261,27.235609331862,-37.5206556339717));
#57215=CARTESIAN_POINT('Ctrl Pts',(-25.0325142722349,27.1950912813079,-37.5148046548887));
#57216=CARTESIAN_POINT('Ctrl Pts',(-25.13945301256,27.149751531684,-37.5089536758058));
#57217=CARTESIAN_POINT('Ctrl Pts',(-25.2441670440814,27.099779630439,-37.5031026967228));
#57218=CARTESIAN_POINT('Ctrl Pts',(-25.3488904904021,27.0498032362392,-37.4972511915805));
#57219=CARTESIAN_POINT('Ctrl Pts',(-25.4513884571926,26.9951940405561,-37.4913996864383));
#57220=CARTESIAN_POINT('Ctrl Pts',(-25.5512340618596,26.9361884312553,-37.485548181296));
#57221=CARTESIAN_POINT('Ctrl Pts',(-25.6511128230791,26.8771632274758,-37.4796947329962));
#57222=CARTESIAN_POINT('Ctrl Pts',(-25.7483371150815,26.8137389172578,-37.4738412846964));
#57223=CARTESIAN_POINT('Ctrl Pts',(-25.8425080233662,26.746195860494,-37.4679878363966));
#57224=CARTESIAN_POINT('Ctrl Pts',(-25.9367860244216,26.6785759926084,-37.4621277314551));
#57225=CARTESIAN_POINT('Ctrl Pts',(-26.0280033749201,26.6068282703091,-37.4562676265136));
#57226=CARTESIAN_POINT('Ctrl Pts',(-26.115793243649,26.5312741443805,-37.4504075215721));
#57227=CARTESIAN_POINT('Ctrl Pts',(-26.2036422333607,26.455669137476,-37.4445434702166));
#57228=CARTESIAN_POINT('Ctrl Pts',(-26.2880588448778,26.3762529053144,-37.4386794188611));
#57229=CARTESIAN_POINT('Ctrl Pts',(-26.3687134582335,26.2933834081876,-37.4328153675056));
#57230=CARTESIAN_POINT('Ctrl Pts',(-26.4494869403885,26.2103917779649,-37.4269426737091));
#57231=CARTESIAN_POINT('Ctrl Pts',(-26.5264870848545,26.1239370328087,-37.4210699799125));
#57232=CARTESIAN_POINT('Ctrl Pts',(-26.5994247896218,26.0344098418268,-37.415197286116));
#57233=CARTESIAN_POINT('Ctrl Pts',(-26.6193939130889,26.0098987945421,-37.4135894407926));
#57234=CARTESIAN_POINT('Ctrl Pts',(-26.6390587807226,25.9851576081264,-37.4119815954692));
#57235=CARTESIAN_POINT('Ctrl Pts',(-26.6584140418247,25.9601946527716,-37.4103737501458));
#57236=CARTESIAN_POINT('Ctrl Pts',(-26.7291514682649,25.8689628575081,-37.4044975783034));
#57237=CARTESIAN_POINT('Ctrl Pts',(-26.7959908196883,25.7744564661028,-37.3986214064611));
#57238=CARTESIAN_POINT('Ctrl Pts',(-26.8586138433327,25.677042232547,-37.3927452346187));
#57239=CARTESIAN_POINT('Ctrl Pts',(-26.9211569946811,25.5797522456028,-37.3868765575173));
#57240=CARTESIAN_POINT('Ctrl Pts',(-26.9794942885468,25.4795621324493,-37.3810078804158));
#57241=CARTESIAN_POINT('Ctrl Pts',(-27.0333477349422,25.3768714862413,-37.3751392033143));
#57242=CARTESIAN_POINT('Ctrl Pts',(-27.087145447102,25.2742871170695,-37.3692765998489));
#57243=CARTESIAN_POINT('Ctrl Pts',(-27.1364683490371,25.1692077231058,-37.3634139963835));
#57244=CARTESIAN_POINT('Ctrl Pts',(-27.1810821829406,25.0620610657453,-37.3575513929181));
#57245=CARTESIAN_POINT('Ctrl Pts',(-27.2256605731297,24.9549995316571,-37.3516934470314));
#57246=CARTESIAN_POINT('Ctrl Pts',(-27.2655371788725,24.8458743797659,-37.3458355011447));
#57247=CARTESIAN_POINT('Ctrl Pts',(-27.3005243861613,24.735136499681,-37.339977555258));
#57248=CARTESIAN_POINT('Ctrl Pts',(-27.3354938900251,24.6244546526406,-37.3341225734748));
#57249=CARTESIAN_POINT('Ctrl Pts',(-27.3655787921991,24.5121620925942,-37.3282675916916));
#57250=CARTESIAN_POINT('Ctrl Pts',(-27.3906404183595,24.3987275637102,-37.3224126099085));
#57251=CARTESIAN_POINT('Ctrl Pts',(-27.4156946046748,24.28532670923,-37.316559366247));
#57252=CARTESIAN_POINT('Ctrl Pts',(-27.4357283956122,24.1707849630344,-37.3107061225856));
#57253=CARTESIAN_POINT('Ctrl Pts',(-27.4506537679473,24.0555833107248,-37.3048528789242));
#57254=CARTESIAN_POINT('Ctrl Pts',(-27.4655812071526,23.9403657052536,-37.2989988247037));
#57255=CARTESIAN_POINT('Ctrl Pts',(-27.4753987597261,23.8244884195871,-37.2931447704833));
#57256=CARTESIAN_POINT('Ctrl Pts',(-27.480070080354,23.7084392386109,-37.2872907162628));
#57257=CARTESIAN_POINT('Ctrl Pts',(-27.4822318146903,23.6547354749008,-37.2845816515201));
#57258=CARTESIAN_POINT('Ctrl Pts',(-27.4832921953411,23.6009949538121,-37.2818725867774));
#57259=CARTESIAN_POINT('Ctrl Pts',(-27.4832513978708,23.5472661202319,-37.2791635220347));
#57260=CARTESIAN_POINT('',(-27.4892186348263,23.5489291036097,-36.0291635220347));
#57261=CARTESIAN_POINT('Ctrl Pts',(-27.4793303240496,23.5472396509144,-37.2791620358212));
#57262=CARTESIAN_POINT('Ctrl Pts',(-27.4824652871287,23.1002827872345,-37.2566036368044));
#57263=CARTESIAN_POINT('Ctrl Pts',(-27.2053647626636,21.343565728798,-37.1677496006624));
#57264=CARTESIAN_POINT('Ctrl Pts',(-24.614878454963,19.0217514026673,-37.012599927396));
#57265=CARTESIAN_POINT('Ctrl Pts',(-20.3158239957554,20.2067180428611,-36.813713016021));
#57266=CARTESIAN_POINT('Ctrl Pts',(-18.9889351267585,24.4641093933195,-36.6148261046462));
#57267=CARTESIAN_POINT('Ctrl Pts',(-21.8535102169566,27.881743770226,-36.4159391932714));
#57268=CARTESIAN_POINT('Ctrl Pts',(-26.1957055928295,27.3294759798774,-36.2207183324008));
#57269=CARTESIAN_POINT('Ctrl Pts',(-27.4838407068465,24.7818274601648,-36.0917931086553));
#57270=CARTESIAN_POINT('Ctrl Pts',(-27.4892186348263,23.5489291036097,-36.0291635220347));
#57271=CARTESIAN_POINT('',(-27.4833700092727,23.5538806451607,-34.7791635220347));
#57272=CARTESIAN_POINT('Ctrl Pts',(-27.4892186348263,23.5489291036097,-36.0291635220347));
#57273=CARTESIAN_POINT('Ctrl Pts',(-27.489533434215,23.4767608539724,-36.0254974715303));
#57274=CARTESIAN_POINT('Ctrl Pts',(-27.4549757162681,22.099833590961,-35.9555357839008));
#57275=CARTESIAN_POINT('Ctrl Pts',(-25.8447397533594,19.503515670751,-35.8192784591468));
#57276=CARTESIAN_POINT('Ctrl Pts',(-21.3859325269578,19.4324291079409,-35.6203915477717));
#57277=CARTESIAN_POINT('Ctrl Pts',(-18.9159518808349,23.1452731377106,-35.4215046363969));
#57278=CARTESIAN_POINT('Ctrl Pts',(-20.7045006089515,27.2302588939586,-35.222617725022));
#57279=CARTESIAN_POINT('Ctrl Pts',(-25.1080540740967,27.9336308163746,-35.023730813647));
#57280=CARTESIAN_POINT('Ctrl Pts',(-27.316972897996,25.462713316296,-34.8759127459847));
#57281=CARTESIAN_POINT('Ctrl Pts',(-27.4861582946516,23.8547890233352,-34.7943903154472));
#57282=CARTESIAN_POINT('Ctrl Pts',(-27.4833700092727,23.5538806451607,-34.7791635220347));
#57283=CARTESIAN_POINT('',(-27.4767519051405,23.5499334425378,-33.5291635220347));
#57284=CARTESIAN_POINT('Ctrl Pts',(-27.4833700092727,23.5538806451607,-34.7791635220347));
#57285=CARTESIAN_POINT('Ctrl Pts',(-27.4740184336399,22.5446699387121,-34.7280946783222));
#57286=CARTESIAN_POINT('Ctrl Pts',(-26.5635452019007,20.2103566681747,-34.6107301974847));
#57287=CARTESIAN_POINT('Ctrl Pts',(-22.6305263658179,18.9901149666739,-34.4270700795225));
#57288=CARTESIAN_POINT('Ctrl Pts',(-19.2165813045135,21.8590859145908,-34.2281831681474));
#57289=CARTESIAN_POINT('Ctrl Pts',(-19.7849126662585,26.2820955963449,-34.0292962567727));
#57290=CARTESIAN_POINT('Ctrl Pts',(-23.8132721161679,28.1947731237778,-33.8304093453977));
#57291=CARTESIAN_POINT('Ctrl Pts',(-26.9873304880107,26.2205621386255,-33.6636984338185));
#57292=CARTESIAN_POINT('Ctrl Pts',(-27.4762637887713,24.2270688085383,-33.5632831593641));
#57293=CARTESIAN_POINT('Ctrl Pts',(-27.4767519051405,23.5499334425378,-33.5291635220347));
#57294=CARTESIAN_POINT('',(-27.4845450668246,23.5467337760579,-32.2791635220347));
#57295=CARTESIAN_POINT('Ctrl Pts',(-27.4767519051405,23.5499334425378,-33.5291635220347));
#57296=CARTESIAN_POINT('Ctrl Pts',(-27.4772122157835,22.9113713386183,-33.4969875222391));
#57297=CARTESIAN_POINT('Ctrl Pts',(-27.0277930863398,20.9577225774089,-33.3985158853185));
#57298=CARTESIAN_POINT('Ctrl Pts',(-23.9492676055535,18.9154345414229,-33.2337486112731));
#57299=CARTESIAN_POINT('Ctrl Pts',(-19.8665869552278,20.7092388476606,-33.0348616998981));
#57300=CARTESIAN_POINT('Ctrl Pts',(-19.1688826463395,25.1136938512856,-32.8359747885233));
#57301=CARTESIAN_POINT('Ctrl Pts',(-22.4972857831852,28.0814788401733,-32.6370878771483));
#57302=CARTESIAN_POINT('Ctrl Pts',(-26.5063577130066,26.9653307208194,-32.4514841216523));
#57303=CARTESIAN_POINT('Ctrl Pts',(-27.4748464854124,24.5935520426802,-32.332176003281));
#57304=CARTESIAN_POINT('Ctrl Pts',(-27.4845450668246,23.5467337760579,-32.2791635220347));
#57305=CARTESIAN_POINT('',(-27.4885670794543,23.5522069440821,-31.0291635220347));
#57306=CARTESIAN_POINT('Ctrl Pts',(-27.4845450668246,23.5467337760579,-32.2791635220347));
#57307=CARTESIAN_POINT('Ctrl Pts',(-27.4869752071552,23.2844361079365,-32.265880366156));
#57308=CARTESIAN_POINT('Ctrl Pts',(-27.3433199675825,21.7156705685443,-32.1863015731523));
#57309=CARTESIAN_POINT('Ctrl Pts',(-25.2358406503036,19.2144084931583,-32.0404271430236));
#57310=CARTESIAN_POINT('Ctrl Pts',(-20.8135660294717,19.7884314539895,-31.8415402316489));
#57311=CARTESIAN_POINT('Ctrl Pts',(-18.9060742714317,23.8192490354008,-31.642653320274));
#57312=CARTESIAN_POINT('Ctrl Pts',(-21.2661885731902,27.6028816370503,-31.443766408899));
#57313=CARTESIAN_POINT('Ctrl Pts',(-25.7251639961269,27.6624916971592,-31.2448794975241));
#57314=CARTESIAN_POINT('Ctrl Pts',(-27.4348385173242,25.0781310411118,-31.106678535236));
#57315=CARTESIAN_POINT('Ctrl Pts',(-27.4892390080544,23.6626852313028,-31.0347732100729));
#57316=CARTESIAN_POINT('Ctrl Pts',(-27.4885670794543,23.5522069440821,-31.0291635220347));
#57317=CARTESIAN_POINT('',(-27.4784969839717,23.5528208098879,-29.7791635220347));
#57318=CARTESIAN_POINT('Ctrl Pts',(-27.4885670794543,23.5522069440821,-31.0291635220347));
#57319=CARTESIAN_POINT('Ctrl Pts',(-27.4812981146679,22.3570460602959,-30.9684775729479));
#57320=CARTESIAN_POINT('Ctrl Pts',(-26.2622685644213,19.8434146916342,-30.8414959867364));
#57321=CARTESIAN_POINT('Ctrl Pts',(-21.9811740242355,19.1708983019553,-30.6482187633994));
#57322=CARTESIAN_POINT('Ctrl Pts',(-19.0176748890843,22.5031179912306,-30.4493318520245));
#57323=CARTESIAN_POINT('Ctrl Pts',(-20.2192303082857,26.7975655408241,-30.2504449406496));
#57324=CARTESIAN_POINT('Ctrl Pts',(-24.4817127266861,28.1080077617663,-30.0515580292749));
#57325=CARTESIAN_POINT('Ctrl Pts',(-27.1724268576346,25.8349750791294,-29.8944642230698));
#57326=CARTESIAN_POINT('Ctrl Pts',(-27.481392228598,24.0385560742375,-29.8036660539898));
#57327=CARTESIAN_POINT('Ctrl Pts',(-27.4784969839717,23.5528208098879,-29.7791635220347));
#57328=CARTESIAN_POINT('',(-27.4826813963389,23.5473322497447,-28.5291634804562));
#57329=CARTESIAN_POINT('Ctrl Pts',(-27.4784969839717,23.5528208098879,-29.7791635220347));
#57330=CARTESIAN_POINT('Ctrl Pts',(-27.4735586672547,22.7243192891093,-29.7373704168648));
#57331=CARTESIAN_POINT('Ctrl Pts',(-26.8116566502793,20.5743666249437,-29.62928167457));
#57332=CARTESIAN_POINT('Ctrl Pts',(-23.2752795542552,18.9064242947988,-29.4548972951501));
#57333=CARTESIAN_POINT('Ctrl Pts',(-19.49468736946,21.2714058832831,-29.2560103837753));
#57334=CARTESIAN_POINT('Ctrl Pts',(-19.440815713535,25.7304543273257,-29.0571234724003));
#57335=CARTESIAN_POINT('Ctrl Pts',(-23.1631680707165,28.1860821718098,-28.8582365610254));
#57336=CARTESIAN_POINT('Ctrl Pts',(-26.771662874525,26.5895273166329,-28.6822499109035));
#57337=CARTESIAN_POINT('Ctrl Pts',(-27.4732871731943,24.4072281778359,-28.5725588979067));
#57338=CARTESIAN_POINT('Ctrl Pts',(-27.4791742225268,23.5473356782317,-28.5291635220347));
#57339=CARTESIAN_POINT('',(-27.4847176457149,23.5488150353494,-27.2791635220347));
#57340=CARTESIAN_POINT('Ctrl Pts',(-27.4832514471146,23.5473316924836,-28.5291634736981));
#57341=CARTESIAN_POINT('Ctrl Pts',(-27.4831520660432,23.4135120543238,-28.5224170883845));
#57342=CARTESIAN_POINT('Ctrl Pts',(-27.4762189501434,23.2799706350553,-28.515670703071));
#57343=CARTESIAN_POINT('Ctrl Pts',(-27.4625607997496,23.1473468160422,-28.5089243177574));
#57344=CARTESIAN_POINT('Ctrl Pts',(-27.4488274434656,23.0139927303323,-28.5021407848141));
#57345=CARTESIAN_POINT('Ctrl Pts',(-27.4282949044146,22.8815665128418,-28.4953572518708));
#57346=CARTESIAN_POINT('Ctrl Pts',(-27.4011229596204,22.7506989391669,-28.4885737189276));
#57347=CARTESIAN_POINT('Ctrl Pts',(-27.3737751256306,22.6189842346574,-28.4817462748781));
#57348=CARTESIAN_POINT('Ctrl Pts',(-27.3397017424326,22.4888485496326,-28.4749188308287));
#57349=CARTESIAN_POINT('Ctrl Pts',(-27.299113931195,22.3609135525412,-28.4680913867792));
#57350=CARTESIAN_POINT('Ctrl Pts',(-27.2839969931815,22.3132641385466,-28.4655485039447));
#57351=CARTESIAN_POINT('Ctrl Pts',(-27.2679768501773,22.2659197797332,-28.4630056211102));
#57352=CARTESIAN_POINT('Ctrl Pts',(-27.2510660667031,22.2189117867702,-28.4604627382757));
#57353=CARTESIAN_POINT('Ctrl Pts',(-27.2120138771227,22.1103559025446,-28.454590441307));
#57354=CARTESIAN_POINT('Ctrl Pts',(-27.1681158137966,22.0033378902036,-28.4487181443383));
#57355=CARTESIAN_POINT('Ctrl Pts',(-27.1195122154757,21.8983220520033,-28.4428458473695));
#57356=CARTESIAN_POINT('Ctrl Pts',(-27.0709716035582,21.793442305989,-28.4369811604313));
#57357=CARTESIAN_POINT('Ctrl Pts',(-27.0177377554039,21.6905599459593,-28.4311164734931));
#57358=CARTESIAN_POINT('Ctrl Pts',(-26.9600002446536,21.590122552849,-28.4252517865549));
#57359=CARTESIAN_POINT('Ctrl Pts',(-26.9023221133187,21.4897884533098,-28.41939313108));
#57360=CARTESIAN_POINT('Ctrl Pts',(-26.8401497369302,21.3918946754604,-28.4135344756052));
#57361=CARTESIAN_POINT('Ctrl Pts',(-26.7737197968873,21.2968666814172,-28.4076758201303));
#57362=CARTESIAN_POINT('Ctrl Pts',(-26.7046950448759,21.1981268102276,-28.4015883204124));
#57363=CARTESIAN_POINT('Ctrl Pts',(-26.6310735312265,21.1024815795914,-28.3955008206945));
#57364=CARTESIAN_POINT('Ctrl Pts',(-26.5531722413835,21.0103780826005,-28.3894133209766));
#57365=CARTESIAN_POINT('Ctrl Pts',(-26.4782862867854,20.9218396475129,-28.3835614508932));
#57366=CARTESIAN_POINT('Ctrl Pts',(-26.3994460029958,20.8365742086214,-28.3777095808098));
#57367=CARTESIAN_POINT('Ctrl Pts',(-26.3169752153742,20.7549467180826,-28.3718577107264));
#57368=CARTESIAN_POINT('Ctrl Pts',(-26.2345169846798,20.6733316560714,-28.3660067316434));
#57369=CARTESIAN_POINT('Ctrl Pts',(-26.1484296429749,20.595353731781,-28.3601557525604));
#57370=CARTESIAN_POINT('Ctrl Pts',(-26.0590742194072,20.5213413842254,-28.3543047734774));
#57371=CARTESIAN_POINT('Ctrl Pts',(-25.9697107619269,20.4473223822474,-28.3484532683351));
#57372=CARTESIAN_POINT('Ctrl Pts',(-25.8770789568492,20.3772699294884,-28.3426017631928));
#57373=CARTESIAN_POINT('Ctrl Pts',(-25.7815727191508,20.3114720172029,-28.3367502580505));
#57374=CARTESIAN_POINT('Ctrl Pts',(-25.6860347659098,20.245652254863,-28.3308968097507));
#57375=CARTESIAN_POINT('Ctrl Pts',(-25.5876208222482,20.1840900767421,-28.3250433614509));
#57376=CARTESIAN_POINT('Ctrl Pts',(-25.4867529475112,20.1270296146845,-28.3191899131511));
#57377=CARTESIAN_POINT('Ctrl Pts',(-25.3857703640979,20.0699042624912,-28.3133298082095));
#57378=CARTESIAN_POINT('Ctrl Pts',(-25.2823286395667,20.0172910482452,-28.307469703268));
#57379=CARTESIAN_POINT('Ctrl Pts',(-25.1768736337033,19.969387721275,-28.3016095983264));
#57380=CARTESIAN_POINT('Ctrl Pts',(-25.0713476104936,19.9214521344121,-28.2957455469709));
#57381=CARTESIAN_POINT('Ctrl Pts',(-24.9638059888764,19.8782329043096,-28.2898814956155));
#57382=CARTESIAN_POINT('Ctrl Pts',(-24.8547121167039,19.8398786703325,-28.28401744426));
#57383=CARTESIAN_POINT('Ctrl Pts',(-24.7454574619413,19.8014679098708,-28.2781447504634));
#57384=CARTESIAN_POINT('Ctrl Pts',(-24.6346463849799,19.7679365748156,-28.2722720566669));
#57385=CARTESIAN_POINT('Ctrl Pts',(-24.5227548832301,19.7393827915618,-28.2663993628703));
#57386=CARTESIAN_POINT('Ctrl Pts',(-24.4921208617703,19.7315652433541,-28.2647915175471));
#57387=CARTESIAN_POINT('Ctrl Pts',(-24.4614058959691,19.7241205002501,-28.2631836722239));
#57388=CARTESIAN_POINT('Ctrl Pts',(-24.4306198297197,19.7170498993556,-28.2615758269007));
#57389=CARTESIAN_POINT('Ctrl Pts',(-24.3181805789353,19.6912261042424,-28.255703529932));
#57390=CARTESIAN_POINT('Ctrl Pts',(-24.2044157653797,19.6703105089654,-28.2498312329633));
#57391=CARTESIAN_POINT('Ctrl Pts',(-24.0897918733749,19.6544360192313,-28.2439589359946));
#57392=CARTESIAN_POINT('Ctrl Pts',(-23.975316524831,19.6385821015751,-28.2380942490564));
#57393=CARTESIAN_POINT('Ctrl Pts',(-23.8599847174821,19.6277563541091,-28.2322295621182));
#57394=CARTESIAN_POINT('Ctrl Pts',(-23.7442754812678,19.6220412218181,-28.22636487518));
#57395=CARTESIAN_POINT('Ctrl Pts',(-23.6286852447595,19.6163319671828,-28.2205062197052));
#57396=CARTESIAN_POINT('Ctrl Pts',(-23.5127187618572,19.6157228936424,-28.2146475642303));
#57397=CARTESIAN_POINT('Ctrl Pts',(-23.3968619173076,19.6202448574755,-28.2087889087555));
#57398=CARTESIAN_POINT('Ctrl Pts',(-23.2764796023646,19.6249434531987,-28.2027014090376));
#57399=CARTESIAN_POINT('Ctrl Pts',(-23.156216115906,19.6351821660239,-28.1966139093197));
#57400=CARTESIAN_POINT('Ctrl Pts',(-23.0366189489219,19.6509359835478,-28.1905264096018));
#57401=CARTESIAN_POINT('Ctrl Pts',(-22.9216510448618,19.6660800160307,-28.1846745395184));
#57402=CARTESIAN_POINT('Ctrl Pts',(-22.8072992848527,19.6863200852052,-28.178822669435));
#57403=CARTESIAN_POINT('Ctrl Pts',(-22.6940457506019,19.7115810234753,-28.1729707993516));
#57404=CARTESIAN_POINT('Ctrl Pts',(-22.5808094602314,19.7368381155378,-28.1671198202686));
#57405=CARTESIAN_POINT('Ctrl Pts',(-22.4686714665002,19.7671144667109,-28.1612688411857));
#57406=CARTESIAN_POINT('Ctrl Pts',(-22.3581032422207,19.8022838723258,-28.1554178621027));
#57407=CARTESIAN_POINT('Ctrl Pts',(-22.2475250767937,19.8374564400087,-28.1495663569604));
#57408=CARTESIAN_POINT('Ctrl Pts',(-22.1385173553449,19.8775228113692,-28.1437148518181));
#57409=CARTESIAN_POINT('Ctrl Pts',(-22.0315352974928,19.9223072506102,-28.1378633466758));
#57410=CARTESIAN_POINT('Ctrl Pts',(-21.9245177132281,19.9671065617886,-28.132009898376));
#57411=CARTESIAN_POINT('Ctrl Pts',(-21.8195275112575,20.016626896724,-28.1261564500762));
#57412=CARTESIAN_POINT('Ctrl Pts',(-21.7169982247661,20.0706451334193,-28.1203030017764));
#57413=CARTESIAN_POINT('Ctrl Pts',(-21.6143523402122,20.1247248005795,-28.1144428968349));
#57414=CARTESIAN_POINT('Ctrl Pts',(-21.5141733229946,20.1833123862658,-28.1085827918934));
#57415=CARTESIAN_POINT('Ctrl Pts',(-21.4168685490566,20.246139673055,-28.1027226869518));
#57416=CARTESIAN_POINT('Ctrl Pts',(-21.3194982464434,20.3090092700896,-28.0968586355964));
#57417=CARTESIAN_POINT('Ctrl Pts',(-21.2250063775183,20.3761240146521,-28.0909945842409));
#57418=CARTESIAN_POINT('Ctrl Pts',(-21.1337684542299,20.4471744302985,-28.0851305328855));
#57419=CARTESIAN_POINT('Ctrl Pts',(-21.0423960644554,20.5183295600745,-28.0792578390889));
#57420=CARTESIAN_POINT('Ctrl Pts',(-20.9542875049638,20.5934316702461,-28.0733851452923));
#57421=CARTESIAN_POINT('Ctrl Pts',(-20.8697826279166,20.6721333376818,-28.0675124514957));
#57422=CARTESIAN_POINT('Ctrl Pts',(-20.8466466061759,20.6936805377068,-28.0659046061725));
#57423=CARTESIAN_POINT('Ctrl Pts',(-20.823780477776,20.7154973545272,-28.0642967608492));
#57424=CARTESIAN_POINT('Ctrl Pts',(-20.801190688688,20.7375762290729,-28.0626889155259));
#57425=CARTESIAN_POINT('Ctrl Pts',(-20.7186865148945,20.8182144012839,-28.0568166185572));
#57426=CARTESIAN_POINT('Ctrl Pts',(-20.6395951691016,20.9026208817799,-28.0509443215885));
#57427=CARTESIAN_POINT('Ctrl Pts',(-20.5642806216622,20.9904750506424,-28.0450720246198));
#57428=CARTESIAN_POINT('Ctrl Pts',(-20.4890636758949,21.0782153674793,-28.0392073376817));
#57429=CARTESIAN_POINT('Ctrl Pts',(-20.4176140617805,21.1693941766258,-28.0333426507435));
#57430=CARTESIAN_POINT('Ctrl Pts',(-20.3502600776578,21.2636530271656,-28.0274779638053));
#57431=CARTESIAN_POINT('Ctrl Pts',(-20.2829753628914,21.3578149383784,-28.0216193083305));
#57432=CARTESIAN_POINT('Ctrl Pts',(-20.2197781389261,21.4550502560889,-28.0157606528557));
#57433=CARTESIAN_POINT('Ctrl Pts',(-20.1609570069702,21.5549668764342,-28.0099019973809));
#57434=CARTESIAN_POINT('Ctrl Pts',(-20.0998382697911,21.658786327976,-28.003814497663));
#57435=CARTESIAN_POINT('Ctrl Pts',(-20.0434447579164,21.765500475276,-27.997726997945));
#57436=CARTESIAN_POINT('Ctrl Pts',(-19.9920513700819,21.874635184714,-27.9916394982271));
#57437=CARTESIAN_POINT('Ctrl Pts',(-19.9426472727203,21.9795456029174,-27.9857876281438));
#57438=CARTESIAN_POINT('Ctrl Pts',(-19.8978636085097,22.0866922726609,-27.9799357580604));
#57439=CARTESIAN_POINT('Ctrl Pts',(-19.8578977232899,22.1956289792436,-27.974083887977));
#57440=CARTESIAN_POINT('Ctrl Pts',(-19.8179379232396,22.3045490992222,-27.968232908894));
#57441=CARTESIAN_POINT('Ctrl Pts',(-19.7827945859869,22.4152583261415,-27.9623819298111));
#57442=CARTESIAN_POINT('Ctrl Pts',(-19.7526163844688,22.5272917830402,-27.9565309507281));
#57443=CARTESIAN_POINT('Ctrl Pts',(-19.7224354696399,22.6393353128249,-27.9506794455858));
#57444=CARTESIAN_POINT('Ctrl Pts',(-19.6972206855005,22.7527029100921,-27.9448279404435));
#57445=CARTESIAN_POINT('Ctrl Pts',(-19.6770702480778,22.8669165982909,-27.9389764353013));
#57446=CARTESIAN_POINT('Ctrl Pts',(-19.6569131191335,22.9811682143692,-27.9331229870015));
#57447=CARTESIAN_POINT('Ctrl Pts',(-19.6418237527632,23.0962660731868,-27.9272695387017));
#57448=CARTESIAN_POINT('Ctrl Pts',(-19.6318487757525,23.2117248291026,-27.921416090402));
#57449=CARTESIAN_POINT('Ctrl Pts',(-19.6218624550269,23.3273148866953,-27.9155559854605));
#57450=CARTESIAN_POINT('Ctrl Pts',(-19.6170021681654,23.4432662484759,-27.9096958805189));
#57451=CARTESIAN_POINT('Ctrl Pts',(-19.6172624633169,23.5590911993404,-27.9038357755774));
#57452=CARTESIAN_POINT('Ctrl Pts',(-19.617522933761,23.6749941510601,-27.897971724222));
#57453=CARTESIAN_POINT('Ctrl Pts',(-19.6229108334802,23.7907701104263,-27.8921076728665));
#57454=CARTESIAN_POINT('Ctrl Pts',(-19.6333687748771,23.9059358677986,-27.8862436215111));
#57455=CARTESIAN_POINT('Ctrl Pts',(-19.643842129192,24.021271356508,-27.8803709277145));
#57456=CARTESIAN_POINT('Ctrl Pts',(-19.6594003829685,24.1359944402673,-27.874498233918));
#57457=CARTESIAN_POINT('Ctrl Pts',(-19.6799349477978,24.2496313988199,-27.8686255401214));
#57458=CARTESIAN_POINT('Ctrl Pts',(-19.6855569681471,24.28074329716,-27.867017694798));
#57459=CARTESIAN_POINT('Ctrl Pts',(-19.6915517104226,24.3117738690118,-27.8654098494745));
#57460=CARTESIAN_POINT('Ctrl Pts',(-19.6979162993722,24.3427136052739,-27.8638020041511));
#57461=CARTESIAN_POINT('Ctrl Pts',(-19.7211615430849,24.455714101537,-27.8579297071824));
#57462=CARTESIAN_POINT('Ctrl Pts',(-19.7494219059978,24.5678802587197,-27.8520574102136));
#57463=CARTESIAN_POINT('Ctrl Pts',(-19.7826243865996,24.6787325537996,-27.8461851132449));
#57464=CARTESIAN_POINT('Ctrl Pts',(-19.8157838394234,24.7894411931088,-27.8403204263067));
#57465=CARTESIAN_POINT('Ctrl Pts',(-19.853872555986,24.8988389639505,-27.8344557393685));
#57466=CARTESIAN_POINT('Ctrl Pts',(-19.8967664246872,25.006455905508,-27.8285910524303));
#57467=CARTESIAN_POINT('Ctrl Pts',(-19.9396161797296,25.113962169778,-27.8227323969555));
#57468=CARTESIAN_POINT('Ctrl Pts',(-19.9872611052841,25.2196908659592,-27.8168737414807));
#57469=CARTESIAN_POINT('Ctrl Pts',(-20.0395273189796,25.3231872402522,-27.8110150860059));
#57470=CARTESIAN_POINT('Ctrl Pts',(-20.0938350970176,25.4307262740836,-27.804927586288));
#57471=CARTESIAN_POINT('Ctrl Pts',(-20.1531324157586,25.5358546023575,-27.7988400865701));
#57472=CARTESIAN_POINT('Ctrl Pts',(-20.2171689730529,25.6380846588336,-27.7927525868522));
#57473=CARTESIAN_POINT('Ctrl Pts',(-20.2787268590882,25.7363576833655,-27.7869007167688));
#57474=CARTESIAN_POINT('Ctrl Pts',(-20.3446636810568,25.8319522487235,-27.7810488466854));
#57475=CARTESIAN_POINT('Ctrl Pts',(-20.4147107048366,25.9244611265793,-27.775196976602));
#57476=CARTESIAN_POINT('Ctrl Pts',(-20.4847470633201,26.0169559191173,-27.769345997519));
#57477=CARTESIAN_POINT('Ctrl Pts',(-20.5588921298173,26.1063656288389,-27.763495018436));
#57478=CARTESIAN_POINT('Ctrl Pts',(-20.6368351595661,26.1923138890026,-27.7576440393531));
#57479=CARTESIAN_POINT('Ctrl Pts',(-20.7147851971434,26.278269876742,-27.7517925342108));
#57480=CARTESIAN_POINT('Ctrl Pts',(-20.7965335990762,26.360763490015,-27.7459410290685));
#57481=CARTESIAN_POINT('Ctrl Pts',(-20.8817313255989,26.4394537314412,-27.7400895239262));
#57482=CARTESIAN_POINT('Ctrl Pts',(-20.9669573444319,26.5181701041836,-27.7342360756264));
#57483=CARTESIAN_POINT('Ctrl Pts',(-21.0556346619889,26.5930803133196,-27.7283826273266));
#57484=CARTESIAN_POINT('Ctrl Pts',(-21.1473801525931,26.663882781058,-27.7225291790269));
#57485=CARTESIAN_POINT('Ctrl Pts',(-21.2392299777422,26.7347657665766,-27.7166690740853));
#57486=CARTESIAN_POINT('Ctrl Pts',(-21.3341546127783,26.8015314340299,-27.7108089691438));
#57487=CARTESIAN_POINT('Ctrl Pts',(-21.4317407878446,26.863920739462,-27.7049488642023));
#57488=CARTESIAN_POINT('Ctrl Pts',(-21.5293926810921,26.9263520601866,-27.6990848128468));
#57489=CARTESIAN_POINT('Ctrl Pts',(-21.6297093264324,26.984400943882,-27.6932207614914));
#57490=CARTESIAN_POINT('Ctrl Pts',(-21.7322531710581,27.0378544764016,-27.6873567101359));
#57491=CARTESIAN_POINT('Ctrl Pts',(-21.8349481448411,27.0913867887578,-27.6814840163394));
#57492=CARTESIAN_POINT('Ctrl Pts',(-21.9398764957877,27.1403100590439,-27.6756113225428));
#57493=CARTESIAN_POINT('Ctrl Pts',(-22.0465809784596,27.1844595786293,-27.6697386287463));
#57494=CARTESIAN_POINT('Ctrl Pts',(-22.0757948808678,27.1965469785609,-27.6681307834229));
#57495=CARTESIAN_POINT('Ctrl Pts',(-22.1051418339389,27.2082768408679,-27.6665229380995));
#57496=CARTESIAN_POINT('Ctrl Pts',(-22.1346122833106,27.2196464444755,-27.6649150927761));
#57497=CARTESIAN_POINT('Ctrl Pts',(-22.2422465364298,27.2611713895868,-27.6590427958074));
#57498=CARTESIAN_POINT('Ctrl Pts',(-22.3518897306156,27.2980260351271,-27.6531704988387));
#57499=CARTESIAN_POINT('Ctrl Pts',(-22.4630989746921,27.3300125959704,-27.64729820187));
#57500=CARTESIAN_POINT('Ctrl Pts',(-22.5741641004203,27.3619577047713,-27.6414335149318));
#57501=CARTESIAN_POINT('Ctrl Pts',(-22.68679084653,27.3890471613059,-27.6355688279936));
#57502=CARTESIAN_POINT('Ctrl Pts',(-22.8005167395195,27.4111313490015,-27.6297041410553));
#57503=CARTESIAN_POINT('Ctrl Pts',(-22.9141256725473,27.4331928244925,-27.6238454855805));
#57504=CARTESIAN_POINT('Ctrl Pts',(-23.0288311006609,27.4502591916687,-27.6179868301057));
#57505=CARTESIAN_POINT('Ctrl Pts',(-23.1441564410661,27.4622309269792,-27.6121281746308));
#57506=CARTESIAN_POINT('Ctrl Pts',(-23.2639864908444,27.4746702888155,-27.6060406749129));
#57507=CARTESIAN_POINT('Ctrl Pts',(-23.3844854318614,27.4816087777917,-27.599953175195));
#57508=CARTESIAN_POINT('Ctrl Pts',(-23.5051077675357,27.4829934270837,-27.5938656754771));
#57509=CARTESIAN_POINT('Ctrl Pts',(-23.6210611589498,27.4843244805774,-27.5880138053937));
#57510=CARTESIAN_POINT('Ctrl Pts',(-23.7371281182293,27.4805236410682,-27.5821619353103));
#57511=CARTESIAN_POINT('Ctrl Pts',(-23.8528207751636,27.4715968749066,-27.5763100652269));
#57512=CARTESIAN_POINT('Ctrl Pts',(-23.9684958168387,27.4626714679263,-27.5704590861439));
#57513=CARTESIAN_POINT('Ctrl Pts',(-24.0837962574401,27.448621717909,-27.5646081070609));
#57514=CARTESIAN_POINT('Ctrl Pts',(-24.198237482596,27.4295056174576,-27.558757127978));
#57515=CARTESIAN_POINT('Ctrl Pts',(-24.3126889971193,27.4103877982848,-27.5529056228357));
#57516=CARTESIAN_POINT('Ctrl Pts',(-24.4262807348698,27.3862027912702,-27.5470541176933));
#57517=CARTESIAN_POINT('Ctrl Pts',(-24.5385371382397,27.3570599258849,-27.541202612551));
#57518=CARTESIAN_POINT('Ctrl Pts',(-24.6508308195173,27.3279073827885,-27.5353491642513));
#57519=CARTESIAN_POINT('Ctrl Pts',(-24.7617878847632,27.2937938113849,-27.5294957159515));
#57520=CARTESIAN_POINT('Ctrl Pts',(-24.8709475158518,27.2548785261531,-27.5236422676517));
#57521=CARTESIAN_POINT('Ctrl Pts',(-24.9802312851447,27.2159189857918,-27.5177821627102));
#57522=CARTESIAN_POINT('Ctrl Pts',(-25.087713150762,27.1721469713227,-27.5119220577686));
#57523=CARTESIAN_POINT('Ctrl Pts',(-25.1929517848003,27.1237701493707,-27.5060619528271));
#57524=CARTESIAN_POINT('Ctrl Pts',(-25.298261290472,27.075360748657,-27.5001979014716));
#57525=CARTESIAN_POINT('Ctrl Pts',(-25.4013241898144,27.0223405542987,-27.4943338501162));
#57526=CARTESIAN_POINT('Ctrl Pts',(-25.5017248387421,26.9649625976918,-27.4884697987607));
#57527=CARTESIAN_POINT('Ctrl Pts',(-25.6022734581846,26.9075000774305,-27.4825971049641));
#57528=CARTESIAN_POINT('Ctrl Pts',(-25.7001516482383,26.8456671968592,-27.4767244111675));
#57529=CARTESIAN_POINT('Ctrl Pts',(-25.7949736762255,26.7797596122398,-27.470851717371));
#57530=CARTESIAN_POINT('Ctrl Pts',(-25.820934361308,26.7617152180713,-27.4692438720477));
#57531=CARTESIAN_POINT('Ctrl Pts',(-25.846666163512,26.7433656219047,-27.4676360267245));
#57532=CARTESIAN_POINT('Ctrl Pts',(-25.8721616290135,26.7247173911289,-27.4660281814012));
#57533=CARTESIAN_POINT('Ctrl Pts',(-25.9644504744281,26.6572142624953,-27.4602080802354));
#57534=CARTESIAN_POINT('Ctrl Pts',(-26.0539612220893,26.5855601120598,-27.4543879790697));
#57535=CARTESIAN_POINT('Ctrl Pts',(-26.1402920289457,26.5100134008654,-27.4485678779039));
#57536=CARTESIAN_POINT('Ctrl Pts',(-26.2265105992982,26.4345649060442,-27.4427553433048));
#57537=CARTESIAN_POINT('Ctrl Pts',(-26.3095571329673,26.3552341851834,-27.4369428087057));
#57538=CARTESIAN_POINT('Ctrl Pts',(-26.3890593711334,26.2723224662023,-27.4311302741066));
#57539=CARTESIAN_POINT('Ctrl Pts',(-26.4684804720688,26.18949536405,-27.425323671579));
#57540=CARTESIAN_POINT('Ctrl Pts',(-26.5443641797559,26.1030948327763,-27.4195170690514));
#57541=CARTESIAN_POINT('Ctrl Pts',(-26.6163725091683,26.0134612690394,-27.4137104665238));
#57542=CARTESIAN_POINT('Ctrl Pts',(-26.6883287911869,25.9238924921604,-27.4079080609903));
#57543=CARTESIAN_POINT('Ctrl Pts',(-26.7564150022,25.8310956573359,-27.4021056554567));
#57544=CARTESIAN_POINT('Ctrl Pts',(-26.8203316570448,25.7354462333935,-27.3963032499232));
#57545=CARTESIAN_POINT('Ctrl Pts',(-26.8842242657599,25.6398327937881,-27.3905030273167));
#57546=CARTESIAN_POINT('Ctrl Pts',(-26.9439502017762,25.5413692477434,-27.3847028047102));
#57547=CARTESIAN_POINT('Ctrl Pts',(-26.9992521721443,25.4404616418657,-27.3789025821037));
#57548=CARTESIAN_POINT('Ctrl Pts',(-27.0545473189922,25.3395664866308,-27.3731030751667));
#57549=CARTESIAN_POINT('Ctrl Pts',(-27.1054193830347,25.2362282407594,-27.3673035682298));
#57550=CARTESIAN_POINT('Ctrl Pts',(-27.1516564893883,25.1308785258831,-27.3615040612928));
#57551=CARTESIAN_POINT('Ctrl Pts',(-27.1978995808798,25.0255151740681,-27.3557038036417));
#57552=CARTESIAN_POINT('Ctrl Pts',(-27.2395063536526,24.9181402220512,-27.3499035459907));
#57553=CARTESIAN_POINT('Ctrl Pts',(-27.2763129679182,24.8092055195402,-27.3441032883396));
#57554=CARTESIAN_POINT('Ctrl Pts',(-27.313155386537,24.7001648486686,-27.3382973883745));
#57555=CARTESIAN_POINT('Ctrl Pts',(-27.345188187438,24.5895617975059,-27.3324914884095));
#57556=CARTESIAN_POINT('Ctrl Pts',(-27.3722973508228,24.4778636574209,-27.3266855884444));
#57557=CARTESIAN_POINT('Ctrl Pts',(-27.3994204194904,24.3661082232691,-27.3208767104206));
#57558=CARTESIAN_POINT('Ctrl Pts',(-27.421614740824,24.253256995109,-27.3150678323969));
#57559=CARTESIAN_POINT('Ctrl Pts',(-27.4388177417771,24.1397859123718,-27.3092589543731));
#57560=CARTESIAN_POINT('Ctrl Pts',(-27.4560471045766,24.0261409467597,-27.3034411748355));
#57561=CARTESIAN_POINT('Ctrl Pts',(-27.4682698270097,23.9118746484371,-27.2976233952979));
#57562=CARTESIAN_POINT('Ctrl Pts',(-27.4754753431419,23.7974667717586,-27.2918056157603));
#57563=CARTESIAN_POINT('Ctrl Pts',(-27.4806945629316,23.7145969477095,-27.2875915845184));
#57564=CARTESIAN_POINT('Ctrl Pts',(-27.4832825346391,23.6316528966433,-27.2833775532766));
#57565=CARTESIAN_POINT('Ctrl Pts',(-27.4832522691901,23.5488155707394,-27.2791635220347));
#57566=CARTESIAN_POINT('',(-27.4832508680474,23.5538700228986,-26.0291635220347));
#57567=CARTESIAN_POINT('Ctrl Pts',(-27.4891202243453,23.5488134268231,-27.2791635220347));
#57568=CARTESIAN_POINT('Ctrl Pts',(-27.4894904774531,23.4699199363944,-27.2751561046986));
#57569=CARTESIAN_POINT('Ctrl Pts',(-27.487326383654,23.3910471511404,-27.2711486873625));
#57570=CARTESIAN_POINT('Ctrl Pts',(-27.4037747347876,22.0101217003781,-27.2008456329014));
#57571=CARTESIAN_POINT('Ctrl Pts',(-25.8238780958542,19.4917580292825,-27.0682543586514));
#57572=CARTESIAN_POINT('Ctrl Pts',(-21.364764015651,19.4436248667672,-26.8693674472766));
#57573=CARTESIAN_POINT('Ctrl Pts',(-18.9139285828196,23.1691343437126,-26.6704805359016));
#57574=CARTESIAN_POINT('Ctrl Pts',(-20.7234817635613,27.2448591219192,-26.4715936245267));
#57575=CARTESIAN_POINT('Ctrl Pts',(-25.1305976095771,27.9255536946904,-26.2727067131518));
#57576=CARTESIAN_POINT('Ctrl Pts',(-27.3216959316878,25.4490306024728,-26.1252300123211));
#57577=CARTESIAN_POINT('Ctrl Pts',(-27.4863078274828,23.8479932003446,-26.0440489486155));
#57578=CARTESIAN_POINT('Ctrl Pts',(-27.4835763998974,23.5538703223161,-26.0291635220347));
#57579=CARTESIAN_POINT('',(-27.4832525262206,23.5500450338769,-24.7791635219934));
#57580=CARTESIAN_POINT('Ctrl Pts',(-27.4832508680474,23.5538700228986,-26.0291635220347));
#57581=CARTESIAN_POINT('Ctrl Pts',(-27.4833559273522,23.4396477491317,-26.0233822513878));
#57582=CARTESIAN_POINT('Ctrl Pts',(-27.4784809167359,23.3252787802462,-26.0176009807409));
#57583=CARTESIAN_POINT('Ctrl Pts',(-27.4686142799239,23.2112389478804,-26.011819710094));
#57584=CARTESIAN_POINT('Ctrl Pts',(-27.4587552319999,23.0972868288391,-26.0060428860905));
#57585=CARTESIAN_POINT('Ctrl Pts',(-27.443912227658,22.9836637651824,-26.000266062087));
#57586=CARTESIAN_POINT('Ctrl Pts',(-27.4241257767461,22.8708446414902,-25.9944892380835));
#57587=CARTESIAN_POINT('Ctrl Pts',(-27.4043473789285,22.7580714352318,-25.9887147652499));
#57588=CARTESIAN_POINT('Ctrl Pts',(-27.3796296050901,22.6461019372493,-25.9829402924164));
#57589=CARTESIAN_POINT('Ctrl Pts',(-27.3500646256575,22.5354042422586,-25.9771658195828));
#57590=CARTESIAN_POINT('Ctrl Pts',(-27.3205040698356,22.4247231102257,-25.9713922107451));
#57591=CARTESIAN_POINT('Ctrl Pts',(-27.2860978596516,22.315313813927,-25.9656186019074));
#57592=CARTESIAN_POINT('Ctrl Pts',(-27.2469887198259,22.207631753009,-25.9598449930697));
#57593=CARTESIAN_POINT('Ctrl Pts',(-27.2078753655144,22.0999380880382,-25.9540707620554));
#57594=CARTESIAN_POINT('Ctrl Pts',(-27.1640582205472,21.9939724279231,-25.9482965310411));
#57595=CARTESIAN_POINT('Ctrl Pts',(-27.1157287660695,21.8901717438694,-25.9425223000268));
#57596=CARTESIAN_POINT('Ctrl Pts',(-27.0673511770414,21.7862676777415,-25.9367423180679));
#57597=CARTESIAN_POINT('Ctrl Pts',(-27.0144524833506,21.6845332802459,-25.930962336109));
#57598=CARTESIAN_POINT('Ctrl Pts',(-26.9572709229612,21.5853823880031,-25.9251823541501));
#57599=CARTESIAN_POINT('Ctrl Pts',(-26.9000607778477,21.4861819308155,-25.9193994828124));
#57600=CARTESIAN_POINT('Ctrl Pts',(-26.8385637324964,21.3895679085275,-25.9136166114747));
#57601=CARTESIAN_POINT('Ctrl Pts',(-26.7730612243053,21.2959248867343,-25.907833740137));
#57602=CARTESIAN_POINT('Ctrl Pts',(-26.7074515266995,21.202128625913,-25.9020414056106));
#57603=CARTESIAN_POINT('Ctrl Pts',(-26.6378235327476,21.1113134143342,-25.8962490710843));
#57604=CARTESIAN_POINT('Ctrl Pts',(-26.5644990173714,21.023830729306,-25.8904567365579));
#57605=CARTESIAN_POINT('Ctrl Pts',(-26.4989941395618,20.9456775691545,-25.8852821211726));
#57606=CARTESIAN_POINT('Ctrl Pts',(-26.4305398127726,20.870183700961,-25.8801075057874));
#57607=CARTESIAN_POINT('Ctrl Pts',(-26.359388676242,20.7975732693399,-25.8749328904021));
#57608=CARTESIAN_POINT('Ctrl Pts',(-26.2786443943463,20.715172938927,-25.8690605934334));
#57609=CARTESIAN_POINT('Ctrl Pts',(-26.1941361993304,20.6361902832086,-25.8631882964647));
#57610=CARTESIAN_POINT('Ctrl Pts',(-26.106185179249,20.5609888596232,-25.857315999496));
#57611=CARTESIAN_POINT('Ctrl Pts',(-26.0183481367047,20.4858848911104,-25.8514513125577));
#57612=CARTESIAN_POINT('Ctrl Pts',(-25.9270774529613,20.4145526762032,-25.8455866256195));
#57613=CARTESIAN_POINT('Ctrl Pts',(-25.8327320011325,20.3473200516702,-25.8397219386813));
#57614=CARTESIAN_POINT('Ctrl Pts',(-25.7384835776947,20.2801565716826,-25.8338632832065));
#57615=CARTESIAN_POINT('Ctrl Pts',(-25.6411670105871,20.2170845343467,-25.8280046277317));
#57616=CARTESIAN_POINT('Ctrl Pts',(-25.5411747747554,20.1583920360246,-25.8221459722568));
#57617=CARTESIAN_POINT('Ctrl Pts',(-25.4372767541204,20.0974069570225,-25.8160584725389));
#57618=CARTESIAN_POINT('Ctrl Pts',(-25.3304901211217,20.0411508246606,-25.809970972821));
#57619=CARTESIAN_POINT('Ctrl Pts',(-25.2212893627608,19.9898979272736,-25.8038834731031));
#57620=CARTESIAN_POINT('Ctrl Pts',(-25.116315452198,19.9406288823774,-25.7980316030197));
#57621=CARTESIAN_POINT('Ctrl Pts',(-25.0091112380853,19.8959831446882,-25.7921797329363));
#57622=CARTESIAN_POINT('Ctrl Pts',(-24.9001231887229,19.8561574856385,-25.7863278628529));
#57623=CARTESIAN_POINT('Ctrl Pts',(-24.7911517337818,19.8163378904076,-25.78047688377));
#57624=CARTESIAN_POINT('Ctrl Pts',(-24.6803973717949,19.7813370564274,-25.774625904687));
#57625=CARTESIAN_POINT('Ctrl Pts',(-24.5683251706689,19.7513030582514,-25.768774925604));
#57626=CARTESIAN_POINT('Ctrl Pts',(-24.4562428931736,19.72126635973,-25.7629234204617));
#57627=CARTESIAN_POINT('Ctrl Pts',(-24.3428429403163,19.6961974917576,-25.7570719153194));
#57628=CARTESIAN_POINT('Ctrl Pts',(-24.2286034146487,19.6761940551615,-25.7512204101771));
#57629=CARTESIAN_POINT('Ctrl Pts',(-24.1143259525213,19.6561839758595,-25.7453669618773));
#57630=CARTESIAN_POINT('Ctrl Pts',(-23.999208770172,19.6412427439838,-25.7395135135775));
#57631=CARTESIAN_POINT('Ctrl Pts',(-23.8837372728448,19.631416361679,-25.7336600652777));
#57632=CARTESIAN_POINT('Ctrl Pts',(-23.7681344593515,19.6215788046438,-25.7277999603362));
#57633=CARTESIAN_POINT('Ctrl Pts',(-23.6521769387767,19.6168677421984,-25.7219398553946));
#57634=CARTESIAN_POINT('Ctrl Pts',(-23.5363524188044,19.6172770948447,-25.7160797504531));
#57635=CARTESIAN_POINT('Ctrl Pts',(-23.420449898267,19.6176867231644,-25.7102156990976));
#57636=CARTESIAN_POINT('Ctrl Pts',(-23.304680968581,19.6232236130841,-25.7043516477422));
#57637=CARTESIAN_POINT('Ctrl Pts',(-23.1895287651332,19.6338297552006,-25.6984875963867));
#57638=CARTESIAN_POINT('Ctrl Pts',(-23.0742068503238,19.6444515286533,-25.6926149025901));
#57639=CARTESIAN_POINT('Ctrl Pts',(-22.9595038838278,19.6601574092395,-25.6867422087936));
#57640=CARTESIAN_POINT('Ctrl Pts',(-22.8458934457647,19.6808381989988,-25.680869514997));
#57641=CARTESIAN_POINT('Ctrl Pts',(-22.8147888082951,19.6865002532873,-25.6792616696737));
#57642=CARTESIAN_POINT('Ctrl Pts',(-22.7837659769105,19.6925349245322,-25.6776538243505));
#57643=CARTESIAN_POINT('Ctrl Pts',(-22.7528344570043,19.6989393252466,-25.6760459790272));
#57644=CARTESIAN_POINT('Ctrl Pts',(-22.6398639691377,19.7223299725667,-25.6701736820585));
#57645=CARTESIAN_POINT('Ctrl Pts',(-22.527734273729,19.7507346612045,-25.6643013850898));
#57646=CARTESIAN_POINT('Ctrl Pts',(-22.4169247994566,19.7840797726003,-25.6584290881211));
#57647=CARTESIAN_POINT('Ctrl Pts',(-22.3062589254623,19.8173816713799,-25.6525644011829));
#57648=CARTESIAN_POINT('Ctrl Pts',(-22.1969102624293,19.8556111428307,-25.6466997142447));
#57649=CARTESIAN_POINT('Ctrl Pts',(-22.0893486110632,19.8986434706521,-25.6408350273065));
#57650=CARTESIAN_POINT('Ctrl Pts',(-21.9818975801219,19.9416315424182,-25.6349763718317));
#57651=CARTESIAN_POINT('Ctrl Pts',(-21.8762302868094,19.9894124931336,-25.6291177163569));
#57652=CARTESIAN_POINT('Ctrl Pts',(-21.7728012607751,20.0418118553384,-25.6232590608821));
#57653=CARTESIAN_POINT('Ctrl Pts',(-21.6653322058849,20.0962579827837,-25.6171715611642));
#57654=CARTESIAN_POINT('Ctrl Pts',(-21.5602802757069,20.1556905444095,-25.6110840614463));
#57655=CARTESIAN_POINT('Ctrl Pts',(-21.4581327139585,20.2198586108137,-25.6049965617284));
#57656=CARTESIAN_POINT('Ctrl Pts',(-21.3599389910202,20.2815429156188,-25.599144691645));
#57657=CARTESIAN_POINT('Ctrl Pts',(-21.264429360388,20.3476027057622,-25.5932928215616));
#57658=CARTESIAN_POINT('Ctrl Pts',(-21.1720107042132,20.4177687232732,-25.5874409514782));
#57659=CARTESIAN_POINT('Ctrl Pts',(-21.0796061196191,20.48792405737,-25.5815899723952));
#57660=CARTESIAN_POINT('Ctrl Pts',(-20.9902919028745,20.5621841258165,-25.5757389933123));
#57661=CARTESIAN_POINT('Ctrl Pts',(-20.904444020505,20.6402376997528,-25.5698880142293));
#57662=CARTESIAN_POINT('Ctrl Pts',(-20.8185884195846,20.7182982914567,-25.564036509087));
#57663=CARTESIAN_POINT('Ctrl Pts',(-20.7362000784633,20.8001527885639,-25.5581850039447));
#57664=CARTESIAN_POINT('Ctrl Pts',(-20.657619545052,20.8854517127606,-25.5523334988024));
#57665=CARTESIAN_POINT('Ctrl Pts',(-20.5790129167564,20.9707789628729,-25.5464800505027));
#57666=CARTESIAN_POINT('Ctrl Pts',(-20.5042168904685,21.0595526106144,-25.5406266022029));
#57667=CARTESIAN_POINT('Ctrl Pts',(-20.4335325506769,21.1513891425185,-25.5347731539032));
#57668=CARTESIAN_POINT('Ctrl Pts',(-20.362767827442,21.2433301125014,-25.5289130489616));
#57669=CARTESIAN_POINT('Ctrl Pts',(-20.2961243759044,21.3383405911567,-25.5230529440201));
#57670=CARTESIAN_POINT('Ctrl Pts',(-20.2338607079589,21.4360069756005,-25.5171928390786));
#57671=CARTESIAN_POINT('Ctrl Pts',(-20.1715551093299,21.5337391322418,-25.5113287877231));
#57672=CARTESIAN_POINT('Ctrl Pts',(-20.1136353734299,21.6341303989133,-25.5054647363677));
#57673=CARTESIAN_POINT('Ctrl Pts',(-20.0603138511328,21.7367429491661,-25.4996006850122));
#57674=CARTESIAN_POINT('Ctrl Pts',(-20.0069137435559,21.8395067298343,-25.4937279912157));
#57675=CARTESIAN_POINT('Ctrl Pts',(-19.9581255484152,21.9444979543378,-25.4878552974191));
#57676=CARTESIAN_POINT('Ctrl Pts',(-19.9141133857657,22.0512591656495,-25.4819826036226));
#57677=CARTESIAN_POINT('Ctrl Pts',(-19.9020635918652,22.080488599411,-25.4803747582992));
#57678=CARTESIAN_POINT('Ctrl Pts',(-19.8903715065191,22.1098506236019,-25.4787669129758));
#57679=CARTESIAN_POINT('Ctrl Pts',(-19.8790398385043,22.1393356803663,-25.4771590676524));
#57680=CARTESIAN_POINT('Ctrl Pts',(-19.8376534446978,22.247023283732,-25.4712867706837));
#57681=CARTESIAN_POINT('Ctrl Pts',(-19.800939931946,22.3567138161882,-25.465414473715));
#57682=CARTESIAN_POINT('Ctrl Pts',(-19.7690965152443,22.4679641323916,-25.4595421767462));
#57683=CARTESIAN_POINT('Ctrl Pts',(-19.7372943650818,22.5790702770206,-25.453677489808));
#57684=CARTESIAN_POINT('Ctrl Pts',(-19.7103498728486,22.6917317918906,-25.4478128028698));
#57685=CARTESIAN_POINT('Ctrl Pts',(-19.6884120598263,22.8054860113383,-25.4419481159316));
#57686=CARTESIAN_POINT('Ctrl Pts',(-19.6664968084713,22.9191232416926,-25.4360894604568));
#57687=CARTESIAN_POINT('Ctrl Pts',(-19.6495780723987,23.0338505379084,-25.430230804982));
#57688=CARTESIAN_POINT('Ctrl Pts',(-19.6377547617519,23.1491911895073,-25.4243721495072));
#57689=CARTESIAN_POINT('Ctrl Pts',(-19.6254696221774,23.2690371485482,-25.4182846497892));
#57690=CARTESIAN_POINT('Ctrl Pts',(-19.6186862117189,23.3895449190781,-25.4121971500713));
#57691=CARTESIAN_POINT('Ctrl Pts',(-19.6174567951449,23.5101689368029,-25.4061096503534));
#57692=CARTESIAN_POINT('Ctrl Pts',(-19.6162749657563,23.6261239451599,-25.40025778027));
#57693=CARTESIAN_POINT('Ctrl Pts',(-19.6202251712741,23.7421859169408,-25.3944059101866));
#57694=CARTESIAN_POINT('Ctrl Pts',(-19.6293008175015,23.8578669900171,-25.3885540401033));
#57695=CARTESIAN_POINT('Ctrl Pts',(-19.6383750818792,23.9735304495979,-25.3827030610203));
#57696=CARTESIAN_POINT('Ctrl Pts',(-19.6525732029681,24.088812713784,-25.3768520819373));
#57697=CARTESIAN_POINT('Ctrl Pts',(-19.6718365645521,24.2032292432368,-25.3710011028544));
#57698=CARTESIAN_POINT('Ctrl Pts',(-19.6911016580977,24.3176560598371,-25.3651495977121));
#57699=CARTESIAN_POINT('Ctrl Pts',(-19.7154328288233,24.4312165792996,-25.3592980925698));
#57700=CARTESIAN_POINT('Ctrl Pts',(-19.7447201353424,24.5434353851088,-25.3534465874275));
#57701=CARTESIAN_POINT('Ctrl Pts',(-19.7740171675384,24.6556914563404,-25.3475931391277));
#57702=CARTESIAN_POINT('Ctrl Pts',(-19.8082735038125,24.7666045281894,-25.3417396908279));
#57703=CARTESIAN_POINT('Ctrl Pts',(-19.8473292367804,24.8757139879369,-25.3358862425282));
#57704=CARTESIAN_POINT('Ctrl Pts',(-19.8864293845975,24.9849475288328,-25.3300261375866));
#57705=CARTESIAN_POINT('Ctrl Pts',(-19.9303396836271,25.0923729742652,-25.3241660326451));
#57706=CARTESIAN_POINT('Ctrl Pts',(-19.9788518994618,25.1975492639468,-25.3183059277036));
#57707=CARTESIAN_POINT('Ctrl Pts',(-20.0273967852376,25.3027963832769,-25.3124418763481));
#57708=CARTESIAN_POINT('Ctrl Pts',(-20.080549569632,25.4057909644049,-25.3065778249927));
#57709=CARTESIAN_POINT('Ctrl Pts',(-20.1380566865571,25.5061176892215,-25.3007137736372));
#57710=CARTESIAN_POINT('Ctrl Pts',(-20.195648557493,25.6065922756033,-25.2948410798407));
#57711=CARTESIAN_POINT('Ctrl Pts',(-20.2576073484846,25.7043908104936,-25.2889683860441));
#57712=CARTESIAN_POINT('Ctrl Pts',(-20.3236369071072,25.7991279420206,-25.2830956922475));
#57713=CARTESIAN_POINT('Ctrl Pts',(-20.3417146957188,25.8250653838747,-25.2814878469242));
#57714=CARTESIAN_POINT('Ctrl Pts',(-20.3600973915214,25.8507735502683,-25.2798800016008));
#57715=CARTESIAN_POINT('Ctrl Pts',(-20.3787784175389,25.8762449958357,-25.2782721562774));
#57716=CARTESIAN_POINT('Ctrl Pts',(-20.4470067047137,25.9692737781571,-25.2723998593087));
#57717=CARTESIAN_POINT('Ctrl Pts',(-20.5194459800455,26.059453855328,-25.26652756234));
#57718=CARTESIAN_POINT('Ctrl Pts',(-20.5958300209873,26.1463797682195,-25.2606552653713));
#57719=CARTESIAN_POINT('Ctrl Pts',(-20.6721150742784,26.2331930320313,-25.2547905784331));
#57720=CARTESIAN_POINT('Ctrl Pts',(-20.7523344566912,26.3167602102763,-25.2489258914949));
#57721=CARTESIAN_POINT('Ctrl Pts',(-20.8361794721605,26.3967058384452,-25.2430612045567));
#57722=CARTESIAN_POINT('Ctrl Pts',(-20.91993825828,26.4765692475399,-25.2372025490819));
#57723=CARTESIAN_POINT('Ctrl Pts',(-21.0073149634256,26.5528182313041,-25.2313438936071));
#57724=CARTESIAN_POINT('Ctrl Pts',(-21.097961988199,26.6251118927519,-25.2254852381323));
#57725=CARTESIAN_POINT('Ctrl Pts',(-21.1921497656012,26.7002294082915,-25.2193977384144));
#57726=CARTESIAN_POINT('Ctrl Pts',(-21.2898682539351,26.7710759639824,-25.2133102386965));
#57727=CARTESIAN_POINT('Ctrl Pts',(-21.3906867121297,26.8373126879689,-25.2072227389786));
#57728=CARTESIAN_POINT('Ctrl Pts',(-21.4876027772966,26.9009855785613,-25.2013708688951));
#57729=CARTESIAN_POINT('Ctrl Pts',(-21.587382915016,26.9603986203455,-25.1955189988117));
#57730=CARTESIAN_POINT('Ctrl Pts',(-21.6896131142508,27.0152936509676,-25.1896671287283));
#57731=CARTESIAN_POINT('Ctrl Pts',(-21.7918277480081,27.0701803233221,-25.1838161496454));
#57732=CARTESIAN_POINT('Ctrl Pts',(-21.8964913374521,27.1205501567852,-25.1779651705624));
#57733=CARTESIAN_POINT('Ctrl Pts',(-22.0031645469578,27.1661905521094,-25.1721141914794));
#57734=CARTESIAN_POINT('Ctrl Pts',(-22.109847347412,27.2118350509445,-25.1662626863371));
#57735=CARTESIAN_POINT('Ctrl Pts',(-22.2185397470311,27.2527491037203,-25.1604111811948));
#57736=CARTESIAN_POINT('Ctrl Pts',(-22.328782341944,27.2887682231888,-25.1545596760525));
#57737=CARTESIAN_POINT('Ctrl Pts',(-22.4390615460226,27.3247993038227,-25.1487062277527));
#57738=CARTESIAN_POINT('Ctrl Pts',(-22.5508915762814,27.3559320906272,-25.1428527794529));
#57739=CARTESIAN_POINT('Ctrl Pts',(-22.6637984747916,27.3820521356663,-25.1369993311532));
#57740=CARTESIAN_POINT('Ctrl Pts',(-22.7768337729629,27.4082018848686,-25.1311392262116));
#57741=CARTESIAN_POINT('Ctrl Pts',(-22.8909479807313,27.4293274209012,-25.1252791212701));
#57742=CARTESIAN_POINT('Ctrl Pts',(-23.0056574671519,27.4453655230818,-25.1194190163285));
#57743=CARTESIAN_POINT('Ctrl Pts',(-23.1204442032322,27.4614144259204,-25.1135549649731));
#57744=CARTESIAN_POINT('Ctrl Pts',(-23.2358266056756,27.4723690339487,-25.1076909136176));
#57745=CARTESIAN_POINT('Ctrl Pts',(-23.3513181971683,27.478218179526,-25.1018268622621));
#57746=CARTESIAN_POINT('Ctrl Pts',(-23.4669800002124,27.4840759455763,-25.0959541684656));
#57747=CARTESIAN_POINT('Ctrl Pts',(-23.5827509016543,27.4848132292374,-25.090081474669));
#57748=CARTESIAN_POINT('Ctrl Pts',(-23.6981466155584,27.4804708894904,-25.0842087808724));
#57749=CARTESIAN_POINT('Ctrl Pts',(-23.7297400316901,27.4792820295061,-25.0826009355491));
#57750=CARTESIAN_POINT('Ctrl Pts',(-23.7613053697927,27.4777127128804,-25.0809930902258));
#57751=CARTESIAN_POINT('Ctrl Pts',(-23.7928328108208,27.4757644483974,-25.0793852449025));
#57752=CARTESIAN_POINT('Ctrl Pts',(-23.9079797678678,27.468648846261,-25.0735129479338));
#57753=CARTESIAN_POINT('Ctrl Pts',(-24.0230062790909,27.456450623236,-25.0676406509651));
#57754=CARTESIAN_POINT('Ctrl Pts',(-24.1374273203492,27.4391745889702,-25.0617683539964));
#57755=CARTESIAN_POINT('Ctrl Pts',(-24.2517000810251,27.4219209430728,-25.0559036670582));
#57756=CARTESIAN_POINT('Ctrl Pts',(-24.3653685271285,27.3996026332139,-25.05003898012));
#57757=CARTESIAN_POINT('Ctrl Pts',(-24.4779499107581,27.3722764160882,-25.0441742931818));
#57758=CARTESIAN_POINT('Ctrl Pts',(-24.5904155114828,27.344978302266,-25.038315637707));
#57759=CARTESIAN_POINT('Ctrl Pts',(-24.7017958741413,27.3126826223473,-25.0324569822321));
#57760=CARTESIAN_POINT('Ctrl Pts',(-24.811616304169,27.2754975482653,-25.0265983267573));
#57761=CARTESIAN_POINT('Ctrl Pts',(-24.9257264169218,27.2368599924377,-25.0205108270394));
#57762=CARTESIAN_POINT('Ctrl Pts',(-25.0381517984308,27.1929433554071,-25.0144233273215));
#57763=CARTESIAN_POINT('Ctrl Pts',(-25.1483745163087,27.1439268522597,-25.0083358276036));
#57764=CARTESIAN_POINT('Ctrl Pts',(-25.2543308292697,27.0968076372038,-25.0024839575202));
#57765=CARTESIAN_POINT('Ctrl Pts',(-25.3582514125868,27.0449762009867,-24.9966320874368));
#57766=CARTESIAN_POINT('Ctrl Pts',(-25.4596952794236,26.9886413103438,-24.9907802173534));
#57767=CARTESIAN_POINT('Ctrl Pts',(-25.5611237005096,26.9323149972,-24.9849292382704));
#57768=CARTESIAN_POINT('Ctrl Pts',(-25.6600757936188,26.8714867936446,-24.9790782591874));
#57769=CARTESIAN_POINT('Ctrl Pts',(-25.7561352159074,26.8064114012041,-24.9732272801044));
#57770=CARTESIAN_POINT('Ctrl Pts',(-25.8522032748621,26.7413301578599,-24.9673757749621));
#57771=CARTESIAN_POINT('Ctrl Pts',(-25.9453778037202,26.6720011983877,-24.9615242698198));
#57772=CARTESIAN_POINT('Ctrl Pts',(-26.0352720893322,26.5987221146418,-24.9556727646776));
#57773=CARTESIAN_POINT('Ctrl Pts',(-26.1251962268789,26.5254186965079,-24.9498193163778));
#57774=CARTESIAN_POINT('Ctrl Pts',(-26.2118376349368,26.4481628068202,-24.9439658680781));
#57775=CARTESIAN_POINT('Ctrl Pts',(-26.2948438321841,26.3672913303754,-24.9381124197784));
#57776=CARTESIAN_POINT('Ctrl Pts',(-26.3779444255028,26.2863278855003,-24.9322523148368));
#57777=CARTESIAN_POINT('Ctrl Pts',(-26.4574012603598,26.2017409356693,-24.9263922098953));
#57778=CARTESIAN_POINT('Ctrl Pts',(-26.5328997251062,26.1139031942518,-24.9205321049538));
#57779=CARTESIAN_POINT('Ctrl Pts',(-26.6084490333431,26.026006299613,-24.9146680535983));
#57780=CARTESIAN_POINT('Ctrl Pts',(-26.6800344088042,25.9348545785614,-24.9088040022429));
#57781=CARTESIAN_POINT('Ctrl Pts',(-26.7473834943546,25.8408512760399,-24.9029399508875));
#57782=CARTESIAN_POINT('Ctrl Pts',(-26.8148318390131,25.7467094314152,-24.8970672570909));
#57783=CARTESIAN_POINT('Ctrl Pts',(-26.8780312082338,25.6497079626739,-24.8911945632943));
#57784=CARTESIAN_POINT('Ctrl Pts',(-26.9367542002845,25.5502763937106,-24.8853218694978));
#57785=CARTESIAN_POINT('Ctrl Pts',(-26.9528315731928,25.5230536934146,-24.8837140241744));
#57786=CARTESIAN_POINT('Ctrl Pts',(-26.9685736841801,25.4956489626921,-24.882106178851));
#57787=CARTESIAN_POINT('Ctrl Pts',(-26.9839764950017,25.4680712780328,-24.8804983335276));
#57788=CARTESIAN_POINT('Ctrl Pts',(-27.0428859532857,25.3625979015933,-24.8743489820812));
#57789=CARTESIAN_POINT('Ctrl Pts',(-27.0970105455507,25.2542673935842,-24.8681996306348));
#57790=CARTESIAN_POINT('Ctrl Pts',(-27.1460768847945,25.1435309824525,-24.8620502791883));
#57791=CARTESIAN_POINT('Ctrl Pts',(-27.1950567706787,25.032989685424,-24.8559117627074));
#57792=CARTESIAN_POINT('Ctrl Pts',(-27.238996010439,24.9200512530229,-24.8497732462264));
#57793=CARTESIAN_POINT('Ctrl Pts',(-27.2776665386152,24.8051922995753,-24.8436347297455));
#57794=CARTESIAN_POINT('Ctrl Pts',(-27.3162505695764,24.6905902595975,-24.8375099437359));
#57795=CARTESIAN_POINT('Ctrl Pts',(-27.3495892676818,24.5740765989749,-24.8313851577262));
#57796=CARTESIAN_POINT('Ctrl Pts',(-27.3775025586027,24.4561477969037,-24.8252603717166));
#57797=CARTESIAN_POINT('Ctrl Pts',(-27.4053783968587,24.3383772258314,-24.8191438036401));
#57798=CARTESIAN_POINT('Ctrl Pts',(-27.4278432409376,24.2191956400605,-24.8130272355637));
#57799=CARTESIAN_POINT('Ctrl Pts',(-27.4447663970275,24.0991156774114,-24.8069106674872));
#57800=CARTESIAN_POINT('Ctrl Pts',(-27.4616615688625,23.9792342798678,-24.8008042138124));
#57801=CARTESIAN_POINT('Ctrl Pts',(-27.4730332684047,23.8584578192019,-24.7946977601377));
#57802=CARTESIAN_POINT('Ctrl Pts',(-27.4788017190277,23.7373094286559,-24.788591306463));
#57803=CARTESIAN_POINT('Ctrl Pts',(-27.4817703656354,23.6749622262403,-24.7854487116536));
#57804=CARTESIAN_POINT('Ctrl Pts',(-27.4832558220972,23.6125166982619,-24.7823061168441));
#57805=CARTESIAN_POINT('Ctrl Pts',(-27.4832525262206,23.5500450346982,-24.7791635220347));
#57806=CARTESIAN_POINT('',(-27.4832509332757,23.5467066668166,-23.5291635220347));
#57807=CARTESIAN_POINT('Ctrl Pts',(-27.4832525262206,23.5500450338768,-24.7791635219934));
#57808=CARTESIAN_POINT('Ctrl Pts',(-27.483246071975,23.4277085761306,-24.7730094691767));
#57809=CARTESIAN_POINT('Ctrl Pts',(-27.4775273894719,23.3054919752915,-24.76685541636));
#57810=CARTESIAN_POINT('Ctrl Pts',(-27.466155630688,23.1839303793606,-24.7607013635433));
#57811=CARTESIAN_POINT('Ctrl Pts',(-27.4547662630801,23.0621805489794,-24.7545377813622));
#57812=CARTESIAN_POINT('Ctrl Pts',(-27.4377063854403,22.9410880911425,-24.7483741991811));
#57813=CARTESIAN_POINT('Ctrl Pts',(-27.4150864501085,22.8211792959528,-24.742210617));
#57814=CARTESIAN_POINT('Ctrl Pts',(-27.3924085127843,22.7009630308734,-24.7360312301739));
#57815=CARTESIAN_POINT('Ctrl Pts',(-27.3641420805642,22.5819368368814,-24.7298518433478));
#57816=CARTESIAN_POINT('Ctrl Pts',(-27.3304482090873,22.4646146359764,-24.7236724565217));
#57817=CARTESIAN_POINT('Ctrl Pts',(-27.2967063493928,22.3471253398976,-24.7174842687551));
#57818=CARTESIAN_POINT('Ctrl Pts',(-27.2575217357048,22.2313452068291,-24.7112960809885));
#57819=CARTESIAN_POINT('Ctrl Pts',(-27.2131038988971,22.1177690721807,-24.7051078932219));
#57820=CARTESIAN_POINT('Ctrl Pts',(-27.1685852853359,22.0039352519955,-24.6989056654767));
#57821=CARTESIAN_POINT('Ctrl Pts',(-27.1188098567107,21.8923157411691,-24.6927034377316));
#57822=CARTESIAN_POINT('Ctrl Pts',(-27.0640340105662,21.7833827802026,-24.6865012099865));
#57823=CARTESIAN_POINT('Ctrl Pts',(-27.049639061038,21.7547554821242,-24.6848712807086));
#57824=CARTESIAN_POINT('Ctrl Pts',(-27.034899004807,21.7263135716238,-24.6832413514307));
#57825=CARTESIAN_POINT('Ctrl Pts',(-27.0198189886844,21.6980652839981,-24.6816114221528));
#57826=CARTESIAN_POINT('Ctrl Pts',(-26.9654888197847,21.5962925653642,-24.6757391251841));
#57827=CARTESIAN_POINT('Ctrl Pts',(-26.9065858911063,21.4967418751502,-24.6698668282154));
#57828=CARTESIAN_POINT('Ctrl Pts',(-26.8433161667284,21.3998523606526,-24.6639945312467));
#57829=CARTESIAN_POINT('Ctrl Pts',(-26.7801284348885,21.3030884072711,-24.6581298443086));
#57830=CARTESIAN_POINT('Ctrl Pts',(-26.7125853850435,21.2089791143613,-24.6522651573704));
#57831=CARTESIAN_POINT('Ctrl Pts',(-26.6409392828495,21.1179399682614,-24.6464004704322));
#57832=CARTESIAN_POINT('Ctrl Pts',(-26.5693668641865,21.0269944502241,-24.6405418149575));
#57833=CARTESIAN_POINT('Ctrl Pts',(-26.4937000405536,20.9391131215564,-24.6346831594827));
#57834=CARTESIAN_POINT('Ctrl Pts',(-26.4142344943633,20.8546827742021,-24.6288245040079));
#57835=CARTESIAN_POINT('Ctrl Pts',(-26.3316649539457,20.7669545031141,-24.62273700429));
#57836=CARTESIAN_POINT('Ctrl Pts',(-26.2449941268371,20.6829526868011,-24.6166495045721));
#57837=CARTESIAN_POINT('Ctrl Pts',(-26.1546002825104,20.6030739159977,-24.6105620048541));
#57838=CARTESIAN_POINT('Ctrl Pts',(-26.0677053243423,20.5262870230496,-24.6047101347708));
#57839=CARTESIAN_POINT('Ctrl Pts',(-25.9773705431083,20.4533102273088,-24.5988582646874));
#57840=CARTESIAN_POINT('Ctrl Pts',(-25.8839691058204,20.3844578523682,-24.593006394604));
#57841=CARTESIAN_POINT('Ctrl Pts',(-25.7905818897506,20.3156159608278,-24.5871554155211));
#57842=CARTESIAN_POINT('Ctrl Pts',(-25.6941292786793,20.2508974866819,-24.5813044364382));
#57843=CARTESIAN_POINT('Ctrl Pts',(-25.5950159761787,20.1905752471771,-24.5754534573552));
#57844=CARTESIAN_POINT('Ctrl Pts',(-25.4958937624383,20.1302475841225,-24.5696019522129));
#57845=CARTESIAN_POINT('Ctrl Pts',(-25.394110734862,20.0743171563871,-24.5637504470707));
#57846=CARTESIAN_POINT('Ctrl Pts',(-25.2900982923399,20.0230120055657,-24.5578989419284));
#57847=CARTESIAN_POINT('Ctrl Pts',(-25.1860513095499,19.9716898174205,-24.5520454936287));
#57848=CARTESIAN_POINT('Ctrl Pts',(-25.0797738102331,19.9249961431086,-24.5461920453289));
#57849=CARTESIAN_POINT('Ctrl Pts',(-24.9717187038767,19.8831115579463,-24.5403385970292));
#57850=CARTESIAN_POINT('Ctrl Pts',(-24.8635407154007,19.8411793409156,-24.5344784920877));
#57851=CARTESIAN_POINT('Ctrl Pts',(-24.7535814706499,19.8040672784442,-24.5286183871461));
#57852=CARTESIAN_POINT('Ctrl Pts',(-24.6423107267535,19.7719066107119,-24.5227582822046));
#57853=CARTESIAN_POINT('Ctrl Pts',(-24.5309650489753,19.7397242847827,-24.5168942308492));
#57854=CARTESIAN_POINT('Ctrl Pts',(-24.4183065142351,19.7125000900164,-24.5110301794938));
#57855=CARTESIAN_POINT('Ctrl Pts',(-24.3048150870377,19.6903141448707,-24.5051661281384));
#57856=CARTESIAN_POINT('Ctrl Pts',(-24.1911563961316,19.6680955020706,-24.4992934343418));
#57857=CARTESIAN_POINT('Ctrl Pts',(-24.0766627701595,19.6509299895671,-24.4934207405453));
#57858=CARTESIAN_POINT('Ctrl Pts',(-23.9618193905294,19.6388459150525,-24.4875480467488));
#57859=CARTESIAN_POINT('Ctrl Pts',(-23.9303771942756,19.6355374975916,-24.4859402014251));
#57860=CARTESIAN_POINT('Ctrl Pts',(-23.8989087792088,19.6326096694182,-24.4843323561015));
#57861=CARTESIAN_POINT('Ctrl Pts',(-23.8674240791189,19.6300623310146,-24.4827245107778));
#57862=CARTESIAN_POINT('Ctrl Pts',(-23.7524332238541,19.6207587448015,-24.4768522138091));
#57863=CARTESIAN_POINT('Ctrl Pts',(-23.6368400278673,19.6165033986725,-24.4709799168404));
#57864=CARTESIAN_POINT('Ctrl Pts',(-23.5211252854633,19.6173603893228,-24.4651076198717));
#57865=CARTESIAN_POINT('Ctrl Pts',(-23.4055605001756,19.6182162693812,-24.4592429329335));
#57866=CARTESIAN_POINT('Ctrl Pts',(-23.2898748912665,19.624171308076,-24.4533782459953));
#57867=CARTESIAN_POINT('Ctrl Pts',(-23.1745543746449,19.6352378580576,-24.4475135590571));
#57868=CARTESIAN_POINT('Ctrl Pts',(-23.0593524579555,19.6462930267854,-24.4416549035823));
#57869=CARTESIAN_POINT('Ctrl Pts',(-22.9445152957341,19.6624492113657,-24.4357962481075));
#57870=CARTESIAN_POINT('Ctrl Pts',(-22.8305281314116,19.683666726667,-24.4299375926326));
#57871=CARTESIAN_POINT('Ctrl Pts',(-22.7120885280519,19.7057130168041,-24.4238500929147));
#57872=CARTESIAN_POINT('Ctrl Pts',(-22.5945671342954,19.7332240950283,-24.4177625931968));
#57873=CARTESIAN_POINT('Ctrl Pts',(-22.4785020792672,19.7660960909901,-24.4116750934789));
#57874=CARTESIAN_POINT('Ctrl Pts',(-22.3669295692514,19.7976957063764,-24.4058232233955));
#57875=CARTESIAN_POINT('Ctrl Pts',(-22.2567031877513,19.8342488216843,-24.3999713533121));
#57876=CARTESIAN_POINT('Ctrl Pts',(-22.148289093069,19.8756113904726,-24.3941194832287));
#57877=CARTESIAN_POINT('Ctrl Pts',(-22.0398915054184,19.9169676614338,-24.3882685041458));
#57878=CARTESIAN_POINT('Ctrl Pts',(-21.933306042056,19.9631317825476,-24.3824175250628));
#57879=CARTESIAN_POINT('Ctrl Pts',(-21.828980988146,20.0139107391958,-24.3765665459798));
#57880=CARTESIAN_POINT('Ctrl Pts',(-21.7246465544096,20.0646942613608,-24.3707150408375));
#57881=CARTESIAN_POINT('Ctrl Pts',(-21.6225733058471,20.120093262952,-24.3648635356952));
#57882=CARTESIAN_POINT('Ctrl Pts',(-21.5231862870665,20.1798680669942,-24.359012030553));
#57883=CARTESIAN_POINT('Ctrl Pts',(-21.4237662640206,20.2396627209476,-24.3531585822532));
#57884=CARTESIAN_POINT('Ctrl Pts',(-21.3270345985799,20.3038358538226,-24.3473051339534));
#57885=CARTESIAN_POINT('Ctrl Pts',(-21.2333880285658,20.3721040338824,-24.3414516856536));
#57886=CARTESIAN_POINT('Ctrl Pts',(-21.1396349620668,20.440449849687,-24.3355915807121));
#57887=CARTESIAN_POINT('Ctrl Pts',(-21.0489743279428,20.5128997641621,-24.3297314757706));
#57888=CARTESIAN_POINT('Ctrl Pts',(-20.9617704644022,20.5891295036341,-24.323871370829));
#57889=CARTESIAN_POINT('Ctrl Pts',(-20.8745078745173,20.6654105790646,-24.3180073194736));
#57890=CARTESIAN_POINT('Ctrl Pts',(-20.7907069887246,20.7454762631683,-24.3121432681181));
#57891=CARTESIAN_POINT('Ctrl Pts',(-20.7106946531889,20.8289660611772,-24.3062792167627));
#57892=CARTESIAN_POINT('Ctrl Pts',(-20.6305643954427,20.9125789064823,-24.3004065229661));
#57893=CARTESIAN_POINT('Ctrl Pts',(-20.554234103199,20.9996256278098,-24.2945338291696));
#57894=CARTESIAN_POINT('Ctrl Pts',(-20.4819898533138,21.0897133354086,-24.288661135373));
#57895=CARTESIAN_POINT('Ctrl Pts',(-20.4622105861936,21.1143778427662,-24.2870532900497));
#57896=CARTESIAN_POINT('Ctrl Pts',(-20.4427373428466,21.1392701330953,-24.2854454447263));
#57897=CARTESIAN_POINT('Ctrl Pts',(-20.4235754091814,21.1643817951381,-24.2838375994029));
#57898=CARTESIAN_POINT('Ctrl Pts',(-20.3535907139232,21.2560965482624,-24.2779653024342));
#57899=CARTESIAN_POINT('Ctrl Pts',(-20.2875275970532,21.3510468485179,-24.2720930054655));
#57900=CARTESIAN_POINT('Ctrl Pts',(-20.2256998739005,21.4488628425701,-24.2662207084968));
#57901=CARTESIAN_POINT('Ctrl Pts',(-20.1639522745668,21.5465520748624,-24.2603560215586));
#57902=CARTESIAN_POINT('Ctrl Pts',(-20.1064293726592,21.6470992695062,-24.2544913346203));
#57903=CARTESIAN_POINT('Ctrl Pts',(-20.0534042188184,21.7501022944257,-24.2486266476821));
#57904=CARTESIAN_POINT('Ctrl Pts',(-20.0004335980289,21.8529993871822,-24.2427679922073));
#57905=CARTESIAN_POINT('Ctrl Pts',(-19.9519517127152,21.9583469212006,-24.2369093367325));
#57906=CARTESIAN_POINT('Ctrl Pts',(-19.9081874697557,22.0657152015449,-24.2310506812576));
#57907=CARTESIAN_POINT('Ctrl Pts',(-19.8627137569192,22.1772773814879,-24.2249631815397));
#57908=CARTESIAN_POINT('Ctrl Pts',(-19.8223339932062,22.2910210059157,-24.2188756818218));
#57909=CARTESIAN_POINT('Ctrl Pts',(-19.7872516723537,22.4064371914391,-24.2127881821039));
#57910=CARTESIAN_POINT('Ctrl Pts',(-19.7535272874064,22.5173859478259,-24.2069363120205));
#57911=CARTESIAN_POINT('Ctrl Pts',(-19.7246980045834,22.6298797604081,-24.2010844419371));
#57912=CARTESIAN_POINT('Ctrl Pts',(-19.700894613521,22.7434485791769,-24.1952325718537));
#57913=CARTESIAN_POINT('Ctrl Pts',(-19.6770948467414,22.8570001060604,-24.1893815927707));
#57914=CARTESIAN_POINT('Ctrl Pts',(-19.6583195349616,22.9716259092027,-24.1835306136877));
#57915=CARTESIAN_POINT('Ctrl Pts',(-19.6446486088804,23.08684450619,-24.1776796346047));
#57916=CARTESIAN_POINT('Ctrl Pts',(-19.6309764536514,23.2020734624381,-24.1718281294624));
#57917=CARTESIAN_POINT('Ctrl Pts',(-19.6224096451481,23.3178949079546,-24.1659766243201));
#57918=CARTESIAN_POINT('Ctrl Pts',(-19.6189762937397,23.4338216900134,-24.1601251191778));
#57919=CARTESIAN_POINT('Ctrl Pts',(-19.61554180219,23.5497869688329,-24.154271670878));
#57920=CARTESIAN_POINT('Ctrl Pts',(-19.6172441696736,23.6658572407673,-24.1484182225783));
#57921=CARTESIAN_POINT('Ctrl Pts',(-19.6240593939259,23.7815455167614,-24.1425647742785));
#57922=CARTESIAN_POINT('Ctrl Pts',(-19.6308823685682,23.8973653554466,-24.1367046693369));
#57923=CARTESIAN_POINT('Ctrl Pts',(-19.6428297810778,24.0128019182055,-24.1308445643954));
#57924=CARTESIAN_POINT('Ctrl Pts',(-19.6598257548193,24.1273733975231,-24.1249844594538));
#57925=CARTESIAN_POINT('Ctrl Pts',(-19.6768331742854,24.2420220335613,-24.1191204080984));
#57926=CARTESIAN_POINT('Ctrl Pts',(-19.6988958463412,24.3558040212941,-24.1132563567429));
#57927=CARTESIAN_POINT('Ctrl Pts',(-19.7258871548982,24.4682495168548,-24.1073923053874));
#57928=CARTESIAN_POINT('Ctrl Pts',(-19.752918243256,24.5808607346297,-24.1015196115908));
#57929=CARTESIAN_POINT('Ctrl Pts',(-19.784892351572,24.692131133233,-24.0956469177943));
#57930=CARTESIAN_POINT('Ctrl Pts',(-19.8216335717749,24.8016076578396,-24.0897742239977));
#57931=CARTESIAN_POINT('Ctrl Pts',(-19.8316927032601,24.831580498956,-24.0881663786745));
#57932=CARTESIAN_POINT('Ctrl Pts',(-19.8421088912036,24.86141900349,-24.0865585333513));
#57933=CARTESIAN_POINT('Ctrl Pts',(-19.8528779163308,24.8911141776766,-24.0849506880281));
#57934=CARTESIAN_POINT('Ctrl Pts',(-19.8922093822981,24.9995691881455,-24.0790783910594));
#57935=CARTESIAN_POINT('Ctrl Pts',(-19.93638274772,25.1064738593082,-24.0732060940907));
#57936=CARTESIAN_POINT('Ctrl Pts',(-19.9852564792695,25.2113642516566,-24.067333797122));
#57937=CARTESIAN_POINT('Ctrl Pts',(-20.0340668743444,25.3161187143867,-24.0614691101838));
#57938=CARTESIAN_POINT('Ctrl Pts',(-20.0875653491538,25.4188637180978,-24.0556044232456));
#57939=CARTESIAN_POINT('Ctrl Pts',(-20.1455611786818,25.5191521712702,-24.0497397363074));
#57940=CARTESIAN_POINT('Ctrl Pts',(-20.2034973631297,25.6193374840466,-24.0438810808325));
#57941=CARTESIAN_POINT('Ctrl Pts',(-20.265921496741,25.7170709157377,-24.0380224253577));
#57942=CARTESIAN_POINT('Ctrl Pts',(-20.3325958038284,25.8119276148173,-24.0321637698829));
#57943=CARTESIAN_POINT('Ctrl Pts',(-20.4018744680766,25.9104895001116,-24.026076270165));
#57944=CARTESIAN_POINT('Ctrl Pts',(-20.4757419136197,26.005944923763,-24.0199887704471));
#57945=CARTESIAN_POINT('Ctrl Pts',(-20.5538800053159,26.0978476100309,-24.0139012707292));
#57946=CARTESIAN_POINT('Ctrl Pts',(-20.6289935958473,26.1861930072016,-24.0080494006458));
#57947=CARTESIAN_POINT('Ctrl Pts',(-20.7080530782955,26.2712552411972,-24.0021975305624));
#57948=CARTESIAN_POINT('Ctrl Pts',(-20.7907336890445,26.3526701945455,-23.996345660479));
#57949=CARTESIAN_POINT('Ctrl Pts',(-20.8734017109186,26.4340727517269,-23.9904946813961));
#57950=CARTESIAN_POINT('Ctrl Pts',(-20.959689470363,26.511828842475,-23.9846437023131));
#57951=CARTESIAN_POINT('Ctrl Pts',(-21.0492350940756,26.5856109580958,-23.9787927232302));
#57952=CARTESIAN_POINT('Ctrl Pts',(-21.1387887688015,26.659399707439,-23.9729412180879));
#57953=CARTESIAN_POINT('Ctrl Pts',(-21.2316005710262,26.7292135084901,-23.9670897129456));
#57954=CARTESIAN_POINT('Ctrl Pts',(-21.3272758458338,26.7947653848235,-23.9612382078033));
#57955=CARTESIAN_POINT('Ctrl Pts',(-21.4229828923173,26.860339029508,-23.9553847595035));
#57956=CARTESIAN_POINT('Ctrl Pts',(-21.5215549613443,26.9216477017299,-23.9495313112038));
#57957=CARTESIAN_POINT('Ctrl Pts',(-21.6225693666104,26.9784483567679,-23.943677862904));
#57958=CARTESIAN_POINT('Ctrl Pts',(-21.7236986471903,27.0353136064847,-23.9378177579625));
#57959=CARTESIAN_POINT('Ctrl Pts',(-21.8272754472104,27.0876604037582,-23.931957653021));
#57960=CARTESIAN_POINT('Ctrl Pts',(-21.9328533993863,27.1352921474878,-23.9260975480794));
#57961=CARTESIAN_POINT('Ctrl Pts',(-22.038502451705,27.1829559682157,-23.920233496724));
#57962=CARTESIAN_POINT('Ctrl Pts',(-22.1461549565958,27.2258982599727,-23.9143694453686));
#57963=CARTESIAN_POINT('Ctrl Pts',(-22.2553471851667,27.2639715764705,-23.9085053940131));
#57964=CARTESIAN_POINT('Ctrl Pts',(-22.3647003412857,27.3021010054367,-23.9026327002166));
#57965=CARTESIAN_POINT('Ctrl Pts',(-22.475597355576,27.3353470191732,-23.89676000642));
#57966=CARTESIAN_POINT('Ctrl Pts',(-22.5875619796419,27.3636127167527,-23.8908873126234));
#57967=CARTESIAN_POINT('Ctrl Pts',(-22.6182160207729,27.3713513919228,-23.8892794673));
#57968=CARTESIAN_POINT('Ctrl Pts',(-22.6489500464356,27.3787170548861,-23.8876716219767));
#57969=CARTESIAN_POINT('Ctrl Pts',(-22.6797542093278,27.3857083938776,-23.8860637766533));
#57970=CARTESIAN_POINT('Ctrl Pts',(-22.7922595540549,27.411242702539,-23.8801914796846));
#57971=CARTESIAN_POINT('Ctrl Pts',(-22.9060778242296,27.4318654158321,-23.8743191827158));
#57972=CARTESIAN_POINT('Ctrl Pts',(-23.0207421949965,27.4474448291476,-23.8684468857471));
#57973=CARTESIAN_POINT('Ctrl Pts',(-23.1352579698452,27.4630040527807,-23.8625821988089));
#57974=CARTESIAN_POINT('Ctrl Pts',(-23.2506172589443,27.4735329184887,-23.8567175118707));
#57975=CARTESIAN_POINT('Ctrl Pts',(-23.3663408217403,27.4789502145074,-23.8508528249325));
#57976=CARTESIAN_POINT('Ctrl Pts',(-23.4819453700963,27.4843619391763,-23.8449941694577));
#57977=CARTESIAN_POINT('Ctrl Pts',(-23.5979130365375,27.4846725312448,-23.8391355139829));
#57978=CARTESIAN_POINT('Ctrl Pts',(-23.7137578585075,27.4798523851276,-23.8332768585081));
#57979=CARTESIAN_POINT('Ctrl Pts',(-23.8341276812585,27.4748439598575,-23.8271893587902));
#57980=CARTESIAN_POINT('Ctrl Pts',(-23.9543644165304,27.464295741682,-23.8211018590723));
#57981=CARTESIAN_POINT('Ctrl Pts',(-24.0739206395242,27.4482341520769,-23.8150143593543));
#57982=CARTESIAN_POINT('Ctrl Pts',(-24.1888491844183,27.4327942604865,-23.8091624892709));
#57983=CARTESIAN_POINT('Ctrl Pts',(-24.3031484709066,27.4122599349419,-23.8033106191875));
#57984=CARTESIAN_POINT('Ctrl Pts',(-24.4163366123485,27.3867075835927,-23.7974587491042));
#57985=CARTESIAN_POINT('Ctrl Pts',(-24.5295075198667,27.3611591228212,-23.7916077700212));
#57986=CARTESIAN_POINT('Ctrl Pts',(-24.6415672156015,27.3305942464073,-23.7857567909382));
#57987=CARTESIAN_POINT('Ctrl Pts',(-24.7520445531331,27.2951403720982,-23.7799058118553));
#57988=CARTESIAN_POINT('Ctrl Pts',(-24.8625318236407,27.2596833101446,-23.774054306713));
#57989=CARTESIAN_POINT('Ctrl Pts',(-24.9714360594924,27.2193365027986,-23.7682028015706));
#57990=CARTESIAN_POINT('Ctrl Pts',(-25.0783024948938,27.174276856939,-23.7623512964283));
#57991=CARTESIAN_POINT('Ctrl Pts',(-25.1852044183119,27.1292022477519,-23.7564978481286));
#57992=CARTESIAN_POINT('Ctrl Pts',(-25.2900668149801,27.0794118486079,-23.7506443998288));
#57993=CARTESIAN_POINT('Ctrl Pts',(-25.39245672743,27.0251298966113,-23.744790951529));
#57994=CARTESIAN_POINT('Ctrl Pts',(-25.494963079444,26.9707862142482,-23.7389308465875));
#57995=CARTESIAN_POINT('Ctrl Pts',(-25.5949909696208,26.9119409776187,-23.7330707416459));
#57996=CARTESIAN_POINT('Ctrl Pts',(-25.6921337137158,26.8488634517788,-23.7272106367044));
#57997=CARTESIAN_POINT('Ctrl Pts',(-25.7893418773691,26.7857434471732,-23.7213465853489));
#57998=CARTESIAN_POINT('Ctrl Pts',(-25.8836606905278,26.7183857177358,-23.7154825339935));
#57999=CARTESIAN_POINT('Ctrl Pts',(-25.9747154390308,26.6471007053942,-23.709618482638));
#58000=CARTESIAN_POINT('Ctrl Pts',(-26.0659043840567,26.5757106331743,-23.7037457888415));
#58001=CARTESIAN_POINT('Ctrl Pts',(-26.1538193507051,26.5003819942174,-23.6978730950449));
#58002=CARTESIAN_POINT('Ctrl Pts',(-26.2381213821525,26.4214630852301,-23.6920004012483));
#58003=CARTESIAN_POINT('Ctrl Pts',(-26.2612018681621,26.3998564081015,-23.690392555925));
#58004=CARTESIAN_POINT('Ctrl Pts',(-26.2840117677736,26.3779808097334,-23.6887847106017));
#58005=CARTESIAN_POINT('Ctrl Pts',(-26.3065446544932,26.3558438657619,-23.6871768652783));
#58006=CARTESIAN_POINT('Ctrl Pts',(-26.3876711510968,26.2761429054605,-23.6813880438199));
#58007=CARTESIAN_POINT('Ctrl Pts',(-26.4654924669509,26.1927680362001,-23.6755992223615));
#58008=CARTESIAN_POINT('Ctrl Pts',(-26.5396500511236,26.1060286312048,-23.6698104009031));
#58009=CARTESIAN_POINT('Ctrl Pts',(-26.614723138346,26.0182183958866,-23.6639501142836));
#58010=CARTESIAN_POINT('Ctrl Pts',(-26.6860410514383,25.9269602310897,-23.6580898276641));
#58011=CARTESIAN_POINT('Ctrl Pts',(-26.7532673635898,25.8326164349,-23.6522295410446));
#58012=CARTESIAN_POINT('Ctrl Pts',(-26.8195082059408,25.7396556234232,-23.6464551603048));
#58013=CARTESIAN_POINT('Ctrl Pts',(-26.8817763186912,25.6436993807576,-23.640680779565));
#58014=CARTESIAN_POINT('Ctrl Pts',(-26.9397886290073,25.5451294815363,-23.6349063988252));
#58015=CARTESIAN_POINT('Ctrl Pts',(-26.997763743313,25.4466227828146,-23.6291357204707));
#58016=CARTESIAN_POINT('Ctrl Pts',(-27.051488261838,25.3455061234113,-23.6233650421162));
#58017=CARTESIAN_POINT('Ctrl Pts',(-27.1007222013158,25.242190510787,-23.6175943637617));
#58018=CARTESIAN_POINT('Ctrl Pts',(-27.149937291019,25.1389144537224,-23.6118258947772));
#58019=CARTESIAN_POINT('Ctrl Pts',(-27.1946650365021,25.0334415013223,-23.6060574257927));
#58020=CARTESIAN_POINT('Ctrl Pts',(-27.2347116519353,24.9262067428771,-23.6002889568082));
#58021=CARTESIAN_POINT('Ctrl Pts',(-27.2758596720533,24.8160226998534,-23.5943618372437));
#58022=CARTESIAN_POINT('Ctrl Pts',(-27.3120651220472,24.7039789531522,-23.5884347176793));
#58023=CARTESIAN_POINT('Ctrl Pts',(-27.3431712727172,24.590568072286,-23.5825075981148));
#58024=CARTESIAN_POINT('Ctrl Pts',(-27.373455648871,24.4801533246521,-23.576737063525));
#58025=CARTESIAN_POINT('Ctrl Pts',(-27.3989067254962,24.3684432134283,-23.5709665289351));
#58026=CARTESIAN_POINT('Ctrl Pts',(-27.4194311967607,24.2559050366811,-23.5651959943452));
#58027=CARTESIAN_POINT('Ctrl Pts',(-27.4407910734182,24.1387862303738,-23.5591905822935));
#58028=CARTESIAN_POINT('Ctrl Pts',(-27.4568146917436,24.0207710190427,-23.5531851702417));
#58029=CARTESIAN_POINT('Ctrl Pts',(-27.4674563763962,23.9023931840644,-23.54717975819));
#58030=CARTESIAN_POINT('Ctrl Pts',(-27.4780980610489,23.7840153490861,-23.5411743461382));
#58031=CARTESIAN_POINT('Ctrl Pts',(-27.4833578310401,23.6652754085337,-23.5351689340865));
#58032=CARTESIAN_POINT('Ctrl Pts',(-27.4832509332757,23.5467066668166,-23.5291635220347));
#58033=CARTESIAN_POINT('',(-27.4886967943341,23.5521013327097,-22.2791635220347));
#58034=CARTESIAN_POINT('Ctrl Pts',(-27.4843392770373,23.5467056856009,-23.5291635220347));
#58035=CARTESIAN_POINT('Ctrl Pts',(-27.4868379542081,23.2776309960683,-23.5155389993243));
#58036=CARTESIAN_POINT('Ctrl Pts',(-27.3387877591575,21.7019972671522,-23.4356188394893));
#58037=CARTESIAN_POINT('Ctrl Pts',(-25.2134988325905,19.2057890924782,-23.2894030425282));
#58038=CARTESIAN_POINT('Ctrl Pts',(-20.7942376834532,19.8025688486209,-23.0905161311538));
#58039=CARTESIAN_POINT('Ctrl Pts',(-18.9075205083243,23.8431521583261,-22.8916292197787));
#58040=CARTESIAN_POINT('Ctrl Pts',(-21.2870804239101,27.6145855449523,-22.6927423084039));
#58041=CARTESIAN_POINT('Ctrl Pts',(-25.7463036211984,27.6512414910055,-22.4938553970289));
#58042=CARTESIAN_POINT('Ctrl Pts',(-27.4384619512156,25.064519459982,-22.3559958015726));
#58043=CARTESIAN_POINT('Ctrl Pts',(-27.48929941677,23.655847641776,-22.2844318432412));
#58044=CARTESIAN_POINT('Ctrl Pts',(-27.4886967943341,23.5521013327097,-22.2791635220347));
#58045=CARTESIAN_POINT('',(-27.4786334210255,23.5528998401325,-21.0291635220348));
#58046=CARTESIAN_POINT('Ctrl Pts',(-27.4886967943341,23.5521013327097,-22.2791635220347));
#58047=CARTESIAN_POINT('Ctrl Pts',(-27.4817161209215,22.3503221452475,-22.2181362061162));
#58048=CARTESIAN_POINT('Ctrl Pts',(-26.250718358874,19.8306521089372,-22.0908132530728));
#58049=CARTESIAN_POINT('Ctrl Pts',(-21.9586513526617,19.1790334203923,-21.8971946629042));
#58050=CARTESIAN_POINT('Ctrl Pts',(-19.0123446419315,22.5264640691018,-21.6983077515295));
#58051=CARTESIAN_POINT('Ctrl Pts',(-20.2359905307524,26.8146695119866,-21.4994208401545));
#58052=CARTESIAN_POINT('Ctrl Pts',(-24.5051621953605,28.1031525268998,-21.3005339287797));
#58053=CARTESIAN_POINT('Ctrl Pts',(-27.1783184065575,25.8212684194662,-21.1437814894064));
#58054=CARTESIAN_POINT('Ctrl Pts',(-27.4815824957208,24.0318261664217,-21.0533246871581));
#58055=CARTESIAN_POINT('Ctrl Pts',(-27.4786334210255,23.5528998401325,-21.0291635220348));
#58056=CARTESIAN_POINT('',(-27.4825165310185,23.5474017168375,-19.7791634816917));
#58057=CARTESIAN_POINT('Ctrl Pts',(-27.4786334210255,23.5528998401325,-21.0291635220348));
#58058=CARTESIAN_POINT('Ctrl Pts',(-27.4734905521056,22.717703864157,-20.9870290500331));
#58059=CARTESIAN_POINT('Ctrl Pts',(-26.8032339315992,20.5608468367781,-20.8785989409065));
#58060=CARTESIAN_POINT('Ctrl Pts',(-23.2513783123186,18.9079012919564,-20.7038731946549));
#58061=CARTESIAN_POINT('Ctrl Pts',(-19.4830103574363,21.2923127787233,-20.5049862832801));
#58062=CARTESIAN_POINT('Ctrl Pts',(-19.4520931154282,25.7515794567508,-20.3060993719051));
#58063=CARTESIAN_POINT('Ctrl Pts',(-23.18703691035,28.188013332395,-20.1072124605302));
#58064=CARTESIAN_POINT('Ctrl Pts',(-26.7802818937802,26.576037175659,-19.9315671772402));
#58065=CARTESIAN_POINT('Ctrl Pts',(-27.4733345361709,24.4006161878087,-19.822217531075));
#58066=CARTESIAN_POINT('Ctrl Pts',(-27.4790222659213,23.5474050497456,-19.7791635220348));
#58067=CARTESIAN_POINT('',(-27.4847537623865,23.5487013432092,-18.5291635220347));
#58068=CARTESIAN_POINT('Ctrl Pts',(-27.4832514979866,23.5474010158096,-19.7791634732061));
#58069=CARTESIAN_POINT('Ctrl Pts',(-27.4831548869444,23.4141486881421,-19.7724466029512));
#58070=CARTESIAN_POINT('Ctrl Pts',(-27.4762823074789,23.2811691169794,-19.7657297326962));
#58071=CARTESIAN_POINT('Ctrl Pts',(-27.4627405440319,23.1490960119743,-19.7590128624413));
#58072=CARTESIAN_POINT('Ctrl Pts',(-27.4491281784238,23.0163343226009,-19.7522609727033));
#58073=CARTESIAN_POINT('Ctrl Pts',(-27.4287770222172,22.8844887235092,-19.7455090829653));
#58074=CARTESIAN_POINT('Ctrl Pts',(-27.4018449061974,22.7541839538263,-19.7387571932273));
#58075=CARTESIAN_POINT('Ctrl Pts',(-27.3747435418534,22.6230603155519,-19.7319628728825));
#58076=CARTESIAN_POINT('Ctrl Pts',(-27.3409783391831,22.493497077691,-19.7251685525378));
#58077=CARTESIAN_POINT('Ctrl Pts',(-27.3007584029886,22.3661095042748,-19.7183742321931));
#58078=CARTESIAN_POINT('Ctrl Pts',(-27.2831265664499,22.3102646401587,-19.7153957007222));
#58079=CARTESIAN_POINT('Ctrl Pts',(-27.2642548609165,22.2548376114924,-19.7124171692514));
#58080=CARTESIAN_POINT('Ctrl Pts',(-27.2441637335036,22.1998788674267,-19.7094386377806));
#58081=CARTESIAN_POINT('Ctrl Pts',(-27.2045532517075,22.0915254491934,-19.7035663408119));
#58082=CARTESIAN_POINT('Ctrl Pts',(-27.1601048768239,21.9847348274173,-19.6976940438432));
#58083=CARTESIAN_POINT('Ctrl Pts',(-27.1109613358181,21.8799705757854,-19.6918217468745));
#58084=CARTESIAN_POINT('Ctrl Pts',(-27.0618814809385,21.7753420903032,-19.6859570599363));
#58085=CARTESIAN_POINT('Ctrl Pts',(-27.0081187338839,21.6727351235627,-19.6800923729981));
#58086=CARTESIAN_POINT('Ctrl Pts',(-26.9498649697813,21.5725962747063,-19.6742276860599));
#58087=CARTESIAN_POINT('Ctrl Pts',(-26.8916711160285,21.4725604123873,-19.668369030585));
#58088=CARTESIAN_POINT('Ctrl Pts',(-26.8289956387334,21.3749879743061,-19.6625103751102));
#58089=CARTESIAN_POINT('Ctrl Pts',(-26.7620774062967,21.2803031985846,-19.6566517196354));
#58090=CARTESIAN_POINT('Ctrl Pts',(-26.6925452887602,21.1819199521262,-19.6505642199175));
#58091=CARTESIAN_POINT('Ctrl Pts',(-26.6184324006713,21.0866549678212,-19.6444767201996));
#58092=CARTESIAN_POINT('Ctrl Pts',(-26.5400580247613,20.994953701102,-19.6383892204817));
#58093=CARTESIAN_POINT('Ctrl Pts',(-26.4647172958995,20.9068019271075,-19.6325373503983));
#58094=CARTESIAN_POINT('Ctrl Pts',(-26.3854391385356,20.8219434615173,-19.6266854803149));
#58095=CARTESIAN_POINT('Ctrl Pts',(-26.3025492523911,20.740741584707,-19.6208336102315));
#58096=CARTESIAN_POINT('Ctrl Pts',(-26.2196719869855,20.6595520716208,-19.6149826311485));
#58097=CARTESIAN_POINT('Ctrl Pts',(-26.1331843814294,20.5820183295237,-19.6091316520655));
#58098=CARTESIAN_POINT('Ctrl Pts',(-26.0434491507821,20.5084669346199,-19.6032806729825));
#58099=CARTESIAN_POINT('Ctrl Pts',(-25.953705852074,20.434908926738,-19.5974291678402));
#58100=CARTESIAN_POINT('Ctrl Pts',(-25.8607146675498,20.3653342398886,-19.5915776626979));
#58101=CARTESIAN_POINT('Ctrl Pts',(-25.7648709894502,20.3000288337671,-19.5857261575556));
#58102=CARTESIAN_POINT('Ctrl Pts',(-25.6689954837516,20.2347017411421,-19.5798727092559));
#58103=CARTESIAN_POINT('Ctrl Pts',(-25.5702659423666,20.1736469809691,-19.5740192609561));
#58104=CARTESIAN_POINT('Ctrl Pts',(-25.4691056757582,20.1171065092367,-19.5681658126563));
#58105=CARTESIAN_POINT('Ctrl Pts',(-25.3678303679599,20.0605017387103,-19.5623057077148));
#58106=CARTESIAN_POINT('Ctrl Pts',(-25.2641191786131,20.00842170519,-19.5564456027732));
#58107=CARTESIAN_POINT('Ctrl Pts',(-25.1584189795438,19.961061860246,-19.5505854978317));
#58108=CARTESIAN_POINT('Ctrl Pts',(-25.052647598006,19.9136701214106,-19.5447214464762));
#58109=CARTESIAN_POINT('Ctrl Pts',(-24.9448849230039,19.8710050524779,-19.5388573951208));
#58110=CARTESIAN_POINT('Ctrl Pts',(-24.8355950613967,19.8332129056829,-19.5329933437653));
#58111=CARTESIAN_POINT('Ctrl Pts',(-24.72614412835,19.7953650608077,-19.5271206499687));
#58112=CARTESIAN_POINT('Ctrl Pts',(-24.6151619113872,19.7624045886342,-19.5212479561722));
#58113=CARTESIAN_POINT('Ctrl Pts',(-24.5031249067341,19.7344271639807,-19.5153752623756));
#58114=CARTESIAN_POINT('Ctrl Pts',(-24.4724510490102,19.7267674131157,-19.5137674170523));
#58115=CARTESIAN_POINT('Ctrl Pts',(-24.4416981670942,19.7194808790896,-19.5121595717289));
#58116=CARTESIAN_POINT('Ctrl Pts',(-24.4108761116318,19.7125688483176,-19.5105517264056));
#58117=CARTESIAN_POINT('Ctrl Pts',(-24.2983054182734,19.6873241952645,-19.5046794294369));
#58118=CARTESIAN_POINT('Ctrl Pts',(-24.1844344454888,19.6669945005741,-19.4988071324682));
#58119=CARTESIAN_POINT('Ctrl Pts',(-24.0697303555742,19.6517102668859,-19.4929348354995));
#58120=CARTESIAN_POINT('Ctrl Pts',(-23.9551749130504,19.6364458403506,-19.4870701485613));
#58121=CARTESIAN_POINT('Ctrl Pts',(-23.8397889064191,19.626213926151,-19.4812054616231));
#58122=CARTESIAN_POINT('Ctrl Pts',(-23.7240517836723,19.6210945022925,-19.4753407746849));
#58123=CARTESIAN_POINT('Ctrl Pts',(-23.608433689311,19.615980343441,-19.4694821192101));
#58124=CARTESIAN_POINT('Ctrl Pts',(-23.4924656075789,19.6159682349018,-19.4636234637352));
#58125=CARTESIAN_POINT('Ctrl Pts',(-23.3766335756227,19.6210865313714,-19.4577648082604));
#58126=CARTESIAN_POINT('Ctrl Pts',(-23.2562770424747,19.6264047530092,-19.4516773085425));
#58127=CARTESIAN_POINT('Ctrl Pts',(-23.1360678549191,19.6372624066566,-19.4455898088246));
#58128=CARTESIAN_POINT('Ctrl Pts',(-23.0165533679367,19.6536316619399,-19.4395023091067));
#58129=CARTESIAN_POINT('Ctrl Pts',(-22.901664943573,19.6693673103537,-19.4336504390233));
#58130=CARTESIAN_POINT('Ctrl Pts',(-22.7874188878009,19.6901957562352,-19.4277985689399));
#58131=CARTESIAN_POINT('Ctrl Pts',(-22.6742968890025,19.7160393513876,-19.4219466988565));
#58132=CARTESIAN_POINT('Ctrl Pts',(-22.5611921140569,19.7418790116177,-19.4160957197736));
#58133=CARTESIAN_POINT('Ctrl Pts',(-22.4492114586774,19.7727322107903,-19.4102447406906));
#58134=CARTESIAN_POINT('Ctrl Pts',(-22.3388257397701,19.8084703189233,-19.4043937616076));
#58135=CARTESIAN_POINT('Ctrl Pts',(-22.2284300961243,19.8442116402562,-19.3985422564653));
#58136=CARTESIAN_POINT('Ctrl Pts',(-22.1196300673251,19.8848386163031,-19.392690751323));
#58137=CARTESIAN_POINT('Ctrl Pts',(-22.0128799623301,19.9301731702759,-19.3868392461807));
#58138=CARTESIAN_POINT('Ctrl Pts',(-21.9060944079491,19.9755227788672,-19.380985797881));
#58139=CARTESIAN_POINT('Ctrl Pts',(-21.8013605112626,20.0255829123746,-19.3751323495812));
#58140=CARTESIAN_POINT('Ctrl Pts',(-21.699110651154,20.0801282200722,-19.3692789012814));
#58141=CARTESIAN_POINT('Ctrl Pts',(-21.5967445107514,20.1347355576289,-19.3634187963399));
#58142=CARTESIAN_POINT('Ctrl Pts',(-21.4968684102677,20.1938380553713,-19.3575586913983));
#58143=CARTESIAN_POINT('Ctrl Pts',(-21.3998883395547,20.2571654023937,-19.3516985864568));
#58144=CARTESIAN_POINT('Ctrl Pts',(-21.3028429588338,20.3205353964209,-19.3458345351014));
#58145=CARTESIAN_POINT('Ctrl Pts',(-21.208697826273,20.3881356645102,-19.3399704837459));
#58146=CARTESIAN_POINT('Ctrl Pts',(-21.1178268557636,20.4596548013071,-19.3341064323905));
#58147=CARTESIAN_POINT('Ctrl Pts',(-21.0268219595834,20.531279343035,-19.3282337385939));
#58148=CARTESIAN_POINT('Ctrl Pts',(-20.9391011681863,20.6068340117496,-19.3223610447973));
#58149=CARTESIAN_POINT('Ctrl Pts',(-20.8550025408124,20.6859696394764,-19.3164883510008));
#58150=CARTESIAN_POINT('Ctrl Pts',(-20.8319777434356,20.7076356505707,-19.3148805056774));
#58151=CARTESIAN_POINT('Ctrl Pts',(-20.8092242237213,20.7295698855669,-19.3132726603541));
#58152=CARTESIAN_POINT('Ctrl Pts',(-20.7867483886439,20.7517647523133,-19.3116648150308));
#58153=CARTESIAN_POINT('Ctrl Pts',(-20.7046604064988,20.8328265602026,-19.3057925180621));
#58154=CARTESIAN_POINT('Ctrl Pts',(-20.626004605136,20.9176390583445,-19.2999202210933));
#58155=CARTESIAN_POINT('Ctrl Pts',(-20.551143299641,21.00587975747,-19.2940479241246));
#58156=CARTESIAN_POINT('Ctrl Pts',(-20.4763790084525,21.0940061036575,-19.2881832371864));
#58157=CARTESIAN_POINT('Ctrl Pts',(-20.4053996992186,21.1855515036248,-19.2823185502482));
#58158=CARTESIAN_POINT('Ctrl Pts',(-20.3385318207419,21.2801558212345,-19.27645386331));
#58159=CARTESIAN_POINT('Ctrl Pts',(-20.2717327116923,21.3746628442257,-19.2705952078352));
#58160=CARTESIAN_POINT('Ctrl Pts',(-20.209036860163,21.4722221919493,-19.2647365523604));
#58161=CARTESIAN_POINT('Ctrl Pts',(-20.1507308451182,21.5724402801143,-19.2588778968856));
#58162=CARTESIAN_POINT('Ctrl Pts',(-20.0901473457704,21.676572975074,-19.2527903971677));
#58163=CARTESIAN_POINT('Ctrl Pts',(-20.0343039100533,21.7835760035491,-19.2467028974498));
#58164=CARTESIAN_POINT('Ctrl Pts',(-19.9834729923779,21.8929738231136,-19.2406153977319));
#58165=CARTESIAN_POINT('Ctrl Pts',(-19.9346095935704,21.9981371672063,-19.2347635276485));
#58166=CARTESIAN_POINT('Ctrl Pts',(-19.8903780781764,22.1055129487554,-19.2289116575651));
#58167=CARTESIAN_POINT('Ctrl Pts',(-19.8509734924559,22.214653943101,-19.2230597874817));
#58168=CARTESIAN_POINT('Ctrl Pts',(-19.8115749064419,22.3237783197377,-19.2172088083987));
#58169=CARTESIAN_POINT('Ctrl Pts',(-19.7770019291389,22.4346669860602,-19.2113578293158));
#58170=CARTESIAN_POINT('Ctrl Pts',(-19.7474008384818,22.5468543059475,-19.2055068502328));
#58171=CARTESIAN_POINT('Ctrl Pts',(-19.7177970864018,22.6590517125545,-19.1996553450905));
#58172=CARTESIAN_POINT('Ctrl Pts',(-19.6931662150729,22.7725476051101,-19.1938038399482));
#58173=CARTESIAN_POINT('Ctrl Pts',(-19.6736039787566,22.8868635078125,-19.1879523348059));
#58174=CARTESIAN_POINT('Ctrl Pts',(-19.6540352462474,23.0012173723376,-19.1820988865061));
#58175=CARTESIAN_POINT('Ctrl Pts',(-19.6395385653444,23.1163913812315,-19.1762454382064));
#58176=CARTESIAN_POINT('Ctrl Pts',(-19.6301580638171,23.2318999552646,-19.1703919899066));
#58177=CARTESIAN_POINT('Ctrl Pts',(-19.6207668946226,23.3475398876284,-19.164531884965));
#58178=CARTESIAN_POINT('Ctrl Pts',(-19.6165035512497,23.4635147322737,-19.1586717800235));
#58179=CARTESIAN_POINT('Ctrl Pts',(-19.6173600713241,23.5793368086224,-19.152811675082));
#58180=CARTESIAN_POINT('Ctrl Pts',(-19.6182171682113,23.6952368838906,-19.1469476237265));
#58181=CARTESIAN_POINT('Ctrl Pts',(-19.6242009727242,23.8109835741852,-19.1410835723711));
#58182=CARTESIAN_POINT('Ctrl Pts',(-19.6352516106229,23.9260939716803,-19.1352195210156));
#58183=CARTESIAN_POINT('Ctrl Pts',(-19.646318534956,24.0413740189231,-19.1293468272191));
#58184=CARTESIAN_POINT('Ctrl Pts',(-19.662467138922,24.1560154939564,-19.1234741334225));
#58185=CARTESIAN_POINT('Ctrl Pts',(-19.6835863969961,24.2695452417774,-19.1176014396259));
#58186=CARTESIAN_POINT('Ctrl Pts',(-19.6893684965749,24.3006277876107,-19.1159935943026));
#58187=CARTESIAN_POINT('Ctrl Pts',(-19.6955228944996,24.3316270893847,-19.1143857489792));
#58188=CARTESIAN_POINT('Ctrl Pts',(-19.7020466666069,24.3625336529246,-19.1127779036558));
#58189=CARTESIAN_POINT('Ctrl Pts',(-19.7258732913532,24.475412993214,-19.1069056066871));
#58190=CARTESIAN_POINT('Ctrl Pts',(-19.7547106739523,24.5874321893099,-19.1010333097184));
#58191=CARTESIAN_POINT('Ctrl Pts',(-19.7884833454349,24.6981121003305,-19.0951610127497));
#58192=CARTESIAN_POINT('Ctrl Pts',(-19.8222122502174,24.8086485789765,-19.0892963258115));
#58193=CARTESIAN_POINT('Ctrl Pts',(-19.8608636055139,24.9178488323108,-19.0834316388733));
#58194=CARTESIAN_POINT('Ctrl Pts',(-19.9043108821663,25.0252435446287,-19.0775669519351));
#58195=CARTESIAN_POINT('Ctrl Pts',(-19.9477134760145,25.1325278082081,-19.0717082964603));
#58196=CARTESIAN_POINT('Ctrl Pts',(-19.9959020265119,25.2380098433052,-19.0658496409854));
#58197=CARTESIAN_POINT('Ctrl Pts',(-20.0487003126699,25.3412357972347,-19.0599909855106));
#58198=CARTESIAN_POINT('Ctrl Pts',(-20.1035609463894,25.4484938478449,-19.0539034857927));
#58199=CARTESIAN_POINT('Ctrl Pts',(-20.1633986451923,25.5533155403398,-19.0478159860748));
#58200=CARTESIAN_POINT('Ctrl Pts',(-20.2279606004165,25.6552146034111,-19.0417284863569));
#58201=CARTESIAN_POINT('Ctrl Pts',(-20.2900235477364,25.7531694463428,-19.0358766162735));
#58202=CARTESIAN_POINT('Ctrl Pts',(-20.3564515851535,25.8484233242809,-19.0300247461901));
#58203=CARTESIAN_POINT('Ctrl Pts',(-20.4269738858302,25.9405703976464,-19.0241728761067));
#58204=CARTESIAN_POINT('Ctrl Pts',(-20.4974854488454,26.0327034407821,-19.0183218970237));
#58205=CARTESIAN_POINT('Ctrl Pts',(-20.5720897844552,26.1217302917127,-19.0124709179407));
#58206=CARTESIAN_POINT('Ctrl Pts',(-20.6504742146036,26.2072761882941,-19.0066199388578));
#58207=CARTESIAN_POINT('Ctrl Pts',(-20.7288656922667,26.2928297762749,-19.0007684337155));
#58208=CARTESIAN_POINT('Ctrl Pts',(-20.8110376608059,26.3749014829454,-18.9949169285732));
#58209=CARTESIAN_POINT('Ctrl Pts',(-20.8966393297389,26.4531521121841,-18.9890654234309));
#58210=CARTESIAN_POINT('Ctrl Pts',(-20.9822694251227,26.5314287267534,-18.9832119751311));
#58211=CARTESIAN_POINT('Ctrl Pts',(-21.0713311806373,26.605881462006,-18.9773585268313));
#58212=CARTESIAN_POINT('Ctrl Pts',(-21.1634399232597,26.6762107163502,-18.9715050785316));
#58213=CARTESIAN_POINT('Ctrl Pts',(-21.2556534135233,26.7466199503283,-18.96564497359));
#58214=CARTESIAN_POINT('Ctrl Pts',(-21.3509204783491,26.8128960926927,-18.9597848686485));
#58215=CARTESIAN_POINT('Ctrl Pts',(-21.4488265198836,26.874782230296,-18.9539247637069));
#58216=CARTESIAN_POINT('Ctrl Pts',(-21.5467984950092,26.9367100443397,-18.9480607123515));
#58217=CARTESIAN_POINT('Ctrl Pts',(-21.6474126275914,26.9942417621599,-18.942196660996));
#58218=CARTESIAN_POINT('Ctrl Pts',(-21.7502302746088,27.0471667248075,-18.9363326096406));
#58219=CARTESIAN_POINT('Ctrl Pts',(-21.8531994543136,27.1001696882853,-18.930459915844));
#58220=CARTESIAN_POINT('Ctrl Pts',(-21.9583782557738,27.148552174076,-18.9245872220475));
#58221=CARTESIAN_POINT('Ctrl Pts',(-22.0653085917438,27.1921518294789,-18.9187145282509));
#58222=CARTESIAN_POINT('Ctrl Pts',(-22.094584329006,27.2040886857949,-18.9171066829276));
#58223=CARTESIAN_POINT('Ctrl Pts',(-22.1239912746833,27.215667324323,-18.9154988376043));
#58224=CARTESIAN_POINT('Ctrl Pts',(-22.1535198605328,27.2268850732069,-18.9138909922809));
#58225=CARTESIAN_POINT('Ctrl Pts',(-22.2613664441935,27.2678554027602,-18.9080186953122));
#58226=CARTESIAN_POINT('Ctrl Pts',(-22.371197901153,27.3041451532595,-18.9021463983435));
#58227=CARTESIAN_POINT('Ctrl Pts',(-22.4825703279712,27.3355588220561,-18.8962741013748));
#58228=CARTESIAN_POINT('Ctrl Pts',(-22.5937984249692,27.3669317812327,-18.8904094144366));
#58229=CARTESIAN_POINT('Ctrl Pts',(-22.7065631263732,27.3934411137744,-18.8845447274984));
#58230=CARTESIAN_POINT('Ctrl Pts',(-22.8204011946328,27.4149395857504,-18.8786800405602));
#58231=CARTESIAN_POINT('Ctrl Pts',(-22.9341221875655,27.4364159478938,-18.8728213850854));
#58232=CARTESIAN_POINT('Ctrl Pts',(-23.0489139478978,27.4528916235118,-18.8669627296105));
#58233=CARTESIAN_POINT('Ctrl Pts',(-23.1642993868358,27.4642695436621,-18.8611040741357));
#58234=CARTESIAN_POINT('Ctrl Pts',(-23.284191882649,27.476091895395,-18.8550165744178));
#58235=CARTESIAN_POINT('Ctrl Pts',(-23.4047249441723,27.4824100039208,-18.8489290746999));
#58236=CARTESIAN_POINT('Ctrl Pts',(-23.5253528093961,27.4831737111522,-18.842841574982));
#58237=CARTESIAN_POINT('Ctrl Pts',(-23.6413115163265,27.4839078574696,-18.8369897048986));
#58238=CARTESIAN_POINT('Ctrl Pts',(-23.7573573723373,27.4795095941686,-18.8311378348152));
#58239=CARTESIAN_POINT('Ctrl Pts',(-23.8730025443944,27.4699873989144,-18.8252859647318));
#58240=CARTESIAN_POINT('Ctrl Pts',(-23.9886301084224,27.4604666535011,-18.8194349856488));
#58241=CARTESIAN_POINT('Ctrl Pts',(-24.1038566979243,27.4458235612667,-18.8135840065658));
#58242=CARTESIAN_POINT('Ctrl Pts',(-24.2181980034755,27.4261186086797,-18.8077330274829));
#58243=CARTESIAN_POINT('Ctrl Pts',(-24.3325495894105,27.4064118844278,-18.8018815223406));
#58244=CARTESIAN_POINT('Ctrl Pts',(-24.4460153257643,27.3816424653162,-18.7960300171983));
#58245=CARTESIAN_POINT('Ctrl Pts',(-24.5581202240218,27.35192212738,-18.790178512056));
#58246=CARTESIAN_POINT('Ctrl Pts',(-24.6702623498755,27.3221919199667,-18.7843250637562));
#58247=CARTESIAN_POINT('Ctrl Pts',(-24.7810423396812,27.2875076304317,-18.7784716154564));
#58248=CARTESIAN_POINT('Ctrl Pts',(-24.8900002015165,27.2480309432821,-18.7726181671567));
#58249=CARTESIAN_POINT('Ctrl Pts',(-24.9990819721007,27.208509362567,-18.7667580622151));
#58250=CARTESIAN_POINT('Ctrl Pts',(-25.1063370898653,27.1641846471078,-18.7608979572736));
#58251=CARTESIAN_POINT('Ctrl Pts',(-25.211325301753,27.1152667325873,-18.755037852332));
#58252=CARTESIAN_POINT('Ctrl Pts',(-25.3163842166304,27.066315874913,-18.7491738009766));
#58253=CARTESIAN_POINT('Ctrl Pts',(-25.4191728201105,27.0127658494672,-18.7433097496211));
#58254=CARTESIAN_POINT('Ctrl Pts',(-25.5192767761365,26.954871823891,-18.7374456982657));
#58255=CARTESIAN_POINT('Ctrl Pts',(-25.619528265411,26.8968924740778,-18.7315730044691));
#58256=CARTESIAN_POINT('Ctrl Pts',(-25.7170868635152,26.8345565683424,-18.7257003106725));
#58257=CARTESIAN_POINT('Ctrl Pts',(-25.8115683648219,26.7681617446531,-18.7198276168759));
#58258=CARTESIAN_POINT('Ctrl Pts',(-25.837435819397,26.7499839525769,-18.7182197715526));
#58259=CARTESIAN_POINT('Ctrl Pts',(-25.8630728230474,26.7315021407593,-18.7166119262293));
#58260=CARTESIAN_POINT('Ctrl Pts',(-25.8884719558549,26.7127229148721,-18.715004080906));
#58261=CARTESIAN_POINT('Ctrl Pts',(-25.9803593868226,26.6447845787322,-18.709187316323));
#58262=CARTESIAN_POINT('Ctrl Pts',(-26.0694515345047,26.5727136196195,-18.7033705517401));
#58263=CARTESIAN_POINT('Ctrl Pts',(-26.155348143687,26.4967701122248,-18.6975537871571));
#58264=CARTESIAN_POINT('Ctrl Pts',(-26.2411330667938,26.4209253494997,-18.6917445857552));
#58265=CARTESIAN_POINT('Ctrl Pts',(-26.3237303977159,26.3412183244325,-18.6859353843533));
#58266=CARTESIAN_POINT('Ctrl Pts',(-26.4027696642176,26.2579517411081,-18.6801261829514));
#58267=CARTESIAN_POINT('Ctrl Pts',(-26.4817283079108,26.1747700926027,-18.6743229071375));
#58268=CARTESIAN_POINT('Ctrl Pts',(-26.557135814654,26.0880364092415,-18.6685196313236));
#58269=CARTESIAN_POINT('Ctrl Pts',(-26.6286561731011,25.9980923999398,-18.6627163555098));
#58270=CARTESIAN_POINT('Ctrl Pts',(-26.7001248679531,25.9082133627802,-18.6569172717623));
#58271=CARTESIAN_POINT('Ctrl Pts',(-26.7677117365892,25.815128940433,-18.6511181880149));
#58272=CARTESIAN_POINT('Ctrl Pts',(-26.8311194402516,25.7192157237131,-18.6453191042674));
#58273=CARTESIAN_POINT('Ctrl Pts',(-26.8945033838994,25.6233384474121,-18.6395221935416));
#58274=CARTESIAN_POINT('Ctrl Pts',(-26.9537110422492,25.524634834789,-18.6337252828158));
#58275=CARTESIAN_POINT('Ctrl Pts',(-27.0084874227957,25.4235118404842,-18.6279283720901));
#58276=CARTESIAN_POINT('Ctrl Pts',(-27.0632571596509,25.3224011111364,-18.6221321644572));
#58277=CARTESIAN_POINT('Ctrl Pts',(-27.1135964864597,25.2188719546065,-18.6163359568244));
#58278=CARTESIAN_POINT('Ctrl Pts',(-27.1592959605735,25.1133566640101,-18.6105397491915));
#58279=CARTESIAN_POINT('Ctrl Pts',(-27.2050014738847,25.0078274295408,-18.6047427755883));
#58280=CARTESIAN_POINT('Ctrl Pts',(-27.2460657490443,24.9003119269598,-18.5989458019851));
#58281=CARTESIAN_POINT('Ctrl Pts',(-27.2823274847592,24.7912624207381,-18.5931488283819));
#58282=CARTESIAN_POINT('Ctrl Pts',(-27.3186242467916,24.6821075802696,-18.5873462553049));
#58283=CARTESIAN_POINT('Ctrl Pts',(-27.3501090735423,24.5714161786179,-18.581543682228));
#58284=CARTESIAN_POINT('Ctrl Pts',(-27.3766705692112,24.4596556338248,-18.575741109151));
#58285=CARTESIAN_POINT('Ctrl Pts',(-27.4032457905336,24.3478373367671,-18.5699355375943));
#58286=CARTESIAN_POINT('Ctrl Pts',(-27.4248925360662,24.2349492107402,-18.5641299660375));
#58287=CARTESIAN_POINT('Ctrl Pts',(-27.4415509003059,24.1214670329453,-18.5583243944808));
#58288=CARTESIAN_POINT('Ctrl Pts',(-27.4582343676282,24.0078138448145,-18.5525100743014));
#58289=CARTESIAN_POINT('Ctrl Pts',(-27.4699143998778,23.8935652367043,-18.5466957541221));
#58290=CARTESIAN_POINT('Ctrl Pts',(-27.476583114686,23.7792004582255,-18.5408814339428));
#58291=CARTESIAN_POINT('Ctrl Pts',(-27.4810630544585,23.7023719636196,-18.5369754633068));
#58292=CARTESIAN_POINT('Ctrl Pts',(-27.4832825003658,23.6254910618527,-18.5330694926707));
#58293=CARTESIAN_POINT('Ctrl Pts',(-27.4832522260306,23.5487019351943,-18.5291635220347));
#58294=CARTESIAN_POINT('',(-27.4832508811685,23.5538557292739,-17.2791635220348));
#58295=CARTESIAN_POINT('Ctrl Pts',(-27.4890146679522,23.5486996633349,-18.5291635220347));
#58296=CARTESIAN_POINT('Ctrl Pts',(-27.4894437676505,23.4630796333703,-18.5248147378669));
#58297=CARTESIAN_POINT('Ctrl Pts',(-27.4868948921978,23.3774856217654,-18.520465953699));
#58298=CARTESIAN_POINT('Ctrl Pts',(-27.3957955962931,21.9903054538677,-18.4498215324062));
#58299=CARTESIAN_POINT('Ctrl Pts',(-25.8029561903201,19.480107932479,-18.3172302581562));
#58300=CARTESIAN_POINT('Ctrl Pts',(-21.3436534168568,19.454929445721,-18.1183433467813));
#58301=CARTESIAN_POINT('Ctrl Pts',(-18.9120281411762,23.1930056488349,-17.9194564354064));
#58302=CARTESIAN_POINT('Ctrl Pts',(-20.7425378238047,27.2593614477559,-17.7205695240317));
#58303=CARTESIAN_POINT('Ctrl Pts',(-25.1530992680317,27.9173606333916,-17.5216826126568));
#58304=CARTESIAN_POINT('Ctrl Pts',(-27.3263780446851,25.4353497891762,-17.3745472786577));
#58305=CARTESIAN_POINT('Ctrl Pts',(-27.4864548523518,23.841195331127,-17.2937075817838));
#58306=CARTESIAN_POINT('Ctrl Pts',(-27.4837830291836,23.5538562167988,-17.2791635220348));
#58307=CARTESIAN_POINT('',(-27.4832525305424,23.550157346478,-16.029163521997));
#58308=CARTESIAN_POINT('Ctrl Pts',(-27.4832508811685,23.5538557292739,-17.2791635220348));
#58309=CARTESIAN_POINT('Ctrl Pts',(-27.4833554833984,23.4396792545031,-17.2733834885699));
#58310=CARTESIAN_POINT('Ctrl Pts',(-27.4784840087521,23.3253527973785,-17.267603455105));
#58311=CARTESIAN_POINT('Ctrl Pts',(-27.4686240491294,23.2113518805405,-17.2618234216402));
#58312=CARTESIAN_POINT('Ctrl Pts',(-27.4587719553128,23.0974419082031,-17.2560479992106));
#58313=CARTESIAN_POINT('Ctrl Pts',(-27.4439393254061,22.9838573821482,-17.2502725767811));
#58314=CARTESIAN_POINT('Ctrl Pts',(-27.4241658163455,22.8710729803218,-17.2444971543516));
#58315=CARTESIAN_POINT('Ctrl Pts',(-27.4044007235877,22.7583365835151,-17.2387241901456));
#58316=CARTESIAN_POINT('Ctrl Pts',(-27.3796990029499,22.6464000529191,-17.2329512259396));
#58317=CARTESIAN_POINT('Ctrl Pts',(-27.3501519843061,22.5357313884744,-17.2271782617335));
#58318=CARTESIAN_POINT('Ctrl Pts',(-27.3206099289805,22.4250813141896,-17.221406267272));
#58319=CARTESIAN_POINT('Ctrl Pts',(-27.2862243030079,22.3156990939649,-17.2156342728105));
#58320=CARTESIAN_POINT('Ctrl Pts',(-27.2471370162021,22.2080401385893,-17.2098622783489));
#58321=CARTESIAN_POINT('Ctrl Pts',(-27.2080462240232,22.1003715282889,-17.2040897662512));
#58322=CARTESIAN_POINT('Ctrl Pts',(-27.1642530792576,21.9944268897999,-17.1983172541535));
#58323=CARTESIAN_POINT('Ctrl Pts',(-27.1159482858359,21.8906433039252,-17.1925447420557));
#58324=CARTESIAN_POINT('Ctrl Pts',(-27.0675959483043,21.7867575688049,-17.186766548349));
#58325=CARTESIAN_POINT('Ctrl Pts',(-27.0147232731088,21.6850375211772,-17.1809883546422));
#58326=CARTESIAN_POINT('Ctrl Pts',(-26.9575677724546,21.5858972048549,-17.1752101609355));
#58327=CARTESIAN_POINT('Ctrl Pts',(-26.9003845973986,21.4867088852973,-17.1694291694568));
#58328=CARTESIAN_POINT('Ctrl Pts',(-26.8389146971259,21.3901031427884,-17.1636481779782));
#58329=CARTESIAN_POINT('Ctrl Pts',(-26.7734388437342,21.2964648314265,-17.1578671864995));
#58330=CARTESIAN_POINT('Ctrl Pts',(-26.7078547407901,21.2026717102413,-17.1520766374556));
#58331=CARTESIAN_POINT('Ctrl Pts',(-26.6382517134931,21.1118561586708,-17.1462860884118));
#58332=CARTESIAN_POINT('Ctrl Pts',(-26.5649509698691,21.0243700469246,-17.1404955393679));
#58333=CARTESIAN_POINT('Ctrl Pts',(-26.4949621506987,20.94083679266,-17.1349666228809));
#58334=CARTESIAN_POINT('Ctrl Pts',(-26.4216027264079,20.8603388731378,-17.129437706394));
#58335=CARTESIAN_POINT('Ctrl Pts',(-26.345181578633,20.7831492407819,-17.123908789907));
#58336=CARTESIAN_POINT('Ctrl Pts',(-26.2640141970163,20.7011656468592,-17.1180364929383));
#58337=CARTESIAN_POINT('Ctrl Pts',(-26.1791005452029,20.6226190577235,-17.1121641959696));
#58338=CARTESIAN_POINT('Ctrl Pts',(-26.0907635784659,20.5478713731418,-17.1062918990009));
#58339=CARTESIAN_POINT('Ctrl Pts',(-26.0025410894224,20.473220555623,-17.1004272120627));
#58340=CARTESIAN_POINT('Ctrl Pts',(-25.9109044204077,20.4023591169809,-17.0945625251245));
#58341=CARTESIAN_POINT('Ctrl Pts',(-25.8162141273757,20.3356130422808,-17.0886978381862));
#58342=CARTESIAN_POINT('Ctrl Pts',(-25.7216212173822,20.26893561174,-17.0828391827114));
#58343=CARTESIAN_POINT('Ctrl Pts',(-25.6239812657574,20.2063653634263,-17.0769805272366));
#58344=CARTESIAN_POINT('Ctrl Pts',(-25.5236882252713,20.1481883695544,-17.0711218717617));
#58345=CARTESIAN_POINT('Ctrl Pts',(-25.4194776502871,20.0877389310604,-17.0650343720438));
#58346=CARTESIAN_POINT('Ctrl Pts',(-25.3124028442579,20.0320332461679,-17.0589468723259));
#58347=CARTESIAN_POINT('Ctrl Pts',(-25.2029396998435,19.9813431570764,-17.052859372608));
#58348=CARTESIAN_POINT('Ctrl Pts',(-25.0977135594381,19.9326151357826,-17.0470075025246));
#58349=CARTESIAN_POINT('Ctrl Pts',(-24.9902809442824,19.8885218413018,-17.0411556324412));
#58350=CARTESIAN_POINT('Ctrl Pts',(-24.8810893296753,19.8492577441892,-17.0353037623578));
#58351=CARTESIAN_POINT('Ctrl Pts',(-24.7719143404843,19.8099996253923,-17.0294527832748));
#58352=CARTESIAN_POINT('Ctrl Pts',(-24.660981273252,19.7755693818141,-17.0236018041918));
#58353=CARTESIAN_POINT('Ctrl Pts',(-24.548755951962,19.7461126920309,-17.0177508251089));
#58354=CARTESIAN_POINT('Ctrl Pts',(-24.4365205405355,19.7166533538078,-17.0118993199666));
#58355=CARTESIAN_POINT('Ctrl Pts',(-24.3229930439467,19.6921685632684,-17.0060478148242));
#58356=CARTESIAN_POINT('Ctrl Pts',(-24.2086520608296,19.6727534588337,-17.0001963096819));
#58357=CARTESIAN_POINT('Ctrl Pts',(-24.0942731075614,19.6533319070655,-16.9943428613822));
#58358=CARTESIAN_POINT('Ctrl Pts',(-23.9790805379398,19.6389834581653,-16.9884894130824));
#58359=CARTESIAN_POINT('Ctrl Pts',(-23.8635599875814,19.6297516149636,-16.9826359647826));
#58360=CARTESIAN_POINT('Ctrl Pts',(-23.7479080652722,19.6205092731515,-16.9767758598411));
#58361=CARTESIAN_POINT('Ctrl Pts',(-23.6319278300723,19.6163951839207,-16.9709157548996));
#58362=CARTESIAN_POINT('Ctrl Pts',(-23.5161069519088,19.6174007572968,-16.965055649958));
#58363=CARTESIAN_POINT('Ctrl Pts',(-23.4002080756329,19.6184070078635,-16.9591915986026));
#58364=CARTESIAN_POINT('Ctrl Pts',(-23.2844691818779,19.6245397644162,-16.9533275472471));
#58365=CARTESIAN_POINT('Ctrl Pts',(-23.1693731010162,19.6357385312995,-16.9474634958917));
#58366=CARTESIAN_POINT('Ctrl Pts',(-23.0541073915066,19.6469538029297,-16.9415908020951));
#58367=CARTESIAN_POINT('Ctrl Pts',(-22.9394867934044,19.663249928192,-16.9357181082986));
#58368=CARTESIAN_POINT('Ctrl Pts',(-22.8259843184395,19.6845152727397,-16.929845414502));
#58369=CARTESIAN_POINT('Ctrl Pts',(-22.7949092394588,19.6903373683511,-16.9282375691787));
#58370=CARTESIAN_POINT('Ctrl Pts',(-22.7639178835875,19.6965316548715,-16.9266297238553));
#58371=CARTESIAN_POINT('Ctrl Pts',(-22.7330197412293,19.7030951959216,-16.925021878532));
#58372=CARTESIAN_POINT('Ctrl Pts',(-22.6201711574278,19.7270670678756,-16.9191495815633));
#58373=CARTESIAN_POINT('Ctrl Pts',(-22.5081891655635,19.7560485865944,-16.9132772845946));
#58374=CARTESIAN_POINT('Ctrl Pts',(-22.3975528089986,19.789963666554,-16.9074049876259));
#58375=CARTESIAN_POINT('Ctrl Pts',(-22.2870598283654,19.8238347952634,-16.9015403006877));
#58376=CARTESIAN_POINT('Ctrl Pts',(-22.1779094067485,19.8626266507924,-16.8956756137495));
#58377=CARTESIAN_POINT('Ctrl Pts',(-22.0705706966308,19.9062121001151,-16.8898109268113));
#58378=CARTESIAN_POINT('Ctrl Pts',(-21.9633423776573,19.9497527245315,-16.8839522713365));
#58379=CARTESIAN_POINT('Ctrl Pts',(-21.8579224448277,19.9980769823059,-16.8780936158617));
#58380=CARTESIAN_POINT('Ctrl Pts',(-21.7547645236691,20.0510080685224,-16.8722349603868));
#58381=CARTESIAN_POINT('Ctrl Pts',(-21.6475771632496,20.1060066895878,-16.8661474606689));
#58382=CARTESIAN_POINT('Ctrl Pts',(-21.5428325640239,20.1659792362117,-16.860059960951));
#58383=CARTESIAN_POINT('Ctrl Pts',(-21.4410166715523,20.2306722741479,-16.8539724612331));
#58384=CARTESIAN_POINT('Ctrl Pts',(-21.3431417799254,20.2928612303443,-16.8481205911497));
#58385=CARTESIAN_POINT('Ctrl Pts',(-21.2479734685871,20.3594117970913,-16.8422687210663));
#58386=CARTESIAN_POINT('Ctrl Pts',(-21.1559172282474,20.4300526254914,-16.8364168509829));
#58387=CARTESIAN_POINT('Ctrl Pts',(-21.0638750043073,20.500682698183,-16.8305658719));
#58388=CARTESIAN_POINT('Ctrl Pts',(-20.9749442370804,20.5754015426521,-16.824714892817));
#58389=CARTESIAN_POINT('Ctrl Pts',(-20.889499286008,20.6538959988119,-16.818863913734));
#58390=CARTESIAN_POINT('Ctrl Pts',(-20.8040466526123,20.7323975123785,-16.8130124085918));
#58391=CARTESIAN_POINT('Ctrl Pts',(-20.7220807628415,20.8146750327801,-16.8071609034495));
#58392=CARTESIAN_POINT('Ctrl Pts',(-20.6439403610962,20.9003773333058,-16.8013093983072));
#58393=CARTESIAN_POINT('Ctrl Pts',(-20.5657740106245,20.9861080936998,-16.7954559500074));
#58394=CARTESIAN_POINT('Ctrl Pts',(-20.4914359525828,21.0752655903474,-16.7896025017077));
#58395=CARTESIAN_POINT('Ctrl Pts',(-20.4212252932704,21.1674647649802,-16.7837490534079));
#58396=CARTESIAN_POINT('Ctrl Pts',(-20.3509347891924,21.2597687900952,-16.7778889484664));
#58397=CARTESIAN_POINT('Ctrl Pts',(-20.2847813030186,21.355121068276,-16.7720288435248));
#58398=CARTESIAN_POINT('Ctrl Pts',(-20.2230212141286,21.4531066713853,-16.7661687385833));
#58399=CARTESIAN_POINT('Ctrl Pts',(-20.1612195336844,21.5511582616652,-16.7603046872278));
#58400=CARTESIAN_POINT('Ctrl Pts',(-20.1038173460744,21.6518463497796,-16.7544406358724));
#58401=CARTESIAN_POINT('Ctrl Pts',(-20.0510247455741,21.7547320219687,-16.748576584517));
#58402=CARTESIAN_POINT('Ctrl Pts',(-19.9981543393189,21.8577693271009,-16.7427038907204));
#58403=CARTESIAN_POINT('Ctrl Pts',(-19.9499072505361,21.963010305963,-16.7368311969239));
#58404=CARTESIAN_POINT('Ctrl Pts',(-19.9064452422692,22.0699966627535,-16.7309585031273));
#58405=CARTESIAN_POINT('Ctrl Pts',(-19.894546071436,22.0992877375805,-16.7293506578039));
#58406=CARTESIAN_POINT('Ctrl Pts',(-19.8830052869491,22.1287095597155,-16.7277428124805));
#58407=CARTESIAN_POINT('Ctrl Pts',(-19.871825548349,22.158252557485,-16.7261349671571));
#58408=CARTESIAN_POINT('Ctrl Pts',(-19.8309940428943,22.2661517774694,-16.7202626701884));
#58409=CARTESIAN_POINT('Ctrl Pts',(-19.7948456669953,22.3760298455675,-16.7143903732197));
#58410=CARTESIAN_POINT('Ctrl Pts',(-19.7635753518695,22.4874426071099,-16.708518076251));
#58411=CARTESIAN_POINT('Ctrl Pts',(-19.7323455605886,22.5987109865619,-16.7026533893128));
#58412=CARTESIAN_POINT('Ctrl Pts',(-19.7059813694057,22.7115097100381,-16.6967887023746));
#58413=CARTESIAN_POINT('Ctrl Pts',(-19.6846294159788,22.8253753508929,-16.6909240154364));
#58414=CARTESIAN_POINT('Ctrl Pts',(-19.6632994216993,22.9391238880638,-16.6850653599616));
#58415=CARTESIAN_POINT('Ctrl Pts',(-19.6469714877987,23.0539367562528,-16.6792067044868));
#58416=CARTESIAN_POINT('Ctrl Pts',(-19.6357420691627,23.1693367421408,-16.6733480490119));
#58417=CARTESIAN_POINT('Ctrl Pts',(-19.6240740195439,23.2892443531206,-16.667260549294));
#58418=CARTESIAN_POINT('Ctrl Pts',(-19.6179110329326,23.409785445747,-16.6611730495761));
#58419=CARTESIAN_POINT('Ctrl Pts',(-19.6173025650211,23.5304141939125,-16.6550855498582));
#58420=CARTESIAN_POINT('Ctrl Pts',(-19.6167176491553,23.6463737496085,-16.6492336797748));
#58421=CARTESIAN_POINT('Ctrl Pts',(-19.621265250812,23.7624138493004,-16.6433818096914));
#58422=CARTESIAN_POINT('Ctrl Pts',(-19.6309362645296,23.8780466712681,-16.637529939608));
#58423=CARTESIAN_POINT('Ctrl Pts',(-19.6406058057474,23.9936618870872,-16.6316789605251));
#58424=CARTESIAN_POINT('Ctrl Pts',(-19.6553971735216,24.1088695366498,-16.6258279814421));
#58425=CARTESIAN_POINT('Ctrl Pts',(-19.675249258165,24.2231853887741,-16.6199770023591));
#58426=CARTESIAN_POINT('Ctrl Pts',(-19.6951031277018,24.3375115189934,-16.6141254972168));
#58427=CARTESIAN_POINT('Ctrl Pts',(-19.7200185478864,24.4509452850703,-16.6082739920746));
#58428=CARTESIAN_POINT('Ctrl Pts',(-19.7498831315029,24.56301184273,-16.6024224869323));
#58429=CARTESIAN_POINT('Ctrl Pts',(-19.7797576324976,24.6751156152542,-16.5965690386325));
#58430=CARTESIAN_POINT('Ctrl Pts',(-19.8145844585482,24.7858508773396,-16.5907155903327));
#58431=CARTESIAN_POINT('Ctrl Pts',(-19.8542013333078,24.8947578455203,-16.584862142033));
#58432=CARTESIAN_POINT('Ctrl Pts',(-19.8938632610568,25.0037886645727,-16.5790020370914));
#58433=CARTESIAN_POINT('Ctrl Pts',(-19.9383259688121,25.110986651057,-16.5731419321499));
#58434=CARTESIAN_POINT('Ctrl Pts',(-19.9873789544936,25.2159118224514,-16.5672818272084));
#58435=CARTESIAN_POINT('Ctrl Pts',(-20.0364649742909,25.3209076543818,-16.5614177758529));
#58436=CARTESIAN_POINT('Ctrl Pts',(-20.0901472363368,25.4236272580234,-16.5555537244974));
#58437=CARTESIAN_POINT('Ctrl Pts',(-20.1481700399834,25.5236566260435,-16.549689673142));
#58438=CARTESIAN_POINT('Ctrl Pts',(-20.20627835766,25.6238334173842,-16.5438169793454));
#58439=CARTESIAN_POINT('Ctrl Pts',(-20.2687397621095,25.7213117132355,-16.5379442855488));
#58440=CARTESIAN_POINT('Ctrl Pts',(-20.3352561211675,25.8157076913255,-16.5320715917523));
#58441=CARTESIAN_POINT('Ctrl Pts',(-20.3534671875948,25.8415517310749,-16.5304637464289));
#58442=CARTESIAN_POINT('Ctrl Pts',(-20.3719819769394,25.8671649288407,-16.5288559011056));
#58443=CARTESIAN_POINT('Ctrl Pts',(-20.3907938739861,25.8925398732117,-16.5272480557822));
#58444=CARTESIAN_POINT('Ctrl Pts',(-20.4595001384502,25.9852162064063,-16.5213757588135));
#58445=CARTESIAN_POINT('Ctrl Pts',(-20.5324026710907,26.0750221954256,-16.5155034618448));
#58446=CARTESIAN_POINT('Ctrl Pts',(-20.6092331657192,26.161553756938,-16.5096311648761));
#58447=CARTESIAN_POINT('Ctrl Pts',(-20.6859640941281,26.2479731804187,-16.5037664779379));
#58448=CARTESIAN_POINT('Ctrl Pts',(-20.7666125897615,26.3311263087217,-16.4979017909997));
#58449=CARTESIAN_POINT('Ctrl Pts',(-20.8508680278774,26.4106392713771,-16.4920371040615));
#58450=CARTESIAN_POINT('Ctrl Pts',(-20.9350368145494,26.4900704599277,-16.4861784485867));
#58451=CARTESIAN_POINT('Ctrl Pts',(-21.0228048664517,26.5658686471914,-16.4803197931119));
#58452=CARTESIAN_POINT('Ctrl Pts',(-21.1138228339669,26.6376947300248,-16.4744611376371));
#58453=CARTESIAN_POINT('Ctrl Pts',(-21.2083960434611,26.7123264029175,-16.4683736379192));
#58454=CARTESIAN_POINT('Ctrl Pts',(-21.3064779316249,26.782668997622,-16.4622861382013));
#58455=CARTESIAN_POINT('Ctrl Pts',(-21.4076360186946,26.8483858640841,-16.4561986384834));
#58456=CARTESIAN_POINT('Ctrl Pts',(-21.504878566678,26.9115590193441,-16.4503467684));
#58457=CARTESIAN_POINT('Ctrl Pts',(-21.6049632209802,26.9704576389421,-16.4444948983166));
#58458=CARTESIAN_POINT('Ctrl Pts',(-21.7074746471155,27.0248256951357,-16.4386430282332));
#58459=CARTESIAN_POINT('Ctrl Pts',(-21.8099704649541,27.0791854732984,-16.4327920491502));
#58460=CARTESIAN_POINT('Ctrl Pts',(-21.9148919548463,27.1290158660044,-16.4269410700672));
#58461=CARTESIAN_POINT('Ctrl Pts',(-22.0217986925976,27.174106538377,-16.4210900909842));
#58462=CARTESIAN_POINT('Ctrl Pts',(-22.1287150422937,27.219201264835,-16.4152385858419));
#58463=CARTESIAN_POINT('Ctrl Pts',(-22.237616613764,27.25955526316,-16.4093870806996));
#58464=CARTESIAN_POINT('Ctrl Pts',(-22.3480431624985,27.295006413142,-16.4035355755573));
#58465=CARTESIAN_POINT('Ctrl Pts',(-22.4585063814865,27.3304693356792,-16.3976821272575));
#58466=CARTESIAN_POINT('Ctrl Pts',(-22.5704951913178,27.361026046148,-16.3918286789577));
#58467=CARTESIAN_POINT('Ctrl Pts',(-22.6835350512033,27.3865645379069,-16.3859752306578));
#58468=CARTESIAN_POINT('Ctrl Pts',(-22.796703461955,27.4121320724763,-16.3801151257163));
#58469=CARTESIAN_POINT('Ctrl Pts',(-22.9109249050284,27.4326699065753,-16.3742550207747));
#58470=CARTESIAN_POINT('Ctrl Pts',(-23.0257154304476,27.4481173099306,-16.3683949158332));
#58471=CARTESIAN_POINT('Ctrl Pts',(-23.1405832601013,27.4635751161453,-16.3625308644777));
#58472=CARTESIAN_POINT('Ctrl Pts',(-23.2560205244885,27.473935628753,-16.3566668131223));
#58473=CARTESIAN_POINT('Ctrl Pts',(-23.3715406952535,27.4791901844848,-16.3508027617668));
#58474=CARTESIAN_POINT('Ctrl Pts',(-23.4872311196903,27.4844524843829,-16.3449300679702));
#58475=CARTESIAN_POINT('Ctrl Pts',(-23.6030042825371,27.4845938081323,-16.3390573741736));
#58476=CARTESIAN_POINT('Ctrl Pts',(-23.718376114603,27.479657507116,-16.333184680377));
#58477=CARTESIAN_POINT('Ctrl Pts',(-23.7499629922859,27.4783060304721,-16.3315768350538));
#58478=CARTESIAN_POINT('Ctrl Pts',(-23.7815198338473,27.4765742467638,-16.3299689897305));
#58479=CARTESIAN_POINT('Ctrl Pts',(-23.8130368281386,27.4744637153007,-16.3283611444073));
#58480=CARTESIAN_POINT('Ctrl Pts',(-23.9281456308094,27.4667554691566,-16.3224888474386));
#58481=CARTESIAN_POINT('Ctrl Pts',(-24.0431078256081,27.4539652894805,-16.3166165504699));
#58482=CARTESIAN_POINT('Ctrl Pts',(-24.1574384195787,27.4361004825994,-16.3107442535012));
#58483=CARTESIAN_POINT('Ctrl Pts',(-24.271620850179,27.4182588270892,-16.304879566563));
#58484=CARTESIAN_POINT('Ctrl Pts',(-24.385172903006,27.3953556855317,-16.2990148796249));
#58485=CARTESIAN_POINT('Ctrl Pts',(-24.4976121287189,27.3674502988953,-16.2931501926867));
#58486=CARTESIAN_POINT('Ctrl Pts',(-24.6099357177269,27.3395736112022,-16.2872915372119));
#58487=CARTESIAN_POINT('Ctrl Pts',(-24.7211483572374,27.3067050100721,-16.2814328817371));
#58488=CARTESIAN_POINT('Ctrl Pts',(-24.8307759158083,27.268955109575,-16.2755742262623));
#58489=CARTESIAN_POINT('Ctrl Pts',(-24.9446856233762,27.2297306647146,-16.2694867265444));
#58490=CARTESIAN_POINT('Ctrl Pts',(-25.0568834470654,27.1852358810322,-16.2633992268265));
#58491=CARTESIAN_POINT('Ctrl Pts',(-25.1668523838908,27.1356526373837,-16.2573117271086));
#58492=CARTESIAN_POINT('Ctrl Pts',(-25.2725647389349,27.0879886187241,-16.2514598570252));
#58493=CARTESIAN_POINT('Ctrl Pts',(-25.376217134358,27.0356229205971,-16.2456079869418));
#58494=CARTESIAN_POINT('Ctrl Pts',(-25.4773696638282,26.9787665770257,-16.2397561168584));
#58495=CARTESIAN_POINT('Ctrl Pts',(-25.5785067919058,26.9219188903498,-16.2339051377754));
#58496=CARTESIAN_POINT('Ctrl Pts',(-25.67714445058,26.8605821202231,-16.2280541586925));
#58497=CARTESIAN_POINT('Ctrl Pts',(-25.772867613642,26.7950131079923,-16.2222031796095));
#58498=CARTESIAN_POINT('Ctrl Pts',(-25.8685993831377,26.7294382004762,-16.2163516744672));
#58499=CARTESIAN_POINT('Ctrl Pts',(-25.9614157950425,26.6596305280433,-16.210500169325));
#58500=CARTESIAN_POINT('Ctrl Pts',(-26.0509316732348,26.5858896692757,-16.2046486641827));
#58501=CARTESIAN_POINT('Ctrl Pts',(-26.1404772777018,26.5121243227739,-16.1987952158829));
#58502=CARTESIAN_POINT('Ctrl Pts',(-26.2267198501632,26.4344234554869,-16.1929417675831));
#58503=CARTESIAN_POINT('Ctrl Pts',(-26.3093086481386,26.3531257622044,-16.1870883192833));
#58504=CARTESIAN_POINT('Ctrl Pts',(-26.3919913675111,26.2717356157911,-16.1812282143418));
#58505=CARTESIAN_POINT('Ctrl Pts',(-26.4710117240994,26.1867407692892,-16.1753681094003));
#58506=CARTESIAN_POINT('Ctrl Pts',(-26.5460570290276,26.0985155506459,-16.1695080044587));
#58507=CARTESIAN_POINT('Ctrl Pts',(-26.6211528722716,26.0102309178398,-16.1636439531033));
#58508=CARTESIAN_POINT('Ctrl Pts',(-26.692268080494,25.9187119067542,-16.1577799017478));
#58509=CARTESIAN_POINT('Ctrl Pts',(-26.7591323759396,25.8243631589935,-16.1519158503924));
#58510=CARTESIAN_POINT('Ctrl Pts',(-26.8260952160093,25.7298753600124,-16.1460431565958));
#58511=CARTESIAN_POINT('Ctrl Pts',(-26.8887944165423,25.6325498471169,-16.1401704627993));
#58512=CARTESIAN_POINT('Ctrl Pts',(-26.9470047898657,25.5328173090992,-16.1342977690027));
#58513=CARTESIAN_POINT('Ctrl Pts',(-26.9629418163417,25.5055122085104,-16.1326899236793));
#58514=CARTESIAN_POINT('Ctrl Pts',(-26.9785426483065,25.4780268057239,-16.1310820783559));
#58515=CARTESIAN_POINT('Ctrl Pts',(-26.9938032942917,25.4503701978966,-16.1294742330325));
#58516=CARTESIAN_POINT('Ctrl Pts',(-27.0522995010747,25.3443585223778,-16.1233111353102));
#58517=CARTESIAN_POINT('Ctrl Pts',(-27.1059736427251,25.23550369087,-16.1171480375878));
#58518=CARTESIAN_POINT('Ctrl Pts',(-27.154553849024,25.1242604776381,-16.1109849398655));
#58519=CARTESIAN_POINT('Ctrl Pts',(-27.2030468990792,25.0132168424102,-16.1048328991659));
#58520=CARTESIAN_POINT('Ctrl Pts',(-27.2464640757081,24.8997936829022,-16.0986808584663));
#58521=CARTESIAN_POINT('Ctrl Pts',(-27.2845789882971,24.7844708736078,-16.0925288177667));
#58522=CARTESIAN_POINT('Ctrl Pts',(-27.3226063178148,24.6694130610072,-16.08639091365));
#58523=CARTESIAN_POINT('Ctrl Pts',(-27.3553555609326,24.552464635243,-16.0802530095332));
#58524=CARTESIAN_POINT('Ctrl Pts',(-27.3826484412697,24.4341250294386,-16.0741151054165));
#58525=CARTESIAN_POINT('Ctrl Pts',(-27.4099034846243,24.3159494815696,-16.0679857104702));
#58526=CARTESIAN_POINT('Ctrl Pts',(-27.4317171487945,24.1963869374792,-16.0618563155239));
#58527=CARTESIAN_POINT('Ctrl Pts',(-27.4479606124416,24.0759527478596,-16.0557269205776));
#58528=CARTESIAN_POINT('Ctrl Pts',(-27.4641760744772,23.955726171066,-16.0496080919083));
#58529=CARTESIAN_POINT('Ctrl Pts',(-27.4748404285476,23.8346312936653,-16.043489263239));
#58530=CARTESIAN_POINT('Ctrl Pts',(-27.4798758177641,23.7131937161043,-16.0373704345697));
#58531=CARTESIAN_POINT('Ctrl Pts',(-27.4821270655716,23.6589007769734,-16.034634797058));
#58532=CARTESIAN_POINT('Ctrl Pts',(-27.4832538466711,23.6045394782566,-16.0318991595464));
#58533=CARTESIAN_POINT('Ctrl Pts',(-27.4832525305424,23.5501573472289,-16.0291635220348));
#58534=CARTESIAN_POINT('',(-27.4832509111211,23.5466821780573,-14.7791635220348));
#58535=CARTESIAN_POINT('Ctrl Pts',(-27.4832525305424,23.5501573464781,-16.029163521997));
#58536=CARTESIAN_POINT('Ctrl Pts',(-27.4832495762865,23.4280891425663,-16.023023005778));
#58537=CARTESIAN_POINT('Ctrl Pts',(-27.4775593913889,23.3061351717897,-16.016882489559));
#58538=CARTESIAN_POINT('Ctrl Pts',(-27.4662395404907,23.1848284671646,-16.0107419733401));
#58539=CARTESIAN_POINT('Ctrl Pts',(-27.4549031186718,23.0633441838946,-16.0045924681328));
#58540=CARTESIAN_POINT('Ctrl Pts',(-27.4379206219041,22.9425094045615,-15.9984429629255));
#58541=CARTESIAN_POINT('Ctrl Pts',(-27.4154009443107,22.8228484153681,-15.9922934577182));
#58542=CARTESIAN_POINT('Ctrl Pts',(-27.3928252781756,22.70288992439,-15.9861286635785));
#58543=CARTESIAN_POINT('Ctrl Pts',(-27.3646849766341,22.5841114015368,-15.9799638694388));
#58544=CARTESIAN_POINT('Ctrl Pts',(-27.3311395629083,22.467024828394,-15.9737990752992));
#58545=CARTESIAN_POINT('Ctrl Pts',(-27.2975481124793,22.3497775692078,-15.9676258207839));
#58546=CARTESIAN_POINT('Ctrl Pts',(-27.2585368602675,22.2342272233437,-15.9614525662687));
#58547=CARTESIAN_POINT('Ctrl Pts',(-27.2143138399266,22.1208667441917,-15.9552793117535));
#58548=CARTESIAN_POINT('Ctrl Pts',(-27.1699909375302,22.0072502292108,-15.9490921143338));
#58549=CARTESIAN_POINT('Ctrl Pts',(-27.1204328800064,21.89583378649,-15.9429049169141));
#58550=CARTESIAN_POINT('Ctrl Pts',(-27.0658946150256,21.7870878366333,-15.9367177194943));
#58551=CARTESIAN_POINT('Ctrl Pts',(-27.0478820837194,21.7511719557942,-15.9346742535487));
#58552=CARTESIAN_POINT('Ctrl Pts',(-27.0293266648687,21.7155471448263,-15.9326307876031));
#58553=CARTESIAN_POINT('Ctrl Pts',(-27.010238574576,21.6802296486622,-15.9305873216575));
#58554=CARTESIAN_POINT('Ctrl Pts',(-26.9553852333662,21.5787379521096,-15.9247150246888));
#58555=CARTESIAN_POINT('Ctrl Pts',(-26.8959706312279,21.4794917935849,-15.9188427277201));
#58556=CARTESIAN_POINT('Ctrl Pts',(-26.8322029900957,21.3829292543315,-15.9129704307514));
#58557=CARTESIAN_POINT('Ctrl Pts',(-26.7685179867621,21.2864918524602,-15.9071057438132));
#58558=CARTESIAN_POINT('Ctrl Pts',(-26.7004913884387,21.1927314956184,-15.901241056875));
#58559=CARTESIAN_POINT('Ctrl Pts',(-26.6283775962247,21.1020623660598,-15.8953763699368));
#58560=CARTESIAN_POINT('Ctrl Pts',(-26.5563379685318,21.0114864840251,-15.8895177144619));
#58561=CARTESIAN_POINT('Ctrl Pts',(-26.480219763546,20.923995827398,-15.8836590589871));
#58562=CARTESIAN_POINT('Ctrl Pts',(-26.4003206508387,20.8399756609232,-15.8778004035123));
#58563=CARTESIAN_POINT('Ctrl Pts',(-26.3173006084149,20.7526735927419,-15.8717129037944));
#58564=CARTESIAN_POINT('Ctrl Pts',(-26.2301985161906,20.6691190420241,-15.8656254040765));
#58565=CARTESIAN_POINT('Ctrl Pts',(-26.1393946801444,20.5897066470441,-15.8595379043586));
#58566=CARTESIAN_POINT('Ctrl Pts',(-26.0521055998583,20.5133680778498,-15.8536860342752));
#58567=CARTESIAN_POINT('Ctrl Pts',(-25.9613963551964,20.4408572624481,-15.8478341641918));
#58568=CARTESIAN_POINT('Ctrl Pts',(-25.8676417262599,20.3724865993275,-15.8419822941084));
#58569=CARTESIAN_POINT('Ctrl Pts',(-25.7739013723181,20.3041263462621,-15.8361313150254));
#58570=CARTESIAN_POINT('Ctrl Pts',(-25.6771168899722,20.2399052355939,-15.8302803359425));
#58571=CARTESIAN_POINT('Ctrl Pts',(-25.5776943818048,20.1800939976754,-15.8244293568595));
#58572=CARTESIAN_POINT('Ctrl Pts',(-25.4782629345972,20.120277382151,-15.8185778517172));
#58573=CARTESIAN_POINT('Ctrl Pts',(-25.3761933443143,20.0648716406712,-15.8127263465749));
#58574=CARTESIAN_POINT('Ctrl Pts',(-25.2719181780131,20.0141025911112,-15.8068748414326));
#58575=CARTESIAN_POINT('Ctrl Pts',(-25.1676083841988,19.9633166822549,-15.8010213931328));
#58576=CARTESIAN_POINT('Ctrl Pts',(-25.0610919294624,19.9171707078654,-15.795167944833));
#58577=CARTESIAN_POINT('Ctrl Pts',(-24.9528226468318,19.8758429094388,-15.7893144965333));
#58578=CARTESIAN_POINT('Ctrl Pts',(-24.8444302385168,19.8344681123314,-15.7834543915917));
#58579=CARTESIAN_POINT('Ctrl Pts',(-24.7342814100818,19.7979225752351,-15.7775942866502));
#58580=CARTESIAN_POINT('Ctrl Pts',(-24.6228465880132,19.7663351184373,-15.7717341817086));
#58581=CARTESIAN_POINT('Ctrl Pts',(-24.5113367215664,19.7347263894643,-15.7658701303532));
#58582=CARTESIAN_POINT('Ctrl Pts',(-24.3985395383644,19.7080824841138,-15.7600060789977));
#58583=CARTESIAN_POINT('Ctrl Pts',(-24.2849354089757,19.6864810490843,-15.7541420276423));
#58584=CARTESIAN_POINT('Ctrl Pts',(-24.1711638497779,19.6648477778517,-15.7482693338457));
#58585=CARTESIAN_POINT('Ctrl Pts',(-24.0565833784125,19.6482718679334,-15.7423966400491));
#58586=CARTESIAN_POINT('Ctrl Pts',(-23.9416793155779,19.6367791290941,-15.7365239462526));
#58587=CARTESIAN_POINT('Ctrl Pts',(-23.9102205052853,19.6336326094501,-15.7349161009293));
#58588=CARTESIAN_POINT('Ctrl Pts',(-23.8787374356743,19.6308668090165,-15.733308255606));
#58589=CARTESIAN_POINT('Ctrl Pts',(-23.8472400398909,19.6284815771413,-15.7317004102828));
#58590=CARTESIAN_POINT('Ctrl Pts',(-23.7322028164066,19.6197700489188,-15.7258281133141));
#58591=CARTESIAN_POINT('Ctrl Pts',(-23.6165892468438,19.6161097945448,-15.7199558163454));
#58592=CARTESIAN_POINT('Ctrl Pts',(-23.5008804490858,19.6175624348955,-15.7140835193766));
#58593=CARTESIAN_POINT('Ctrl Pts',(-23.3853216007404,19.6190131927396,-15.7082188324384));
#58594=CARTESIAN_POINT('Ctrl Pts',(-23.2696681791491,19.6255636636195,-15.7023541455002));
#58595=CARTESIAN_POINT('Ctrl Pts',(-23.1544061573703,19.6372236986884,-15.696489458562));
#58596=CARTESIAN_POINT('Ctrl Pts',(-23.0392626753654,19.6488717421412,-15.6906308030872));
#58597=CARTESIAN_POINT('Ctrl Pts',(-22.9245102013308,19.6656188562266,-15.6847721476124));
#58598=CARTESIAN_POINT('Ctrl Pts',(-22.8106337679824,19.6874228584669,-15.6789134921376));
#58599=CARTESIAN_POINT('Ctrl Pts',(-22.6923092208463,19.7100785442394,-15.6728259924197));
#58600=CARTESIAN_POINT('Ctrl Pts',(-22.5749310020614,19.7381942190563,-15.6667384927018));
#58601=CARTESIAN_POINT('Ctrl Pts',(-22.459036698933,19.7716632438341,-15.6606509929839));
#58602=CARTESIAN_POINT('Ctrl Pts',(-22.3476283315013,19.8038367787653,-15.6547991229005));
#58603=CARTESIAN_POINT('Ctrl Pts',(-22.237591573722,19.8409568185651,-15.6489472528171));
#58604=CARTESIAN_POINT('Ctrl Pts',(-22.1293918362178,19.8828769190728,-15.6430953827337));
#58605=CARTESIAN_POINT('Ctrl Pts',(-22.0212085731075,19.924790636864,-15.6372444036507));
#58606=CARTESIAN_POINT('Ctrl Pts',(-21.9148621594914,19.9715028128932,-15.6313934245677));
#58607=CARTESIAN_POINT('Ctrl Pts',(-21.8107998810192,20.0228181274763,-15.6255424454848));
#58608=CARTESIAN_POINT('Ctrl Pts',(-21.7067282463467,20.0741380558001,-15.6196909403425));
#58609=CARTESIAN_POINT('Ctrl Pts',(-21.6049415258437,20.1300617625678,-15.6138394352002));
#58610=CARTESIAN_POINT('Ctrl Pts',(-21.5058635247093,20.1903473859915,-15.6079879300579));
#58611=CARTESIAN_POINT('Ctrl Pts',(-21.4067526219276,20.2506530289584,-15.6021344817581));
#58612=CARTESIAN_POINT('Ctrl Pts',(-21.3103525800872,20.3153232540631,-15.5962810334583));
#58613=CARTESIAN_POINT('Ctrl Pts',(-21.2170586727406,20.3840725910494,-15.5904275851586));
#58614=CARTESIAN_POINT('Ctrl Pts',(-21.123658669963,20.4529001109606,-15.584567480217));
#58615=CARTESIAN_POINT('Ctrl Pts',(-21.0333721851245,20.5258157563511,-15.5787073752755));
#58616=CARTESIAN_POINT('Ctrl Pts',(-20.9465618823528,20.6024933823517,-15.5728472703339));
#58617=CARTESIAN_POINT('Ctrl Pts',(-20.8596931182755,20.6792226459343,-15.5669832189785));
#58618=CARTESIAN_POINT('Ctrl Pts',(-20.7763054943334,20.7597186483438,-15.561119167623));
#58619=CARTESIAN_POINT('Ctrl Pts',(-20.6967239966534,20.8436192170933,-15.5552551162676));
#58620=CARTESIAN_POINT('Ctrl Pts',(-20.6170252117318,20.9276434385328,-15.549382422471));
#58621=CARTESIAN_POINT('Ctrl Pts',(-20.5411440184189,21.0150819295381,-15.5435097286744));
#58622=CARTESIAN_POINT('Ctrl Pts',(-20.4693644673144,21.105540332935,-15.5376370348779));
#58623=CARTESIAN_POINT('Ctrl Pts',(-20.449712426947,21.130306330601,-15.5360291895545));
#58624=CARTESIAN_POINT('Ctrl Pts',(-20.4303675788492,21.1552985329118,-15.5344213442312));
#58625=CARTESIAN_POINT('Ctrl Pts',(-20.4113351655613,21.1805085015109,-15.5328134989078));
#58626=CARTESIAN_POINT('Ctrl Pts',(-20.3418235146362,21.2725822974392,-15.5269412019391));
#58627=CARTESIAN_POINT('Ctrl Pts',(-20.2762500456629,21.3678714106469,-15.5210689049704));
#58628=CARTESIAN_POINT('Ctrl Pts',(-20.2149266659304,21.4660043772829,-15.5151966080017));
#58629=CARTESIAN_POINT('Ctrl Pts',(-20.1536827564278,21.5640101713876,-15.5093319210635));
#58630=CARTESIAN_POINT('Ctrl Pts',(-20.0966782002179,21.6648521426388,-15.5034672341253));
#58631=CARTESIAN_POINT('Ctrl Pts',(-20.0441839742809,21.7681267587147,-15.4976025471871));
#58632=CARTESIAN_POINT('Ctrl Pts',(-19.9917437353691,21.871295163313,-15.4917438917123));
#58633=CARTESIAN_POINT('Ctrl Pts',(-19.943804786518,21.9768908701874,-15.4858852362375));
#58634=CARTESIAN_POINT('Ctrl Pts',(-19.9005938196463,22.0844830117585,-15.4800265807627));
#58635=CARTESIAN_POINT('Ctrl Pts',(-19.8556949943487,22.1962777971454,-15.4739390810447));
#58636=CARTESIAN_POINT('Ctrl Pts',(-19.8159012800347,22.3102277761564,-15.4678515813268));
#58637=CARTESIAN_POINT('Ctrl Pts',(-19.7814135481827,22.4258230246267,-15.4617640816089));
#58638=CARTESIAN_POINT('Ctrl Pts',(-19.7482607374031,22.5369439129474,-15.4559122115255));
#58639=CARTESIAN_POINT('Ctrl Pts',(-19.7200109173269,22.6495846386329,-15.4500603414421));
#58640=CARTESIAN_POINT('Ctrl Pts',(-19.6967924561964,22.7632744846406,-15.4442084713588));
#58641=CARTESIAN_POINT('Ctrl Pts',(-19.6735775302877,22.8769470203355,-15.4383574922758));
#58642=CARTESIAN_POINT('Ctrl Pts',(-19.6553925228255,22.9916679538306,-15.4325065131928));
#58643=CARTESIAN_POINT('Ctrl Pts',(-19.642314884938,23.1069553976346,-15.4266555341099));
#58644=CARTESIAN_POINT('Ctrl Pts',(-19.6292360712449,23.2222532068893,-15.4208040289676));
#58645=CARTESIAN_POINT('Ctrl Pts',(-19.6212655865731,23.3381172169335,-15.4149525238253));
#58646=CARTESIAN_POINT('Ctrl Pts',(-19.6184290332188,23.4540601367925,-15.409101018683));
#58647=CARTESIAN_POINT('Ctrl Pts',(-19.6155915379069,23.5700415587711,-15.4032475703832));
#58648=CARTESIAN_POINT('Ctrl Pts',(-19.6178913740379,23.6861015296295,-15.3973941220835));
#58649=CARTESIAN_POINT('Ctrl Pts',(-19.6253020328076,23.8017531903207,-15.3915406737837));
#58650=CARTESIAN_POINT('Ctrl Pts',(-19.6327211191055,23.9175363720635,-15.3856805688421));
#58651=CARTESIAN_POINT('Ctrl Pts',(-19.6452626023982,24.0329099040543,-15.3798204639006));
#58652=CARTESIAN_POINT('Ctrl Pts',(-19.6628481268706,24.1473923757494,-15.3739603589591));
#58653=CARTESIAN_POINT('Ctrl Pts',(-19.6804454940931,24.2619519442239,-15.3680963076036));
#58654=CARTESIAN_POINT('Ctrl Pts',(-19.7030935857089,24.3756188531146,-15.3622322562482));
#58655=CARTESIAN_POINT('Ctrl Pts',(-19.7306633687071,24.4879239165574,-15.3563682048927));
#58656=CARTESIAN_POINT('Ctrl Pts',(-19.7582737840619,24.6003944952455,-15.3504955110962));
#58657=CARTESIAN_POINT('Ctrl Pts',(-19.7908202517915,24.7114988275022,-15.3446228172996));
#58658=CARTESIAN_POINT('Ctrl Pts',(-19.8281245339796,24.8207847700214,-15.338750123503));
#58659=CARTESIAN_POINT('Ctrl Pts',(-19.8383378224184,24.8507054329533,-15.3371422781797));
#58660=CARTESIAN_POINT('Ctrl Pts',(-19.8489074710648,24.8804899230745,-15.3355344328563));
#58661=CARTESIAN_POINT('Ctrl Pts',(-19.859829214403,24.9101292684588,-15.3339265875329));
#58662=CARTESIAN_POINT('Ctrl Pts',(-19.8997184496214,25.0183803766504,-15.3280542905642));
#58663=CARTESIAN_POINT('Ctrl Pts',(-19.9444415395107,25.1250562415868,-15.3221819935955));
#58664=CARTESIAN_POINT('Ctrl Pts',(-19.9938545644128,25.2296936584732,-15.3163096966268));
#58665=CARTESIAN_POINT('Ctrl Pts',(-20.0432035539589,25.3341954735775,-15.3104450096886));
#58666=CARTESIAN_POINT('Ctrl Pts',(-20.097230217098,25.4366637236095,-15.3045803227504));
#58667=CARTESIAN_POINT('Ctrl Pts',(-20.1557415298627,25.5366523047623,-15.2987156358122));
#58668=CARTESIAN_POINT('Ctrl Pts',(-20.2141926674051,25.6365380539187,-15.2928569803373));
#58669=CARTESIAN_POINT('Ctrl Pts',(-20.2771190731792,25.7339488520042,-15.2869983248625));
#58670=CARTESIAN_POINT('Ctrl Pts',(-20.3442807876536,25.8284610771116,-15.2811396693877));
#58671=CARTESIAN_POINT('Ctrl Pts',(-20.4140658978505,25.9266650329769,-15.2750521696698));
#58672=CARTESIAN_POINT('Ctrl Pts',(-20.4884237375113,26.0217389468359,-15.2689646699519));
#58673=CARTESIAN_POINT('Ctrl Pts',(-20.5670338784302,26.1132381865151,-15.262877170234));
#58674=CARTESIAN_POINT('Ctrl Pts',(-20.6426012465145,26.2011957533564,-15.2570253001506));
#58675=CARTESIAN_POINT('Ctrl Pts',(-20.7220975536018,26.2858498883814,-15.2511734300672));
#58676=CARTESIAN_POINT('Ctrl Pts',(-20.8051961660232,26.3668381507175,-15.2453215599838));
#58677=CARTESIAN_POINT('Ctrl Pts',(-20.8882821259252,26.4478140818543,-15.2394705809008));
#58678=CARTESIAN_POINT('Ctrl Pts',(-20.9749690046405,26.5251249616645,-15.2336196018178));
#58679=CARTESIAN_POINT('Ctrl Pts',(-21.0648932477556,26.5984451485969,-15.2277686227348));
#58680=CARTESIAN_POINT('Ctrl Pts',(-21.1548255759256,26.6717719277198,-15.2219171175925));
#58681=CARTESIAN_POINT('Ctrl Pts',(-21.247995526713,26.7411070394578,-15.2160656124502));
#58682=CARTESIAN_POINT('Ctrl Pts',(-21.3440069731715,26.8061655427402,-15.2102141073079));
#58683=CARTESIAN_POINT('Ctrl Pts',(-21.4400503029412,26.8712456505352,-15.2043606590081));
#58684=CARTESIAN_POINT('Ctrl Pts',(-21.5389366626332,26.9320460941914,-15.1985072107084));
#58685=CARTESIAN_POINT('Ctrl Pts',(-21.6402421204302,26.9883260080561,-15.1926537624086));
#58686=CARTESIAN_POINT('Ctrl Pts',(-21.7416627845308,27.0446699244038,-15.186793657467));
#58687=CARTESIAN_POINT('Ctrl Pts',(-21.8455076761515,27.0964828491577,-15.1809335525255));
#58688=CARTESIAN_POINT('Ctrl Pts',(-21.9513294218846,27.1435704815724,-15.1750734475839));
#58689=CARTESIAN_POINT('Ctrl Pts',(-22.0572224319403,27.1906898245604,-15.1692093962285));
#58690=CARTESIAN_POINT('Ctrl Pts',(-22.1650945631609,27.2330773880264,-15.163345344873));
#58691=CARTESIAN_POINT('Ctrl Pts',(-22.2744813337942,27.2705881147578,-15.1574812935176));
#58692=CARTESIAN_POINT('Ctrl Pts',(-22.3840293186918,27.3081541248125,-15.151608599721));
#58693=CARTESIAN_POINT('Ctrl Pts',(-22.495096003106,27.3408288370704,-15.1457359059244));
#58694=CARTESIAN_POINT('Ctrl Pts',(-22.6072046461377,27.3685178034567,-15.1398632121278));
#58695=CARTESIAN_POINT('Ctrl Pts',(-22.6378981172501,27.3760985792731,-15.1382553668046));
#58696=CARTESIAN_POINT('Ctrl Pts',(-22.6686696516916,27.3833059360911,-15.1366475214813));
#58697=CARTESIAN_POINT('Ctrl Pts',(-22.6995093955379,27.3901386128538,-15.135039676158));
#58698=CARTESIAN_POINT('Ctrl Pts',(-22.8121446917831,27.4150934430607,-15.1291673791893));
#58699=CARTESIAN_POINT('Ctrl Pts',(-22.9260676128191,27.4351299844707,-15.1232950822206));
#58700=CARTESIAN_POINT('Ctrl Pts',(-23.0408106620039,27.4501189372787,-15.1174227852519));
#58701=CARTESIAN_POINT('Ctrl Pts',(-23.1554050133099,27.4650884655942,-15.1115580983137));
#58702=CARTESIAN_POINT('Ctrl Pts',(-23.2708169730786,27.4750233605024,-15.1056934113755));
#58703=CARTESIAN_POINT('Ctrl Pts',(-23.3865668890551,27.4798448782861,-15.0998287244373));
#58704=CARTESIAN_POINT('Ctrl Pts',(-23.502197763489,27.4846614374407,-15.0939700689625));
#58705=CARTESIAN_POINT('Ctrl Pts',(-23.6181654922608,27.4843750623702,-15.0881114134877));
#58706=CARTESIAN_POINT('Ctrl Pts',(-23.7339839668532,27.4789586494554,-15.0822527580129));
#58707=CARTESIAN_POINT('Ctrl Pts',(-23.8543264130753,27.4733306666814,-15.076165258295));
#58708=CARTESIAN_POINT('Ctrl Pts',(-23.9745072565679,27.4621636494907,-15.0700777585771));
#58709=CARTESIAN_POINT('Ctrl Pts',(-24.0939792157942,27.44548683697,-15.0639902588592));
#58710=CARTESIAN_POINT('Ctrl Pts',(-24.2088267585288,27.4294555359765,-15.0581383887758));
#58711=CARTESIAN_POINT('Ctrl Pts',(-24.3230188267413,27.40833310774,-15.0522865186924));
#58712=CARTESIAN_POINT('Ctrl Pts',(-24.4360739334993,27.3821984399899,-15.0464346486091));
#58713=CARTESIAN_POINT('Ctrl Pts',(-24.5491118265893,27.3560677514806,-15.0405836695261));
#58714=CARTESIAN_POINT('Ctrl Pts',(-24.6610126997775,27.324926433942,-15.0347326904432));
#58715=CARTESIAN_POINT('Ctrl Pts',(-24.7713060687906,27.2889043287387,-15.0288817113602));
#58716=CARTESIAN_POINT('Ctrl Pts',(-24.881609354239,27.2528789848015,-15.0230302062179));
#58717=CARTESIAN_POINT('Ctrl Pts',(-24.9903044552207,27.2119721091944,-15.0171787010756));
#58718=CARTESIAN_POINT('Ctrl Pts',(-25.0969375226245,27.1663629474353,-15.0113271959334));
#58719=CARTESIAN_POINT('Ctrl Pts',(-25.2036060005487,27.1207386398664,-15.0054737476336));
#58720=CARTESIAN_POINT('Ctrl Pts',(-25.3082107034252,27.0704091036279,-14.9996202993338));
#58721=CARTESIAN_POINT('Ctrl Pts',(-25.4103198338202,27.0156008015744,-14.9937668510341));
#58722=CARTESIAN_POINT('Ctrl Pts',(-25.5125450844689,26.9607301705801,-14.9879067460925));
#58723=CARTESIAN_POINT('Ctrl Pts',(-25.6122687336126,26.9013708032601,-14.982046641151));
#58724=CARTESIAN_POINT('Ctrl Pts',(-25.7090854884818,26.8377940545784,-14.9761865362095));
#58725=CARTESIAN_POINT('Ctrl Pts',(-25.8059674433759,26.7741744909356,-14.9703224848541));
#58726=CARTESIAN_POINT('Ctrl Pts',(-25.8999382716577,26.7063321320246,-14.9644584334986));
#58727=CARTESIAN_POINT('Ctrl Pts',(-25.9906248621826,26.6345793445638,-14.9585943821432));
#58728=CARTESIAN_POINT('Ctrl Pts',(-26.081445106639,26.5627208078177,-14.9527216883466));
#58729=CARTESIAN_POINT('Ctrl Pts',(-26.1689711416627,26.4869406098711,-14.9468489945501));
#58730=CARTESIAN_POINT('Ctrl Pts',(-26.2528658078369,26.4075887876531,-14.9409763007535));
#58731=CARTESIAN_POINT('Ctrl Pts',(-26.2758347640507,26.3858635861221,-14.9393684554301));
#58732=CARTESIAN_POINT('Ctrl Pts',(-26.2985317531343,26.3638708598036,-14.9377606101066));
#58733=CARTESIAN_POINT('Ctrl Pts',(-26.3209503876758,26.3416182173146,-14.9361527647832));
#58734=CARTESIAN_POINT('Ctrl Pts',(-26.4016830745772,26.2614832913686,-14.9303626854257));
#58735=CARTESIAN_POINT('Ctrl Pts',(-26.4790900040286,26.1776901938045,-14.9245726060681));
#58736=CARTESIAN_POINT('Ctrl Pts',(-26.552814138775,26.0905503086653,-14.9187825267106));
#58737=CARTESIAN_POINT('Ctrl Pts',(-26.6268868880288,26.0029983708348,-14.9129650681824));
#58738=CARTESIAN_POINT('Ctrl Pts',(-26.697241562853,25.9120681579657,-14.9071476096542));
#58739=CARTESIAN_POINT('Ctrl Pts',(-26.7635508773111,25.8181155659305,-14.9013301511261));
#58740=CARTESIAN_POINT('Ctrl Pts',(-26.829383469992,25.7248384332484,-14.895554516423));
#58741=CARTESIAN_POINT('Ctrl Pts',(-26.8912284090564,25.6285825744804,-14.8897788817199));
#58742=CARTESIAN_POINT('Ctrl Pts',(-26.9488042042189,25.529731132028,-14.8840032470168));
#58743=CARTESIAN_POINT('Ctrl Pts',(-27.0063428259051,25.430943512433,-14.8782313413186));
#58744=CARTESIAN_POINT('Ctrl Pts',(-27.059617567142,25.3295640059362,-14.8724594356204));
#58745=CARTESIAN_POINT('Ctrl Pts',(-27.1083901535948,25.2260047996669,-14.8666875299221));
#58746=CARTESIAN_POINT('Ctrl Pts',(-27.157143839213,25.1224857256844,-14.8609178610098));
#58747=CARTESIAN_POINT('Ctrl Pts',(-27.2013986573955,25.0167890160884,-14.8551481920975));
#58748=CARTESIAN_POINT('Ctrl Pts',(-27.2409626339126,24.9093507405751,-14.8493785231852));
#58749=CARTESIAN_POINT('Ctrl Pts',(-27.2810860317898,24.8003933238754,-14.8435272730894));
#58750=CARTESIAN_POINT('Ctrl Pts',(-27.3163847168276,24.6896451152041,-14.8376760229935));
#58751=CARTESIAN_POINT('Ctrl Pts',(-27.3467096178911,24.577580421253,-14.8318247728976));
#58752=CARTESIAN_POINT('Ctrl Pts',(-27.3766216786034,24.4670413655066,-14.8260531811703));
#58753=CARTESIAN_POINT('Ctrl Pts',(-27.4016944754199,24.3552218779928,-14.820281589443));
#58754=CARTESIAN_POINT('Ctrl Pts',(-27.4218359661124,24.2425896680222,-14.8145099977156));
#58755=CARTESIAN_POINT('Ctrl Pts',(-27.4423944401166,24.1276256667932,-14.8086189184355));
#58756=CARTESIAN_POINT('Ctrl Pts',(-27.4578150786415,24.011815377055,-14.8027278391554));
#58757=CARTESIAN_POINT('Ctrl Pts',(-27.4680555937978,23.8956626742372,-14.7968367598752));
#58758=CARTESIAN_POINT('Ctrl Pts',(-27.4782961089542,23.7795099714194,-14.7909456805951));
#58759=CARTESIAN_POINT('Ctrl Pts',(-27.4833565176931,23.6630153255504,-14.7850546013149));
#58760=CARTESIAN_POINT('Ctrl Pts',(-27.4832509111211,23.5466821780573,-14.7791635220348));
#58761=CARTESIAN_POINT('',(-27.4888203141544,23.551993354051,-13.5291635220348));
#58762=CARTESIAN_POINT('Ctrl Pts',(-27.4841329879773,23.5466813773129,-14.7791635220348));
#58763=CARTESIAN_POINT('Ctrl Pts',(-27.4866979788519,23.2708277947411,-14.7651976324926));
#58764=CARTESIAN_POINT('Ctrl Pts',(-27.3342151592236,21.6883218579646,-14.6849361058252));
#58765=CARTESIAN_POINT('Ctrl Pts',(-25.1911129410817,19.1972848142637,-14.5383789420335));
#58766=CARTESIAN_POINT('Ctrl Pts',(-20.7749823681344,19.8168055518416,-14.3394920306583));
#58767=CARTESIAN_POINT('Ctrl Pts',(-18.909089771392,23.8670475198046,-14.1406051192836));
#58768=CARTESIAN_POINT('Ctrl Pts',(-21.3080322456564,27.6261817534765,-13.9417182079087));
#58769=CARTESIAN_POINT('Ctrl Pts',(-25.7673850538621,27.6398826141424,-13.7428312965338));
#58770=CARTESIAN_POINT('Ctrl Pts',(-27.4420482966652,25.0509108913852,-13.6053130679092));
#58771=CARTESIAN_POINT('Ctrl Pts',(-27.4893561445465,23.6490092491261,-13.5340904764095));
#58772=CARTESIAN_POINT('Ctrl Pts',(-27.4888203141544,23.551993354051,-13.5291635220348));
#58773=CARTESIAN_POINT('',(-27.4787742047217,23.5529763597193,-12.2791635220348));
#58774=CARTESIAN_POINT('Ctrl Pts',(-27.4888203141544,23.551993354051,-13.5291635220348));
#58775=CARTESIAN_POINT('Ctrl Pts',(-27.4821461696749,22.3435921321586,-13.4677948392845));
#58776=CARTESIAN_POINT('Ctrl Pts',(-26.2391084225207,19.817910182807,-13.3401305194094));
#58777=CARTESIAN_POINT('Ctrl Pts',(-21.9361708563877,19.1872843702759,-13.1461705624091));
#58778=CARTESIAN_POINT('Ctrl Pts',(-19.0071346432534,22.5498372759953,-12.9472836510342));
#58779=CARTESIAN_POINT('Ctrl Pts',(-20.2528385767197,26.8316869804742,-12.7483967396594));
#58780=CARTESIAN_POINT('Ctrl Pts',(-24.5285863602099,28.0981766462875,-12.5495098282844));
#58781=CARTESIAN_POINT('Ctrl Pts',(-27.1841649778446,25.8075615147313,-12.3930987557429));
#58782=CARTESIAN_POINT('Ctrl Pts',(-27.4817723373124,24.0250936006054,-12.3029833203264));
#58783=CARTESIAN_POINT('Ctrl Pts',(-27.4787742047217,23.5529763597193,-12.2791635220348));
#58784=CARTESIAN_POINT('',(-27.4823549449185,23.5474739030226,-11.0291634828679));
#58785=CARTESIAN_POINT('Ctrl Pts',(-27.4787742047217,23.5529763597193,-12.2791635220348));
#58786=CARTESIAN_POINT('Ctrl Pts',(-27.4734278875462,22.71108947265,-12.2366876832014));
#58787=CARTESIAN_POINT('Ctrl Pts',(-26.7947582611164,20.547334820768,-12.127916207243));
#58788=CARTESIAN_POINT('Ctrl Pts',(-23.2274849901484,18.9095013051977,-11.9528490941598));
#58789=CARTESIAN_POINT('Ctrl Pts',(-19.4714411218787,21.3132795065398,-11.7539621827848));
#58790=CARTESIAN_POINT('Ctrl Pts',(-19.4634791130517,25.7726462539626,-11.55507527141));
#58791=CARTESIAN_POINT('Ctrl Pts',(-23.2109153747127,28.1898215985376,-11.356188360035));
#58792=CARTESIAN_POINT('Ctrl Pts',(-26.7888475756172,26.5625387526775,-11.1808844435768));
#58793=CARTESIAN_POINT('Ctrl Pts',(-27.4733876852228,24.3940033727517,-11.0718761642433));
#58794=CARTESIAN_POINT('Ctrl Pts',(-27.4788743631229,23.5474771390092,-11.0291635220348));
#58795=CARTESIAN_POINT('',(-27.4847851822191,23.5485896828163,-9.7791635220348));
#58796=CARTESIAN_POINT('Ctrl Pts',(-27.4832515495671,23.5474730694262,-11.0291634727785));
#58797=CARTESIAN_POINT('Ctrl Pts',(-27.4831577687811,23.4147712357825,-11.0224752375737));
#58798=CARTESIAN_POINT('Ctrl Pts',(-27.4763438388193,23.2823366808379,-11.015787002369));
#58799=CARTESIAN_POINT('Ctrl Pts',(-27.4629146449167,23.1507976684699,-11.0090987671643));
#58800=CARTESIAN_POINT('Ctrl Pts',(-27.4494191222458,23.0186089655308,-11.0023774977801));
#58801=CARTESIAN_POINT('Ctrl Pts',(-27.4292429435521,22.8873248327967,-10.9956562283959));
#58802=CARTESIAN_POINT('Ctrl Pts',(-27.4025420174753,22.7575642463385,-10.9889349590116));
#58803=CARTESIAN_POINT('Ctrl Pts',(-27.375678109144,22.6270116022238,-10.982172663049));
#58804=CARTESIAN_POINT('Ctrl Pts',(-27.3422096534684,22.4980013167981,-10.9754103670863));
#58805=CARTESIAN_POINT('Ctrl Pts',(-27.3023437719518,22.3711425602402,-10.9686480711237));
#58806=CARTESIAN_POINT('Ctrl Pts',(-27.2822337950174,22.3071498283289,-10.9652368931776));
#58807=CARTESIAN_POINT('Ctrl Pts',(-27.2604966784544,22.2437042265049,-10.9618257152314));
#58808=CARTESIAN_POINT('Ctrl Pts',(-27.2371635166089,22.1808817311746,-10.9584145372853));
#58809=CARTESIAN_POINT('Ctrl Pts',(-27.1969957922217,22.072733650154,-10.9525422403166));
#58810=CARTESIAN_POINT('Ctrl Pts',(-27.151998283603,21.966173248751,-10.9466699433479));
#58811=CARTESIAN_POINT('Ctrl Pts',(-27.1023161021502,21.8616633597997,-10.9407976463792));
#58812=CARTESIAN_POINT('Ctrl Pts',(-27.052698304859,21.7572889073645,-10.934932959441));
#58813=CARTESIAN_POINT('Ctrl Pts',(-26.9984080835449,21.6549600528605,-10.9290682725029));
#58814=CARTESIAN_POINT('Ctrl Pts',(-26.9396396097369,21.5551224018036,-10.9232035855647));
#58815=CARTESIAN_POINT('Ctrl Pts',(-26.8809315756252,21.4553874275208,-10.9173449300899));
#58816=CARTESIAN_POINT('Ctrl Pts',(-26.8177546582395,21.3581389147464,-10.9114862746151));
#58817=CARTESIAN_POINT('Ctrl Pts',(-26.7503499066524,21.2637998663661,-10.9056276191403));
#58818=CARTESIAN_POINT('Ctrl Pts',(-26.6803122660988,21.1657758516631,-10.8995401194223));
#58819=CARTESIAN_POINT('Ctrl Pts',(-26.6057099674625,21.0708936380837,-10.8934526197044));
#58820=CARTESIAN_POINT('Ctrl Pts',(-26.5268645823014,20.979597031597,-10.8873651199865));
#58821=CARTESIAN_POINT('Ctrl Pts',(-26.4510710756044,20.8918342545996,-10.8815132499032));
#58822=CARTESIAN_POINT('Ctrl Pts',(-26.3713571454313,20.8073850109463,-10.8756613798198));
#58823=CARTESIAN_POINT('Ctrl Pts',(-26.288050357235,20.7266108996056,-10.8698095097364));
#58824=CARTESIAN_POINT('Ctrl Pts',(-26.2047562532546,20.6458490868577,-10.8639585306534));
#58825=CARTESIAN_POINT('Ctrl Pts',(-26.1178706756531,20.5687615814942,-10.8581075515705));
#58826=CARTESIAN_POINT('Ctrl Pts',(-26.0277580157897,20.4956730882557,-10.8522565724875));
#58827=CARTESIAN_POINT('Ctrl Pts',(-25.9376372539309,20.4225780236584,-10.8464050673452));
#58828=CARTESIAN_POINT('Ctrl Pts',(-25.8442891541018,20.3534829463545,-10.840553562203));
#58829=CARTESIAN_POINT('Ctrl Pts',(-25.7481105753298,20.2886717769027,-10.8347020570607));
#58830=CARTESIAN_POINT('Ctrl Pts',(-25.6519000577456,20.2238390850725,-10.8288486087609));
#58831=CARTESIAN_POINT('Ctrl Pts',(-25.5528575348373,20.1632933607165,-10.8229951604612));
#58832=CARTESIAN_POINT('Ctrl Pts',(-25.4514075569683,20.1072743775557,-10.8171417121614));
#58833=CARTESIAN_POINT('Ctrl Pts',(-25.349842208445,20.0511916886468,-10.8112816072199));
#58834=CARTESIAN_POINT('Ctrl Pts',(-25.24586430249,19.9996462159032,-10.8054215022784));
#58835=CARTESIAN_POINT('Ctrl Pts',(-25.1399217111285,19.9528311079579,-10.7995613973369));
#58836=CARTESIAN_POINT('Ctrl Pts',(-25.0339077740625,19.9059844729675,-10.7936973459814));
#58837=CARTESIAN_POINT('Ctrl Pts',(-24.925926901242,19.863874695772,-10.787833294626));
#58838=CARTESIAN_POINT('Ctrl Pts',(-24.8164439462352,19.8266456376004,-10.7819692432706));
#58839=CARTESIAN_POINT('Ctrl Pts',(-24.7067996352075,19.7893617112287,-10.776096549474));
#58840=CARTESIAN_POINT('Ctrl Pts',(-24.5956492191233,19.7569729753454,-10.7702238556775));
#58841=CARTESIAN_POINT('Ctrl Pts',(-24.4834696803974,19.7295726506565,-10.7643511618809));
#58842=CARTESIAN_POINT('Ctrl Pts',(-24.4527567992256,19.7220709001074,-10.7627433165574));
#58843=CARTESIAN_POINT('Ctrl Pts',(-24.4219668161049,19.7149427682426,-10.7611354712339));
#58844=CARTESIAN_POINT('Ctrl Pts',(-24.3911095881728,19.7081894907525,-10.7595276259104));
#58845=CARTESIAN_POINT('Ctrl Pts',(-24.2784104352126,19.6835246487091,-10.7536553289417));
#58846=CARTESIAN_POINT('Ctrl Pts',(-24.164436320627,19.663781393315,-10.747783031973));
#58847=CARTESIAN_POINT('Ctrl Pts',(-24.0496550723067,19.6490878206842,-10.7419107350043));
#58848=CARTESIAN_POINT('Ctrl Pts',(-23.9350225713685,19.6344132897566,-10.7360460480661));
#58849=CARTESIAN_POINT('Ctrl Pts',(-23.8195854230289,19.6247754799554,-10.7301813611279));
#58850=CARTESIAN_POINT('Ctrl Pts',(-23.7038234806278,19.6202519001874,-10.7243166741897));
#58851=CARTESIAN_POINT('Ctrl Pts',(-23.5881805921378,19.615732972638,-10.7184580187149));
#58852=CARTESIAN_POINT('Ctrl Pts',(-23.4722139845741,19.616317829421,-10.71259936324));
#58853=CARTESIAN_POINT('Ctrl Pts',(-23.3564098346046,19.6220323228993,-10.7067407077652));
#58854=CARTESIAN_POINT('Ctrl Pts',(-23.2360822725383,19.627970029526,-10.7006532080473));
#58855=CARTESIAN_POINT('Ctrl Pts',(-23.115930569268,19.6394463362824,-10.6945657083294));
#58856=CARTESIAN_POINT('Ctrl Pts',(-22.9965019292611,19.6564305955619,-10.6884782086115));
#58857=CARTESIAN_POINT('Ctrl Pts',(-22.8816960289827,19.6727574429332,-10.6826263385281));
#58858=CARTESIAN_POINT('Ctrl Pts',(-22.7675587048147,19.6941737135958,-10.6767744684447));
#58859=CARTESIAN_POINT('Ctrl Pts',(-22.6545712390499,19.7205992808101,-10.6709225983613));
#58860=CARTESIAN_POINT('Ctrl Pts',(-22.5416009766541,19.7470208244916,-10.6650716192783));
#58861=CARTESIAN_POINT('Ctrl Pts',(-22.4297806269636,19.7784500540953,-10.6592206401954));
#58862=CARTESIAN_POINT('Ctrl Pts',(-22.3195803385021,19.8147559177346,-10.6533696611124));
#58863=CARTESIAN_POINT('Ctrl Pts',(-22.2093701419741,19.8510650456204,-10.6475181559701));
#58864=CARTESIAN_POINT('Ctrl Pts',(-22.1007806888794,19.8922515497934,-10.6416666508278));
#58865=CARTESIAN_POINT('Ctrl Pts',(-21.994265365476,19.9381350171933,-10.6358151456855));
#58866=CARTESIAN_POINT('Ctrl Pts',(-21.8877146706524,19.9840337214939,-10.6299616973857));
#58867=CARTESIAN_POINT('Ctrl Pts',(-21.7832398545578,20.0346323270471,-10.6241082490859));
#58868=CARTESIAN_POINT('Ctrl Pts',(-21.681272130316,20.0897032603698,-10.6182548007862));
#58869=CARTESIAN_POINT('Ctrl Pts',(-21.57918844663,20.144836821302,-10.6123946958446));
#58870=CARTESIAN_POINT('Ctrl Pts',(-21.479617909463,20.2044526649637,-10.6065345909031));
#58871=CARTESIAN_POINT('Ctrl Pts',(-21.3829651118169,20.2682783941298,-10.6006744859615));
#58872=CARTESIAN_POINT('Ctrl Pts',(-21.286247224561,20.3321471059297,-10.5948104346061));
#58873=CARTESIAN_POINT('Ctrl Pts',(-21.1924513230845,20.4002311062293,-10.5889463832507));
#58874=CARTESIAN_POINT('Ctrl Pts',(-21.1019497133133,20.4722170690155,-10.5830823318952));
#58875=CARTESIAN_POINT('Ctrl Pts',(-21.0113147222349,20.5443091247411,-10.5772096380986));
#58876=CARTESIAN_POINT('Ctrl Pts',(-20.9239840234159,20.6203143499014,-10.5713369443021));
#58877=CARTESIAN_POINT('Ctrl Pts',(-20.8402938742161,20.6998818409314,-10.5654642505055));
#58878=CARTESIAN_POINT('Ctrl Pts',(-20.8173809113305,20.7216660889738,-10.5638564051822));
#58879=CARTESIAN_POINT('Ctrl Pts',(-20.7947406032408,20.743717160917,-10.5622485598589));
#58880=CARTESIAN_POINT('Ctrl Pts',(-20.7723793177545,20.766027431729,-10.5606407145355));
#58881=CARTESIAN_POINT('Ctrl Pts',(-20.6907097024792,20.8475107272674,-10.5547684175668));
#58882=CARTESIAN_POINT('Ctrl Pts',(-20.6124915298197,20.9327269956377,-10.5488961205981));
#58883=CARTESIAN_POINT('Ctrl Pts',(-20.5380854499933,21.0213518867661,-10.5430238236294));
#58884=CARTESIAN_POINT('Ctrl Pts',(-20.4637757945373,21.109861927074,-10.5371591366912));
#58885=CARTESIAN_POINT('Ctrl Pts',(-20.3932686710403,21.2017714920319,-10.531294449753));
#58886=CARTESIAN_POINT('Ctrl Pts',(-20.3268886701188,21.2967187698237,-10.5254297628148));
#58887=CARTESIAN_POINT('Ctrl Pts',(-20.2605769368729,21.3915684002841,-10.5195711073399));
#58888=CARTESIAN_POINT('Ctrl Pts',(-20.1983841191357,21.4894491928289,-10.5137124518651));
#58889=CARTESIAN_POINT('Ctrl Pts',(-20.1405947660332,21.5899660931685,-10.5078537963903));
#58890=CARTESIAN_POINT('Ctrl Pts',(-20.0805481098984,21.6944092721694,-10.5017662966724));
#58891=CARTESIAN_POINT('Ctrl Pts',(-20.0252562301151,21.8016983463826,-10.4956787969545));
#58892=CARTESIAN_POINT('Ctrl Pts',(-19.9749891295499,21.9113563771781,-10.4895912972366));
#58893=CARTESIAN_POINT('Ctrl Pts',(-19.9266677241112,22.0167698604725,-10.4837394271532));
#58894=CARTESIAN_POINT('Ctrl Pts',(-19.8829895296096,22.1243719085128,-10.4778875570697));
#58895=CARTESIAN_POINT('Ctrl Pts',(-19.8441472875572,22.2337142985312,-10.4720356869863));
#58896=CARTESIAN_POINT('Ctrl Pts',(-19.8053109595893,22.3430400401764,-10.4661847079034));
#58897=CARTESIAN_POINT('Ctrl Pts',(-19.7713092583735,22.4541052075011,-10.4603337288204));
#58898=CARTESIAN_POINT('Ctrl Pts',(-19.7422860629667,22.5664434175634,-10.4544827497374));
#58899=CARTESIAN_POINT('Ctrl Pts',(-19.7132602580953,22.6787917279119,-10.4486312445951));
#58900=CARTESIAN_POINT('Ctrl Pts',(-19.689213952262,22.7924129082668,-10.4427797394528));
#58901=CARTESIAN_POINT('Ctrl Pts',(-19.6702404354251,22.9068279962544,-10.4369282343105));
#58902=CARTESIAN_POINT('Ctrl Pts',(-19.6512606178964,23.0212810790022,-10.4310747860107));
#58903=CARTESIAN_POINT('Ctrl Pts',(-19.6373570066032,23.1365281860155,-10.4252213377109));
#58904=CARTESIAN_POINT('Ctrl Pts',(-19.6285712291301,23.2520835173433,-10.4193678894112));
#58905=CARTESIAN_POINT('Ctrl Pts',(-19.6197754603201,23.3677702601752,-10.4135077844696));
#58906=CARTESIAN_POINT('Ctrl Pts',(-19.6161091734087,23.4837655145072,-10.4076476795281));
#58907=CARTESIAN_POINT('Ctrl Pts',(-19.6175618957094,23.5995816472105,-10.4017875745865));
#58908=CARTESIAN_POINT('Ctrl Pts',(-19.6190155963277,23.7154757748305,-10.3959235232311));
#58909=CARTESIAN_POINT('Ctrl Pts',(-19.6255951470715,23.8311901289213,-10.3900594718756));
#58910=CARTESIAN_POINT('Ctrl Pts',(-19.637238188645,23.946242116268,-10.3841954205201));
#58911=CARTESIAN_POINT('Ctrl Pts',(-19.6488983897376,24.0614636672775,-10.3783227267236));
#58912=CARTESIAN_POINT('Ctrl Pts',(-19.6656369159767,24.1760204957395,-10.372450032927));
#58913=CARTESIAN_POINT('Ctrl Pts',(-19.6873403076637,24.2894400244426,-10.3665773391304));
#58914=CARTESIAN_POINT('Ctrl Pts',(-19.6932823332539,24.3204923941232,-10.3649694938071));
#58915=CARTESIAN_POINT('Ctrl Pts',(-19.6995962237446,24.3514596043792,-10.3633616484839));
#58916=CARTESIAN_POINT('Ctrl Pts',(-19.7062790061382,24.3823321762144,-10.3617538031606));
#58917=CARTESIAN_POINT('Ctrl Pts',(-19.7306863805445,24.4950873693786,-10.3558815061919));
#58918=CARTESIAN_POINT('Ctrl Pts',(-19.7601000186777,24.6069566360287,-10.3500092092232));
#58919=CARTESIAN_POINT('Ctrl Pts',(-19.7944419861104,24.7174612301205,-10.3441369122545));
#58920=CARTESIAN_POINT('Ctrl Pts',(-19.8287394490808,24.8278226190343,-10.3382722253163));
#58921=CARTESIAN_POINT('Ctrl Pts',(-19.8679524189018,24.9368224612007,-10.3324075383781));
#58922=CARTESIAN_POINT('Ctrl Pts',(-19.9119519522107,25.0439920984628,-10.3265428514399));
#58923=CARTESIAN_POINT('Ctrl Pts',(-19.955906234754,25.1510515184619,-10.3206841959651));
#58924=CARTESIAN_POINT('Ctrl Pts',(-20.0046371332621,25.2562840973421,-10.3148255404903));
#58925=CARTESIAN_POINT('Ctrl Pts',(-20.0579660927985,25.3592368955584,-10.3089668850155));
#58926=CARTESIAN_POINT('Ctrl Pts',(-20.1133781284661,25.466211120753,-10.3028793852976));
#58927=CARTESIAN_POINT('Ctrl Pts',(-20.1737546217122,25.5707233998347,-10.2967918855797));
#58928=CARTESIAN_POINT('Ctrl Pts',(-20.2388402640609,25.672288769313,-10.2907043858618));
#58929=CARTESIAN_POINT('Ctrl Pts',(-20.3014066280802,25.7699228349722,-10.2848525157784));
#58930=CARTESIAN_POINT('Ctrl Pts',(-20.3683241206917,25.8648335013899,-10.279000645695));
#58931=CARTESIAN_POINT('Ctrl Pts',(-20.4393198295186,25.956616328491,-10.2731487756116));
#58932=CARTESIAN_POINT('Ctrl Pts',(-20.5103047286033,26.0483851808221,-10.2672977965287));
#58933=CARTESIAN_POINT('Ctrl Pts',(-20.5853663564104,26.1370268138693,-10.2614468174457));
#58934=CARTESIAN_POINT('Ctrl Pts',(-20.6641901098758,26.2221680800167,-10.2555958383628));
#58935=CARTESIAN_POINT('Ctrl Pts',(-20.7430209503551,26.3073170011833,-10.2497443332205));
#58936=CARTESIAN_POINT('Ctrl Pts',(-20.8256143080533,26.388964626461,-10.2438928280782));
#58937=CARTESIAN_POINT('Ctrl Pts',(-20.9116176510668,26.4667735699753,-10.2380413229359));
#58938=CARTESIAN_POINT('Ctrl Pts',(-20.9976495539183,26.5446083521459,-10.2321878746362));
#58939=CARTESIAN_POINT('Ctrl Pts',(-21.0870933873727,26.6186016406174,-10.2263344263364));
#58940=CARTESIAN_POINT('Ctrl Pts',(-21.1795629412545,26.6884558179363,-10.2204809780366));
#58941=CARTESIAN_POINT('Ctrl Pts',(-21.2721376530984,26.7583894346234,-10.2146208730951));
#58942=CARTESIAN_POINT('Ctrl Pts',(-21.3677446232639,26.8241742956702,-10.2087607681536));
#58943=CARTESIAN_POINT('Ctrl Pts',(-21.4659679368872,26.8855556255449,-10.2029006632121));
#58944=CARTESIAN_POINT('Ctrl Pts',(-21.5642573977646,26.9469782919036,-10.1970366118566));
#58945=CARTESIAN_POINT('Ctrl Pts',(-21.6651663514486,27.0039913193353,-10.1911725605012));
#58946=CARTESIAN_POINT('Ctrl Pts',(-21.7682550763275,27.0563863096705,-10.1853085091458));
#58947=CARTESIAN_POINT('Ctrl Pts',(-21.8714957334084,27.1088585197625,-10.1794358153492));
#58948=CARTESIAN_POINT('Ctrl Pts',(-21.9769221982844,27.1566989389869,-10.1735631215527));
#58949=CARTESIAN_POINT('Ctrl Pts',(-22.0840755540415,27.199747574875,-10.1676904277561));
#58950=CARTESIAN_POINT('Ctrl Pts',(-22.1134123503931,27.2115335712662,-10.1660825824327));
#58951=CARTESIAN_POINT('Ctrl Pts',(-22.1428785094352,27.2229606791983,-10.1644747371092));
#58952=CARTESIAN_POINT('Ctrl Pts',(-22.1724644492979,27.2340262761045,-10.1628668917858));
#58953=CARTESIAN_POINT('Ctrl Pts',(-22.2805205057102,27.2744409044409,-10.1569945948171));
#58954=CARTESIAN_POINT('Ctrl Pts',(-22.390537315057,27.3101647982694,-10.1511222978484));
#58955=CARTESIAN_POINT('Ctrl Pts',(-22.5020699733967,27.3410047425992,-10.1452500008797));
#58956=CARTESIAN_POINT('Ctrl Pts',(-22.6134580942689,27.3718047208103,-10.1393853139414));
#58957=CARTESIAN_POINT('Ctrl Pts',(-22.7263577628541,27.3977332268973,-10.1335206270032));
#58958=CARTESIAN_POINT('Ctrl Pts',(-22.8403049898277,27.4186454134731,-10.127655940065));
#58959=CARTESIAN_POINT('Ctrl Pts',(-22.9541350292116,27.4395360931742,-10.1217972845902));
#58960=CARTESIAN_POINT('Ctrl Pts',(-23.0690100799351,27.4554206406507,-10.1159386291154));
#58961=CARTESIAN_POINT('Ctrl Pts',(-23.1844525598468,27.4662044441411,-10.1100799736406));
#58962=CARTESIAN_POINT('Ctrl Pts',(-23.3044043247042,27.4774094724941,-10.1039924739227));
#58963=CARTESIAN_POINT('Ctrl Pts',(-23.4249683127691,27.483107033148,-10.0979049742048));
#58964=CARTESIAN_POINT('Ctrl Pts',(-23.5455985110658,27.4832497780817,-10.0918174744869));
#58965=CARTESIAN_POINT('Ctrl Pts',(-23.6615594607623,27.483386997769,-10.0859656044035));
#58966=CARTESIAN_POINT('Ctrl Pts',(-23.7775811384447,27.4783914272242,-10.0801137343201));
#58967=CARTESIAN_POINT('Ctrl Pts',(-23.8931757611827,27.4682740552029,-10.0742618642367));
#58968=CARTESIAN_POINT('Ctrl Pts',(-24.0087527835882,27.4581582236435,-10.0684108851537));
#58969=CARTESIAN_POINT('Ctrl Pts',(-24.1239024686402,27.4429221772143,-10.0625599060707));
#58970=CARTESIAN_POINT('Ctrl Pts',(-24.2381408246955,27.4226288946465,-10.0567089269878));
#58971=CARTESIAN_POINT('Ctrl Pts',(-24.3523894518784,27.4023337875173,-10.0508574218455));
#58972=CARTESIAN_POINT('Ctrl Pts',(-24.4657261801457,27.3769806126651,-10.0450059167032));
#58973=CARTESIAN_POINT('Ctrl Pts',(-24.5776766026615,27.3466835897271,-10.0391544115609));
#58974=CARTESIAN_POINT('Ctrl Pts',(-24.6896642014754,27.3163765058074,-10.0333009632611));
#58975=CARTESIAN_POINT('Ctrl Pts',(-24.8002641803195,27.2811224172283,-10.0274475149614));
#58976=CARTESIAN_POINT('Ctrl Pts',(-24.9090173856644,27.2410853742401,-10.0215940666616));
#58977=CARTESIAN_POINT('Ctrl Pts',(-25.0178942670191,27.2010028004401,-10.0157339617201));
#58978=CARTESIAN_POINT('Ctrl Pts',(-25.1249197948141,27.1561265585363,-10.0098738567785));
#58979=CARTESIAN_POINT('Ctrl Pts',(-25.2296548025042,27.1066688477064,-10.004013751837));
#58980=CARTESIAN_POINT('Ctrl Pts',(-25.3344603426669,27.0571778302038,-9.99814970048156));
#58981=CARTESIAN_POINT('Ctrl Pts',(-25.4369719265244,27.0030993926744,-9.99228564912612));
#58982=CARTESIAN_POINT('Ctrl Pts',(-25.536776537028,26.944690832243,-9.98642159777068));
#58983=CARTESIAN_POINT('Ctrl Pts',(-25.6367282396045,26.886196189253,-9.98054890397411));
#58984=CARTESIAN_POINT('Ctrl Pts',(-25.733964660587,26.8233589101714,-9.97467621017755));
#58985=CARTESIAN_POINT('Ctrl Pts',(-25.8281031315803,26.756478606786,-9.96880351638099));
#58986=CARTESIAN_POINT('Ctrl Pts',(-25.8538766701948,26.7381678984893,-9.96719567105761));
#58987=CARTESIAN_POINT('Ctrl Pts',(-25.8794181959453,26.7195543607642,-9.96558782573423));
#58988=CARTESIAN_POINT('Ctrl Pts',(-25.9047203230156,26.7006446373899,-9.96397998041085));
#58989=CARTESIAN_POINT('Ctrl Pts',(-25.99620696118,26.6322714521903,-9.95816638367587));
#58990=CARTESIAN_POINT('Ctrl Pts',(-26.0848810300192,26.5597839066081,-9.95235278694089));
#58991=CARTESIAN_POINT('Ctrl Pts',(-26.1703438557641,26.4834437040411,-9.94653919020591));
#58992=CARTESIAN_POINT('Ctrl Pts',(-26.2556955458028,26.4072027741373,-9.94073315346175));
#58993=CARTESIAN_POINT('Ctrl Pts',(-26.3378439815586,26.3271194246759,-9.9349271167176));
#58994=CARTESIAN_POINT('Ctrl Pts',(-26.4164204716666,26.2434978491271,-9.92912107997345));
#58995=CARTESIAN_POINT('Ctrl Pts',(-26.4949168496792,26.1599615293543,-9.9233209627323));
#58996=CARTESIAN_POINT('Ctrl Pts',(-26.5698482352409,26.0728944618218,-9.91752084549115));
#58997=CARTESIAN_POINT('Ctrl Pts',(-26.6408805851238,25.9826396792005,-9.91172072825));
#58998=CARTESIAN_POINT('Ctrl Pts',(-26.7118616411519,25.8924500713302,-9.90592479938741));
#58999=CARTESIAN_POINT('Ctrl Pts',(-26.7789490000741,25.799077656742,-9.90012887052482));
#59000=CARTESIAN_POINT('Ctrl Pts',(-26.8418474637209,25.7029001580966,-9.89433294166223));
#59001=CARTESIAN_POINT('Ctrl Pts',(-26.9047224438966,25.6067585678247,-9.88853917674008));
#59002=CARTESIAN_POINT('Ctrl Pts',(-26.9634114058272,25.5078143278235,-9.88274541181792));
#59003=CARTESIAN_POINT('Ctrl Pts',(-27.0176616508371,25.4064753094028,-9.87695164689577));
#59004=CARTESIAN_POINT('Ctrl Pts',(-27.0719054207339,25.3051483864411,-9.87115857349646));
#59005=CARTESIAN_POINT('Ctrl Pts',(-27.1217113278621,25.201427625859,-9.86536550009714));
#59006=CARTESIAN_POINT('Ctrl Pts',(-27.1668723540204,25.0957460000586,-9.85957242669782));
#59007=CARTESIAN_POINT('Ctrl Pts',(-27.2120394611068,24.9900501442368,-9.85377857326169));
#59008=CARTESIAN_POINT('Ctrl Pts',(-27.252560279181,24.8823932873311,-9.84798471982556));
#59009=CARTESIAN_POINT('Ctrl Pts',(-27.2882760361925,24.7732281160042,-9.84219086638942));
#59010=CARTESIAN_POINT('Ctrl Pts',(-27.3240260308546,24.6639582973366,-9.83639145888007));
#59011=CARTESIAN_POINT('Ctrl Pts',(-27.3549616363811,24.5531776795425,-9.83059205137072));
#59012=CARTESIAN_POINT('Ctrl Pts',(-27.3809740699463,24.4413538145859,-9.82479264386136));
#59013=CARTESIAN_POINT('Ctrl Pts',(-27.4070000385292,24.3294717644551,-9.81899021875343));
#59014=CARTESIAN_POINT('Ctrl Pts',(-27.4280976577133,24.2165458013837,-9.81318779364549));
#59015=CARTESIAN_POINT('Ctrl Pts',(-27.4442096767031,24.1030515483667,-9.80738536853755));
#59016=CARTESIAN_POINT('Ctrl Pts',(-27.4603455593391,23.9893891980616,-9.80157434940922));
#59017=CARTESIAN_POINT('Ctrl Pts',(-27.4714810570642,23.8751572971363,-9.79576333028089));
#59018=CARTESIAN_POINT('Ctrl Pts',(-27.4776109559515,23.7608345998186,-9.78995231115256));
#59019=CARTESIAN_POINT('Ctrl Pts',(-27.4814045639771,23.6900837587301,-9.7863560481133));
#59020=CARTESIAN_POINT('Ctrl Pts',(-27.4832820636393,23.6192981373075,-9.78275978507405));
#59021=CARTESIAN_POINT('Ctrl Pts',(-27.4832521804468,23.5485903307078,-9.7791635220348));
#59022=CARTESIAN_POINT('',(-27.4839897010956,23.5538383238888,-8.5291635220348));
#59023=CARTESIAN_POINT('Ctrl Pts',(-27.4889022247121,23.5485879428334,-9.7791635220348));
#59024=CARTESIAN_POINT('Ctrl Pts',(-27.4893933224062,23.456239996285,-9.77447337103519));
#59025=CARTESIAN_POINT('Ctrl Pts',(-27.4445143940911,22.059032543948,-9.70348758291055));
#59026=CARTESIAN_POINT('Ctrl Pts',(-25.7819745911596,19.4685656890507,-9.56620615766113));
#59027=CARTESIAN_POINT('Ctrl Pts',(-21.3226012899819,19.4663425452466,-9.36731924628616));
#59028=CARTESIAN_POINT('Ctrl Pts',(-18.9102506062613,23.21688642052,-9.16843233491138));
#59029=CARTESIAN_POINT('Ctrl Pts',(-20.7616682847246,27.27376548718,-8.96954542353633));
#59030=CARTESIAN_POINT('Ctrl Pts',(-25.1755584532003,27.9090518495824,-8.77065851216153));
#59031=CARTESIAN_POINT('Ctrl Pts',(-27.3310193809219,25.4216709344377,-8.62386454499429));
#59032=CARTESIAN_POINT('Ctrl Pts',(-27.4865993094704,23.8343954513882,-8.54336621495207));
#59033=CARTESIAN_POINT('Ctrl Pts',(-27.4839897010956,23.5538383238888,-8.5291635220348));
#59034=CARTESIAN_POINT('',(-27.4767287689123,23.5502697193127,-7.2791635220348));
#59035=CARTESIAN_POINT('Ctrl Pts',(-27.4839897010956,23.5538383238888,-8.5291635220348));
#59036=CARTESIAN_POINT('Ctrl Pts',(-27.4744181230669,22.5248048247472,-8.47707057782711));
#59037=CARTESIAN_POINT('Ctrl Pts',(-26.5336429110486,20.1706869477114,-8.35868199649442));
#59038=CARTESIAN_POINT('Ctrl Pts',(-22.560216303688,19.0048615584841,-8.17399777803684));
#59039=CARTESIAN_POINT('Ctrl Pts',(-19.1909822903886,21.9262101075659,-7.97511086666202));
#59040=CARTESIAN_POINT('Ctrl Pts',(-19.8275480236813,26.3399159483343,-7.77622395528699));
#59041=CARTESIAN_POINT('Ctrl Pts',(-23.8849635665489,28.1901576336603,-7.57733704391218));
#59042=CARTESIAN_POINT('Ctrl Pts',(-27.0088482393263,26.1795939710675,-7.4116502328281));
#59043=CARTESIAN_POINT('Ctrl Pts',(-27.476754263685,24.207090521581,-7.31225905886896));
#59044=CARTESIAN_POINT('Ctrl Pts',(-27.4767287689123,23.5502697193127,-7.2791635220348));
#59045=CARTESIAN_POINT('',(-27.4839264031395,23.5466608562294,-6.02916352203481));
#59046=CARTESIAN_POINT('Ctrl Pts',(-27.4767287689123,23.5502697193127,-7.2791635220348));
#59047=CARTESIAN_POINT('Ctrl Pts',(-27.4767031935903,22.8913737292682,-7.245963421744));
#59048=CARTESIAN_POINT('Ctrl Pts',(-27.0066715029592,20.9167266579016,-7.14646768432824));
#59049=CARTESIAN_POINT('Ctrl Pts',(-23.8776470449471,18.909825432299,-6.9806763097875));
#59050=CARTESIAN_POINT('Ctrl Pts',(-19.8231539683923,20.7664624656976,-6.78178939841262));
#59051=CARTESIAN_POINT('Ctrl Pts',(-19.1935484656661,25.1811665432707,-6.58290248703777));
#59052=CARTESIAN_POINT('Ctrl Pts',(-22.5673846120303,28.0971989229123,-6.38401557566277));
#59053=CARTESIAN_POINT('Ctrl Pts',(-26.5367194223868,26.9257733735504,-6.19943592066184));
#59054=CARTESIAN_POINT('Ctrl Pts',(-27.4743736257135,24.5736712048814,-6.08115190278585));
#59055=CARTESIAN_POINT('Ctrl Pts',(-27.4839264031395,23.5466608562294,-6.02916352203481));
#59056=CARTESIAN_POINT('',(-27.4847663727323,23.5518813974934,-4.77916352203479));
#59057=CARTESIAN_POINT('Ctrl Pts',(-27.4839264031395,23.5466608562294,-6.02916352203481));
#59058=CARTESIAN_POINT('Ctrl Pts',(-27.486555337408,23.2640265417046,-6.01485626566089));
#59059=CARTESIAN_POINT('Ctrl Pts',(-27.3296020251925,21.674644395198,-5.93425337216194));
#59060=CARTESIAN_POINT('Ctrl Pts',(-25.1686835689709,19.1888958838517,-5.78735484153822));
#59061=CARTESIAN_POINT('Ctrl Pts',(-20.7558005937558,19.8311411864055,-5.58846793016332));
#59062=CARTESIAN_POINT('Ctrl Pts',(-18.9107820190502,23.8909344866399,-5.38958101878834));
#59063=CARTESIAN_POINT('Ctrl Pts',(-21.3290434832377,27.6376699553445,-5.19069410741347));
#59064=CARTESIAN_POINT('Ctrl Pts',(-25.788407735483,27.6284153675624,-4.99180719603861));
#59065=CARTESIAN_POINT('Ctrl Pts',(-27.4455976798272,25.0373053559045,-4.85463033424573));
#59066=CARTESIAN_POINT('Ctrl Pts',(-27.4894091699444,23.6421701040578,-4.78374910957776));
#59067=CARTESIAN_POINT('Ctrl Pts',(-27.4889373831764,23.5518831242674,-4.77916352203479));
#59068=CARTESIAN_POINT('',(-27.4824137648665,23.5530535657996,-3.52916356170341));
#59069=CARTESIAN_POINT('Ctrl Pts',(-27.4832521946535,23.5518807706325,-4.77916352203479));
#59070=CARTESIAN_POINT('Ctrl Pts',(-27.4832995073027,23.4375974003668,-4.77335077744995));
#59071=CARTESIAN_POINT('Ctrl Pts',(-27.4783614066125,23.3231104330131,-4.7675380328651));
#59072=CARTESIAN_POINT('Ctrl Pts',(-27.4684108958793,23.208896364083,-4.76172528828025));
#59073=CARTESIAN_POINT('Ctrl Pts',(-27.458472701503,23.0948236649049,-4.75591973848558));
#59074=CARTESIAN_POINT('Ctrl Pts',(-27.4435344664143,22.9810236096023,-4.7501141886909));
#59075=CARTESIAN_POINT('Ctrl Pts',(-27.4236211929847,22.8679738395655,-4.74430863889623));
#59076=CARTESIAN_POINT('Ctrl Pts',(-27.4037269798246,22.7550322767053,-4.73850864596515));
#59077=CARTESIAN_POINT('Ctrl Pts',(-27.3788672694762,22.6428399848093,-4.73270865303407));
#59078=CARTESIAN_POINT('Ctrl Pts',(-27.3491188987623,22.5318698309578,-4.726908660103));
#59079=CARTESIAN_POINT('Ctrl Pts',(-27.3193892046031,22.4209693461372,-4.72111230851035));
#59080=CARTESIAN_POINT('Ctrl Pts',(-27.2847770608197,22.3112898807109,-4.71531595691771));
#59081=CARTESIAN_POINT('Ctrl Pts',(-27.2454103083026,22.2032937327808,-4.70951960532507));
#59082=CARTESIAN_POINT('Ctrl Pts',(-27.2060559748648,22.0953316545322,-4.70372508231481));
#59083=CARTESIAN_POINT('Ctrl Pts',(-27.1619501578594,21.9890522349221,-4.69793055930455));
#59084=CARTESIAN_POINT('Ctrl Pts',(-27.1132702123033,21.8849015153416,-4.69213603629429));
#59085=CARTESIAN_POINT('Ctrl Pts',(-27.0645932674965,21.7807572158625,-4.68634187047239));
#59086=CARTESIAN_POINT('Ctrl Pts',(-27.011342933768,21.6787417380542,-4.68054770465049));
#59087=CARTESIAN_POINT('Ctrl Pts',(-26.9537439098953,21.579279310539,-4.67475353882859));
#59088=CARTESIAN_POINT('Ctrl Pts',(-26.896133815525,21.4797977664054,-4.66895825937153));
#59089=CARTESIAN_POINT('Ctrl Pts',(-26.8341735820922,21.3828706129,-4.66316297991446));
#59090=CARTESIAN_POINT('Ctrl Pts',(-26.7681324437633,21.2888950032387,-4.6573677004574));
#59091=CARTESIAN_POINT('Ctrl Pts',(-26.7020219864012,21.1948207535695,-4.6515663380772));
#59092=CARTESIAN_POINT('Ctrl Pts',(-26.6318223156162,21.1037045788478,-4.64576497569699));
#59093=CARTESIAN_POINT('Ctrl Pts',(-26.5578443679754,21.0159123125573,-4.63996361331678));
#59094=CARTESIAN_POINT('Ctrl Pts',(-26.4838243075402,20.9280700695132,-4.63415894844457));
#59095=CARTESIAN_POINT('Ctrl Pts',(-26.4060219746012,20.8435558116978,-4.62835428357235));
#59096=CARTESIAN_POINT('Ctrl Pts',(-26.3247854260627,20.7626987262821,-4.62254961870013));
#59097=CARTESIAN_POINT('Ctrl Pts',(-26.2434216288695,20.6817149866016,-4.61673586142051));
#59098=CARTESIAN_POINT('Ctrl Pts',(-26.1586131871594,20.6044001411639,-4.61092210414089));
#59099=CARTESIAN_POINT('Ctrl Pts',(-26.0707416448313,20.5310434248986,-4.60510834686127));
#59100=CARTESIAN_POINT('Ctrl Pts',(-26.014944394605,20.4844628944472,-4.60141668900378));
#59101=CARTESIAN_POINT('Ctrl Pts',(-25.9579127026491,20.4394774646879,-4.59772503114629));
#59102=CARTESIAN_POINT('Ctrl Pts',(-25.8997499236222,20.3961518666356,-4.5940333732888));
#59103=CARTESIAN_POINT('Ctrl Pts',(-25.8072307563115,20.3272341099171,-4.58816107632009));
#59104=CARTESIAN_POINT('Ctrl Pts',(-25.7115216787875,20.2622751428022,-4.58228877935138));
#59105=CARTESIAN_POINT('Ctrl Pts',(-25.6129961542005,20.201584475913,-4.57641648238267));
#59106=CARTESIAN_POINT('Ctrl Pts',(-25.5145983108687,20.1409724593082,-4.57055179544447));
#59107=CARTESIAN_POINT('Ctrl Pts',(-25.4133916275155,20.0846179578096,-4.56468710850628));
#59108=CARTESIAN_POINT('Ctrl Pts',(-25.3097813717287,20.0327893462313,-4.55882242156808));
#59109=CARTESIAN_POINT('Ctrl Pts',(-25.2062776726035,19.9810140371353,-4.55296376609324));
#59110=CARTESIAN_POINT('Ctrl Pts',(-25.1003756853129,19.9337555435576,-4.54710511061841));
#59111=CARTESIAN_POINT('Ctrl Pts',(-24.9925077271812,19.8912377802767,-4.54124645514357));
#59112=CARTESIAN_POINT('Ctrl Pts',(-24.8804263515962,19.847059235713,-4.53515895542567));
#59113=CARTESIAN_POINT('Ctrl Pts',(-24.7662226761918,19.8079995641882,-4.52907145570777));
#59114=CARTESIAN_POINT('Ctrl Pts',(-24.6504079070978,19.7742563518801,-4.52298395598987));
#59115=CARTESIAN_POINT('Ctrl Pts',(-24.5390759951661,19.7418192424306,-4.51713208590647));
#59116=CARTESIAN_POINT('Ctrl Pts',(-24.4262558259643,19.7142948016807,-4.51128021582307));
#59117=CARTESIAN_POINT('Ctrl Pts',(-24.3124189327844,19.6918083663538,-4.50542834573966));
#59118=CARTESIAN_POINT('Ctrl Pts',(-24.1985993723066,19.6693253547912,-4.4995773666567));
#59119=CARTESIAN_POINT('Ctrl Pts',(-24.0837638010889,19.6518789035333,-4.49372638757373));
#59120=CARTESIAN_POINT('Ctrl Pts',(-23.968394595011,19.6395433613665,-4.48787540849076));
#59121=CARTESIAN_POINT('Ctrl Pts',(-23.853015016131,19.6272067101157,-4.48202390334846));
#59122=CARTESIAN_POINT('Ctrl Pts',(-23.7371021180777,19.6199819253913,-4.47617239820615));
#59123=CARTESIAN_POINT('Ctrl Pts',(-23.6211433464772,19.617891473452,-4.47032089306385));
#59124=CARTESIAN_POINT('Ctrl Pts',(-23.5051460674937,19.6158003273192,-4.4644674447641));
#59125=CARTESIAN_POINT('Ctrl Pts',(-23.389103297769,19.6188469117042,-4.45861399646435));
#59126=CARTESIAN_POINT('Ctrl Pts',(-23.2735017156984,19.6270015856234,-4.4527605481646));
#59127=CARTESIAN_POINT('Ctrl Pts',(-23.157768669526,19.6351655331776,-4.44690044322306));
#59128=CARTESIAN_POINT('Ctrl Pts',(-23.0424782250408,19.6484491357631,-4.44104033828151));
#59129=CARTESIAN_POINT('Ctrl Pts',(-22.9281112786345,19.6667709415175,-4.43518023333997));
#59130=CARTESIAN_POINT('Ctrl Pts',(-22.8136673132476,19.6851050858613,-4.42931618198451));
#59131=CARTESIAN_POINT('Ctrl Pts',(-22.7001484881982,19.7084841061587,-4.42345213062905));
#59132=CARTESIAN_POINT('Ctrl Pts',(-22.5880231493654,19.7367759530611,-4.41758807927359));
#59133=CARTESIAN_POINT('Ctrl Pts',(-22.4757325601657,19.7651094964982,-4.41171538547702));
#59134=CARTESIAN_POINT('Ctrl Pts',(-22.3648399504818,19.7983701989171,-4.40584269168044));
#59135=CARTESIAN_POINT('Ctrl Pts',(-22.2557963073753,19.836376916744,-4.39996999788387));
#59136=CARTESIAN_POINT('Ctrl Pts',(-22.2259419819702,19.8467825203102,-4.39836215256054));
#59137=CARTESIAN_POINT('Ctrl Pts',(-22.1962261195809,19.8575436004932,-4.39675430723721));
#59138=CARTESIAN_POINT('Ctrl Pts',(-22.1666576645012,19.8686558341352,-4.39514646191389));
#59139=CARTESIAN_POINT('Ctrl Pts',(-22.0586654673578,19.9092407927657,-4.38927416494519));
#59140=CARTESIAN_POINT('Ctrl Pts',(-21.9522795846292,19.9546493699853,-4.3834018679765));
#59141=CARTESIAN_POINT('Ctrl Pts',(-21.8479622854598,20.0047346685922,-4.3775295710078));
#59142=CARTESIAN_POINT('Ctrl Pts',(-21.7437801732253,20.0547550606299,-4.37166488406961));
#59143=CARTESIAN_POINT('Ctrl Pts',(-21.6416616827766,20.1094399443087,-4.36580019713141));
#59144=CARTESIAN_POINT('Ctrl Pts',(-21.5420516666592,20.1685934291718,-4.35993551019322));
#59145=CARTESIAN_POINT('Ctrl Pts',(-21.442544093208,20.2276860783786,-4.35407685471841));
#59146=CARTESIAN_POINT('Ctrl Pts',(-21.3455402160124,20.291237977927,-4.34821819924361));
#59147=CARTESIAN_POINT('Ctrl Pts',(-21.2514621041735,20.3590064474288,-4.3423595437688));
#59148=CARTESIAN_POINT('Ctrl Pts',(-21.153709218423,20.4294220130393,-4.3362720440509));
#59149=CARTESIAN_POINT('Ctrl Pts',(-21.0591157334227,20.5043900729783,-4.33018454433299));
#59150=CARTESIAN_POINT('Ctrl Pts',(-20.9681242103239,20.5835873446571,-4.32409704461509));
#59151=CARTESIAN_POINT('Ctrl Pts',(-20.8806547078126,20.6597191173552,-4.31824517453171));
#59152=CARTESIAN_POINT('Ctrl Pts',(-20.796513849758,20.7397584915599,-4.31239330444832));
#59153=CARTESIAN_POINT('Ctrl Pts',(-20.7160619677825,20.8233765082135,-4.30654143436494));
#59154=CARTESIAN_POINT('Ctrl Pts',(-20.6356223353376,20.9069817932637,-4.30069045528199));
#59155=CARTESIAN_POINT('Ctrl Pts',(-20.558870848705,20.994164339556,-4.29483947619903));
#59156=CARTESIAN_POINT('Ctrl Pts',(-20.4861308033785,21.0845585048402,-4.28898849711608));
#59157=CARTESIAN_POINT('Ctrl Pts',(-20.413384218022,21.1749607974296,-4.28313699197381));
#59158=CARTESIAN_POINT('Ctrl Pts',(-20.34465005012,21.2685749609526,-4.27728548683155));
#59159=CARTESIAN_POINT('Ctrl Pts',(-20.2802106859383,21.3650030431906,-4.27143398168928));
#59160=CARTESIAN_POINT('Ctrl Pts',(-20.2157499228468,21.4614631470953,-4.26558053338955));
#59161=CARTESIAN_POINT('Ctrl Pts',(-20.1555870289678,21.5607386842724,-4.25972708508982));
#59162=CARTESIAN_POINT('Ctrl Pts',(-20.0999601371491,21.6624041818144,-4.25387363679009));
#59163=CARTESIAN_POINT('Ctrl Pts',(-20.0442699854748,21.7641852951039,-4.24801353184856));
#59164=CARTESIAN_POINT('Ctrl Pts',(-19.9931263304524,21.86836143075,-4.24215342690702));
#59165=CARTESIAN_POINT('Ctrl Pts',(-19.9467205901495,21.974483974365,-4.23629332196549));
#59166=CARTESIAN_POINT('Ctrl Pts',(-19.9002835984851,22.0806779848711,-4.23042927061004));
#59167=CARTESIAN_POINT('Ctrl Pts',(-19.8585910231763,22.1888206286094,-4.2245652192546));
#59168=CARTESIAN_POINT('Ctrl Pts',(-19.8217849296931,22.2984465000629,-4.21870116789916));
#59169=CARTESIAN_POINT('Ctrl Pts',(-19.7849245913754,22.4082339381675,-4.2128284741026));
#59170=CARTESIAN_POINT('Ctrl Pts',(-19.7529652217709,22.5195085709564,-4.20695578030604));
#59171=CARTESIAN_POINT('Ctrl Pts',(-19.7259981993774,22.6317930596673,-4.20108308650949));
#59172=CARTESIAN_POINT('Ctrl Pts',(-19.7186150797485,22.662534674389,-4.19947524118601));
#59173=CARTESIAN_POINT('Ctrl Pts',(-19.7116058736916,22.6933519480334,-4.19786739586254));
#59174=CARTESIAN_POINT('Ctrl Pts',(-19.7049717788315,22.724235018766,-4.19625955053907));
#59175=CARTESIAN_POINT('Ctrl Pts',(-19.6807422248015,22.8370285568011,-4.19038725357036));
#59176=CARTESIAN_POINT('Ctrl Pts',(-19.6614391430601,22.951078045903,-4.18451495660165));
#59177=CARTESIAN_POINT('Ctrl Pts',(-19.6471888225963,23.0659151671195,-4.17864265963295));
#59178=CARTESIAN_POINT('Ctrl Pts',(-19.6329569694161,23.180603468547,-4.17277797269474));
#59179=CARTESIAN_POINT('Ctrl Pts',(-19.623764906374,23.2960769658161,-4.16691328575654));
#59180=CARTESIAN_POINT('Ctrl Pts',(-19.6196882892013,23.4118555099198,-4.16104859881834));
#59181=CARTESIAN_POINT('Ctrl Pts',(-19.6156158645741,23.5275149830393,-4.15518994334349));
#59182=CARTESIAN_POINT('Ctrl Pts',(-19.6166484360432,23.6434784683419,-4.14933128786865));
#59183=CARTESIAN_POINT('Ctrl Pts',(-19.6228099787682,23.7592596929737,-4.1434726323938));
#59184=CARTESIAN_POINT('Ctrl Pts',(-19.629212196779,23.8795634342178,-4.1373851326759));
#59185=CARTESIAN_POINT('Ctrl Pts',(-19.6411522946933,23.99966993478,-4.131297632958));
#59186=CARTESIAN_POINT('Ctrl Pts',(-19.6585975125088,24.1190321125942,-4.1252101332401));
#59187=CARTESIAN_POINT('Ctrl Pts',(-19.6753674760346,24.2337741232403,-4.11935826315671));
#59188=CARTESIAN_POINT('Ctrl Pts',(-19.6972242437108,24.3478279137254,-4.11350639307332));
#59189=CARTESIAN_POINT('Ctrl Pts',(-19.7240858312803,24.4607125146937,-4.10765452298992));
#59190=CARTESIAN_POINT('Ctrl Pts',(-19.7509433289288,24.5735799279553,-4.10180354390695));
#59191=CARTESIAN_POINT('Ctrl Pts',(-19.7828040356436,24.6852781036165,-4.09595256482398));
#59192=CARTESIAN_POINT('Ctrl Pts',(-19.8195350853847,24.7953374026173,-4.09010158574101));
#59193=CARTESIAN_POINT('Ctrl Pts',(-19.8562694376005,24.9054065970081,-4.08425008059872));
#59194=CARTESIAN_POINT('Ctrl Pts',(-19.897874872455,25.0138362296735,-4.07839857545642));
#59195=CARTESIAN_POINT('Ctrl Pts',(-19.9441692278176,25.1201736142657,-4.07254707031413));
#59196=CARTESIAN_POINT('Ctrl Pts',(-19.9904789565281,25.2265463111891,-4.06669362201433));
#59197=CARTESIAN_POINT('Ctrl Pts',(-20.0414805369979,25.3308249996716,-4.06084017371453));
#59198=CARTESIAN_POINT('Ctrl Pts',(-20.0969447326303,25.4325793484093,-4.05498672541473));
#59199=CARTESIAN_POINT('Ctrl Pts',(-20.1524720030967,25.5344494139364,-4.0491266204732));
#59200=CARTESIAN_POINT('Ctrl Pts',(-20.2124718202358,25.633789046664,-4.04326651553167));
#59201=CARTESIAN_POINT('Ctrl Pts',(-20.2766702268169,25.7301947082655,-4.03740641059013));
#59202=CARTESIAN_POINT('Ctrl Pts',(-20.3409118670067,25.8266652930459,-4.03154235923471));
#59203=CARTESIAN_POINT('Ctrl Pts',(-20.4093574831997,25.9201976396138,-4.02567830787928));
#59204=CARTESIAN_POINT('Ctrl Pts',(-20.4816923143348,26.0104206544937,-4.01981425652385));
#59205=CARTESIAN_POINT('Ctrl Pts',(-20.5541337525718,26.1007766400877,-4.01394156272729));
#59206=CARTESIAN_POINT('Ctrl Pts',(-20.6304755740057,26.187813250247,-4.00806886893072));
#59207=CARTESIAN_POINT('Ctrl Pts',(-20.7103655794784,26.2711955848716,-4.00219617513415));
#59208=CARTESIAN_POINT('Ctrl Pts',(-20.7322381265803,26.2940242732758,-4.00058832981082));
#59209=CARTESIAN_POINT('Ctrl Pts',(-20.7543764429403,26.3165792787735,-3.99898048448748));
#59210=CARTESIAN_POINT('Ctrl Pts',(-20.7767728789984,26.3388542630432,-3.99737263916415));
#59211=CARTESIAN_POINT('Ctrl Pts',(-20.8585708739085,26.4202086823437,-3.99150034219543));
#59212=CARTESIAN_POINT('Ctrl Pts',(-20.9440884886437,26.4980972726453,-3.98562804522671));
#59213=CARTESIAN_POINT('Ctrl Pts',(-21.0329999831643,26.5721606386557,-3.97975574825799));
#59214=CARTESIAN_POINT('Ctrl Pts',(-21.1217962554489,26.6461280244254,-3.97389106131979));
#59215=CARTESIAN_POINT('Ctrl Pts',(-21.2139773463907,26.7162797818324,-3.96802637438158));
#59216=CARTESIAN_POINT('Ctrl Pts',(-21.3091801937043,26.7822927195472,-3.96216168744338));
#59217=CARTESIAN_POINT('Ctrl Pts',(-21.4042851308495,26.8482377670881,-3.95630303196855));
#59218=CARTESIAN_POINT('Ctrl Pts',(-21.5024053053512,26.9100522272334,-3.95044437649372));
#59219=CARTESIAN_POINT('Ctrl Pts',(-21.6031445672889,26.9674530781868,-3.94458572101889));
#59220=CARTESIAN_POINT('Ctrl Pts',(-21.7078187935275,27.0270960569363,-3.93849822130099));
#59221=CARTESIAN_POINT('Ctrl Pts',(-21.8153205367264,27.0819733074569,-3.93241072158309));
#59222=CARTESIAN_POINT('Ctrl Pts',(-21.9251718193941,27.131816670239,-3.92632322186519));
#59223=CARTESIAN_POINT('Ctrl Pts',(-22.0307710743358,27.1797307395676,-3.92047135178177));
#59224=CARTESIAN_POINT('Ctrl Pts',(-22.1385409513973,27.2229931830441,-3.91461948169836));
#59225=CARTESIAN_POINT('Ctrl Pts',(-22.2480324870229,27.2614129910729,-3.90876761161494));
#59226=CARTESIAN_POINT('Ctrl Pts',(-22.3575073515665,27.2998269493366,-3.90291663253196));
#59227=CARTESIAN_POINT('Ctrl Pts',(-22.4687029635005,27.3333996013773,-3.89706565344898));
#59228=CARTESIAN_POINT('Ctrl Pts',(-22.5811523878769,27.3619888698022,-3.891214674366));
#59229=CARTESIAN_POINT('Ctrl Pts',(-22.6936119225386,27.3905807086775,-3.8853631692237));
#59230=CARTESIAN_POINT('Ctrl Pts',(-22.8073250930779,27.4141881713822,-3.87951166408139));
#59231=CARTESIAN_POINT('Ctrl Pts',(-22.921812580521,27.4327198178113,-3.87366015893909));
#59232=CARTESIAN_POINT('Ctrl Pts',(-23.0363380867664,27.4512576181967,-3.8678067106393));
#59233=CARTESIAN_POINT('Ctrl Pts',(-23.1516380133544,27.4647161846424,-3.86195326233952));
#59234=CARTESIAN_POINT('Ctrl Pts',(-23.2672264032402,27.4730557654305,-3.85609981403973));
#59235=CARTESIAN_POINT('Ctrl Pts',(-23.3829462422248,27.4814048301329,-3.85023970909818));
#59236=CARTESIAN_POINT('Ctrl Pts',(-23.4989547867203,27.4846232600772,-3.84437960415663));
#59237=CARTESIAN_POINT('Ctrl Pts',(-23.6147644476646,27.4827234105054,-3.83851949921508));
#59238=CARTESIAN_POINT('Ctrl Pts',(-23.7306520991673,27.4808222815037,-3.83265544785962));
#59239=CARTESIAN_POINT('Ctrl Pts',(-23.8463401888123,27.4737960346405,-3.82679139650416));
#59240=CARTESIAN_POINT('Ctrl Pts',(-23.9613463677351,27.4617088919223,-3.8209273451487));
#59241=CARTESIAN_POINT('Ctrl Pts',(-24.0765220428081,27.4496039351687,-3.81505465135212));
#59242=CARTESIAN_POINT('Ctrl Pts',(-24.1910133941017,27.4324232574492,-3.80918195755554));
#59243=CARTESIAN_POINT('Ctrl Pts',(-24.3043482859667,27.4102821421231,-3.80330926375897));
#59244=CARTESIAN_POINT('Ctrl Pts',(-24.3353774834963,27.4042202751229,-3.80170141843573));
#59245=CARTESIAN_POINT('Ctrl Pts',(-24.3663200865554,27.3977868747735,-3.80009357311249));
#59246=CARTESIAN_POINT('Ctrl Pts',(-24.3971666276965,27.3909849506467,-3.79848572778926));
#59247=CARTESIAN_POINT('Ctrl Pts',(-24.5098267495501,27.3661424375926,-3.79261343082056));
#59248=CARTESIAN_POINT('Ctrl Pts',(-24.6215816235178,27.3362971184701,-3.78674113385187));
#59249=CARTESIAN_POINT('Ctrl Pts',(-24.7319528080094,27.3015287754486,-3.78086883688317));
#59250=CARTESIAN_POINT('Ctrl Pts',(-24.842180960212,27.2668054894384,-3.77500414994495));
#59251=CARTESIAN_POINT('Ctrl Pts',(-24.9510285982303,27.2271719898143,-3.76913946300673));
#59252=CARTESIAN_POINT('Ctrl Pts',(-25.0580275652196,27.1827590283543,-3.76327477606851));
#59253=CARTESIAN_POINT('Ctrl Pts',(-25.1649164904692,27.138391742845,-3.7574161205937));
#59254=CARTESIAN_POINT('Ctrl Pts',(-25.269960146855,27.0892549299618,-3.75155746511889));
#59255=CARTESIAN_POINT('Ctrl Pts',(-25.3727062875652,27.0355288920007,-3.74569880964408));
#59256=CARTESIAN_POINT('Ctrl Pts',(-25.4794657830293,26.9797042676756,-3.73961130992617));
#59257=CARTESIAN_POINT('Ctrl Pts',(-25.5837441841579,26.9189247277497,-3.73352381020827));
#59258=CARTESIAN_POINT('Ctrl Pts',(-25.6850575167591,26.8534474511233,-3.72743631049037));
#59259=CARTESIAN_POINT('Ctrl Pts',(-25.7824493011653,26.7905046118643,-3.72158444040697));
#59260=CARTESIAN_POINT('Ctrl Pts',(-25.8771009079708,26.7232211908274,-3.71573257032357));
#59261=CARTESIAN_POINT('Ctrl Pts',(-25.9686089537636,26.6518716598006,-3.70988070024017));
#59262=CARTESIAN_POINT('Ctrl Pts',(-26.0601030666242,26.5805329923888,-3.70402972115721));
#59263=CARTESIAN_POINT('Ctrl Pts',(-26.148454244243,26.5051297000753,-3.69817874207425));
#59264=CARTESIAN_POINT('Ctrl Pts',(-26.2332905563915,26.4259778242123,-3.69232776299129));
#59265=CARTESIAN_POINT('Ctrl Pts',(-26.318134496141,26.3468188318338,-3.68647625784899));
#59266=CARTESIAN_POINT('Ctrl Pts',(-26.3994626399264,26.2639108679347,-3.68062475270668));
#59267=CARTESIAN_POINT('Ctrl Pts',(-26.4769389654279,26.1776077643567,-3.67477324756437));
#59268=CARTESIAN_POINT('Ctrl Pts',(-26.5544410191304,26.0912760013968,-3.6689197992646));
#59269=CARTESIAN_POINT('Ctrl Pts',(-26.628088435124,26.0015471643409,-3.66306635096482));
#59270=CARTESIAN_POINT('Ctrl Pts',(-26.6975850892375,25.9088086095155,-3.65721290266504));
#59271=CARTESIAN_POINT('Ctrl Pts',(-26.7671607761376,25.8159645908156,-3.6513527977235));
#59272=CARTESIAN_POINT('Ctrl Pts',(-26.8325760315004,25.7201043537356,-3.64549269278197));
#59273=CARTESIAN_POINT('Ctrl Pts',(-26.8935776874398,25.6216447936664,-3.63963258784043));
#59274=CARTESIAN_POINT('Ctrl Pts',(-26.9546204241767,25.5231189272458,-3.63376853648498));
#59275=CARTESIAN_POINT('Ctrl Pts',(-27.0112434416218,25.4219906120911,-3.62790448512954));
#59276=CARTESIAN_POINT('Ctrl Pts',(-27.0632400408178,25.318700371112,-3.62204043377409));
#59277=CARTESIAN_POINT('Ctrl Pts',(-27.1153132726214,25.2152579009365,-3.61616773997752));
#59278=CARTESIAN_POINT('Ctrl Pts',(-27.1627463092014,25.1096475214814,-3.61029504618096));
#59279=CARTESIAN_POINT('Ctrl Pts',(-27.2053809310488,25.0023287639327,-3.6044223523844));
#59280=CARTESIAN_POINT('Ctrl Pts',(-27.2170535773205,24.9729466833391,-3.60281450706105));
#59281=CARTESIAN_POINT('Ctrl Pts',(-27.2283668383697,24.9434366266009,-3.60120666173771));
#59282=CARTESIAN_POINT('Ctrl Pts',(-27.2393181286426,24.9138081856414,-3.59959881641437));
#59283=CARTESIAN_POINT('Ctrl Pts',(-27.2854146357158,24.7890952427623,-3.59283102454024));
#59284=CARTESIAN_POINT('Ctrl Pts',(-27.3252216568937,24.6619388292607,-3.58606323266611));
#59285=CARTESIAN_POINT('Ctrl Pts',(-27.3585091715111,24.532937814626,-3.57929544079198));
#59286=CARTESIAN_POINT('Ctrl Pts',(-27.3916624030074,24.4044571950725,-3.57255495045197));
#59287=CARTESIAN_POINT('Ctrl Pts',(-27.4183485169574,24.2741469668576,-3.56581446011196));
#59288=CARTESIAN_POINT('Ctrl Pts',(-27.438386915938,24.142620668971,-3.55907396977195));
#59289=CARTESIAN_POINT('Ctrl Pts',(-27.4582772032158,24.0120665337798,-3.55238330105211));
#59290=CARTESIAN_POINT('Ctrl Pts',(-27.4716175947566,23.880314395183,-3.54569263233228));
#59291=CARTESIAN_POINT('Ctrl Pts',(-27.4782789309084,23.7479836801672,-3.53900196361245));
#59292=CARTESIAN_POINT('Ctrl Pts',(-27.4815440175391,23.6831211302845,-3.53572249947944));
#59293=CARTESIAN_POINT('Ctrl Pts',(-27.4832051818487,23.6181198580839,-3.53244303534644));
#59294=CARTESIAN_POINT('Ctrl Pts',(-27.4832515337037,23.5530543510895,-3.52916357121343));
#59295=CARTESIAN_POINT('',(-27.4787306259862,23.5475518707578,-2.27916352203481));
#59296=CARTESIAN_POINT('Ctrl Pts',(-27.4789192294965,23.5530502901666,-3.52916352203482));
#59297=CARTESIAN_POINT('Ctrl Pts',(-27.4733707979894,22.7044760387893,-3.48634631636971));
#59298=CARTESIAN_POINT('Ctrl Pts',(-26.7862294952183,20.5338307647598,-3.37723347357964));
#59299=CARTESIAN_POINT('Ctrl Pts',(-23.2036002208863,18.9112242921254,-3.20182499366464));
#59300=CARTESIAN_POINT('Ctrl Pts',(-19.4599799693547,21.3343055111431,-3.00293808228964));
#59301=CARTESIAN_POINT('Ctrl Pts',(-19.4749734046927,25.7936541607236,-2.8040511709148));
#59302=CARTESIAN_POINT('Ctrl Pts',(-23.2348028310531,28.1915069223165,-2.60516425953992));
#59303=CARTESIAN_POINT('Ctrl Pts',(-26.7973600627289,26.5490322383971,-2.4302017099133));
#59304=CARTESIAN_POINT('Ctrl Pts',(-27.4734464956764,24.3873896537201,-2.32153479741155));
#59305=CARTESIAN_POINT('Ctrl Pts',(-27.4787306259862,23.5475518707578,-2.27916352203481));
#59306=CARTESIAN_POINT('',(-27.4887831525091,23.5484783899485,-1.02916352203483));
#59307=CARTESIAN_POINT('Ctrl Pts',(-27.4787306259862,23.5475518707578,-2.27916352203481));
#59308=CARTESIAN_POINT('Ctrl Pts',(-27.4817142379717,23.0733489408066,-2.25523916028659));
#59309=CARTESIAN_POINT('Ctrl Pts',(-27.1823788944945,21.2887449913975,-2.16501916141351));
#59310=CARTESIAN_POINT('Ctrl Pts',(-24.5214140722119,19.0007914543429,-2.00850352541525));
#59311=CARTESIAN_POINT('Ctrl Pts',(-20.2476685784447,20.2740214556172,-1.80961661404031));
#59312=CARTESIAN_POINT('Ctrl Pts',(-19.0087177247742,24.5578300372182,-1.61072970266545));
#59313=CARTESIAN_POINT('Ctrl Pts',(-21.9430523000085,27.9157603197271,-1.41184279129057));
#59314=CARTESIAN_POINT('Ctrl Pts',(-26.2426709926684,27.278694135458,-1.21798739774704));
#59315=CARTESIAN_POINT('Ctrl Pts',(-27.4820131566245,24.7548508141379,-1.09042764132844));
#59316=CARTESIAN_POINT('Ctrl Pts',(-27.4887831525091,23.5484783899485,-1.02916352203483));
#59317=CARTESIAN_POINT('',(-27.4832509175595,23.553815786008,0.220836477965203));
#59318=CARTESIAN_POINT('Ctrl Pts',(-27.4887831525091,23.5484783899485,-1.02916352203483));
#59319=CARTESIAN_POINT('Ctrl Pts',(-27.4893391607469,23.4494010762854,-1.02413200420349));
#59320=CARTESIAN_POINT('Ctrl Pts',(-27.4409537024358,22.045426077291,-0.952804849247351));
#59321=CARTESIAN_POINT('Ctrl Pts',(-25.7609338543555,19.4571316048489,-0.815182057165814));
#59322=CARTESIAN_POINT('Ctrl Pts',(-21.3016081928786,19.477863862914,-0.616295145791017));
#59323=CARTESIAN_POINT('Ctrl Pts',(-18.9085960251757,23.2407760259621,-0.417408234416091));
#59324=CARTESIAN_POINT('Ctrl Pts',(-20.7808726393893,27.2880708585003,-0.21852132304123));
#59325=CARTESIAN_POINT('Ctrl Pts',(-25.1979745699378,27.9006275634348,-0.0196344116663155));
#59326=CARTESIAN_POINT('Ctrl Pts',(-27.3356200838471,25.4079940948567,0.126818188669141));
#59327=CARTESIAN_POINT('Ctrl Pts',(-27.4867411403313,23.8275935976074,0.206975151879653));
#59328=CARTESIAN_POINT('Ctrl Pts',(-27.4841962167909,23.553816642439,0.220836477965203));
#59329=CARTESIAN_POINT('',(-27.4832525295589,23.5503821330865,1.47083647793937));
#59330=CARTESIAN_POINT('Ctrl Pts',(-27.4832509175595,23.553815786008,0.220836477965203));
#59331=CARTESIAN_POINT('Ctrl Pts',(-27.4833542858497,23.4397213984313,0.226614518140672));
#59332=CARTESIAN_POINT('Ctrl Pts',(-27.4784887302081,23.3254706986072,0.232392558316141));
#59333=CARTESIAN_POINT('Ctrl Pts',(-27.4686401989256,23.2115386564409,0.23817059849161));
#59334=CARTESIAN_POINT('Ctrl Pts',(-27.4586996367026,23.0965419608061,0.244002632349603));
#59335=CARTESIAN_POINT('Ctrl Pts',(-27.4436824350315,22.9818703461215,0.249834666207596));
#59336=CARTESIAN_POINT('Ctrl Pts',(-27.4236280539117,22.8680127909239,0.255666700065589));
#59337=CARTESIAN_POINT('Ctrl Pts',(-27.4037855365418,22.7553580795567,0.261437121622734));
#59338=CARTESIAN_POINT('Ctrl Pts',(-27.3790118409753,22.6435007384169,0.26720754317988));
#59339=CARTESIAN_POINT('Ctrl Pts',(-27.3493971970699,22.5329085330647,0.272977964737026));
#59340=CARTESIAN_POINT('Ctrl Pts',(-27.319788509928,22.4223385725053,0.278747225617147));
#59341=CARTESIAN_POINT('Ctrl Pts',(-27.2853409196067,22.3130336535003,0.284516486497268));
#59342=CARTESIAN_POINT('Ctrl Pts',(-27.2461952705643,22.2054490995922,0.290285747377388));
#59343=CARTESIAN_POINT('Ctrl Pts',(-27.2070473908893,22.0978584152042,0.296055337006728));
#59344=CARTESIAN_POINT('Ctrl Pts',(-27.1632010670632,21.9919886908855,0.301824926636067));
#59345=CARTESIAN_POINT('Ctrl Pts',(-27.1148459892455,21.8882770558276,0.307594516265406));
#59346=CARTESIAN_POINT('Ctrl Pts',(-27.0655761090386,21.7826033589589,0.313473257500241));
#59347=CARTESIAN_POINT('Ctrl Pts',(-27.0116253273253,21.6791706589197,0.319351998735076));
#59348=CARTESIAN_POINT('Ctrl Pts',(-26.9532435959297,21.5784156173595,0.32523073996991));
#59349=CARTESIAN_POINT('Ctrl Pts',(-26.8958639473396,21.4793899677219,0.33100857660038));
#59350=CARTESIAN_POINT('Ctrl Pts',(-26.8342045364938,21.3829511128856,0.336786413230851));
#59351=CARTESIAN_POINT('Ctrl Pts',(-26.7685460230031,21.289483635102,0.34256424986132));
#59352=CARTESIAN_POINT('Ctrl Pts',(-26.701167511159,21.193567671976,0.348493443398336));
#59353=CARTESIAN_POINT('Ctrl Pts',(-26.6295777721164,21.1007813005844,0.354422636935352));
#59354=CARTESIAN_POINT('Ctrl Pts',(-26.5541226147364,21.0115021453419,0.360351830472368));
#59355=CARTESIAN_POINT('Ctrl Pts',(-26.4786674573564,20.9222229900995,0.366281024009383));
#59356=CARTESIAN_POINT('Ctrl Pts',(-26.3993472589769,20.8364513510652,0.372210217546399));
#59357=CARTESIAN_POINT('Ctrl Pts',(-26.3165455762268,20.7545215375228,0.378139411083413));
#59358=CARTESIAN_POINT('Ctrl Pts',(-26.234538458803,20.6733779228458,0.384011708052126));
#59359=CARTESIAN_POINT('Ctrl Pts',(-26.1488206543725,20.5957096994031,0.389884005020839));
#59360=CARTESIAN_POINT('Ctrl Pts',(-26.0597188269229,20.521875422893,0.395756301989552));
#59361=CARTESIAN_POINT('Ctrl Pts',(-25.9707324683655,20.4481368297416,0.401620988927755));
#59362=CARTESIAN_POINT('Ctrl Pts',(-25.8783711231886,20.3782225643042,0.407485675865959));
#59363=CARTESIAN_POINT('Ctrl Pts',(-25.7829986843189,20.3124548823746,0.413350362804161));
#59364=CARTESIAN_POINT('Ctrl Pts',(-25.6877243300318,20.2467548383885,0.419209018279003));
#59365=CARTESIAN_POINT('Ctrl Pts',(-25.5894453798566,20.185193128862,0.425067673753843));
#59366=CARTESIAN_POINT('Ctrl Pts',(-25.4885587108555,20.1280517550265,0.430926329228684));
#59367=CARTESIAN_POINT('Ctrl Pts',(-25.3837313197037,20.0686783887996,0.437013828946586));
#59368=CARTESIAN_POINT('Ctrl Pts',(-25.276088687191,20.0140780125991,0.443101328664488));
#59369=CARTESIAN_POINT('Ctrl Pts',(-25.1661094794257,19.9645175548076,0.44918882838239));
#59370=CARTESIAN_POINT('Ctrl Pts',(-25.0603872509999,19.9168754400298,0.455040698465796));
#59371=CARTESIAN_POINT('Ctrl Pts',(-24.9525063801961,19.8738905225357,0.460892568549203));
#59372=CARTESIAN_POINT('Ctrl Pts',(-24.8429163207115,19.8357526557266,0.466744438632609));
#59373=CARTESIAN_POINT('Ctrl Pts',(-24.7333429473099,19.7976205957545,0.472595417715589));
#59374=CARTESIAN_POINT('Ctrl Pts',(-24.6220612929769,19.764334254902,0.478446396798569));
#59375=CARTESIAN_POINT('Ctrl Pts',(-24.5095386567988,19.7360345082742,0.484297375881548));
#59376=CARTESIAN_POINT('Ctrl Pts',(-24.3970059037529,19.7077322172269,0.490148881023854));
#59377=CARTESIAN_POINT('Ctrl Pts',(-24.2832323479808,19.6844175125015,0.49600038616616));
#59378=CARTESIAN_POINT('Ctrl Pts',(-24.168697542221,19.6661806002086,0.501851891308466));
#59379=CARTESIAN_POINT('Ctrl Pts',(-24.0541247019454,19.6479376318341,0.507705339608255));
#59380=CARTESIAN_POINT('Ctrl Pts',(-23.9387905170403,19.6347758738111,0.513558787908044));
#59381=CARTESIAN_POINT('Ctrl Pts',(-23.8231810452553,19.626733826949,0.519412236207833));
#59382=CARTESIAN_POINT('Ctrl Pts',(-23.7074401003969,19.6186826345334,0.525272341149383));
#59383=CARTESIAN_POINT('Ctrl Pts',(-23.5914236564294,19.6157628029639,0.531132446090934));
#59384=CARTESIAN_POINT('Ctrl Pts',(-23.4756192689992,19.6179607220621,0.536992551032484));
#59385=CARTESIAN_POINT('Ctrl Pts',(-23.3597368945622,19.6201601213213,0.542856602387933));
#59386=CARTESIAN_POINT('Ctrl Pts',(-23.2440672725678,19.6274841078253,0.548720653743383));
#59387=CARTESIAN_POINT('Ctrl Pts',(-23.1290925849853,19.6398672182899,0.554584705098832));
#59388=CARTESIAN_POINT('Ctrl Pts',(-23.0139484476643,19.6522685789874,0.56045739889541));
#59389=CARTESIAN_POINT('Ctrl Pts',(-22.8995016959622,19.6697438824968,0.566330092691988));
#59390=CARTESIAN_POINT('Ctrl Pts',(-22.7862241672427,19.6921766306376,0.572202786488567));
#59391=CARTESIAN_POINT('Ctrl Pts',(-22.7552106747825,19.6983183418242,0.573810631811822));
#59392=CARTESIAN_POINT('Ctrl Pts',(-22.7242847327741,19.7048313622487,0.575418477135078));
#59393=CARTESIAN_POINT('Ctrl Pts',(-22.6934558008877,19.7117126579819,0.577026322458334));
#59394=CARTESIAN_POINT('Ctrl Pts',(-22.5808599929164,19.7368450581513,0.582898619427047));
#59395=CARTESIAN_POINT('Ctrl Pts',(-22.4691823062669,19.7669779178527,0.58877091639576));
#59396=CARTESIAN_POINT('Ctrl Pts',(-22.3589009755982,19.8020302237477,0.594643213364473));
#59397=CARTESIAN_POINT('Ctrl Pts',(-22.2487625607758,19.837037104638,0.600507900302673));
#59398=CARTESIAN_POINT('Ctrl Pts',(-22.1400172936811,19.8769506296518,0.606372587240873));
#59399=CARTESIAN_POINT('Ctrl Pts',(-22.0331329930736,19.9216388424824,0.612237274179074));
#59400=CARTESIAN_POINT('Ctrl Pts',(-21.9263586162782,19.9662810962835,0.61809592965389));
#59401=CARTESIAN_POINT('Ctrl Pts',(-21.8214417782464,20.0156881122291,0.623954585128706));
#59402=CARTESIAN_POINT('Ctrl Pts',(-21.7188342602223,20.069678424608,0.629813240603522));
#59403=CARTESIAN_POINT('Ctrl Pts',(-21.6122188021685,20.1257776461426,0.635900740321426));
#59404=CARTESIAN_POINT('Ctrl Pts',(-21.5080971834041,20.1868253809196,0.64198824003933));
#59405=CARTESIAN_POINT('Ctrl Pts',(-21.4069527145798,20.2525632052176,0.648075739757234));
#59406=CARTESIAN_POINT('Ctrl Pts',(-21.3097232577186,20.3157565070959,0.65392760984064));
#59407=CARTESIAN_POINT('Ctrl Pts',(-21.215245141355,20.3832833235894,0.659779479924045));
#59408=CARTESIAN_POINT('Ctrl Pts',(-21.1239210411182,20.4548681455736,0.665631350007451));
#59409=CARTESIAN_POINT('Ctrl Pts',(-21.0326108458059,20.5264420681178,0.67148232909043));
#59410=CARTESIAN_POINT('Ctrl Pts',(-20.9444540370291,20.6020725126803,0.677333308173409));
#59411=CARTESIAN_POINT('Ctrl Pts',(-20.8598217303437,20.6814424816657,0.683184287256388));
#59412=CARTESIAN_POINT('Ctrl Pts',(-20.7751818143996,20.760819586775,0.689035792398682));
#59413=CARTESIAN_POINT('Ctrl Pts',(-20.6940673320361,20.8439366018822,0.694887297540977));
#59414=CARTESIAN_POINT('Ctrl Pts',(-20.6168133937526,20.930438831449,0.700738802683271));
#59415=CARTESIAN_POINT('Ctrl Pts',(-20.5395338011181,21.016969786523,0.706592250983026));
#59416=CARTESIAN_POINT('Ctrl Pts',(-20.4661175769582,21.1068878832106,0.712445699282781));
#59417=CARTESIAN_POINT('Ctrl Pts',(-20.3968598474688,21.1998050042915,0.718299147582536));
#59418=CARTESIAN_POINT('Ctrl Pts',(-20.3275233569016,21.292827792316,0.724159252524087));
#59419=CARTESIAN_POINT('Ctrl Pts',(-20.2623550473619,21.3888560804346,0.730019357465638));
#59420=CARTESIAN_POINT('Ctrl Pts',(-20.2016070128739,21.4874723230232,0.735879462407188));
#59421=CARTESIAN_POINT('Ctrl Pts',(-20.1408180683868,21.586154977479,0.741743513762649));
#59422=CARTESIAN_POINT('Ctrl Pts',(-20.0844555268447,21.6874286963877,0.74760756511811));
#59423=CARTESIAN_POINT('Ctrl Pts',(-20.032724952684,21.7908524262881,0.75347161647357));
#59424=CARTESIAN_POINT('Ctrl Pts',(-19.9809181379835,21.8944285821209,0.759344310270141));
#59425=CARTESIAN_POINT('Ctrl Pts',(-19.9337570829936,22.0001606969211,0.765217004066713));
#59426=CARTESIAN_POINT('Ctrl Pts',(-19.8913988239385,22.1075888337928,0.771089697863284));
#59427=CARTESIAN_POINT('Ctrl Pts',(-19.8798018411765,22.1370008606147,0.772697543186596));
#59428=CARTESIAN_POINT('Ctrl Pts',(-19.868564571837,22.1665399381564,0.774305388509909));
#59429=CARTESIAN_POINT('Ctrl Pts',(-19.8576895767773,22.1961964678715,0.775913233833221));
#59430=CARTESIAN_POINT('Ctrl Pts',(-19.8179710792338,22.3045103380075,0.781785530801923));
#59431=CARTESIAN_POINT('Ctrl Pts',(-19.7829558356901,22.4147547376324,0.787657827770625));
#59432=CARTESIAN_POINT('Ctrl Pts',(-19.7528341943719,22.5264835287602,0.793530124739327));
#59433=CARTESIAN_POINT('Ctrl Pts',(-19.7227515883086,22.6380675282483,0.799394811677539));
#59434=CARTESIAN_POINT('Ctrl Pts',(-19.6975500796778,22.7511316983346,0.80525949861575));
#59435=CARTESIAN_POINT('Ctrl Pts',(-19.6773715272965,22.8652111272698,0.811124185553962));
#59436=CARTESIAN_POINT('Ctrl Pts',(-19.6572137272932,22.9791732326535,0.816982841028771));
#59437=CARTESIAN_POINT('Ctrl Pts',(-19.6420686800746,23.0941481154408,0.82284149650358));
#59438=CARTESIAN_POINT('Ctrl Pts',(-19.6320279224084,23.2096575945813,0.828700151978389));
#59439=CARTESIAN_POINT('Ctrl Pts',(-19.6215949639039,23.3296789757166,0.834787651696293));
#59440=CARTESIAN_POINT('Ctrl Pts',(-19.6166732984749,23.4502771292055,0.840875151414198));
#59441=CARTESIAN_POINT('Ctrl Pts',(-19.6173067598043,23.5709057487116,0.846962651132102));
#59442=CARTESIAN_POINT('Ctrl Pts',(-19.6179157016645,23.6868651807281,0.8528145212155));
#59443=CARTESIAN_POINT('Ctrl Pts',(-19.6236577182559,23.8028523121815,0.858666391298898));
#59444=CARTESIAN_POINT('Ctrl Pts',(-19.6345186823776,23.9183794409474,0.864518261382296));
#59445=CARTESIAN_POINT('Ctrl Pts',(-19.6453779928187,24.0338889796573,0.870369240465256));
#59446=CARTESIAN_POINT('Ctrl Pts',(-19.6613546623991,24.1489382434858,0.876220219548216));
#59447=CARTESIAN_POINT('Ctrl Pts',(-19.6823825994137,24.2630436560501,0.882071198631177));
#59448=CARTESIAN_POINT('Ctrl Pts',(-19.7034124270423,24.3771593277895,0.887922703773483));
#59449=CARTESIAN_POINT('Ctrl Pts',(-19.7294943500053,24.4903305730067,0.893774208915788));
#59450=CARTESIAN_POINT('Ctrl Pts',(-19.7605110984266,24.6020837296412,0.899625714058094));
#59451=CARTESIAN_POINT('Ctrl Pts',(-19.7915381468347,24.7138739970659,0.905479162357853));
#59452=CARTESIAN_POINT('Ctrl Pts',(-19.8275031687529,24.8242448414057,0.911332610657612));
#59453=CARTESIAN_POINT('Ctrl Pts',(-19.868239162872,24.932738174229,0.917186058957371));
#59454=CARTESIAN_POINT('Ctrl Pts',(-19.9090214826623,25.041354887531,0.923046163898914));
#59455=CARTESIAN_POINT('Ctrl Pts',(-19.9545854586558,25.1480894404129,0.928906268840457));
#59456=CARTESIAN_POINT('Ctrl Pts',(-20.0047160702204,25.2525040408314,0.934766373782001));
#59457=CARTESIAN_POINT('Ctrl Pts',(-20.0548804416144,25.3569889579484,0.940630425137458));
#59458=CARTESIAN_POINT('Ctrl Pts',(-20.1096173774465,25.4591504481802,0.946494476492915));
#59459=CARTESIAN_POINT('Ctrl Pts',(-20.168666928332,25.5585771586242,0.952358527848371));
#59460=CARTESIAN_POINT('Ctrl Pts',(-20.2278035064681,25.6581504041919,0.958231221644946));
#59461=CARTESIAN_POINT('Ctrl Pts',(-20.291265159128,25.7549804813868,0.964103915441522));
#59462=CARTESIAN_POINT('Ctrl Pts',(-20.3587498184206,25.8486866576085,0.969976609238097));
#59463=CARTESIAN_POINT('Ctrl Pts',(-20.3772259892545,25.8743418411452,0.971584454561435));
#59464=CARTESIAN_POINT('Ctrl Pts',(-20.396003490345,25.8997630680443,0.973192299884774));
#59465=CARTESIAN_POINT('Ctrl Pts',(-20.4150756305256,25.9249429953923,0.974800145208113));
#59466=CARTESIAN_POINT('Ctrl Pts',(-20.4847323750791,26.0169070723418,0.980672442176815));
#59467=CARTESIAN_POINT('Ctrl Pts',(-20.5585556146544,26.1059577558187,0.986544739145517));
#59468=CARTESIAN_POINT('Ctrl Pts',(-20.636272897164,26.1916937461722,0.992417036114219));
#59469=CARTESIAN_POINT('Ctrl Pts',(-20.7138894642477,26.2773186294914,0.998281723052427));
#59470=CARTESIAN_POINT('Ctrl Pts',(-20.7953897637771,26.3596370586016,1.00414640999064));
#59471=CARTESIAN_POINT('Ctrl Pts',(-20.8804593384015,26.4382783807904,1.01001109692884));
#59472=CARTESIAN_POINT('Ctrl Pts',(-20.9654414242936,26.5168388253022,1.01586975240365));
#59473=CARTESIAN_POINT('Ctrl Pts',(-21.0539851821937,26.5917294059123,1.02172840787846));
#59474=CARTESIAN_POINT('Ctrl Pts',(-21.1457377898646,26.6626146340731,1.02758706335327));
#59475=CARTESIAN_POINT('Ctrl Pts',(-21.2410743352061,26.7362687016809,1.03367456307118));
#59476=CARTESIAN_POINT('Ctrl Pts',(-21.3398752163534,26.8055977958626,1.03976206278909));
#59477=CARTESIAN_POINT('Ctrl Pts',(-21.4417045105835,26.870269736871,1.04584956250699));
#59478=CARTESIAN_POINT('Ctrl Pts',(-21.5395922852253,26.9324384127412,1.05170143259039));
#59479=CARTESIAN_POINT('Ctrl Pts',(-21.6402780083667,26.9903035194359,1.05755330267378));
#59480=CARTESIAN_POINT('Ctrl Pts',(-21.7433437316768,27.0436133187329,1.06340517275718));
#59481=CARTESIAN_POINT('Ctrl Pts',(-21.8463937622933,27.0969150011283,1.06925615184014));
#59482=CARTESIAN_POINT('Ctrl Pts',(-21.9518227054845,27.1456625653336,1.0751071309231));
#59483=CARTESIAN_POINT('Ctrl Pts',(-22.0591879949576,27.1896502218741,1.08095811000606));
#59484=CARTESIAN_POINT('Ctrl Pts',(-22.1665629376033,27.2336418333281,1.08680961514834));
#59485=CARTESIAN_POINT('Ctrl Pts',(-22.2758741900719,27.2728725296398,1.09266112029062));
#59486=CARTESIAN_POINT('Ctrl Pts',(-22.386659863185,27.3071849374997,1.0985126254329));
#59487=CARTESIAN_POINT('Ctrl Pts',(-22.497482325809,27.3415087397636,1.10436607373268));
#59488=CARTESIAN_POINT('Ctrl Pts',(-22.6097797879941,27.3709108837117,1.11021952203246));
#59489=CARTESIAN_POINT('Ctrl Pts',(-22.7230765809695,27.3952842541307,1.11607297033224));
#59490=CARTESIAN_POINT('Ctrl Pts',(-22.8365022170003,27.4196853423643,1.12193307527378));
#59491=CARTESIAN_POINT('Ctrl Pts',(-22.950929047777,27.4390461555089,1.12779318021532));
#59492=CARTESIAN_POINT('Ctrl Pts',(-23.0658725237412,27.4533109488711,1.13365328515686));
#59493=CARTESIAN_POINT('Ctrl Pts',(-23.1808934069419,27.4675853486788,1.13951733651228));
#59494=CARTESIAN_POINT('Ctrl Pts',(-23.2964312170446,27.4767568625767,1.14538138786771));
#59495=CARTESIAN_POINT('Ctrl Pts',(-23.4119993622882,27.4808218366613,1.15124543922313));
#59496=CARTESIAN_POINT('Ctrl Pts',(-23.527737831909,27.4848928017062,1.15711813301971));
#59497=CARTESIAN_POINT('Ctrl Pts',(-23.6435063140853,27.4838422101904,1.16299082681629));
#59498=CARTESIAN_POINT('Ctrl Pts',(-23.7588212115915,27.4777183947878,1.16886352061288));
#59499=CARTESIAN_POINT('Ctrl Pts',(-23.790392501547,27.4760417965695,1.17047136593626));
#59500=CARTESIAN_POINT('Ctrl Pts',(-23.8219298416358,27.4739852206697,1.17207921125964));
#59501=CARTESIAN_POINT('Ctrl Pts',(-23.8534234372826,27.4715503273232,1.17368705658302));
#59502=CARTESIAN_POINT('Ctrl Pts',(-23.9684467816063,27.4626574216374,1.17955935355172));
#59503=CARTESIAN_POINT('Ctrl Pts',(-24.0832712063095,27.4486843611038,1.18543165052042));
#59504=CARTESIAN_POINT('Ctrl Pts',(-24.1974118193595,27.4296434447614,1.19130394748912));
#59505=CARTESIAN_POINT('Ctrl Pts',(-24.3114045152403,27.4106272039344,1.19716863442735));
#59506=CARTESIAN_POINT('Ctrl Pts',(-24.4247147577485,27.386556235168,1.20303332136557));
#59507=CARTESIAN_POINT('Ctrl Pts',(-24.5368607330095,27.3574947432034,1.20889800830379));
#59508=CARTESIAN_POINT('Ctrl Pts',(-24.648891373155,27.3284631391641,1.21475666377861));
#59509=CARTESIAN_POINT('Ctrl Pts',(-24.7597597299366,27.2944513236904,1.22061531925343));
#59510=CARTESIAN_POINT('Ctrl Pts',(-24.8689928358335,27.2555747862678,1.22647397472825));
#59511=CARTESIAN_POINT('Ctrl Pts',(-24.982492683058,27.2151796970515,1.23256147444615));
#59512=CARTESIAN_POINT('Ctrl Pts',(-25.0942264779404,27.1695321725109,1.23864897416405));
#59513=CARTESIAN_POINT('Ctrl Pts',(-25.203679117374,27.1188194045112,1.24473647388195));
#59514=CARTESIAN_POINT('Ctrl Pts',(-25.3088951594163,27.0700695821448,1.25058834396536));
#59515=CARTESIAN_POINT('Ctrl Pts',(-25.4120029462824,27.0166395371803,1.25644021404876));
#59516=CARTESIAN_POINT('Ctrl Pts',(-25.5125647675914,26.9587448213801,1.26229208413216));
#59517=CARTESIAN_POINT('Ctrl Pts',(-25.6131112774487,26.9008589205767,1.26814306321514));
#59518=CARTESIAN_POINT('Ctrl Pts',(-25.7111122343585,26.8385099067658,1.27399404229811));
#59519=CARTESIAN_POINT('Ctrl Pts',(-25.8061552783399,26.7719588804598,1.27984502138109));
#59520=CARTESIAN_POINT('Ctrl Pts',(-25.9012068676054,26.7054018705761,1.28569652652338));
#59521=CARTESIAN_POINT('Ctrl Pts',(-25.993299676627,26.6346423342866,1.29154803166567));
#59522=CARTESIAN_POINT('Ctrl Pts',(-26.0820516339175,26.5599837997614,1.29739953680796));
#59523=CARTESIAN_POINT('Ctrl Pts',(-26.170833063801,26.485300472762,1.30325298510774));
#59524=CARTESIAN_POINT('Ctrl Pts',(-26.2562711197593,26.4067158389205,1.30910643340751));
#59525=CARTESIAN_POINT('Ctrl Pts',(-26.3380185648302,26.3245721860407,1.31495988170728));
#59526=CARTESIAN_POINT('Ctrl Pts',(-26.4198589744973,26.2423351179903,1.32081998664883));
#59527=CARTESIAN_POINT('Ctrl Pts',(-26.4980001043688,26.1565312456439,1.32668009159037));
#59528=CARTESIAN_POINT('Ctrl Pts',(-26.5721331359211,26.0675380963049,1.33254019653192));
#59529=CARTESIAN_POINT('Ctrl Pts',(-26.64631609143,25.97848501565,1.33840424788735));
#59530=CARTESIAN_POINT('Ctrl Pts',(-26.7164853243102,25.8862387095584,1.34426829924277));
#59531=CARTESIAN_POINT('Ctrl Pts',(-26.7823747369962,25.7912065807531,1.3501323505982));
#59532=CARTESIAN_POINT('Ctrl Pts',(-26.8483612575241,25.6960343935597,1.35600504439478));
#59533=CARTESIAN_POINT('Ctrl Pts',(-26.9100551496453,25.5980685378605,1.36187773819136));
#59534=CARTESIAN_POINT('Ctrl Pts',(-26.9672356716477,25.4977419979746,1.36775043198794));
#59535=CARTESIAN_POINT('Ctrl Pts',(-26.9828907420586,25.470274269612,1.36935827731127));
#59536=CARTESIAN_POINT('Ctrl Pts',(-26.9982077795287,25.4426297097966,1.3709661226346));
#59537=CARTESIAN_POINT('Ctrl Pts',(-27.0131828864579,25.4148174562963,1.37257396795793));
#59538=CARTESIAN_POINT('Ctrl Pts',(-27.0708508582076,25.3077146318063,1.37876565521078));
#59539=CARTESIAN_POINT('Ctrl Pts',(-27.1236204990138,25.1977965269381,1.38495734246363));
#59540=CARTESIAN_POINT('Ctrl Pts',(-27.1712229605583,25.0855251958459,1.39114902971648));
#59541=CARTESIAN_POINT('Ctrl Pts',(-27.2187367175758,24.9734630761055,1.39732917910613));
#59542=CARTESIAN_POINT('Ctrl Pts',(-27.2611023414214,24.8590567836819,1.40350932849577));
#59543=CARTESIAN_POINT('Ctrl Pts',(-27.2980967767422,24.7427928936361,1.40968947788542));
#59544=CARTESIAN_POINT('Ctrl Pts',(-27.335001395954,24.6268112722648,1.41585462293816));
#59545=CARTESIAN_POINT('Ctrl Pts',(-27.366560718547,24.508981373887,1.4220197679909));
#59546=CARTESIAN_POINT('Ctrl Pts',(-27.3926000459075,24.3898087120767,1.42818491304364));
#59547=CARTESIAN_POINT('Ctrl Pts',(-27.4186007329442,24.2708128931694,1.43434090950364));
#59548=CARTESIAN_POINT('Ctrl Pts',(-27.4390976638491,24.1504786166865,1.44049690596364));
#59549=CARTESIAN_POINT('Ctrl Pts',(-27.453965740447,24.0293268305339,1.44665290242364));
#59550=CARTESIAN_POINT('Ctrl Pts',(-27.468806040479,23.9084013803542,1.4527973982406));
#59551=CARTESIAN_POINT('Ctrl Pts',(-27.4780384049081,23.7866618085343,1.45894189405755));
#59552=CARTESIAN_POINT('Ctrl Pts',(-27.4815887897958,23.6646388321663,1.4650863898745));
#59553=CARTESIAN_POINT('Ctrl Pts',(-27.482696286455,23.6265753424482,1.46700308589613));
#59554=CARTESIAN_POINT('Ctrl Pts',(-27.4832512740033,23.5884843489477,1.46891978191775));
#59555=CARTESIAN_POINT('Ctrl Pts',(-27.4832525295589,23.5503821330864,1.47083647793938));
#59556=CARTESIAN_POINT('',(-27.4832508767861,23.5466445538181,2.72083647796517));
#59557=CARTESIAN_POINT('Ctrl Pts',(-27.4832525295589,23.5503821325739,1.47083647796516));
#59558=CARTESIAN_POINT('Ctrl Pts',(-27.4832565348913,23.4288322440574,1.47695093043155));
#59559=CARTESIAN_POINT('Ctrl Pts',(-27.4776214550004,23.3073853627606,1.48306538289793));
#59560=CARTESIAN_POINT('Ctrl Pts',(-27.4664017061686,23.1865704682608,1.48917983536432));
#59561=CARTESIAN_POINT('Ctrl Pts',(-27.4551673184688,23.0655979415951,1.49530226560852));
#59562=CARTESIAN_POINT('Ctrl Pts',(-27.4383337613979,22.9452594005174,1.50142469585272));
#59563=CARTESIAN_POINT('Ctrl Pts',(-27.4160068384167,22.8260753157752,1.50754712609692));
#59564=CARTESIAN_POINT('Ctrl Pts',(-27.3936277081329,22.7066125415072,1.51368387249068));
#59565=CARTESIAN_POINT('Ctrl Pts',(-27.36572960262,22.5883099702222,1.51982061888443));
#59566=CARTESIAN_POINT('Ctrl Pts',(-27.3324690086286,22.4716759133652,1.52595736527819));
#59567=CARTESIAN_POINT('Ctrl Pts',(-27.2991660722478,22.3548933755562,1.53210192405514));
#59568=CARTESIAN_POINT('Ctrl Pts',(-27.2604871411608,22.2397839267865,1.53824648283209));
#59569=CARTESIAN_POINT('Ctrl Pts',(-27.216637287345,22.1268369832575,1.54439104160904));
#59570=CARTESIAN_POINT('Ctrl Pts',(-27.1726892208608,22.013637066919,1.55054936265568));
#59571=CARTESIAN_POINT('Ctrl Pts',(-27.1235472255114,21.9026096631,1.55670768370233));
#59572=CARTESIAN_POINT('Ctrl Pts',(-27.0694633883307,21.7942217954791,1.56286600474897));
#59573=CARTESIAN_POINT('Ctrl Pts',(-27.0443026454344,21.7437978719478,1.56573096294358));
#59574=CARTESIAN_POINT('Ctrl Pts',(-27.0180729803856,21.6939448245498,1.5685959211382));
#59575=CARTESIAN_POINT('Ctrl Pts',(-26.9908029476806,21.6447075085956,1.57146087933281));
#59576=CARTESIAN_POINT('Ctrl Pts',(-26.9349076362968,21.5437859168715,1.57733317630148));
#59577=CARTESIAN_POINT('Ctrl Pts',(-26.874474423979,21.4451567032586,1.58320547327015));
#59578=CARTESIAN_POINT('Ctrl Pts',(-26.8097160317601,21.3492557820968,1.58907777023883));
#59579=CARTESIAN_POINT('Ctrl Pts',(-26.7450415612745,21.2534791409125,1.594942457177));
#59580=CARTESIAN_POINT('Ctrl Pts',(-26.6760532866023,21.1604241004678,1.60080714411518));
#59581=CARTESIAN_POINT('Ctrl Pts',(-26.6030098594493,21.0705022019559,1.60667183105336));
#59582=CARTESIAN_POINT('Ctrl Pts',(-26.5300415528889,20.9806727824878,1.61253048652813));
#59583=CARTESIAN_POINT('Ctrl Pts',(-26.4530266481982,20.8939704146855,1.6183891420029));
#59584=CARTESIAN_POINT('Ctrl Pts',(-26.3722667655501,20.8107772783081,1.62424779747767));
#59585=CARTESIAN_POINT('Ctrl Pts',(-26.2883523307525,20.7243345447474,1.63033529719559));
#59586=CARTESIAN_POINT('Ctrl Pts',(-26.2003946439296,20.6416811555589,1.6364227969135));
#59587=CARTESIAN_POINT('Ctrl Pts',(-26.1087780537844,20.5632078127767,1.64251029663142));
#59588=CARTESIAN_POINT('Ctrl Pts',(-26.0207076787775,20.4877719477666,1.64836216671479));
#59589=CARTESIAN_POINT('Ctrl Pts',(-25.929256728141,20.4161988449634,1.65421403679816));
#59590=CARTESIAN_POINT('Ctrl Pts',(-25.8348031783186,20.3487970278634,1.66006590688154));
#59591=CARTESIAN_POINT('Ctrl Pts',(-25.740364009908,20.2814054733031,1.66591688596448));
#59592=CARTESIAN_POINT('Ctrl Pts',(-25.6429234877185,20.2181841816864,1.67176786504742));
#59593=CARTESIAN_POINT('Ctrl Pts',(-25.5428904800334,20.1593996881107,1.67761884413036));
#59594=CARTESIAN_POINT('Ctrl Pts',(-25.4428484784184,20.1006099092434,1.68347034927262));
#59595=CARTESIAN_POINT('Ctrl Pts',(-25.3402138843688,20.0462579308662,1.68932185441488));
#59596=CARTESIAN_POINT('Ctrl Pts',(-25.2354215668566,19.9965651055227,1.69517335955713));
#59597=CARTESIAN_POINT('Ctrl Pts',(-25.1305944500972,19.9468557782736,1.70102680785686));
#59598=CARTESIAN_POINT('Ctrl Pts',(-25.0236085584117,19.9018088576026,1.70688025615659));
#59599=CARTESIAN_POINT('Ctrl Pts',(-24.9149195358079,19.8615979032581,1.71273370445632));
#59600=CARTESIAN_POINT('Ctrl Pts',(-24.8061069101838,19.8213412203267,1.71859380939783));
#59601=CARTESIAN_POINT('Ctrl Pts',(-24.6955876757186,19.7859316241654,1.72445391433934));
#59602=CARTESIAN_POINT('Ctrl Pts',(-24.5838335601979,19.7554930850998,1.73031401928085));
#59603=CARTESIAN_POINT('Ctrl Pts',(-24.4720041852746,19.7250340475833,1.73617807063628));
#59604=CARTESIAN_POINT('Ctrl Pts',(-24.3589386756682,19.699552823751,1.74204212199172));
#59605=CARTESIAN_POINT('Ctrl Pts',(-24.2451181758774,19.6791221106758,1.74790617334715));
#59606=CARTESIAN_POINT('Ctrl Pts',(-24.1311299273907,19.658661286808,1.7537788671437));
#59607=CARTESIAN_POINT('Ctrl Pts',(-24.0163848761487,19.6432658841415,1.75965156094026));
#59608=CARTESIAN_POINT('Ctrl Pts',(-23.9013685828456,19.6329567146,1.76552425473681));
#59609=CARTESIAN_POINT('Ctrl Pts',(-23.8698790457211,19.6301342364304,1.76713210006043));
#59610=CARTESIAN_POINT('Ctrl Pts',(-23.838369170144,19.6276927070489,1.76873994538405));
#59611=CARTESIAN_POINT('Ctrl Pts',(-23.8068488871828,19.6256318735477,1.77034779070766));
#59612=CARTESIAN_POINT('Ctrl Pts',(-23.691728073404,19.6181051381433,1.77622008767637));
#59613=CARTESIAN_POINT('Ctrl Pts',(-23.576082947962,19.6156353424828,1.78209238464508));
#59614=CARTESIAN_POINT('Ctrl Pts',(-23.4603952376413,19.6182791509723,1.78796468161378));
#59615=CARTESIAN_POINT('Ctrl Pts',(-23.3448574494052,19.620919533296,1.79382936855199));
#59616=CARTESIAN_POINT('Ctrl Pts',(-23.2292775954971,19.6286603320366,1.7996940554902));
#59617=CARTESIAN_POINT('Ctrl Pts',(-23.1141417246397,19.6415063946356,1.80555874242841));
#59618=CARTESIAN_POINT('Ctrl Pts',(-22.9991242638178,19.6543392458635,1.81141739790324));
#59619=CARTESIAN_POINT('Ctrl Pts',(-22.884550286192,19.6722668719838,1.81727605337807));
#59620=CARTESIAN_POINT('Ctrl Pts',(-22.7709043644959,19.695242099246,1.8231347088529));
#59621=CARTESIAN_POINT('Ctrl Pts',(-22.6528193330005,19.7191147591213,1.82922220857081));
#59622=CARTESIAN_POINT('Ctrl Pts',(-22.5357367913787,19.748437376039,1.83530970828871));
#59623=CARTESIAN_POINT('Ctrl Pts',(-22.4201932005747,19.7830977819992,1.84139720800661));
#59624=CARTESIAN_POINT('Ctrl Pts',(-22.3091219704004,19.816416583168,1.84724907809001));
#59625=CARTESIAN_POINT('Ctrl Pts',(-22.1994732024405,19.8546675060611,1.8531009481734));
#59626=CARTESIAN_POINT('Ctrl Pts',(-22.0917107749805,19.8976993227837,1.85895281825679));
#59627=CARTESIAN_POINT('Ctrl Pts',(-21.9839647553298,19.9407245875209,1.86480379733975));
#59628=CARTESIAN_POINT('Ctrl Pts',(-21.8781048889094,19.988529145461,1.87065477642272));
#59629=CARTESIAN_POINT('Ctrl Pts',(-21.774576426809,20.0409130823762,1.87650575550569));
#59630=CARTESIAN_POINT('Ctrl Pts',(-21.6710386565036,20.0933017291114,1.88235726064798));
#59631=CARTESIAN_POINT('Ctrl Pts',(-21.5698330760904,20.1502703866578,1.88820876579028));
#59632=CARTESIAN_POINT('Ctrl Pts',(-21.4713809782929,20.2115728428862,1.89406027093257));
#59633=CARTESIAN_POINT('Ctrl Pts',(-21.372896186697,20.2728956563258,1.89991371923234));
#59634=CARTESIAN_POINT('Ctrl Pts',(-21.2771670466177,20.3385549117402,1.9057671675321));
#59635=CARTESIAN_POINT('Ctrl Pts',(-21.1845858716859,20.4082610845822,1.91162061583187));
#59636=CARTESIAN_POINT('Ctrl Pts',(-21.0918994118545,20.4780465284792,1.9174807207734));
#59637=CARTESIAN_POINT('Ctrl Pts',(-21.0023683930215,20.5518878269099,1.92334082571494));
#59638=CARTESIAN_POINT('Ctrl Pts',(-20.9163521023681,20.6294551185901,1.92920093065647));
#59639=CARTESIAN_POINT('Ctrl Pts',(-20.8302778851264,20.7070746469865,1.93506498201192));
#59640=CARTESIAN_POINT('Ctrl Pts',(-20.7477234028567,20.7884248755529,1.94092903336736));
#59641=CARTESIAN_POINT('Ctrl Pts',(-20.6690098958248,20.8731403051994,1.94679308472281));
#59642=CARTESIAN_POINT('Ctrl Pts',(-20.5901803807961,20.9579805884783,1.95266577851937));
#59643=CARTESIAN_POINT('Ctrl Pts',(-20.5152034056408,21.0461956575109,1.95853847231594));
#59644=CARTESIAN_POINT('Ctrl Pts',(-20.4443589459188,21.1373882516653,1.96441116611251));
#59645=CARTESIAN_POINT('Ctrl Pts',(-20.4249629179298,21.1623552584793,1.96601901143586));
#59646=CARTESIAN_POINT('Ctrl Pts',(-20.4058763947519,21.1875452953443,1.96762685675921));
#59647=CARTESIAN_POINT('Ctrl Pts',(-20.3871045317731,21.2129498703781,1.96923470208257));
#59648=CARTESIAN_POINT('Ctrl Pts',(-20.3185444828267,21.3057344229689,1.97510699905128));
#59649=CARTESIAN_POINT('Ctrl Pts',(-20.2539555094522,21.4016935780694,1.98097929602));
#59650=CARTESIAN_POINT('Ctrl Pts',(-20.1936456781143,21.5004526803671,1.98685159298872));
#59651=CARTESIAN_POINT('Ctrl Pts',(-20.1334140035282,21.5990837987113,1.99271627992692));
#59652=CARTESIAN_POINT('Ctrl Pts',(-20.0774506565707,21.7005072989065,1.99858096686513));
#59653=CARTESIAN_POINT('Ctrl Pts',(-20.0260224454153,21.8043168802549,2.00444565380333));
#59654=CARTESIAN_POINT('Ctrl Pts',(-19.9746471249556,21.9080196999476,2.01030430927816));
#59655=CARTESIAN_POINT('Ctrl Pts',(-19.9277978455624,22.0141033515988,2.01616296475299));
#59656=CARTESIAN_POINT('Ctrl Pts',(-19.8856968512728,22.1221346566254,2.02202162022782));
#59657=CARTESIAN_POINT('Ctrl Pts',(-19.8419513550642,22.2343857595787,2.02810911994572));
#59658=CARTESIAN_POINT('Ctrl Pts',(-19.8033328874315,22.3487393838029,2.03419661966362));
#59659=CARTESIAN_POINT('Ctrl Pts',(-19.7700370594367,22.4646835641454,2.04028411938152));
#59660=CARTESIAN_POINT('Ctrl Pts',(-19.7380300173382,22.5761398781879,2.04613598946493));
#59661=CARTESIAN_POINT('Ctrl Pts',(-19.7109413531281,22.6890654717823,2.05198785954834));
#59662=CARTESIAN_POINT('Ctrl Pts',(-19.6888945821195,22.802988331256,2.05783972963174));
#59663=CARTESIAN_POINT('Ctrl Pts',(-19.6668511679323,22.9168938449386,2.06369070871472));
#59664=CARTESIAN_POINT('Ctrl Pts',(-19.6498481990855,23.0317959168469,2.0695416877977));
#59665=CARTESIAN_POINT('Ctrl Pts',(-19.6379581614747,23.1472118876537,2.07539266688068));
#59666=CARTESIAN_POINT('Ctrl Pts',(-19.6260670548351,23.2626382354668,2.08124417202299));
#59667=CARTESIAN_POINT('Ctrl Pts',(-19.6192898356407,23.3785781627976,2.08709567716529));
#59668=CARTESIAN_POINT('Ctrl Pts',(-19.6176470880733,23.4945441409154,2.0929471823076));
#59669=CARTESIAN_POINT('Ctrl Pts',(-19.6160037949852,23.6105486288105,2.0988006306074));
#59670=CARTESIAN_POINT('Ctrl Pts',(-19.6194983697534,23.7265787715718,2.1046540789072));
#59671=CARTESIAN_POINT('Ctrl Pts',(-19.6280992926678,23.8421480088679,2.110507527207));
#59672=CARTESIAN_POINT('Ctrl Pts',(-19.6367099966991,23.9578486734819,2.11636763214855));
#59673=CARTESIAN_POINT('Ctrl Pts',(-19.650438608828,24.0730869739565,2.12222773709011));
#59674=CARTESIAN_POINT('Ctrl Pts',(-19.6692018211744,24.18738233195,2.12808784203166));
#59675=CARTESIAN_POINT('Ctrl Pts',(-19.68797766937,24.3017546607135,2.1339518933871));
#59676=CARTESIAN_POINT('Ctrl Pts',(-19.7117947841775,24.4151823789874,2.13981594474255));
#59677=CARTESIAN_POINT('Ctrl Pts',(-19.7405193090625,24.5271976541939,2.14567999609799));
#59678=CARTESIAN_POINT('Ctrl Pts',(-19.7692861681632,24.6393780175559,2.15155268989457));
#59679=CARTESIAN_POINT('Ctrl Pts',(-19.8029747522637,24.7501413892508,2.15742538369115));
#59680=CARTESIAN_POINT('Ctrl Pts',(-19.8414021779883,24.8590374849297,2.16329807748773));
#59681=CARTESIAN_POINT('Ctrl Pts',(-19.8519229643388,24.8888514143157,2.16490592281098));
#59682=CARTESIAN_POINT('Ctrl Pts',(-19.8627986900844,24.9185255093086,2.16651376813422));
#59683=CARTESIAN_POINT('Ctrl Pts',(-19.8740249975681,24.9480508423717,2.16812161345746));
#59684=CARTESIAN_POINT('Ctrl Pts',(-19.9150265855024,25.0558855459591,2.17399391042616));
#59685=CARTESIAN_POINT('Ctrl Pts',(-19.9608455544848,25.1620953242776,2.17986620739486));
#59686=CARTESIAN_POINT('Ctrl Pts',(-20.0113332236989,25.2662184787625,2.18573850436356));
#59687=CARTESIAN_POINT('Ctrl Pts',(-20.0617554649033,25.3702066979084,2.19160319130175));
#59688=CARTESIAN_POINT('Ctrl Pts',(-20.1168341958406,25.4721133021733,2.19746787823994));
#59689=CARTESIAN_POINT('Ctrl Pts',(-20.1763718100455,25.5714941986126,2.20333256517813));
#59690=CARTESIAN_POINT('Ctrl Pts',(-20.2358481935414,25.6707728880215,2.20919122065295));
#59691=CARTESIAN_POINT('Ctrl Pts',(-20.2997741279791,25.7675306837463,2.21504987612777));
#59692=CARTESIAN_POINT('Ctrl Pts',(-20.3679053052723,25.8613464567619,2.22090853160259));
#59693=CARTESIAN_POINT('Ctrl Pts',(-20.4386977463598,25.9588267565034,2.22699603132049));
#59694=CARTESIAN_POINT('Ctrl Pts',(-20.5140304501644,26.0531301029606,2.2330835310384));
#59695=CARTESIAN_POINT('Ctrl Pts',(-20.5935784278852,26.1438151863963,2.23917103075631));
#59696=CARTESIAN_POINT('Ctrl Pts',(-20.6700473318014,26.2309901106441,2.2450229008397));
#59697=CARTESIAN_POINT('Ctrl Pts',(-20.7504109570101,26.3148213289378,2.25087477092309));
#59698=CARTESIAN_POINT('Ctrl Pts',(-20.8343389557518,26.3949497823717,2.25672664100648));
#59699=CARTESIAN_POINT('Ctrl Pts',(-20.9182541756929,26.4750660355201,2.26257762008945));
#59700=CARTESIAN_POINT('Ctrl Pts',(-21.0057323911758,26.551480359402,2.26842859917242));
#59701=CARTESIAN_POINT('Ctrl Pts',(-21.0964067145099,26.6238708725893,2.27427957825539));
#59702=CARTESIAN_POINT('Ctrl Pts',(-21.1870891903378,26.6962678943801,2.28013108339766));
#59703=CARTESIAN_POINT('Ctrl Pts',(-21.280968022188,26.7646401283626,2.28598258853994));
#59704=CARTESIAN_POINT('Ctrl Pts',(-21.3776441705826,26.8287067267727,2.29183409368221));
#59705=CARTESIAN_POINT('Ctrl Pts',(-21.4743524230222,26.892794600306,2.297687541982));
#59706=CARTESIAN_POINT('Ctrl Pts',(-21.5738594947173,26.9525737669501,2.30354099028179));
#59707=CARTESIAN_POINT('Ctrl Pts',(-21.6757389965578,27.0078077382803,2.30939443858158));
#59708=CARTESIAN_POINT('Ctrl Pts',(-21.7777343575141,27.0631045226294,2.31525454352312));
#59709=CARTESIAN_POINT('Ctrl Pts',(-21.8821071700526,27.1138455976081,2.32111464846465));
#59710=CARTESIAN_POINT('Ctrl Pts',(-21.9884080841103,27.1598412785671,2.32697475340619));
#59711=CARTESIAN_POINT('Ctrl Pts',(-22.0947805851808,27.2058679347385,2.33283880476165));
#59712=CARTESIAN_POINT('Ctrl Pts',(-22.2030833879159,27.2471426867111,2.33870285611711));
#59713=CARTESIAN_POINT('Ctrl Pts',(-22.3128505417866,27.2835252668922,2.34456690747257));
#59714=CARTESIAN_POINT('Ctrl Pts',(-22.4227794705302,27.3199614677337,2.35043960126913));
#59715=CARTESIAN_POINT('Ctrl Pts',(-22.5341766614188,27.3514909946883,2.3563122950657));
#59716=CARTESIAN_POINT('Ctrl Pts',(-22.6465644264571,27.3780243128292,2.36218498886226));
#59717=CARTESIAN_POINT('Ctrl Pts',(-22.6773343165076,27.3852886914881,2.36379283418562));
#59718=CARTESIAN_POINT('Ctrl Pts',(-22.708178421327,27.392178867261,2.36540067950899));
#59719=CARTESIAN_POINT('Ctrl Pts',(-22.7390868745305,27.3986936806061,2.36700852483235));
#59720=CARTESIAN_POINT('Ctrl Pts',(-22.8519731163951,27.4224875854688,2.37288082180105));
#59721=CARTESIAN_POINT('Ctrl Pts',(-22.9660962800474,27.4413502058351,2.37875311876975));
#59722=CARTESIAN_POINT('Ctrl Pts',(-23.080987562454,27.4551570617236,2.38462541573845));
#59723=CARTESIAN_POINT('Ctrl Pts',(-23.1957299548836,27.4689460250234,2.39049010267667));
#59724=CARTESIAN_POINT('Ctrl Pts',(-23.3112380798912,27.4776922042941,2.39635478961489));
#59725=CARTESIAN_POINT('Ctrl Pts',(-23.4270314999599,27.4813217981074,2.40221947655312));
#59726=CARTESIAN_POINT('Ctrl Pts',(-23.5427058337444,27.4849476591106,2.40807813202794));
#59727=CARTESIAN_POINT('Ctrl Pts',(-23.6586644682903,27.4834673883464,2.41393678750276));
#59728=CARTESIAN_POINT('Ctrl Pts',(-23.774421041805,27.4768588882157,2.41979544297758));
#59729=CARTESIAN_POINT('Ctrl Pts',(-23.8946991690384,27.4699922542491,2.42588294269548));
#59730=CARTESIAN_POINT('Ctrl Pts',(-24.014758676644,27.4575885431502,2.43197044241338));
#59731=CARTESIAN_POINT('Ctrl Pts',(-24.1340526131114,27.4396826268286,2.43805794213129));
#59732=CARTESIAN_POINT('Ctrl Pts',(-24.2487290238372,27.422469797113,2.44390981221469));
#59733=CARTESIAN_POINT('Ctrl Pts',(-24.3626975806099,27.4001728582094,2.44976168229809));
#59734=CARTESIAN_POINT('Ctrl Pts',(-24.4754776341793,27.3728756506704,2.45561355238148));
#59735=CARTESIAN_POINT('Ctrl Pts',(-24.5882405159602,27.3455825993795,2.46146453146446));
#59736=CARTESIAN_POINT('Ctrl Pts',(-24.6998148526737,27.3132908904538,2.46731551054743));
#59737=CARTESIAN_POINT('Ctrl Pts',(-24.8097315217236,27.276135202106,2.4731664896304));
#59738=CARTESIAN_POINT('Ctrl Pts',(-24.9196580733395,27.2389761731043,2.47901799477268));
#59739=CARTESIAN_POINT('Ctrl Pts',(-25.0279262693765,27.1969524277186,2.48486949991497));
#59740=CARTESIAN_POINT('Ctrl Pts',(-25.1340841301445,27.1502478744343,2.49072100505725));
#59741=CARTESIAN_POINT('Ctrl Pts',(-25.2402772436273,27.1035278115845,2.49657445335703));
#59742=CARTESIAN_POINT('Ctrl Pts',(-25.3443582501698,27.0521240164031,2.5024279016568));
#59743=CARTESIAN_POINT('Ctrl Pts',(-25.4458977067021,26.9962673851835,2.50828134995658));
#59744=CARTESIAN_POINT('Ctrl Pts',(-25.5475526356453,26.9403472328453,2.51414145489812));
#59745=CARTESIAN_POINT('Ctrl Pts',(-25.6466598832259,26.8799643365566,2.52000155983966));
#59746=CARTESIAN_POINT('Ctrl Pts',(-25.7428169718074,26.8153942094704,2.5258616647812));
#59747=CARTESIAN_POINT('Ctrl Pts',(-25.8390388161701,26.7507805984446,2.53172571613667));
#59748=CARTESIAN_POINT('Ctrl Pts',(-25.9323062136828,26.6819743865744,2.53758976749214));
#59749=CARTESIAN_POINT('Ctrl Pts',(-26.0222492888522,26.6092917652773,2.54345381884761));
#59750=CARTESIAN_POINT('Ctrl Pts',(-26.1123249221597,26.5365020243055,2.54932651264417));
#59751=CARTESIAN_POINT('Ctrl Pts',(-26.1990661463341,26.4598247445117,2.55519920644074));
#59752=CARTESIAN_POINT('Ctrl Pts',(-26.2821394235273,26.3796134153976,2.5610719002373));
#59753=CARTESIAN_POINT('Ctrl Pts',(-26.3048834971763,26.3576528952579,2.56267974556062));
#59754=CARTESIAN_POINT('Ctrl Pts',(-26.3273528638878,26.3354276644646,2.56428759088393));
#59755=CARTESIAN_POINT('Ctrl Pts',(-26.3495412149203,26.312945396991,2.56589543620725));
#59756=CARTESIAN_POINT('Ctrl Pts',(-26.4294861757714,26.2319414508042,2.57168852697089));
#59757=CARTESIAN_POINT('Ctrl Pts',(-26.5060637743932,26.1473106300145,2.57748161773453));
#59758=CARTESIAN_POINT('Ctrl Pts',(-26.5789200013633,26.0593683835768,2.58327470849818));
#59759=CARTESIAN_POINT('Ctrl Pts',(-26.6516601170014,25.9715662911354,2.5890585667842));
#59760=CARTESIAN_POINT('Ctrl Pts',(-26.7206903918569,25.8804635973304,2.59484242507023));
#59761=CARTESIAN_POINT('Ctrl Pts',(-26.7856929894963,25.7864130903342,2.60062628335625));
#59762=CARTESIAN_POINT('Ctrl Pts',(-26.8506363999539,25.6924482196766,2.60640487523318));
#59763=CARTESIAN_POINT('Ctrl Pts',(-26.9115591784749,25.5955412156709,2.6121834671101));
#59764=CARTESIAN_POINT('Ctrl Pts',(-26.9681833632604,25.4960782768803,2.61796205898703));
#59765=CARTESIAN_POINT('Ctrl Pts',(-27.0247705829217,25.3966802690004,2.62373687851178));
#59766=CARTESIAN_POINT('Ctrl Pts',(-27.0770645754825,25.294730010542,2.62951169803653));
#59767=CARTESIAN_POINT('Ctrl Pts',(-27.1248308756546,25.190642321619,2.63528651756128));
#59768=CARTESIAN_POINT('Ctrl Pts',(-27.17257829933,25.0865957665269,2.64105905496745));
#59769=CARTESIAN_POINT('Ctrl Pts',(-27.2158014107761,24.9804138465547,2.64683159237361));
#59770=CARTESIAN_POINT('Ctrl Pts',(-27.2543122718042,24.8725348168723,2.65260412977978));
#59771=CARTESIAN_POINT('Ctrl Pts',(-27.2928316263285,24.764631994678,2.65837794030794));
#59772=CARTESIAN_POINT('Ctrl Pts',(-27.3266365003827,24.6550317122609,2.66415175083611));
#59773=CARTESIAN_POINT('Ctrl Pts',(-27.355587737806,24.5441906430099,2.66992556136427));
#59774=CARTESIAN_POINT('Ctrl Pts',(-27.3845409577316,24.4333419836629,2.67569976726732));
#59775=CARTESIAN_POINT('Ctrl Pts',(-27.4086397803666,24.3212527826688,2.68147397317038));
#59776=CARTESIAN_POINT('Ctrl Pts',(-27.4277957832568,24.2083918271792,2.68724817907344));
#59777=CARTESIAN_POINT('Ctrl Pts',(-27.4469700873666,24.0954230468399,2.69302790152453));
#59778=CARTESIAN_POINT('Ctrl Pts',(-27.4611920749221,23.9816814607547,2.69880762397564));
#59779=CARTESIAN_POINT('Ctrl Pts',(-27.4704250188582,23.8676429393665,2.70458734642673));
#59780=CARTESIAN_POINT('Ctrl Pts',(-27.4790775289498,23.760773509207,2.71000372360621));
#59781=CARTESIAN_POINT('Ctrl Pts',(-27.4833490335356,23.6536436393539,2.71542010078569));
#59782=CARTESIAN_POINT('Ctrl Pts',(-27.4832508767861,23.5466445538181,2.72083647796517));
#59783=CARTESIAN_POINT('',(-27.4847337162098,23.55176910164,3.97083647796515));
#59784=CARTESIAN_POINT('Ctrl Pts',(-27.4837197232878,23.5466441237168,2.72083647796517));
#59785=CARTESIAN_POINT('Ctrl Pts',(-27.486410087491,23.2572272739644,2.73548510117082));
#59786=CARTESIAN_POINT('Ctrl Pts',(-27.3249482139625,21.6609649344543,2.81642936150173));
#59787=CARTESIAN_POINT('Ctrl Pts',(-25.146211310607,19.1806225235481,2.96366925895684));
#59788=CARTESIAN_POINT('Ctrl Pts',(-20.7366928686042,19.8455753724331,3.16255617033201));
#59789=CARTESIAN_POINT('Ctrl Pts',(-18.9125972064597,23.9148124258598,3.36144308170675));
#59790=CARTESIAN_POINT('Ctrl Pts',(-21.3501135798777,27.6490498461272,3.56032999308169));
#59791=CARTESIAN_POINT('Ctrl Pts',(-25.8093711089935,27.6168400551356,3.7592169044566));
#59792=CARTESIAN_POINT('Ctrl Pts',(-27.4491102260847,25.0237028729037,3.8960523994177));
#59793=CARTESIAN_POINT('Ctrl Pts',(-27.4894584729477,23.6353302575449,3.96659225725393));
#59794=CARTESIAN_POINT('Ctrl Pts',(-27.4890477443728,23.5517707645087,3.97083647796515));
#59795=CARTESIAN_POINT('',(-27.4825761731824,23.5531249265093,5.22083643712987));
#59796=CARTESIAN_POINT('Ctrl Pts',(-27.4832522395187,23.5517685305957,3.97083647796515));
#59797=CARTESIAN_POINT('Ctrl Pts',(-27.4832963124207,23.4374289286688,3.9766526763897));
#59798=CARTESIAN_POINT('Ctrl Pts',(-27.4783500636744,23.3228856127001,3.98246887481425));
#59799=CARTESIAN_POINT('Ctrl Pts',(-27.4683864150193,23.2086154840257,3.9882850732388));
#59800=CARTESIAN_POINT('Ctrl Pts',(-27.4584351814101,23.0944877398273,3.99409402448183));
#59801=CARTESIAN_POINT('Ctrl Pts',(-27.4434790122282,22.9806329226432,3.99990297572487));
#59802=CARTESIAN_POINT('Ctrl Pts',(-27.4235428263286,22.8675290931842,4.0057119269679));
#59803=CARTESIAN_POINT('Ctrl Pts',(-27.4036259005948,22.7545345322945,4.01151526623657));
#59804=CARTESIAN_POINT('Ctrl Pts',(-27.3787385972726,22.6422899296219,4.01731860550524));
#59805=CARTESIAN_POINT('Ctrl Pts',(-27.3489576702902,22.5312685916811,4.02312194477391));
#59806=CARTESIAN_POINT('Ctrl Pts',(-27.3191958220377,22.4203183779916,4.02892156621529));
#59807=CARTESIAN_POINT('Ctrl Pts',(-27.2845466920075,22.3105902772112,4.03472118765667));
#59808=CARTESIAN_POINT('Ctrl Pts',(-27.2451380415968,22.2025470487672,4.04052080909804));
#59809=CARTESIAN_POINT('Ctrl Pts',(-27.2057421880805,22.0945389044421,4.04631854726907));
#59810=CARTESIAN_POINT('Ctrl Pts',(-27.1615900298808,21.98821494112,4.05211628544009));
#59811=CARTESIAN_POINT('Ctrl Pts',(-27.1128588527272,21.8840216949444,4.05791402361112));
#59812=CARTESIAN_POINT('Ctrl Pts',(-27.0641311585802,21.779835895865,4.06371134739526));
#59813=CARTESIAN_POINT('Ctrl Pts',(-27.0108252750434,21.6777808932096,4.06950867117941));
#59814=CARTESIAN_POINT('Ctrl Pts',(-26.9531658491457,21.5782814482573,4.07530599496355));
#59815=CARTESIAN_POINT('Ctrl Pts',(-26.895495941529,21.4787639156254,4.08110437262427));
#59816=CARTESIAN_POINT('Ctrl Pts',(-26.8334711306767,21.3818032286698,4.08690275028499));
#59817=CARTESIAN_POINT('Ctrl Pts',(-26.7673606250504,21.2877971143075,4.09270112794572));
#59818=CARTESIAN_POINT('Ctrl Pts',(-26.7011810180815,21.1936927409977,4.0985055663025));
#59819=CARTESIAN_POINT('Ctrl Pts',(-26.6309074328281,21.1025494518367,4.10431000465928));
#59820=CARTESIAN_POINT('Ctrl Pts',(-26.5568508219523,21.0147337049021,4.11011444301607));
#59821=CARTESIAN_POINT('Ctrl Pts',(-26.4827528227106,20.9268688799686,4.11592212532658));
#59822=CARTESIAN_POINT('Ctrl Pts',(-26.4048678745775,20.8423356092517,4.1217298076371));
#59823=CARTESIAN_POINT('Ctrl Pts',(-26.3235440984385,20.7614637469662,4.12753748994761));
#59824=CARTESIAN_POINT('Ctrl Pts',(-26.2420916307683,20.6804639082844,4.13335436267654));
#59825=CARTESIAN_POINT('Ctrl Pts',(-26.1571897801108,20.6031373315479,4.13917123540548));
#59826=CARTESIAN_POINT('Ctrl Pts',(-26.0692202443632,20.5297739830978,4.14498810813441));
#59827=CARTESIAN_POINT('Ctrl Pts',(-26.0087143748169,20.4793143193849,4.14898898115839));
#59828=CARTESIAN_POINT('Ctrl Pts',(-25.9467579266626,20.4307286938456,4.15298985418237));
#59829=CARTESIAN_POINT('Ctrl Pts',(-25.8834825318848,20.3840992242546,4.15699072720635));
#59830=CARTESIAN_POINT('Ctrl Pts',(-25.7906098246731,20.31565863859,4.16286302417505));
#59831=CARTESIAN_POINT('Ctrl Pts',(-25.6945676280462,20.2511932106756,4.16873532114375));
#59832=CARTESIAN_POINT('Ctrl Pts',(-25.595730993464,20.1910105245688,4.17460761811246));
#59833=CARTESIAN_POINT('Ctrl Pts',(-25.4970224433104,20.1309058304433,4.18047230505067));
#59834=CARTESIAN_POINT('Ctrl Pts',(-25.3955270066242,20.0750730539903,4.18633699198889));
#59835=CARTESIAN_POINT('Ctrl Pts',(-25.2916513271279,20.023778480285,4.19220167892711));
#59836=CARTESIAN_POINT('Ctrl Pts',(-25.1878824772655,19.9725366598379,4.19806033440193));
#59837=CARTESIAN_POINT('Ctrl Pts',(-25.0817386220792,19.9258239406549,4.20391898987675));
#59838=CARTESIAN_POINT('Ctrl Pts',(-24.9736532258043,19.8838620091221,4.20977764535157));
#59839=CARTESIAN_POINT('Ctrl Pts',(-24.8613459187506,19.840261007584,4.21586514506947));
#59840=CARTESIAN_POINT('Ctrl Pts',(-24.7469426902543,19.8017897361575,4.22195264478738));
#59841=CARTESIAN_POINT('Ctrl Pts',(-24.6309557567804,19.7686431468835,4.22804014450528));
#59842=CARTESIAN_POINT('Ctrl Pts',(-24.5194583444578,19.7367795669036,4.23389201458867));
#59843=CARTESIAN_POINT('Ctrl Pts',(-24.40649798337,19.7098362515877,4.23974388467207));
#59844=CARTESIAN_POINT('Ctrl Pts',(-24.2925468457534,19.687936108702,4.24559575475546));
#59845=CARTESIAN_POINT('Ctrl Pts',(-24.1786130582335,19.6660393003121,4.25144673383843));
#59846=CARTESIAN_POINT('Ctrl Pts',(-24.0636891999744,19.6491842155817,4.25729771292141));
#59847=CARTESIAN_POINT('Ctrl Pts',(-23.9482580231877,19.6374427192013,4.26314869200438));
#59848=CARTESIAN_POINT('Ctrl Pts',(-23.8328164680277,19.6257001671474,4.26900019714666));
#59849=CARTESIAN_POINT('Ctrl Pts',(-23.7168679149511,19.6190721592409,4.27485170228894));
#59850=CARTESIAN_POINT('Ctrl Pts',(-23.6008999187749,19.6175786522348,4.28070320743123));
#59851=CARTESIAN_POINT('Ctrl Pts',(-23.4848934121511,19.6160846492677,4.28655665573101));
#59852=CARTESIAN_POINT('Ctrl Pts',(-23.368867862719,19.619728542918,4.2924101040308));
#59853=CARTESIAN_POINT('Ctrl Pts',(-23.2533097898436,19.6284781873365,4.29826355233058));
#59854=CARTESIAN_POINT('Ctrl Pts',(-23.1376203023466,19.6372377820006,4.30412365727212));
#59855=CARTESIAN_POINT('Ctrl Pts',(-23.0223997649561,19.6511146854975,4.30998376221366));
#59856=CARTESIAN_POINT('Ctrl Pts',(-22.908128648405,19.6700249715491,4.3158438671552));
#59857=CARTESIAN_POINT('Ctrl Pts',(-22.7937805774088,19.6889479924948,4.32170791851065));
#59858=CARTESIAN_POINT('Ctrl Pts',(-22.6803836038382,19.7129110602377,4.3275719698661));
#59859=CARTESIAN_POINT('Ctrl Pts',(-22.5684053876209,19.7417797162897,4.33343602122155));
#59860=CARTESIAN_POINT('Ctrl Pts',(-22.4562621378658,19.770690918978,4.33930871501812));
#59861=CARTESIAN_POINT('Ctrl Pts',(-22.345542212482,19.8045220190324,4.34518140881469));
#59862=CARTESIAN_POINT('Ctrl Pts',(-22.2366956600887,19.8430895537476,4.35105410261126));
#59863=CARTESIAN_POINT('Ctrl Pts',(-22.206895294824,19.8536486995965,4.35266194793459));
#59864=CARTESIAN_POINT('Ctrl Pts',(-22.177235220616,19.8645626045907,4.35426979325792));
#59865=CARTESIAN_POINT('Ctrl Pts',(-22.1477243593861,19.8758268995876,4.35587763858125));
#59866=CARTESIAN_POINT('Ctrl Pts',(-22.0399425109518,19.916967228452,4.36174993554996));
#59867=CARTESIAN_POINT('Ctrl Pts',(-21.9337917860359,19.9629228432228,4.36762223251866));
#59868=CARTESIAN_POINT('Ctrl Pts',(-21.82973369148,20.0135444690365,4.37349452948737));
#59869=CARTESIAN_POINT('Ctrl Pts',(-21.7258104479508,20.0641004932433,4.37935921642557));
#59870=CARTESIAN_POINT('Ctrl Pts',(-21.6239748101192,20.1193103244505,4.38522390336377));
#59871=CARTESIAN_POINT('Ctrl Pts',(-21.5246706162578,20.1789757848434,4.39108859030197));
#59872=CARTESIAN_POINT('Ctrl Pts',(-21.4254685505429,20.2385798830456,4.39694724577681));
#59873=CARTESIAN_POINT('Ctrl Pts',(-21.3287931026507,20.3026302843108,4.40280590125166));
#59874=CARTESIAN_POINT('Ctrl Pts',(-21.2350650868523,20.3708821387946,4.4086645567265));
#59875=CARTESIAN_POINT('Ctrl Pts',(-21.1376759722027,20.4417999708297,4.41475205644441));
#59876=CARTESIAN_POINT('Ctrl Pts',(-21.043469651172,20.5172539733303,4.42083955616231));
#59877=CARTESIAN_POINT('Ctrl Pts',(-20.9528870148963,20.596918589833,4.42692705588021));
#59878=CARTESIAN_POINT('Ctrl Pts',(-20.8658105723731,20.673499617779,4.4327789259636));
#59879=CARTESIAN_POINT('Ctrl Pts',(-20.7820828452387,20.7539710607026,4.438630796047));
#59880=CARTESIAN_POINT('Ctrl Pts',(-20.7020624669695,20.8380021090371,4.44448266613039));
#59881=CARTESIAN_POINT('Ctrl Pts',(-20.6220542725305,20.9220203628805,4.45033364521336));
#59882=CARTESIAN_POINT('Ctrl Pts',(-20.5457525895909,21.0095968452202,4.45618462429634));
#59883=CARTESIAN_POINT('Ctrl Pts',(-20.4734788271562,21.1003642544327,4.46203560337931));
#59884=CARTESIAN_POINT('Ctrl Pts',(-20.4011985666146,21.1911398245089,4.46788710852161));
#59885=CARTESIAN_POINT('Ctrl Pts',(-20.3329472040104,21.2851065683714,4.47373861366392));
#59886=CARTESIAN_POINT('Ctrl Pts',(-20.269005073342,21.3818650854435,4.47959011880622));
#59887=CARTESIAN_POINT('Ctrl Pts',(-20.2050417088844,21.4786557339123,4.48544356710597));
#59888=CARTESIAN_POINT('Ctrl Pts',(-20.1453906496107,21.578239654348,4.49129701540573));
#59889=CARTESIAN_POINT('Ctrl Pts',(-20.0902878350205,21.6801901536513,4.49715046370548));
#59890=CARTESIAN_POINT('Ctrl Pts',(-20.0351223565645,21.7822565928107,4.50301056864701));
#59891=CARTESIAN_POINT('Ctrl Pts',(-19.9845156433017,21.8866946187397,4.50887067358855));
#59892=CARTESIAN_POINT('Ctrl Pts',(-19.9386568014461,21.9930546376379,4.51473077853008));
#59893=CARTESIAN_POINT('Ctrl Pts',(-19.8927670765306,22.0994862833521,4.52059482988553));
#59894=CARTESIAN_POINT('Ctrl Pts',(-19.8516317360271,22.2078421138009,4.52645888124098));
#59895=CARTESIAN_POINT('Ctrl Pts',(-19.8153904477701,22.317655998328,4.53232293259642));
#59896=CARTESIAN_POINT('Ctrl Pts',(-19.7790957470887,22.4276317265999,4.53819562639299));
#59897=CARTESIAN_POINT('Ctrl Pts',(-19.7477096057703,22.5390694012931,4.54406832018956));
#59898=CARTESIAN_POINT('Ctrl Pts',(-19.7213209439203,22.6514912195832,4.54994101398612));
#59899=CARTESIAN_POINT('Ctrl Pts',(-19.7140961697342,22.6822704328438,4.55154885930946));
#59900=CARTESIAN_POINT('Ctrl Pts',(-19.7072456936328,22.7131233792419,4.5531567046328));
#59901=CARTESIAN_POINT('Ctrl Pts',(-19.7007706624597,22.7440401909085,4.55476454995614));
#59902=CARTESIAN_POINT('Ctrl Pts',(-19.6771220531203,22.8569569602004,4.56063684692485));
#59903=CARTESIAN_POINT('Ctrl Pts',(-19.658406316016,22.9711043040757,4.56650914389356));
#59904=CARTESIAN_POINT('Ctrl Pts',(-19.644747327712,23.0860132596933,4.57238144086227));
#59905=CARTESIAN_POINT('Ctrl Pts',(-19.6311060403721,23.2007733024299,4.57824612780046));
#59906=CARTESIAN_POINT('Ctrl Pts',(-19.6225085183239,23.3162925874392,4.58411081473865));
#59907=CARTESIAN_POINT('Ctrl Pts',(-19.6190279446485,23.4320905826255,4.58997550167683));
#59908=CARTESIAN_POINT('Ctrl Pts',(-19.6155509505254,23.5477694868228,4.59583415715163));
#59909=CARTESIAN_POINT('Ctrl Pts',(-19.6171804498143,23.6637261203512,4.60169281262643));
#59910=CARTESIAN_POINT('Ctrl Pts',(-19.6239379141862,23.7794740933833,4.60755146810123));
#59911=CARTESIAN_POINT('Ctrl Pts',(-19.6309593310684,23.899743284192,4.61363896781914));
#59912=CARTESIAN_POINT('Ctrl Pts',(-19.6435175391514,24.019786729766,4.61972646753705));
#59913=CARTESIAN_POINT('Ctrl Pts',(-19.6615769626702,24.1390575239252,4.62581396725495));
#59914=CARTESIAN_POINT('Ctrl Pts',(-19.6789373577603,24.2537116881154,4.63166583733836));
#59915=CARTESIAN_POINT('Ctrl Pts',(-19.7013809468752,24.3676514560851,4.63751770742176));
#59916=CARTESIAN_POINT('Ctrl Pts',(-19.7288232709736,24.4803962868786,4.64336957750517));
#59917=CARTESIAN_POINT('Ctrl Pts',(-19.7562614167287,24.5931239512464,4.64922055658814));
#59918=CARTESIAN_POINT('Ctrl Pts',(-19.788696686414,24.7046566386473,4.65507153567112));
#59919=CARTESIAN_POINT('Ctrl Pts',(-19.8259937982043,24.8145254001937,4.66092251475409));
#59920=CARTESIAN_POINT('Ctrl Pts',(-19.8632942633637,24.9244040399989,4.66677401989639));
#59921=CARTESIAN_POINT('Ctrl Pts',(-19.9054573067041,25.0326180650866,4.67262552503868));
#59922=CARTESIAN_POINT('Ctrl Pts',(-19.9522984382295,25.1387157328168,4.67847703018097));
#59923=CARTESIAN_POINT('Ctrl Pts',(-19.9991551246748,25.2448486332723,4.68433047848072));
#59924=CARTESIAN_POINT('Ctrl Pts',(-20.0506928214555,25.3488634009369,4.69018392678047));
#59925=CARTESIAN_POINT('Ctrl Pts',(-20.1066800798098,25.4503308902423,4.69603737508021));
#59926=CARTESIAN_POINT('Ctrl Pts',(-20.1627310078344,25.5519137701165,4.70189748002175));
#59927=CARTESIAN_POINT('Ctrl Pts',(-20.223241397446,25.6509432275333,4.70775758496329));
#59928=CARTESIAN_POINT('Ctrl Pts',(-20.2879352177625,25.7470171397533,4.71361768990483));
#59929=CARTESIAN_POINT('Ctrl Pts',(-20.352672605318,25.8431557517404,4.71948174126029));
#59930=CARTESIAN_POINT('Ctrl Pts',(-20.4215987881028,25.9363345237726,4.72534579261576));
#59931=CARTESIAN_POINT('Ctrl Pts',(-20.4943970989599,26.0261839875767,4.73120984397122));
#59932=CARTESIAN_POINT('Ctrl Pts',(-20.5673026999952,26.1161658715545,4.73708253776779));
#59933=CARTESIAN_POINT('Ctrl Pts',(-20.6440915455078,26.2028083462002,4.74295523156437));
#59934=CARTESIAN_POINT('Ctrl Pts',(-20.7244097170516,26.2857783288551,4.74882792536094));
#59935=CARTESIAN_POINT('Ctrl Pts',(-20.7463994888618,26.3084941221882,4.7504357706843));
#59936=CARTESIAN_POINT('Ctrl Pts',(-20.7686536175801,26.330934868149,4.75204361600766));
#59937=CARTESIAN_POINT('Ctrl Pts',(-20.7911644211204,26.3530942678773,4.75365146133102));
#59938=CARTESIAN_POINT('Ctrl Pts',(-20.8733801177873,26.4340265403806,4.75952375829973));
#59939=CARTESIAN_POINT('Ctrl Pts',(-20.9592975440606,26.5114738824377,4.76539605526844));
#59940=CARTESIAN_POINT('Ctrl Pts',(-21.0485891141686,26.5850785803194,4.77126835223715));
#59941=CARTESIAN_POINT('Ctrl Pts',(-21.137764969493,26.6585878923581,4.77713303917535));
#59942=CARTESIAN_POINT('Ctrl Pts',(-21.2303059570408,26.7282642026665,4.78299772611355));
#59943=CARTESIAN_POINT('Ctrl Pts',(-21.3258473556551,26.7937861931213,4.78886241305175));
#59944=CARTESIAN_POINT('Ctrl Pts',(-21.4212904959224,26.8592407983109,4.79472106852659));
#59945=CARTESIAN_POINT('Ctrl Pts',(-21.5197275707047,26.9205493493921,4.80057972400143));
#59946=CARTESIAN_POINT('Ctrl Pts',(-21.6207609784277,26.9774308675666,4.80643837947628));
#59947=CARTESIAN_POINT('Ctrl Pts',(-21.725740840045,27.0365342279414,4.81252587919418));
#59948=CARTESIAN_POINT('Ctrl Pts',(-21.833523648774,27.0908573681119,4.81861337891208));
#59949=CARTESIAN_POINT('Ctrl Pts',(-21.9436300530602,27.1401345925909,4.82470087862998));
#59950=CARTESIAN_POINT('Ctrl Pts',(-22.0494745545946,27.1875044372043,4.83055274871338));
#59951=CARTESIAN_POINT('Ctrl Pts',(-22.1574657044648,27.2302115439549,4.83640461879677));
#59952=CARTESIAN_POINT('Ctrl Pts',(-22.2671535618097,27.2680672168932,4.84225648888017));
#59953=CARTESIAN_POINT('Ctrl Pts',(-22.3768247181811,27.3059171259611,4.84810746796314));
#59954=CARTESIAN_POINT('Ctrl Pts',(-22.488191677708,27.3389169351142,4.85395844704612));
#59955=CARTESIAN_POINT('Ctrl Pts',(-22.6007867802616,27.3669269724681,4.85980942612909));
#59956=CARTESIAN_POINT('Ctrl Pts',(-22.7133920061983,27.3949395281938,4.86566093127138));
#59957=CARTESIAN_POINT('Ctrl Pts',(-22.8272251934898,27.4179613204876,4.87151243641367));
#59958=CARTESIAN_POINT('Ctrl Pts',(-22.9418065588099,27.4359033778307,4.87736394155595));
#59959=CARTESIAN_POINT('Ctrl Pts',(-23.0564259741077,27.4538513933405,4.88321738985575));
#59960=CARTESIAN_POINT('Ctrl Pts',(-23.1717936532784,27.4667162557484,4.88907083815554));
#59961=CARTESIAN_POINT('Ctrl Pts',(-23.2874234410873,27.4744607154086,4.89492428645533));
#59962=CARTESIAN_POINT('Ctrl Pts',(-23.4031847250729,27.482213982201,4.90078439139687));
#59963=CARTESIAN_POINT('Ctrl Pts',(-23.5192082999409,27.4848351960528,4.90664449633841));
#59964=CARTESIAN_POINT('Ctrl Pts',(-23.6350066466901,27.4823392219887,4.91250460127995));
#59965=CARTESIAN_POINT('Ctrl Pts',(-23.7508829763782,27.4798415670423,4.91836865263539));
#59966=CARTESIAN_POINT('Ctrl Pts',(-23.8665333644483,27.4722198894168,4.92423270399083));
#59967=CARTESIAN_POINT('Ctrl Pts',(-23.9814757990205,27.4595408932399,4.93009675534627));
#59968=CARTESIAN_POINT('Ctrl Pts',(-24.0965876357965,27.4468432107535,4.93596944914284));
#59969=CARTESIAN_POINT('Ctrl Pts',(-24.2109890297344,27.4290733972227,4.9418421429394));
#59970=CARTESIAN_POINT('Ctrl Pts',(-24.3242084448811,27.4063491648769,4.94771483673597));
#59971=CARTESIAN_POINT('Ctrl Pts',(-24.3552060268187,27.4001276501906,4.9493226820593));
#59972=CARTESIAN_POINT('Ctrl Pts',(-24.386115102903,27.3935350528374,4.95093052738262));
#59973=CARTESIAN_POINT('Ctrl Pts',(-24.4169262213039,27.3865744310841,4.95253837270595));
#59974=CARTESIAN_POINT('Ctrl Pts',(-24.5294569694817,27.3611523102935,4.95841066967465));
#59975=CARTESIAN_POINT('Ctrl Pts',(-24.6410567289838,27.3307321096338,4.96428296664336));
#59976=CARTESIAN_POINT('Ctrl Pts',(-24.751247475251,27.2953960730756,4.97015526361206));
#59977=CARTESIAN_POINT('Ctrl Pts',(-24.8612954230623,27.2601058292145,4.97601995055026));
#59978=CARTESIAN_POINT('Ctrl Pts',(-24.9699375988315,27.2199125432252,4.98188463748845));
#59979=CARTESIAN_POINT('Ctrl Pts',(-25.0767065249837,27.1749493750689,4.98774932442665));
#59980=CARTESIAN_POINT('Ctrl Pts',(-25.1833656459794,27.1300324487162,4.99360797990148));
#59981=CARTESIAN_POINT('Ctrl Pts',(-25.2881549706174,27.0803555570138,4.99946663537631));
#59982=CARTESIAN_POINT('Ctrl Pts',(-25.390623186214,27.0261013278852,5.00532529085113));
#59983=CARTESIAN_POINT('Ctrl Pts',(-25.4970939005645,26.9697278807804,5.01141279056904));
#59984=CARTESIAN_POINT('Ctrl Pts',(-25.6010580471928,26.9084123555736,5.01750029028694));
#59985=CARTESIAN_POINT('Ctrl Pts',(-25.7020329821909,26.8424144190959,5.02358779000484));
#59986=CARTESIAN_POINT('Ctrl Pts',(-25.7990994673934,26.7789710732336,5.02943966008824));
#59987=CARTESIAN_POINT('Ctrl Pts',(-25.8934034674278,26.7112013086271,5.03529153017163));
#59988=CARTESIAN_POINT('Ctrl Pts',(-25.9845430171159,26.6393816699119,5.04114340025503));
#59989=CARTESIAN_POINT('Ctrl Pts',(-26.075668689979,26.5675729663896,5.046994379338));
#59990=CARTESIAN_POINT('Ctrl Pts',(-26.1636305459032,26.4917158706057,5.05284535842097));
#59991=CARTESIAN_POINT('Ctrl Pts',(-26.2480582864638,26.4121283342985,5.05869633750394));
#59992=CARTESIAN_POINT('Ctrl Pts',(-26.3324936178905,26.3325336423061,5.06454784264622));
#59993=CARTESIAN_POINT('Ctrl Pts',(-26.4133939014749,26.2492081266143,5.0703993477885));
#59994=CARTESIAN_POINT('Ctrl Pts',(-26.4904249407582,26.1625073441079,5.07625085293078));
#59995=CARTESIAN_POINT('Ctrl Pts',(-26.5674815603729,26.0757777701589,5.08210430123054));
#59996=CARTESIAN_POINT('Ctrl Pts',(-26.640666106341,25.9856710095174,5.0879577495303));
#59997=CARTESIAN_POINT('Ctrl Pts',(-26.7096844523967,25.8925759377264,5.09381119783007));
#59998=CARTESIAN_POINT('Ctrl Pts',(-26.7787812872988,25.7993749966237,5.09967130277159));
#59999=CARTESIAN_POINT('Ctrl Pts',(-26.8437022192963,25.7031792936232,5.10553140771312));
#60000=CARTESIAN_POINT('Ctrl Pts',(-26.9041962298964,25.6044070218165,5.11139151265465));
#60001=CARTESIAN_POINT('Ctrl Pts',(-26.9647309794266,25.5055682330665,5.1172555640101));
#60002=CARTESIAN_POINT('Ctrl Pts',(-27.0208326716819,25.4041497813098,5.12311961536555));
#60003=CARTESIAN_POINT('Ctrl Pts',(-27.072296878109,25.3005932476371,5.128983666721));
#60004=CARTESIAN_POINT('Ctrl Pts',(-27.1238369325031,25.1968840923057,5.13485636051757));
#60005=CARTESIAN_POINT('Ctrl Pts',(-27.1707256934761,25.0910309426017,5.14072905431413));
#60006=CARTESIAN_POINT('Ctrl Pts',(-27.2128073091294,24.9834941380839,5.1466017481107));
#60007=CARTESIAN_POINT('Ctrl Pts',(-27.2243285515562,24.954052359877,5.14820959343408));
#60008=CARTESIAN_POINT('Ctrl Pts',(-27.2354897547434,24.9244844572167,5.14981743875746));
#60009=CARTESIAN_POINT('Ctrl Pts',(-27.2462883825474,24.894800035209,5.15142528408085));
#60010=CARTESIAN_POINT('Ctrl Pts',(-27.2919542468375,24.7692688277693,5.15822463374541));
#60011=CARTESIAN_POINT('Ctrl Pts',(-27.3312583294848,24.6413065928319,5.16502398340998));
#60012=CARTESIAN_POINT('Ctrl Pts',(-27.3639717707758,24.5115196982296,5.17182333307454));
#60013=CARTESIAN_POINT('Ctrl Pts',(-27.3965467409697,24.382282172112,5.17859390211042));
#60014=CARTESIAN_POINT('Ctrl Pts',(-27.4225866449772,24.2512355293688,5.1853644711463));
#60015=CARTESIAN_POINT('Ctrl Pts',(-27.4419122083623,24.119000244653,5.19213504018218));
#60016=CARTESIAN_POINT('Ctrl Pts',(-27.461088734335,23.9877847493355,5.19885339505647));
#60017=CARTESIAN_POINT('Ctrl Pts',(-27.4736539935025,23.8553990195052,5.20557174993076));
#60018=CARTESIAN_POINT('Ctrl Pts',(-27.4794802654773,23.7224687216122,5.21229010480506));
#60019=CARTESIAN_POINT('Ctrl Pts',(-27.4819507716076,23.6661024693548,5.21513887962616));
#60020=CARTESIAN_POINT('Ctrl Pts',(-27.4832101997752,23.6096385311086,5.21798765444727));
#60021=CARTESIAN_POINT('Ctrl Pts',(-27.4832514823194,23.5531255756082,5.22083642926838));
#60022=CARTESIAN_POINT('',(-27.4785911626596,23.547629167803,6.47083647796516));
#60023=CARTESIAN_POINT('Ctrl Pts',(-27.4790683860637,23.5531215548671,5.22083647796515));
#60024=CARTESIAN_POINT('Ctrl Pts',(-27.473319408008,22.6978634849193,5.263995050462));
#60025=CARTESIAN_POINT('Ctrl Pts',(-26.7776474908277,20.520334858285,5.3734492600839));
#60026=CARTESIAN_POINT('Ctrl Pts',(-23.1797246374427,18.9130702070832,5.54919910683057));
#60027=CARTESIAN_POINT('Ctrl Pts',(-19.4486272035729,21.3553902353711,5.7480860182055));
#60028=CARTESIAN_POINT('Ctrl Pts',(-19.4865756857664,25.8146026203464,5.94697292958035));
#60029=CARTESIAN_POINT('Ctrl Pts',(-23.2586986463879,28.1930692590768,6.14585984095524));
#60030=CARTESIAN_POINT('Ctrl Pts',(-26.8058194983606,26.5355178218322,6.32048102375024));
#60031=CARTESIAN_POINT('Ctrl Pts',(-27.473510843006,24.3807749536279,6.42880656942016));
#60032=CARTESIAN_POINT('Ctrl Pts',(-27.4785911626596,23.547629167803,6.47083647796516));
#60033=CARTESIAN_POINT('',(-27.4886577079825,23.5483711242969,7.72083647796516));
#60034=CARTESIAN_POINT('Ctrl Pts',(-27.4785911626596,23.547629167803,6.47083647796516));
#60035=CARTESIAN_POINT('Ctrl Pts',(-27.4815242563085,23.0666171883284,6.49510220654513));
#60036=CARTESIAN_POINT('Ctrl Pts',(-27.1765185624428,21.2750381511308,6.58566357225004));
#60037=CARTESIAN_POINT('Ctrl Pts',(-24.4979820906171,18.99585251465,6.74252057507997));
#60038=CARTESIAN_POINT('Ctrl Pts',(-20.2308473862112,20.2910654685983,6.94140748645481));
#60039=CARTESIAN_POINT('Ctrl Pts',(-19.0139645713602,24.5811950000388,7.14029439782973));
#60040=CARTESIAN_POINT('Ctrl Pts',(-21.9655457782616,27.9239758125756,7.33918130920452));
#60041=CARTESIAN_POINT('Ctrl Pts',(-26.2542626229903,27.2659458526094,7.53269533591654));
#60042=CARTESIAN_POINT('Ctrl Pts',(-27.4815868075466,24.7481226885398,7.65991372550328));
#60043=CARTESIAN_POINT('Ctrl Pts',(-27.4886577079825,23.5483711242969,7.72083647796516));
#60044=CARTESIAN_POINT('',(-27.4832509407115,23.5537901392572,8.97083647796516));
#60045=CARTESIAN_POINT('Ctrl Pts',(-27.4886577079825,23.5483711242969,7.72083647796516));
#60046=CARTESIAN_POINT('Ctrl Pts',(-27.489281303125,23.4425629242642,7.72620936262824));
#60047=CARTESIAN_POINT('Ctrl Pts',(-27.4373560099309,22.0318165836772,7.79787788441659));
#60048=CARTESIAN_POINT('Ctrl Pts',(-25.739834537459,19.4458059828765,7.93584204332904));
#60049=CARTESIAN_POINT('Ctrl Pts',(-21.2806746818376,19.4894930934159,8.1347289547043));
#60050=CARTESIAN_POINT('Ctrl Pts',(-18.9070644417657,23.2646738321175,8.33361586607897));
#60051=CARTESIAN_POINT('Ctrl Pts',(-20.8001503789075,27.3022771826442,8.53250277745392));
#60052=CARTESIAN_POINT('Ctrl Pts',(-25.220347024252,27.8920879981818,8.73138968882892));
#60053=CARTESIAN_POINT('Ctrl Pts',(-27.3401802964048,25.3943193256145,8.87750092233257));
#60054=CARTESIAN_POINT('Ctrl Pts',(-27.4868802877149,23.8207898070215,8.95731651871135));
#60055=CARTESIAN_POINT('Ctrl Pts',(-27.4844023746644,23.5537911749356,8.97083647796516));
#60056=CARTESIAN_POINT('',(-27.4832525242572,23.5504943982642,10.220836477917));
#60057=CARTESIAN_POINT('Ctrl Pts',(-27.4832509407115,23.5537901392572,8.97083647796516));
#60058=CARTESIAN_POINT('Ctrl Pts',(-27.4833535323691,23.4397320310741,8.97661376058633));
#60059=CARTESIAN_POINT('Ctrl Pts',(-27.4784903597999,23.3255145710099,8.9823910432075));
#60060=CARTESIAN_POINT('Ctrl Pts',(-27.4686465801482,23.2116124852729,8.98816832582867));
#60061=CARTESIAN_POINT('Ctrl Pts',(-27.458636643878,23.0957878061744,8.99404312523492));
#60062=CARTESIAN_POINT('Ctrl Pts',(-27.4434763704664,22.9802896886087,8.99991792464117));
#60063=CARTESIAN_POINT('Ctrl Pts',(-27.4232054851861,22.8656180160302,9.00579272404742));
#60064=CARTESIAN_POINT('Ctrl Pts',(-27.403298315435,22.7530038691839,9.01156211336696));
#60065=CARTESIAN_POINT('Ctrl Pts',(-27.3784624844721,22.641187194019,9.0173315026865));
#60066=CARTESIAN_POINT('Ctrl Pts',(-27.3487878283232,22.5306356427288,9.02310089200604));
#60067=CARTESIAN_POINT('Ctrl Pts',(-27.3191196006254,22.420108040334,9.02886903149688));
#60068=CARTESIAN_POINT('Ctrl Pts',(-27.2846147411839,22.3108454287445,9.03463717098771));
#60069=CARTESIAN_POINT('Ctrl Pts',(-27.2454137135604,22.2033030745768,9.04040531047856));
#60070=CARTESIAN_POINT('Ctrl Pts',(-27.2062110518577,22.0957562375486,9.04617369041201));
#60071=CARTESIAN_POINT('Ctrl Pts',(-27.1623119798,21.989930200693,9.05194207034546));
#60072=CARTESIAN_POINT('Ctrl Pts',(-27.1139058262283,21.886262088105,9.05771045027891));
#60073=CARTESIAN_POINT('Ctrl Pts',(-27.063938476956,21.7792504706168,9.06366487205388));
#60074=CARTESIAN_POINT('Ctrl Pts',(-27.0091685897512,21.6745387763222,9.06961929382886));
#60075=CARTESIAN_POINT('Ctrl Pts',(-26.9498560258286,21.5725809000351,9.07557371560384));
#60076=CARTESIAN_POINT('Ctrl Pts',(-26.8923154352202,21.4736690332947,9.0813502479775));
#60077=CARTESIAN_POINT('Ctrl Pts',(-26.830500027148,21.3773491085231,9.08712678035116));
#60078=CARTESIAN_POINT('Ctrl Pts',(-26.7646907147518,21.2840053767481,9.09290331272483));
#60079=CARTESIAN_POINT('Ctrl Pts',(-26.6958414871195,21.1863498382988,9.09894667920047));
#60080=CARTESIAN_POINT('Ctrl Pts',(-26.6226208652533,21.0919524606182,9.1049900456761));
#60081=CARTESIAN_POINT('Ctrl Pts',(-26.5453959638536,21.0012125514679,9.11103341215174));
#60082=CARTESIAN_POINT('Ctrl Pts',(-26.468171062454,20.9104726423175,9.11707677862737));
#60083=CARTESIAN_POINT('Ctrl Pts',(-26.3869422980837,20.8233905312141,9.123120145103));
#60084=CARTESIAN_POINT('Ctrl Pts',(-26.302117430245,20.7403186214173,9.12916351157864));
#60085=CARTESIAN_POINT('Ctrl Pts',(-26.2196936989872,20.6595982272378,9.13503580854734));
#60086=CARTESIAN_POINT('Ctrl Pts',(-26.1335772200464,20.58237227963,9.14090810551604));
#60087=CARTESIAN_POINT('Ctrl Pts',(-26.0440964988077,20.508997647984,9.14678040248474));
#60088=CARTESIAN_POINT('Ctrl Pts',(-25.9547317374774,20.4357181040332,9.15264508942294));
#60089=CARTESIAN_POINT('Ctrl Pts',(-25.8620117206126,20.3662802104368,9.15850977636114));
#60090=CARTESIAN_POINT('Ctrl Pts',(-25.7663019951844,20.3010043455187,9.16437446329934));
#60091=CARTESIAN_POINT('Ctrl Pts',(-25.6706907012169,20.2357956127412,9.17023311877418));
#60092=CARTESIAN_POINT('Ctrl Pts',(-25.5720961539414,20.1747406262546,9.17609177424902));
#60093=CARTESIAN_POINT('Ctrl Pts',(-25.4709166768101,20.1181193405628,9.18195042972386));
#60094=CARTESIAN_POINT('Ctrl Pts',(-25.3657850401848,20.0592863775806,9.18803792944176));
#60095=CARTESIAN_POINT('Ctrl Pts',(-25.2578627692656,20.0052408333131,9.19412542915967));
#60096=CARTESIAN_POINT('Ctrl Pts',(-25.1476298978777,19.9562471685924,9.20021292887757));
#60097=CARTESIAN_POINT('Ctrl Pts',(-25.0416638244199,19.9091499079532,9.20606479896096));
#60098=CARTESIAN_POINT('Ctrl Pts',(-24.9335631108894,19.8667208948667,9.21191666904436));
#60099=CARTESIAN_POINT('Ctrl Pts',(-24.8237781823305,19.8291476665807,9.21776853912775));
#60100=CARTESIAN_POINT('Ctrl Pts',(-24.714009969525,19.7915801591603,9.22361951821072));
#60101=CARTESIAN_POINT('Ctrl Pts',(-24.6025584425741,19.7588671003197,9.22947049729369));
#60102=CARTESIAN_POINT('Ctrl Pts',(-24.4898916195508,19.7311469577971,9.23532147637667));
#60103=CARTESIAN_POINT('Ctrl Pts',(-24.3772146666962,19.703424322967,9.24117298151895));
#60104=CARTESIAN_POINT('Ctrl Pts',(-24.2633226019928,19.6806955956168,9.24702448666124));
#60105=CARTESIAN_POINT('Ctrl Pts',(-24.1486954361764,19.6630485120838,9.25287599180353));
#60106=CARTESIAN_POINT('Ctrl Pts',(-24.0340302051732,19.6453955683385,9.25872944010331));
#60107=CARTESIAN_POINT('Ctrl Pts',(-23.9186297960107,19.6328276867713,9.26458288840309));
#60108=CARTESIAN_POINT('Ctrl Pts',(-23.8029804581881,19.6253808656177,9.27043633670287));
#60109=CARTESIAN_POINT('Ctrl Pts',(-23.6871996019558,19.6179255758114,9.27629644164441));
#60110=CARTESIAN_POINT('Ctrl Pts',(-23.5711696648056,19.615602997042,9.28215654658595));
#60111=CARTESIAN_POINT('Ctrl Pts',(-23.4553781258636,19.618397009537,9.28801665152749));
#60112=CARTESIAN_POINT('Ctrl Pts',(-23.3395086085669,19.6211929036245,9.29388070288295));
#60113=CARTESIAN_POINT('Ctrl Pts',(-23.2238782205669,19.6291122218805,9.29974475423841));
#60114=CARTESIAN_POINT('Ctrl Pts',(-23.1089688004609,19.6420870197757,9.30560880559387));
#60115=CARTESIAN_POINT('Ctrl Pts',(-22.993890026808,19.655080939933,9.31148149939044));
#60116=CARTESIAN_POINT('Ctrl Pts',(-22.8795347485061,19.6731451457662,9.31735419318701));
#60117=CARTESIAN_POINT('Ctrl Pts',(-22.7663741969737,19.6961607117766,9.32322688698358));
#60118=CARTESIAN_POINT('Ctrl Pts',(-22.7353927309093,19.7024619887468,9.32483473230689));
#60119=CARTESIAN_POINT('Ctrl Pts',(-22.7045007255135,19.7091341193546,9.32644257763021));
#60120=CARTESIAN_POINT('Ctrl Pts',(-22.6737076247133,19.7161740210158,9.32805042295352));
#60121=CARTESIAN_POINT('Ctrl Pts',(-22.5612426818085,19.7418856940143,9.33392271992222));
#60122=CARTESIAN_POINT('Ctrl Pts',(-22.4497215887658,19.7725930341085,9.33979501689092));
#60123=CARTESIAN_POINT('Ctrl Pts',(-22.3396221568778,19.8082125672401,9.34566731385962));
#60124=CARTESIAN_POINT('Ctrl Pts',(-22.2296654051097,19.8437859402855,9.35153200079782));
#60125=CARTESIAN_POINT('Ctrl Pts',(-22.1211270403851,19.884258720983,9.35739668773601));
#60126=CARTESIAN_POINT('Ctrl Pts',(-22.0144741959979,19.9294965465986,9.3632613746742));
#60127=CARTESIAN_POINT('Ctrl Pts',(-21.9079310373844,19.9746878479425,9.36912003014902));
#60128=CARTESIAN_POINT('Ctrl Pts',(-21.8032699203359,20.0246342863084,9.37497868562384));
#60129=CARTESIAN_POINT('Ctrl Pts',(-21.7009416859858,20.0791520727698,9.38083734109866));
#60130=CARTESIAN_POINT('Ctrl Pts',(-21.5946164206724,20.1357993719891,9.38692484081657));
#60131=CARTESIAN_POINT('Ctrl Pts',(-21.4908104349089,20.1973822814301,9.39301234053447));
#60132=CARTESIAN_POINT('Ctrl Pts',(-21.3900057026632,20.2636398928727,9.39909984025238));
#60133=CARTESIAN_POINT('Ctrl Pts',(-21.2931028321534,20.3273328624275,9.40495171033577));
#60134=CARTESIAN_POINT('Ctrl Pts',(-21.1989735731815,20.3953451261943,9.41080358041916));
#60135=CARTESIAN_POINT('Ctrl Pts',(-21.108019177812,20.4673991058587,9.41665545050255));
#60136=CARTESIAN_POINT('Ctrl Pts',(-21.0170786310761,20.5394421146497,9.42250642958552));
#60137=CARTESIAN_POINT('Ctrl Pts',(-20.9293123107232,20.6155253591264,9.42835740866849));
#60138=CARTESIAN_POINT('Ctrl Pts',(-20.8450896955939,20.6953299355138,9.43420838775146));
#60139=CARTESIAN_POINT('Ctrl Pts',(-20.7608595080411,20.7751416871005,9.44005989289374));
#60140=CARTESIAN_POINT('Ctrl Pts',(-20.6801739591736,20.8586751513727,9.44591139803602));
#60141=CARTESIAN_POINT('Ctrl Pts',(-20.603366329196,20.9455739124543,9.4517629031783));
#60142=CARTESIAN_POINT('Ctrl Pts',(-20.5265331930761,21.0325015307231,9.45761635147808));
#60143=CARTESIAN_POINT('Ctrl Pts',(-20.4535808101237,21.1227963583906,9.46346979977786));
#60144=CARTESIAN_POINT('Ctrl Pts',(-20.3848023047259,21.2160687641672,9.46932324807764));
#60145=CARTESIAN_POINT('Ctrl Pts',(-20.3159455832326,21.3094472409228,9.47518335301919));
#60146=CARTESIAN_POINT('Ctrl Pts',(-20.2512724588572,21.4058097215403,9.48104345796073));
#60147=CARTESIAN_POINT('Ctrl Pts',(-20.1910328728978,21.5047373682314,9.48690356290228));
#60148=CARTESIAN_POINT('Ctrl Pts',(-20.1307527193476,21.603731636501,9.49276761425773));
#60149=CARTESIAN_POINT('Ctrl Pts',(-20.0749122480346,21.7052941492416,9.49863166561318));
#60150=CARTESIAN_POINT('Ctrl Pts',(-20.0237147502748,21.8089828006584,9.50449571696863));
#60151=CARTESIAN_POINT('Ctrl Pts',(-19.9724417976234,21.9128242684489,9.51036841076519));
#60152=CARTESIAN_POINT('Ctrl Pts',(-19.9258256412901,22.0187977518141,9.51624110456176));
#60153=CARTESIAN_POINT('Ctrl Pts',(-19.8840209478159,22.1264425115816,9.52211379835832));
#60154=CARTESIAN_POINT('Ctrl Pts',(-19.8725755220495,22.1559138461296,9.52372164368168));
#60155=CARTESIAN_POINT('Ctrl Pts',(-19.8614904589547,22.1855103780289,9.52532948900504));
#60156=CARTESIAN_POINT('Ctrl Pts',(-19.8507682699444,22.2152224956778,9.52693733432841));
#60157=CARTESIAN_POINT('Ctrl Pts',(-19.8116078624674,22.3237393883593,9.53280963129712));
#60158=CARTESIAN_POINT('Ctrl Pts',(-19.7771605843996,22.4341625741623,9.53868192826584));
#60159=CARTESIAN_POINT('Ctrl Pts',(-19.7476144848749,22.5460449411623,9.54455422523456));
#60160=CARTESIAN_POINT('Ctrl Pts',(-19.7181066747487,22.6577823174997,9.55041891217275));
#60161=CARTESIAN_POINT('Ctrl Pts',(-19.6934875168102,22.770974718556,9.55628359911094));
#60162=CARTESIAN_POINT('Ctrl Pts',(-19.6738964747858,22.8851565084995,9.56214828604914));
#60163=CARTESIAN_POINT('Ctrl Pts',(-19.6543255809215,22.9992208696208,9.56800694152399));
#60164=CARTESIAN_POINT('Ctrl Pts',(-19.6397725868679,23.114272190741,9.57386559699884));
#60165=CARTESIAN_POINT('Ctrl Pts',(-19.6303265666629,23.2298318259442,9.5797242524737));
#60166=CARTESIAN_POINT('Ctrl Pts',(-19.6205115765887,23.3499053222813,9.5858117521916));
#60167=CARTESIAN_POINT('Ctrl Pts',(-19.6162107756016,23.4705272130242,9.5918992519095));
#60168=CARTESIAN_POINT('Ctrl Pts',(-19.6174651846001,23.5911509734333,9.5979867516274));
#60169=CARTESIAN_POINT('Ctrl Pts',(-19.6186710390282,23.7071057344349,9.60383862171081));
#60170=CARTESIAN_POINT('Ctrl Pts',(-19.6250100427651,23.8230617711427,9.60969049179422));
#60171=CARTESIAN_POINT('Ctrl Pts',(-19.6364655582687,23.9385314606164,9.61554236187763));
#60172=CARTESIAN_POINT('Ctrl Pts',(-19.6479193295659,24.0539835687796,9.6213933409606));
#60173=CARTESIAN_POINT('Ctrl Pts',(-19.6644880228585,24.1689490656949,9.62724432004356));
#60174=CARTESIAN_POINT('Ctrl Pts',(-19.6861030580268,24.2829447216045,9.63309529912653));
#60175=CARTESIAN_POINT('Ctrl Pts',(-19.7077200365947,24.3969506268206,9.63894680426882));
#60176=CARTESIAN_POINT('Ctrl Pts',(-19.7343841819661,24.5099861115191,9.64479830941112));
#60177=CARTESIAN_POINT('Ctrl Pts',(-19.7659757875636,24.6215781235813,9.65064981455341));
#60178=CARTESIAN_POINT('Ctrl Pts',(-19.7975778840457,24.7332071929219,9.65650326285319));
#60179=CARTESIAN_POINT('Ctrl Pts',(-19.8341105818946,24.8433914389366,9.66235671115298));
#60180=CARTESIAN_POINT('Ctrl Pts',(-19.8754045239268,24.9516736389307,9.66821015945276));
#60181=CARTESIAN_POINT('Ctrl Pts',(-19.9167454261378,25.0600789792991,9.67407026439431));
#60182=CARTESIAN_POINT('Ctrl Pts',(-19.9628582324617,25.1665775698071,9.67993036933586));
#60183=CARTESIAN_POINT('Ctrl Pts',(-20.0135256715073,25.2707327310666,9.68579047427741));
#60184=CARTESIAN_POINT('Ctrl Pts',(-20.0642272319021,25.3749580343087,9.69165452563288));
#60185=CARTESIAN_POINT('Ctrl Pts',(-20.1194893359217,25.4768364034066,9.69751857698835));
#60186=CARTESIAN_POINT('Ctrl Pts',(-20.1790499201176,25.5759578290411,9.70338262834383));
#60187=CARTESIAN_POINT('Ctrl Pts',(-20.2386982847252,25.6752253398705,9.70925532214042));
#60188=CARTESIAN_POINT('Ctrl Pts',(-20.3026575456328,25.7717274546252,9.71512801593701));
#60189=CARTESIAN_POINT('Ctrl Pts',(-20.3706236790665,25.8650850006944,9.7210007097336));
#60190=CARTESIAN_POINT('Ctrl Pts',(-20.389231669465,25.8906447351257,9.72260855505684));
#60191=CARTESIAN_POINT('Ctrl Pts',(-20.4081397817965,25.915968964871,9.72421640038009));
#60192=CARTESIAN_POINT('Ctrl Pts',(-20.4273412871845,25.9410503815583,9.72582424570333));
#60193=CARTESIAN_POINT('Ctrl Pts',(-20.4974705093515,26.0326546702633,9.73169654267202));
#60194=CARTESIAN_POINT('Ctrl Pts',(-20.5717511741554,26.121324156364,9.73756883964072));
#60195=CARTESIAN_POINT('Ctrl Pts',(-20.6499087673609,26.2066589480193,9.74344113660941));
#60196=CARTESIAN_POINT('Ctrl Pts',(-20.7279650745329,26.2918831525619,9.7493058235476));
#60197=CARTESIAN_POINT('Ctrl Pts',(-20.8098880421657,26.3737809545392,9.7551705104858));
#60198=CARTESIAN_POINT('Ctrl Pts',(-20.8953613090781,26.451983324872,9.761035197424));
#60199=CARTESIAN_POINT('Ctrl Pts',(-20.980746672086,26.5301052689622,9.7668938528988));
#60200=CARTESIAN_POINT('Ctrl Pts',(-21.069674768672,26.6045390634698,9.77275250837361));
#60201=CARTESIAN_POINT('Ctrl Pts',(-21.1617910542897,26.6749510405035,9.77861116384841));
#60202=CARTESIAN_POINT('Ctrl Pts',(-21.2575054831589,26.7481133713783,9.78469866356632));
#60203=CARTESIAN_POINT('Ctrl Pts',(-21.3566619384073,26.8169329528803,9.79078616328422));
#60204=CARTESIAN_POINT('Ctrl Pts',(-21.4588227931366,26.8810798536485,9.79687366300213));
#60205=CARTESIAN_POINT('Ctrl Pts',(-21.5570292945226,26.9427438120784,9.80272553308551));
#60206=CARTESIAN_POINT('Ctrl Pts',(-21.6580115539928,27.000089855443,9.8085774031689));
#60207=CARTESIAN_POINT('Ctrl Pts',(-21.761350332889,27.0528684003144,9.81442927325229));
#60208=CARTESIAN_POINT('Ctrl Pts',(-21.8646733775168,27.1056389091726,9.82028025233526));
#60209=CARTESIAN_POINT('Ctrl Pts',(-21.9703518601126,27.1538431143281,9.82613123141824));
#60210=CARTESIAN_POINT('Ctrl Pts',(-22.0779421609116,27.1972775072168,9.83198221050121));
#60211=CARTESIAN_POINT('Ctrl Pts',(-22.1855421351137,27.2407158052754,9.8378337156435));
#60212=CARTESIAN_POINT('Ctrl Pts',(-22.2950538858743,27.2793832837907,9.84368522078579));
#60213=CARTESIAN_POINT('Ctrl Pts',(-22.4060147200292,27.3131249491907,9.84953672592807));
#60214=CARTESIAN_POINT('Ctrl Pts',(-22.5170124018609,27.346877819463,9.8553901742278));
#60215=CARTESIAN_POINT('Ctrl Pts',(-22.6294597286488,27.3757015038207,9.86124362252752));
#60216=CARTESIAN_POINT('Ctrl Pts',(-22.7428804865309,27.3994913370541,9.86709707082725));
#60217=CARTESIAN_POINT('Ctrl Pts',(-22.8564302284443,27.423308224494,9.87295717576878));
#60218=CARTESIAN_POINT('Ctrl Pts',(-22.9709552061766,27.4420797498071,9.87881728071031));
#60219=CARTESIAN_POINT('Ctrl Pts',(-23.0859705896342,27.4557526633389,9.88467738565183));
#60220=CARTESIAN_POINT('Ctrl Pts',(-23.2010634287541,27.4694347847223,9.89054143700728));
#60221=CARTESIAN_POINT('Ctrl Pts',(-23.3166469199654,27.4780114268376,9.89640548836271));
#60222=CARTESIAN_POINT('Ctrl Pts',(-23.4322344591452,27.4814814406426,9.90226953971816));
#60223=CARTESIAN_POINT('Ctrl Pts',(-23.547992351284,27.4849565685553,9.90814223351471));
#60224=CARTESIAN_POINT('Ctrl Pts',(-23.6637538915088,27.4833100532698,9.91401492731127));
#60225=CARTESIAN_POINT('Ctrl Pts',(-23.779035737802,27.4765927162176,9.91988762110782));
#60226=CARTESIAN_POINT('Ctrl Pts',(-23.8105979788894,27.4747536216999,9.92149546643126));
#60227=CARTESIAN_POINT('Ctrl Pts',(-23.8421243145612,27.4725347292978,9.9231033117547));
#60228=CARTESIAN_POINT('Ctrl Pts',(-23.873604958918,27.4699377496433,9.92471115707814));
#60229=CARTESIAN_POINT('Ctrl Pts',(-23.9885810015351,27.4604528598152,9.93058345404684));
#60230=CARTESIAN_POINT('Ctrl Pts',(-24.1033319762176,27.4458889064202,9.93645575101554));
#60231=CARTESIAN_POINT('Ctrl Pts',(-24.2173730606687,27.4262606843973,9.94232804798424));
#60232=CARTESIAN_POINT('Ctrl Pts',(-24.3312663569315,27.4066578989912,9.94819273492245));
#60233=CARTESIAN_POINT('Ctrl Pts',(-24.4444511888035,27.382003965661,9.95405742186065));
#60234=CARTESIAN_POINT('Ctrl Pts',(-24.5564460792985,27.3523655685146,9.95992210879885));
#60235=CARTESIAN_POINT('Ctrl Pts',(-24.6683257900591,27.3227576526044,9.96578076427366));
#60236=CARTESIAN_POINT('Ctrl Pts',(-24.7790175963813,27.2881755742929,9.97163941974847));
#60237=CARTESIAN_POINT('Ctrl Pts',(-24.8880491315122,27.2487372562152,9.97749807522328));
#60238=CARTESIAN_POINT('Ctrl Pts',(-25.0013395344395,27.2077584426965,9.98358557494119));
#60239=CARTESIAN_POINT('Ctrl Pts',(-25.1128368706313,27.1615363544954,9.9896730746591));
#60240=CARTESIAN_POINT('Ctrl Pts',(-25.2220270074075,27.1102608325769,9.99576057437701));
#60241=CARTESIAN_POINT('Ctrl Pts',(-25.326990707516,27.06097003888,10.0016124444604));
#60242=CARTESIAN_POINT('Ctrl Pts',(-25.4298220881502,27.0070099371923,10.0074643145438));
#60243=CARTESIAN_POINT('Ctrl Pts',(-25.5300845543172,26.9485983296077,10.0133161846272));
#60244=CARTESIAN_POINT('Ctrl Pts',(-25.6303317546121,26.8901956157214,10.0191671637101));
#60245=CARTESIAN_POINT('Ctrl Pts',(-25.7280104610633,26.8273429516219,10.0250181427931));
#60246=CARTESIAN_POINT('Ctrl Pts',(-25.8227096632119,26.7603035570541,10.0308691218761));
#60247=CARTESIAN_POINT('Ctrl Pts',(-25.9174173797301,26.6932581349997,10.0367206270184));
#60248=CARTESIAN_POINT('Ctrl Pts',(-26.0091447219964,26.6220254730379,10.0425721321607));
#60249=CARTESIAN_POINT('Ctrl Pts',(-26.0975111860478,26.5469110620944,10.0484236373029));
#60250=CARTESIAN_POINT('Ctrl Pts',(-26.185906994679,26.4717717072897,10.0542770856028));
#60251=CARTESIAN_POINT('Ctrl Pts',(-26.2709393910506,26.3927483079109,10.0601305339026));
#60252=CARTESIAN_POINT('Ctrl Pts',(-26.3522629047852,26.3101849346872,10.0659839822024));
#60253=CARTESIAN_POINT('Ctrl Pts',(-26.4336789010134,26.2275276689804,10.0718440871439));
#60254=CARTESIAN_POINT('Ctrl Pts',(-26.5113773057353,26.1413226888989,10.0777041920854));
#60255=CARTESIAN_POINT('Ctrl Pts',(-26.585051247904,26.0519491064392,10.083564297027));
#60256=CARTESIAN_POINT('Ctrl Pts',(-26.6587748048618,25.9625153364655,10.0894283483824));
#60257=CARTESIAN_POINT('Ctrl Pts',(-26.7284682547061,25.8699090446739,10.0952923997379));
#60258=CARTESIAN_POINT('Ctrl Pts',(-26.7938676005712,25.7745389981715,10.1011564510933));
#60259=CARTESIAN_POINT('Ctrl Pts',(-26.8593633320171,25.6790283952582,10.1070291448899));
#60260=CARTESIAN_POINT('Ctrl Pts',(-26.9205521110534,25.5807462578784,10.1129018386864));
#60261=CARTESIAN_POINT('Ctrl Pts',(-26.977215427752,25.4801267009194,10.118774532483));
#60262=CARTESIAN_POINT('Ctrl Pts',(-26.9927288960029,25.4525787493833,10.1203823778064));
#60263=CARTESIAN_POINT('Ctrl Pts',(-27.0079034255219,25.4248557088185,10.1219902231297));
#60264=CARTESIAN_POINT('Ctrl Pts',(-27.0227351657991,25.3969667369354,10.1235980684531));
#60265=CARTESIAN_POINT('Ctrl Pts',(-27.0799881477026,25.289310671451,10.1298046185599));
#60266=CARTESIAN_POINT('Ctrl Pts',(-27.1323036867167,25.1788532239254,10.1360111686667));
#60267=CARTESIAN_POINT('Ctrl Pts',(-27.1794144389584,25.0660601879827,10.1422177187735));
#60268=CARTESIAN_POINT('Ctrl Pts',(-27.2264356367954,24.9534815640945,10.1484124706417));
#60269=CARTESIAN_POINT('Ctrl Pts',(-27.2682716265022,24.8385765123253,10.1546072225098));
#60270=CARTESIAN_POINT('Ctrl Pts',(-27.304701012513,24.7218350532766,10.1608019743779));
#60271=CARTESIAN_POINT('Ctrl Pts',(-27.3410394327568,24.6053851027469,10.1669812576803));
#60272=CARTESIAN_POINT('Ctrl Pts',(-27.3719980621105,24.4871082138234,10.1731605409826));
#60273=CARTESIAN_POINT('Ctrl Pts',(-27.3974039812322,24.3675130313621,10.1793398242849));
#60274=CARTESIAN_POINT('Ctrl Pts',(-27.4227708432076,24.2481017055262,10.1855096080225));
#60275=CARTESIAN_POINT('Ctrl Pts',(-27.4426019248462,24.127376457047,10.1916793917601));
#60276=CARTESIAN_POINT('Ctrl Pts',(-27.4567739781773,24.0058611226663,10.1978491754977));
#60277=CARTESIAN_POINT('Ctrl Pts',(-27.4709185023618,23.8845818312486,10.2040069744595));
#60278=CARTESIAN_POINT('Ctrl Pts',(-27.4794258697771,23.7625158535628,10.2101647734214));
#60279=CARTESIAN_POINT('Ctrl Pts',(-27.4822239293042,23.640196560829,10.2163225723832));
#60280=CARTESIAN_POINT('Ctrl Pts',(-27.4829076246993,23.6103082984926,10.2178272075611));
#60281=CARTESIAN_POINT('Ctrl Pts',(-27.4832506848561,23.5804049575549,10.219331842739));
#60282=CARTESIAN_POINT('Ctrl Pts',(-27.4832525242572,23.5504943982643,10.220836477917));
#60283=CARTESIAN_POINT('',(-27.4832508647148,23.5466314190111,11.4708364779651));
#60284=CARTESIAN_POINT('Ctrl Pts',(-27.4832525242573,23.5504943973073,10.2208364779651));
#60285=CARTESIAN_POINT('Ctrl Pts',(-27.4832599837499,23.429194869929,10.2269383878019));
#60286=CARTESIAN_POINT('Ctrl Pts',(-27.477651540728,23.3079927501158,10.2330402976386));
#60287=CARTESIAN_POINT('Ctrl Pts',(-27.4664800506225,23.187415074988,10.2391422074754));
#60288=CARTESIAN_POINT('Ctrl Pts',(-27.4552948215406,23.0666891104377,10.2452516215926));
#60289=CARTESIAN_POINT('Ctrl Pts',(-27.4385329343121,22.9465894793983,10.2513610357098));
#60290=CARTESIAN_POINT('Ctrl Pts',(-27.4162986599985,22.8276348362125,10.257470449827));
#60291=CARTESIAN_POINT('Ctrl Pts',(-27.3940139545882,22.7084103837659,10.2635937211292));
#60292=CARTESIAN_POINT('Ctrl Pts',(-27.3662321195515,22.5903364639223,10.2697169924315));
#60293=CARTESIAN_POINT('Ctrl Pts',(-27.3331081374179,22.473919652774,10.2758402637338));
#60294=CARTESIAN_POINT('Ctrl Pts',(-27.2999435623553,22.35736017462,10.2819710390105));
#60295=CARTESIAN_POINT('Ctrl Pts',(-27.2614238943629,22.2424621963302,10.2881018142873));
#60296=CARTESIAN_POINT('Ctrl Pts',(-27.2177527405278,22.1297134726727,10.2942325895641));
#60297=CARTESIAN_POINT('Ctrl Pts',(-27.1739841470157,22.0167131825178,10.3003770439106));
#60298=CARTESIAN_POINT('Ctrl Pts',(-27.1250412370664,21.9058720615225,10.3065214982572));
#60299=CARTESIAN_POINT('Ctrl Pts',(-27.0711746862601,21.7976555496452,10.3126659526038));
#60300=CARTESIAN_POINT('Ctrl Pts',(-27.0424812173744,21.7400111103785,10.3159389616785));
#60301=CARTESIAN_POINT('Ctrl Pts',(-27.0123914487368,21.6831109281034,10.3192119707533));
#60302=CARTESIAN_POINT('Ctrl Pts',(-26.9809482499123,21.6270219451551,10.322484979828));
#60303=CARTESIAN_POINT('Ctrl Pts',(-26.9245341682743,21.5263894210691,10.3283572767967));
#60304=CARTESIAN_POINT('Ctrl Pts',(-26.8635940462272,21.4280726043284,10.3342295737654));
#60305=CARTESIAN_POINT('Ctrl Pts',(-26.7983428459281,21.3325063084802,10.3401018707341));
#60306=CARTESIAN_POINT('Ctrl Pts',(-26.7331762060025,21.2370638589619,10.3459665576723));
#60307=CARTESIAN_POINT('Ctrl Pts',(-26.6637098289418,21.1443651801547,10.3518312446105));
#60308=CARTESIAN_POINT('Ctrl Pts',(-26.5902044815023,21.0548204763463,10.3576959315487));
#60309=CARTESIAN_POINT('Ctrl Pts',(-26.516774729711,20.9653678636601,10.3635545870235));
#60310=CARTESIAN_POINT('Ctrl Pts',(-26.4393145304274,20.8790630917514,10.3694132424984));
#60311=CARTESIAN_POINT('Ctrl Pts',(-26.3581274671624,20.7962867826753,10.3752718979732));
#60312=CARTESIAN_POINT('Ctrl Pts',(-26.2737691656977,20.7102771580581,10.3813593976911));
#60313=CARTESIAN_POINT('Ctrl Pts',(-26.185387172064,20.6280776409253,10.387446897409));
#60314=CARTESIAN_POINT('Ctrl Pts',(-26.0933678410765,20.5500769496348,10.3935343971269));
#60315=CARTESIAN_POINT('Ctrl Pts',(-26.0049103141682,20.4750954411338,10.3993862672103));
#60316=CARTESIAN_POINT('Ctrl Pts',(-25.9130921406373,20.403994045741,10.4052381372937));
#60317=CARTESIAN_POINT('Ctrl Pts',(-25.818292880096,20.337079337168,10.4110900073771));
#60318=CARTESIAN_POINT('Ctrl Pts',(-25.7235080536041,20.2701748169679,10.4169409864601));
#60319=CARTESIAN_POINT('Ctrl Pts',(-25.6257433802275,20.2074559544305,10.4227919655431));
#60320=CARTESIAN_POINT('Ctrl Pts',(-25.5254090948665,20.1491871764037,10.428642944626));
#60321=CARTESIAN_POINT('Ctrl Pts',(-25.4250657884878,20.0909131594531,10.4344944497683));
#60322=CARTESIAN_POINT('Ctrl Pts',(-25.3221527683472,20.0370902299994,10.4403459549106));
#60323=CARTESIAN_POINT('Ctrl Pts',(-25.2171060371046,19.9879374990924,10.4461974600529));
#60324=CARTESIAN_POINT('Ctrl Pts',(-25.1120244221296,19.9387684456335,10.4520509083527));
#60325=CARTESIAN_POINT('Ctrl Pts',(-25.0048080613511,19.8942728496352,10.4579043566524));
#60326=CARTESIAN_POINT('Ctrl Pts',(-24.8959134861679,19.8546219230423,10.4637578049522));
#60327=CARTESIAN_POINT('Ctrl Pts',(-24.7868950742064,19.8149259047357,10.4696179098937));
#60328=CARTESIAN_POINT('Ctrl Pts',(-24.6761950272078,19.780085694034,10.4754780148353));
#60329=CARTESIAN_POINT('Ctrl Pts',(-24.5642857048657,19.7502228313224,10.4813381197768));
#60330=CARTESIAN_POINT('Ctrl Pts',(-24.4523010185992,19.7203398578419,10.4872021711323));
#60331=CARTESIAN_POINT('Ctrl Pts',(-24.3391058381589,19.6954409953037,10.4930662224877));
#60332=CARTESIAN_POINT('Ctrl Pts',(-24.225181675889,19.6755964630455,10.4989302738432));
#60333=CARTESIAN_POINT('Ctrl Pts',(-24.1110896121454,19.655722683908,10.5048029676397));
#60334=CARTESIAN_POINT('Ctrl Pts',(-23.9962668307793,19.6409181546278,10.5106756614363));
#60335=CARTESIAN_POINT('Ctrl Pts',(-23.8811989931845,19.6312011873473,10.5165483552328));
#60336=CARTESIAN_POINT('Ctrl Pts',(-23.8496953441007,19.6285408442509,10.5181562005562));
#60337=CARTESIAN_POINT('Ctrl Pts',(-23.8181733178316,19.6262615495909,10.5197640458795));
#60338=CARTESIAN_POINT('Ctrl Pts',(-23.7866428440123,19.6243629993408,10.5213718912029));
#60339=CARTESIAN_POINT('Ctrl Pts',(-23.6714848103734,19.6174289673683,10.5272441881716));
#60340=CARTESIAN_POINT('Ctrl Pts',(-23.555828503464,19.6155545071208,10.5331164851403));
#60341=CARTESIAN_POINT('Ctrl Pts',(-23.4401559353756,19.6187938024845,10.538988782109));
#60342=CARTESIAN_POINT('Ctrl Pts',(-23.3246332697492,19.6220288999786,10.5448534690472));
#60343=CARTESIAN_POINT('Ctrl Pts',(-23.2090947942574,19.6303645628526,10.5507181559854));
#60344=CARTESIAN_POINT('Ctrl Pts',(-23.0940265761364,19.6438031364664,10.5565828429236));
#60345=CARTESIAN_POINT('Ctrl Pts',(-22.9790766984739,19.6572278893487,10.5624414983984));
#60346=CARTESIAN_POINT('Ctrl Pts',(-22.8645965243403,19.6757450667168,10.5683001538732));
#60347=CARTESIAN_POINT('Ctrl Pts',(-22.7510703772143,19.6993050010258,10.5741588093481));
#60348=CARTESIAN_POINT('Ctrl Pts',(-22.6331097987892,19.7237852071202,10.580246309066));
#60349=CARTESIAN_POINT('Ctrl Pts',(-22.5161797515239,19.753710137564,10.5863338087839));
#60350=CARTESIAN_POINT('Ctrl Pts',(-22.4008161118513,19.7889648643203,10.5924213085018));
#60351=CARTESIAN_POINT('Ctrl Pts',(-22.2899178674166,19.822854981834,10.5982731785852));
#60352=CARTESIAN_POINT('Ctrl Pts',(-22.1804674552739,19.8616698333616,10.6041250486686));
#60353=CARTESIAN_POINT('Ctrl Pts',(-22.0729279690916,19.9052558051208,10.609976918752));
#60354=CARTESIAN_POINT('Ctrl Pts',(-21.9654048567738,19.9488351405195,10.615827897835));
#60355=CARTESIAN_POINT('Ctrl Pts',(-21.8597924749099,19.9971839965083,10.6216788769179));
#60356=CARTESIAN_POINT('Ctrl Pts',(-21.7565350395982,20.0501001695035,10.6275298560009));
#60357=CARTESIAN_POINT('Ctrl Pts',(-21.6532683204493,20.1030211001721,10.6333813611432));
#60358=CARTESIAN_POINT('Ctrl Pts',(-21.5523573366669,20.1605099756308,10.6392328662855));
#60359=CARTESIAN_POINT('Ctrl Pts',(-21.4542221079744,20.2223184183378,10.6450843714278));
#60360=CARTESIAN_POINT('Ctrl Pts',(-21.3560542907092,20.2841473862829,10.6509378197276));
#60361=CARTESIAN_POINT('Ctrl Pts',(-21.2606644110128,20.3502985535691,10.6567912680273));
#60362=CARTESIAN_POINT('Ctrl Pts',(-21.168443286942,20.4204803799852,10.6626447163271));
#60363=CARTESIAN_POINT('Ctrl Pts',(-21.0761172874275,20.4907420183779,10.6685048212686));
#60364=CARTESIAN_POINT('Ctrl Pts',(-20.9869675652956,20.5650432144048,10.6743649262102));
#60365=CARTESIAN_POINT('Ctrl Pts',(-20.9013517049511,20.6430522616612,10.6802250311517));
#60366=CARTESIAN_POINT('Ctrl Pts',(-20.815678187683,20.7211138431287,10.6860890825072));
#60367=CARTESIAN_POINT('Ctrl Pts',(-20.7335435631579,20.8028879569104,10.6919531338626));
#60368=CARTESIAN_POINT('Ctrl Pts',(-20.6552671859175,20.888007455121,10.6978171852181));
#60369=CARTESIAN_POINT('Ctrl Pts',(-20.5768754449228,20.9732524024802,10.7036898790146));
#60370=CARTESIAN_POINT('Ctrl Pts',(-20.5023535650337,21.0618522592839,10.7095625728112));
#60371=CARTESIAN_POINT('Ctrl Pts',(-20.4319794731352,21.1534083289424,10.7154352666078));
#60372=CARTESIAN_POINT('Ctrl Pts',(-20.4127122239881,21.1784748492689,10.7170431119311));
#60373=CARTESIAN_POINT('Ctrl Pts',(-20.3937556236361,21.2037628034635,10.7186509572544));
#60374=CARTESIAN_POINT('Ctrl Pts',(-20.3751147836853,21.2292636732183,10.7202588025778));
#60375=CARTESIAN_POINT('Ctrl Pts',(-20.3070332671685,21.3223999208331,10.7261310995465));
#60376=CARTESIAN_POINT('Ctrl Pts',(-20.2429391154088,21.4186902871183,10.7320033965152));
#60377=CARTESIAN_POINT('Ctrl Pts',(-20.1831384621879,21.5177585359016,10.7378756934839));
#60378=CARTESIAN_POINT('Ctrl Pts',(-20.1234153058645,21.6166984001021,10.7437403804221));
#60379=CARTESIAN_POINT('Ctrl Pts',(-20.0679747948712,21.7184086372237,10.7496050673603));
#60380=CARTESIAN_POINT('Ctrl Pts',(-20.0170816423457,21.8224815785119,10.7554697542985));
#60381=CARTESIAN_POINT('Ctrl Pts',(-19.9662408302416,21.9264474872952,10.7613284097733));
#60382=CARTESIAN_POINT('Ctrl Pts',(-19.919938254969,22.0327708979367,10.7671870652482));
#60383=CARTESIAN_POINT('Ctrl Pts',(-19.878393927761,22.1410174935541,10.773045720723));
#60384=CARTESIAN_POINT('Ctrl Pts',(-19.8352268425406,22.2534922965384,10.7791332204409));
#60385=CARTESIAN_POINT('Ctrl Pts',(-19.7971975410473,22.3680432006966,10.7852207201588));
#60386=CARTESIAN_POINT('Ctrl Pts',(-19.7644989963251,22.4841572407186,10.7913082198767));
#60387=CARTESIAN_POINT('Ctrl Pts',(-19.7330661183788,22.5957768396601,10.7971600899601));
#60388=CARTESIAN_POINT('Ctrl Pts',(-19.7065591165186,22.708840380511,10.8030119600435));
#60389=CARTESIAN_POINT('Ctrl Pts',(-19.6850990746519,22.8228752200368,10.808863830127));
#60390=CARTESIAN_POINT('Ctrl Pts',(-19.6636423002717,22.9368926967214,10.8147148092099));
#60391=CARTESIAN_POINT('Ctrl Pts',(-19.6472310344,23.0518807718897,10.8205657882929));
#60392=CARTESIAN_POINT('Ctrl Pts',(-19.6359352774022,23.167356419476,10.8264167673759));
#60393=CARTESIAN_POINT('Ctrl Pts',(-19.6246385048072,23.2828424494341,10.8322682725182));
#60394=CARTESIAN_POINT('Ctrl Pts',(-19.6184581956386,23.3988157275114,10.8381197776605));
#60395=CARTESIAN_POINT('Ctrl Pts',(-19.6174124241694,23.5147886254762,10.8439712828028));
#60396=CARTESIAN_POINT('Ctrl Pts',(-19.6163663054223,23.6308000355159,10.8498247311025));
#60397=CARTESIAN_POINT('Ctrl Pts',(-19.6204581185209,23.746810652045,10.8556781794023));
#60398=CARTESIAN_POINT('Ctrl Pts',(-19.6296538395216,23.8623340834315,10.8615316277021));
#60399=CARTESIAN_POINT('Ctrl Pts',(-19.638860018054,23.9779888900451,10.8673917326436));
#60400=CARTESIAN_POINT('Ctrl Pts',(-19.6531816567781,24.0931549933546,10.8732518375851));
#60401=CARTESIAN_POINT('Ctrl Pts',(-19.6725329750599,24.207352250227,10.8791119425267));
#60402=CARTESIAN_POINT('Ctrl Pts',(-19.6918973252433,24.321626411804,10.8849759938821));
#60403=CARTESIAN_POINT('Ctrl Pts',(-19.7162980127044,24.4349300246412,10.8908400452375));
#60404=CARTESIAN_POINT('Ctrl Pts',(-19.7455987744352,24.5467959514079,10.896704096593));
#60405=CARTESIAN_POINT('Ctrl Pts',(-19.7749427196399,24.6588267462206,10.9025767903895));
#60406=CARTESIAN_POINT('Ctrl Pts',(-19.8092010304325,24.7694152327351,10.9084494841861));
#60407=CARTESIAN_POINT('Ctrl Pts',(-19.848188507946,24.8781120739913,10.9143221779827));
#60408=CARTESIAN_POINT('Ctrl Pts',(-19.8588626271084,24.9078714508511,10.915930023306));
#60409=CARTESIAN_POINT('Ctrl Pts',(-19.8698909611422,24.9374891680603,10.9175378686294));
#60410=CARTESIAN_POINT('Ctrl Pts',(-19.8812691064921,24.9669563206325,10.9191457139527));
#60411=CARTESIAN_POINT('Ctrl Pts',(-19.9228252484156,25.0745785329279,10.9250180109214));
#60412=CARTESIAN_POINT('Ctrl Pts',(-19.9691903429848,25.1805510432062,10.9308903078901));
#60413=CARTESIAN_POINT('Ctrl Pts',(-20.020213334682,25.2844129243793,10.9367626048588));
#60414=CARTESIAN_POINT('Ctrl Pts',(-20.0711702046341,25.3881402088028,10.942627291797));
#60415=CARTESIAN_POINT('Ctrl Pts',(-20.1267727871619,25.489761935863,10.9484919787352));
#60416=CARTESIAN_POINT('Ctrl Pts',(-20.1868211923751,25.5888350357117,10.9543566656733));
#60417=CARTESIAN_POINT('Ctrl Pts',(-20.2468078415624,25.6878062450789,10.9602153211481));
#60418=CARTESIAN_POINT('Ctrl Pts',(-20.3112310060147,25.7842336893521,10.9660739766229));
#60419=CARTESIAN_POINT('Ctrl Pts',(-20.3798442130501,25.8776975027025,10.9719326320977));
#60420=CARTESIAN_POINT('Ctrl Pts',(-20.4511375123865,25.974812094925,10.9780201318156));
#60421=CARTESIAN_POINT('Ctrl Pts',(-20.5269546603845,26.0687264041915,10.9841076315335));
#60422=CARTESIAN_POINT('Ctrl Pts',(-20.606968400833,26.1590007995461,10.9901951312514));
#60423=CARTESIAN_POINT('Ctrl Pts',(-20.683885039139,26.2457809322692,10.9960470013348));
#60424=CARTESIAN_POINT('Ctrl Pts',(-20.7646791348476,26.3291973546086,11.0018988714182));
#60425=CARTESIAN_POINT('Ctrl Pts',(-20.8490184962602,26.4088927129365,11.0077507415016));
#60426=CARTESIAN_POINT('Ctrl Pts',(-20.9333450162381,26.4885759369214,11.0136017205845));
#60427=CARTESIAN_POINT('Ctrl Pts',(-21.0212154282485,26.5645389395703,11.0194526996675));
#60428=CARTESIAN_POINT('Ctrl Pts',(-21.112261192523,26.636461732336,11.0253036787504));
#60429=CARTESIAN_POINT('Ctrl Pts',(-21.203315142688,26.7083909916531,11.0311551838927));
#60430=CARTESIAN_POINT('Ctrl Pts',(-21.2975446882551,26.7762790627085,11.037006689035));
#60431=CARTESIAN_POINT('Ctrl Pts',(-21.3945493493224,26.8398471555821,11.0428581941773));
#60432=CARTESIAN_POINT('Ctrl Pts',(-21.4915862235257,26.9034363580353,11.0487116424771));
#60433=CARTESIAN_POINT('Ctrl Pts',(-21.5913997001102,26.9627025032952,11.0545650907769));
#60434=CARTESIAN_POINT('Ctrl Pts',(-21.6935621782513,27.0174113009795,11.0604185390766));
#60435=CARTESIAN_POINT('Ctrl Pts',(-21.7958408373142,27.0721823144466,11.0662786440181));
#60436=CARTESIAN_POINT('Ctrl Pts',(-21.9004734651811,27.1223854405725,11.0721387489597));
#60437=CARTESIAN_POINT('Ctrl Pts',(-22.007009741309,27.1678333103257,11.0779988539012));
#60438=CARTESIAN_POINT('Ctrl Pts',(-22.1136177629511,27.2133117863747,11.0838629052566));
#60439=CARTESIAN_POINT('Ctrl Pts',(-22.2221315994582,27.2540284846328,11.0897269566121));
#60440=CARTESIAN_POINT('Ctrl Pts',(-22.3320845844241,27.2898455379241,11.0955910079675));
#60441=CARTESIAN_POINT('Ctrl Pts',(-22.4421996181414,27.3257153784023,11.1014637017641));
#60442=CARTESIAN_POINT('Ctrl Pts',(-22.5537576366229,27.3566710518781,11.1073363955606));
#60443=CARTESIAN_POINT('Ctrl Pts',(-22.6662804973064,27.3826254835897,11.1132090893572));
#60444=CARTESIAN_POINT('Ctrl Pts',(-22.6970873742863,27.3897313728283,11.1148169346806));
#60445=CARTESIAN_POINT('Ctrl Pts',(-22.7279665387796,27.3964626821058,11.1164247800041));
#60446=CARTESIAN_POINT('Ctrl Pts',(-22.7589081185634,27.4028183026846,11.1180326253275));
#60447=CARTESIAN_POINT('Ctrl Pts',(-22.871915347879,27.4260307914202,11.1239049222962));
#60448=CARTESIAN_POINT('Ctrl Pts',(-22.9861340979795,27.4443056937332,11.1297772192649));
#60449=CARTESIAN_POINT('Ctrl Pts',(-23.1010949312611,27.4575209445337,11.1356495162336));
#60450=CARTESIAN_POINT('Ctrl Pts',(-23.2159067844326,27.4707190694187,11.1415142031718));
#60451=CARTESIAN_POINT('Ctrl Pts',(-23.3314584014597,27.4788705353511,11.14737889011));
#60452=CARTESIAN_POINT('Ctrl Pts',(-23.4472689712856,27.4819040150133,11.1532435770482));
#60453=CARTESIAN_POINT('Ctrl Pts',(-23.5629604371909,27.4849343749316,11.159102232523));
#60454=CARTESIAN_POINT('Ctrl Pts',(-23.6789099154205,27.4828572072494,11.1649608879978));
#60455=CARTESIAN_POINT('Ctrl Pts',(-23.7946309368751,27.4756529182893,11.1708195434726));
#60456=CARTESIAN_POINT('Ctrl Pts',(-23.9148721233533,27.468167223457,11.1769070431906));
#60457=CARTESIAN_POINT('Ctrl Pts',(-24.0348661900667,27.4551456502361,11.1829945429085));
#60458=CARTESIAN_POINT('Ctrl Pts',(-24.1540663722603,27.4366258855989,11.1890820426264));
#60459=CARTESIAN_POINT('Ctrl Pts',(-24.2686526576711,27.4188229678734,11.1949339127098));
#60460=CARTESIAN_POINT('Ctrl Pts',(-24.3825049272021,27.395939652118,11.2007857827932));
#60461=CARTESIAN_POINT('Ctrl Pts',(-24.4951429695548,27.3680622519971,11.2066376528766));
#60462=CARTESIAN_POINT('Ctrl Pts',(-24.6077638617413,27.3401890964639,11.2124886319595));
#60463=CARTESIAN_POINT('Ctrl Pts',(-24.7191704931788,27.30732346776,11.2183396110425));
#60464=CARTESIAN_POINT('Ctrl Pts',(-24.8288944407653,27.2696024572009,11.2241905901254));
#60465=CARTESIAN_POINT('Ctrl Pts',(-24.9386282535905,27.2318780551601,11.2300420952677));
#60466=CARTESIAN_POINT('Ctrl Pts',(-25.046678690865,27.189297537853,11.23589360041));
#60467=CARTESIAN_POINT('Ctrl Pts',(-25.1525947255868,27.1420471379699,11.2417451055523));
#60468=CARTESIAN_POINT('Ctrl Pts',(-25.2585459327178,27.0947810472577,11.247598553852));
#60469=CARTESIAN_POINT('Ctrl Pts',(-25.3623609505943,27.0428421586952,11.2534520021518));
#60470=CARTESIAN_POINT('Ctrl Pts',(-25.4636115304138,26.9864635761469,11.2593054504515));
#60471=CARTESIAN_POINT('Ctrl Pts',(-25.5649772541291,26.9300208789076,11.2651655553931));
#60472=CARTESIAN_POINT('Ctrl Pts',(-25.6637723575134,26.8691286114636,11.2710256603346));
#60473=CARTESIAN_POINT('Ctrl Pts',(-25.7595957865131,26.8040643551386,11.2768857652761));
#60474=CARTESIAN_POINT('Ctrl Pts',(-25.8554837465946,26.7389562821092,11.2827498166316));
#60475=CARTESIAN_POINT('Ctrl Pts',(-25.9483957168541,26.6696708722956,11.288613867987));
#60476=CARTESIAN_POINT('Ctrl Pts',(-26.0379634543475,26.596526216922,11.2944779193424));
#60477=CARTESIAN_POINT('Ctrl Pts',(-26.1276631968066,26.5232737609274,11.300350613139));
#60478=CARTESIAN_POINT('Ctrl Pts',(-26.2140085625529,26.4461509820488,11.3062233069355));
#60479=CARTESIAN_POINT('Ctrl Pts',(-26.2966678378037,26.365513082046,11.3120960007321));
#60480=CARTESIAN_POINT('Ctrl Pts',(-26.3192985646483,26.343435773931,11.3137038460556));
#60481=CARTESIAN_POINT('Ctrl Pts',(-26.3416532255523,26.3210951727694,11.315311691379));
#60482=CARTESIAN_POINT('Ctrl Pts',(-26.3637255513613,26.2984989849086,11.3169195367024));
#60483=CARTESIAN_POINT('Ctrl Pts',(-26.443276563939,26.2170599177125,11.3227143824589));
#60484=CARTESIAN_POINT('Ctrl Pts',(-26.5194391806909,26.1320095390702,11.3285092282153));
#60485=CARTESIAN_POINT('Ctrl Pts',(-26.5918609065626,26.0436653522937,11.3343040739718));
#60486=CARTESIAN_POINT('Ctrl Pts',(-26.664166907015,25.9554623340401,11.3400896599246));
#60487=CARTESIAN_POINT('Ctrl Pts',(-26.7327436429163,25.8639763052162,11.3458752458775));
#60488=CARTESIAN_POINT('Ctrl Pts',(-26.797274995011,25.7695619113698,11.3516608318304));
#60489=CARTESIAN_POINT('Ctrl Pts',(-26.8617474105324,25.6752337463202,11.3574411337996));
#60490=CARTESIAN_POINT('Ctrl Pts',(-26.9221815439285,25.5779828781755,11.3632214357688));
#60491=CARTESIAN_POINT('Ctrl Pts',(-26.9783013276128,25.4781971504011,11.369001737738));
#60492=CARTESIAN_POINT('Ctrl Pts',(-27.0343843040768,25.3784768689814,11.3747782485869));
#60493=CARTESIAN_POINT('Ctrl Pts',(-27.0861583463047,25.2762254011407,11.3805547594359));
#60494=CARTESIAN_POINT('Ctrl Pts',(-27.1333910325968,25.1718589831335,11.3863312702848));
#60495=CARTESIAN_POINT('Ctrl Pts',(-27.1806048955167,25.0675341576774,11.392105479054));
#60496=CARTESIAN_POINT('Ctrl Pts',(-27.2232808258136,24.9610964447608,11.3978796878231));
#60497=CARTESIAN_POINT('Ctrl Pts',(-27.2612330492045,24.8529852743008,11.4036538965923));
#60498=CARTESIAN_POINT('Ctrl Pts',(-27.299192984464,24.7448521357169,11.4094292786771));
#60499=CARTESIAN_POINT('Ctrl Pts',(-27.3324271438471,24.6350452581093,11.415204660762));
#60500=CARTESIAN_POINT('Ctrl Pts',(-27.3607986331734,24.5240222213549,11.4209800428468));
#60501=CARTESIAN_POINT('Ctrl Pts',(-27.3891719891915,24.41299187988,11.4267558049208));
#60502=CARTESIAN_POINT('Ctrl Pts',(-27.4126819414435,24.3007456345179,11.4325315669949));
#60503=CARTESIAN_POINT('Ctrl Pts',(-27.4312423860383,24.1877529242258,11.4383073290689));
#60504=CARTESIAN_POINT('Ctrl Pts',(-27.4498198554455,24.074656569881,11.4440883890368));
#60505=CARTESIAN_POINT('Ctrl Pts',(-27.4634386876286,23.9608128045669,11.4498694490047));
#60506=CARTESIAN_POINT('Ctrl Pts',(-27.4720645078,23.8466978454926,11.4556505089726));
#60507=CARTESIAN_POINT('Ctrl Pts',(-27.4796174155358,23.7467769405775,11.4607124986368));
#60508=CARTESIAN_POINT('Ctrl Pts',(-27.4833429503497,23.6466483696507,11.4657744883009));
#60509=CARTESIAN_POINT('Ctrl Pts',(-27.4832508647148,23.5466314190111,11.4708364779651));
#60510=CARTESIAN_POINT('',(-27.4846964008749,23.5516548132277,12.7208364779651));
#60511=CARTESIAN_POINT('Ctrl Pts',(-27.4835131464095,23.5466311775283,11.4708364779651));
#60512=CARTESIAN_POINT('Ctrl Pts',(-27.4862622880016,23.2504300277655,11.4858264680025));
#60513=CARTESIAN_POINT('Ctrl Pts',(-27.3202535819363,21.6472835327814,11.567112095165));
#60514=CARTESIAN_POINT('Ctrl Pts',(-25.1236967614753,19.1724649525787,11.714693359452));
#60515=CARTESIAN_POINT('Ctrl Pts',(-20.7176596990131,19.8601077274406,11.9135802708271));
#60516=CARTESIAN_POINT('Ctrl Pts',(-18.9145352855183,23.9386807047295,12.1124671822019));
#60517=CARTESIAN_POINT('Ctrl Pts',(-21.3712419772517,27.660321124278,12.311354093577));
#60518=CARTESIAN_POINT('Ctrl Pts',(-25.8302746188912,27.6051569835897,12.5102410049518));
#60519=CARTESIAN_POINT('Ctrl Pts',(-27.4525860600378,25.010103460541,12.6467351330812));
#60520=CARTESIAN_POINT('Ctrl Pts',(-27.4895040349668,23.6284897608082,12.7169336240856));
#60521=CARTESIAN_POINT('Ctrl Pts',(-27.4891511394909,23.5516564009483,12.7208364779651));
#60522=CARTESIAN_POINT('',(-27.482741765581,23.5531935453585,13.9708364359043));
#60523=CARTESIAN_POINT('Ctrl Pts',(-27.4832522818912,23.5516542985269,12.7208364779651));
#60524=CARTESIAN_POINT('Ctrl Pts',(-27.4832930552431,23.4372546857449,12.7266562861414));
#60525=CARTESIAN_POINT('Ctrl Pts',(-27.4783382662288,23.3226513759092,12.7324760943177));
#60526=CARTESIAN_POINT('Ctrl Pts',(-27.4683607881123,23.208321703911,12.7382959024941));
#60527=CARTESIAN_POINT('Ctrl Pts',(-27.4583958193384,23.0941353736489,12.7441084140396));
#60528=CARTESIAN_POINT('Ctrl Pts',(-27.4434207162572,22.9802224150746,12.7499209255851));
#60529=CARTESIAN_POINT('Ctrl Pts',(-27.423460347452,22.8670613315512,12.7557334371306));
#60530=CARTESIAN_POINT('Ctrl Pts',(-27.4035194302777,22.7540105249298,12.7615402843103));
#60531=CARTESIAN_POINT('Ctrl Pts',(-27.3786029801996,22.6417105489896,12.7673471314901));
#60532=CARTESIAN_POINT('Ctrl Pts',(-27.3487877011582,22.5306351689815,12.7731539786698));
#60533=CARTESIAN_POINT('Ctrl Pts',(-27.3189918880954,22.4196323085352,12.7789570346403));
#60534=CARTESIAN_POINT('Ctrl Pts',(-27.2843037141321,22.3098528600586,12.7847600906107));
#60535=CARTESIAN_POINT('Ctrl Pts',(-27.2448508933787,22.2017600601401,12.7905631465812));
#60536=CARTESIAN_POINT('Ctrl Pts',(-27.2054112340786,22.0937033199585,12.7963642666533));
#60537=CARTESIAN_POINT('Ctrl Pts',(-27.1612102309948,21.9873325055485,12.8021653867254));
#60538=CARTESIAN_POINT('Ctrl Pts',(-27.11242513171,21.8830946604364,12.8079665067975));
#60539=CARTESIAN_POINT('Ctrl Pts',(-27.063643982512,21.7788652553715,12.813767157158));
#60540=CARTESIAN_POINT('Ctrl Pts',(-27.0102796537688,21.6767688577968,12.8195678075185));
#60541=CARTESIAN_POINT('Ctrl Pts',(-26.9525567705978,21.5772307715662,12.825368457879));
#60542=CARTESIAN_POINT('Ctrl Pts',(-26.8948239780363,21.4776755974545,12.8311701040475));
#60543=CARTESIAN_POINT('Ctrl Pts',(-26.8327313557761,21.380679971763,12.836971750216));
#60544=CARTESIAN_POINT('Ctrl Pts',(-26.7665481149689,21.2866422028151,12.8427733963845));
#60545=CARTESIAN_POINT('Ctrl Pts',(-26.7002959762773,21.1925065389433,12.8485810821658));
#60546=CARTESIAN_POINT('Ctrl Pts',(-26.6299449589489,21.1013352252773,12.8543887679471));
#60547=CARTESIAN_POINT('Ctrl Pts',(-26.5558060586206,21.0134953504133,12.8601964537284));
#60548=CARTESIAN_POINT('Ctrl Pts',(-26.4816264793564,20.925607279088,12.8660073261023));
#60549=CARTESIAN_POINT('Ctrl Pts',(-26.4036551647765,20.8410545951663,12.8718181984763));
#60550=CARTESIAN_POINT('Ctrl Pts',(-26.322240325152,20.7601678245713,12.8776290708503));
#60551=CARTESIAN_POINT('Ctrl Pts',(-26.2406953369027,20.6791517495154,12.8834492324036));
#60552=CARTESIAN_POINT('Ctrl Pts',(-26.1556961415334,20.6018135745485,12.8892693939569));
#60553=CARTESIAN_POINT('Ctrl Pts',(-26.0676246149804,20.5284440013119,12.8950895555102));
#60554=CARTESIAN_POINT('Ctrl Pts',(-26.0024289188029,20.4741315510499,12.899397979574));
#60555=CARTESIAN_POINT('Ctrl Pts',(-25.9355503310069,20.4219929789331,12.9037064036378));
#60556=CARTESIAN_POINT('Ctrl Pts',(-25.8671533126791,20.3721304806912,12.9080148277016));
#60557=CARTESIAN_POINT('Ctrl Pts',(-25.7739295265685,20.304168879664,12.9138871246703));
#60558=CARTESIAN_POINT('Ctrl Pts',(-25.6775567558279,20.2401986991976,12.919759421639));
#60559=CARTESIAN_POINT('Ctrl Pts',(-25.5784116302886,20.1805255886336,12.9256317186077));
#60560=CARTESIAN_POINT('Ctrl Pts',(-25.479394988958,20.1209298096817,12.9314964055459));
#60561=CARTESIAN_POINT('Ctrl Pts',(-25.3776134884321,20.0656202377682,12.9373610924841));
#60562=CARTESIAN_POINT('Ctrl Pts',(-25.273475137793,20.0148610611736,12.9432257794223));
#60563=CARTESIAN_POINT('Ctrl Pts',(-25.1694438869288,19.9641540872148,12.9490844348971));
#60564=CARTESIAN_POINT('Ctrl Pts',(-25.0630609765168,19.917988380251,12.9549430903719));
#60565=CARTESIAN_POINT('Ctrl Pts',(-24.954761006217,19.8765833924012,12.9608017458467));
#60566=CARTESIAN_POINT('Ctrl Pts',(-24.8422307436875,19.8335610892568,12.9668892455646));
#60567=CARTESIAN_POINT('Ctrl Pts',(-24.7276309936318,19.795679237366,12.9729767452825));
#60568=CARTESIAN_POINT('Ctrl Pts',(-24.6114749692762,19.7631301494662,12.9790642450005));
#60569=CARTESIAN_POINT('Ctrl Pts',(-24.4998150110944,19.7318409432979,12.9849161150839));
#60570=CARTESIAN_POINT('Ctrl Pts',(-24.3867174514184,19.7054794673777,12.9907679851673));
#60571=CARTESIAN_POINT('Ctrl Pts',(-24.2726550889171,19.6841661972576,12.9966198552507));
#60572=CARTESIAN_POINT('Ctrl Pts',(-24.158610093448,19.6628561722766,13.0024708343336));
#60573=CARTESIAN_POINT('Ctrl Pts',(-24.043600993476,19.6465929007108,13.0083218134166));
#60574=CARTESIAN_POINT('Ctrl Pts',(-23.9281109047522,19.6354457612507,13.0141727924996));
#60575=CARTESIAN_POINT('Ctrl Pts',(-23.8126104323579,19.6242976195555,13.0200242976419));
#60576=CARTESIAN_POINT('Ctrl Pts',(-23.6966292967386,19.6182665641003,13.0258758027842));
#60577=CARTESIAN_POINT('Ctrl Pts',(-23.5806551489824,19.6173700416035,13.0317273079265));
#60578=CARTESIAN_POINT('Ctrl Pts',(-23.4646424887362,19.6164732213911,13.0375807562262));
#60579=CARTESIAN_POINT('Ctrl Pts',(-23.3486372341189,19.6207143277486,13.043434204526));
#60580=CARTESIAN_POINT('Ctrl Pts',(-23.2331257325736,19.6300587108124,13.0492876528258));
#60581=CARTESIAN_POINT('Ctrl Pts',(-23.1174828693683,19.6394137204689,13.0551477577673));
#60582=CARTESIAN_POINT('Ctrl Pts',(-23.0023352922621,19.6538835571578,13.0610078627089));
#60583=CARTESIAN_POINT('Ctrl Pts',(-22.8881630335975,19.6733818224095,13.0668679676504));
#60584=CARTESIAN_POINT('Ctrl Pts',(-22.7739138870627,19.6928932185223,13.0727320190059));
#60585=CARTESIAN_POINT('Ctrl Pts',(-22.6606417698388,19.7174396987215,13.0785960703613));
#60586=CARTESIAN_POINT('Ctrl Pts',(-22.5488136435096,19.7468843989424,13.0844601217167));
#60587=CARTESIAN_POINT('Ctrl Pts',(-22.436820704845,19.7763724947739,13.0903328155133));
#60588=CARTESIAN_POINT('Ctrl Pts',(-22.3262763976908,19.810773095985,13.0962055093099));
#60589=CARTESIAN_POINT('Ctrl Pts',(-22.2176298202984,19.8499004256005,13.1020782031064));
#60590=CARTESIAN_POINT('Ctrl Pts',(-22.1878842048435,19.860612833929,13.1036860484298));
#60591=CARTESIAN_POINT('Ctrl Pts',(-22.1582807047688,19.8716792745307,13.1052938937531));
#60592=CARTESIAN_POINT('Ctrl Pts',(-22.1288282193865,19.8830953323938,13.1069017390765));
#60593=CARTESIAN_POINT('Ctrl Pts',(-22.0212595757361,19.9247899413284,13.1127740360452));
#60594=CARTESIAN_POINT('Ctrl Pts',(-21.9153468214851,19.9712913758882,13.1186463330139));
#60595=CARTESIAN_POINT('Ctrl Pts',(-21.8115506889431,20.0224479875033,13.1245186299826));
#60596=CARTESIAN_POINT('Ctrl Pts',(-21.7078890679457,20.0735383042125,13.1303833169208));
#60597=CARTESIAN_POINT('Ctrl Pts',(-21.606338981239,20.1292716199616,13.136248003859));
#60598=CARTESIAN_POINT('Ctrl Pts',(-21.5073432410617,20.1894474748295,13.1421126907972));
#60599=CARTESIAN_POINT('Ctrl Pts',(-21.4084493118058,20.2495614425978,13.147971346272));
#60600=CARTESIAN_POINT('Ctrl Pts',(-21.3121048549879,20.3141086483293,13.1538300017469));
#60601=CARTESIAN_POINT('Ctrl Pts',(-21.2187294188977,20.3828420792116,13.1596886572217));
#60602=CARTESIAN_POINT('Ctrl Pts',(-21.1217066560299,20.4542602984438,13.1657761569396));
#60603=CARTESIAN_POINT('Ctrl Pts',(-21.0278899953097,20.530198244076,13.1718636566575));
#60604=CARTESIAN_POINT('Ctrl Pts',(-20.9377186461754,20.6103280943972,13.1779511563754));
#60605=CARTESIAN_POINT('Ctrl Pts',(-20.8510375710491,20.6873563482964,13.1838030264588));
#60606=CARTESIAN_POINT('Ctrl Pts',(-20.7677251935074,20.7682577275535,13.1896548965422));
#60607=CARTESIAN_POINT('Ctrl Pts',(-20.6881384393773,20.8526995808587,13.1955067666256));
#60608=CARTESIAN_POINT('Ctrl Pts',(-20.6085638030542,20.937128577124,13.2013577457086));
#60609=CARTESIAN_POINT('Ctrl Pts',(-20.5327139457,21.0250966748513,13.2072087247916));
#60610=CARTESIAN_POINT('Ctrl Pts',(-20.4609083813151,21.1162349227772,13.2130597038745));
#60611=CARTESIAN_POINT('Ctrl Pts',(-20.3890963609188,21.2073813649086,13.2189112090168));
#60612=CARTESIAN_POINT('Ctrl Pts',(-20.3213296121823,21.3016981991171,13.2247627141591));
#60613=CARTESIAN_POINT('Ctrl Pts',(-20.2578864094083,21.3987845870517,13.2306142193014));
#60614=CARTESIAN_POINT('Ctrl Pts',(-20.1944221385279,21.4959032152621,13.2364676676012));
#60615=CARTESIAN_POINT('Ctrl Pts',(-20.1352844945324,21.5957928801159,13.242321115901));
#60616=CARTESIAN_POINT('Ctrl Pts',(-20.0807072173211,21.6980256796289,13.2481745642008));
#60617=CARTESIAN_POINT('Ctrl Pts',(-20.0260678738943,21.8003747400344,13.2540346691423));
#60618=CARTESIAN_POINT('Ctrl Pts',(-19.9759994434011,21.9050718887787,13.2598947740839));
#60619=CARTESIAN_POINT('Ctrl Pts',(-19.9306887151902,22.0116665645623,13.2657548790254));
#60620=CARTESIAN_POINT('Ctrl Pts',(-19.8853474730397,22.1183330251887,13.2716189303809));
#60621=CARTESIAN_POINT('Ctrl Pts',(-19.8447704573727,22.226899171064,13.2774829817363));
#60622=CARTESIAN_POINT('Ctrl Pts',(-19.8090949346873,22.3368981587441,13.2833470330918));
#60623=CARTESIAN_POINT('Ctrl Pts',(-19.7733668334029,22.447059262974,13.2892197268884));
#60624=CARTESIAN_POINT('Ctrl Pts',(-19.7425547520611,22.5586570266223,13.2950924206849));
#60625=CARTESIAN_POINT('Ctrl Pts',(-19.7167451500187,22.6712131954641,13.3009651144815));
#60626=CARTESIAN_POINT('Ctrl Pts',(-19.7096789127216,22.7020291916575,13.3025729598048));
#60627=CARTESIAN_POINT('Ctrl Pts',(-19.7029873481038,22.7329169932492,13.3041808051281));
#60628=CARTESIAN_POINT('Ctrl Pts',(-19.696671552197,22.7638667265975,13.3057886504514));
#60629=CARTESIAN_POINT('Ctrl Pts',(-19.6736045142047,22.8769037350026,13.3116609474201));
#60630=CARTESIAN_POINT('Ctrl Pts',(-19.6554766176795,22.9911459088993,13.3175332443888));
#60631=CARTESIAN_POINT('Ctrl Pts',(-19.6424093234802,23.1061236539844,13.3234055413575));
#60632=CARTESIAN_POINT('Ctrl Pts',(-19.6293589634565,23.2209523970433,13.3292702282957));
#60633=CARTESIAN_POINT('Ctrl Pts',(-19.6213562102248,23.3365144086873,13.3351349152339));
#60634=CARTESIAN_POINT('Ctrl Pts',(-19.6184717722774,23.4523287864651,13.3409996021721));
#60635=CARTESIAN_POINT('Ctrl Pts',(-19.6155903007938,23.5680240564051,13.3468582576469));
#60636=CARTESIAN_POINT('Ctrl Pts',(-19.6178166847231,23.6839707654648,13.3527169131217));
#60637=CARTESIAN_POINT('Ctrl Pts',(-19.6251698916784,23.7996824197319,13.3585755685965));
#60638=CARTESIAN_POINT('Ctrl Pts',(-19.632810321374,23.9199138731327,13.3646630683144));
#60639=CARTESIAN_POINT('Ctrl Pts',(-19.64598630685,24.0398910827279,13.3707505680323));
#60640=CARTESIAN_POINT('Ctrl Pts',(-19.6646594575217,24.1590673327158,13.3768380677502));
#60641=CARTESIAN_POINT('Ctrl Pts',(-19.6826098241487,24.2736306122677,13.3826899378336));
#60642=CARTESIAN_POINT('Ctrl Pts',(-19.7056396399772,24.3874533384701,13.388541807917));
#60643=CARTESIAN_POINT('Ctrl Pts',(-19.7336619734197,24.5000554115013,13.3943936780003));
#60644=CARTESIAN_POINT('Ctrl Pts',(-19.7616800402071,24.6126403398431,13.4002446570833));
#60645=CARTESIAN_POINT('Ctrl Pts',(-19.7946890133718,24.7240045835165,13.4060956361663));
#60646=CARTESIAN_POINT('Ctrl Pts',(-19.8325511988876,24.8336798962333,13.4119466152492));
#60647=CARTESIAN_POINT('Ctrl Pts',(-19.8704167885783,24.9433650698164,13.4177981203915));
#60648=CARTESIAN_POINT('Ctrl Pts',(-19.9131363231405,25.0513606197998,13.4236496255338));
#60649=CARTESIAN_POINT('Ctrl Pts',(-19.9605229896014,25.157215759222,13.4295011306761));
#60650=CARTESIAN_POINT('Ctrl Pts',(-20.0079253921428,25.2631060508317,13.4353545789759));
#60651=CARTESIAN_POINT('Ctrl Pts',(-20.0599978395555,25.366854141428,13.4412080272757));
#60652=CARTESIAN_POINT('Ctrl Pts',(-20.1165066770451,25.4680320825499,13.4470614755754));
#60653=CARTESIAN_POINT('Ctrl Pts',(-20.1730797773534,25.5693250849607,13.452921580517));
#60654=CARTESIAN_POINT('Ctrl Pts',(-20.2340991359933,25.6680417429184,13.4587816854585));
#60655=CARTESIAN_POINT('Ctrl Pts',(-20.2992866557453,25.7637813599267,13.4646417904));
#60656=CARTESIAN_POINT('Ctrl Pts',(-20.364518075212,25.8595854515748,13.4705058417554));
#60657=CARTESIAN_POINT('Ctrl Pts',(-20.4339229981362,25.9524081799576,13.4763698931109));
#60658=CARTESIAN_POINT('Ctrl Pts',(-20.5071828596569,26.0418817117944,13.4822339444663));
#60659=CARTESIAN_POINT('Ctrl Pts',(-20.5805506915894,26.1314871097565,13.4881066382629));
#60660=CARTESIAN_POINT('Ctrl Pts',(-20.6577845263789,26.2177331529788,13.4939793320594));
#60661=CARTESIAN_POINT('Ctrl Pts',(-20.7385287356696,26.3002885850704,13.499852025856));
#60662=CARTESIAN_POINT('Ctrl Pts',(-20.760635149489,26.3228908813947,13.5014598711794));
#60663=CARTESIAN_POINT('Ctrl Pts',(-20.7830045008615,26.3452167731694,13.5030677165028));
#60664=CARTESIAN_POINT('Ctrl Pts',(-20.8056290753783,26.3672600011626,13.5046755618262));
#60665=CARTESIAN_POINT('Ctrl Pts',(-20.8882602951966,26.4477679822721,13.5105478587949));
#60666=CARTESIAN_POINT('Ctrl Pts',(-20.9745752563114,26.524772023834,13.5164201557637));
#60667=CARTESIAN_POINT('Ctrl Pts',(-21.0642445359001,26.5979161031613,13.5222924527324));
#60668=CARTESIAN_POINT('Ctrl Pts',(-21.1537976112236,26.6709653935707,13.5281571396706));
#60669=CARTESIAN_POINT('Ctrl Pts',(-21.2466960431651,26.7401644104516,13.5340218266087));
#60670=CARTESIAN_POINT('Ctrl Pts',(-21.3425734613611,26.8051937174014,13.5398865135469));
#60671=CARTESIAN_POINT('Ctrl Pts',(-21.4383522756347,26.8701561457801,13.5457451690218));
#60672=CARTESIAN_POINT('Ctrl Pts',(-21.5371036422464,26.9309571632024,13.5516038244966));
#60673=CARTESIAN_POINT('Ctrl Pts',(-21.6384285185044,26.9873178413138,13.5574624799714));
#60674=CARTESIAN_POINT('Ctrl Pts',(-21.7437112336749,27.0458800171542,13.5635499796893));
#60675=CARTESIAN_POINT('Ctrl Pts',(-21.8517722518342,27.0996476074844,13.5696374794072));
#60676=CARTESIAN_POINT('Ctrl Pts',(-21.9621308600668,27.1483573878799,13.5757249791251));
#60677=CARTESIAN_POINT('Ctrl Pts',(-22.0682178034569,27.1951817525409,13.5815768492085));
#60678=CARTESIAN_POINT('Ctrl Pts',(-22.1764273645156,27.2373323908848,13.5874287192919));
#60679=CARTESIAN_POINT('Ctrl Pts',(-22.2863086369991,27.2746229256082,13.5932805893753));
#60680=CARTESIAN_POINT('Ctrl Pts',(-22.3961731790597,27.3119077825085,13.5991315684583));
#60681=CARTESIAN_POINT('Ctrl Pts',(-22.5077085351043,27.3443338743233,13.6049825475412));
#60682=CARTESIAN_POINT('Ctrl Pts',(-22.6204463322158,27.3717639383776,13.6108335266242));
#60683=CARTESIAN_POINT('Ctrl Pts',(-22.7331942655399,27.3991964686586,13.6166850317665));
#60684=CARTESIAN_POINT('Ctrl Pts',(-22.8471444531569,27.4216319804948,13.6225365369087));
#60685=CARTESIAN_POINT('Ctrl Pts',(-22.9618166601015,27.4389839733115,13.628388042051));
#60686=CARTESIAN_POINT('Ctrl Pts',(-23.0765269471901,27.4563417283473,13.6342414903508));
#60687=CARTESIAN_POINT('Ctrl Pts',(-23.191959321854,27.4686125458157,13.6400949386506));
#60688=CARTESIAN_POINT('Ctrl Pts',(-23.3076274435509,27.4757616791302,13.6459483869503));
#60689=CARTESIAN_POINT('Ctrl Pts',(-23.423427105019,27.4829189425616,13.6518084918918));
#60690=CARTESIAN_POINT('Ctrl Pts',(-23.5394626357905,27.4849428708623,13.6576685968334));
#60691=CARTESIAN_POINT('Ctrl Pts',(-23.6552465998438,27.481850838446,13.6635287017749));
#60692=CARTESIAN_POINT('Ctrl Pts',(-23.7711085371503,27.4787567237393,13.6693927531303));
#60693=CARTESIAN_POINT('Ctrl Pts',(-23.8867181590657,27.4705398173159,13.6752568044858));
#60694=CARTESIAN_POINT('Ctrl Pts',(-24.0015938034672,27.4572693036564,13.6811208558412));
#60695=CARTESIAN_POINT('Ctrl Pts',(-24.1166387516373,27.4439792319089,13.6869935496378));
#60696=CARTESIAN_POINT('Ctrl Pts',(-24.2309471567365,27.425620753443,13.6928662434344));
#60697=CARTESIAN_POINT('Ctrl Pts',(-24.3440480950026,27.402314006239,13.6987389372309));
#60698=CARTESIAN_POINT('Ctrl Pts',(-24.3750132399536,27.3959330087285,13.7003467825543));
#60699=CARTESIAN_POINT('Ctrl Pts',(-24.4058879700136,27.3891813890663,13.7019546278777));
#60700=CARTESIAN_POINT('Ctrl Pts',(-24.4366628492207,27.3820622541338,13.7035624732011));
#60701=CARTESIAN_POINT('Ctrl Pts',(-24.5490612418088,27.3560611992589,13.7094347701699));
#60702=CARTESIAN_POINT('Ctrl Pts',(-24.6605029296012,27.3250669231564,13.7153070671386));
#60703=CARTESIAN_POINT('Ctrl Pts',(-24.770510317737,27.2891641294191,13.7211793641073));
#60704=CARTESIAN_POINT('Ctrl Pts',(-24.8803751450342,27.2533078628513,13.7270440510455));
#60705=CARTESIAN_POINT('Ctrl Pts',(-24.9888089796828,27.2125558555647,13.7329087379836));
#60706=CARTESIAN_POINT('Ctrl Pts',(-25.0953450357647,27.1670436721757,13.7387734249218));
#60707=CARTESIAN_POINT('Ctrl Pts',(-25.2017715261828,27.1215782952179,13.7446320803967));
#60708=CARTESIAN_POINT('Ctrl Pts',(-25.3063037422964,27.0713626410672,13.7504907358715));
#60709=CARTESIAN_POINT('Ctrl Pts',(-25.4084913175092,27.0165816584351,13.7563493913464));
#60710=CARTESIAN_POINT('Ctrl Pts',(-25.5146704294149,26.9596608823714,13.7624368910643));
#60711=CARTESIAN_POINT('Ctrl Pts',(-25.6183175666323,26.8978109966629,13.7685243907822));
#60712=CARTESIAN_POINT('Ctrl Pts',(-25.7189514283267,26.8312941491908,13.7746118905001));
#60713=CARTESIAN_POINT('Ctrl Pts',(-25.815690042194,26.7673519778886,13.7804637605835));
#60714=CARTESIAN_POINT('Ctrl Pts',(-25.9096439365277,26.6990976655203,13.7863156306669));
#60715=CARTESIAN_POINT('Ctrl Pts',(-26.0004125750353,26.6268098222407,13.7921675007503));
#60716=CARTESIAN_POINT('Ctrl Pts',(-26.0911673931926,26.5545329854423,13.7980184798333));
#60717=CARTESIAN_POINT('Ctrl Pts',(-26.178737596551,26.4782240962994,13.8038694589162));
#60718=CARTESIAN_POINT('Ctrl Pts',(-26.2627545283017,26.3982030085109,13.8097204379992));
#60719=CARTESIAN_POINT('Ctrl Pts',(-26.3467790139833,26.3181747260564,13.8155719431415));
#60720=CARTESIAN_POINT('Ctrl Pts',(-26.4272492936185,26.2344338665853,13.8214234482839));
#60721=CARTESIAN_POINT('Ctrl Pts',(-26.5038330054651,26.1473377026039,13.8272749534262));
#60722=CARTESIAN_POINT('Ctrl Pts',(-26.5804421490952,26.0602126158826,13.833128401726));
#60723=CARTESIAN_POINT('Ctrl Pts',(-26.6531618857459,25.9697303193629,13.8389818500258));
#60724=CARTESIAN_POINT('Ctrl Pts',(-26.7217000948503,25.8762811975002,13.8448352983256));
#60725=CARTESIAN_POINT('Ctrl Pts',(-26.790316246781,25.7827258036941,13.8506954032671));
#60726=CARTESIAN_POINT('Ctrl Pts',(-26.8547411350955,25.6861971838299,13.8565555082086));
#60727=CARTESIAN_POINT('Ctrl Pts',(-26.9147258973461,25.5871148176181,13.8624156131502));
#60728=CARTESIAN_POINT('Ctrl Pts',(-26.9747510555795,25.4879657256342,13.8682796645056));
#60729=CARTESIAN_POINT('Ctrl Pts',(-27.0303299360249,25.3862598247289,13.874143715861));
#60730=CARTESIAN_POINT('Ctrl Pts',(-27.0812603859501,25.2824397424722,13.8800077672165));
#60731=CARTESIAN_POINT('Ctrl Pts',(-27.1322658971921,25.1784666501384,13.8858804610131));
#60732=CARTESIAN_POINT('Ctrl Pts',(-27.1786091400688,25.0723735351517,13.8917531548096));
#60733=CARTESIAN_POINT('Ctrl Pts',(-27.2201366344214,24.9646215332459,13.8976258486062));
#60734=CARTESIAN_POINT('Ctrl Pts',(-27.2315061677044,24.9351208375963,13.8992336939295));
#60735=CARTESIAN_POINT('Ctrl Pts',(-27.2425150172714,24.9054958725268,13.9008415392527));
#60736=CARTESIAN_POINT('Ctrl Pts',(-27.2531606964563,24.8757562560714,13.902449384576));
#60737=CARTESIAN_POINT('Ctrl Pts',(-27.2983956243064,24.7493886113882,13.9092813363875));
#60738=CARTESIAN_POINT('Ctrl Pts',(-27.3371941851859,24.6206022531953,13.9161132881989));
#60739=CARTESIAN_POINT('Ctrl Pts',(-27.3693286506375,24.490011329321,13.9229452400104));
#60740=CARTESIAN_POINT('Ctrl Pts',(-27.4013201927057,24.3600012303152,13.9297468055792));
#60741=CARTESIAN_POINT('Ctrl Pts',(-27.4267066893909,24.2282026987485,13.9365483711479));
#60742=CARTESIAN_POINT('Ctrl Pts',(-27.4453101639974,24.0952433949541,13.9433499367166));
#60743=CARTESIAN_POINT('Ctrl Pts',(-27.4637638403299,23.9633547016042,13.9500967349473));
#60744=CARTESIAN_POINT('Ctrl Pts',(-27.4755432042108,23.8303239872224,13.956843533178));
#60745=CARTESIAN_POINT('Ctrl Pts',(-27.4805219515887,23.6967833715941,13.9635903314086));
#60746=CARTESIAN_POINT('Ctrl Pts',(-27.4823043522775,23.6489755863823,13.966005697544));
#60747=CARTESIAN_POINT('Ctrl Pts',(-27.4832156005693,23.601102622559,13.9684210636793));
#60748=CARTESIAN_POINT('Ctrl Pts',(-27.483251431705,23.5531940472059,13.9708364298146));
#60749=CARTESIAN_POINT('',(-27.4784560775625,23.547708951101,15.2208364779651));
#60750=CARTESIAN_POINT('Ctrl Pts',(-27.4792215614382,23.5531900791572,13.9708364779651));
#60751=CARTESIAN_POINT('Ctrl Pts',(-27.4732738423167,22.6912517315234,14.0143364172937));
#60752=CARTESIAN_POINT('Ctrl Pts',(-26.7690121054188,20.5068472925696,14.1241319937473));
#60753=CARTESIAN_POINT('Ctrl Pts',(-23.1558588724936,18.9150390011558,14.3002232073257));
#60754=CARTESIAN_POINT('Ctrl Pts',(-19.4373831253637,21.3765331205073,14.4991101187006));
#60755=CARTESIAN_POINT('Ctrl Pts',(-19.498285648829,25.8354910777289,14.6979970300756));
#60756=CARTESIAN_POINT('Ctrl Pts',(-23.282602187513,28.1945085674187,14.8968839414505));
#60757=CARTESIAN_POINT('Ctrl Pts',(-26.8142260262799,26.5219956903167,15.0711637574136));
#60758=CARTESIAN_POINT('Ctrl Pts',(-27.4735806028515,24.3741591972422,15.1791479362519));
#60759=CARTESIAN_POINT('Ctrl Pts',(-27.4784560775625,23.547708951101,15.2208364779651));
#60760=CARTESIAN_POINT('',(-27.4851245771615,23.5482800713537,16.4708358638271));
#60761=CARTESIAN_POINT('Ctrl Pts',(-27.4784560775625,23.547708951101,15.2208364779651));
#60762=CARTESIAN_POINT('Ctrl Pts',(-27.4813338772278,23.0598880961595,15.2454435733768));
#60763=CARTESIAN_POINT('Ctrl Pts',(-27.1706132058826,21.2613315865969,15.3363463059134));
#60764=CARTESIAN_POINT('Ctrl Pts',(-24.4745249954599,18.9910342604509,15.4935446755753));
#60765=CARTESIAN_POINT('Ctrl Pts',(-20.2141141537653,20.308195845668,15.6924315869498));
#60766=CARTESIAN_POINT('Ctrl Pts',(-19.0193316234954,24.6045326442667,15.8913184983251));
#60767=CARTESIAN_POINT('Ctrl Pts',(-21.9880812491219,27.9320754076229,16.0902054096997));
#60768=CARTESIAN_POINT('Ctrl Pts',(-26.2657817837741,27.2531790242803,16.2833774930198));
#60769=CARTESIAN_POINT('Ctrl Pts',(-27.4811614233285,24.7414234327789,16.4102539392149));
#60770=CARTESIAN_POINT('Ctrl Pts',(-27.4885259363507,23.5483003261169,16.4708347482849));
#60771=CARTESIAN_POINT('',(-27.4832509670657,23.5537607171193,17.7208364779651));
#60772=CARTESIAN_POINT('Ctrl Pts',(-27.4832520314764,23.5482689205262,16.4708364779651));
#60773=CARTESIAN_POINT('Ctrl Pts',(-27.4831953477107,23.4358793426591,16.4765507294599));
#60774=CARTESIAN_POINT('Ctrl Pts',(-27.4783216466447,23.3236146971763,16.4822649809548));
#60775=CARTESIAN_POINT('Ctrl Pts',(-27.4686601516153,23.2117695570205,16.4879792324497));
#60776=CARTESIAN_POINT('Ctrl Pts',(-27.4587314377627,23.0968309901582,16.4938515294185));
#60777=CARTESIAN_POINT('Ctrl Pts',(-27.4437245671289,22.9821370985901,16.4997238263873));
#60778=CARTESIAN_POINT('Ctrl Pts',(-27.4236562063245,22.8681726438799,16.5055961233561));
#60779=CARTESIAN_POINT('Ctrl Pts',(-27.4036138525219,22.7543558780523,16.5114608102944));
#60780=CARTESIAN_POINT('Ctrl Pts',(-27.3785231236498,22.6412670725969,16.5173254972326));
#60781=CARTESIAN_POINT('Ctrl Pts',(-27.3484525621856,22.5293874434603,16.5231901841709));
#60782=CARTESIAN_POINT('Ctrl Pts',(-27.3184129264115,22.4176228755186,16.5290488396457));
#60783=CARTESIAN_POINT('Ctrl Pts',(-27.2834037515192,22.3070654072013,16.5349074951206));
#60784=CARTESIAN_POINT('Ctrl Pts',(-27.2435447829588,22.1981869464696,16.5407661505955));
#60785=CARTESIAN_POINT('Ctrl Pts',(-27.2021288879794,22.0850555971636,16.5468536503134));
#60786=CARTESIAN_POINT('Ctrl Pts',(-27.1554766799918,21.9737375442461,16.5529411500312));
#60787=CARTESIAN_POINT('Ctrl Pts',(-27.1037799834882,21.8647461836355,16.5590286497491));
#60788=CARTESIAN_POINT('Ctrl Pts',(-27.0540843176646,21.7599735656369,16.5648805198325));
#60789=CARTESIAN_POINT('Ctrl Pts',(-26.9997276110195,21.6573512782908,16.570732389916));
#60790=CARTESIAN_POINT('Ctrl Pts',(-26.9409293496113,21.5573150724549,16.5765842599994));
#60791=CARTESIAN_POINT('Ctrl Pts',(-26.8821400407731,21.4572940980409,16.5824352390823));
#60792=CARTESIAN_POINT('Ctrl Pts',(-26.8189107312199,21.3598587785107,16.5882862181653));
#60793=CARTESIAN_POINT('Ctrl Pts',(-26.7515062255472,21.2654191050321,16.5941371972483));
#60794=CARTESIAN_POINT('Ctrl Pts',(-26.6840956595608,21.170970940518,16.5999887023906));
#60795=CARTESIAN_POINT('Ctrl Pts',(-26.6125093913782,21.0795192939652,16.6058402075329));
#60796=CARTESIAN_POINT('Ctrl Pts',(-26.5370543786821,20.9914434870741,16.6116917126751));
#60797=CARTESIAN_POINT('Ctrl Pts',(-26.4615743090189,20.9033384321249,16.6175451609749));
#60798=CARTESIAN_POINT('Ctrl Pts',(-26.3822232090504,20.818611759726,16.6233986092747));
#60799=CARTESIAN_POINT('Ctrl Pts',(-26.299346480719,20.7376076093062,16.6292520575744));
#60800=CARTESIAN_POINT('Ctrl Pts',(-26.2163755035511,20.6565113395775,16.6351121625159));
#60801=CARTESIAN_POINT('Ctrl Pts',(-26.129871191171,20.5791463305167,16.6409722674575));
#60802=CARTESIAN_POINT('Ctrl Pts',(-26.0402138375049,20.5058179872236,16.646832372399));
#60803=CARTESIAN_POINT('Ctrl Pts',(-25.9504961052224,20.4324402618808,16.6526964237545));
#60804=CARTESIAN_POINT('Ctrl Pts',(-25.8576214340356,20.3631048619561,16.6585604751099));
#60805=CARTESIAN_POINT('Ctrl Pts',(-25.7619996072334,20.2980742041968,16.6644245264654));
#60806=CARTESIAN_POINT('Ctrl Pts',(-25.6662368529464,20.2329477042294,16.6702972202619));
#60807=CARTESIAN_POINT('Ctrl Pts',(-25.5677192129509,20.1721388247979,16.6761699140585));
#60808=CARTESIAN_POINT('Ctrl Pts',(-25.4668816425129,20.1158643981889,16.6820426078551));
#60809=CARTESIAN_POINT('Ctrl Pts',(-25.4392740025383,20.1004574015422,16.6836504531781));
#60810=CARTESIAN_POINT('Ctrl Pts',(-25.4114925834006,20.0853900170775,16.6852582985012));
#60811=CARTESIAN_POINT('Ctrl Pts',(-25.3835465576077,20.0706660599206,16.6868661438242));
#60812=CARTESIAN_POINT('Ctrl Pts',(-25.281479922094,20.0168900854908,16.6927384407929));
#60813=CARTESIAN_POINT('Ctrl Pts',(-25.1768741769919,19.9675187069325,16.6986107377616));
#60814=CARTESIAN_POINT('Ctrl Pts',(-25.0701461693482,19.9227999365224,16.7044830347303));
#60815=CARTESIAN_POINT('Ctrl Pts',(-24.9635564727262,19.8781391180872,16.7103477216685));
#60816=CARTESIAN_POINT('Ctrl Pts',(-24.8548503606384,19.8381190757424,16.7162124086067));
#60817=CARTESIAN_POINT('Ctrl Pts',(-24.7444697382494,19.8029422611711,16.7220770955449));
#60818=CARTESIAN_POINT('Ctrl Pts',(-24.6342026354205,19.7678016237515,16.7279357510197));
#60819=CARTESIAN_POINT('Ctrl Pts',(-24.5222648391915,19.7374944314917,16.7337944064945));
#60820=CARTESIAN_POINT('Ctrl Pts',(-24.4091181011403,19.7121750267941,16.7396530619694));
#60821=CARTESIAN_POINT('Ctrl Pts',(-24.2915517518424,19.685866623848,16.7457405616873));
#60822=CARTESIAN_POINT('Ctrl Pts',(-24.1726805100561,19.6649437824608,16.7518280614052));
#60823=CARTESIAN_POINT('Ctrl Pts',(-24.0530399936515,19.6495226297273,16.7579155611231));
#60824=CARTESIAN_POINT('Ctrl Pts',(-23.9380304181026,19.634698385536,16.7637674312065));
#60825=CARTESIAN_POINT('Ctrl Pts',(-23.8223104616508,19.6249578980686,16.7696193012899));
#60826=CARTESIAN_POINT('Ctrl Pts',(-23.706365370323,19.6203520518327,16.7754711713734));
#60827=CARTESIAN_POINT('Ctrl Pts',(-23.5904379326896,19.6157469068789,16.7813221504563));
#60828=CARTESIAN_POINT('Ctrl Pts',(-23.4742858412814,19.6162748651003,16.7871731295393));
#60829=CARTESIAN_POINT('Ctrl Pts',(-23.3583971666563,19.6219347595548,16.7930241086223));
#60830=CARTESIAN_POINT('Ctrl Pts',(-23.2424980725241,19.6275951628883,16.7988756137646));
#60831=CARTESIAN_POINT('Ctrl Pts',(-23.1268628551714,19.6383883995298,16.8047271189069));
#60832=CARTESIAN_POINT('Ctrl Pts',(-23.0119765679496,19.6542612602904,16.8105786240492));
#60833=CARTESIAN_POINT('Ctrl Pts',(-22.8970521294927,19.6701393920825,16.816432072349));
#60834=CARTESIAN_POINT('Ctrl Pts',(-22.7828775249739,19.6911004456078,16.8222855206488));
#60835=CARTESIAN_POINT('Ctrl Pts',(-22.6699289890613,19.7170398503672,16.8281389689486));
#60836=CARTESIAN_POINT('Ctrl Pts',(-22.5568520061372,19.7430087538624,16.8339990738902));
#60837=CARTESIAN_POINT('Ctrl Pts',(-22.445004277946,19.7739672161251,16.8398591788317));
#60838=CARTESIAN_POINT('Ctrl Pts',(-22.3348483119114,19.8097603738981,16.8457192837733));
#60839=CARTESIAN_POINT('Ctrl Pts',(-22.2246181627281,19.8455776361227,16.8515833351288));
#60840=CARTESIAN_POINT('Ctrl Pts',(-22.1160824304322,19.88623593227,16.8574473864842));
#60841=CARTESIAN_POINT('Ctrl Pts',(-22.0096833958758,19.9315323521606,16.8633114378397));
#60842=CARTESIAN_POINT('Ctrl Pts',(-21.9031275503816,19.9768955299321,16.8691841316363));
#60843=CARTESIAN_POINT('Ctrl Pts',(-21.7987150589729,20.0269102962088,16.8750568254329));
#60844=CARTESIAN_POINT('Ctrl Pts',(-21.696863458051,20.0813279228709,16.8809295192294));
#60845=CARTESIAN_POINT('Ctrl Pts',(-21.6689781934873,20.0962265587555,16.8825373645528));
#60846=CARTESIAN_POINT('Ctrl Pts',(-21.6412847153458,20.1114549727474,16.8841452098762));
#60847=CARTESIAN_POINT('Ctrl Pts',(-21.6137911914852,20.1270075100991,16.8857530551995));
#60848=CARTESIAN_POINT('Ctrl Pts',(-21.5133772185241,20.1838096891512,16.8916253521682));
#60849=CARTESIAN_POINT('Ctrl Pts',(-21.415296409598,20.2451289344945,16.8974976491369));
#60850=CARTESIAN_POINT('Ctrl Pts',(-21.3199827450967,20.310748606864,16.9033699461056));
#60851=CARTESIAN_POINT('Ctrl Pts',(-21.224792599535,20.3762832413495,16.9092346330438));
#60852=CARTESIAN_POINT('Ctrl Pts',(-21.1323628044818,20.4461069878894,16.915099319982));
#60853=CARTESIAN_POINT('Ctrl Pts',(-21.0431025544099,20.5199574979717,16.9209640069202));
#60854=CARTESIAN_POINT('Ctrl Pts',(-20.9539341029175,20.5937320574274,16.926822662395));
#60855=CARTESIAN_POINT('Ctrl Pts',(-20.8679290293262,20.6715248812851,16.9326813178698));
#60856=CARTESIAN_POINT('Ctrl Pts',(-20.7854667807917,20.7530309188064,16.9385399733446));
#60857=CARTESIAN_POINT('Ctrl Pts',(-20.6997834841974,20.8377206539431,16.9446274730625));
#60858=CARTESIAN_POINT('Ctrl Pts',(-20.6179258011946,20.926419341357,16.9507149727804));
#60859=CARTESIAN_POINT('Ctrl Pts',(-20.5402809556218,21.0187391283648,16.9568024724983));
#60860=CARTESIAN_POINT('Ctrl Pts',(-20.4656415190728,21.1074854815033,16.9626543425817));
#60861=CARTESIAN_POINT('Ctrl Pts',(-20.3948951413588,21.1995774760393,16.9685062126651));
#60862=CARTESIAN_POINT('Ctrl Pts',(-20.3283469285187,21.2946343715823,16.9743580827485));
#60863=CARTESIAN_POINT('Ctrl Pts',(-20.2618088482491,21.3896767938487,16.9802090618314));
#60864=CARTESIAN_POINT('Ctrl Pts',(-20.1994678989163,21.4876828809792,16.9860600409144));
#60865=CARTESIAN_POINT('Ctrl Pts',(-20.1415869215794,21.5882413802424,16.9919110199973));
#60866=CARTESIAN_POINT('Ctrl Pts',(-20.0837007401858,21.6888089206825,16.9977625251396));
#60867=CARTESIAN_POINT('Ctrl Pts',(-20.0302755341599,21.7919289711599,17.0036140302819));
#60868=CARTESIAN_POINT('Ctrl Pts',(-19.9815287296177,21.8971646863294,17.0094655354241));
#60869=CARTESIAN_POINT('Ctrl Pts',(-19.9327657373229,22.0024353479889,17.0153189837239));
#60870=CARTESIAN_POINT('Ctrl Pts',(-19.8886844093961,22.1098226964525,17.0211724320236));
#60871=CARTESIAN_POINT('Ctrl Pts',(-19.8494541939489,22.2188695427157,17.0270258803234));
#60872=CARTESIAN_POINT('Ctrl Pts',(-19.810179365228,22.3280403989222,17.0328859852649));
#60873=CARTESIAN_POINT('Ctrl Pts',(-19.7757668003091,22.4388741305334,17.0387460902064));
#60874=CARTESIAN_POINT('Ctrl Pts',(-19.7463362150053,22.5508979121381,17.0446061951479));
#60875=CARTESIAN_POINT('Ctrl Pts',(-19.7168858100443,22.6629971347484,17.0504702465033));
#60876=CARTESIAN_POINT('Ctrl Pts',(-19.6924241523058,22.7762876000631,17.0563342978588));
#60877=CARTESIAN_POINT('Ctrl Pts',(-19.6730196016011,22.8902875282269,17.0621983492142));
#60878=CARTESIAN_POINT('Ctrl Pts',(-19.6535864524622,23.0044554695282,17.0680710430107));
#60879=CARTESIAN_POINT('Ctrl Pts',(-19.6392253365247,23.1193345518576,17.0739437368073));
#60880=CARTESIAN_POINT('Ctrl Pts',(-19.6299526907736,23.2344390467421,17.0798164306038));
#60881=CARTESIAN_POINT('Ctrl Pts',(-19.6274139954791,23.2659527319807,17.0814242759273));
#60882=CARTESIAN_POINT('Ctrl Pts',(-19.6252564167311,23.2974833231318,17.0830321212507));
#60883=CARTESIAN_POINT('Ctrl Pts',(-19.6234796121694,23.3290208918079,17.0846399665742));
#60884=CARTESIAN_POINT('Ctrl Pts',(-19.616990229211,23.4442048378238,17.0905122635429));
#60885=CARTESIAN_POINT('Ctrl Pts',(-19.6155623039825,23.559867519613,17.0963845605116));
#60886=CARTESIAN_POINT('Ctrl Pts',(-19.619248159034,23.6755267194855,17.1022568574803));
#60887=CARTESIAN_POINT('Ctrl Pts',(-19.6229292375102,23.7910360342203,17.1081215444185));
#60888=CARTESIAN_POINT('Ctrl Pts',(-19.6317109043909,23.9065414666524,17.1139862313567));
#60889=CARTESIAN_POINT('Ctrl Pts',(-19.6455936284308,24.0215569441134,17.1198509182949));
#60890=CARTESIAN_POINT('Ctrl Pts',(-19.6594620749581,24.136454135356,17.1257095737697));
#60891=CARTESIAN_POINT('Ctrl Pts',(-19.6784210946069,24.25086196595,17.1315682292445));
#60892=CARTESIAN_POINT('Ctrl Pts',(-19.7024191503464,24.3642963077809,17.1374268847194));
#60893=CARTESIAN_POINT('Ctrl Pts',(-19.7273545912803,24.4821614949153,17.1435143844373));
#60894=CARTESIAN_POINT('Ctrl Pts',(-19.7577307373536,24.5989751378054,17.1496018841552));
#60895=CARTESIAN_POINT('Ctrl Pts',(-19.7934305924967,24.7142018077215,17.1556893838731));
#60896=CARTESIAN_POINT('Ctrl Pts',(-19.8277486087554,24.8249683841057,17.1615412539565));
#60897=CARTESIAN_POINT('Ctrl Pts',(-19.8669857325947,24.9342681257803,17.1673931240399));
#60898=CARTESIAN_POINT('Ctrl Pts',(-19.9109865634842,25.0416385355941,17.1732449941233));
#60899=CARTESIAN_POINT('Ctrl Pts',(-19.9549806948472,25.1489925972867,17.1790959732063));
#60900=CARTESIAN_POINT('Ctrl Pts',(-20.0037369343856,25.2544175287995,17.1849469522892));
#60901=CARTESIAN_POINT('Ctrl Pts',(-20.057051365012,25.3574698980036,17.1907979313722));
#60902=CARTESIAN_POINT('Ctrl Pts',(-20.1103705891188,25.4605315326075,17.1966494365145));
#60903=CARTESIAN_POINT('Ctrl Pts',(-20.1682486290471,25.5612198136707,17.2025009416568));
#60904=CARTESIAN_POINT('Ctrl Pts',(-20.2304354875114,25.6591156835259,17.2083524467991));
#60905=CARTESIAN_POINT('Ctrl Pts',(-20.2926429968777,25.7570440624683,17.2142058950989));
#60906=CARTESIAN_POINT('Ctrl Pts',(-20.3591619484272,25.8521778375781,17.2200593433987));
#60907=CARTESIAN_POINT('Ctrl Pts',(-20.4296992952674,25.9441273192774,17.2259127916984));
#60908=CARTESIAN_POINT('Ctrl Pts',(-20.500316858388,26.0361813675039,17.23177289664));
#60909=CARTESIAN_POINT('Ctrl Pts',(-20.5749616861977,26.1250435662641,17.2376330015815));
#60910=CARTESIAN_POINT('Ctrl Pts',(-20.6533006942169,26.2103576144564,17.2434931065231));
#60911=CARTESIAN_POINT('Ctrl Pts',(-20.731692458655,26.2957291163205,17.2493571578785));
#60912=CARTESIAN_POINT('Ctrl Pts',(-20.813783064929,26.3775474186261,17.255221209234));
#60913=CARTESIAN_POINT('Ctrl Pts',(-20.8992041349393,26.4554945866809,17.2610852605894));
#60914=CARTESIAN_POINT('Ctrl Pts',(-20.9847510985551,26.5335566333016,17.266957954386));
#60915=CARTESIAN_POINT('Ctrl Pts',(-21.0736380060136,26.6077358951632,17.2728306481826));
#60916=CARTESIAN_POINT('Ctrl Pts',(-21.1654650906881,26.6777559867234,17.2787033419791));
#60917=CARTESIAN_POINT('Ctrl Pts',(-21.1906058103928,26.6969263164998,17.2803111873025));
#60918=CARTESIAN_POINT('Ctrl Pts',(-21.2159667629754,26.7157851448936,17.2819190326258));
#60919=CARTESIAN_POINT('Ctrl Pts',(-21.2415394104567,26.7343273932239,17.2835268779492));
#60920=CARTESIAN_POINT('Ctrl Pts',(-21.3349378102311,26.802048825803,17.2893991749179));
#60921=CARTESIAN_POINT('Ctrl Pts',(-21.4314749109175,26.865770746052,17.2952714718866));
#60922=CARTESIAN_POINT('Ctrl Pts',(-21.5307732972389,26.9251884750276,17.3011437688554));
#60923=CARTESIAN_POINT('Ctrl Pts',(-21.6299430007376,26.9845292033452,17.3070084557936));
#60924=CARTESIAN_POINT('Ctrl Pts',(-21.7318665222518,27.0395766225099,17.3128731427318));
#60925=CARTESIAN_POINT('Ctrl Pts',(-21.836135174072,27.0900675952672,17.31873782967));
#60926=CARTESIAN_POINT('Ctrl Pts',(-21.9402965921111,27.1405066412198,17.3245964851448));
#60927=CARTESIAN_POINT('Ctrl Pts',(-22.0467979734028,27.1863983824184,17.3304551406196));
#60928=CARTESIAN_POINT('Ctrl Pts',(-22.1552041548916,27.2275244860621,17.3363137960944));
#60929=CARTESIAN_POINT('Ctrl Pts',(-22.2678447773122,27.2702570115374,17.3424012958123));
#60930=CARTESIAN_POINT('Ctrl Pts',(-22.3825416496926,27.3078437762513,17.3484887955303));
#60931=CARTESIAN_POINT('Ctrl Pts',(-22.4987810655237,27.3400937890333,17.3545762952482));
#60932=CARTESIAN_POINT('Ctrl Pts',(-22.6105211873366,27.3710954964228,17.3604281653316));
#60933=CARTESIAN_POINT('Ctrl Pts',(-22.7236862226805,27.3971657897267,17.366280035415));
#60934=CARTESIAN_POINT('Ctrl Pts',(-22.8378030643677,27.4181854107016,17.3721319054984));
#60935=CARTESIAN_POINT('Ctrl Pts',(-22.9519025307281,27.439201831248,17.3779828845813));
#60936=CARTESIAN_POINT('Ctrl Pts',(-23.0669531088498,27.4551690336427,17.3838338636643));
#60937=CARTESIAN_POINT('Ctrl Pts',(-23.1824715060122,27.4660188828889,17.3896848427473));
#60938=CARTESIAN_POINT('Ctrl Pts',(-23.2980002893902,27.4768697076408,17.3955363478896));
#60939=CARTESIAN_POINT('Ctrl Pts',(-23.4139965638272,27.4826022259509,17.4013878530319));
#60940=CARTESIAN_POINT('Ctrl Pts',(-23.5299726349456,27.4832002462955,17.4072393581742));
#60941=CARTESIAN_POINT('Ctrl Pts',(-23.6459872191925,27.4837984652297,17.413092806474));
#60942=CARTESIAN_POINT('Ctrl Pts',(-23.7619811736217,27.4792587936734,17.4189462547738));
#60943=CARTESIAN_POINT('Ctrl Pts',(-23.8774682415842,27.4696171331572,17.4247997030735));
#60944=CARTESIAN_POINT('Ctrl Pts',(-23.9930866434205,27.4599645079794,17.4306598080151));
#60945=CARTESIAN_POINT('Ctrl Pts',(-24.1081965960394,27.4451983474994,17.4365199129566));
#60946=CARTESIAN_POINT('Ctrl Pts',(-24.2223182910646,27.4254062854286,17.4423800178982));
#60947=CARTESIAN_POINT('Ctrl Pts',(-24.3365168399086,27.4056008946428,17.4482440692536));
#60948=CARTESIAN_POINT('Ctrl Pts',(-24.4497254031651,27.380762951168,17.4541081206091));
#60949=CARTESIAN_POINT('Ctrl Pts',(-24.5614773730632,27.351030520501,17.4599721719645));
#60950=CARTESIAN_POINT('Ctrl Pts',(-24.6733940430572,27.3212542701663,17.4658448657611));
#60951=CARTESIAN_POINT('Ctrl Pts',(-24.7838494423243,27.2865692592731,17.4717175595577));
#60952=CARTESIAN_POINT('Ctrl Pts',(-24.8923949522613,27.2471624200894,17.4775902533542));
#60953=CARTESIAN_POINT('Ctrl Pts',(-24.9221128971362,27.2363734867173,17.4791980986775));
#60954=CARTESIAN_POINT('Ctrl Pts',(-24.9516878158783,27.2252308880272,17.4808059440008));
#60955=CARTESIAN_POINT('Ctrl Pts',(-24.9811108205685,27.2137390619219,17.482413789324));
#60956=CARTESIAN_POINT('Ctrl Pts',(-25.0885717925615,27.1717677263545,17.4882860862928));
#60957=CARTESIAN_POINT('Ctrl Pts',(-25.1943645086282,27.1249938430823,17.4941583832615));
#60958=CARTESIAN_POINT('Ctrl Pts',(-25.2980286283046,27.073570246025,17.5000306802302));
#60959=CARTESIAN_POINT('Ctrl Pts',(-25.4015584075147,27.0222132898655,17.5058953671684));
#60960=CARTESIAN_POINT('Ctrl Pts',(-25.5029647090802,26.9662187848019,17.5117600541066));
#60961=CARTESIAN_POINT('Ctrl Pts',(-25.6018052381816,26.9057883298201,17.5176247410448));
#60962=CARTESIAN_POINT('Ctrl Pts',(-25.7005441159865,26.845420023778,17.5234833965196));
#60963=CARTESIAN_POINT('Ctrl Pts',(-25.7967221193422,26.7806250563976,17.5293420519944));
#60964=CARTESIAN_POINT('Ctrl Pts',(-25.8899203371206,26.711651519524,17.5352007074693));
#60965=CARTESIAN_POINT('Ctrl Pts',(-25.9867589593731,26.6399838155492,17.5412882071872));
#60966=CARTESIAN_POINT('Ctrl Pts',(-26.0803798570342,26.5638046521469,17.5473757069051));
#60967=CARTESIAN_POINT('Ctrl Pts',(-26.1703446658817,26.4834429803983,17.553463206623));
#60968=CARTESIAN_POINT('Ctrl Pts',(-26.2568271953025,26.4061918782135,17.5593150767064));
#60969=CARTESIAN_POINT('Ctrl Pts',(-26.3399310694826,26.3250763339968,17.5651669467898));
#60970=CARTESIAN_POINT('Ctrl Pts',(-26.4193002199693,26.2404299166269,17.5710188168732));
#60971=CARTESIAN_POINT('Ctrl Pts',(-26.4986572857812,26.1557963874436,17.5768697959561));
#60972=CARTESIAN_POINT('Ctrl Pts',(-26.5742804758724,26.0676333555151,17.5827207750391));
#60973=CARTESIAN_POINT('Ctrl Pts',(-26.6458512269233,25.9763105932616,17.5885717541221));
#60974=CARTESIAN_POINT('Ctrl Pts',(-26.7174284128734,25.884979620213,17.5944232592644));
#60975=CARTESIAN_POINT('Ctrl Pts',(-26.7849521804736,25.7904886774804,17.6002747644067));
#60976=CARTESIAN_POINT('Ctrl Pts',(-26.8481452880373,25.6932393183217,17.606126269549));
#60977=CARTESIAN_POINT('Ctrl Pts',(-26.9113593806564,25.5959576647677,17.6119797178487));
#60978=CARTESIAN_POINT('Ctrl Pts',(-26.9702397285101,25.4959161198048,17.6178331661485));
#60979=CARTESIAN_POINT('Ctrl Pts',(-27.0245536938258,25.3935431856094,17.6236866144483));
#60980=CARTESIAN_POINT('Ctrl Pts',(-27.078929425914,25.2910538311581,17.6295467193898));
#60981=CARTESIAN_POINT('Ctrl Pts',(-27.1287282165997,25.1862281609553,17.6354068243314));
#60982=CARTESIAN_POINT('Ctrl Pts',(-27.1737644368266,25.0795172155745,17.6412669292729));
#60983=CARTESIAN_POINT('Ctrl Pts',(-27.2188309861292,24.9727344070507,17.6471309806284));
#60984=CARTESIAN_POINT('Ctrl Pts',(-27.2591284352385,24.8640641819386,17.6529950319838));
#60985=CARTESIAN_POINT('Ctrl Pts',(-27.2945207196926,24.7539737354384,17.6588590833393));
#60986=CARTESIAN_POINT('Ctrl Pts',(-27.3299651653089,24.6437210375963,17.6647317771358));
#60987=CARTESIAN_POINT('Ctrl Pts',(-27.3604899095314,24.5320443381553,17.6706044709324));
#60988=CARTESIAN_POINT('Ctrl Pts',(-27.3860097242403,24.4194221122888,17.676477164729));
#60989=CARTESIAN_POINT('Ctrl Pts',(-27.3929966226132,24.3885880307863,17.6780850100523));
#60990=CARTESIAN_POINT('Ctrl Pts',(-27.3996086647322,24.3576831084718,17.6796928553756));
#60991=CARTESIAN_POINT('Ctrl Pts',(-27.4058447799821,24.3267172217752,17.6813007006989));
#60992=CARTESIAN_POINT('Ctrl Pts',(-27.4386430309124,24.1638551062664,17.6897570091953));
#60993=CARTESIAN_POINT('Ctrl Pts',(-27.4611308481835,23.9988525117614,17.6982133176916));
#60994=CARTESIAN_POINT('Ctrl Pts',(-27.4730914971859,23.8327829739827,17.7066696261879));
#60995=CARTESIAN_POINT('Ctrl Pts',(-27.4797707214065,23.7400442205251,17.7113919101136));
#60996=CARTESIAN_POINT('Ctrl Pts',(-27.4831678227789,23.6469731076509,17.7161141940394));
#60997=CARTESIAN_POINT('Ctrl Pts',(-27.4832509670657,23.5537607171193,17.7208364779651));
#60998=CARTESIAN_POINT('',(-27.4767571638619,23.5506058536415,18.9708364779651));
#60999=CARTESIAN_POINT('Ctrl Pts',(-27.4846078470131,23.5537486008167,17.720837152879));
#61000=CARTESIAN_POINT('Ctrl Pts',(-27.4748958087803,22.5049130723347,17.7739539726106));
#61001=CARTESIAN_POINT('Ctrl Pts',(-26.5032239293697,20.1311413592398,17.8933664294671));
#61002=CARTESIAN_POINT('Ctrl Pts',(-22.4901423490843,19.0206921520514,18.0790745234486));
#61003=CARTESIAN_POINT('Ctrl Pts',(-19.1664228912539,21.9937216082251,18.2779614348238));
#61004=CARTESIAN_POINT('Ctrl Pts',(-19.8710711855328,26.397071011008,18.4768483461984));
#61005=CARTESIAN_POINT('Ctrl Pts',(-23.9565751937948,28.1844356017042,18.6757352575734));
#61006=CARTESIAN_POINT('Ctrl Pts',(-27.0299249841624,26.1385950912699,18.8403979681622));
#61007=CARTESIAN_POINT('Ctrl Pts',(-27.4772652391045,24.187090675563,18.9387650416262));
#61008=CARTESIAN_POINT('Ctrl Pts',(-27.4767571638619,23.5506058536415,18.9708364779651));
#61009=CARTESIAN_POINT('',(-27.4833068676715,23.5466220118607,20.2208364779651));
#61010=CARTESIAN_POINT('Ctrl Pts',(-27.4767571638619,23.5506058536415,18.9708364779651));
#61011=CARTESIAN_POINT('Ctrl Pts',(-27.4762149845553,22.871397597657,19.0050606787511));
#61012=CARTESIAN_POINT('Ctrl Pts',(-26.9851084914367,20.8757618441067,19.105580516662));
#61013=CARTESIAN_POINT('Ctrl Pts',(-23.8059484060801,18.9053229895029,19.2723959916981));
#61014=CARTESIAN_POINT('Ctrl Pts',(-19.7806098338932,20.8243499723508,19.4712829030729));
#61015=CARTESIAN_POINT('Ctrl Pts',(-19.219253287995,25.2482502888139,19.670169814448));
#61016=CARTESIAN_POINT('Ctrl Pts',(-22.637717838874,28.1118346329506,19.8690567258227));
#61017=CARTESIAN_POINT('Ctrl Pts',(-26.566569641527,26.8860911980051,20.0526122803286));
#61018=CARTESIAN_POINT('Ctrl Pts',(-27.4739820892811,24.5538076996726,20.1698721977093));
#61019=CARTESIAN_POINT('Ctrl Pts',(-27.4833068676715,23.5466220118607,20.2208364779651));
#61020=CARTESIAN_POINT('',(-27.4892473091168,23.551540164831,21.4708364779651));
#61021=CARTESIAN_POINT('Ctrl Pts',(-27.4833068676715,23.5466220118607,20.2208364779651));
#61022=CARTESIAN_POINT('Ctrl Pts',(-27.4861119991187,23.2436348385735,20.2361678348342));
#61023=CARTESIAN_POINT('Ctrl Pts',(-27.3155179850287,21.6336002486415,20.3177948288287));
#61024=CARTESIAN_POINT('Ctrl Pts',(-25.1011405181817,19.1644233871128,20.465717459947));
#61025=CARTESIAN_POINT('Ctrl Pts',(-20.6987015893344,19.8747378663381,20.6646043713225));
#61026=CARTESIAN_POINT('Ctrl Pts',(-18.916596204868,23.9625386907771,20.8634912826971));
#61027=CARTESIAN_POINT('Ctrl Pts',(-21.3924281154842,27.6714834911175,21.0623781940721));
#61028=CARTESIAN_POINT('Ctrl Pts',(-25.8511177112576,27.5933664625134,21.2612651054469));
#61029=CARTESIAN_POINT('Ctrl Pts',(-27.456025305492,24.9965071357817,21.3974178667446));
#61030=CARTESIAN_POINT('Ctrl Pts',(-27.4895458388405,23.6216486653013,21.4672749909173));
#61031=CARTESIAN_POINT('Ctrl Pts',(-27.4892473091168,23.551540164831,21.4708364779651));
#61032=CARTESIAN_POINT('',(-27.4820795739567,23.5532667202166,22.7208360305048));
#61033=CARTESIAN_POINT('Ctrl Pts',(-27.4892473091168,23.551540164831,21.4708364779651));
#61034=CARTESIAN_POINT('Ctrl Pts',(-27.4839888290946,22.3166073597353,21.5335706280423));
#61035=CARTESIAN_POINT('Ctrl Pts',(-26.1920695173065,19.7671546223778,21.6626004152444));
#61036=CARTESIAN_POINT('Ctrl Pts',(-21.8466825212323,19.221442065576,21.8579258395718));
#61037=CARTESIAN_POINT('Ctrl Pts',(-18.9874998465852,22.643588996177,22.0568127509464));
#61038=CARTESIAN_POINT('Ctrl Pts',(-20.3211000319204,26.8988828435244,22.2556996623214));
#61039=CARTESIAN_POINT('Ctrl Pts',(-24.6220175775656,28.0770693513325,22.4545865736964));
#61040=CARTESIAN_POINT('Ctrl Pts',(-27.2070963238024,25.7527407920887,22.6096316859959));
#61041=CARTESIAN_POINT('Ctrl Pts',(-27.4825225817787,23.9981564321766,22.6983811611705));
#61042=CARTESIAN_POINT('Ctrl Pts',(-27.4793788461029,23.5532850883259,22.7208349992202));
#61043=CARTESIAN_POINT('',(-27.4815531016315,23.5477787515071,23.970837000806));
#61044=CARTESIAN_POINT('Ctrl Pts',(-27.4832513827808,23.5532587505456,22.7208364779651));
#61045=CARTESIAN_POINT('Ctrl Pts',(-27.4833401065471,23.4371825470975,22.7266894177816));
#61046=CARTESIAN_POINT('Ctrl Pts',(-27.4782858174004,23.3210503319215,22.7325423575982));
#61047=CARTESIAN_POINT('Ctrl Pts',(-27.4681003776954,23.2053507259815,22.7383952974147));
#61048=CARTESIAN_POINT('Ctrl Pts',(-27.4579162907114,23.089666486025,22.7442474599064));
#61049=CARTESIAN_POINT('Ctrl Pts',(-27.4426024440398,22.9744151518856,22.7500996223982));
#61050=CARTESIAN_POINT('Ctrl Pts',(-27.4222226876323,22.860081457594,22.7559517848899));
#61051=CARTESIAN_POINT('Ctrl Pts',(-27.4018407298981,22.7457354135073,22.761804579505));
#61052=CARTESIAN_POINT('Ctrl Pts',(-27.3763918465693,22.6323076125064,22.7676573741202));
#61053=CARTESIAN_POINT('Ctrl Pts',(-27.3459911178517,22.5202731214364,22.7735101687353));
#61054=CARTESIAN_POINT('Ctrl Pts',(-27.3155797841398,22.4081995482394,22.7793650050402));
#61055=CARTESIAN_POINT('Ctrl Pts',(-27.2802132775954,22.2975206494814,22.785219841345));
#61056=CARTESIAN_POINT('Ctrl Pts',(-27.2400564931379,22.1886961699838,22.7910746776498));
#61057=CARTESIAN_POINT('Ctrl Pts',(-27.1998511006222,22.07973996314,22.7969366009818));
#61058=CARTESIAN_POINT('Ctrl Pts',(-27.1548439971764,21.9726430441766,22.8027985243139));
#61059=CARTESIAN_POINT('Ctrl Pts',(-27.10524824809,21.8678451920742,22.8086604476459));
#61060=CARTESIAN_POINT('Ctrl Pts',(-27.0556185970657,21.7629757037863,22.8145263779859));
#61061=CARTESIAN_POINT('Ctrl Pts',(-27.0013942467496,21.6604087757148,22.8203923083259));
#61062=CARTESIAN_POINT('Ctrl Pts',(-26.9428333494117,21.5605579834644,22.8262582386659));
#61063=CARTESIAN_POINT('Ctrl Pts',(-26.8841781246888,21.460546355835,22.8321336175952));
#61064=CARTESIAN_POINT('Ctrl Pts',(-26.8211726303032,21.3632599443681,22.8380089965245));
#61065=CARTESIAN_POINT('Ctrl Pts',(-26.7541174424854,21.2690820791851,22.8438843754538));
#61066=CARTESIAN_POINT('Ctrl Pts',(-26.721872079453,21.2237940179436,22.8467097157846));
#61067=CARTESIAN_POINT('Ctrl Pts',(-26.6886908358786,21.1792242803724,22.8495350561154));
#61068=CARTESIAN_POINT('Ctrl Pts',(-26.6546102315833,21.1354125222651,22.8523603964462));
#61069=CARTESIAN_POINT('Ctrl Pts',(-26.5837757812643,21.0443524642875,22.8582326934149));
#61070=CARTESIAN_POINT('Ctrl Pts',(-26.508812673025,20.9562591766196,22.8641049903835));
#61071=CARTESIAN_POINT('Ctrl Pts',(-26.4299985006656,20.8715304195308,22.8699772873522));
#61072=CARTESIAN_POINT('Ctrl Pts',(-26.3512864652145,20.7869114641824,22.8758419742904));
#61073=CARTESIAN_POINT('Ctrl Pts',(-26.2687335692525,20.7056486684967,22.8817066612286));
#61074=CARTESIAN_POINT('Ctrl Pts',(-26.1826590139729,20.628108607782,22.8875713481667));
#61075=CARTESIAN_POINT('Ctrl Pts',(-26.0966729809851,20.5506482921657,22.8934300036415));
#61076=CARTESIAN_POINT('Ctrl Pts',(-26.0071727979275,20.4769033712574,22.8992886591163));
#61077=CARTESIAN_POINT('Ctrl Pts',(-25.9145155751801,20.4072047654,22.9051473145911));
#61078=CARTESIAN_POINT('Ctrl Pts',(-25.8182390797001,20.3347836706077,22.911234814309));
#61079=CARTESIAN_POINT('Ctrl Pts',(-25.7185541928124,20.2667317731929,22.9173223140269));
#61080=CARTESIAN_POINT('Ctrl Pts',(-25.6159010759208,20.2033756155626,22.9234098137448));
#61081=CARTESIAN_POINT('Ctrl Pts',(-25.5172213664276,20.1424717928744,22.9292616838282));
#61082=CARTESIAN_POINT('Ctrl Pts',(-25.4157993222026,20.0859071894331,22.9351135539116));
#61083=CARTESIAN_POINT('Ctrl Pts',(-25.3120560965544,20.033928144092,22.9409654239949));
#61084=CARTESIAN_POINT('Ctrl Pts',(-25.2083286667556,19.9819570130332,22.9468164030779));
#61085=CARTESIAN_POINT('Ctrl Pts',(-25.1022811277337,19.9345702369693,22.9526673821608));
#61086=CARTESIAN_POINT('Ctrl Pts',(-24.994358657412,19.8919678930057,22.9585183612438));
#61087=CARTESIAN_POINT('Ctrl Pts',(-24.8864264838219,19.8493617186815,22.9643698663861));
#61088=CARTESIAN_POINT('Ctrl Pts',(-24.7766194283531,19.8115409833825,22.9702213715283));
#61089=CARTESIAN_POINT('Ctrl Pts',(-24.6654013671529,19.778657103394,22.9760728766706));
#61090=CARTESIAN_POINT('Ctrl Pts',(-24.554146372856,19.7457623033849,22.9819263249703));
#61091=CARTESIAN_POINT('Ctrl Pts',(-24.4414798373255,19.7178077357211,22.98777977327));
#61092=CARTESIAN_POINT('Ctrl Pts',(-24.3278787683951,19.6948943854263,22.9936332215698));
#61093=CARTESIAN_POINT('Ctrl Pts',(-24.2141485103808,19.6719549776765,22.9994933265113));
#61094=CARTESIAN_POINT('Ctrl Pts',(-24.0994820031775,19.6540683118901,23.0053534314528));
#61095=CARTESIAN_POINT('Ctrl Pts',(-23.9843644735907,19.6412838925385,23.0112135363943));
#61096=CARTESIAN_POINT('Ctrl Pts',(-23.8691694195529,19.6284908636806,23.0170775877497));
#61097=CARTESIAN_POINT('Ctrl Pts',(-23.7535231497996,19.6208069504418,23.0229416391052));
#61098=CARTESIAN_POINT('Ctrl Pts',(-23.6379122628203,19.6182295445362,23.0288056904606));
#61099=CARTESIAN_POINT('Ctrl Pts',(-23.5221309884716,19.6156483400488,23.0346783842571));
#61100=CARTESIAN_POINT('Ctrl Pts',(-23.406385612704,19.6181886542474,23.0405510780537));
#61101=CARTESIAN_POINT('Ctrl Pts',(-23.2911590707109,19.6257959351097,23.0464237718502));
#61102=CARTESIAN_POINT('Ctrl Pts',(-23.2596119710132,19.6278786813558,23.0480316171738));
#61103=CARTESIAN_POINT('Ctrl Pts',(-23.2281037082547,19.6303409369221,23.0496394624973));
#61104=CARTESIAN_POINT('Ctrl Pts',(-23.1966440548342,19.6331809156661,23.0512473078209));
#61105=CARTESIAN_POINT('Ctrl Pts',(-23.0817446769464,19.6435533055507,23.0571196047896));
#61106=CARTESIAN_POINT('Ctrl Pts',(-22.9671095780651,19.6590028697379,23.0629919017583));
#61107=CARTESIAN_POINT('Ctrl Pts',(-22.8532234517959,19.6795110701941,23.068864198727));
#61108=CARTESIAN_POINT('Ctrl Pts',(-22.7394849129014,19.6999926936513,23.0747288856652));
#61109=CARTESIAN_POINT('Ctrl Pts',(-22.6264938195099,19.7255198440746,23.0805935726034));
#61110=CARTESIAN_POINT('Ctrl Pts',(-22.5147311193557,19.7560221216389,23.0864582595416));
#61111=CARTESIAN_POINT('Ctrl Pts',(-22.4030833601422,19.7864930295202,23.0923169150165));
#61112=CARTESIAN_POINT('Ctrl Pts',(-22.2926618777462,19.821928779163,23.0981755704913));
#61113=CARTESIAN_POINT('Ctrl Pts',(-22.1839381143039,19.862207804087,23.1040342259661));
#61114=CARTESIAN_POINT('Ctrl Pts',(-22.070967504899,19.9040601632018,23.110121725684));
#61115=CARTESIAN_POINT('Ctrl Pts',(-21.9598303945074,19.9511417956007,23.1162092254019));
#61116=CARTESIAN_POINT('Ctrl Pts',(-21.8510394346335,20.0032588961237,23.1222967251198));
#61117=CARTESIAN_POINT('Ctrl Pts',(-21.7464594604354,20.0533586933339,23.1281485952032));
#61118=CARTESIAN_POINT('Ctrl Pts',(-21.6440477960159,20.1081111947209,23.1340004652866));
#61119=CARTESIAN_POINT('Ctrl Pts',(-21.5442393416026,20.1672952335335,23.13985233537));
#61120=CARTESIAN_POINT('Ctrl Pts',(-21.4444460839341,20.226470261038,23.145703314453));
#61121=CARTESIAN_POINT('Ctrl Pts',(-21.3472556036489,20.2900752735786,23.1515542935359));
#61122=CARTESIAN_POINT('Ctrl Pts',(-21.2530768665124,20.3578438856564,23.1574052726189));
#61123=CARTESIAN_POINT('Ctrl Pts',(-21.1588896618013,20.4256185907846,23.1632567777612));
#61124=CARTESIAN_POINT('Ctrl Pts',(-21.067715074096,20.4975573981569,23.1691082829035));
#61125=CARTESIAN_POINT('Ctrl Pts',(-20.9799312371807,20.5733518879087,23.1749597880458));
#61126=CARTESIAN_POINT('Ctrl Pts',(-20.8921182491639,20.6491715473607,23.1808132363455));
#61127=CARTESIAN_POINT('Ctrl Pts',(-20.8076985636316,20.7288491651498,23.1866666846453));
#61128=CARTESIAN_POINT('Ctrl Pts',(-20.7270149839343,20.8120380132683,23.1925201329451));
#61129=CARTESIAN_POINT('Ctrl Pts',(-20.6462396494869,20.895321465171,23.1983802378866));
#61130=CARTESIAN_POINT('Ctrl Pts',(-20.5692091892525,20.9821238204571,23.2042403428281));
#61131=CARTESIAN_POINT('Ctrl Pts',(-20.4962275378319,21.0720636089395,23.2101004477697));
#61132=CARTESIAN_POINT('Ctrl Pts',(-20.4231967378365,21.1620639662406,23.2159644991251));
#61133=CARTESIAN_POINT('Ctrl Pts',(-20.3542204213109,21.2552056324765,23.2218285504806));
#61134=CARTESIAN_POINT('Ctrl Pts',(-20.2895594209725,21.351077814285,23.227692601836));
#61135=CARTESIAN_POINT('Ctrl Pts',(-20.2248031232274,21.4470912925511,23.2335652956326));
#61136=CARTESIAN_POINT('Ctrl Pts',(-20.1643750497878,21.5458429667048,23.2394379894291));
#61137=CARTESIAN_POINT('Ctrl Pts',(-20.1084903520673,21.6468970475846,23.2453106832257));
#61138=CARTESIAN_POINT('Ctrl Pts',(-20.0931900566675,21.6745639645026,23.2469185285491));
#61139=CARTESIAN_POINT('Ctrl Pts',(-20.0782300418381,21.7024033481281,23.2485263738725));
#61140=CARTESIAN_POINT('Ctrl Pts',(-20.0636140872636,21.7304060112923,23.2501342191959));
#61141=CARTESIAN_POINT('Ctrl Pts',(-20.0102325682249,21.8326795021697,23.2560065161646));
#61142=CARTESIAN_POINT('Ctrl Pts',(-19.9612654151198,21.937475078632,23.2618788131334));
#61143=CARTESIAN_POINT('Ctrl Pts',(-19.9169590290309,22.0443749392236,23.2677511101021));
#61144=CARTESIAN_POINT('Ctrl Pts',(-19.8727100604997,22.1511362660858,23.2736157970404));
#61145=CARTESIAN_POINT('Ctrl Pts',(-19.833110004441,22.2599960757257,23.2794804839786));
#61146=CARTESIAN_POINT('Ctrl Pts',(-19.7983596049401,22.3705116846552,23.2853451709168));
#61147=CARTESIAN_POINT('Ctrl Pts',(-19.7636449440497,22.480913635199,23.2912038263917));
#61148=CARTESIAN_POINT('Ctrl Pts',(-19.73377014244,22.5929676059282,23.2970624818665));
#61149=CARTESIAN_POINT('Ctrl Pts',(-19.7088877586521,22.7062112528272,23.3029211373414));
#61150=CARTESIAN_POINT('Ctrl Pts',(-19.6830334470375,22.8238782963172,23.3090086370593));
#61151=CARTESIAN_POINT('Ctrl Pts',(-19.662569694719,22.9428294302189,23.3150961367772));
#61152=CARTESIAN_POINT('Ctrl Pts',(-19.6476105600349,23.0625285923154,23.3211836364951));
#61153=CARTESIAN_POINT('Ctrl Pts',(-19.6332304505008,23.177594543551,23.3270355065785));
#61154=CARTESIAN_POINT('Ctrl Pts',(-19.6239368024115,23.2933512432391,23.3328873766619));
#61155=CARTESIAN_POINT('Ctrl Pts',(-19.6197786264781,23.4093132525164,23.3387392467454));
#61156=CARTESIAN_POINT('Ctrl Pts',(-19.6156210836648,23.5252576055233,23.3445902258284));
#61157=CARTESIAN_POINT('Ctrl Pts',(-19.6165974731049,23.64140679296,23.3504412049114));
#61158=CARTESIAN_POINT('Ctrl Pts',(-19.6227047435426,23.7572727524113,23.3562921839944));
#61159=CARTESIAN_POINT('Ctrl Pts',(-19.6288125630827,23.8731491293273,23.3621436891367));
#61160=CARTESIAN_POINT('Ctrl Pts',(-19.6400521589127,23.9887418148016,23.367995194279));
#61161=CARTESIAN_POINT('Ctrl Pts',(-19.6563684495664,24.1035659645255,23.3738466994214));
#61162=CARTESIAN_POINT('Ctrl Pts',(-19.672690158505,24.2184282448499,23.3797001477212));
#61163=CARTESIAN_POINT('Ctrl Pts',(-19.6940918563675,24.332521072892,23.385553596021));
#61164=CARTESIAN_POINT('Ctrl Pts',(-19.7204671348071,24.4453686212546,23.3914070443208));
#61165=CARTESIAN_POINT('Ctrl Pts',(-19.7468724076655,24.5583445017839,23.3972671492624));
#61166=CARTESIAN_POINT('Ctrl Pts',(-19.77826245625,24.670071873261,23.4031272542039));
#61167=CARTESIAN_POINT('Ctrl Pts',(-19.8144806328283,24.7800888295989,23.4089873591455));
#61168=CARTESIAN_POINT('Ctrl Pts',(-19.8507232000819,24.8901798754717,23.414851410501));
#61169=CARTESIAN_POINT('Ctrl Pts',(-19.8918002234453,24.9985578270231,23.4207154618565));
#61170=CARTESIAN_POINT('Ctrl Pts',(-19.9375070867115,25.1047811900846,23.426579513212));
#61171=CARTESIAN_POINT('Ctrl Pts',(-19.9832813127701,25.2111611051785,23.4324522070086));
#61172=CARTESIAN_POINT('Ctrl Pts',(-20.0336988176947,25.3153797235017,23.4383249008052));
#61173=CARTESIAN_POINT('Ctrl Pts',(-20.0885092632119,25.417020472044,23.4441975946018));
#61174=CARTESIAN_POINT('Ctrl Pts',(-20.1035154463245,25.4448480087466,23.4458054399248));
#61175=CARTESIAN_POINT('Ctrl Pts',(-20.1188506646454,25.472482487263,23.4474132852478));
#61176=CARTESIAN_POINT('Ctrl Pts',(-20.1345092319351,25.4999157616267,23.4490211305708));
#61177=CARTESIAN_POINT('Ctrl Pts',(-20.1916986617359,25.6001096867417,23.4548934275394));
#61178=CARTESIAN_POINT('Ctrl Pts',(-20.2533961163809,25.6979530259088,23.4607657245081));
#61179=CARTESIAN_POINT('Ctrl Pts',(-20.3193832827261,25.7930126383646,23.4666380214768));
#61180=CARTESIAN_POINT('Ctrl Pts',(-20.3852849349444,25.8879490611122,23.472502708415));
#61181=CARTESIAN_POINT('Ctrl Pts',(-20.4554650102053,25.9801085946985,23.4783673953532));
#61182=CARTESIAN_POINT('Ctrl Pts',(-20.5296595821508,26.0690830605645,23.4842320822914));
#61183=CARTESIAN_POINT('Ctrl Pts',(-20.6037778496235,26.1579660217618,23.4900907377662));
#61184=CARTESIAN_POINT('Ctrl Pts',(-20.6819021385134,26.2436701150863,23.495949393241));
#61185=CARTESIAN_POINT('Ctrl Pts',(-20.763725935402,26.3258170739372,23.5018080487158));
#61186=CARTESIAN_POINT('Ctrl Pts',(-20.8487458418672,26.4111727653555,23.5078955484337));
#61187=CARTESIAN_POINT('Ctrl Pts',(-20.9377599009622,26.4926873940978,23.5139830481516));
#61188=CARTESIAN_POINT('Ctrl Pts',(-21.0303787679168,26.569975236617,23.5200705478695));
#61189=CARTESIAN_POINT('Ctrl Pts',(-21.1194126244761,26.6442714886755,23.5259224179529));
#61190=CARTESIAN_POINT('Ctrl Pts',(-21.2117770673393,26.7146617942,23.5317742880363));
#61191=CARTESIAN_POINT('Ctrl Pts',(-21.307090181013,26.7808425193724,23.5376261581197));
#61192=CARTESIAN_POINT('Ctrl Pts',(-21.4023887823984,26.8470131679275,23.5434771372026));
#61193=CARTESIAN_POINT('Ctrl Pts',(-21.5006348224522,26.9089752748323,23.5493281162856));
#61194=CARTESIAN_POINT('Ctrl Pts',(-21.6014160367423,26.9664675887337,23.5551790953685));
#61195=CARTESIAN_POINT('Ctrl Pts',(-21.7022063122337,27.0239650717476,23.5610306005108));
#61196=CARTESIAN_POINT('Ctrl Pts',(-21.8055318559913,27.0769917580158,23.5668821056531));
#61197=CARTESIAN_POINT('Ctrl Pts',(-21.9109549864961,27.1253319095972,23.5727336107954));
#61198=CARTESIAN_POINT('Ctrl Pts',(-22.0164131257273,27.1736881138906,23.5785870590951));
#61199=CARTESIAN_POINT('Ctrl Pts',(-22.1239698612128,27.2173545166911,23.5844405073949));
#61200=CARTESIAN_POINT('Ctrl Pts',(-22.2331673531572,27.2561634362463,23.5902939556947));
#61201=CARTESIAN_POINT('Ctrl Pts',(-22.3424890263619,27.2950164899703,23.5961540606362));
#61202=CARTESIAN_POINT('Ctrl Pts',(-22.4534547905528,27.3290008961693,23.6020141655777));
#61203=CARTESIAN_POINT('Ctrl Pts',(-22.5655913616488,27.3579987653874,23.6078742705193));
#61204=CARTESIAN_POINT('Ctrl Pts',(-22.6778034497074,27.3870161628556,23.6137383218747));
#61205=CARTESIAN_POINT('Ctrl Pts',(-22.7911875112451,27.411040251181,23.6196023732302));
#61206=CARTESIAN_POINT('Ctrl Pts',(-22.9052615060763,27.4300045310973,23.6254664245856));
#61207=CARTESIAN_POINT('Ctrl Pts',(-23.0195036232043,27.4489967605765,23.6313391183822));
#61208=CARTESIAN_POINT('Ctrl Pts',(-23.134437294166,27.4629142491113,23.6372118121788));
#61209=CARTESIAN_POINT('Ctrl Pts',(-23.2495767306492,27.4717424351194,23.6430845059753));
#61210=CARTESIAN_POINT('Ctrl Pts',(-23.2810999823131,27.4741594447711,23.6446923512988));
#61211=CARTESIAN_POINT('Ctrl Pts',(-23.3126386683647,27.4761952754471,23.6463001966222));
#61212=CARTESIAN_POINT('Ctrl Pts',(-23.3441828618122,27.4778503078361,23.6479080419457));
#61213=CARTESIAN_POINT('Ctrl Pts',(-23.4593910033285,27.4838949450528,23.6537803389143));
#61214=CARTESIAN_POINT('Ctrl Pts',(-23.5750583359852,27.4848763139783,23.659652635883));
#61215=CARTESIAN_POINT('Ctrl Pts',(-23.6907024436814,27.4807439541785,23.6655249328516));
#61216=CARTESIAN_POINT('Ctrl Pts',(-23.806196685798,27.4766169495888,23.6713896197898));
#61217=CARTESIAN_POINT('Ctrl Pts',(-23.9216673535017,27.4673894095967,23.6772543067279));
#61218=CARTESIAN_POINT('Ctrl Pts',(-24.0366283759371,27.4530627420602,23.6831189936661));
#61219=CARTESIAN_POINT('Ctrl Pts',(-24.1514711681574,27.4387508086044,23.6889776491408));
#61220=CARTESIAN_POINT('Ctrl Pts',(-24.2658049499038,27.4193502292692,23.6948363046156));
#61221=CARTESIAN_POINT('Ctrl Pts',(-24.3791457956417,27.3949144098029,23.7006949600903));
#61222=CARTESIAN_POINT('Ctrl Pts',(-24.4969138346452,27.3695241057051,23.7067824598082));
#61223=CARTESIAN_POINT('Ctrl Pts',(-24.6136093319937,27.3386971967743,23.7128699595262));
#61224=CARTESIAN_POINT('Ctrl Pts',(-24.7286973146415,27.302552745369,23.7189574592441));
#61225=CARTESIAN_POINT('Ctrl Pts',(-24.839330571942,27.2678073418933,23.7248093293275));
#61226=CARTESIAN_POINT('Ctrl Pts',(-24.9484780139794,27.2281485305923,23.7306611994108));
#61227=CARTESIAN_POINT('Ctrl Pts',(-25.0556777470133,27.1837334964278,23.7365130694942));
#61228=CARTESIAN_POINT('Ctrl Pts',(-25.162861157913,27.1393252248561,23.7423640485771));
#61229=CARTESIAN_POINT('Ctrl Pts',(-25.2680970676615,27.0901623285052,23.74821502766));
#61230=CARTESIAN_POINT('Ctrl Pts',(-25.3709428347095,27.0364504349272,23.7540660067429));
#61231=CARTESIAN_POINT('Ctrl Pts',(-25.4737978485814,26.9827337121332,23.7599175118852));
#61232=CARTESIAN_POINT('Ctrl Pts',(-25.5742619261146,26.9244673704379,23.7657690170274));
#61233=CARTESIAN_POINT('Ctrl Pts',(-25.671916977944,26.861903023144,23.7716205221696));
#61234=CARTESIAN_POINT('Ctrl Pts',(-25.7696044588906,26.7993178995921,23.7774739704694));
#61235=CARTESIAN_POINT('Ctrl Pts',(-25.8644807113959,26.732432155279,23.7833274187691));
#61236=CARTESIAN_POINT('Ctrl Pts',(-25.9561571801695,26.6615403394106,23.7891808670688));
#61237=CARTESIAN_POINT('Ctrl Pts',(-26.047937904995,26.590567904154,23.7950409720103));
#61238=CARTESIAN_POINT('Ctrl Pts',(-26.1365112558465,26.5155805571818,23.8009010769518));
#61239=CARTESIAN_POINT('Ctrl Pts',(-26.2215222202368,26.4369127560839,23.8067611818933));
#61240=CARTESIAN_POINT('Ctrl Pts',(-26.3065904341911,26.3581919771455,23.8126252332487));
#61241=CARTESIAN_POINT('Ctrl Pts',(-26.3880911947336,26.2757861019824,23.8184892846041));
#61242=CARTESIAN_POINT('Ctrl Pts',(-26.4657079917605,26.190064733418,23.8243533359595));
#61243=CARTESIAN_POINT('Ctrl Pts',(-26.5434391804522,26.1042170286681,23.830226029756));
#61244=CARTESIAN_POINT('Ctrl Pts',(-26.6172747186063,26.0150443954609,23.8360987235525));
#61245=CARTESIAN_POINT('Ctrl Pts',(-26.6869397661427,25.9229476645016,23.841971417349));
#61246=CARTESIAN_POINT('Ctrl Pts',(-26.7060128908106,25.8977331201467,23.8435792626729));
#61247=CARTESIAN_POINT('Ctrl Pts',(-26.7247736661513,25.8722995471868,23.8451871079967));
#61248=CARTESIAN_POINT('Ctrl Pts',(-26.7432170464849,25.8466555031449,23.8467949533206));
#61249=CARTESIAN_POINT('Ctrl Pts',(-26.811152181329,25.7521971360545,23.8527173594581));
#61250=CARTESIAN_POINT('Ctrl Pts',(-26.8750041066385,25.6545661064609,23.8586397655956));
#61251=CARTESIAN_POINT('Ctrl Pts',(-26.9344653447686,25.5541468991256,23.8645621717331));
#61252=CARTESIAN_POINT('Ctrl Pts',(-26.9938469440751,25.4538621872664,23.8704766457543));
#61253=CARTESIAN_POINT('Ctrl Pts',(-27.0488493477093,25.3507970685784,23.8763911197755));
#61254=CARTESIAN_POINT('Ctrl Pts',(-27.0992066329202,25.2453672143606,23.8823055937967));
#61255=CARTESIAN_POINT('Ctrl Pts',(-27.1495079646061,25.1400545064893,23.8882134960643));
#61256=CARTESIAN_POINT('Ctrl Pts',(-27.1951742719672,25.0323826519989,23.8941213983319));
#61257=CARTESIAN_POINT('Ctrl Pts',(-27.2359844121268,24.9227937899311,23.9000293005995));
#61258=CARTESIAN_POINT('Ctrl Pts',(-27.2767543114318,24.8133129880036,23.9059313773778));
#61259=CARTESIAN_POINT('Ctrl Pts',(-27.3126774360233,24.7019193187062,23.911833454156));
#61260=CARTESIAN_POINT('Ctrl Pts',(-27.3435801479668,24.589076191236,23.9177355309343));
#61261=CARTESIAN_POINT('Ctrl Pts',(-27.3744644883382,24.4763001486755,23.9236340989452));
#61262=CARTESIAN_POINT('Ctrl Pts',(-27.4003342475389,24.3620767509935,23.929532666956));
#61263=CARTESIAN_POINT('Ctrl Pts',(-27.4210652880595,24.2468855808382,23.9354312349669));
#61264=CARTESIAN_POINT('Ctrl Pts',(-27.4418044325967,24.1316493810493,23.9413321087999));
#61265=CARTESIAN_POINT('Ctrl Pts',(-27.4574007443461,24.0154450455376,23.9472329826329));
#61266=CARTESIAN_POINT('Ctrl Pts',(-27.4677809366463,23.8987639323588,23.953133856466));
#61267=CARTESIAN_POINT('Ctrl Pts',(-27.4781611289466,23.7820828191799,23.959034730299));
#61268=CARTESIAN_POINT('Ctrl Pts',(-27.4833251596027,23.6649253317523,23.9649356041321));
#61269=CARTESIAN_POINT('Ctrl Pts',(-27.4832517595538,23.5477880529337,23.9708364779651));
#61270=CARTESIAN_POINT('',(-27.4850558412115,23.5481778231382,25.2208358612592));
#61271=CARTESIAN_POINT('Ctrl Pts',(-27.4783256425004,23.5477610787469,23.9708379942064));
#61272=CARTESIAN_POINT('Ctrl Pts',(-27.481139687066,23.0531416688158,23.9957859510361));
#61273=CARTESIAN_POINT('Ctrl Pts',(-27.1646539659434,21.2476181443352,24.0870295449907));
#61274=CARTESIAN_POINT('Ctrl Pts',(-24.4510434083163,18.9863368193904,24.2445687760702));
#61275=CARTESIAN_POINT('Ctrl Pts',(-20.1974693245192,20.3254121329573,24.4434556874452));
#61276=CARTESIAN_POINT('Ctrl Pts',(-19.0248187389452,24.6278423513666,24.64234259882));
#61277=CARTESIAN_POINT('Ctrl Pts',(-22.0106581154577,27.9400588904565,24.841229510195));
#61278=CARTESIAN_POINT('Ctrl Pts',(-26.2772539213587,27.2403899709072,25.0340602178841));
#61279=CARTESIAN_POINT('Ctrl Pts',(-27.4807589030166,24.7347075626642,25.1605952884482));
#61280=CARTESIAN_POINT('Ctrl Pts',(-27.4883884996962,23.5481984972521,25.2208347218874));
#61281=CARTESIAN_POINT('',(-27.4832675014334,23.5537273857095,26.4708364861422));
#61282=CARTESIAN_POINT('Ctrl Pts',(-27.4832519785574,23.5481666328942,25.2208364779651));
#61283=CARTESIAN_POINT('Ctrl Pts',(-27.4831888029344,23.4290478671883,25.2268920962917));
#61284=CARTESIAN_POINT('Ctrl Pts',(-27.4777145063877,23.3100758243375,25.2329477146182));
#61285=CARTESIAN_POINT('Ctrl Pts',(-27.4668658374458,23.1916033811171,25.2390033329447));
#61286=CARTESIAN_POINT('Ctrl Pts',(-27.4563455896034,23.0767174470138,25.2448756299034));
#61287=CARTESIAN_POINT('Ctrl Pts',(-27.4407485117847,22.9621023256229,25.2507479268621));
#61288=CARTESIAN_POINT('Ctrl Pts',(-27.4200937657703,22.8482426862899,25.2566202238209));
#61289=CARTESIAN_POINT('Ctrl Pts',(-27.3994657866663,22.7345306000068,25.2624849107491));
#61290=CARTESIAN_POINT('Ctrl Pts',(-27.3737932466934,22.6215724518033,25.2683495976774));
#61291=CARTESIAN_POINT('Ctrl Pts',(-27.3431471645599,22.5098490984151,25.2742142846057));
#61292=CARTESIAN_POINT('Ctrl Pts',(-27.3125326000033,22.3982406455016,25.2800729400706));
#61293=CARTESIAN_POINT('Ctrl Pts',(-27.2769547759334,22.2878648577489,25.2859315955355));
#61294=CARTESIAN_POINT('Ctrl Pts',(-27.2365358654385,22.1791930204553,25.2917902510004));
#61295=CARTESIAN_POINT('Ctrl Pts',(-27.1945381566028,22.0662763652207,25.2978777507221));
#61296=CARTESIAN_POINT('Ctrl Pts',(-27.1473135383742,21.9551999371496,25.3039652504437));
#61297=CARTESIAN_POINT('Ctrl Pts',(-27.0950564754956,21.8464761379119,25.3100527501653));
#61298=CARTESIAN_POINT('Ctrl Pts',(-27.0448221335849,21.741960724992,25.315904620239));
#61299=CARTESIAN_POINT('Ctrl Pts',(-26.989937881809,21.6396196077161,25.3217564903127));
#61300=CARTESIAN_POINT('Ctrl Pts',(-26.9306254464183,21.5398874013262,25.3276083603864));
#61301=CARTESIAN_POINT('Ctrl Pts',(-26.8713220418845,21.4401703800702,25.3334593394597));
#61302=CARTESIAN_POINT('Ctrl Pts',(-26.8075920055672,21.3430618350799,25.339310318533));
#61303=CARTESIAN_POINT('Ctrl Pts',(-26.7397022490512,21.2489703889635,25.3451612976064));
#61304=CARTESIAN_POINT('Ctrl Pts',(-26.6718063885919,21.1548704831194,25.3510128027391));
#61305=CARTESIAN_POINT('Ctrl Pts',(-26.599750306352,21.0637885506526,25.3568643078719));
#61306=CARTESIAN_POINT('Ctrl Pts',(-26.5238429085688,20.9761023281205,25.3627158130046));
#61307=CARTESIAN_POINT('Ctrl Pts',(-26.4479103035901,20.8883869869013,25.3685692612949));
#61308=CARTESIAN_POINT('Ctrl Pts',(-26.3681241103962,20.8040699102383,25.3744227095852));
#61309=CARTESIAN_POINT('Ctrl Pts',(-26.2848314978683,20.723493454985,25.3802761578756));
#61310=CARTESIAN_POINT('Ctrl Pts',(-26.2014441635507,20.6428253668026,25.3861362628078));
#61311=CARTESIAN_POINT('Ctrl Pts',(-26.1145427481355,20.5659066782754,25.3919963677401));
#61312=CARTESIAN_POINT('Ctrl Pts',(-26.0245091126335,20.4930408328289,25.3978564726723));
#61313=CARTESIAN_POINT('Ctrl Pts',(-25.9344148451114,20.4201259167948,25.4037205240186));
#61314=CARTESIAN_POINT('Ctrl Pts',(-25.8411844890698,20.3512695234804,25.4095845753648));
#61315=CARTESIAN_POINT('Ctrl Pts',(-25.7452291732017,20.2867319567266,25.4154486267111));
#61316=CARTESIAN_POINT('Ctrl Pts',(-25.6491324383487,20.22209927448,25.4213213204987));
#61317=CARTESIAN_POINT('Ctrl Pts',(-25.5503030799719,20.161798336786,25.4271940142863));
#61318=CARTESIAN_POINT('Ctrl Pts',(-25.4491771637542,20.106043734052,25.4330667080738));
#61319=CARTESIAN_POINT('Ctrl Pts',(-25.4214905778971,20.0907790555872,25.4346745534892));
#61320=CARTESIAN_POINT('Ctrl Pts',(-25.3936319633703,20.0758548794012,25.4362823989045));
#61321=CARTESIAN_POINT('Ctrl Pts',(-25.3656105122009,20.0612749733527,25.4378902443198));
#61322=CARTESIAN_POINT('Ctrl Pts',(-25.2632684082845,20.0080251166311,25.443762541282));
#61323=CARTESIAN_POINT('Ctrl Pts',(-25.1584099018201,19.9591928679016,25.4496348382441));
#61324=CARTESIAN_POINT('Ctrl Pts',(-25.0514531110148,19.9150240903652,25.4555071352063));
#61325=CARTESIAN_POINT('Ctrl Pts',(-24.9446349277183,19.8709125520575,25.4613718221378));
#61326=CARTESIAN_POINT('Ctrl Pts',(-24.8357242461717,19.831452622943,25.4672365090693));
#61327=CARTESIAN_POINT('Ctrl Pts',(-24.7251640078375,19.796844477242,25.4731011960008));
#61328=CARTESIAN_POINT('Ctrl Pts',(-24.6147174737893,19.7622719238529,25.4789598514688));
#61329=CARTESIAN_POINT('Ctrl Pts',(-24.5026251494462,19.7325413517449,25.4848185069368));
#61330=CARTESIAN_POINT('Ctrl Pts',(-24.3893495747704,19.7078047243322,25.4906771624049));
#61331=CARTESIAN_POINT('Ctrl Pts',(-24.2716493561908,19.6821018624247,25.4967646621253));
#61332=CARTESIAN_POINT('Ctrl Pts',(-24.1526719854879,19.6617912078772,25.5028521618457));
#61333=CARTESIAN_POINT('Ctrl Pts',(-24.0329536712201,19.6469861290642,25.5089396615661));
#61334=CARTESIAN_POINT('Ctrl Pts',(-23.9178693093251,19.6327541123638,25.5147915316425));
#61335=CARTESIAN_POINT('Ctrl Pts',(-23.8021007454281,19.6236094418233,25.5206434017189));
#61336=CARTESIAN_POINT('Ctrl Pts',(-23.6861334810624,19.6196005033917,25.5264952717952));
#61337=CARTESIAN_POINT('Ctrl Pts',(-23.5701838737685,19.6155921753574,25.5323462508711));
#61338=CARTESIAN_POINT('Ctrl Pts',(-23.4540360391832,19.6167180389193,25.538197229947));
#61339=CARTESIAN_POINT('Ctrl Pts',(-23.3381780353898,19.622974414726,25.5440482090229));
#61340=CARTESIAN_POINT('Ctrl Pts',(-23.222309614848,19.6292313530411,25.5498997141581));
#61341=CARTESIAN_POINT('Ctrl Pts',(-23.1067314897063,19.6406196982961,25.5557512192932));
#61342=CARTESIAN_POINT('Ctrl Pts',(-22.9919284329852,19.6570837451142,25.5616027244284));
#61343=CARTESIAN_POINT('Ctrl Pts',(-22.8770872526689,19.6735532592837,25.5674561727209));
#61344=CARTESIAN_POINT('Ctrl Pts',(-22.7630220615436,19.6951017679341,25.5733096210135));
#61345=CARTESIAN_POINT('Ctrl Pts',(-22.6502085496725,19.7216222504544,25.5791630693061));
#61346=CARTESIAN_POINT('Ctrl Pts',(-22.5372667443421,19.748172892522,25.5850231742404));
#61347=CARTESIAN_POINT('Ctrl Pts',(-22.4255798620429,19.7797066994432,25.5908832791747));
#61348=CARTESIAN_POINT('Ctrl Pts',(-22.3156096068854,19.8160664291787,25.5967433841091));
#61349=CARTESIAN_POINT('Ctrl Pts',(-22.2055652936444,19.8524506449164,25.6026074354572));
#61350=CARTESIAN_POINT('Ctrl Pts',(-22.0972402948686,19.8936671081312,25.6084714868054));
#61351=CARTESIAN_POINT('Ctrl Pts',(-21.9910758410352,19.9395106346174,25.6143355381536));
#61352=CARTESIAN_POINT('Ctrl Pts',(-21.8847549219887,19.9854217253107,25.620208231943));
#61353=CARTESIAN_POINT('Ctrl Pts',(-21.7806012734547,20.0359733095945,25.6260809257323));
#61354=CARTESIAN_POINT('Ctrl Pts',(-21.6790311459315,20.0909145133063,25.6319536195216));
#61355=CARTESIAN_POINT('Ctrl Pts',(-21.6512229428726,20.1059564964796,25.6335614649126));
#61356=CARTESIAN_POINT('Ctrl Pts',(-21.6236082212991,20.1213272661659,25.6351693103035));
#61357=CARTESIAN_POINT('Ctrl Pts',(-21.5961951198538,20.1370211256463,25.6367771556945));
#61358=CARTESIAN_POINT('Ctrl Pts',(-21.4960748752334,20.1943394503662,25.6426494527118));
#61359=CARTESIAN_POINT('Ctrl Pts',(-21.3983110161499,20.2561627712394,25.6485217497292));
#61360=CARTESIAN_POINT('Ctrl Pts',(-21.3033364020601,20.3222722178772,25.6543940467465));
#61361=CARTESIAN_POINT('Ctrl Pts',(-21.2084848675243,20.3882959919246,25.6602587337335));
#61362=CARTESIAN_POINT('Ctrl Pts',(-21.1164157259102,20.4585946118878,25.6661234207205));
#61363=CARTESIAN_POINT('Ctrl Pts',(-21.0275368157894,20.5329036263259,25.6719881077075));
#61364=CARTESIAN_POINT('Ctrl Pts',(-20.9387493120618,20.6071362185963,25.6778467632312));
#61365=CARTESIAN_POINT('Ctrl Pts',(-20.8531458290784,20.6853707380602,25.6837054187549));
#61366=CARTESIAN_POINT('Ctrl Pts',(-20.7711042386705,20.7673001847462,25.6895640742786));
#61367=CARTESIAN_POINT('Ctrl Pts',(-20.6858580324472,20.8524298668164,25.6956515739783));
#61368=CARTESIAN_POINT('Ctrl Pts',(-20.6044580258697,20.9415487550151,25.7017390736779));
#61369=CARTESIAN_POINT('Ctrl Pts',(-20.5272894410991,21.0342670085045,25.7078265733775));
#61370=CARTESIAN_POINT('Ctrl Pts',(-20.453107829823,21.1233964056421,25.7136784435097));
#61371=CARTESIAN_POINT('Ctrl Pts',(-20.382836448119,21.2158513597159,25.7195303136419));
#61372=CARTESIAN_POINT('Ctrl Pts',(-20.3167784380616,21.3112495647897,25.725382183774));
#61373=CARTESIAN_POINT('Ctrl Pts',(-20.2507304859382,21.4066332446175,25.7312331629057));
#61374=CARTESIAN_POINT('Ctrl Pts',(-20.1888948651744,21.5049589446407,25.7370841420373));
#61375=CARTESIAN_POINT('Ctrl Pts',(-20.1315322963575,21.6058140645527,25.7429351211689));
#61376=CARTESIAN_POINT('Ctrl Pts',(-20.0741645700954,21.7066782523076,25.7487866263597));
#61377=CARTESIAN_POINT('Ctrl Pts',(-20.0212708996425,21.8100719526892,25.7546381315505));
#61378=CARTESIAN_POINT('Ctrl Pts',(-19.973066459502,21.915557206897,25.7604896367413));
#61379=CARTESIAN_POINT('Ctrl Pts',(-19.9248460117182,22.021077490457,25.7663430850893));
#61380=CARTESIAN_POINT('Ctrl Pts',(-19.8813180623491,22.1286903331453,25.7721965334374));
#61381=CARTESIAN_POINT('Ctrl Pts',(-19.8426497038071,22.2379376797462,25.7780499817854));
#61382=CARTESIAN_POINT('Ctrl Pts',(-19.8039373709488,22.347309264291,25.7839100867746));
#61383=CARTESIAN_POINT('Ctrl Pts',(-19.7700957974783,22.4583186729053,25.7897701917639));
#61384=CARTESIAN_POINT('Ctrl Pts',(-19.7412422636771,22.5704924701789,25.7956302967531));
#61385=CARTESIAN_POINT('Ctrl Pts',(-19.7123692988283,22.6827418094784,25.801494348156));
#61386=CARTESIAN_POINT('Ctrl Pts',(-19.6884911473059,22.7961566952951,25.8073583995588));
#61387=CARTESIAN_POINT('Ctrl Pts',(-19.6696736879759,22.9102550022567,25.8132224509617));
#61388=CARTESIAN_POINT('Ctrl Pts',(-19.6508284954699,23.0245214673303,25.8190951448049));
#61389=CARTESIAN_POINT('Ctrl Pts',(-19.6370589297637,23.1394729548704,25.8249678386481));
#61390=CARTESIAN_POINT('Ctrl Pts',(-19.6283789272586,23.2546236582208,25.8308405324914));
#61391=CARTESIAN_POINT('Ctrl Pts',(-19.626002488476,23.2861499852147,25.8324483773507));
#61392=CARTESIAN_POINT('Ctrl Pts',(-19.6240072479966,23.3176912560264,25.8340562222101));
#61393=CARTESIAN_POINT('Ctrl Pts',(-19.6223928123571,23.3492375441713,25.8356640670695));
#61394=CARTESIAN_POINT('Ctrl Pts',(-19.6164964441009,23.4644533678718,25.8415363639624));
#61395=CARTESIAN_POINT('Ctrl Pts',(-19.615663930763,23.580121866316,25.8474086608553));
#61396=CARTESIAN_POINT('Ctrl Pts',(-19.619945111908,23.6957605588742,25.8532809577482));
#61397=CARTESIAN_POINT('Ctrl Pts',(-19.6242207449823,23.811249392871,25.8591456446107));
#61398=CARTESIAN_POINT('Ctrl Pts',(-19.6335968787783,23.9267080885084,25.8650103314732));
#61399=CARTESIAN_POINT('Ctrl Pts',(-19.6480714799083,24.0416505771553,25.8708750183357));
#61400=CARTESIAN_POINT('Ctrl Pts',(-19.6625311948174,24.1564748546504,25.8767336737351));
#61401=CARTESIAN_POINT('Ctrl Pts',(-19.6820788962216,24.2707835734378,25.8825923291344));
#61402=CARTESIAN_POINT('Ctrl Pts',(-19.7066605556467,24.3840928771222,25.8884509845337));
#61403=CARTESIAN_POINT('Ctrl Pts',(-19.7322023967884,24.5018281440757,25.89453848428));
#61404=CARTESIAN_POINT('Ctrl Pts',(-19.7631794580564,24.6184838737862,25.9006259840263));
#61405=CARTESIAN_POINT('Ctrl Pts',(-19.7994719887203,24.7335252468569,25.9067134837726));
#61406=CARTESIAN_POINT('Ctrl Pts',(-19.8343597391252,24.8441136967807,25.9125653537814));
#61407=CARTESIAN_POINT('Ctrl Pts',(-19.8741589810529,24.953210009544,25.9184172237903));
#61408=CARTESIAN_POINT('Ctrl Pts',(-19.9187119352538,25.0603524940826,25.9242690937992));
#61409=CARTESIAN_POINT('Ctrl Pts',(-19.9632581058659,25.1674786652122,25.9301200728081));
#61410=CARTESIAN_POINT('Ctrl Pts',(-20.0125563909366,25.2726512180256,25.935971051817));
#61411=CARTESIAN_POINT('Ctrl Pts',(-20.0664005934423,25.3754277759758,25.9418220308259));
#61412=CARTESIAN_POINT('Ctrl Pts',(-20.1202496370651,25.4782135745374,25.9476735358947));
#61413=CARTESIAN_POINT('Ctrl Pts',(-20.1786452187761,25.5786025837979,25.9535250409634));
#61414=CARTESIAN_POINT('Ctrl Pts',(-20.2413351874361,25.6761770385543,25.9593765460322));
#61415=CARTESIAN_POINT('Ctrl Pts',(-20.304045974077,25.7737838956739,25.9652299942591));
#61416=CARTESIAN_POINT('Ctrl Pts',(-20.3710537599934,25.8685739921877,25.971083442486));
#61417=CARTESIAN_POINT('Ctrl Pts',(-20.4420634961868,25.9601591521987,25.9769368907129));
#61418=CARTESIAN_POINT('Ctrl Pts',(-20.5131539858863,26.0518484644455,25.9827969955829));
#61419=CARTESIAN_POINT('Ctrl Pts',(-20.5882552562493,26.1403252385755,25.9886571004528));
#61420=CARTESIAN_POINT('Ctrl Pts',(-20.6670323930936,26.2252348928264,25.9945172053228));
#61421=CARTESIAN_POINT('Ctrl Pts',(-20.7458625814187,26.3102017284253,26.0003812566073));
#61422=CARTESIAN_POINT('Ctrl Pts',(-20.8283732718001,26.391596371224,26.0062453078918));
#61423=CARTESIAN_POINT('Ctrl Pts',(-20.9141944544012,26.469102787041,26.0121093591763));
#61424=CARTESIAN_POINT('Ctrl Pts',(-21.0001421203178,26.5467234318648,26.0179820529035));
#61425=CARTESIAN_POINT('Ctrl Pts',(-21.0894096984637,26.6204441505506,26.0238547466307));
#61426=CARTESIAN_POINT('Ctrl Pts',(-21.181596004773,26.6899906190947,26.0297274403578));
#61427=CARTESIAN_POINT('Ctrl Pts',(-21.2068350847242,26.7090312873912,26.0313352863866));
#61428=CARTESIAN_POINT('Ctrl Pts',(-21.2322927913215,26.7277593244731,26.0329431324155));
#61429=CARTESIAN_POINT('Ctrl Pts',(-21.257960560544,26.7461696956708,26.0345509784443));
#61430=CARTESIAN_POINT('Ctrl Pts',(-21.3517063298641,26.8134094466769,26.0404232753943));
#61431=CARTESIAN_POINT('Ctrl Pts',(-21.4485701703373,26.8766335814062,26.0462955723443));
#61432=CARTESIAN_POINT('Ctrl Pts',(-21.5481731033077,26.9355393677587,26.0521678692943));
#61433=CARTESIAN_POINT('Ctrl Pts',(-21.6476469587745,26.9943688168827,26.058032556213));
#61434=CARTESIAN_POINT('Ctrl Pts',(-21.749852495235,27.0488908380479,26.0638972431318));
#61435=CARTESIAN_POINT('Ctrl Pts',(-21.8543796758573,27.0988444012723,26.0697619300506));
#61436=CARTESIAN_POINT('Ctrl Pts',(-21.958799356805,27.1487465903779,26.0756205855053));
#61437=CARTESIAN_POINT('Ctrl Pts',(-22.0655355619873,27.1940894896742,26.08147924096));
#61438=CARTESIAN_POINT('Ctrl Pts',(-22.1741520102149,27.2346570093248,26.0873378964147));
#61439=CARTESIAN_POINT('Ctrl Pts',(-22.287011113101,27.2768091322196,26.0934253961399));
#61440=CARTESIAN_POINT('Ctrl Pts',(-22.4018999500598,27.3138049776414,26.0995128958651));
#61441=CARTESIAN_POINT('Ctrl Pts',(-22.5183038382273,27.3454562013346,26.1056003955903));
#61442=CARTESIAN_POINT('Ctrl Pts',(-22.6302020655757,27.3758822968923,26.111452265652));
#61443=CARTESIAN_POINT('Ctrl Pts',(-22.743499802301,27.4013697087658,26.1173041357137));
#61444=CARTESIAN_POINT('Ctrl Pts',(-22.8577233335861,27.4218016156873,26.1231560057754));
#61445=CARTESIAN_POINT('Ctrl Pts',(-22.9719294732892,27.4422304116632,26.1290069848361));
#61446=CARTESIAN_POINT('Ctrl Pts',(-23.0870607204648,27.4576051604215,26.1348579638968));
#61447=CARTESIAN_POINT('Ctrl Pts',(-23.2026334380633,27.4678602156951,26.1407089429576));
#61448=CARTESIAN_POINT('Ctrl Pts',(-23.3182165467511,27.4781161929961,26.1465604480771));
#61449=CARTESIAN_POINT('Ctrl Pts',(-23.4342407929771,27.483251525221,26.1524119531966));
#61450=CARTESIAN_POINT('Ctrl Pts',(-23.5502184054799,27.4832525315461,26.1582634583162));
#61451=CARTESIAN_POINT('Ctrl Pts',(-23.6662345316134,27.4832535382055,26.1641169065927));
#61452=CARTESIAN_POINT('Ctrl Pts',(-23.7822035800667,27.4781168286814,26.1699703548692));
#61453=CARTESIAN_POINT('Ctrl Pts',(-23.8976394854457,27.4678808071133,26.1758238031457));
#61454=CARTESIAN_POINT('Ctrl Pts',(-24.0132066665041,27.4576331449669,26.1816839080634));
#61455=CARTESIAN_POINT('Ctrl Pts',(-24.1282390823215,27.4422746326328,26.1875440129811));
#61456=CARTESIAN_POINT('Ctrl Pts',(-24.2422573819904,27.4218953725521,26.1934041178988));
#61457=CARTESIAN_POINT('Ctrl Pts',(-24.356352465841,27.4015023883165,26.19926816923));
#61458=CARTESIAN_POINT('Ctrl Pts',(-24.4694316713346,27.3760820142201,26.2051322205612));
#61459=CARTESIAN_POINT('Ctrl Pts',(-24.5810291076006,27.345774715869,26.2109962718924));
#61460=CARTESIAN_POINT('Ctrl Pts',(-24.6927910162044,27.3154227506116,26.2168689656644));
#61461=CARTESIAN_POINT('Ctrl Pts',(-24.8030664047997,27.2801696120006,26.2227416594364));
#61462=CARTESIAN_POINT('Ctrl Pts',(-24.9114076229943,27.2402045391636,26.2286143532083));
#61463=CARTESIAN_POINT('Ctrl Pts',(-24.9410696402747,27.2292627692551,26.2302221987453));
#61464=CARTESIAN_POINT('Ctrl Pts',(-24.9705868127282,27.2179680748707,26.2318300442823));
#61465=CARTESIAN_POINT('Ctrl Pts',(-24.9999502753945,27.2063249396082,26.2334378898193));
#61466=CARTESIAN_POINT('Ctrl Pts',(-25.1071937747825,27.163800984461,26.2393101870964));
#61467=CARTESIAN_POINT('Ctrl Pts',(-25.2127443181152,27.1164831324113,26.2451824843735));
#61468=CARTESIAN_POINT('Ctrl Pts',(-25.3161423577351,27.0645265850778,26.2510547816507));
#61469=CARTESIAN_POINT('Ctrl Pts',(-25.4194064017332,27.0126373692904,26.2569194688983));
#61470=CARTESIAN_POINT('Ctrl Pts',(-25.5205231233169,26.9561215965882,26.262784156146));
#61471=CARTESIAN_POINT('Ctrl Pts',(-25.6190512712638,26.8951831401157,26.2686488433937));
#61472=CARTESIAN_POINT('Ctrl Pts',(-25.7174780891955,26.8343073550204,26.2745074991787));
#61473=CARTESIAN_POINT('Ctrl Pts',(-25.813321279255,26.7690181493974,26.2803661549637));
#61474=CARTESIAN_POINT('Ctrl Pts',(-25.9061632129341,26.6995657682618,26.2862248107487));
#61475=CARTESIAN_POINT('Ctrl Pts',(-26.0026316273711,26.627400521142,26.2923123103506));
#61476=CARTESIAN_POINT('Ctrl Pts',(-26.0958591363951,26.5507404384385,26.2983998099525));
#61477=CARTESIAN_POINT('Ctrl Pts',(-26.1854090749907,26.4699167233987,26.3044873095544));
#61478=CARTESIAN_POINT('Ctrl Pts',(-26.2714927987967,26.3922214566954,26.3103391799478));
#61479=CARTESIAN_POINT('Ctrl Pts',(-26.354178018873,26.3106791910452,26.3161910503412));
#61480=CARTESIAN_POINT('Ctrl Pts',(-26.433110388563,26.2256253238654,26.3220429207346));
#61481=CARTESIAN_POINT('Ctrl Pts',(-26.5120307400745,26.1405844069182,26.3278939001269));
#61482=CARTESIAN_POINT('Ctrl Pts',(-26.5871990962165,26.0520332544666,26.3337448795193));
#61483=CARTESIAN_POINT('Ctrl Pts',(-26.6582988013325,25.9603432739251,26.3395958589117));
#61484=CARTESIAN_POINT('Ctrl Pts',(-26.7294048989848,25.8686450495868,26.3454473643625));
#61485=CARTESIAN_POINT('Ctrl Pts',(-26.7964413650836,25.7738077628449,26.3512988698133));
#61486=CARTESIAN_POINT('Ctrl Pts',(-26.8591330286557,25.67623438882,26.3571503752641));
#61487=CARTESIAN_POINT('Ctrl Pts',(-26.9218455107501,25.5786286128239,26.3630038238711));
#61488=CARTESIAN_POINT('Ctrl Pts',(-26.9802100980387,25.4782852904618,26.3688572724781));
#61489=CARTESIAN_POINT('Ctrl Pts',(-27.0339963615948,25.3756341158102,26.3747107210852));
#61490=CARTESIAN_POINT('Ctrl Pts',(-27.0878437917777,25.2728662045481,26.3805708263306));
#61491=CARTESIAN_POINT('Ctrl Pts',(-27.1371023141482,25.1677855688989,26.386430931576));
#61492=CARTESIAN_POINT('Ctrl Pts',(-27.1815886238932,25.0608441990527,26.3922910368214));
#61493=CARTESIAN_POINT('Ctrl Pts',(-27.2261048923698,24.9538308109199,26.3981550884792));
#61494=CARTESIAN_POINT('Ctrl Pts',(-27.265842407552,24.844954580822,26.4040191401369));
#61495=CARTESIAN_POINT('Ctrl Pts',(-27.300667511722,24.7346833982218,26.4098831917946));
#61496=CARTESIAN_POINT('Ctrl Pts',(-27.3355439411133,24.624249698007,26.4157558858888));
#61497=CARTESIAN_POINT('Ctrl Pts',(-27.3654934034944,24.5124173399615,26.421628579983));
#61498=CARTESIAN_POINT('Ctrl Pts',(-27.3904331348813,24.3996652316849,26.4275012740772));
#61499=CARTESIAN_POINT('Ctrl Pts',(-27.397261203266,24.3687956487736,26.4291091164495));
#61500=CARTESIAN_POINT('Ctrl Pts',(-27.4037140570737,24.3378571558806,26.4307169588218));
#61501=CARTESIAN_POINT('Ctrl Pts',(-27.4097906765489,24.3068596347614,26.4323248011941));
#61502=CARTESIAN_POINT('Ctrl Pts',(-27.4421880595738,24.1415969309467,26.4408969827157));
#61503=CARTESIAN_POINT('Ctrl Pts',(-27.4639789012828,23.9741922082478,26.4494691642373));
#61504=CARTESIAN_POINT('Ctrl Pts',(-27.4749442882531,23.8057591186902,26.4580413457589));
#61505=CARTESIAN_POINT('Ctrl Pts',(-27.4804000591723,23.7219561161772,26.4623063898276));
#61506=CARTESIAN_POINT('Ctrl Pts',(-27.4831766269209,23.6378988905708,26.4665714338964));
#61507=CARTESIAN_POINT('Ctrl Pts',(-27.483250996526,23.5537275325671,26.4708364779651));
#61508=CARTESIAN_POINT('',(-27.4767779762767,23.5507168464414,27.7208364779651));
#61509=CARTESIAN_POINT('Ctrl Pts',(-27.4848126564242,23.5537136372146,26.4708372516642));
#61510=CARTESIAN_POINT('Ctrl Pts',(-27.4750743970666,22.4982795966798,26.5242954052991));
#61511=CARTESIAN_POINT('Ctrl Pts',(-26.4929708527558,20.1179887131869,26.6440491960592));
#61512=CARTESIAN_POINT('Ctrl Pts',(-22.4668397420095,19.0262093874363,26.8300986239438));
#61513=CARTESIAN_POINT('Ctrl Pts',(-19.1584684333861,22.0163084907552,27.0289855353188));
#61514=CARTESIAN_POINT('Ctrl Pts',(-19.8857744770669,26.4159729476211,27.2278724466937));
#61515=CARTESIAN_POINT('Ctrl Pts',(-23.9804249150498,28.1822817349765,27.4267593580686));
#61516=CARTESIAN_POINT('Ctrl Pts',(-27.036853459589,26.124923812395,27.5910807018257));
#61517=CARTESIAN_POINT('Ctrl Pts',(-27.4774395641842,24.1804189441493,27.6891064084579));
#61518=CARTESIAN_POINT('Ctrl Pts',(-27.4767779762767,23.5507168464414,27.7208364779651));
#61519=CARTESIAN_POINT('',(-27.4832508103722,23.5465728691724,28.9708364828311));
#61520=CARTESIAN_POINT('Ctrl Pts',(-27.4767779762767,23.5507168464414,27.7208364779651));
#61521=CARTESIAN_POINT('Ctrl Pts',(-27.4760572668075,22.8647426025963,27.7554020455828));
#61522=CARTESIAN_POINT('Ctrl Pts',(-26.9778217625069,20.8621128540598,27.8562632503257));
#61523=CARTESIAN_POINT('Ctrl Pts',(-23.7820353409766,18.9040740354896,28.0234200921932));
#61524=CARTESIAN_POINT('Ctrl Pts',(-19.766626082321,20.8437801165488,28.2223070035682));
#61525=CARTESIAN_POINT('Ctrl Pts',(-19.2280545259956,25.2705428060829,28.4211939149431));
#61526=CARTESIAN_POINT('Ctrl Pts',(-22.6612055347411,28.1164329704806,28.6200808263178));
#61527=CARTESIAN_POINT('Ctrl Pts',(-26.5764164330689,26.8729013389392,28.803295013992));
#61528=CARTESIAN_POINT('Ctrl Pts',(-27.4738633797249,24.5471524573527,28.920213564541));
#61529=CARTESIAN_POINT('Ctrl Pts',(-27.4830944336655,23.5465731116532,28.9708364779651));
#61530=CARTESIAN_POINT('',(-25.2989497345943,27.0731131722205,29.9999401439846));
#61531=CARTESIAN_POINT('Ctrl Pts',(-27.4832508103721,23.5465728691724,28.9708364828311));
#61532=CARTESIAN_POINT('Ctrl Pts',(-27.483105894416,23.391679804188,28.9786728438705));
#61533=CARTESIAN_POINT('Ctrl Pts',(-27.4738070756413,23.2371955920286,28.9865092049099));
#61534=CARTESIAN_POINT('Ctrl Pts',(-27.4555207700342,23.0840240612928,28.9943455659493));
#61535=CARTESIAN_POINT('Ctrl Pts',(-27.4372344644271,22.9308525305571,29.0021819269888));
#61536=CARTESIAN_POINT('Ctrl Pts',(-27.4099608272759,22.778993144504,29.0100182880282));
#61537=CARTESIAN_POINT('Ctrl Pts',(-27.3739131308343,22.6293244006311,29.0178546490677));
#61538=CARTESIAN_POINT('Ctrl Pts',(-27.34689356463,22.5171401299844,29.0237283968188));
#61539=CARTESIAN_POINT('Ctrl Pts',(-27.3148874883134,22.4059583868975,29.0296021445699));
#61540=CARTESIAN_POINT('Ctrl Pts',(-27.2779840235745,22.2962561503422,29.035475892321));
#61541=CARTESIAN_POINT('Ctrl Pts',(-27.2411284068907,22.1866961508015,29.0413420243263));
#61542=CARTESIAN_POINT('Ctrl Pts',(-27.1993881599582,22.0786122309629,29.0472081563316));
#61543=CARTESIAN_POINT('Ctrl Pts',(-27.1529031639015,21.9724700935057,29.0530742883369));
#61544=CARTESIAN_POINT('Ctrl Pts',(-27.106466020728,21.8664372215693,29.058934381591));
#61545=CARTESIAN_POINT('Ctrl Pts',(-27.0552940085456,21.7623425322087,29.064794474845));
#61546=CARTESIAN_POINT('Ctrl Pts',(-26.9995762403214,21.6606348579035,29.070654568099));
#61547=CARTESIAN_POINT('Ctrl Pts',(-26.9417014418957,21.5549897228528,29.0767415261133));
#61548=CARTESIAN_POINT('Ctrl Pts',(-26.8789219544355,21.4519205880235,29.0828284841276));
#61549=CARTESIAN_POINT('Ctrl Pts',(-26.8115041026131,21.3519060641921,29.088915442142));
#61550=CARTESIAN_POINT('Ctrl Pts',(-26.7466744075751,21.25573107635,29.0947687231515));
#61551=CARTESIAN_POINT('Ctrl Pts',(-26.677556166298,21.1623808660154,29.1006220041611));
#61552=CARTESIAN_POINT('Ctrl Pts',(-26.6044316819318,21.072253597422,29.1064752851707));
#61553=CARTESIAN_POINT('Ctrl Pts',(-26.5313184814589,20.9821402364343,29.1123276629561));
#61554=CARTESIAN_POINT('Ctrl Pts',(-26.4542005273581,20.8952491490648,29.1181800407415));
#61555=CARTESIAN_POINT('Ctrl Pts',(-26.3734010795189,20.8119462528212,29.1240324185269));
#61556=CARTESIAN_POINT('Ctrl Pts',(-26.2925945571716,20.7286360628765,29.1298853087254));
#61557=CARTESIAN_POINT('Ctrl Pts',(-26.2081061879956,20.6489149851832,29.1357381989239));
#61558=CARTESIAN_POINT('Ctrl Pts',(-26.1202963266871,20.5731123113118,29.1415910891225));
#61559=CARTESIAN_POINT('Ctrl Pts',(-26.0324575387834,20.4972846662899,29.1474459073981));
#61560=CARTESIAN_POINT('Ctrl Pts',(-25.9412953956253,20.4253782616515,29.1533007256738));
#61561=CARTESIAN_POINT('Ctrl Pts',(-25.8472030073224,20.3576818570636,29.1591555439494));
#61562=CARTESIAN_POINT('Ctrl Pts',(-25.7530041086937,20.2899088217701,29.1650169897388));
#61563=CARTESIAN_POINT('Ctrl Pts',(-25.6558686799156,20.226355540039,29.1708784355283));
#61564=CARTESIAN_POINT('Ctrl Pts',(-25.5562185432465,20.1672672582269,29.1767398813177));
#61565=CARTESIAN_POINT('Ctrl Pts',(-25.4565015736801,20.1081393473565,29.1826052582348));
#61566=CARTESIAN_POINT('Ctrl Pts',(-25.3542669013857,20.0534825936248,29.1884706351519));
#61567=CARTESIAN_POINT('Ctrl Pts',(-25.2499590890195,20.0034953340578,29.1943360120689));
#61568=CARTESIAN_POINT('Ctrl Pts',(-25.1454981624262,19.9534346978143,29.2002099988172));
#61569=CARTESIAN_POINT('Ctrl Pts',(-25.0389584008463,19.9080573971475,29.2060839855654));
#61570=CARTESIAN_POINT('Ctrl Pts',(-24.9308024499856,19.8675129368945,29.2119579723136));
#61571=CARTESIAN_POINT('Ctrl Pts',(-24.9014428602792,19.856506896927,29.2135525016899));
#61572=CARTESIAN_POINT('Ctrl Pts',(-24.8719642487308,19.8458566934534,29.2151470310662));
#61573=CARTESIAN_POINT('Ctrl Pts',(-24.8423760146667,19.835564670682,29.2167415604425));
#61574=CARTESIAN_POINT('Ctrl Pts',(-24.7333753579618,19.7976496927734,29.2226156774572));
#61575=CARTESIAN_POINT('Ctrl Pts',(-24.6225228972636,19.7644732561446,29.228489794472));
#61576=CARTESIAN_POINT('Ctrl Pts',(-24.5102682538304,19.7362180780937,29.2343639114867));
#61577=CARTESIAN_POINT('Ctrl Pts',(-24.3981586609349,19.7079994101474,29.2402304382245));
#61578=CARTESIAN_POINT('Ctrl Pts',(-24.2846508853829,19.6846894546324,29.2460969649623));
#61579=CARTESIAN_POINT('Ctrl Pts',(-24.1702124777709,19.6664221201983,29.2519634917001));
#61580=CARTESIAN_POINT('Ctrl Pts',(-24.0558913871888,19.6481735126013,29.2578240043426));
#61581=CARTESIAN_POINT('Ctrl Pts',(-23.9406419677007,19.6349573083073,29.2636845169851));
#61582=CARTESIAN_POINT('Ctrl Pts',(-23.8249441676021,19.6268568716617,29.2695450296275));
#61583=CARTESIAN_POINT('Ctrl Pts',(-23.7047788202789,19.6184436452894,29.2756318397188));
#61584=CARTESIAN_POINT('Ctrl Pts',(-23.584130207103,19.6155493418606,29.28171864981));
#61585=CARTESIAN_POINT('Ctrl Pts',(-23.4635448920503,19.6182084341252,29.2878054599013));
#61586=CARTESIAN_POINT('Ctrl Pts',(-23.3475765420952,19.6207657151852,29.2936592184826));
#61587=CARTESIAN_POINT('Ctrl Pts',(-23.2316671832364,19.6284589440699,29.2995129770639));
#61588=CARTESIAN_POINT('Ctrl Pts',(-23.1163044713861,19.6412656960864,29.3053667356452));
#61589=CARTESIAN_POINT('Ctrl Pts',(-23.000959155594,19.6540705169156,29.3112196115122));
#61590=CARTESIAN_POINT('Ctrl Pts',(-22.8861607333545,19.6719872821083,29.3170724873791));
#61591=CARTESIAN_POINT('Ctrl Pts',(-22.7723918519182,19.6949416800431,29.3229253632461));
#61592=CARTESIAN_POINT('Ctrl Pts',(-22.6586126238183,19.7178981655562,29.3287787714004));
#61593=CARTESIAN_POINT('Ctrl Pts',(-22.5458635275998,19.7458931128794,29.3346321795547));
#61594=CARTESIAN_POINT('Ctrl Pts',(-22.4346164315061,19.7788012073421,29.340485587709));
#61595=CARTESIAN_POINT('Ctrl Pts',(-22.3233323253789,19.8117202497731,29.3463409431935));
#61596=CARTESIAN_POINT('Ctrl Pts',(-22.2135516088998,19.8495555724328,29.352196298678));
#61597=CARTESIAN_POINT('Ctrl Pts',(-22.1057297411984,19.8921323986561,29.3580516541626));
#61598=CARTESIAN_POINT('Ctrl Pts',(-21.9977853623585,19.9347576022223,29.3639136627155));
#61599=CARTESIAN_POINT('Ctrl Pts',(-21.8918046592129,19.9821349108153,29.3697756712685));
#61600=CARTESIAN_POINT('Ctrl Pts',(-21.7882219911841,20.0340418761291,29.3756376798215));
#61601=CARTESIAN_POINT('Ctrl Pts',(-21.6845695848194,20.085983788461,29.3815036350456));
#61602=CARTESIAN_POINT('Ctrl Pts',(-21.583318788317,20.1424612293499,29.3873695902696));
#61603=CARTESIAN_POINT('Ctrl Pts',(-21.4848767760092,20.2032072694026,29.3932355454937));
#61604=CARTESIAN_POINT('Ctrl Pts',(-21.3862899701283,20.2640426578543,29.3991101286663));
#61605=CARTESIAN_POINT('Ctrl Pts',(-21.2905205340972,20.3291589447689,29.4049847118389));
#61606=CARTESIAN_POINT('Ctrl Pts',(-21.1979443244108,20.3982475986481,29.4108592950115));
#61607=CARTESIAN_POINT('Ctrl Pts',(-21.1728922030347,20.4169437339571,29.4124490206135));
#61608=CARTESIAN_POINT('Ctrl Pts',(-21.1480737204606,20.4359305512005,29.4140387462155));
#61609=CARTESIAN_POINT('Ctrl Pts',(-21.1234958640683,20.4552014697353,29.4156284718175));
#61610=CARTESIAN_POINT('Ctrl Pts',(-21.0328446115116,20.5262789825668,29.4214919049315));
#61611=CARTESIAN_POINT('Ctrl Pts',(-20.9451640888828,20.601463754417,29.4273553380455));
#61612=CARTESIAN_POINT('Ctrl Pts',(-20.8608504638897,20.6804780601218,29.4332187711595));
#61613=CARTESIAN_POINT('Ctrl Pts',(-20.7766465412602,20.7593895585271,29.4390745752282));
#61614=CARTESIAN_POINT('Ctrl Pts',(-20.6958011049263,20.8421204017871,29.4449303792968));
#61615=CARTESIAN_POINT('Ctrl Pts',(-20.6186790592074,20.9283513178015,29.4507861833654));
#61616=CARTESIAN_POINT('Ctrl Pts',(-20.5416365654878,21.014493285945,29.4566359471259));
#61617=CARTESIAN_POINT('Ctrl Pts',(-20.4683100983462,21.1041278389244,29.4624857108863));
#61618=CARTESIAN_POINT('Ctrl Pts',(-20.399028822363,21.1968978763673,29.4683354746468));
#61619=CARTESIAN_POINT('Ctrl Pts',(-20.326892500554,21.2934909194404,29.4744263041695));
#61620=CARTESIAN_POINT('Ctrl Pts',(-20.2591422635406,21.3934831060891,29.4805171336923));
#61621=CARTESIAN_POINT('Ctrl Pts',(-20.1961045467497,21.4964316302783,29.486607963215));
#61622=CARTESIAN_POINT('Ctrl Pts',(-20.1356316620657,21.5951914608784,29.4924509735604));
#61623=CARTESIAN_POINT('Ctrl Pts',(-20.0794955649851,21.6966713802769,29.4982939839058));
#61624=CARTESIAN_POINT('Ctrl Pts',(-20.0279405678685,21.8004504201712,29.5041369942511));
#61625=CARTESIAN_POINT('Ctrl Pts',(-19.9763932007642,21.9042141010238,29.5099791398454));
#61626=CARTESIAN_POINT('Ctrl Pts',(-19.9294257701819,22.0102758545438,29.5158212854397));
#61627=CARTESIAN_POINT('Ctrl Pts',(-19.8872362410366,22.1181908520249,29.5216634310339));
#61628=CARTESIAN_POINT('Ctrl Pts',(-19.8450426584752,22.2261162175855,29.5275061379203));
#61629=CARTESIAN_POINT('Ctrl Pts',(-19.8076280409059,22.3358947947495,29.5333488448066));
#61630=CARTESIAN_POINT('Ctrl Pts',(-19.7751416191933,22.447063246795,29.5391915516929));
#61631=CARTESIAN_POINT('Ctrl Pts',(-19.7426441471454,22.5582695130593,29.5450362459901));
#61632=CARTESIAN_POINT('Ctrl Pts',(-19.7150783203228,22.6708661963421,29.5508809402874));
#61633=CARTESIAN_POINT('Ctrl Pts',(-19.6925428826197,22.7843770434866,29.5567256345846));
#61634=CARTESIAN_POINT('Ctrl Pts',(-19.6699813573313,22.8980192936209,29.5625770948459));
#61635=CARTESIAN_POINT('Ctrl Pts',(-19.6524619248555,23.0125774127814,29.5684285551071));
#61636=CARTESIAN_POINT('Ctrl Pts',(-19.6400318126782,23.1275671539273,29.5742800153683));
#61637=CARTESIAN_POINT('Ctrl Pts',(-19.6275932055195,23.2426354813074,29.5801354746318));
#61638=CARTESIAN_POINT('Ctrl Pts',(-19.6202508698198,23.3581356051378,29.5859909338952));
#61639=CARTESIAN_POINT('Ctrl Pts',(-19.6179999132308,23.4735821685314,29.5918463931586));
#61640=CARTESIAN_POINT('Ctrl Pts',(-19.6157455789338,23.5892019670618,29.5977106389226));
#61641=CARTESIAN_POINT('Ctrl Pts',(-19.6185978609437,23.7047676317724,29.6035748846865));
#61642=CARTESIAN_POINT('Ctrl Pts',(-19.6264999418224,23.8197977291557,29.6094391304504));
#61643=CARTESIAN_POINT('Ctrl Pts',(-19.6287800281479,23.8529888032655,29.6111312146977));
#61644=CARTESIAN_POINT('Ctrl Pts',(-19.6314802181483,23.886135348282,29.612823298945));
#61645=CARTESIAN_POINT('Ctrl Pts',(-19.6345983585675,23.9192259676965,29.6145153831924));
#61646=CARTESIAN_POINT('Ctrl Pts',(-19.6454412758116,24.0342941813218,29.6203993803821));
#61647=CARTESIAN_POINT('Ctrl Pts',(-19.6613785537232,24.1490735677679,29.6262833775718));
#61648=CARTESIAN_POINT('Ctrl Pts',(-19.6823889312802,24.2630780142579,29.6321673747616));
#61649=CARTESIAN_POINT('Ctrl Pts',(-19.7033720247706,24.3769344146267,29.6380437309953));
#61650=CARTESIAN_POINT('Ctrl Pts',(-19.7294150418344,24.4900174753028,29.643920087229));
#61651=CARTESIAN_POINT('Ctrl Pts',(-19.7604448812621,24.6018451204501,29.6497964434627));
#61652=CARTESIAN_POINT('Ctrl Pts',(-19.7914426384536,24.7135571452464,29.6556667240398));
#61653=CARTESIAN_POINT('Ctrl Pts',(-19.8274168522906,24.8240159422113,29.661537004617));
#61654=CARTESIAN_POINT('Ctrl Pts',(-19.8682433048668,24.9327492056714,29.6674072851941));
#61655=CARTESIAN_POINT('Ctrl Pts',(-19.9105500442143,25.0454249231371,29.6734904105846));
#61656=CARTESIAN_POINT('Ctrl Pts',(-19.9580674810231,25.1562471619692,29.6795735359752));
#61657=CARTESIAN_POINT('Ctrl Pts',(-20.0106005710162,25.2647066714332,29.6856566613657));
#61658=CARTESIAN_POINT('Ctrl Pts',(-20.0612353894315,25.3692470205321,29.6915199743669));
#61659=CARTESIAN_POINT('Ctrl Pts',(-20.1165294634138,25.471592034314,29.6973832873681));
#61660=CARTESIAN_POINT('Ctrl Pts',(-20.1762592759672,25.5713063435232,29.7032466003692));
#61661=CARTESIAN_POINT('Ctrl Pts',(-20.2359791282306,25.6710040247975,29.7091089356292));
#61662=CARTESIAN_POINT('Ctrl Pts',(-20.3001330366619,25.7680715208699,29.7149712708892));
#61663=CARTESIAN_POINT('Ctrl Pts',(-20.3684523581246,25.8620995542008,29.7208336061492));
#61664=CARTESIAN_POINT('Ctrl Pts',(-20.436776660008,25.9561344420957,29.7266963687684));
#61665=CARTESIAN_POINT('Ctrl Pts',(-20.5092667365253,26.0471290938087,29.7325591313877));
#61666=CARTESIAN_POINT('Ctrl Pts',(-20.5856120051761,26.1347051910645,29.738421894007));
#61667=CARTESIAN_POINT('Ctrl Pts',(-20.6619811356613,26.222308660368,29.7442864890419));
#61668=CARTESIAN_POINT('Ctrl Pts',(-20.7422075839998,26.3064911403823,29.7501510840769));
#61669=CARTESIAN_POINT('Ctrl Pts',(-20.8259425513158,26.3869097423579,29.7560156791119));
#61670=CARTESIAN_POINT('Ctrl Pts',(-20.909769426386,26.4674166120351,29.7618867111442));
#61671=CARTESIAN_POINT('Ctrl Pts',(-20.9971122099963,26.5441510722723,29.7677577431765));
#61672=CARTESIAN_POINT('Ctrl Pts',(-21.0875874616023,26.6168091922745,29.7736287752088));
#61673=CARTESIAN_POINT('Ctrl Pts',(-21.1781217604102,26.6895147314173,29.7795036388746));
#61674=CARTESIAN_POINT('Ctrl Pts',(-21.2717922672247,26.7581383894613,29.7853785025405));
#61675=CARTESIAN_POINT('Ctrl Pts',(-21.3681862871104,26.8224193832236,29.7912533662064));
#61676=CARTESIAN_POINT('Ctrl Pts',(-21.4647179948349,26.8867921950377,29.7971366214435));
#61677=CARTESIAN_POINT('Ctrl Pts',(-21.5639806290897,26.9468097497583,29.8030198766806));
#61678=CARTESIAN_POINT('Ctrl Pts',(-21.6655365762954,27.0022569881608,29.8089031319177));
#61679=CARTESIAN_POINT('Ctrl Pts',(-21.6914245530531,27.0163912349335,29.8104028528009));
#61680=CARTESIAN_POINT('Ctrl Pts',(-21.7174614503872,27.0302287427097,29.8119025736841));
#61681=CARTESIAN_POINT('Ctrl Pts',(-21.7436398252607,27.0437664545165,29.8134022945673));
#61682=CARTESIAN_POINT('Ctrl Pts',(-21.8453103654917,27.096343685897,29.8192268514058));
#61683=CARTESIAN_POINT('Ctrl Pts',(-21.9494591145075,27.144572387477,29.8250514082443));
#61684=CARTESIAN_POINT('Ctrl Pts',(-22.0556742954077,27.1882086743131,29.8308759650828));
#61685=CARTESIAN_POINT('Ctrl Pts',(-22.1617537537081,27.2317892023562,29.8366930792565));
#61686=CARTESIAN_POINT('Ctrl Pts',(-22.2698940091309,27.2707888232274,29.8425101934301));
#61687=CARTESIAN_POINT('Ctrl Pts',(-22.379658318945,27.3050092733591,29.8483273076037));
#61688=CARTESIAN_POINT('Ctrl Pts',(-22.4893129316497,27.3391955239913,29.8541386082246));
#61689=CARTESIAN_POINT('Ctrl Pts',(-22.6005879721008,27.3686119767023,29.8599499088454));
#61690=CARTESIAN_POINT('Ctrl Pts',(-22.7130270413074,27.3931085631175,29.8657612094662));
#61691=CARTESIAN_POINT('Ctrl Pts',(-22.825387957362,27.4175881226625,29.8715684708197));
#61692=CARTESIAN_POINT('Ctrl Pts',(-22.9389108834846,27.43715452698,29.8773757321732));
#61693=CARTESIAN_POINT('Ctrl Pts',(-23.0531252998253,27.4517078390551,29.8831829935267));
#61694=CARTESIAN_POINT('Ctrl Pts',(-23.1672987307487,27.4662559287284,29.8889881709661));
#61695=CARTESIAN_POINT('Ctrl Pts',(-23.2821627419183,27.4757944482306,29.8947933484056));
#61696=CARTESIAN_POINT('Ctrl Pts',(-23.3972383674406,27.4802748809357,29.900598525845));
#61697=CARTESIAN_POINT('Ctrl Pts',(-23.5123016844848,27.4847548344141,29.9064030823632));
#61698=CARTESIAN_POINT('Ctrl Pts',(-23.6275761505149,27.4841777605835,29.9122076388813));
#61699=CARTESIAN_POINT('Ctrl Pts',(-23.7425802607441,27.4785472055493,29.9180121953995));
#61700=CARTESIAN_POINT('Ctrl Pts',(-23.8576010389199,27.4729158344591,29.9238175931923));
#61701=CARTESIAN_POINT('Ctrl Pts',(-23.9723509632556,27.4622295477953,29.9296229909851));
#61702=CARTESIAN_POINT('Ctrl Pts',(-24.0863519321435,27.4465439007833,29.9354283887779));
#61703=CARTESIAN_POINT('Ctrl Pts',(-24.2004654002933,27.4308427747474,29.9412395154954));
#61704=CARTESIAN_POINT('Ctrl Pts',(-24.3138280197813,27.4101324947749,29.9470506422129));
#61705=CARTESIAN_POINT('Ctrl Pts',(-24.4259701600802,27.3845200804359,29.9528617689304));
#61706=CARTESIAN_POINT('Ctrl Pts',(-24.5381711727251,27.3588942200997,29.9586759463714));
#61707=CARTESIAN_POINT('Ctrl Pts',(-24.6491500250568,27.328361212771,29.9644901238124));
#61708=CARTESIAN_POINT('Ctrl Pts',(-24.7584523537206,27.2930779604385,29.9703043012534));
#61709=CARTESIAN_POINT('Ctrl Pts',(-24.8679220240612,27.2577406895076,29.97612738019));
#61710=CARTESIAN_POINT('Ctrl Pts',(-24.9757096508579,27.2176387965406,29.9819504591267));
#61711=CARTESIAN_POINT('Ctrl Pts',(-25.0813807158189,27.1729774017028,29.9877735380633));
#61712=CARTESIAN_POINT('Ctrl Pts',(-25.1549762723192,27.1418725745831,29.9918290733704));
#61713=CARTESIAN_POINT('Ctrl Pts',(-25.2275456364601,27.1085571364939,29.9958846086775));
#61714=CARTESIAN_POINT('Ctrl Pts',(-25.2989497345943,27.0731131722205,29.9999401439846));
#61715=CARTESIAN_POINT('',(-21.801558056363,27.073114526145,30.));
#61716=CARTESIAN_POINT('Origin',(-23.5502525316942,23.5502525316942,30.));
#61717=CARTESIAN_POINT('',(-27.4823597385963,23.5463452821269,29.1541635220348));
#61718=CARTESIAN_POINT('Ctrl Pts',(-21.801558056363,27.073114526145,30.));
#61719=CARTESIAN_POINT('Ctrl Pts',(-20.6276058013427,26.4903826945007,29.933704362875));
#61720=CARTESIAN_POINT('Ctrl Pts',(-18.9286240350797,24.0691044546063,29.8011130886252));
#61721=CARTESIAN_POINT('Ctrl Pts',(-20.6189893842979,19.933885741136,29.6022261772502));
#61722=CARTESIAN_POINT('Ctrl Pts',(-25.0066490640735,19.1336642374115,29.4033392658754));
#61723=CARTESIAN_POINT('Ctrl Pts',(-27.2951287691289,21.5759483018016,29.2539850474702));
#61724=CARTESIAN_POINT('Ctrl Pts',(-27.4853611242349,23.2148653571988,29.17092646619));
#61725=CARTESIAN_POINT('Ctrl Pts',(-27.4823597385963,23.5463452821269,29.1541635220348));
#61726=CARTESIAN_POINT('',(-27.4808119672486,23.5510682671432,27.9041634967419));
#61727=CARTESIAN_POINT('Ctrl Pts',(-27.4823597385963,23.5463452821269,29.1541635220348));
#61728=CARTESIAN_POINT('Ctrl Pts',(-27.4734909675771,24.5258327274734,29.104630829065));
#61729=CARTESIAN_POINT('Ctrl Pts',(-26.6075785985611,26.8308346334369,28.9888024989704));
#61730=CARTESIAN_POINT('Ctrl Pts',(-22.7363170503599,28.1302192147636,28.8066785317506));
#61731=CARTESIAN_POINT('Ctrl Pts',(-19.256958269279,25.3414769801662,28.6077916203758));
#61732=CARTESIAN_POINT('Ctrl Pts',(-19.7226238927422,20.9062869097954,28.4089047090008));
#61733=CARTESIAN_POINT('Ctrl Pts',(-23.7056346214918,18.9009230350342,28.2100177976262));
#61734=CARTESIAN_POINT('Ctrl Pts',(-26.9542144477632,20.8185459147253,28.0417707353038));
#61735=CARTESIAN_POINT('Ctrl Pts',(-27.4755714141968,22.8435015405095,27.9398193101068));
#61736=CARTESIAN_POINT('Ctrl Pts',(-27.476881774362,23.5510669492537,27.9041635220347));
#61737=CARTESIAN_POINT('',(-27.4835625131296,23.5535968072644,26.6541635220347));
#61738=CARTESIAN_POINT('Ctrl Pts',(-27.4832524469294,23.5510690854955,27.9041634810362));
#61739=CARTESIAN_POINT('Ctrl Pts',(-27.483226718146,23.674993930109,27.8979287463526));
#61740=CARTESIAN_POINT('Ctrl Pts',(-27.4773396257473,23.798767939476,27.8916940116689));
#61741=CARTESIAN_POINT('Ctrl Pts',(-27.4656591995897,23.9218432003061,27.8854592769853));
#61742=CARTESIAN_POINT('Ctrl Pts',(-27.4539388249783,24.0453393932415,27.8792032187637));
#61743=CARTESIAN_POINT('Ctrl Pts',(-27.4363855054114,24.1681317315402,27.8729471605421));
#61744=CARTESIAN_POINT('Ctrl Pts',(-27.4131189223168,24.289679504558,27.8666911023205));
#61745=CARTESIAN_POINT('Ctrl Pts',(-27.3898124520038,24.4114356537924,27.8604243189847));
#61746=CARTESIAN_POINT('Ctrl Pts',(-27.3607732399586,24.5319426631247,27.854157535649));
#61747=CARTESIAN_POINT('Ctrl Pts',(-27.3261710053763,24.6506745780502,27.8478907523132));
#61748=CARTESIAN_POINT('Ctrl Pts',(-27.2914641228452,24.7697655753152,27.8416050162702));
#61749=CARTESIAN_POINT('Ctrl Pts',(-27.2511606637123,24.8870704295725,27.8353192802272));
#61750=CARTESIAN_POINT('Ctrl Pts',(-27.2054795296194,25.0020805496216,27.8290335441842));
#61751=CARTESIAN_POINT('Ctrl Pts',(-27.1648072009441,25.1044801396603,27.8234370210816));
#61752=CARTESIAN_POINT('Ctrl Pts',(-27.1198725839544,25.2050608095957,27.8178404979789));
#61753=CARTESIAN_POINT('Ctrl Pts',(-27.0708602533607,25.3034810593374,27.8122439748763));
#61754=CARTESIAN_POINT('Ctrl Pts',(-27.0194322238423,25.4067522045293,27.8063716127209));
#61755=CARTESIAN_POINT('Ctrl Pts',(-26.9633702720088,25.5079315737953,27.8004992505656));
#61756=CARTESIAN_POINT('Ctrl Pts',(-26.9028678598677,25.6065743599341,27.7946268884102));
#61757=CARTESIAN_POINT('Ctrl Pts',(-26.8424438475145,25.7050893235079,27.7887621357357));
#61758=CARTESIAN_POINT('Ctrl Pts',(-26.7775910316421,25.8010738913747,27.7828973830612));
#61759=CARTESIAN_POINT('Ctrl Pts',(-26.7085498266344,25.894105598073,27.7770326303867));
#61760=CARTESIAN_POINT('Ctrl Pts',(-26.6395796198831,25.9870416359751,27.771173908708));
#61761=CARTESIAN_POINT('Ctrl Pts',(-26.5664298359389,26.0770305226398,27.7653151870293));
#61762=CARTESIAN_POINT('Ctrl Pts',(-26.4893851003473,26.1636772472509,27.7594564653505));
#61763=CARTESIAN_POINT('Ctrl Pts',(-26.4093321581784,26.2537070874619,27.7533689902735));
#61764=CARTESIAN_POINT('Ctrl Pts',(-26.3250741477172,26.3401280706287,27.7472815151964));
#61765=CARTESIAN_POINT('Ctrl Pts',(-26.2369779545704,26.4225330719741,27.7411940401194));
#61766=CARTESIAN_POINT('Ctrl Pts',(-26.1522904003884,26.5017496393084,27.7353421030832));
#61767=CARTESIAN_POINT('Ctrl Pts',(-26.0640564887503,26.5772549144733,27.7294901660471));
#61768=CARTESIAN_POINT('Ctrl Pts',(-25.9726403486848,26.6487241329995,27.7236382290109));
#61769=CARTESIAN_POINT('Ctrl Pts',(-25.8812381248608,26.7201824717959,27.7177871828128));
#61770=CARTESIAN_POINT('Ctrl Pts',(-25.7866549613817,26.787605721061,27.7119361366146));
#61771=CARTESIAN_POINT('Ctrl Pts',(-25.6892876858399,26.8507097135599,27.7060850904164));
#61772=CARTESIAN_POINT('Ctrl Pts',(-25.5919116546241,26.9138193806346,27.7002335180676));
#61773=CARTESIAN_POINT('Ctrl Pts',(-25.4917513605651,26.9726087939943,27.6943819457188));
#61774=CARTESIAN_POINT('Ctrl Pts',(-25.3892315831579,27.026837788563,27.68853037337));
#61775=CARTESIAN_POINT('Ctrl Pts',(-25.2866777612029,27.08108479138,27.6826768578436));
#61776=CARTESIAN_POINT('Ctrl Pts',(-25.1817632631024,27.1307681709063,27.6768233423172));
#61777=CARTESIAN_POINT('Ctrl Pts',(-25.0749357138907,27.1756946004532,27.6709698267908));
#61778=CARTESIAN_POINT('Ctrl Pts',(-24.967986685618,27.2206721181371,27.6651096549331));
#61779=CARTESIAN_POINT('Ctrl Pts',(-24.8591206454175,27.2608817285548,27.6592494830753));
#61780=CARTESIAN_POINT('Ctrl Pts',(-24.7488034557539,27.2961789434695,27.6533893112175));
#61781=CARTESIAN_POINT('Ctrl Pts',(-24.6384119770577,27.3314999279885,27.6475251930436));
#61782=CARTESIAN_POINT('Ctrl Pts',(-24.5265678009756,27.3619018218082,27.6416610748698));
#61783=CARTESIAN_POINT('Ctrl Pts',(-24.4137484405707,27.3872909489313,27.6357969566959));
#61784=CARTESIAN_POINT('Ctrl Pts',(-24.3007628216028,27.4127174912621,27.6299241967441));
#61785=CARTESIAN_POINT('Ctrl Pts',(-24.1867995555143,27.4331164509735,27.6240514367923));
#61786=CARTESIAN_POINT('Ctrl Pts',(-24.0723428370296,27.4484457943577,27.6181786768405));
#61787=CARTESIAN_POINT('Ctrl Pts',(-24.0410193454553,27.4526409920244,27.6165714723941));
#61788=CARTESIAN_POINT('Ctrl Pts',(-24.0096589026459,27.4564567976675,27.6149642679477));
#61789=CARTESIAN_POINT('Ctrl Pts',(-23.9782714292153,27.4598930296639,27.6133570635013));
#61790=CARTESIAN_POINT('Ctrl Pts',(-23.8635896720581,27.47244813781,27.6074847517197));
#61791=CARTESIAN_POINT('Ctrl Pts',(-23.7481629177312,27.4799740475433,27.601612439938));
#61792=CARTESIAN_POINT('Ctrl Pts',(-23.6324699563696,27.4823930804386,27.5957401281563));
#61793=CARTESIAN_POINT('Ctrl Pts',(-23.5169269156114,27.4848089786326,27.5898754260038));
#61794=CARTESIAN_POINT('Ctrl Pts',(-23.4011187633041,27.4821311517403,27.5840107238512));
#61795=CARTESIAN_POINT('Ctrl Pts',(-23.2855308734857,27.4743334997268,27.5781460216987));
#61796=CARTESIAN_POINT('Ctrl Pts',(-23.170061850753,27.4665438665825,27.5722873506282));
#61797=CARTESIAN_POINT('Ctrl Pts',(-23.0548130499301,27.4536449084763,27.5664286795578));
#61798=CARTESIAN_POINT('Ctrl Pts',(-22.9402706455418,27.4356625613521,27.5605700084873));
#61799=CARTESIAN_POINT('Ctrl Pts',(-22.8212545422657,27.416977875153,27.5544825144723));
#61800=CARTESIAN_POINT('Ctrl Pts',(-22.7030015944435,27.3928046108824,27.5483950204572));
#61801=CARTESIAN_POINT('Ctrl Pts',(-22.5860526519863,27.3632313661452,27.5423075264422));
#61802=CARTESIAN_POINT('Ctrl Pts',(-22.473630045844,27.3348027102241,27.5364556399038));
#61803=CARTESIAN_POINT('Ctrl Pts',(-22.3624128206967,27.3013844096332,27.5306037533654));
#61804=CARTESIAN_POINT('Ctrl Pts',(-22.2528710272477,27.2631072597869,27.524751866827));
#61805=CARTESIAN_POINT('Ctrl Pts',(-22.1433459070482,27.2248359360682,27.5189008709985));
#61806=CARTESIAN_POINT('Ctrl Pts',(-22.0354961016288,27.1817073699025,27.5130498751701));
#61807=CARTESIAN_POINT('Ctrl Pts',(-21.9297751816476,27.1339018111279,27.5071988793416));
#61808=CARTESIAN_POINT('Ctrl Pts',(-21.8240447514147,27.0860919519471,27.5013473571798));
#61809=CARTESIAN_POINT('Ctrl Pts',(-21.7204439640015,27.033604434127,27.495495835018));
#61810=CARTESIAN_POINT('Ctrl Pts',(-21.6194044795231,26.9766668089565,27.4896443128562));
#61811=CARTESIAN_POINT('Ctrl Pts',(-21.5183314376796,26.9197102735879,27.4837908472793));
#61812=CARTESIAN_POINT('Ctrl Pts',(-21.4198217502063,26.8583008948426,27.4779373817024));
#61813=CARTESIAN_POINT('Ctrl Pts',(-21.3242800202089,26.792710762437,27.4720839161254));
#61814=CARTESIAN_POINT('Ctrl Pts',(-21.2286296339778,26.7270460366914,27.4662237936089));
#61815=CARTESIAN_POINT('Ctrl Pts',(-21.1359542833283,26.6571913013016,27.4603636710924));
#61816=CARTESIAN_POINT('Ctrl Pts',(-21.0466273407646,26.5834603886243,27.4545035485759));
#61817=CARTESIAN_POINT('Ctrl Pts',(-20.957240239299,26.5096798204835,27.4486394794501));
#61818=CARTESIAN_POINT('Ctrl Pts',(-20.8712063422712,26.4320181533777,27.4427754103244));
#61819=CARTESIAN_POINT('Ctrl Pts',(-20.7888625704094,26.3508264874604,27.4369113411986));
#61820=CARTESIAN_POINT('Ctrl Pts',(-20.7063974385128,26.2695151595069,27.4310386294808));
#61821=CARTESIAN_POINT('Ctrl Pts',(-20.6276335663296,26.1846637512108,27.4251659177629));
#61822=CARTESIAN_POINT('Ctrl Pts',(-20.5528680385805,26.0966568987265,27.4192932060451));
#61823=CARTESIAN_POINT('Ctrl Pts',(-20.5324005958888,26.0725645761826,27.4176855214055));
#61824=CARTESIAN_POINT('Ctrl Pts',(-20.512232546352,26.0482359470459,27.416077836766));
#61825=CARTESIAN_POINT('Ctrl Pts',(-20.4923694101848,26.0236792670531,27.4144701521264));
#61826=CARTESIAN_POINT('Ctrl Pts',(-20.4198168088736,25.9339829070196,27.4085978819217));
#61827=CARTESIAN_POINT('Ctrl Pts',(-20.3510925689731,25.8409413013264,27.402725611717));
#61828=CARTESIAN_POINT('Ctrl Pts',(-20.2865208506764,25.7449152653097,27.3968533415123));
#61829=CARTESIAN_POINT('Ctrl Pts',(-20.2220328168015,25.6490136782547,27.390988681722));
#61830=CARTESIAN_POINT('Ctrl Pts',(-20.16168683094,25.5501356924103,27.3851240219316));
#61831=CARTESIAN_POINT('Ctrl Pts',(-20.1057672190686,25.4486755433296,27.3792593621413));
#61832=CARTESIAN_POINT('Ctrl Pts',(-20.0499051206154,25.3473197461889,27.3734007341638));
#61833=CARTESIAN_POINT('Ctrl Pts',(-19.9984605392699,25.2433874281164,27.3675421061864));
#61834=CARTESIAN_POINT('Ctrl Pts',(-19.9516744554885,25.1373016265402,27.3616834782089));
#61835=CARTESIAN_POINT('Ctrl Pts',(-19.9030605566341,25.0270713184896,27.3555959683148));
#61836=CARTESIAN_POINT('Ctrl Pts',(-19.8594768223093,24.9145162110629,27.3495084584207));
#61837=CARTESIAN_POINT('Ctrl Pts',(-19.8211410761401,24.800139227381,27.3434209485267));
#61838=CARTESIAN_POINT('Ctrl Pts',(-19.784289435815,24.6901901619447,27.3375691066426));
#61839=CARTESIAN_POINT('Ctrl Pts',(-19.7522871494092,24.5785580873333,27.3317172647585));
#61840=CARTESIAN_POINT('Ctrl Pts',(-19.7252782618679,24.4657091582838,27.3258654228744));
#61841=CARTESIAN_POINT('Ctrl Pts',(-19.698273487673,24.3528774156784,27.3200144722026));
#61842=CARTESIAN_POINT('Ctrl Pts',(-19.6762606964705,24.2388295890369,27.3141635215308));
#61843=CARTESIAN_POINT('Ctrl Pts',(-19.6593334183605,24.1240447009457,27.308312570859));
#61844=CARTESIAN_POINT('Ctrl Pts',(-19.6424046188457,24.0092494961179,27.3024610943104));
#61845=CARTESIAN_POINT('Ctrl Pts',(-19.6305623013696,23.8937175071375,27.2966096177617));
#61846=CARTESIAN_POINT('Ctrl Pts',(-19.6238483570215,23.7779348918206,27.2907581412131));
#61847=CARTESIAN_POINT('Ctrl Pts',(-19.6171321832835,23.6621138304607,27.2849047216601));
#61848=CARTESIAN_POINT('Ctrl Pts',(-19.6155477926907,23.5460423897593,27.2790513021072));
#61849=CARTESIAN_POINT('Ctrl Pts',(-19.6190849799541,23.4302080393346,27.2731978825542));
#61850=CARTESIAN_POINT('Ctrl Pts',(-19.6226261897369,23.3142419611053,27.267337806443));
#61851=CARTESIAN_POINT('Ctrl Pts',(-19.6313005898805,23.1985139247478,27.2614777303317));
#61852=CARTESIAN_POINT('Ctrl Pts',(-19.6450459748211,23.083507689028,27.2556176542204));
#61853=CARTESIAN_POINT('Ctrl Pts',(-19.6588006162657,22.9684240050817,27.2497536317797));
#61854=CARTESIAN_POINT('Ctrl Pts',(-19.6776329753126,22.8540634965506,27.2438896093389));
#61855=CARTESIAN_POINT('Ctrl Pts',(-19.7014297885899,22.7408993997651,27.2380255868981));
#61856=CARTESIAN_POINT('Ctrl Pts',(-19.7252616741966,22.6275685189475,27.2321529219167));
#61857=CARTESIAN_POINT('Ctrl Pts',(-19.754072514336,22.5154379679629,27.2262802569353));
#61858=CARTESIAN_POINT('Ctrl Pts',(-19.7876992981181,22.4049655962468,27.2204075919539));
#61859=CARTESIAN_POINT('Ctrl Pts',(-19.7969073501856,22.374714848588,27.2187994748864));
#61860=CARTESIAN_POINT('Ctrl Pts',(-19.8064762409999,22.3445883171907,27.217191357819));
#61861=CARTESIAN_POINT('Ctrl Pts',(-19.8164020055153,22.3145951163264,27.2155832407515));
#61862=CARTESIAN_POINT('Ctrl Pts',(-19.8526475929278,22.2050699324456,27.2097109326137));
#61863=CARTESIAN_POINT('Ctrl Pts',(-19.8937770450568,22.0969574122162,27.2038386244759));
#61864=CARTESIAN_POINT('Ctrl Pts',(-19.9396620167432,21.9907253170083,27.1979663163381));
#61865=CARTESIAN_POINT('Ctrl Pts',(-19.9854875261016,21.884630887957,27.1921016181236));
#61866=CARTESIAN_POINT('Ctrl Pts',(-20.0360561372611,21.7804124139129,27.186236919909));
#61867=CARTESIAN_POINT('Ctrl Pts',(-20.0911898562017,21.6785222073647,27.1803722216945));
#61868=CARTESIAN_POINT('Ctrl Pts',(-20.1462668745483,21.5767367866961,27.1745135548502));
#61869=CARTESIAN_POINT('Ctrl Pts',(-20.2058994668376,21.4772752322489,27.1686548880059));
#61870=CARTESIAN_POINT('Ctrl Pts',(-20.2698619777202,21.3805689572073,27.1627962211616));
#61871=CARTESIAN_POINT('Ctrl Pts',(-20.3363227454924,21.2800855146568,27.1567087256706));
#61872=CARTESIAN_POINT('Ctrl Pts',(-20.4074583835905,21.1825773885528,27.1506212301795));
#61873=CARTESIAN_POINT('Ctrl Pts',(-20.4829635182502,21.0884996789477,27.1445337346885));
#61874=CARTESIAN_POINT('Ctrl Pts',(-20.5555462593645,20.9980632063597,27.1386818530747));
#61875=CARTESIAN_POINT('Ctrl Pts',(-20.6321662640687,20.910796894421,27.1328299714609));
#61876=CARTESIAN_POINT('Ctrl Pts',(-20.7125092049126,20.8270739089618,27.1269780898471));
#61877=CARTESIAN_POINT('Ctrl Pts',(-20.7928399133843,20.7433636704933,27.121127099194));
#61878=CARTESIAN_POINT('Ctrl Pts',(-20.876892144824,20.6631959840297,27.1152761085408));
#61879=CARTESIAN_POINT('Ctrl Pts',(-20.9643134406852,20.5869084717525,27.1094251178876));
#61880=CARTESIAN_POINT('Ctrl Pts',(-21.0517425969594,20.5106141001473,27.1035736011474));
#61881=CARTESIAN_POINT('Ctrl Pts',(-21.1425411083622,20.4382008680885,27.0977220844073));
#61882=CARTESIAN_POINT('Ctrl Pts',(-21.2363226005084,20.3699668096933,27.0918705676671));
#61883=CARTESIAN_POINT('Ctrl Pts',(-21.3301352356322,20.3017100921177,27.0860171077541));
#61884=CARTESIAN_POINT('Ctrl Pts',(-21.4269324871336,20.2376355508792,27.080163647841));
#61885=CARTESIAN_POINT('Ctrl Pts',(-21.5262987168613,20.1779980995044,27.074310187928));
#61886=CARTESIAN_POINT('Ctrl Pts',(-21.6257779467384,20.1182928278961,27.0684500714089));
#61887=CARTESIAN_POINT('Ctrl Pts',(-21.7278316313432,20.0630349304664,27.0625899548898));
#61888=CARTESIAN_POINT('Ctrl Pts',(-21.8320191463023,20.0124335660991,27.0567298383707));
#61889=CARTESIAN_POINT('Ctrl Pts',(-21.9362768247783,19.961798125003,27.0508657754442));
#61890=CARTESIAN_POINT('Ctrl Pts',(-22.0426708164094,19.915825624682,27.0450017125176));
#61891=CARTESIAN_POINT('Ctrl Pts',(-22.1507417506603,19.8746765803949,27.0391376495911));
#61892=CARTESIAN_POINT('Ctrl Pts',(-22.2589719577502,19.8334668914474,27.0332649443228));
#61893=CARTESIAN_POINT('Ctrl Pts',(-22.3688836490108,19.7970949755413,27.0273922390545));
#61894=CARTESIAN_POINT('Ctrl Pts',(-22.4800035085378,19.7656711772465,27.0215195337862));
#61895=CARTESIAN_POINT('Ctrl Pts',(-22.5104241166434,19.7570684751087,27.019911798983));
#61896=CARTESIAN_POINT('Ctrl Pts',(-22.540935223925,19.7488363205333,27.0183040641798));
#61897=CARTESIAN_POINT('Ctrl Pts',(-22.5715270262102,19.7409763032073,27.0166963293766));
#61898=CARTESIAN_POINT('Ctrl Pts',(-22.6832644728893,19.7122673615547,27.0108240312959));
#61899=CARTESIAN_POINT('Ctrl Pts',(-22.7964533581284,19.6884308827569,27.0049517332151));
#61900=CARTESIAN_POINT('Ctrl Pts',(-22.9106307722246,19.6696117334738,26.9990794351344));
#61901=CARTESIAN_POINT('Ctrl Pts',(-23.0246602223877,19.6508169721606,26.9932147470379));
#61902=CARTESIAN_POINT('Ctrl Pts',(-23.1396752497509,19.6370266767862,26.9873500589414));
#61903=CARTESIAN_POINT('Ctrl Pts',(-23.2551991045552,19.6283355928576,26.9814853708449));
#61904=CARTESIAN_POINT('Ctrl Pts',(-23.3706041512106,19.6196534470968,26.975626714167));
#61905=CARTESIAN_POINT('Ctrl Pts',(-23.4865165747105,19.6160601126637,26.9697680574892));
#61906=CARTESIAN_POINT('Ctrl Pts',(-23.602451445135,19.6175989398512,26.9639094008114));
#61907=CARTESIAN_POINT('Ctrl Pts',(-23.722914800385,19.6191978745416,26.9578219015276));
#61908=CARTESIAN_POINT('Ctrl Pts',(-23.8434019432624,19.6263381487003,26.9517344022439));
#61909=CARTESIAN_POINT('Ctrl Pts',(-23.9633649206812,19.6390088478942,26.9456469029602));
#61910=CARTESIAN_POINT('Ctrl Pts',(-24.0786845097008,19.6511891042956,26.939795031569));
#61911=CARTESIAN_POINT('Ctrl Pts',(-24.1935193069066,19.6684795683318,26.9339431601778));
#61912=CARTESIAN_POINT('Ctrl Pts',(-24.3073854556428,19.6908175036787,26.9280912887866));
#61913=CARTESIAN_POINT('Ctrl Pts',(-24.4212342679388,19.7131520380124,26.9222403083593));
#61914=CARTESIAN_POINT('Ctrl Pts',(-24.5341143194623,19.7405324360917,26.9163893279319));
#61915=CARTESIAN_POINT('Ctrl Pts',(-24.645551045502,19.7728446684035,26.9105383475045));
#61916=CARTESIAN_POINT('Ctrl Pts',(-24.7569977914472,19.8051598060906,26.9046868409825));
#61917=CARTESIAN_POINT('Ctrl Pts',(-24.8670005568701,19.8424075444164,26.8988353344604));
#61918=CARTESIAN_POINT('Ctrl Pts',(-24.9750997501867,19.8844239208677,26.8929838279384));
#61919=CARTESIAN_POINT('Ctrl Pts',(-25.0832348415141,19.9264542502847,26.8871303782247));
#61920=CARTESIAN_POINT('Ctrl Pts',(-25.1894647186556,19.973256217012,26.881276928511));
#61921=CARTESIAN_POINT('Ctrl Pts',(-25.2933502497918,20.0246179299291,26.8754234787974));
#61922=CARTESIAN_POINT('Ctrl Pts',(-25.3973539220852,20.0760380526377,26.8695633723981));
#61923=CARTESIAN_POINT('Ctrl Pts',(-25.4990075562372,20.1320280882276,26.8637032659988));
#61924=CARTESIAN_POINT('Ctrl Pts',(-25.5978970084691,20.1923303919278,26.8578431595995));
#61925=CARTESIAN_POINT('Ctrl Pts',(-25.6968530570032,20.252673305727,26.8519791067589));
#61926=CARTESIAN_POINT('Ctrl Pts',(-25.7930408747363,20.3173340401402,26.8461150539183));
#61927=CARTESIAN_POINT('Ctrl Pts',(-25.8860771095247,20.3860128850171,26.8402510010777));
#61928=CARTESIAN_POINT('Ctrl Pts',(-25.9792504615759,20.4547929491152,26.8343783057671));
#61929=CARTESIAN_POINT('Ctrl Pts',(-26.069262640328,20.527602683669,26.8285056104564));
#61930=CARTESIAN_POINT('Ctrl Pts',(-26.1557649650478,20.604103526698,26.8226329151457));
#61931=CARTESIAN_POINT('Ctrl Pts',(-26.1794476578128,20.6250480038273,26.8210250827644));
#61932=CARTESIAN_POINT('Ctrl Pts',(-26.2028674896014,20.6462689497625,26.8194172503831));
#61933=CARTESIAN_POINT('Ctrl Pts',(-26.2260178222051,20.667758974009,26.8178094180017));
#61934=CARTESIAN_POINT('Ctrl Pts',(-26.3093104344281,20.7450779606023,26.8120245957553));
#61935=CARTESIAN_POINT('Ctrl Pts',(-26.3894084840011,20.8261585613254,26.8062397735089));
#61936=CARTESIAN_POINT('Ctrl Pts',(-26.4659450914145,20.9107022106752,26.8004549512625));
#61937=CARTESIAN_POINT('Ctrl Pts',(-26.5423814324424,20.9951351040557,26.7946777073925));
#61938=CARTESIAN_POINT('Ctrl Pts',(-26.6152653205548,21.0830217161674,26.7889004635225));
#61939=CARTESIAN_POINT('Ctrl Pts',(-26.684264064457,21.1740242782409,26.7831232196525));
#61940=CARTESIAN_POINT('Ctrl Pts',(-26.753183611698,21.2649223877016,26.7773526068949));
#61941=CARTESIAN_POINT('Ctrl Pts',(-26.8182266293002,21.3589289946375,26.7715819941372));
#61942=CARTESIAN_POINT('Ctrl Pts',(-26.8790990269154,21.4556714253025,26.7658113813796));
#61943=CARTESIAN_POINT('Ctrl Pts',(-26.9399328370013,21.5523525301197,26.7600444266624));
#61944=CARTESIAN_POINT('Ctrl Pts',(-26.9966010533202,21.6517656531312,26.7542774719451));
#61945=CARTESIAN_POINT('Ctrl Pts',(-27.0488517711681,21.7535075966651,26.7485105172279));
#61946=CARTESIAN_POINT('Ctrl Pts',(-27.1010828959889,21.8552113889021,26.7427457250092));
#61947=CARTESIAN_POINT('Ctrl Pts',(-27.1488996201686,21.9592418867917,26.7369809327905));
#61948=CARTESIAN_POINT('Ctrl Pts',(-27.1920954923835,22.0651704296952,26.7312161405717));
#61949=CARTESIAN_POINT('Ctrl Pts',(-27.2352863497094,22.1710866746669,26.7254520176252));
#61950=CARTESIAN_POINT('Ctrl Pts',(-27.2738572622042,22.2789001308291,26.7196878946786));
#61951=CARTESIAN_POINT('Ctrl Pts',(-27.3076498760156,22.3881620890493,26.713923771732));
#61952=CARTESIAN_POINT('Ctrl Pts',(-27.3414613438788,22.4974850082429,26.7081564327846));
#61953=CARTESIAN_POINT('Ctrl Pts',(-27.3704890617876,22.6082576355738,26.7023890938372));
#61954=CARTESIAN_POINT('Ctrl Pts',(-27.3946246312222,22.7200163241179,26.6966217548898));
#61955=CARTESIAN_POINT('Ctrl Pts',(-27.4187677948437,22.8318101772093,26.6908526012659));
#61956=CARTESIAN_POINT('Ctrl Pts',(-27.4380156707845,22.9445902890411,26.6850834476421));
#61957=CARTESIAN_POINT('Ctrl Pts',(-27.4523113303205,23.0578846488431,26.6793142940182));
#61958=CARTESIAN_POINT('Ctrl Pts',(-27.4666225286685,23.1713021550973,26.6735388695544));
#61959=CARTESIAN_POINT('Ctrl Pts',(-27.4759707289721,23.2852346002791,26.6677634450905));
#61960=CARTESIAN_POINT('Ctrl Pts',(-27.4803510307389,23.3992068836048,26.6619880206267));
#61961=CARTESIAN_POINT('Ctrl Pts',(-27.4823291632682,23.4506764610639,26.6593798544293));
#61962=CARTESIAN_POINT('Ctrl Pts',(-27.4832948486706,23.5021541814199,26.656771688232));
#61963=CARTESIAN_POINT('Ctrl Pts',(-27.4832511100809,23.5535965424957,26.6541635220347));
#61964=CARTESIAN_POINT('',(-27.4879134860282,23.5478550324797,25.4041635220347));
#61965=CARTESIAN_POINT('Ctrl Pts',(-27.4854593591317,23.5535984200475,26.6541635220347));
#61966=CARTESIAN_POINT('Ctrl Pts',(-27.487557722953,23.7854233941432,26.6424165168988));
#61967=CARTESIAN_POINT('Ctrl Pts',(-27.363218900229,25.3233322387404,26.5643738746377));
#61968=CARTESIAN_POINT('Ctrl Pts',(-25.3358175318097,27.8458907001547,26.420035595252));
#61969=CARTESIAN_POINT('Ctrl Pts',(-20.9014335845632,27.3744530235421,26.221148683877));
#61970=CARTESIAN_POINT('Ctrl Pts',(-18.9010895943725,23.3888991075444,26.0222617725022));
#61971=CARTESIAN_POINT('Ctrl Pts',(-21.1729321979881,19.5516154275727,25.8233748611272));
#61972=CARTESIAN_POINT('Ctrl Pts',(-25.6293306044078,19.3887401543539,25.6244879497525));
#61973=CARTESIAN_POINT('Ctrl Pts',(-27.4180706748919,21.9610852413708,25.4847508367215));
#61974=CARTESIAN_POINT('Ctrl Pts',(-27.4889222638918,23.4070619638991,25.4113093608156));
#61975=CARTESIAN_POINT('Ctrl Pts',(-27.4879134860282,23.5478550324797,25.4041635220347));
#61976=CARTESIAN_POINT('',(-27.4779394483698,23.5480687660733,24.1541635220347));
#61977=CARTESIAN_POINT('Ctrl Pts',(-27.4879134860282,23.5478550324797,25.4041635220347));
#61978=CARTESIAN_POINT('Ctrl Pts',(-27.4795633106279,24.7132719793335,25.3450137236907));
#61979=CARTESIAN_POINT('Ctrl Pts',(-26.3135078915754,27.199410493852,25.2195682882216));
#61980=CARTESIAN_POINT('Ctrl Pts',(-22.0830319381555,27.9647756739205,25.0278272156278));
#61981=CARTESIAN_POINT('Ctrl Pts',(-19.043145214186,24.7020921303425,24.8289403042528));
#61982=CARTESIAN_POINT('Ctrl Pts',(-20.1449079761709,20.3809656581431,24.630053392878));
#61983=CARTESIAN_POINT('Ctrl Pts',(-24.3758936586293,18.9721451101218,24.431166481503));
#61984=CARTESIAN_POINT('Ctrl Pts',(-27.1453541813937,21.2038557842603,24.2725365245553));
#61985=CARTESIAN_POINT('Ctrl Pts',(-27.4805332539196,23.031697457995,24.1802022047326));
#61986=CARTESIAN_POINT('Ctrl Pts',(-27.4779394483698,23.5480687660733,24.1541635220347));
#61987=CARTESIAN_POINT('',(-27.4799050097769,23.5534460090541,22.9041635220347));
#61988=CARTESIAN_POINT('Ctrl Pts',(-27.4779394483698,23.5480687660733,24.1541635220347));
#61989=CARTESIAN_POINT('Ctrl Pts',(-27.4739293103371,24.3464016332941,24.1139065676076));
#61990=CARTESIAN_POINT('Ctrl Pts',(-26.8489074821203,26.4652081631034,24.0073539760553));
#61991=CARTESIAN_POINT('Ctrl Pts',(-23.3829161640313,28.1992039588926,23.8345057473784));
#61992=CARTESIAN_POINT('Ctrl Pts',(-19.5485592941391,25.9224249673682,23.6356188360036));
#61993=CARTESIAN_POINT('Ctrl Pts',(-19.3914192219412,21.4658206345704,23.4367319246284));
#61994=CARTESIAN_POINT('Ctrl Pts',(-23.0558943504829,18.92463248452,23.2378450132538));
#61995=CARTESIAN_POINT('Ctrl Pts',(-26.7322134398013,20.4503798001738,23.0603222123891));
#61996=CARTESIAN_POINT('Ctrl Pts',(-27.4731489910645,22.6635309292851,22.9490950486494));
#61997=CARTESIAN_POINT('Ctrl Pts',(-27.4799050097769,23.5534460090541,22.9041635220347));
#61998=CARTESIAN_POINT('',(-27.4855853468104,23.5511498130059,21.6541638930713));
#61999=CARTESIAN_POINT('Ctrl Pts',(-27.4799050097769,23.5534460090541,22.9041635220347));
#62000=CARTESIAN_POINT('Ctrl Pts',(-27.4831173718143,23.9765841826572,22.8827994115245));
#62001=CARTESIAN_POINT('Ctrl Pts',(-27.2249116382549,25.7089597706867,22.7951396638892));
#62002=CARTESIAN_POINT('Ctrl Pts',(-24.6962908804443,28.0588384447396,22.6411842791291));
#62003=CARTESIAN_POINT('Ctrl Pts',(-20.3765858683961,26.9515156415358,22.4422973677542));
#62004=CARTESIAN_POINT('Ctrl Pts',(-18.9732114373579,22.7187204199441,22.2434104563792));
#62005=CARTESIAN_POINT('Ctrl Pts',(-21.7757497029281,19.250032706754,22.0445235450043));
#62006=CARTESIAN_POINT('Ctrl Pts',(-26.153814110843,19.7268819672536,21.8481082315933));
#62007=CARTESIAN_POINT('Ctrl Pts',(-27.4855970698216,22.2949686608996,21.717988555307));
#62008=CARTESIAN_POINT('Ctrl Pts',(-27.4895029709821,23.5511384503243,21.6541645161457));
#62009=CARTESIAN_POINT('',(-27.483250851415,23.5466170023887,20.4041635408089));
#62010=CARTESIAN_POINT('Ctrl Pts',(-27.483252427791,23.5511565794069,21.6541635220347));
#62011=CARTESIAN_POINT('Ctrl Pts',(-27.4832412653015,23.5997182533086,21.6516922554413));
#62012=CARTESIAN_POINT('Ctrl Pts',(-27.4823307347554,23.6482685215949,21.649220988848));
#62013=CARTESIAN_POINT('Ctrl Pts',(-27.4805218875495,23.6967850892526,21.6467497222546));
#62014=CARTESIAN_POINT('Ctrl Pts',(-27.4762236511744,23.8120715961606,21.6408774252859));
#62015=CARTESIAN_POINT('Ctrl Pts',(-27.4668413684358,23.9273619587229,21.6350051283172));
#62016=CARTESIAN_POINT('Ctrl Pts',(-27.4523679891428,24.0421711801925,21.6291328313485));
#62017=CARTESIAN_POINT('Ctrl Pts',(-27.4379133662,24.1568316180291,21.6232681444103));
#62018=CARTESIAN_POINT('Ctrl Pts',(-27.4183808183005,24.2710117483807,21.6174034574721));
#62019=CARTESIAN_POINT('Ctrl Pts',(-27.3938152824245,24.3842275800012,21.6115387705339));
#62020=CARTESIAN_POINT('Ctrl Pts',(-27.3692750106643,24.497326976226,21.605680115059));
#62021=CARTESIAN_POINT('Ctrl Pts',(-27.3397121336118,24.6094636447498,21.5998214595842));
#62022=CARTESIAN_POINT('Ctrl Pts',(-27.3052231850132,24.7201603881996,21.5939628041094));
#62023=CARTESIAN_POINT('Ctrl Pts',(-27.2693870677048,24.8351810439491,21.5878753043915));
#62024=CARTESIAN_POINT('Ctrl Pts',(-27.2282322570843,24.9486465408119,21.5817878046736));
#62025=CARTESIAN_POINT('Ctrl Pts',(-27.1819252516888,25.0600347195765,21.5757003049557));
#62026=CARTESIAN_POINT('Ctrl Pts',(-27.1374106575068,25.1671113817798,21.5698484348723));
#62027=CARTESIAN_POINT('Ctrl Pts',(-27.0881354790138,25.2722681324039,21.5639965647889));
#62028=CARTESIAN_POINT('Ctrl Pts',(-27.0342976388113,25.3750590122759,21.5581446947055));
#62029=CARTESIAN_POINT('Ctrl Pts',(-26.9804679959096,25.4778342413019,21.5522937156225));
#62030=CARTESIAN_POINT('Ctrl Pts',(-26.9220772643436,25.5782439497247,21.5464427365396));
#62031=CARTESIAN_POINT('Ctrl Pts',(-26.8593698902985,25.6758656919339,21.5405917574566));
#62032=CARTESIAN_POINT('Ctrl Pts',(-26.7966568782568,25.7734962112773,21.5347402523143));
#62033=CARTESIAN_POINT('Ctrl Pts',(-26.7296266756421,25.8683379182785,21.528888747172));
#62034=CARTESIAN_POINT('Ctrl Pts',(-26.6585673305653,25.9599969395348,21.5230372420297));
#62035=CARTESIAN_POINT('Ctrl Pts',(-26.5874843882269,26.0516863987566,21.5171837937299));
#62036=CARTESIAN_POINT('Ctrl Pts',(-26.5123698960616,26.1401907441226,21.5113303454302));
#62037=CARTESIAN_POINT('Ctrl Pts',(-26.4335520203143,26.2251493631483,21.5054768971304));
#62038=CARTESIAN_POINT('Ctrl Pts',(-26.3546445115273,26.3102045985721,21.4996167921889));
#62039=CARTESIAN_POINT('Ctrl Pts',(-26.2720254943442,26.3917057561524,21.4937566872473));
#62040=CARTESIAN_POINT('Ctrl Pts',(-26.1860598787519,26.4693292057808,21.4878965823058));
#62041=CARTESIAN_POINT('Ctrl Pts',(-26.1000363706979,26.5470049299443,21.4820325309503));
#62042=CARTESIAN_POINT('Ctrl Pts',(-26.0106620946121,26.6207974838015,21.4761684795949));
#62043=CARTESIAN_POINT('Ctrl Pts',(-25.9183335160132,26.6904247326581,21.4703044282395));
#62044=CARTESIAN_POINT('Ctrl Pts',(-25.8258688635199,26.7601545981808,21.4644317344429));
#62045=CARTESIAN_POINT('Ctrl Pts',(-25.7304415581211,26.8257066736033,21.4585590406463));
#62046=CARTESIAN_POINT('Ctrl Pts',(-25.6324754355502,26.8868431236994,21.4526863468497));
#62047=CARTESIAN_POINT('Ctrl Pts',(-25.6056539499634,26.9035812610477,21.4510785015264));
#62048=CARTESIAN_POINT('Ctrl Pts',(-25.5786422915133,26.9199886871719,21.4494706562031));
#62049=CARTESIAN_POINT('Ctrl Pts',(-25.5514494352447,26.9360611431222,21.4478628108797));
#62050=CARTESIAN_POINT('Ctrl Pts',(-25.4521335837017,26.9947622090686,21.441990513911));
#62051=CARTESIAN_POINT('Ctrl Pts',(-25.3500663457444,27.0491880656526,21.4361182169423));
#62052=CARTESIAN_POINT('Ctrl Pts',(-25.2456519463466,27.0990706201282,21.4302459199736));
#62053=CARTESIAN_POINT('Ctrl Pts',(-25.141372859718,27.1488885307748,21.4243812330354));
#62054=CARTESIAN_POINT('Ctrl Pts',(-25.0347530301277,27.1941746713993,21.4185165460972));
#62055=CARTESIAN_POINT('Ctrl Pts',(-24.9262239378743,27.2347052304508,21.412651859159));
#62056=CARTESIAN_POINT('Ctrl Pts',(-24.8178064609984,27.2751941063595,21.4067932036842));
#62057=CARTESIAN_POINT('Ctrl Pts',(-24.7074840120062,27.3109369850299,21.4009345482094));
#62058=CARTESIAN_POINT('Ctrl Pts',(-24.5957102456366,27.3417571365125,21.3950758927345));
#62059=CARTESIAN_POINT('Ctrl Pts',(-24.4795704975035,27.3737811502581,21.3889883930166));
#62060=CARTESIAN_POINT('Ctrl Pts',(-24.3618641514241,27.4004898287756,21.3829008932987));
#62061=CARTESIAN_POINT('Ctrl Pts',(-24.2431205082215,27.4217410008883,21.3768133935808));
#62062=CARTESIAN_POINT('Ctrl Pts',(-24.1289730904882,27.4421696011489,21.3709615234974));
#62063=CARTESIAN_POINT('Ctrl Pts',(-24.0138676289437,27.457555248355,21.365109653414));
#62064=CARTESIAN_POINT('Ctrl Pts',(-23.8982863020791,27.4678233982736,21.3592577833306));
#62065=CARTESIAN_POINT('Ctrl Pts',(-23.7827225735224,27.478089984773,21.3534068042477));
#62066=CARTESIAN_POINT('Ctrl Pts',(-23.6666835353571,27.4832405866847,21.3475558251647));
#62067=CARTESIAN_POINT('Ctrl Pts',(-23.5506567316891,27.4832525109241,21.3417048460817));
#62068=CARTESIAN_POINT('Ctrl Pts',(-23.4346194960948,27.4832644362356,21.3358533409394));
#62069=CARTESIAN_POINT('Ctrl Pts',(-23.3185949105921,27.4781367653861,21.3300018357971));
#62070=CARTESIAN_POINT('Ctrl Pts',(-23.2030700496983,27.4678989328125,21.3241503306548));
#62071=CARTESIAN_POINT('Ctrl Pts',(-23.087506825513,27.4576577004775,21.3182968823551));
#62072=CARTESIAN_POINT('Ctrl Pts',(-22.9724440674643,27.4423029685653,21.3124434340553));
#62073=CARTESIAN_POINT('Ctrl Pts',(-22.8583625526531,27.4219159025082,21.3065899857555));
#62074=CARTESIAN_POINT('Ctrl Pts',(-22.7441513023872,27.40150565193,21.300729880814));
#62075=CARTESIAN_POINT('Ctrl Pts',(-22.6309239298121,27.376051717323,21.2948697758725));
#62076=CARTESIAN_POINT('Ctrl Pts',(-22.5191499596855,27.3456861677886,21.2890096709309));
#62077=CARTESIAN_POINT('Ctrl Pts',(-22.4073007167856,27.3153001689572,21.2831456195755));
#62078=CARTESIAN_POINT('Ctrl Pts',(-22.2969072180469,27.2799960945907,21.27728156822));
#62079=CARTESIAN_POINT('Ctrl Pts',(-22.1884211345414,27.2399549920193,21.2714175168646));
#62080=CARTESIAN_POINT('Ctrl Pts',(-22.0797751642049,27.1998548768557,21.265544823068));
#62081=CARTESIAN_POINT('Ctrl Pts',(-21.9730425992842,27.1550039594364,21.2596721292714));
#62082=CARTESIAN_POINT('Ctrl Pts',(-21.8686526357277,27.1056302598527,21.2537994354748));
#62083=CARTESIAN_POINT('Ctrl Pts',(-21.8400724099367,27.0921125668278,21.2521915901515));
#62084=CARTESIAN_POINT('Ctrl Pts',(-21.8116676205528,27.0782561147456,21.2505837448282));
#62085=CARTESIAN_POINT('Ctrl Pts',(-21.783446702094,27.0640661523193,21.2489758995048));
#62086=CARTESIAN_POINT('Ctrl Pts',(-21.6803760823553,27.0122404747291,21.2431036025361));
#62087=CARTESIAN_POINT('Ctrl Pts',(-21.5794150269874,26.9557890776857,21.2372313055674));
#62088=CARTESIAN_POINT('Ctrl Pts',(-21.4810075876501,26.8949071269474,21.2313590085987));
#62089=CARTESIAN_POINT('Ctrl Pts',(-21.3827276765389,26.834104074382,21.2254943216605));
#62090=CARTESIAN_POINT('Ctrl Pts',(-21.2869951487804,26.7688821016771,21.2196296347223));
#62091=CARTESIAN_POINT('Ctrl Pts',(-21.1942315341809,26.6994832408161,21.2137649477841));
#62092=CARTESIAN_POINT('Ctrl Pts',(-21.1015633211519,26.630155752339,21.2079062923092));
#62093=CARTESIAN_POINT('Ctrl Pts',(-21.0118582770428,26.5566601661541,21.2020476368344));
#62094=CARTESIAN_POINT('Ctrl Pts',(-20.9255103073432,26.4792826195747,21.1961889813596));
#62095=CARTESIAN_POINT('Ctrl Pts',(-20.835789509893,26.3988826378727,21.1901014816417));
#62096=CARTESIAN_POINT('Ctrl Pts',(-20.7496937805493,26.31429148701,21.1840139819238));
#62097=CARTESIAN_POINT('Ctrl Pts',(-20.6676288398422,26.2258776271016,21.1779264822059));
#62098=CARTESIAN_POINT('Ctrl Pts',(-20.5887403973494,26.1408860138395,21.1720746121225));
#62099=CARTESIAN_POINT('Ctrl Pts',(-20.513576812579,26.0523624523329,21.1662227420391));
#62100=CARTESIAN_POINT('Ctrl Pts',(-20.4424614387603,25.9606723131183,21.1603708719557));
#62101=CARTESIAN_POINT('Ctrl Pts',(-20.3713568929038,25.868996134561,21.1545198928727));
#62102=CARTESIAN_POINT('Ctrl Pts',(-20.3042995857251,25.7741546635035,21.1486689137897));
#62103=CARTESIAN_POINT('Ctrl Pts',(-20.2415721475544,25.676545812408,21.1428179347067));
#62104=CARTESIAN_POINT('Ctrl Pts',(-20.1788390695834,25.5789281853374,21.1369664295644));
#62105=CARTESIAN_POINT('Ctrl Pts',(-20.1204368580069,25.4785430313931,21.1311149244221));
#62106=CARTESIAN_POINT('Ctrl Pts',(-20.0666040335643,25.3758160450997,21.1252634192798));
#62107=CARTESIAN_POINT('Ctrl Pts',(-20.0127533324127,25.2730549454104,21.11940997098));
#62108=CARTESIAN_POINT('Ctrl Pts',(-19.963475227414,25.1679508329805,21.1135565226803));
#62109=CARTESIAN_POINT('Ctrl Pts',(-19.9189613131329,25.0609520670088,21.1077030743805));
#62110=CARTESIAN_POINT('Ctrl Pts',(-19.8743967768653,24.9538316202058,21.1018429694389));
#62111=CARTESIAN_POINT('Ctrl Pts',(-19.8346074041967,24.8448126011775,21.0959828644974));
#62112=CARTESIAN_POINT('Ctrl Pts',(-19.7997358812123,24.7343614179281,21.0901227595558));
#62113=CARTESIAN_POINT('Ctrl Pts',(-19.7648408744397,24.6238358527198,21.0842587082004));
#62114=CARTESIAN_POINT('Ctrl Pts',(-19.734870418564,24.5118766011805,21.0783946568449));
#62115=CARTESIAN_POINT('Ctrl Pts',(-19.7099163427907,24.3989615255183,21.0725306054895));
#62116=CARTESIAN_POINT('Ctrl Pts',(-19.684925489691,24.2858800355745,21.0666579116929));
#62117=CARTESIAN_POINT('Ctrl Pts',(-19.6649658429815,24.1718403156909,21.0607852178963));
#62118=CARTESIAN_POINT('Ctrl Pts',(-19.6500775641385,24.0573267101454,21.0549125240998));
#62119=CARTESIAN_POINT('Ctrl Pts',(-19.6460014024419,24.0259748005267,21.0533046787765));
#62120=CARTESIAN_POINT('Ctrl Pts',(-19.6423050752392,23.9945873748693,21.0516968334532));
#62121=CARTESIAN_POINT('Ctrl Pts',(-19.6389887259146,23.9631743664267,21.0500889881299));
#62122=CARTESIAN_POINT('Ctrl Pts',(-19.626876498573,23.8484453489128,21.0442166911612));
#62123=CARTESIAN_POINT('Ctrl Pts',(-19.6197962755918,23.7329907458361,21.0383443941925));
#62124=CARTESIAN_POINT('Ctrl Pts',(-19.6178238894911,23.6172896406746,21.0324720972238));
#62125=CARTESIAN_POINT('Ctrl Pts',(-19.6158540594461,23.5017384749566,21.0266074102856));
#62126=CARTESIAN_POINT('Ctrl Pts',(-19.6189789097497,23.385941851927,21.0207427233475));
#62127=CARTESIAN_POINT('Ctrl Pts',(-19.6272226695634,23.270385240232,21.0148780364093));
#62128=CARTESIAN_POINT('Ctrl Pts',(-19.6354579511863,23.1549474712782,21.0090193809345));
#62129=CARTESIAN_POINT('Ctrl Pts',(-19.648801641763,23.0397496325442,21.0031607254597));
#62130=CARTESIAN_POINT('Ctrl Pts',(-19.6672259317868,22.9252777926755,20.9973020699848));
#62131=CARTESIAN_POINT('Ctrl Pts',(-19.6863698908069,22.8063345819157,20.9912145702669));
#62132=CARTESIAN_POINT('Ctrl Pts',(-19.7109994537516,22.6881756971685,20.985127070549));
#62133=CARTESIAN_POINT('Ctrl Pts',(-19.7410239380902,22.5713416462355,20.9790395708311));
#62134=CARTESIAN_POINT('Ctrl Pts',(-19.7698862608518,22.4590299059386,20.9731877007477));
#62135=CARTESIAN_POINT('Ctrl Pts',(-19.8037335144383,22.347942783184,20.9673358306644));
#62136=CARTESIAN_POINT('Ctrl Pts',(-19.8424330926155,22.2385498187329,20.961483960581));
#62137=CARTESIAN_POINT('Ctrl Pts',(-19.88112677843,22.1291735103553,20.955632981498));
#62138=CARTESIAN_POINT('Ctrl Pts',(-19.9246711820129,22.0214912370001,20.9497820024151));
#62139=CARTESIAN_POINT('Ctrl Pts',(-19.9728843066086,21.9159558688609,20.9439310233321));
#62140=CARTESIAN_POINT('Ctrl Pts',(-20.0211017660281,21.8104110120766,20.9380795181898));
#62141=CARTESIAN_POINT('Ctrl Pts',(-20.0739886091254,21.7070138202552,20.9322280130475));
#62142=CARTESIAN_POINT('Ctrl Pts',(-20.1313156225259,21.6061950708339,20.9263765079053));
#62143=CARTESIAN_POINT('Ctrl Pts',(-20.1886616729795,21.5053428417007,20.9205230596055));
#62144=CARTESIAN_POINT('Ctrl Pts',(-20.2504506214302,21.4070711167174,20.9146696113058));
#62145=CARTESIAN_POINT('Ctrl Pts',(-20.3164088207457,21.3117834447602,20.908816163006));
#62146=CARTESIAN_POINT('Ctrl Pts',(-20.3824420288565,21.2163874100286,20.9029560580645));
#62147=CARTESIAN_POINT('Ctrl Pts',(-20.452653715994,21.1239825417778,20.8970959531229));
#62148=CARTESIAN_POINT('Ctrl Pts',(-20.5267286131565,21.0349409975039,20.8912358481814));
#62149=CARTESIAN_POINT('Ctrl Pts',(-20.6008533951262,20.9458394893228,20.885371796826));
#62150=CARTESIAN_POINT('Ctrl Pts',(-20.6788462899871,20.8601061201963,20.8795077454705));
#62151=CARTESIAN_POINT('Ctrl Pts',(-20.7603549018245,20.7780764523574,20.8736436941151));
#62152=CARTESIAN_POINT('Ctrl Pts',(-20.841983641085,20.6959258891628,20.8677710003186));
#62153=CARTESIAN_POINT('Ctrl Pts',(-20.9271381356132,20.6174902004143,20.861898306522));
#62154=CARTESIAN_POINT('Ctrl Pts',(-21.015432607422,20.5430649832508,20.8560256127254));
#62155=CARTESIAN_POINT('Ctrl Pts',(-21.0396061568191,20.5226886037717,20.854417767402));
#62156=CARTESIAN_POINT('Ctrl Pts',(-21.0640149031018,20.5026125875007,20.8528099220785));
#62157=CARTESIAN_POINT('Ctrl Pts',(-21.0886505667624,20.4828424244141,20.8512020767551));
#62158=CARTESIAN_POINT('Ctrl Pts',(-21.1786268417969,20.4106363066548,20.8453297797864));
#62159=CARTESIAN_POINT('Ctrl Pts',(-21.2719335758181,20.3422714888359,20.8394574828176));
#62160=CARTESIAN_POINT('Ctrl Pts',(-21.3682086985497,20.2780707350582,20.8335851858489));
#62161=CARTESIAN_POINT('Ctrl Pts',(-21.4643590563682,20.2139531803587,20.8277204989107));
#62162=CARTESIAN_POINT('Ctrl Pts',(-21.5634698122484,20.1539891856337,20.8218558119725));
#62163=CARTESIAN_POINT('Ctrl Pts',(-21.6651456301621,20.0984615516671,20.8159911250343));
#62164=CARTESIAN_POINT('Ctrl Pts',(-21.7667168808622,20.042991024396,20.8101324695595));
#62165=CARTESIAN_POINT('Ctrl Pts',(-21.8708475858432,19.9919479797429,20.8042738140847));
#62166=CARTESIAN_POINT('Ctrl Pts',(-21.9771137751809,19.9455717618124,20.7984151586099));
#62167=CARTESIAN_POINT('Ctrl Pts',(-22.087530815472,19.8973840479619,20.7923276588919));
#62168=CARTESIAN_POINT('Ctrl Pts',(-22.2002531906017,19.8542354261917,20.786240159174));
#62169=CARTESIAN_POINT('Ctrl Pts',(-22.3147771445353,19.8163417711477,20.7801526594561));
#62170=CARTESIAN_POINT('Ctrl Pts',(-22.424868205055,19.7799148706831,20.7743007893727));
#62171=CARTESIAN_POINT('Ctrl Pts',(-22.5366235407265,19.7483438338567,20.7684489192893));
#62172=CARTESIAN_POINT('Ctrl Pts',(-22.6495764397381,19.7217709035055,20.7625970492059));
#62173=CARTESIAN_POINT('Ctrl Pts',(-22.7625121406436,19.6952020191245,20.756746070123));
#62174=CARTESIAN_POINT('Ctrl Pts',(-22.8766446400523,19.6736298227336,20.75089509104));
#62175=CARTESIAN_POINT('Ctrl Pts',(-22.9914945537099,19.6571459929467,20.745044111957));
#62176=CARTESIAN_POINT('Ctrl Pts',(-23.10635479348,19.6406606811048,20.7391926068147));
#62177=CARTESIAN_POINT('Ctrl Pts',(-23.2219321665099,19.6292647040536,20.7333411016724));
#62178=CARTESIAN_POINT('Ctrl Pts',(-23.3377403529678,19.6229980742019,20.7274895965301));
#62179=CARTESIAN_POINT('Ctrl Pts',(-23.4535869968036,19.6167293633389,20.7216361482303));
#62180=CARTESIAN_POINT('Ctrl Pts',(-23.5696641939169,19.6155934089932,20.7157826999306));
#62181=CARTESIAN_POINT('Ctrl Pts',(-23.6854845139918,19.6195781225166,20.7099292516308));
#62182=CARTESIAN_POINT('Ctrl Pts',(-23.8014365469203,19.6235673675244,20.7040691466892));
#62183=CARTESIAN_POINT('Ctrl Pts',(-23.9171307063542,19.6326888893325,20.6982090417477));
#62184=CARTESIAN_POINT('Ctrl Pts',(-24.0320834736873,19.6468786137435,20.6923489368062));
#62185=CARTESIAN_POINT('Ctrl Pts',(-24.1471136545145,19.6610778940458,20.6864848854507));
#62186=CARTESIAN_POINT('Ctrl Pts',(-24.2614010424423,19.6803521045682,20.6806208340953));
#62187=CARTESIAN_POINT('Ctrl Pts',(-24.3744728384027,19.7045861543274,20.6747567827398));
#62188=CARTESIAN_POINT('Ctrl Pts',(-24.4877112796192,19.7288559202384,20.6688840889432));
#62189=CARTESIAN_POINT('Ctrl Pts',(-24.5997301548246,19.7581000103351,20.6630113951467));
#62190=CARTESIAN_POINT('Ctrl Pts',(-24.7100722438301,19.7921536459089,20.6571387013501));
#62191=CARTESIAN_POINT('Ctrl Pts',(-24.740282062002,19.8014769616812,20.6555308560268));
#62192=CARTESIAN_POINT('Ctrl Pts',(-24.7703663134547,19.8111605115869,20.6539230107035));
#62193=CARTESIAN_POINT('Ctrl Pts',(-24.8003159039542,19.821200297502,20.6523151653801));
#62194=CARTESIAN_POINT('Ctrl Pts',(-24.9097001133387,19.8578683796494,20.6464428684114));
#62195=CARTESIAN_POINT('Ctrl Pts',(-25.0176528269035,19.8994148182835,20.6405705714427));
#62196=CARTESIAN_POINT('Ctrl Pts',(-25.1237067834616,19.9457094652855,20.634698274474));
#62197=CARTESIAN_POINT('Ctrl Pts',(-25.2296233025146,19.9919441181016,20.6288335875358));
#62198=CARTESIAN_POINT('Ctrl Pts',(-25.3336455825241,20.0429145787256,20.6229689005975));
#62199=CARTESIAN_POINT('Ctrl Pts',(-25.435322002563,20.0984411101362,20.6171042136593));
#62200=CARTESIAN_POINT('Ctrl Pts',(-25.5368938547689,20.1539105359852,20.6112455581845));
#62201=CARTESIAN_POINT('Ctrl Pts',(-25.6361242851046,20.2139265157134,20.6053869027097));
#62202=CARTESIAN_POINT('Ctrl Pts',(-25.7325827556419,20.2782617319448,20.5995282472348));
#62203=CARTESIAN_POINT('Ctrl Pts',(-25.8328089789975,20.3451099383878,20.5934407475169));
#62204=CARTESIAN_POINT('Ctrl Pts',(-25.9300418608491,20.4166215046015,20.587353247799));
#62205=CARTESIAN_POINT('Ctrl Pts',(-26.0238274807427,20.4924893015798,20.5812657480811));
#62206=CARTESIAN_POINT('Ctrl Pts',(-26.1139829285855,20.5654204739831,20.5754138779977));
#62207=CARTESIAN_POINT('Ctrl Pts',(-26.2009526681496,20.6423766291465,20.5695620079143));
#62208=CARTESIAN_POINT('Ctrl Pts',(-26.2843647506304,20.7230420028754,20.5637101378309));
#62209=CARTESIAN_POINT('Ctrl Pts',(-26.3677641328631,20.8036950945677,20.5578591587479));
#62210=CARTESIAN_POINT('Ctrl Pts',(-26.447606637981,20.8880559946041,20.5520081796649));
#62211=CARTESIAN_POINT('Ctrl Pts',(-26.5235560077159,20.9757709451457,20.5461572005819));
#62212=CARTESIAN_POINT('Ctrl Pts',(-26.5995122060301,21.0634937821056,20.5403056954396));
#62213=CARTESIAN_POINT('Ctrl Pts',(-26.6715743025231,21.1545709565156,20.5344541902973));
#62214=CARTESIAN_POINT('Ctrl Pts',(-26.7394457575984,21.2486149477451,20.528602685155));
#62215=CARTESIAN_POINT('Ctrl Pts',(-26.8073397513064,21.3426901689369,20.5227492368552));
#62216=CARTESIAN_POINT('Ctrl Pts',(-26.8710400946581,21.43973383096,20.5168957885554));
#62217=CARTESIAN_POINT('Ctrl Pts',(-26.9302934812866,21.5393293160844,20.5110423402556));
#62218=CARTESIAN_POINT('Ctrl Pts',(-26.9896142518824,21.6390380629022,20.5051822353141));
#62219=CARTESIAN_POINT('Ctrl Pts',(-27.0444777603398,21.7413040696055,20.4993221303725));
#62220=CARTESIAN_POINT('Ctrl Pts',(-27.0946765510513,21.8456859090583,20.493462025431));
#62221=CARTESIAN_POINT('Ctrl Pts',(-27.1449091475065,21.9501380431469,20.4875979740755));
#62222=CARTESIAN_POINT('Ctrl Pts',(-27.1904706089677,22.0567084680319,20.4817339227201));
#62223=CARTESIAN_POINT('Ctrl Pts',(-27.2312021954705,22.1649371983693,20.4758698713646));
#62224=CARTESIAN_POINT('Ctrl Pts',(-27.2719938122011,22.2733254362509,20.469997177568));
#62225=CARTESIAN_POINT('Ctrl Pts',(-27.3079412194039,22.3833764658842,20.4641244837714));
#62226=CARTESIAN_POINT('Ctrl Pts',(-27.3389359012759,22.4946165503754,20.4582517899748));
#62227=CARTESIAN_POINT('Ctrl Pts',(-27.3474217266942,22.5250722246876,20.4566439446516));
#62228=CARTESIAN_POINT('Ctrl Pts',(-27.3555366069571,22.5556169794325,20.4550360993284));
#62229=CARTESIAN_POINT('Ctrl Pts',(-27.3632789899344,22.5862410023232,20.4534282540052));
#62230=CARTESIAN_POINT('Ctrl Pts',(-27.4005143394058,22.7335207478353,20.4456956628015));
#62231=CARTESIAN_POINT('Ctrl Pts',(-27.4292315992316,22.8830345880011,20.4379630715977));
#62232=CARTESIAN_POINT('Ctrl Pts',(-27.4492142270171,23.0339321869424,20.430230480394));
#62233=CARTESIAN_POINT('Ctrl Pts',(-27.4687344541642,23.1813379955728,20.4226768223691));
#62234=CARTESIAN_POINT('Ctrl Pts',(-27.4799196555139,23.3300645645562,20.4151231643441));
#62235=CARTESIAN_POINT('Ctrl Pts',(-27.4826124151087,23.4792965783715,20.4075695063192));
#62236=CARTESIAN_POINT('Ctrl Pts',(-27.4830171393839,23.501726289045,20.4064341844824));
#62237=CARTESIAN_POINT('Ctrl Pts',(-27.4832300997421,23.5241673704898,20.4052988626457));
#62238=CARTESIAN_POINT('Ctrl Pts',(-27.483250851415,23.5466170023887,20.4041635408089));
#62239=CARTESIAN_POINT('',(-27.4768438131603,23.5509604052536,19.1541635220348));
#62240=CARTESIAN_POINT('Ctrl Pts',(-27.482652284421,23.5466179268635,20.4041635220348));
#62241=CARTESIAN_POINT('Ctrl Pts',(-27.4736509478652,24.5326769039293,20.3542894622333));
#62242=CARTESIAN_POINT('Ctrl Pts',(-26.5977887904392,26.8437168577948,20.2381197653068));
#62243=CARTESIAN_POINT('Ctrl Pts',(-22.7128308123558,28.1262197186493,20.0556544312555));
#62244=CARTESIAN_POINT('Ctrl Pts',(-19.2477526204729,25.3192198423143,19.8567675198806));
#62245=CARTESIAN_POINT('Ctrl Pts',(-19.7363070551659,20.8866889912118,19.6578806085056));
#62246=CARTESIAN_POINT('Ctrl Pts',(-23.7295540135405,18.9017472008686,19.4589936971309));
#62247=CARTESIAN_POINT('Ctrl Pts',(-26.9616635618324,20.8321907758035,19.2910880016405));
#62248=CARTESIAN_POINT('Ctrl Pts',(-27.4757215964172,22.8501543544342,19.1894779432751));
#62249=CARTESIAN_POINT('Ctrl Pts',(-27.4768438131603,23.5509604052536,19.1541635220348));
#62250=CARTESIAN_POINT('',(-27.4852583988885,23.553643346945,17.9041635220348));
#62251=CARTESIAN_POINT('Ctrl Pts',(-27.4768438131603,23.5509604052536,19.1541635220348));
#62252=CARTESIAN_POINT('Ctrl Pts',(-27.4778283299092,24.165775055786,19.1231823061502));
#62253=CARTESIAN_POINT('Ctrl Pts',(-27.0518825353482,26.0949196521075,19.0259054531406));
#62254=CARTESIAN_POINT('Ctrl Pts',(-24.0327034582734,28.1771296573096,18.8623329630062));
#62255=CARTESIAN_POINT('Ctrl Pts',(-19.9183683533861,26.4571698245448,18.6634460516312));
#62256=CARTESIAN_POINT('Ctrl Pts',(-19.1414268753694,22.0659994655903,18.4645591402563));
#62257=CARTESIAN_POINT('Ctrl Pts',(-22.4158223687412,19.0387318304797,18.2656722288814));
#62258=CARTESIAN_POINT('Ctrl Pts',(-26.4702848712463,20.0891904388618,18.0788736894743));
#62259=CARTESIAN_POINT('Ctrl Pts',(-27.4755052834716,22.4837319727721,17.958370787192));
#62260=CARTESIAN_POINT('Ctrl Pts',(-27.4852583988885,23.553643346945,17.9041635220348));
#62261=CARTESIAN_POINT('',(-27.4880679510806,23.5479486834992,16.6541635220348));
#62262=CARTESIAN_POINT('Ctrl Pts',(-27.4852583988885,23.553643346945,17.9041635220348));
#62263=CARTESIAN_POINT('Ctrl Pts',(-27.4874333709454,23.792236580268,17.8920751500671));
#62264=CARTESIAN_POINT('Ctrl Pts',(-27.3588666602939,25.3369952882741,17.8136911409746));
#62265=CARTESIAN_POINT('Ctrl Pts',(-25.313681394457,27.8550254035316,17.6690114947566));
#62266=CARTESIAN_POINT('Ctrl Pts',(-20.8817829454537,27.3607670506816,17.470124583382));
#62267=CARTESIAN_POINT('Ctrl Pts',(-18.9019817972975,23.3649689332391,17.271237672007));
#62268=CARTESIAN_POINT('Ctrl Pts',(-21.1935473456834,19.539430733317,17.0723507606322));
#62269=CARTESIAN_POINT('Ctrl Pts',(-25.6507251443653,19.3994977044937,16.8734638492572));
#62270=CARTESIAN_POINT('Ctrl Pts',(-27.4218625880093,21.9747100905248,16.7340681030581));
#62271=CARTESIAN_POINT('Ctrl Pts',(-27.4889989329917,23.4138953184574,16.6609679939839));
#62272=CARTESIAN_POINT('Ctrl Pts',(-27.4880679510806,23.5479486834992,16.6541635220348));
#62273=CARTESIAN_POINT('',(-27.4814458092685,23.5479673557521,15.4041640332968));
#62274=CARTESIAN_POINT('Ctrl Pts',(-27.4880679510806,23.5479486834992,16.6541635220348));
#62275=CARTESIAN_POINT('Ctrl Pts',(-27.4799284218034,24.7199706922043,16.594672356859));
#62276=CARTESIAN_POINT('Ctrl Pts',(-26.3022252840322,27.2122626367951,16.4688855545583));
#62277=CARTESIAN_POINT('Ctrl Pts',(-22.0603268787045,27.9571644187965,16.2768031151325));
#62278=CARTESIAN_POINT('Ctrl Pts',(-19.0372756429476,24.678875778727,16.0779162037576));
#62279=CARTESIAN_POINT('Ctrl Pts',(-20.1612675306071,20.3634780661081,15.8790292923827));
#62280=CARTESIAN_POINT('Ctrl Pts',(-24.3994492957219,18.9764558934434,15.680142381008));
#62281=CARTESIAN_POINT('Ctrl Pts',(-27.1514415008424,21.2175531301115,15.5218542812444));
#62282=CARTESIAN_POINT('Ctrl Pts',(-27.4807207713122,23.038395923409,15.429861818606));
#62283=CARTESIAN_POINT('Ctrl Pts',(-27.4780552727636,23.5479502857209,15.4041649930927));
#62284=CARTESIAN_POINT('',(-27.4822862170138,23.553399450288,14.1541631347917));
#62285=CARTESIAN_POINT('Ctrl Pts',(-27.4832518730933,23.5479764485802,15.4041635220348));
#62286=CARTESIAN_POINT('Ctrl Pts',(-27.4833198073102,23.6653646180412,15.3982514394489));
#62287=CARTESIAN_POINT('Ctrl Pts',(-27.4781278759661,23.7827617822172,15.392339356863));
#62288=CARTESIAN_POINT('Ctrl Pts',(-27.4677002237111,23.8996700188229,15.3864272742771));
#62289=CARTESIAN_POINT('Ctrl Pts',(-27.4572706033443,24.016600320653,15.3805140758466));
#62290=CARTESIAN_POINT('Ctrl Pts',(-27.441603330606,24.1330411114468,15.374600877416));
#62291=CARTESIAN_POINT('Ctrl Pts',(-27.4207744155021,24.2484998710837,15.3686876789855));
#62292=CARTESIAN_POINT('Ctrl Pts',(-27.3999369283831,24.3640061470802,15.3627720470136));
#62293=CARTESIAN_POINT('Ctrl Pts',(-27.373933642155,24.4785291927818,15.3568564150417));
#62294=CARTESIAN_POINT('Ctrl Pts',(-27.3428915187345,24.591587498927,15.3509407830699));
#62295=CARTESIAN_POINT('Ctrl Pts',(-27.3118073488031,24.7047989423829,15.3450171383831));
#62296=CARTESIAN_POINT('Ctrl Pts',(-27.2756708155007,24.8165412958034,15.3390934936964));
#62297=CARTESIAN_POINT('Ctrl Pts',(-27.2346586971704,24.9263485340869,15.3331698490096));
#62298=CARTESIAN_POINT('Ctrl Pts',(-27.1936177556452,25.0362329445708,15.327242041203));
#62299=CARTESIAN_POINT('Ctrl Pts',(-27.1476945583824,25.1441791610812,15.3213142333964));
#62300=CARTESIAN_POINT('Ctrl Pts',(-27.0971131938648,25.2497431739592,15.3153864255898));
#62301=CARTESIAN_POINT('Ctrl Pts',(-27.0464387821752,25.3555013775826,15.3094477132582));
#62302=CARTESIAN_POINT('Ctrl Pts',(-26.9910892698278,25.4588682669344,15.3035090009267));
#62303=CARTESIAN_POINT('Ctrl Pts',(-26.9313340448883,25.559425695246,15.2975702885951));
#62304=CARTESIAN_POINT('Ctrl Pts',(-26.8803475254188,25.6452269499749,15.2925030451494));
#62305=CARTESIAN_POINT('Ctrl Pts',(-26.8261542681029,25.7289831563621,15.2874358017038));
#62306=CARTESIAN_POINT('Ctrl Pts',(-26.7689449230318,25.8104534718642,15.2823685582581));
#62307=CARTESIAN_POINT('Ctrl Pts',(-26.702646497222,25.9048673068994,15.2764962612894));
#62308=CARTESIAN_POINT('Ctrl Pts',(-26.6320793230445,25.9965197419879,15.2706239643207));
#62309=CARTESIAN_POINT('Ctrl Pts',(-26.5575012184891,26.0849999226131,15.264751667352));
#62310=CARTESIAN_POINT('Ctrl Pts',(-26.4830197612344,26.1733654399512,15.2588869804138));
#62311=CARTESIAN_POINT('Ctrl Pts',(-26.4045379742129,26.258566564946,15.2530222934756));
#62312=CARTESIAN_POINT('Ctrl Pts',(-26.3223567574976,26.3402215568418,15.2471576065374));
#62313=CARTESIAN_POINT('Ctrl Pts',(-26.2402600590189,26.4217925716903,15.2412989510626));
#62314=CARTESIAN_POINT('Ctrl Pts',(-26.1544717899351,26.4998244178487,15.2354402955878));
#62315=CARTESIAN_POINT('Ctrl Pts',(-26.065332457127,26.5739691137642,15.229581640113));
#62316=CARTESIAN_POINT('Ctrl Pts',(-25.9727112634665,26.6510099668079,15.2234941403951));
#62317=CARTESIAN_POINT('Ctrl Pts',(-25.8764721712179,26.7238534602628,15.2174066406772));
#62318=CARTESIAN_POINT('Ctrl Pts',(-25.7770388530061,26.7921519254475,15.2113191409593));
#62319=CARTESIAN_POINT('Ctrl Pts',(-25.6814543130309,26.8578067531562,15.2054672708759));
#62320=CARTESIAN_POINT('Ctrl Pts',(-25.5829186002999,26.9192616043388,15.1996154007925));
#62321=CARTESIAN_POINT('Ctrl Pts',(-25.4818403227033,26.9762498471666,15.1937635307091));
#62322=CARTESIAN_POINT('Ctrl Pts',(-25.3807774351936,27.0332294130164,15.1879125516261));
#62323=CARTESIAN_POINT('Ctrl Pts',(-25.2771731125486,27.0857435197654,15.1820615725432));
#62324=CARTESIAN_POINT('Ctrl Pts',(-25.171462219991,27.1335705676174,15.1762105934602));
#62325=CARTESIAN_POINT('Ctrl Pts',(-25.0657418230066,27.1814019155813,15.1703590883179));
#62326=CARTESIAN_POINT('Ctrl Pts',(-24.9579148562495,27.2245451965112,15.1645075831756));
#62327=CARTESIAN_POINT('Ctrl Pts',(-24.8484372395267,27.2628264992199,15.1586560780333));
#62328=CARTESIAN_POINT('Ctrl Pts',(-24.7389232676711,27.3011205143158,15.1528026297336));
#62329=CARTESIAN_POINT('Ctrl Pts',(-24.6277579459064,27.3345492043703,15.1469491814338));
#62330=CARTESIAN_POINT('Ctrl Pts',(-24.515412775287,27.3629883872431,15.1410957331341));
#62331=CARTESIAN_POINT('Ctrl Pts',(-24.4029398438132,27.3914599116422,15.1352356281925));
#62332=CARTESIAN_POINT('Ctrl Pts',(-24.2892847863837,27.4149305019169,15.129375523251));
#62333=CARTESIAN_POINT('Ctrl Pts',(-24.174929829752,27.4333269931604,15.1235154183095));
#62334=CARTESIAN_POINT('Ctrl Pts',(-24.0604978622143,27.4517358732894,15.1176513669541));
#62335=CARTESIAN_POINT('Ctrl Pts',(-23.9453654665833,27.4650638028659,15.1117873155986));
#62336=CARTESIAN_POINT('Ctrl Pts',(-23.8300187871143,27.4732896003858,15.1059232642432));
#62337=CARTESIAN_POINT('Ctrl Pts',(-23.714502109665,27.4815275210892,15.1000505704467));
#62338=CARTESIAN_POINT('Ctrl Pts',(-23.5987709297598,27.4846482911153,15.0941778766501));
#62339=CARTESIAN_POINT('Ctrl Pts',(-23.4833102719325,27.4826827896718,15.0883051828535));
#62340=CARTESIAN_POINT('Ctrl Pts',(-23.4516990752384,27.4821446682554,15.0866973375301));
#62341=CARTESIAN_POINT('Ctrl Pts',(-23.4201081172826,27.4812255927403,15.0850894922067));
#62342=CARTESIAN_POINT('Ctrl Pts',(-23.3885472460941,27.4799268694236,15.0834816468833));
#62343=CARTESIAN_POINT('Ctrl Pts',(-23.27327819284,27.4751835717416,15.0776093499146));
#62344=CARTESIAN_POINT('Ctrl Pts',(-23.1580249122346,27.4653562507003,15.0717370529458));
#62345=CARTESIAN_POINT('Ctrl Pts',(-23.0432724246296,27.450439728617,15.0658647559771));
#62346=CARTESIAN_POINT('Ctrl Pts',(-22.9286686471352,27.4355425371617,15.0600000690389));
#62347=CARTESIAN_POINT('Ctrl Pts',(-22.8145647781872,27.4155693129454,15.0541353821007));
#62348=CARTESIAN_POINT('Ctrl Pts',(-22.7014446319339,27.3905668611866,15.0482706951625));
#62349=CARTESIAN_POINT('Ctrl Pts',(-22.5884408226691,27.3655901228841,15.0424120396877));
#62350=CARTESIAN_POINT('Ctrl Pts',(-22.4764191249956,27.3355945335804,15.0365533842129));
#62351=CARTESIAN_POINT('Ctrl Pts',(-22.3658563600363,27.3006784686462,15.030694728738));
#62352=CARTESIAN_POINT('Ctrl Pts',(-22.2509749160955,27.264398551462,15.0246072290201));
#62353=CARTESIAN_POINT('Ctrl Pts',(-22.1376691536408,27.2228059846972,15.0185197293022));
#62354=CARTESIAN_POINT('Ctrl Pts',(-22.0264605851813,27.1760692815786,15.0124322295843));
#62355=CARTESIAN_POINT('Ctrl Pts',(-21.919556581084,27.1311416220386,15.0065803595009));
#62356=CARTESIAN_POINT('Ctrl Pts',(-21.8145908537228,27.0814608259816,15.0007284894175));
#62357=CARTESIAN_POINT('Ctrl Pts',(-21.7120085948154,27.0272265362747,14.9948766193341));
#62358=CARTESIAN_POINT('Ctrl Pts',(-21.6094419549896,26.9730005042315,14.9890256402511));
#62359=CARTESIAN_POINT('Ctrl Pts',(-21.5092584273983,26.9142225502201,14.9831746611682));
#62360=CARTESIAN_POINT('Ctrl Pts',(-21.411879510756,26.8511387495641,14.9773236820852));
#62361=CARTESIAN_POINT('Ctrl Pts',(-21.3144918388121,26.7880492770675,14.9714721769429));
#62362=CARTESIAN_POINT('Ctrl Pts',(-21.2199096260556,26.7206534131034,14.9656206718006));
#62363=CARTESIAN_POINT('Ctrl Pts',(-21.1285256308694,26.6492407242857,14.9597691666583));
#62364=CARTESIAN_POINT('Ctrl Pts',(-21.0371112890475,26.5778043208684,14.9539157183585));
#62365=CARTESIAN_POINT('Ctrl Pts',(-20.948897602183,26.5023486946252,14.9480622700587));
#62366=CARTESIAN_POINT('Ctrl Pts',(-20.8642439131024,26.4232034015927,14.942208821759));
#62367=CARTESIAN_POINT('Ctrl Pts',(-20.7794939543955,26.3439681031763,14.9363487168174));
#62368=CARTESIAN_POINT('Ctrl Pts',(-20.6983123762814,26.2610350454604,14.9304886118759));
#62369=CARTESIAN_POINT('Ctrl Pts',(-20.6210213976272,26.1747703851698,14.9246285069343));
#62370=CARTESIAN_POINT('Ctrl Pts',(-20.5436783683362,26.0884476310296,14.9187644555789));
#62371=CARTESIAN_POINT('Ctrl Pts',(-20.4702314169168,25.9987891258121,14.9129004042234));
#62372=CARTESIAN_POINT('Ctrl Pts',(-20.4009611453028,25.9061924213351,14.907036352868));
#62373=CARTESIAN_POINT('Ctrl Pts',(-20.3315887831363,25.8134592477999,14.9011636590714));
#62374=CARTESIAN_POINT('Ctrl Pts',(-20.2664056180206,25.7177795728769,14.8952909652749));
#62375=CARTESIAN_POINT('Ctrl Pts',(-20.2056478470824,25.6195781473654,14.8894182714783));
#62376=CARTESIAN_POINT('Ctrl Pts',(-20.189013385753,25.5926922397697,14.887810426155));
#62377=CARTESIAN_POINT('Ctrl Pts',(-20.1727103673945,25.565617437524,14.8862025808317));
#62378=CARTESIAN_POINT('Ctrl Pts',(-20.1567430162745,25.5383627320492,14.8845947355083));
#62379=CARTESIAN_POINT('Ctrl Pts',(-20.0984258223128,25.4388209900542,14.8787224385396));
#62380=CARTESIAN_POINT('Ctrl Pts',(-20.0443944282895,25.3365443877004,14.8728501415709));
#62381=CARTESIAN_POINT('Ctrl Pts',(-19.9949153643375,25.2319381819903,14.8669778446022));
#62382=CARTESIAN_POINT('Ctrl Pts',(-19.9455004213229,25.1274675376154,14.861113157664));
#62383=CARTESIAN_POINT('Ctrl Pts',(-19.900626251599,25.0206736637924,14.8552484707258));
#62384=CARTESIAN_POINT('Ctrl Pts',(-19.8605149992077,24.9119889016868,14.8493837837876));
#62385=CARTESIAN_POINT('Ctrl Pts',(-19.8204449987283,24.8034159150548,14.8435251283128));
#62386=CARTESIAN_POINT('Ctrl Pts',(-19.7851283147536,24.6929562936523,14.8376664728379));
#62387=CARTESIAN_POINT('Ctrl Pts',(-19.7547399244643,24.5810643711485,14.8318078173631));
#62388=CARTESIAN_POINT('Ctrl Pts',(-19.7231645368848,24.464801851599,14.8257203176452));
#62389=CARTESIAN_POINT('Ctrl Pts',(-19.6969104931754,24.3469932670035,14.8196328179273));
#62390=CARTESIAN_POINT('Ctrl Pts',(-19.6761179199509,24.2281684631287,14.8135453182094));
#62391=CARTESIAN_POINT('Ctrl Pts',(-19.6561301675324,24.1139430262197,14.807693448126));
#62392=CARTESIAN_POINT('Ctrl Pts',(-19.64118902936,23.9987790222625,14.8018415780426));
#62393=CARTESIAN_POINT('Ctrl Pts',(-19.6313671875367,23.8831589139519,14.7959897079592));
#62394=CARTESIAN_POINT('Ctrl Pts',(-19.6215468411782,23.7675564098539,14.7901387288762));
#62395=CARTESIAN_POINT('Ctrl Pts',(-19.6168442763347,23.6514983512697,14.7842877497932));
#62396=CARTESIAN_POINT('Ctrl Pts',(-19.6172803036318,23.5354723662843,14.7784367707102));
#62397=CARTESIAN_POINT('Ctrl Pts',(-19.6177163701318,23.419435949446,14.7725852655679));
#62398=CARTESIAN_POINT('Ctrl Pts',(-19.6232919456499,23.3034320253436,14.7667337604256));
#62399=CARTESIAN_POINT('Ctrl Pts',(-19.6339757154914,23.1879475512251,14.7608822552833));
#62400=CARTESIAN_POINT('Ctrl Pts',(-19.6446630331804,23.0724247272265,14.7550288069835));
#62401=CARTESIAN_POINT('Ctrl Pts',(-19.6604618801582,22.9574221076206,14.7491753586837));
#62402=CARTESIAN_POINT('Ctrl Pts',(-19.6812892354332,22.8434201525652,14.7433219103839));
#62403=CARTESIAN_POINT('Ctrl Pts',(-19.7021402759336,22.7292885525323,14.7374618054423));
#62404=CARTESIAN_POINT('Ctrl Pts',(-19.7280311643595,22.6161602953029,14.7316017005008));
#62405=CARTESIAN_POINT('Ctrl Pts',(-19.7588280198721,22.5045043922483,14.7257415955592));
#62406=CARTESIAN_POINT('Ctrl Pts',(-19.7896456151393,22.3927732959314,14.7198775442038));
#62407=CARTESIAN_POINT('Ctrl Pts',(-19.8253756290119,22.2825169204275,14.7140134928483));
#62408=CARTESIAN_POINT('Ctrl Pts',(-19.8658352717163,22.1741862344625,14.7081494414929));
#62409=CARTESIAN_POINT('Ctrl Pts',(-19.9063545438576,22.065695890691,14.7022767476963));
#62410=CARTESIAN_POINT('Ctrl Pts',(-19.9516171956521,21.9591372797747,14.6964040538998));
#62411=CARTESIAN_POINT('Ctrl Pts',(-20.001393551686,21.8549387141325,14.6905313601032));
#62412=CARTESIAN_POINT('Ctrl Pts',(-20.0150214853107,21.8264108898903,14.6889235147799));
#62413=CARTESIAN_POINT('Ctrl Pts',(-20.0289874981503,21.7980598086145,14.6873156694567));
#62414=CARTESIAN_POINT('Ctrl Pts',(-20.0432863089673,21.7698938844963,14.6857078241334));
#62415=CARTESIAN_POINT('Ctrl Pts',(-20.0955095310659,21.6670241193339,14.6798355271647));
#62416=CARTESIAN_POINT('Ctrl Pts',(-20.1523502936252,21.5662817616051,14.673963230196));
#62417=CARTESIAN_POINT('Ctrl Pts',(-20.2136117179652,21.4681101061724,14.6680909332273));
#62418=CARTESIAN_POINT('Ctrl Pts',(-20.2747937523648,21.3700656734081,14.6622262462891));
#62419=CARTESIAN_POINT('Ctrl Pts',(-20.3403848391395,21.2745856653942,14.6563615593509));
#62420=CARTESIAN_POINT('Ctrl Pts',(-20.4101413206848,21.1820906743683,14.6504968724127));
#62421=CARTESIAN_POINT('Ctrl Pts',(-20.4798260620554,21.0896908086508,14.6446382169378));
#62422=CARTESIAN_POINT('Ctrl Pts',(-20.553667429991,21.0002701817873,14.638779561463));
#62423=CARTESIAN_POINT('Ctrl Pts',(-20.6313777685368,20.9142215916248,14.6329209059882));
#62424=CARTESIAN_POINT('Ctrl Pts',(-20.7121235413526,20.8248118677399,14.6268334062703));
#62425=CARTESIAN_POINT('Ctrl Pts',(-20.7970464565817,20.739043366036,14.6207459065524));
#62426=CARTESIAN_POINT('Ctrl Pts',(-20.8857764904659,20.6573203814839,14.6146584068345));
#62427=CARTESIAN_POINT('Ctrl Pts',(-20.9710720395167,20.5787606590055,14.6088065367511));
#62428=CARTESIAN_POINT('Ctrl Pts',(-21.0598851297139,20.5039394024876,14.6029546666677));
#62429=CARTESIAN_POINT('Ctrl Pts',(-21.1518491448553,20.4331785521423,14.5971027965843));
#62430=CARTESIAN_POINT('Ctrl Pts',(-21.2437991576393,20.3624284757797,14.5912518175013));
#62431=CARTESIAN_POINT('Ctrl Pts',(-21.338898813923,20.2957378283611,14.5854008384184));
#62432=CARTESIAN_POINT('Ctrl Pts',(-21.4367491130422,20.2333877018667,14.5795498593354));
#62433=CARTESIAN_POINT('Ctrl Pts',(-21.5346082098449,20.171031969496,14.5736983541931));
#62434=CARTESIAN_POINT('Ctrl Pts',(-21.6352180924672,20.1130177559952,14.5678468490508));
#62435=CARTESIAN_POINT('Ctrl Pts',(-21.738152148686,20.0595819368225,14.5619953439085));
#62436=CARTESIAN_POINT('Ctrl Pts',(-21.8411203870648,20.0061283727773,14.5561418956087));
#62437=CARTESIAN_POINT('Ctrl Pts',(-21.9464139670337,19.9572564166125,14.5502884473089));
#62438=CARTESIAN_POINT('Ctrl Pts',(-22.0535837930351,19.9131559304585,14.5444349990091));
#62439=CARTESIAN_POINT('Ctrl Pts',(-22.1608754943995,19.8690052924756,14.5385748940676));
#62440=CARTESIAN_POINT('Ctrl Pts',(-22.2700473180871,19.8296371124323,14.5327147891261));
#62441=CARTESIAN_POINT('Ctrl Pts',(-22.380632308693,19.7951922746615,14.5268546841845));
#62442=CARTESIAN_POINT('Ctrl Pts',(-22.4912917713688,19.7607242404483,14.5209906328291));
#62443=CARTESIAN_POINT('Ctrl Pts',(-22.6033658971897,19.7311862555468,14.5151265814737));
#62444=CARTESIAN_POINT('Ctrl Pts',(-22.7163764729788,19.7066683035679,14.5092625301182));
#62445=CARTESIAN_POINT('Ctrl Pts',(-22.8295536037973,19.6821142170221,14.5033898363217));
#62446=CARTESIAN_POINT('Ctrl Pts',(-22.9436695331424,19.6625949988642,14.4975171425251));
#62447=CARTESIAN_POINT('Ctrl Pts',(-23.0582397652918,19.6481489403352,14.4916444487286));
#62448=CARTESIAN_POINT('Ctrl Pts',(-23.0896071783288,19.6441938511629,14.4900366034052));
#62449=CARTESIAN_POINT('Ctrl Pts',(-23.1210086406907,19.6406187307726,14.4884287580819));
#62450=CARTESIAN_POINT('Ctrl Pts',(-23.1524342186442,19.6374236841975,14.4868209127585));
#62451=CARTESIAN_POINT('Ctrl Pts',(-23.2672091434939,19.6257544881341,14.4809486157898));
#62452=CARTESIAN_POINT('Ctrl Pts',(-23.3826902211459,19.6191200602394,14.4750763188211));
#62453=CARTESIAN_POINT('Ctrl Pts',(-23.498398078922,19.6175943828427,14.4692040218524));
#62454=CARTESIAN_POINT('Ctrl Pts',(-23.6139559885034,19.6160706826028,14.4633393349142));
#62455=CARTESIAN_POINT('Ctrl Pts',(-23.7297396842375,19.6196425723934,14.457474647976));
#62456=CARTESIAN_POINT('Ctrl Pts',(-23.8452636075533,19.6283324069185,14.4516099610378));
#62457=CARTESIAN_POINT('Ctrl Pts',(-23.9606687217458,19.6370133044928,14.445751305563));
#62458=CARTESIAN_POINT('Ctrl Pts',(-24.0758141851743,19.6508016466365,14.4398926500882));
#62459=CARTESIAN_POINT('Ctrl Pts',(-24.1902140401816,19.6696677474568,14.4340339946133));
#62460=CARTESIAN_POINT('Ctrl Pts',(-24.3090824542876,19.6892707747923,14.4279464948954));
#62461=CARTESIAN_POINT('Ctrl Pts',(-24.4271453696354,19.7143563370762,14.4218589951775));
#62462=CARTESIAN_POINT('Ctrl Pts',(-24.543862632555,19.7448316656838,14.4157714954596));
#62463=CARTESIAN_POINT('Ctrl Pts',(-24.6560621053677,19.7741273818275,14.4099196253762));
#62464=CARTESIAN_POINT('Ctrl Pts',(-24.7670177241516,19.8084032636923,14.4040677552928));
#62465=CARTESIAN_POINT('Ctrl Pts',(-24.8762604636056,19.8475248932487,14.3982158852094));
#62466=CARTESIAN_POINT('Ctrl Pts',(-24.9854865698592,19.8866405661813,14.3923649061264));
#62467=CARTESIAN_POINT('Ctrl Pts',(-25.0929999262666,19.9306003804714,14.3865139270435));
#62468=CARTESIAN_POINT('Ctrl Pts',(-25.1983483686548,19.9792205922973,14.3806629479605));
#62469=CARTESIAN_POINT('Ctrl Pts',(-25.3037062828822,20.0278451755482,14.3748114428182));
#62470=CARTESIAN_POINT('Ctrl Pts',(-25.4068985207907,20.0811308160618,14.3689599376759));
#62471=CARTESIAN_POINT('Ctrl Pts',(-25.5074951930912,20.1388466390442,14.3631084325335));
#62472=CARTESIAN_POINT('Ctrl Pts',(-25.6081252713571,20.1965816281951,14.3572549842337));
#62473=CARTESIAN_POINT('Ctrl Pts',(-25.7061577117494,20.2587495195285,14.3514015359339));
#62474=CARTESIAN_POINT('Ctrl Pts',(-25.801190024885,20.325075109947,14.3455480876341));
#62475=CARTESIAN_POINT('Ctrl Pts',(-25.8963304103959,20.3914761269636,14.3396879826926));
#62476=CARTESIAN_POINT('Ctrl Pts',(-25.9884635196207,20.4620440436949,14.333827877751));
#62477=CARTESIAN_POINT('Ctrl Pts',(-26.0772184150144,20.5364621566787,14.3279677728095));
#62478=CARTESIAN_POINT('Ctrl Pts',(-26.1660330812752,20.6109303856041,14.322103721454));
#62479=CARTESIAN_POINT('Ctrl Pts',(-26.2514646997343,20.6892536950217,14.3162396700985));
#62480=CARTESIAN_POINT('Ctrl Pts',(-26.333179071175,20.7710783961184,14.3103756187431));
#62481=CARTESIAN_POINT('Ctrl Pts',(-26.4150138732873,20.8530236904906,14.3045029249465));
#62482=CARTESIAN_POINT('Ctrl Pts',(-26.4931202165505,20.9384803716216,14.2986302311499));
#62483=CARTESIAN_POINT('Ctrl Pts',(-26.5672039954244,21.0270615231702,14.2927575373534));
#62484=CARTESIAN_POINT('Ctrl Pts',(-26.5874868948088,21.0513135606813,14.2911496920301));
#62485=CARTESIAN_POINT('Ctrl Pts',(-26.6074685251853,21.0757996336955,14.2895418467069));
#62486=CARTESIAN_POINT('Ctrl Pts',(-26.6271434285838,21.1005114415711,14.2879340013836));
#62487=CARTESIAN_POINT('Ctrl Pts',(-26.6988772707787,21.1906096184512,14.2820718672549));
#62488=CARTESIAN_POINT('Ctrl Pts',(-26.7667760253801,21.2840191197142,14.2762097331261));
#62489=CARTESIAN_POINT('Ctrl Pts',(-26.8305176023576,21.3803792482544,14.2703475989974));
#62490=CARTESIAN_POINT('Ctrl Pts',(-26.8941790376487,21.4766182241096,14.2644928352748));
#62491=CARTESIAN_POINT('Ctrl Pts',(-26.9536934585065,21.5758001113278,14.2586380715523));
#62492=CARTESIAN_POINT('Ctrl Pts',(-27.0087785654401,21.6775308027921,14.2527833078297));
#62493=CARTESIAN_POINT('Ctrl Pts',(-27.0638078451477,21.779158393026,14.2469344777476));
#62494=CARTESIAN_POINT('Ctrl Pts',(-27.1144165399632,21.8833292898244,14.2410856476655));
#62495=CARTESIAN_POINT('Ctrl Pts',(-27.1603656938681,21.9896206224028,14.2352368175834));
#62496=CARTESIAN_POINT('Ctrl Pts',(-27.2062794802941,22.0958301415819,14.2293924893986));
#62497=CARTESIAN_POINT('Ctrl Pts',(-27.247540694878,22.2041564717086,14.2235481612138));
#62498=CARTESIAN_POINT('Ctrl Pts',(-27.2839567194601,22.314153005661,14.2177038330291));
#62499=CARTESIAN_POINT('Ctrl Pts',(-27.3203565777141,22.424100708362,14.211862099343));
#62500=CARTESIAN_POINT('Ctrl Pts',(-27.3519153914313,22.5357167483884,14.2060203656569));
#62501=CARTESIAN_POINT('Ctrl Pts',(-27.3784892419353,22.6485360073016,14.2001786319708));
#62502=CARTESIAN_POINT('Ctrl Pts',(-27.4050558725687,22.7613246142606,14.1943384854299));
#62503=CARTESIAN_POINT('Ctrl Pts',(-27.4266401422533,22.8753153859449,14.1884983388891));
#62504=CARTESIAN_POINT('Ctrl Pts',(-27.4431486424174,22.9900303694084,14.1826581923483));
#62505=CARTESIAN_POINT('Ctrl Pts',(-27.4596610348749,23.1047723998102,14.1768166688462));
#62506=CARTESIAN_POINT('Ctrl Pts',(-27.4710952060826,23.2202385729897,14.1709751453442));
#62507=CARTESIAN_POINT('Ctrl Pts',(-27.4774093433978,23.3359434644799,14.1651336218421));
#62508=CARTESIAN_POINT('Ctrl Pts',(-27.4813618919935,23.4083728690927,14.1614769219063));
#62509=CARTESIAN_POINT('Ctrl Pts',(-27.4833091581058,23.480895697148,14.1578202219705));
#62510=CARTESIAN_POINT('Ctrl Pts',(-27.483251278234,23.5533925502411,14.1541635220347));
#62511=CARTESIAN_POINT('',(-27.4855496615812,23.551270215578,12.9041639318795));
#62512=CARTESIAN_POINT('Ctrl Pts',(-27.47973650101,23.5534176803855,14.1541621116859));
#62513=CARTESIAN_POINT('Ctrl Pts',(-27.4829303983389,23.9833541344258,14.1324571044601));
#62514=CARTESIAN_POINT('Ctrl Pts',(-27.219376369067,25.7226727502858,14.0444564601096));
#62515=CARTESIAN_POINT('Ctrl Pts',(-24.6730669936168,28.0646781337204,13.8901601786337));
#62516=CARTESIAN_POINT('Ctrl Pts',(-20.3591193447167,26.9351335953461,13.691273267259));
#62517=CARTESIAN_POINT('Ctrl Pts',(-18.9775525311725,22.6951703500683,13.492386355884));
#62518=CARTESIAN_POINT('Ctrl Pts',(-21.797909317082,19.2409551306886,13.2934994445093));
#62519=CARTESIAN_POINT('Ctrl Pts',(-26.1658556103503,19.7394668882666,13.0974255340282));
#62520=CARTESIAN_POINT('Ctrl Pts',(-27.4850767383724,22.3017466999325,12.9676472606722));
#62521=CARTESIAN_POINT('Ctrl Pts',(-27.4894316120893,23.5512575959394,12.9041646244411));
#62522=CARTESIAN_POINT('',(-27.4832508490902,23.5466144882414,11.654163534408));
#62523=CARTESIAN_POINT('Ctrl Pts',(-27.4832523980892,23.5512776836369,12.9041635220348));
#62524=CARTESIAN_POINT('Ctrl Pts',(-27.4832379908657,23.6065510591407,12.9013508886097));
#62525=CARTESIAN_POINT('Ctrl Pts',(-27.4820584429071,23.6618078252927,12.8985382551845));
#62526=CARTESIAN_POINT('Ctrl Pts',(-27.4797155131848,23.7170148688545,12.8957256217594));
#62527=CARTESIAN_POINT('Ctrl Pts',(-27.4748238771176,23.8322777224003,12.8898533247907));
#62528=CARTESIAN_POINT('Ctrl Pts',(-27.4648482421994,23.9475182605675,12.883981027822));
#62529=CARTESIAN_POINT('Ctrl Pts',(-27.449784054935,24.0622514567429,12.8781087308533));
#62530=CARTESIAN_POINT('Ctrl Pts',(-27.434739389661,24.1768359678079,12.8722440439151));
#62531=CARTESIAN_POINT('Ctrl Pts',(-27.4146193391729,24.2909140382808,12.8663793569769));
#62532=CARTESIAN_POINT('Ctrl Pts',(-27.3894713312815,24.4040019146487,12.8605146700387));
#62533=CARTESIAN_POINT('Ctrl Pts',(-27.364349186542,24.5169734872153,12.8546560145639));
#62534=CARTESIAN_POINT('Ctrl Pts',(-27.3342094588585,24.6289564901327,12.8487973590891));
#62535=CARTESIAN_POINT('Ctrl Pts',(-27.2991511371522,24.7394742292743,12.8429387036143));
#62536=CARTESIAN_POINT('Ctrl Pts',(-27.2627234065209,24.8543088886497,12.8368512038964));
#62537=CARTESIAN_POINT('Ctrl Pts',(-27.220985058488,24.9675610308767,12.8307637041785));
#62538=CARTESIAN_POINT('Ctrl Pts',(-27.1741052772868,25.0787093607415,12.8246762044606));
#62539=CARTESIAN_POINT('Ctrl Pts',(-27.1290400778058,25.185555457907,12.8188243343772));
#62540=CARTESIAN_POINT('Ctrl Pts',(-27.0792242401555,25.2904571630241,12.8129724642938));
#62541=CARTESIAN_POINT('Ctrl Pts',(-27.0248579799646,25.3929695416687,12.8071205942104));
#62542=CARTESIAN_POINT('Ctrl Pts',(-26.9704999975312,25.4954663118716,12.8012696151274));
#62543=CARTESIAN_POINT('Ctrl Pts',(-26.9115931637791,25.5955741138437,12.7954186360445));
#62544=CARTESIAN_POINT('Ctrl Pts',(-26.8483840962645,25.6928717658992,12.7895676569615));
#62545=CARTESIAN_POINT('Ctrl Pts',(-26.7851693456465,25.7901781659498,12.7837161518192));
#62546=CARTESIAN_POINT('Ctrl Pts',(-26.717651817535,25.8846735671451,12.7778646466769));
#62547=CARTESIAN_POINT('Ctrl Pts',(-26.6461215837537,25.9759655840769,12.7720131415347));
#62548=CARTESIAN_POINT('Ctrl Pts',(-26.574567596339,26.0672879171002,12.7661596932349));
#62549=CARTESIAN_POINT('Ctrl Pts',(-26.4989985084209,26.1554044253891,12.7603062449352));
#62550=CARTESIAN_POINT('Ctrl Pts',(-26.4197443382093,26.2399561905277,12.7544527966354));
#62551=CARTESIAN_POINT('Ctrl Pts',(-26.3404000387964,26.3246041093836,12.7485926916939));
#62552=CARTESIAN_POINT('Ctrl Pts',(-26.2573625753744,26.4056788918726,12.7427325867523));
#62553=CARTESIAN_POINT('Ctrl Pts',(-26.1709985190359,26.4828587906101,12.7368724818108));
#62554=CARTESIAN_POINT('Ctrl Pts',(-26.0845763019109,26.5600906651786,12.7310084304554));
#62555=CARTESIAN_POINT('Ctrl Pts',(-25.9948233504204,26.6334221722495,12.7251443791));
#62556=CARTESIAN_POINT('Ctrl Pts',(-25.9021375771657,26.7025732217395,12.7192803277445));
#62557=CARTESIAN_POINT('Ctrl Pts',(-25.8093152035831,26.7718261860726,12.713407633948));
#62558=CARTESIAN_POINT('Ctrl Pts',(-25.7135517222237,26.8368861649056,12.7075349401514));
#62559=CARTESIAN_POINT('Ctrl Pts',(-25.6152721875023,26.8975175079287,12.7016622463549));
#62560=CARTESIAN_POINT('Ctrl Pts',(-25.5883648949098,26.914117355411,12.7000544010314));
#62561=CARTESIAN_POINT('Ctrl Pts',(-25.5612691343649,26.930385517104,12.698446555708));
#62562=CARTESIAN_POINT('Ctrl Pts',(-25.5339939027177,26.946317780315,12.6968387103846));
#62563=CARTESIAN_POINT('Ctrl Pts',(-25.4343771934553,27.0045068234994,12.6909664134159));
#62564=CARTESIAN_POINT('Ctrl Pts',(-25.3320311415903,27.0584065507417,12.6850941164472));
#62565=CARTESIAN_POINT('Ctrl Pts',(-25.2273613467932,27.1077509536639,12.6792218194784));
#62566=CARTESIAN_POINT('Ctrl Pts',(-25.1228271957375,27.1570314101588,12.6733571325402));
#62567=CARTESIAN_POINT('Ctrl Pts',(-25.0159756607799,27.2017681073074,12.667492445602));
#62568=CARTESIAN_POINT('Ctrl Pts',(-24.90723936861,27.2417394576412,12.6616277586638));
#62569=CARTESIAN_POINT('Ctrl Pts',(-24.7986149049096,27.2816696999434,12.655769103189));
#62570=CARTESIAN_POINT('Ctrl Pts',(-24.6881099251499,27.3168442017248,12.6499104477142));
#62571=CARTESIAN_POINT('Ctrl Pts',(-24.5761789878059,27.3470885706416,12.6440517922394));
#62572=CARTESIAN_POINT('Ctrl Pts',(-24.4598759294618,27.3785143112472,12.6379642925215));
#62573=CARTESIAN_POINT('Ctrl Pts',(-24.3420336555078,27.4046167227236,12.6318767928036));
#62574=CARTESIAN_POINT('Ctrl Pts',(-24.2231821916042,27.4252563604424,12.6257892930856));
#62575=CARTESIAN_POINT('Ctrl Pts',(-24.1089311265996,27.4450970970496,12.6199374230022));
#62576=CARTESIAN_POINT('Ctrl Pts',(-23.9937479899243,27.4598900157267,12.6140855529188));
#62577=CARTESIAN_POINT('Ctrl Pts',(-23.8781153374098,27.4695630553231,12.6082336828354));
#62578=CARTESIAN_POINT('Ctrl Pts',(-23.7625002910182,27.4792346221113,12.6023827037525));
#62579=CARTESIAN_POINT('Ctrl Pts',(-23.6464362767046,27.4837878253591,12.5965317246695));
#62580=CARTESIAN_POINT('Ctrl Pts',(-23.530410948932,27.4832024819978,12.5906807455865));
#62581=CARTESIAN_POINT('Ctrl Pts',(-23.4143751893657,27.4826170860086,12.5848292404442));
#62582=CARTESIAN_POINT('Ctrl Pts',(-23.2983785366571,27.476892227073,12.5789777353019));
#62583=CARTESIAN_POINT('Ctrl Pts',(-23.1829079073513,27.4660598465357,12.5731262301596));
#62584=CARTESIAN_POINT('Ctrl Pts',(-23.0673989327634,27.4552238688007,12.5672727818599));
#62585=CARTESIAN_POINT('Ctrl Pts',(-22.9524167402783,27.4392770354723,12.5614193335601));
#62586=CARTESIAN_POINT('Ctrl Pts',(-22.8384416828144,27.4183029857882,12.5555658852603));
#62587=CARTESIAN_POINT('Ctrl Pts',(-22.7243370109608,27.3973050840553,12.5497057803188));
#62588=CARTESIAN_POINT('Ctrl Pts',(-22.6112421669724,27.3712686297945,12.5438456753772));
#62589=CARTESIAN_POINT('Ctrl Pts',(-22.4996259895379,27.3403281073149,12.5379855704357));
#62590=CARTESIAN_POINT('Ctrl Pts',(-22.3879346455937,27.30936674833,12.5321215190802));
#62591=CARTESIAN_POINT('Ctrl Pts',(-22.2777243431423,27.2734948726586,12.5262574677248));
#62592=CARTESIAN_POINT('Ctrl Pts',(-22.1694458152998,27.2328958502848,12.5203934163693));
#62593=CARTESIAN_POINT('Ctrl Pts',(-22.0610077065216,27.1922369930563,12.5145207225728));
#62594=CARTESIAN_POINT('Ctrl Pts',(-21.9545074333599,27.1468372460926,12.5086480287762));
#62595=CARTESIAN_POINT('Ctrl Pts',(-21.8503730123046,27.0969268358219,12.5027753349796));
#62596=CARTESIAN_POINT('Ctrl Pts',(-21.8218627497758,27.083262200389,12.5011674896563));
#62597=CARTESIAN_POINT('Ctrl Pts',(-21.7935296651487,27.0692597134755,12.499559644333));
#62598=CARTESIAN_POINT('Ctrl Pts',(-21.765382165811,27.0549246671431,12.4979517990096));
#62599=CARTESIAN_POINT('Ctrl Pts',(-21.6625796930614,27.0025691028966,12.4920795020409));
#62600=CARTESIAN_POINT('Ctrl Pts',(-21.5619105683994,26.9455987398214,12.4862072050722));
#62601=CARTESIAN_POINT('Ctrl Pts',(-21.4638178329529,26.88421102692,12.4803349081035));
#62602=CARTESIAN_POINT('Ctrl Pts',(-21.3658522179012,26.8229028676193,12.4744702211653));
#62603=CARTESIAN_POINT('Ctrl Pts',(-21.2704566995842,26.75718895981,12.4686055342271));
#62604=CARTESIAN_POINT('Ctrl Pts',(-21.1780515563226,26.6873135021642,12.4627408472889));
#62605=CARTESIAN_POINT('Ctrl Pts',(-21.0857414459664,26.6175099070524,12.456882191814));
#62606=CARTESIAN_POINT('Ctrl Pts',(-20.9964159212524,26.5435535228665,12.4510235363392));
#62607=CARTESIAN_POINT('Ctrl Pts',(-20.9104674095115,26.4657325108234,12.4451648808644));
#62608=CARTESIAN_POINT('Ctrl Pts',(-20.8211616731997,26.3848717415061,12.4390773811465));
#62609=CARTESIAN_POINT('Ctrl Pts',(-20.7355025317112,26.2998385192045,12.4329898814286));
#62610=CARTESIAN_POINT('Ctrl Pts',(-20.6538938034904,26.2110033876666,12.4269023817107));
#62611=CARTESIAN_POINT('Ctrl Pts',(-20.5754439148086,26.1256068089902,12.4210505116273));
#62612=CARTESIAN_POINT('Ctrl Pts',(-20.5007370157935,26.0366975031954,12.4151986415439));
#62613=CARTESIAN_POINT('Ctrl Pts',(-20.4300945745843,25.9446425004928,12.4093467714605));
#62614=CARTESIAN_POINT('Ctrl Pts',(-20.359462889329,25.8526015140015,12.4034957923775));
#62615=CARTESIAN_POINT('Ctrl Pts',(-20.2928946830025,25.7574161107881,12.3976448132945));
#62616=CARTESIAN_POINT('Ctrl Pts',(-20.2306705338695,25.65948565293,12.3917938342115));
#62617=CARTESIAN_POINT('Ctrl Pts',(-20.1684407901866,25.5615463901813,12.3859423290692));
#62618=CARTESIAN_POINT('Ctrl Pts',(-20.1105561018261,25.4608619310883,12.3800908239269));
#62619=CARTESIAN_POINT('Ctrl Pts',(-20.0572527950333,25.3578591923609,12.3742393187846));
#62620=CARTESIAN_POINT('Ctrl Pts',(-20.0039317873726,25.2548222486663,12.3683858704849));
#62621=CARTESIAN_POINT('Ctrl Pts',(-19.9551953763324,25.1494658614805,12.3625324221851));
#62622=CARTESIAN_POINT('Ctrl Pts',(-19.9112328459345,25.042239370327,12.3566789738853));
#62623=CARTESIAN_POINT('Ctrl Pts',(-19.8672203205933,24.9348909393693,12.3508188689438));
#62624=CARTESIAN_POINT('Ctrl Pts',(-19.8279926688025,24.825668542297,12.3449587640022));
#62625=CARTESIAN_POINT('Ctrl Pts',(-19.7936901738434,24.7150393154355,12.3390986590607));
#62626=CARTESIAN_POINT('Ctrl Pts',(-19.7593645783008,24.6043355867136,12.3332346077052));
#62627=CARTESIAN_POINT('Ctrl Pts',(-19.729970848549,24.4922235406083,12.3273705563498));
#62628=CARTESIAN_POINT('Ctrl Pts',(-19.7055983527011,24.3791815057026,12.3215065049943));
#62629=CARTESIAN_POINT('Ctrl Pts',(-19.6811899366595,24.2659728694028,12.3156338111977));
#62630=CARTESIAN_POINT('Ctrl Pts',(-19.6618175929974,24.1518319148381,12.3097611174012));
#62631=CARTESIAN_POINT('Ctrl Pts',(-19.6475189894155,24.0372431866074,12.3038884236046));
#62632=CARTESIAN_POINT('Ctrl Pts',(-19.6436042709413,24.0058707096541,12.3022805782813));
#62633=CARTESIAN_POINT('Ctrl Pts',(-19.6400695647533,23.9744646723945,12.300672732958));
#62634=CARTESIAN_POINT('Ctrl Pts',(-19.6369149631006,23.9430350086886,12.2990648876347));
#62635=CARTESIAN_POINT('Ctrl Pts',(-19.6253934831084,23.8282451615342,12.293192590666));
#62636=CARTESIAN_POINT('Ctrl Pts',(-19.6189076758795,23.7127556415175,12.2873202936973));
#62637=CARTESIAN_POINT('Ctrl Pts',(-19.6175309067666,23.5970459161294,12.2814479967286));
#62638=CARTESIAN_POINT('Ctrl Pts',(-19.6161559218371,23.4814861413559,12.2755833097904));
#62639=CARTESIAN_POINT('Ctrl Pts',(-19.6198768132877,23.3657071382451,12.2697186228522));
#62640=CARTESIAN_POINT('Ctrl Pts',(-19.6287153109279,23.2501944937346,12.263853935914));
#62641=CARTESIAN_POINT('Ctrl Pts',(-19.6375447187264,23.1348006467478,12.2579952804392));
#62642=CARTESIAN_POINT('Ctrl Pts',(-19.6514812327148,23.0196730231942,12.2521366249644));
#62643=CARTESIAN_POINT('Ctrl Pts',(-19.6704945416348,22.9052975421252,12.2462779694896));
#62644=CARTESIAN_POINT('Ctrl Pts',(-19.6902505271479,22.786454454025,12.2401904697717));
#62645=CARTESIAN_POINT('Ctrl Pts',(-19.7154880064553,22.6684239196124,12.2341029700538));
#62646=CARTESIAN_POINT('Ctrl Pts',(-19.746113515873,22.5517459727239,12.2280154703359));
#62647=CARTESIAN_POINT('Ctrl Pts',(-19.7755535997588,22.439584294132,12.2221636002525));
#62648=CARTESIAN_POINT('Ctrl Pts',(-19.8099722444983,22.3286728776249,12.2163117301691));
#62649=CARTESIAN_POINT('Ctrl Pts',(-19.8492344285741,22.2194805751301,12.2104598600857));
#62650=CARTESIAN_POINT('Ctrl Pts',(-19.8884906346254,22.1103048981562,12.2046088810027));
#62651=CARTESIAN_POINT('Ctrl Pts',(-19.9325887738469,22.0028482036436,12.1987579019198));
#62652=CARTESIAN_POINT('Ctrl Pts',(-19.9813445206688,21.8975624189269,12.1929069228368));
#62653=CARTESIAN_POINT('Ctrl Pts',(-20.0301046511016,21.7922671680048,12.1870554176945));
#62654=CARTESIAN_POINT('Ctrl Pts',(-20.0835230478802,21.6891435900266,12.1812039125522));
#62655=CARTESIAN_POINT('Ctrl Pts',(-20.1413682831677,21.5886212768077,12.1753524074099));
#62656=CARTESIAN_POINT('Ctrl Pts',(-20.1992327275986,21.4880655823168,12.1694989591101));
#62657=CARTESIAN_POINT('Ctrl Pts',(-20.261526727583,21.3901132283489,12.1636455108104));
#62658=CARTESIAN_POINT('Ctrl Pts',(-20.3279745622788,21.2951663497889,12.1577920625106));
#62659=CARTESIAN_POINT('Ctrl Pts',(-20.3944979625915,21.2001114960107,12.1519319575691));
#62660=CARTESIAN_POINT('Ctrl Pts',(-20.4651843890375,21.1080692785043,12.1460718526275));
#62661=CARTESIAN_POINT('Ctrl Pts',(-20.5397166610491,21.019410226935,12.140211747686));
#62662=CARTESIAN_POINT('Ctrl Pts',(-20.614299125881,20.9306914690434,12.1343476963305));
#62663=CARTESIAN_POINT('Ctrl Pts',(-20.6927323142933,20.845360717341,12.1284836449751));
#62664=CARTESIAN_POINT('Ctrl Pts',(-20.7746621076773,20.7637517155979,12.1226195936196));
#62665=CARTESIAN_POINT('Ctrl Pts',(-20.8567126492219,20.6820224384769,12.1167468998231));
#62666=CARTESIAN_POINT('Ctrl Pts',(-20.9422697763807,20.6040261359993,12.1108742060265));
#62667=CARTESIAN_POINT('Ctrl Pts',(-21.0309461946421,20.5300564155307,12.10500151223));
#62668=CARTESIAN_POINT('Ctrl Pts',(-21.0552243145874,20.5098047434282,12.1033936669066));
#62669=CARTESIAN_POINT('Ctrl Pts',(-21.0797360821321,20.4898546412696,12.1017858215832));
#62670=CARTESIAN_POINT('Ctrl Pts',(-21.1044731896175,20.4702115563383,12.1001779762598));
#62671=CARTESIAN_POINT('Ctrl Pts',(-21.1948199656351,20.3984695632366,12.0943056792911));
#62672=CARTESIAN_POINT('Ctrl Pts',(-21.2884773827769,20.3305859632771,12.0884333823224));
#62673=CARTESIAN_POINT('Ctrl Pts',(-21.3850817140814,20.2668816524669,12.0825610853537));
#62674=CARTESIAN_POINT('Ctrl Pts',(-21.4815608538448,20.2032598973842,12.0766963984155));
#62675=CARTESIAN_POINT('Ctrl Pts',(-21.5809789712995,20.1438068863899,12.0708317114773));
#62676=CARTESIAN_POINT('Ctrl Pts',(-21.682939279891,20.0888033814625,12.0649670245391));
#62677=CARTESIAN_POINT('Ctrl Pts',(-21.7847947286877,20.0338564441966,12.0591083690643));
#62678=CARTESIAN_POINT('Ctrl Pts',(-21.8891868066446,19.9833501061082,12.0532497135895));
#62679=CARTESIAN_POINT('Ctrl Pts',(-21.9956903173906,19.937521525674,12.0473910581146));
#62680=CARTESIAN_POINT('Ctrl Pts',(-22.1063539490735,19.8899028405228,12.0413035583967));
#62681=CARTESIAN_POINT('Ctrl Pts',(-22.2192969454787,19.8473350477852,12.0352160586788));
#62682=CARTESIAN_POINT('Ctrl Pts',(-22.3340144459951,19.8100314260783,12.0291285589609));
#62683=CARTESIAN_POINT('Ctrl Pts',(-22.444291561465,19.7741717204544,12.0232766888775));
#62684=CARTESIAN_POINT('Ctrl Pts',(-22.5562079336631,19.7431763812675,12.0174248187941));
#62685=CARTESIAN_POINT('Ctrl Pts',(-22.6692961247427,19.7171852469924,12.0115729487107));
#62686=CARTESIAN_POINT('Ctrl Pts',(-22.7823670971168,19.6911980701039,12.0057219696278));
#62687=CARTESIAN_POINT('Ctrl Pts',(-22.8966091308473,19.6702136757237,11.9998709905448));
#62688=CARTESIAN_POINT('Ctrl Pts',(-23.0115423761006,19.6543212735403,11.9940200114618));
#62689=CARTESIAN_POINT('Ctrl Pts',(-23.1264859549587,19.6384274424771,11.9881685063195));
#62690=CARTESIAN_POINT('Ctrl Pts',(-23.24212045937,19.627626570338,11.9823170011772));
#62691=CARTESIAN_POINT('Ctrl Pts',(-23.3579593699759,19.6219561655889,11.9764654960349));
#62692=CARTESIAN_POINT('Ctrl Pts',(-23.4738367481622,19.6162838778217,11.9706120477352));
#62693=CARTESIAN_POINT('Ctrl Pts',(-23.5899182548459,19.6157454653782,11.9647585994354));
#62694=CARTESIAN_POINT('Ctrl Pts',(-23.7057165283975,19.6203263306404,11.9589051511356));
#62695=CARTESIAN_POINT('Ctrl Pts',(-23.8216464897311,19.6249124053412,11.9530450461941));
#62696=CARTESIAN_POINT('Ctrl Pts',(-23.9372921617307,19.6346293613958,11.9471849412525));
#62697=CARTESIAN_POINT('Ctrl Pts',(-24.052170362029,19.6494106364629,11.941324836311));
#62698=CARTESIAN_POINT('Ctrl Pts',(-24.1671259256053,19.6642018657936,11.9354607849556));
#62699=CARTESIAN_POINT('Ctrl Pts',(-24.2813125820686,19.6840641344538,11.9295967336001));
#62700=CARTESIAN_POINT('Ctrl Pts',(-24.3942581310656,19.7088799191728,11.9237326822447));
#62701=CARTESIAN_POINT('Ctrl Pts',(-24.5073701392558,19.7337322774047,11.9178599884481));
#62702=CARTESIAN_POINT('Ctrl Pts',(-24.619236991425,19.763552615995,11.9119872946515));
#62703=CARTESIAN_POINT('Ctrl Pts',(-24.7294023216681,19.798173804801,11.9061146008549));
#62704=CARTESIAN_POINT('Ctrl Pts',(-24.7595637462479,19.8076525071543,11.9045067555316));
#62705=CARTESIAN_POINT('Ctrl Pts',(-24.7895977514064,19.8174907924924,11.9028989102083));
#62706=CARTESIAN_POINT('Ctrl Pts',(-24.8194952636113,19.8276846159302,11.9012910648849));
#62707=CARTESIAN_POINT('Ctrl Pts',(-24.928689268622,19.8649152858239,11.8954187679162));
#62708=CARTESIAN_POINT('Ctrl Pts',(-25.0364266846208,19.9070168787045,11.8895464709475));
#62709=CARTESIAN_POINT('Ctrl Pts',(-25.1422409265707,19.953856842872,11.8836741739788));
#62710=CARTESIAN_POINT('Ctrl Pts',(-25.2479180416664,20.0006361061659,11.8778094870406));
#62711=CARTESIAN_POINT('Ctrl Pts',(-25.3516765644506,20.0521413636079,11.8719448001024));
#62712=CARTESIAN_POINT('Ctrl Pts',(-25.4530658052064,20.1081905557638,11.8660801131642));
#62713=CARTESIAN_POINT('Ctrl Pts',(-25.5543507734753,20.1641821048344,11.8602214576893));
#62714=CARTESIAN_POINT('Ctrl Pts',(-25.653270946747,20.2247080946832,11.8543628022145));
#62715=CARTESIAN_POINT('Ctrl Pts',(-25.7493969629523,20.2895389946802,11.8485041467397));
#62716=CARTESIAN_POINT('Ctrl Pts',(-25.849277746017,20.3569022467331,11.8424166470218));
#62717=CARTESIAN_POINT('Ctrl Pts',(-25.9461412218104,20.4289133880428,11.8363291473039));
#62718=CARTESIAN_POINT('Ctrl Pts',(-26.039535056891,20.5052629570404,11.830241647586));
#62719=CARTESIAN_POINT('Ctrl Pts',(-26.1293138847856,20.5786572534516,11.8243897775026));
#62720=CARTESIAN_POINT('Ctrl Pts',(-26.2158863273361,20.6560600803264,11.8185379074192));
#62721=CARTESIAN_POINT('Ctrl Pts',(-26.2988820661146,20.7371537629853,11.8126860373358));
#62722=CARTESIAN_POINT('Ctrl Pts',(-26.3818651680374,20.8182350983937,11.8068350582528));
#62723=CARTESIAN_POINT('Ctrl Pts',(-26.4612723534058,20.9030058833983,11.8009840791698));
#62724=CARTESIAN_POINT('Ctrl Pts',(-26.5367691894349,20.9911106339017,11.7951331000868));
#62725=CARTESIAN_POINT('Ctrl Pts',(-26.6122728133561,21.0792233058699,11.7892815949445));
#62726=CARTESIAN_POINT('Ctrl Pts',(-26.6838651200353,21.1706702253029,11.7834300898022));
#62727=CARTESIAN_POINT('Ctrl Pts',(-26.7512515686327,21.2650623502172,11.7775785846599));
#62728=CARTESIAN_POINT('Ctrl Pts',(-26.8186603948028,21.3594858207015,11.7717251363601));
#62729=CARTESIAN_POINT('Ctrl Pts',(-26.8818603456322,21.4568561051683,11.7658716880603));
#62730=CARTESIAN_POINT('Ctrl Pts',(-26.9406002627201,21.5567552874704,11.7600182397605));
#62731=CARTESIAN_POINT('Ctrl Pts',(-26.9994069798488,21.6567680768355,11.754158134819));
#62732=CARTESIAN_POINT('Ctrl Pts',(-27.0537433299704,21.7593151476993,11.7482980298774));
#62733=CARTESIAN_POINT('Ctrl Pts',(-27.1034041325464,21.8639540108619,11.7424379249359));
#62734=CARTESIAN_POINT('Ctrl Pts',(-27.1530983785649,21.9686633417498,11.7365738735804));
#62735=CARTESIAN_POINT('Ctrl Pts',(-27.1981106472213,22.0754668899169,11.7307098222249));
#62736=CARTESIAN_POINT('Ctrl Pts',(-27.2382845685065,22.1839038589733,11.7248457708695));
#62737=CARTESIAN_POINT('Ctrl Pts',(-27.2785176981321,22.2925006424758,11.7189730770729));
#62738=CARTESIAN_POINT('Ctrl Pts',(-27.3138981229128,22.4027352593177,11.7131003832763));
#62739=CARTESIAN_POINT('Ctrl Pts',(-27.3443197671237,22.5141334202786,11.7072276894797));
#62740=CARTESIAN_POINT('Ctrl Pts',(-27.3526487044162,22.5446323732845,11.7056198441565));
#62741=CARTESIAN_POINT('Ctrl Pts',(-27.3606062429117,22.5752184960405,11.7040119988332));
#62742=CARTESIAN_POINT('Ctrl Pts',(-27.3681908810109,22.6058819683997,11.70240415351));
#62743=CARTESIAN_POINT('Ctrl Pts',(-27.4061182065104,22.7592160473512,11.6943640503263));
#62744=CARTESIAN_POINT('Ctrl Pts',(-27.4348232418154,22.9149150857894,11.6863239471426));
#62745=CARTESIAN_POINT('Ctrl Pts',(-27.4540696900141,23.0720260221748,11.6782838439589));
#62746=CARTESIAN_POINT('Ctrl Pts',(-27.4722823314705,23.2206978770397,11.6706756081408));
#62747=CARTESIAN_POINT('Ctrl Pts',(-27.4820254920152,23.370634264891,11.6630673723228));
#62748=CARTESIAN_POINT('Ctrl Pts',(-27.4831437745779,23.5210040847501,11.6554591365047));
#62749=CARTESIAN_POINT('Ctrl Pts',(-27.4832072518091,23.5295395480976,11.6550272691391));
#62750=CARTESIAN_POINT('Ctrl Pts',(-27.4832429513159,23.5380764008163,11.6545954017735));
#62751=CARTESIAN_POINT('Ctrl Pts',(-27.4832508490902,23.5466144882414,11.654163534408));
#62752=CARTESIAN_POINT('',(-27.4768104533793,23.5508499486531,10.4041635220348));
#62753=CARTESIAN_POINT('Ctrl Pts',(-27.4828563374966,23.5466150977616,11.6541635220348));
#62754=CARTESIAN_POINT('Ctrl Pts',(-27.4737453654797,24.5392918724205,11.6039480954016));
#62755=CARTESIAN_POINT('Ctrl Pts',(-26.5880752141214,26.8569989905617,11.4874370316434));
#62756=CARTESIAN_POINT('Ctrl Pts',(-22.6892863486302,28.1218483213199,11.3046303307602));
#62757=CARTESIAN_POINT('Ctrl Pts',(-19.2387035696249,25.2970485643742,11.1057434193855));
#62758=CARTESIAN_POINT('Ctrl Pts',(-19.7500687276925,20.8670913572745,10.9068565080105));
#62759=CARTESIAN_POINT('Ctrl Pts',(-23.7534805991851,18.9027317749154,10.7079695966357));
#62760=CARTESIAN_POINT('Ctrl Pts',(-26.96905917351,20.8458290658098,10.5404052679771));
#62761=CARTESIAN_POINT('Ctrl Pts',(-27.4758729437841,22.8568035385642,10.4391365764434));
#62762=CARTESIAN_POINT('Ctrl Pts',(-27.4768104533793,23.5508499486531,10.4041635220348));
#62763=CARTESIAN_POINT('',(-27.4833612647152,23.5536820313857,9.15416357631301));
#62764=CARTESIAN_POINT('Ctrl Pts',(-27.4768104533793,23.5508499486531,10.4041635220348));
#62765=CARTESIAN_POINT('Ctrl Pts',(-27.4776501061447,24.172452106559,10.3728409393185));
#62766=CARTESIAN_POINT('Ctrl Pts',(-27.0450601870018,26.1085981990694,10.2752227194772));
#62767=CARTESIAN_POINT('Ctrl Pts',(-24.0088794396662,28.1795518513951,10.1113088625109));
#62768=CARTESIAN_POINT('Ctrl Pts',(-19.9034526288354,26.4384355765543,9.91242195113609));
#62769=CARTESIAN_POINT('Ctrl Pts',(-19.1491257310881,22.0433239610247,9.71353503976112));
#62770=CARTESIAN_POINT('Ctrl Pts',(-22.4390612090823,19.032951935469,9.51464812838629));
#62771=CARTESIAN_POINT('Ctrl Pts',(-26.4806567721111,20.1023081666841,9.32819125204667));
#62772=CARTESIAN_POINT('Ctrl Pts',(-27.4753001046528,22.4903580385635,9.20803001283191));
#62773=CARTESIAN_POINT('Ctrl Pts',(-27.4850558365148,23.5536670379096,9.15416441074218));
#62774=CARTESIAN_POINT('',(-27.484942279697,23.5480589111923,7.90416291743633));
#62775=CARTESIAN_POINT('Ctrl Pts',(-27.4832510356148,23.5536830066866,9.15416352203477));
#62776=CARTESIAN_POINT('Ctrl Pts',(-27.4831009438724,23.7257613921932,9.14544221748674));
#62777=CARTESIAN_POINT('Ctrl Pts',(-27.4716543896873,23.89736605375,9.1367209129387));
#62778=CARTESIAN_POINT('Ctrl Pts',(-27.4491156108634,24.0673170246647,9.12799960839067));
#62779=CARTESIAN_POINT('Ctrl Pts',(-27.4395317717813,24.1395828190911,9.12429117413927));
#62780=CARTESIAN_POINT('Ctrl Pts',(-27.4279428892403,24.2115500617344,9.12058273988788));
#62781=CARTESIAN_POINT('Ctrl Pts',(-27.4143669509749,24.2831295709763,9.11687430563648));
#62782=CARTESIAN_POINT('Ctrl Pts',(-27.3928694844651,24.3964755565454,9.11100200866777));
#62783=CARTESIAN_POINT('Ctrl Pts',(-27.3663446125213,24.5090647482891,9.10512971169906));
#62784=CARTESIAN_POINT('Ctrl Pts',(-27.3348579229357,24.6204165530412,9.09925741473035));
#62785=CARTESIAN_POINT('Ctrl Pts',(-27.3034120375993,24.7316240546977,9.09339272779215));
#62786=CARTESIAN_POINT('Ctrl Pts',(-27.2670172332676,24.8415969641444,9.08752804085395));
#62787=CARTESIAN_POINT('Ctrl Pts',(-27.2257903493916,24.9498634600155,9.08166335391575));
#62788=CARTESIAN_POINT('Ctrl Pts',(-27.1846058647847,25.0580186105734,9.07580469844092));
#62789=CARTESIAN_POINT('Ctrl Pts',(-27.1385993314306,25.1644704542212,9.0699460429661));
#62790=CARTESIAN_POINT('Ctrl Pts',(-27.0879375884499,25.2687616062142,9.06408738749128));
#62791=CARTESIAN_POINT('Ctrl Pts',(-27.035296953166,25.3771264624625,9.05799988777337));
#62792=CARTESIAN_POINT('Ctrl Pts',(-26.9776301449224,25.4831579513821,9.05191238805547));
#62793=CARTESIAN_POINT('Ctrl Pts',(-26.9151799068011,25.5863646995907,9.04582488833756));
#62794=CARTESIAN_POINT('Ctrl Pts',(-26.8551469380786,25.6855766109227,9.03997301825416));
#62795=CARTESIAN_POINT('Ctrl Pts',(-26.7906941935824,25.7821780039988,9.03412114817076));
#62796=CARTESIAN_POINT('Ctrl Pts',(-26.722084086784,25.8757575491338,9.02826927808736));
#62797=CARTESIAN_POINT('Ctrl Pts',(-26.6534844264982,25.9693228459322,9.02241829900439));
#62798=CARTESIAN_POINT('Ctrl Pts',(-26.5807289068674,26.0598668763354,9.01656731992142));
#62799=CARTESIAN_POINT('Ctrl Pts',(-26.5041224235725,26.1470085198177,9.01071634083845));
#62800=CARTESIAN_POINT('Ctrl Pts',(-26.4275090526175,26.2341579981722,9.00486483569616));
#62801=CARTESIAN_POINT('Ctrl Pts',(-26.3470443026595,26.3179041710017,8.99901333055387));
#62802=CARTESIAN_POINT('Ctrl Pts',(-26.2630719060061,26.3979006915549,8.99316182541158));
#62803=CARTESIAN_POINT('Ctrl Pts',(-26.1790716239477,26.4779237772112,8.98730837711181));
#62804=CARTESIAN_POINT('Ctrl Pts',(-26.0915616781838,26.5541944496501,8.98145492881204));
#62805=CARTESIAN_POINT('Ctrl Pts',(-26.000920491604,26.626405250639,8.97560148051227));
#62806=CARTESIAN_POINT('Ctrl Pts',(-25.9101762263126,26.698698170989,8.96974137557073));
#62807=CARTESIAN_POINT('Ctrl Pts',(-25.8162939362699,26.7669217468522,8.96388127062918));
#62808=CARTESIAN_POINT('Ctrl Pts',(-25.719682841778,26.8308105832595,8.95802116568764));
#62809=CARTESIAN_POINT('Ctrl Pts',(-25.6230066857607,26.8947424447994,8.9521571143322));
#62810=CARTESIAN_POINT('Ctrl Pts',(-25.5235984198017,26.9543335422019,8.94629306297675));
#62811=CARTESIAN_POINT('Ctrl Pts',(-25.4218922566159,27.0093642298177,8.94042901162131));
#62812=CARTESIAN_POINT('Ctrl Pts',(-25.320036198848,27.064476021682,8.93455631782474));
#62813=CARTESIAN_POINT('Ctrl Pts',(-25.2158758552907,27.1150138098997,8.92868362402817));
#62814=CARTESIAN_POINT('Ctrl Pts',(-25.1098658733538,27.1608058444868,8.9228109302316));
#62815=CARTESIAN_POINT('Ctrl Pts',(-25.0808421136298,27.1733429375496,8.92120308490826));
#62816=CARTESIAN_POINT('Ctrl Pts',(-25.0516797978485,27.1855245902506,8.91959523958493));
#62817=CARTESIAN_POINT('Ctrl Pts',(-25.0223884372128,27.1973479342965,8.91798739426159));
#62818=CARTESIAN_POINT('Ctrl Pts',(-24.9154082658157,27.2405300653095,8.91211509729288));
#62819=CARTESIAN_POINT('Ctrl Pts',(-24.8063472719977,27.2790734766344,8.90624280032417));
#62820=CARTESIAN_POINT('Ctrl Pts',(-24.6956452398352,27.3127735674012,8.90037050335546));
#62821=CARTESIAN_POINT('Ctrl Pts',(-24.5850866687145,27.3464299855268,8.89450581641726));
#62822=CARTESIAN_POINT('Ctrl Pts',(-24.4728916802176,27.3752554456401,8.88864112947905));
#62823=CARTESIAN_POINT('Ctrl Pts',(-24.3595203822524,27.3990932072812,8.88277644254084));
#62824=CARTESIAN_POINT('Ctrl Pts',(-24.24626567957,27.4229064532767,8.87691778706602));
#62825=CARTESIAN_POINT('Ctrl Pts',(-24.1318374758005,27.4417421191626,8.8710591315912));
#62826=CARTESIAN_POINT('Ctrl Pts',(-24.0167107600212,27.4554933336456,8.86520047611637));
#62827=CARTESIAN_POINT('Ctrl Pts',(-23.8970870933214,27.4697816826782,8.85911297639847));
#62828=CARTESIAN_POINT('Ctrl Pts',(-23.7767096681456,27.4785801441099,8.85302547668056));
#62829=CARTESIAN_POINT('Ctrl Pts',(-23.6561230980913,27.4818273336242,8.84693797696266));
#62830=CARTESIAN_POINT('Ctrl Pts',(-23.540204087913,27.4849488337563,8.84108610687926));
#62831=CARTESIAN_POINT('Ctrl Pts',(-23.4240922743701,27.4829408065889,8.83523423679586));
#62832=CARTESIAN_POINT('Ctrl Pts',(-23.3082755616338,27.4758016838461,8.82938236671245));
#62833=CARTESIAN_POINT('Ctrl Pts',(-23.1924764830452,27.4686636480996,8.82353138762948));
#62834=CARTESIAN_POINT('Ctrl Pts',(-23.0769728284111,27.4563960955909,8.81768040854651));
#62835=CARTESIAN_POINT('Ctrl Pts',(-22.9622500498651,27.439049528371,8.81182942946354));
#62836=CARTESIAN_POINT('Ctrl Pts',(-22.8475169566374,27.4217014015278,8.80597792432124));
#62837=CARTESIAN_POINT('Ctrl Pts',(-22.7335652878266,27.3992734139972,8.80012641917894));
#62838=CARTESIAN_POINT('Ctrl Pts',(-22.6208722326499,27.3718675384353,8.79427491403665));
#62839=CARTESIAN_POINT('Ctrl Pts',(-22.5081417545628,27.3444525619786,8.78842146573687));
#62840=CARTESIAN_POINT('Ctrl Pts',(-22.3966711226563,27.3120565081404,8.78256801743709));
#62841=CARTESIAN_POINT('Ctrl Pts',(-22.2869235603145,27.2748315562381,8.77671456913731));
#62842=CARTESIAN_POINT('Ctrl Pts',(-22.1770511911632,27.2375642714824,8.77085446419577));
#62843=CARTESIAN_POINT('Ctrl Pts',(-22.0689061943966,27.1954572606458,8.76499435925422));
#62844=CARTESIAN_POINT('Ctrl Pts',(-21.9629330521766,27.1487113504031,8.75913425431268));
#62845=CARTESIAN_POINT('Ctrl Pts',(-21.8568885436779,27.1019339597155,8.75327020295723));
#62846=CARTESIAN_POINT('Ctrl Pts',(-21.7530191716326,27.0505116320596,8.74740615160178));
#62847=CARTESIAN_POINT('Ctrl Pts',(-21.6517444379905,26.994690950093,8.74154210024633));
#62848=CARTESIAN_POINT('Ctrl Pts',(-21.5503204456075,26.938787999584,8.73566940644975));
#62849=CARTESIAN_POINT('Ctrl Pts',(-21.4514990750814,26.8784739719018,8.72979671265317));
#62850=CARTESIAN_POINT('Ctrl Pts',(-21.3556705787541,26.814038531393,8.7239240188566));
#62851=CARTESIAN_POINT('Ctrl Pts',(-21.3294343394752,26.7963971856553,8.7223161735333));
#62852=CARTESIAN_POINT('Ctrl Pts',(-21.3034222427136,26.7784471397982,8.72070832821001));
#62853=CARTESIAN_POINT('Ctrl Pts',(-21.2776418428209,26.7601948453221,8.71910048288671));
#62854=CARTESIAN_POINT('Ctrl Pts',(-21.1834846736277,26.6935324046191,8.713228185918));
#62855=CARTESIAN_POINT('Ctrl Pts',(-21.092105364407,26.62261190846,8.7073558889493));
#62856=CARTESIAN_POINT('Ctrl Pts',(-21.0039137712404,26.5476927591233,8.70148359198059));
#62857=CARTESIAN_POINT('Ctrl Pts',(-20.9158364673745,26.4728706990543,8.69561890504239));
#62858=CARTESIAN_POINT('Ctrl Pts',(-20.8309389765748,26.394060555986,8.68975421810419));
#62859=CARTESIAN_POINT('Ctrl Pts',(-20.7496018750497,26.3115647015578,8.68388953116599));
#62860=CARTESIAN_POINT('Ctrl Pts',(-20.6683484236418,26.2291536889516,8.67803087569118));
#62861=CARTESIAN_POINT('Ctrl Pts',(-20.5906483668093,26.1430647971276,8.67217222021636));
#62862=CARTESIAN_POINT('Ctrl Pts',(-20.5168483688969,26.0536398739016,8.66631356474154));
#62863=CARTESIAN_POINT('Ctrl Pts',(-20.4401656780638,25.9607219344098,8.66022606502364));
#62864=CARTESIAN_POINT('Ctrl Pts',(-20.3676942833698,25.8642023282843,8.65413856530574));
#62865=CARTESIAN_POINT('Ctrl Pts',(-20.2997802152074,25.7645060672571,8.64805106558783));
#62866=CARTESIAN_POINT('Ctrl Pts',(-20.2344949056159,25.6686687622276,8.64219919550444));
#62867=CARTESIAN_POINT('Ctrl Pts',(-20.1734209350139,25.5698965215311,8.63634732542104));
#62868=CARTESIAN_POINT('Ctrl Pts',(-20.1168233557066,25.4685989794134,8.63049545533765));
#62869=CARTESIAN_POINT('Ctrl Pts',(-20.0602343938953,25.3673168607675,8.62464447625468));
#62870=CARTESIAN_POINT('Ctrl Pts',(-20.0081206697716,25.2635105659856,8.61879349717172));
#62871=CARTESIAN_POINT('Ctrl Pts',(-19.9607021025708,25.1576158125924,8.61294251808875));
#62872=CARTESIAN_POINT('Ctrl Pts',(-19.9132792719845,25.0517115382418,8.60709101294646));
#62873=CARTESIAN_POINT('Ctrl Pts',(-19.87055260645,24.943718809312,8.60123950780416));
#62874=CARTESIAN_POINT('Ctrl Pts',(-19.832694255662,24.8340942136413,8.59538800266187));
#62875=CARTESIAN_POINT('Ctrl Pts',(-19.79482333294,24.7244332140289,8.58953455436211));
#62876=CARTESIAN_POINT('Ctrl Pts',(-19.7618240744621,24.6131396606585,8.58368110606234));
#62877=CARTESIAN_POINT('Ctrl Pts',(-19.7338188410917,24.500685530508,8.57782765776258));
#62878=CARTESIAN_POINT('Ctrl Pts',(-19.7057817596898,24.3881035155926,8.57196755282104));
#62879=CARTESIAN_POINT('Ctrl Pts',(-19.6827501390441,24.2743586909295,8.56610744787951));
#62880=CARTESIAN_POINT('Ctrl Pts',(-19.6647952817554,24.1599335621504,8.56024734293797));
#62881=CARTESIAN_POINT('Ctrl Pts',(-19.646828332994,24.0454313752086,8.55438329158253));
#62882=CARTESIAN_POINT('Ctrl Pts',(-19.6339450011017,23.9302483817159,8.54851924022708));
#62883=CARTESIAN_POINT('Ctrl Pts',(-19.6261645905391,23.8148708040808,8.54265518887164));
#62884=CARTESIAN_POINT('Ctrl Pts',(-19.6183727132044,23.6993231829279,8.53678249507507));
#62885=CARTESIAN_POINT('Ctrl Pts',(-19.6156987765524,23.5835808169997,8.5309098012785));
#62886=CARTESIAN_POINT('Ctrl Pts',(-19.6181100290429,23.4681286079983,8.52503710748194));
#62887=CARTESIAN_POINT('Ctrl Pts',(-19.6187701896395,23.4365197244525,8.52342926215857));
#62888=CARTESIAN_POINT('Ctrl Pts',(-19.6198112233587,23.404932550266,8.5218214168352));
#62889=CARTESIAN_POINT('Ctrl Pts',(-19.6212317858923,23.3733769283509,8.52021357151183));
#62890=CARTESIAN_POINT('Ctrl Pts',(-19.62642007418,23.2581270468949,8.51434127454312));
#62891=CARTESIAN_POINT('Ctrl Pts',(-19.6366922870426,23.1429125661555,8.50846897757441));
#62892=CARTESIAN_POINT('Ctrl Pts',(-19.6520517295779,23.0282185228594,8.5025966806057));
#62893=CARTESIAN_POINT('Ctrl Pts',(-19.6673912674956,22.9136731139346,8.4967319936675));
#62894=CARTESIAN_POINT('Ctrl Pts',(-19.6878048703177,22.7996472071662,8.49086730672929));
#62895=CARTESIAN_POINT('Ctrl Pts',(-19.7132438652852,22.6866244323931,8.48500261979109));
#62896=CARTESIAN_POINT('Ctrl Pts',(-19.7386566978389,22.5737178944686,8.47914396431627));
#62897=CARTESIAN_POINT('Ctrl Pts',(-19.769084552294,22.4618128373866,8.47328530884145));
#62898=CARTESIAN_POINT('Ctrl Pts',(-19.8044272131219,22.351385698913,8.46742665336663));
#62899=CARTESIAN_POINT('Ctrl Pts',(-19.8411503894112,22.2366451791477,8.46133915364872));
#62900=CARTESIAN_POINT('Ctrl Pts',(-19.8831800923618,22.1235008399813,8.45525165393082));
#62901=CARTESIAN_POINT('Ctrl Pts',(-19.930345796569,22.0124735394475,8.44916415421291));
#62902=CARTESIAN_POINT('Ctrl Pts',(-19.9756858517975,21.9057437869148,8.44331228412951));
#62903=CARTESIAN_POINT('Ctrl Pts',(-20.0257715249008,21.8009706473841,8.43746041404611));
#62904=CARTESIAN_POINT('Ctrl Pts',(-20.0804014557224,21.6985985384824,8.43160854396271));
#62905=CARTESIAN_POINT('Ctrl Pts',(-20.1350230686402,21.596242016665,8.42575756487973));
#62906=CARTESIAN_POINT('Ctrl Pts',(-20.1941873689816,21.496286163192,8.41990658579677));
#62907=CARTESIAN_POINT('Ctrl Pts',(-20.2576466559519,21.3991515235992,8.4140556067138));
#62908=CARTESIAN_POINT('Ctrl Pts',(-20.3211116485229,21.3020081506675,8.4082041015715));
#62909=CARTESIAN_POINT('Ctrl Pts',(-20.388872169267,21.2076868419514,8.4023525964292));
#62910=CARTESIAN_POINT('Ctrl Pts',(-20.4606371373831,21.1165792349602,8.3965010912869));
#62911=CARTESIAN_POINT('Ctrl Pts',(-20.5324259370829,21.0254413731161,8.39064764298712));
#62912=CARTESIAN_POINT('Ctrl Pts',(-20.6082215726991,20.9375196596236,8.38479419468735));
#62913=CARTESIAN_POINT('Ctrl Pts',(-20.6876931033152,20.853172162295,8.37894074638757));
#62914=CARTESIAN_POINT('Ctrl Pts',(-20.7672550103185,20.7687287435463,8.37308064144603));
#62915=CARTESIAN_POINT('Ctrl Pts',(-20.8505008724078,20.6878679549511,8.3672205365045));
#62916=CARTESIAN_POINT('Ctrl Pts',(-20.9370632915779,20.6109105993324,8.36136043156296));
#62917=CARTESIAN_POINT('Ctrl Pts',(-21.0236840051196,20.5339014177513,8.3554963802075));
#62918=CARTESIAN_POINT('Ctrl Pts',(-21.1136254030629,20.4608011635339,8.34963232885205));
#62919=CARTESIAN_POINT('Ctrl Pts',(-21.2064888532168,20.3918889016715,8.3437682774966));
#62920=CARTESIAN_POINT('Ctrl Pts',(-21.2994891655588,20.3228750768914,8.33789558370003));
#62921=CARTESIAN_POINT('Ctrl Pts',(-21.3954197838516,20.2580617936708,8.33202288990346));
#62922=CARTESIAN_POINT('Ctrl Pts',(-21.4938550485616,20.1976836075159,8.32615019610689));
#62923=CARTESIAN_POINT('Ctrl Pts',(-21.5208049774182,20.1811530701505,8.32454235078357));
#62924=CARTESIAN_POINT('Ctrl Pts',(-21.5479425198958,20.1649547025624,8.32293450546025));
#62925=CARTESIAN_POINT('Ctrl Pts',(-21.5752586683316,20.149092694274,8.32132666013692));
#62926=CARTESIAN_POINT('Ctrl Pts',(-21.6750248170582,20.0911602415446,8.31545436316821));
#62927=CARTESIAN_POINT('Ctrl Pts',(-21.7775092593236,20.0375241154475,8.3095820661995));
#62928=CARTESIAN_POINT('Ctrl Pts',(-21.882305712137,19.9884492795298,8.30370976923078));
#62929=CARTESIAN_POINT('Ctrl Pts',(-21.9869663570703,19.939438040702,8.29784508229258));
#62930=CARTESIAN_POINT('Ctrl Pts',(-22.0939326833089,19.8949765107511,8.29198039535437));
#62931=CARTESIAN_POINT('Ctrl Pts',(-22.2027714952651,19.8552851628986,8.28611570841616));
#62932=CARTESIAN_POINT('Ctrl Pts',(-22.3114983733167,19.8156346351127,8.28025705294133));
#62933=CARTESIAN_POINT('Ctrl Pts',(-22.4220935206719,19.7807446722469,8.2743983974665));
#62934=CARTESIAN_POINT('Ctrl Pts',(-22.5341019315029,19.7507884961056,8.26853974199168));
#62935=CARTESIAN_POINT('Ctrl Pts',(-22.6504854895165,19.7196622053393,8.26245224227378));
#62936=CARTESIAN_POINT('Ctrl Pts',(-22.7683945566312,19.693863187768,8.25636474255587));
#62937=CARTESIAN_POINT('Ctrl Pts',(-22.8872987500339,19.6735295233556,8.25027724283797));
#62938=CARTESIAN_POINT('Ctrl Pts',(-23.0016005035302,19.6539829167066,8.24442537275457));
#62939=CARTESIAN_POINT('Ctrl Pts',(-23.1168213333218,19.6394865102733,8.23857350267116));
#62940=CARTESIAN_POINT('Ctrl Pts',(-23.2324784997017,19.6301111229449,8.23272163258776));
#62941=CARTESIAN_POINT('Ctrl Pts',(-23.3481180562263,19.6207371631044,8.22687065350478));
#62942=CARTESIAN_POINT('Ctrl Pts',(-23.4641934053245,19.6164827054232,8.22101967442181));
#62943=CARTESIAN_POINT('Ctrl Pts',(-23.5802168422007,19.6173666777574,8.21516869533883));
#62944=CARTESIAN_POINT('Ctrl Pts',(-23.6962507107003,19.6182507295693,8.20931719019653));
#62945=CARTESIAN_POINT('Ctrl Pts',(-23.812232244304,19.624274126649,8.20346568505422));
#62946=CARTESIAN_POINT('Ctrl Pts',(-23.9276746102915,19.6354036745112,8.19761417991192));
#62947=CARTESIAN_POINT('Ctrl Pts',(-24.0431553121755,19.6465369182539,8.19176073161215));
#62948=CARTESIAN_POINT('Ctrl Pts',(-24.1580960791646,19.662779644807,8.18590728331237));
#62949=CARTESIAN_POINT('Ctrl Pts',(-24.2720167752056,19.6840469788571,8.1800538350126));
#62950=CARTESIAN_POINT('Ctrl Pts',(-24.3860670238156,19.7053384984841,8.17419373007105));
#62951=CARTESIAN_POINT('Ctrl Pts',(-24.499094479465,19.7316659548117,8.1683336251295));
#62952=CARTESIAN_POINT('Ctrl Pts',(-24.6106306511595,19.7628936572595,8.16247352018795));
#62953=CARTESIAN_POINT('Ctrl Pts',(-24.7222419354847,19.7941423896104,8.1566094688325));
#62954=CARTESIAN_POINT('Ctrl Pts',(-24.8323595443267,19.8302978104149,8.15074541747705));
#62955=CARTESIAN_POINT('Ctrl Pts',(-24.9405332180278,19.8711753901806,8.1448813661216));
#62956=CARTESIAN_POINT('Ctrl Pts',(-25.0488663181304,19.9121132153389,8.13900867232502));
#62957=CARTESIAN_POINT('Ctrl Pts',(-25.1552493867321,19.9577869268456,8.13313597852844));
#62958=CARTESIAN_POINT('Ctrl Pts',(-25.2592550013274,20.0079651973878,8.12726328473186));
#62959=CARTESIAN_POINT('Ctrl Pts',(-25.2877299988013,20.0217031684819,8.12565543940858));
#62960=CARTESIAN_POINT('Ctrl Pts',(-25.3160269493838,20.0357785339095,8.12404759408529));
#62961=CARTESIAN_POINT('Ctrl Pts',(-25.3441374593362,20.0501859799871,8.122439748762));
#62962=CARTESIAN_POINT('Ctrl Pts',(-25.4468048365961,20.1028059681805,8.11656745179331));
#62963=CARTESIAN_POINT('Ctrl Pts',(-25.5473269950698,20.1600352490152,8.11069515482462));
#62964=CARTESIAN_POINT('Ctrl Pts',(-25.6452614032994,20.2216752338242,8.10482285785592));
#62965=CARTESIAN_POINT('Ctrl Pts',(-25.7430688963137,20.2832353381083,8.09895817091773));
#62966=CARTESIAN_POINT('Ctrl Pts',(-25.8382949614041,20.3491945612836,8.09309348397953));
#62967=CARTESIAN_POINT('Ctrl Pts',(-25.9305199501705,20.4193076237567,8.08722879704134));
#62968=CARTESIAN_POINT('Ctrl Pts',(-26.0226500913092,20.489348579334,8.08137014156654));
#62969=CARTESIAN_POINT('Ctrl Pts',(-26.1117849680669,20.5635346283769,8.07551148609173));
#62970=CARTESIAN_POINT('Ctrl Pts',(-26.1975328960942,20.6415766005767,8.06965283061693));
#62971=CARTESIAN_POINT('Ctrl Pts',(-26.2866302137162,20.7226669609493,8.06356533089902));
#62972=CARTESIAN_POINT('Ctrl Pts',(-26.372070209357,20.8079203747251,8.05747783118112));
#62973=CARTESIAN_POINT('Ctrl Pts',(-26.4534500196312,20.8969652600185,8.05139033146321));
#62974=CARTESIAN_POINT('Ctrl Pts',(-26.5316798511226,20.9825634734845,8.04553846137983));
#62975=CARTESIAN_POINT('Ctrl Pts',(-26.6061576641391,21.0716647685679,8.03968659129644));
#62976=CARTESIAN_POINT('Ctrl Pts',(-26.6765629362846,21.1639012888655,8.03383472121305));
#62977=CARTESIAN_POINT('Ctrl Pts',(-26.7469574885872,21.2561237653142,8.0279837421301));
#62978=CARTESIAN_POINT('Ctrl Pts',(-26.8132804821875,21.3514801893151,8.02213276304714));
#62979=CARTESIAN_POINT('Ctrl Pts',(-26.8752523676452,21.4495704779494,8.01628178396418));
#62980=CARTESIAN_POINT('Ctrl Pts',(-26.9372298249719,21.5476695858446,8.0104302788219));
#62981=CARTESIAN_POINT('Ctrl Pts',(-26.9948551756657,21.6485026975033,8.00457877367962));
#62982=CARTESIAN_POINT('Ctrl Pts',(-27.0478931930804,21.7516422893632,7.99872726853734));
#62983=CARTESIAN_POINT('Ctrl Pts',(-27.1009488232661,21.8548161316364,7.99287382023757));
#62984=CARTESIAN_POINT('Ctrl Pts',(-27.1494139021352,21.9602976096887,7.9870203719378));
#62985=CARTESIAN_POINT('Ctrl Pts',(-27.1931003028217,22.0676368982977,7.98116692363804));
#62986=CARTESIAN_POINT('Ctrl Pts',(-27.236836384432,22.175098254986,7.97530681869651));
#62987=CARTESIAN_POINT('Ctrl Pts',(-27.2757827850475,22.2844212560711,7.96944671375498));
#62988=CARTESIAN_POINT('Ctrl Pts',(-27.309800424187,22.395138405708,7.96358660881346));
#62989=CARTESIAN_POINT('Ctrl Pts',(-27.3438409720774,22.5059301164157,7.95772255745801));
#62990=CARTESIAN_POINT('Ctrl Pts',(-27.372946045726,22.6181174459967,7.95185850610257));
#62991=CARTESIAN_POINT('Ctrl Pts',(-27.3970275084582,22.7312218374328,7.94599445474712));
#62992=CARTESIAN_POINT('Ctrl Pts',(-27.4211444624592,22.8444929221638,7.94012176095057));
#62993=CARTESIAN_POINT('Ctrl Pts',(-27.4402229611217,22.9586833600148,7.93424906715401));
#62994=CARTESIAN_POINT('Ctrl Pts',(-27.454226584011,23.073308511041,7.92837637335746));
#62995=CARTESIAN_POINT('Ctrl Pts',(-27.4580605417064,23.1046909599492,7.92676852803404));
#62996=CARTESIAN_POINT('Ctrl Pts',(-27.4615144019953,23.1361059909608,7.92516068271063));
#62997=CARTESIAN_POINT('Ctrl Pts',(-27.4645880981971,23.1675436700113,7.92355283738721));
#62998=CARTESIAN_POINT('Ctrl Pts',(-27.4769435290101,23.2939146718693,7.91708973226972));
#62999=CARTESIAN_POINT('Ctrl Pts',(-27.4831806393559,23.4208935378221,7.91062662715224));
#63000=CARTESIAN_POINT('Ctrl Pts',(-27.4832519138216,23.5480479488766,7.90416352203479));
#63001=CARTESIAN_POINT('',(-27.4815060178495,23.5478800874245,6.65416403612834));
#63002=CARTESIAN_POINT('Ctrl Pts',(-27.488217119783,23.5480801490979,7.90416174611401));
#63003=CARTESIAN_POINT('Ctrl Pts',(-27.4802939371502,24.726698147767,7.84432980608009));
#63004=CARTESIAN_POINT('Ctrl Pts',(-26.2908702967356,27.2250975801982,7.71820222892116));
#63005=CARTESIAN_POINT('Ctrl Pts',(-22.0376613007461,27.9494363878388,7.52577901463738));
#63006=CARTESIAN_POINT('Ctrl Pts',(-19.0315256593045,24.6556295193558,7.32689210326248));
#63007=CARTESIAN_POINT('Ctrl Pts',(-20.1777168887306,20.3460749197242,7.12800519188759));
#63008=CARTESIAN_POINT('Ctrl Pts',(-24.4229824301708,18.9808878760331,6.92911828051277));
#63009=CARTESIAN_POINT('Ctrl Pts',(-27.1574915769292,21.2312579726243,6.77117155548725));
#63010=CARTESIAN_POINT('Ctrl Pts',(-27.4809117896271,23.0451161699384,6.67952046758692));
#63011=CARTESIAN_POINT('Ctrl Pts',(-27.4781757282195,23.5478626436939,6.65416501681149));
#63012=CARTESIAN_POINT('',(-27.4822036273482,23.5533406583821,5.40416311071642));
#63013=CARTESIAN_POINT('Ctrl Pts',(-27.4832518216526,23.5478892317737,6.6541635220348));
#63014=CARTESIAN_POINT('Ctrl Pts',(-27.4833222665197,23.6651234473433,6.64825855696148));
#63015=CARTESIAN_POINT('Ctrl Pts',(-27.4781466245375,23.782371779065,6.64235359188816));
#63016=CARTESIAN_POINT('Ctrl Pts',(-27.4677476936434,23.8991374068391,6.63644862681483));
#63017=CARTESIAN_POINT('Ctrl Pts',(-27.4573471920843,24.0159206710108,6.63054276984966));
#63018=CARTESIAN_POINT('Ctrl Pts',(-27.4417218669083,24.132220684945,6.62463691288448));
#63019=CARTESIAN_POINT('Ctrl Pts',(-27.4209463972919,24.2475458694113,6.6187310559193));
#63020=CARTESIAN_POINT('Ctrl Pts',(-27.4001631103339,24.362914448148,6.61282297671311));
#63021=CARTESIAN_POINT('Ctrl Pts',(-27.3742258936023,24.4773070712476,6.60691489750693));
#63022=CARTESIAN_POINT('Ctrl Pts',(-27.3432604098945,24.5902430296848,6.60100681830074));
#63023=CARTESIAN_POINT('Ctrl Pts',(-27.3122539242018,24.7033285287683,6.59509091609472));
#63024=CARTESIAN_POINT('Ctrl Pts',(-27.2762059788322,24.8149531213812,6.5891750138887));
#63025=CARTESIAN_POINT('Ctrl Pts',(-27.2352920947175,24.9246514617553,6.58325911168269));
#63026=CARTESIAN_POINT('Ctrl Pts',(-27.1943505456958,25.0344239773011,6.57733920929708));
#63027=CARTESIAN_POINT('Ctrl Pts',(-27.1485366593428,25.142267274952,6.57141930691147));
#63028=CARTESIAN_POINT('Ctrl Pts',(-27.098073320373,25.247737922329,6.56549940452586));
#63029=CARTESIAN_POINT('Ctrl Pts',(-27.0475167459688,25.353403435956,6.55956856460259));
#63030=CARTESIAN_POINT('Ctrl Pts',(-26.9922937422482,25.4566871835873,6.55363772467932));
#63031=CARTESIAN_POINT('Ctrl Pts',(-26.9326725741186,25.5571714778916,6.54770688475605));
#63032=CARTESIAN_POINT('Ctrl Pts',(-26.8778435210453,25.6495792397364,6.54225274242501));
#63033=CARTESIAN_POINT('Ctrl Pts',(-26.8192955474047,25.7396196142019,6.53679860009397));
#63034=CARTESIAN_POINT('Ctrl Pts',(-26.7572675138849,25.8269922849389,6.53134445776294));
#63035=CARTESIAN_POINT('Ctrl Pts',(-26.6904839554248,25.9210635867819,6.52547216079422));
#63036=CARTESIAN_POINT('Ctrl Pts',(-26.6194459199246,26.0123515511663,6.51959986382549));
#63037=CARTESIAN_POINT('Ctrl Pts',(-26.5444133369009,26.1004466561804,6.51372756685677));
#63038=CARTESIAN_POINT('Ctrl Pts',(-26.4694779901458,26.1884275969348,6.50786287991856));
#63039=CARTESIAN_POINT('Ctrl Pts',(-26.3905586558662,26.2732235949031,6.50199819298035));
#63040=CARTESIAN_POINT('Ctrl Pts',(-26.3079581952231,26.3544544633212,6.49613350604213));
#63041=CARTESIAN_POINT('Ctrl Pts',(-26.2254426839828,26.4356017908763,6.4902748505673));
#63042=CARTESIAN_POINT('Ctrl Pts',(-26.139253869513,26.5131909936536,6.48441619509246));
#63043=CARTESIAN_POINT('Ctrl Pts',(-26.0497340454763,26.5868758475273,6.47855753961762));
#63044=CARTESIAN_POINT('Ctrl Pts',(-25.9567174982651,26.6634388966939,6.47247003989972));
#63045=CARTESIAN_POINT('Ctrl Pts',(-25.8601047070134,26.7357860181436,6.46638254018182));
#63046=CARTESIAN_POINT('Ctrl Pts',(-25.7603211284155,26.8035717287276,6.46029504046392));
#63047=CARTESIAN_POINT('Ctrl Pts',(-25.6643998856275,26.8687336490942,6.4544431703805));
#63048=CARTESIAN_POINT('Ctrl Pts',(-25.5655491292688,26.9296804569246,6.44859130029709));
#63049=CARTESIAN_POINT('Ctrl Pts',(-25.4641788343479,26.9861476273004,6.44273943021368));
#63050=CARTESIAN_POINT('Ctrl Pts',(-25.3628239739761,27.042606200036,6.4368884511307));
#63051=CARTESIAN_POINT('Ctrl Pts',(-25.2589506988417,27.0945862903713,6.43103747204773));
#63052=CARTESIAN_POINT('Ctrl Pts',(-25.1529950091274,27.1418685399879,6.42518649296475));
#63053=CARTESIAN_POINT('Ctrl Pts',(-25.0470297929768,27.1891550407337,6.41933498782244));
#63054=CARTESIAN_POINT('Ctrl Pts',(-24.9389821675759,27.2317426926378,6.41348348268013));
#63055=CARTESIAN_POINT('Ctrl Pts',(-24.8293089419281,27.269459933741,6.40763197753783));
#63056=CARTESIAN_POINT('Ctrl Pts',(-24.7195992961896,27.3071896999189,6.40177852923805));
#63057=CARTESIAN_POINT('Ctrl Pts',(-24.6082633674985,27.3400457049168,6.39592508093827));
#63058=CARTESIAN_POINT('Ctrl Pts',(-24.4957732899104,27.3679061953707,6.39007163263848));
#63059=CARTESIAN_POINT('Ctrl Pts',(-24.3831552866774,27.3957983692519,6.38421152769694));
#63060=CARTESIAN_POINT('Ctrl Pts',(-24.2693809162986,27.418683590076,6.37835142275539));
#63061=CARTESIAN_POINT('Ctrl Pts',(-24.1549327757671,27.4364911762486,6.37249131781385));
#63062=CARTESIAN_POINT('Ctrl Pts',(-24.040407561576,27.454310754716,6.3666272664584));
#63063=CARTESIAN_POINT('Ctrl Pts',(-23.9252080836176,27.4670458443789,6.36076321510295));
#63064=CARTESIAN_POINT('Ctrl Pts',(-23.8098205887411,27.474677766523,6.3548991637475));
#63065=CARTESIAN_POINT('Ctrl Pts',(-23.6942630357306,27.4823209365969,6.34902646995092));
#63066=CARTESIAN_POINT('Ctrl Pts',(-23.5785173244979,27.4848459196048,6.34315377615434));
#63067=CARTESIAN_POINT('Ctrl Pts',(-23.463068314195,27.4822860910905,6.33728108235776));
#63068=CARTESIAN_POINT('Ctrl Pts',(-23.431460306402,27.4815852528641,6.33567323703452));
#63069=CARTESIAN_POINT('Ctrl Pts',(-23.3998744981043,27.4805035697687,6.33406539171128));
#63070=CARTESIAN_POINT('Ctrl Pts',(-23.368320730476,27.4790423987787,6.33245754638804));
#63071=CARTESIAN_POINT('Ctrl Pts',(-23.2530776213804,27.4737057971468,6.32658524941933));
#63072=CARTESIAN_POINT('Ctrl Pts',(-23.1378764555881,27.4632853207081,6.32071295245062));
#63073=CARTESIAN_POINT('Ctrl Pts',(-23.0232022736771,27.4477782885718,6.31484065548191));
#63074=CARTESIAN_POINT('Ctrl Pts',(-22.9086767003989,27.4322913523176,6.30897596854371));
#63075=CARTESIAN_POINT('Ctrl Pts',(-22.794677158774,27.4117310239195,6.30311128160551));
#63076=CARTESIAN_POINT('Ctrl Pts',(-22.6816872156028,27.3861465984905,6.29724659466731));
#63077=CARTESIAN_POINT('Ctrl Pts',(-22.5688134755146,27.3605884850413,6.29138793919247));
#63078=CARTESIAN_POINT('Ctrl Pts',(-22.456947669383,27.3300166426716,6.28552928371763));
#63079=CARTESIAN_POINT('Ctrl Pts',(-22.3465661056098,27.2945318999652,6.27967062824279));
#63080=CARTESIAN_POINT('Ctrl Pts',(-22.2318729407332,27.2576610919544,6.27358312852489));
#63081=CARTESIAN_POINT('Ctrl Pts',(-22.1187827842212,27.2154858158368,6.26749562880699));
#63082=CARTESIAN_POINT('Ctrl Pts',(-22.0078162742232,27.1681772671798,6.26140812908909));
#63083=CARTESIAN_POINT('Ctrl Pts',(-21.9011449591992,27.1226998966002,6.25555625900569));
#63084=CARTESIAN_POINT('Ctrl Pts',(-21.7964363627984,27.0724794300842,6.24970438892229));
#63085=CARTESIAN_POINT('Ctrl Pts',(-21.6941346431447,27.0177177995529,6.2438525188389));
#63086=CARTESIAN_POINT('Ctrl Pts',(-21.5918484998579,26.9629645069777,6.23800153975592));
#63087=CARTESIAN_POINT('Ctrl Pts',(-21.4919688690131,26.9036716202144,6.23215056067295));
#63088=CARTESIAN_POINT('Ctrl Pts',(-21.3949159770263,26.8400873810616,6.22629958158997));
#63089=CARTESIAN_POINT('Ctrl Pts',(-21.2978543590507,26.7764974250739,6.22044807644767));
#63090=CARTESIAN_POINT('Ctrl Pts',(-21.2036203309646,26.7086155762474,6.21459657130537));
#63091=CARTESIAN_POINT('Ctrl Pts',(-21.1126051553548,26.6367334191493,6.20874506616308));
#63092=CARTESIAN_POINT('Ctrl Pts',(-21.0215597555869,26.564827391552,6.20289161786333));
#63093=CARTESIAN_POINT('Ctrl Pts',(-20.9337356579938,26.4889186702892,6.19703816956359));
#63094=CARTESIAN_POINT('Ctrl Pts',(-20.849490504196,26.409338656809,6.19118472126384));
#63095=CARTESIAN_POINT('Ctrl Pts',(-20.7651495453644,26.3296681435725,6.18532461632229));
#63096=CARTESIAN_POINT('Ctrl Pts',(-20.6843959546835,26.2463182888672,6.17946451138075));
#63097=CARTESIAN_POINT('Ctrl Pts',(-20.6075500618979,26.1596569032424,6.1736044064392));
#63098=CARTESIAN_POINT('Ctrl Pts',(-20.5306524182131,26.0729371565982,6.16774035508373));
#63099=CARTESIAN_POINT('Ctrl Pts',(-20.4576679721178,25.9829017587879,6.16187630372827));
#63100=CARTESIAN_POINT('Ctrl Pts',(-20.3888752753636,25.8899497008073,6.1560122523728));
#63101=CARTESIAN_POINT('Ctrl Pts',(-20.3199811919069,25.7968606500485,6.15013955857623));
#63102=CARTESIAN_POINT('Ctrl Pts',(-20.2552914176074,25.700846701536,6.14426686477966));
#63103=CARTESIAN_POINT('Ctrl Pts',(-20.1950399599862,25.6023338163056,6.13839417098309));
#63104=CARTESIAN_POINT('Ctrl Pts',(-20.1785441187734,25.5753626362491,6.13678632565977));
#63105=CARTESIAN_POINT('Ctrl Pts',(-20.1623806885072,25.5482042702037,6.13517848033645));
#63106=CARTESIAN_POINT('Ctrl Pts',(-20.146553847114,25.5208677312162,6.13357063501314));
#63107=CARTESIAN_POINT('Ctrl Pts',(-20.0887498336375,25.4210271105404,6.12769833804444));
#63108=CARTESIAN_POINT('Ctrl Pts',(-20.0352456414679,25.3184737276152,6.12182604107573));
#63109=CARTESIAN_POINT('Ctrl Pts',(-19.9863057110786,25.2136142060826,6.11595374410703));
#63110=CARTESIAN_POINT('Ctrl Pts',(-19.9374292029522,25.1088905741617,6.11008905716881));
#63111=CARTESIAN_POINT('Ctrl Pts',(-19.8931053671678,25.0018671179666,6.1042243702306));
#63112=CARTESIAN_POINT('Ctrl Pts',(-19.8535541192753,24.8929773164581,6.09835968329238));
#63113=CARTESIAN_POINT('Ctrl Pts',(-19.8140435473655,24.7841995012945,6.09250102781758));
#63114=CARTESIAN_POINT('Ctrl Pts',(-19.779295940751,24.6735595448514,6.08664237234278));
#63115=CARTESIAN_POINT('Ctrl Pts',(-19.7494839355358,24.5615126755029,6.08078371686799));
#63116=CARTESIAN_POINT('Ctrl Pts',(-19.7185074471386,24.4450891567475,6.07469621715008));
#63117=CARTESIAN_POINT('Ctrl Pts',(-19.6928601907367,24.3271469859409,6.06860871743217));
#63118=CARTESIAN_POINT('Ctrl Pts',(-19.672679563618,24.2082167231552,6.06252121771427));
#63119=CARTESIAN_POINT('Ctrl Pts',(-19.6532800706287,24.0938899093469,6.05666934763087));
#63120=CARTESIAN_POINT('Ctrl Pts',(-19.6389319564528,23.9786505192196,6.05081747754747));
#63121=CARTESIAN_POINT('Ctrl Pts',(-19.6297054186723,23.8629813832189,6.04496560746407));
#63122=CARTESIAN_POINT('Ctrl Pts',(-19.6204802857162,23.7473298588962,6.03911462838111));
#63123=CARTESIAN_POINT('Ctrl Pts',(-19.6163752115111,23.6312491307621,6.03326364929815));
#63124=CARTESIAN_POINT('Ctrl Pts',(-19.6174084962593,23.5152269275672,6.02741267021519));
#63125=CARTESIAN_POINT('Ctrl Pts',(-19.6184418739098,23.3991942928596,6.0215611650729));
#63126=CARTESIAN_POINT('Ctrl Pts',(-19.6246145252214,23.2832206069425,6.0157096599306));
#63127=CARTESIAN_POINT('Ctrl Pts',(-19.6358926292203,23.1677926594144,6.0098581547883));
#63128=CARTESIAN_POINT('Ctrl Pts',(-19.647174478432,23.0523263807778,6.00400470648854));
#63129=CARTESIAN_POINT('Ctrl Pts',(-19.6635651113687,22.9374066120962,5.99815125818877));
#63130=CARTESIAN_POINT('Ctrl Pts',(-19.6849790348896,22.8235133797974,5.992297809889));
#63131=CARTESIAN_POINT('Ctrl Pts',(-19.7064173106914,22.709490626162,5.98643770494747));
#63132=CARTESIAN_POINT('Ctrl Pts',(-19.7328902027685,22.5964971454994,5.98057760000594));
#63133=CARTESIAN_POINT('Ctrl Pts',(-19.7642614177415,22.4850012537926,5.97471749506441));
#63134=CARTESIAN_POINT('Ctrl Pts',(-19.7956537592642,22.373430276581,5.96885344370896));
#63135=CARTESIAN_POINT('Ctrl Pts',(-19.8319508629333,22.2633592881424,5.96298939235352));
#63136=CARTESIAN_POINT('Ctrl Pts',(-19.8729676199596,22.1552383102866,5.95712534099807));
#63137=CARTESIAN_POINT('Ctrl Pts',(-19.9140448274981,22.0469579836927,5.95125264720151));
#63138=CARTESIAN_POINT('Ctrl Pts',(-19.9598554079241,21.9406337817025,5.94537995340495));
#63139=CARTESIAN_POINT('Ctrl Pts',(-20.0101674840569,21.8366928287674,5.9395072596084));
#63140=CARTESIAN_POINT('Ctrl Pts',(-20.0239420888843,21.8082355345725,5.93789941428501));
#63141=CARTESIAN_POINT('Ctrl Pts',(-20.0380538586334,21.7799567213217,5.93629156896162));
#63142=CARTESIAN_POINT('Ctrl Pts',(-20.052497468823,21.7518647759088,5.93468372363823));
#63143=CARTESIAN_POINT('Ctrl Pts',(-20.1052495383782,21.6492652015011,5.92881142666951));
#63144=CARTESIAN_POINT('Ctrl Pts',(-20.1626081360278,21.5488167759046,5.9229391297008));
#63145=CARTESIAN_POINT('Ctrl Pts',(-20.224374103766,21.4509617746426,5.91706683273209));
#63146=CARTESIAN_POINT('Ctrl Pts',(-20.2860600277152,21.353233585691,5.91120214579389));
#63147=CARTESIAN_POINT('Ctrl Pts',(-20.3521417448157,21.2580924838499,5.9053374588557));
#63148=CARTESIAN_POINT('Ctrl Pts',(-20.4223734356222,21.165957801516,5.89947277191751));
#63149=CARTESIAN_POINT('Ctrl Pts',(-20.4925328975314,21.0739178739349,5.89361411644268));
#63150=CARTESIAN_POINT('Ctrl Pts',(-20.5668335948011,20.9848785426677,5.88775546096786));
#63151=CARTESIAN_POINT('Ctrl Pts',(-20.644985853295,20.8992311195997,5.88189680549304));
#63152=CARTESIAN_POINT('Ctrl Pts',(-20.7261908078412,20.8102382327495,5.87580930577513));
#63153=CARTESIAN_POINT('Ctrl Pts',(-20.8115541056541,20.7249080223781,5.86972180605723));
#63154=CARTESIAN_POINT('Ctrl Pts',(-20.900703646702,20.6436428733402,5.86363430633932));
#63155=CARTESIAN_POINT('Ctrl Pts',(-20.9864024649988,20.5655232648779,5.85778243625592));
#63156=CARTESIAN_POINT('Ctrl Pts',(-21.0755995334561,20.4911601799772,5.85193056617253));
#63157=CARTESIAN_POINT('Ctrl Pts',(-21.1679265834877,20.4208736673663,5.84607869608913));
#63158=CARTESIAN_POINT('Ctrl Pts',(-21.2602395758866,20.350597856516,5.84022771700616));
#63159=CARTESIAN_POINT('Ctrl Pts',(-21.3556812734628,20.2843976341435,5.83437673792319));
#63160=CARTESIAN_POINT('Ctrl Pts',(-21.4538512338705,20.2225520345816,5.82852575884022));
#63161=CARTESIAN_POINT('Ctrl Pts',(-21.5520300207027,20.1607008745051,5.8226742536979));
#63162=CARTESIAN_POINT('Ctrl Pts',(-21.6529372082114,20.1032053359079,5.81682274855559));
#63163=CARTESIAN_POINT('Ctrl Pts',(-21.75614497047,20.0503000950519,5.81097124341327));
#63164=CARTESIAN_POINT('Ctrl Pts',(-21.8593870057799,19.997377285517,5.80511779511347));
#63165=CARTESIAN_POINT('Ctrl Pts',(-21.9649307672754,19.9490479932454,5.79926434681366));
#63166=CARTESIAN_POINT('Ctrl Pts',(-22.0723261880017,19.9054997660571,5.79341089851385));
#63167=CARTESIAN_POINT('Ctrl Pts',(-22.1798437406413,19.8619020150783,5.7875507935723));
#63168=CARTESIAN_POINT('Ctrl Pts',(-22.289216772189,19.8230963369197,5.78169068863074));
#63169=CARTESIAN_POINT('Ctrl Pts',(-22.399977608201,19.7892212103167,5.77583058368919));
#63170=CARTESIAN_POINT('Ctrl Pts',(-22.5108130347039,19.755323270936,5.76996653233373));
#63171=CARTESIAN_POINT('Ctrl Pts',(-22.6230377273525,19.7263625977631,5.76410248097826));
#63172=CARTESIAN_POINT('Ctrl Pts',(-22.7361730161001,19.7024267115342,5.75823842962279));
#63173=CARTESIAN_POINT('Ctrl Pts',(-22.8494750436791,19.678455548587,5.75236573582621));
#63174=CARTESIAN_POINT('Ctrl Pts',(-22.9636899395163,19.6595240199423,5.74649304202963));
#63175=CARTESIAN_POINT('Ctrl Pts',(-23.0783330171981,19.6456679223103,5.74062034823305));
#63176=CARTESIAN_POINT('Ctrl Pts',(-23.1097203741213,19.6418743545631,5.7390125029098));
#63177=CARTESIAN_POINT('Ctrl Pts',(-23.1411398239651,19.638460925838,5.73740465758655));
#63178=CARTESIAN_POINT('Ctrl Pts',(-23.1725814325873,19.6354276900315,5.73579681226331));
#63179=CARTESIAN_POINT('Ctrl Pts',(-23.2874149058908,19.6243494717635,5.72992451529461));
#63180=CARTESIAN_POINT('Ctrl Pts',(-23.4029286053266,19.618309589997,5.72405221832591));
#63181=CARTESIAN_POINT('Ctrl Pts',(-23.5186427837313,19.6173795584298,5.7181799213572));
#63182=CARTESIAN_POINT('Ctrl Pts',(-23.6342070057502,19.6164507321096,5.71231523441902));
#63183=CARTESIAN_POINT('Ctrl Pts',(-23.7499707805255,19.6206185905788,5.70645054748083));
#63184=CARTESIAN_POINT('Ctrl Pts',(-23.865448440845,19.629902988751,5.70058586054265));
#63185=CARTESIAN_POINT('Ctrl Pts',(-23.9808073396196,19.6391778385009,5.69472720506786));
#63186=CARTESIAN_POINT('Ctrl Pts',(-24.0958802996424,19.6535587285542,5.68886854959307));
#63187=CARTESIAN_POINT('Ctrl Pts',(-24.2101815225078,19.6730134718626,5.68300989411828));
#63188=CARTESIAN_POINT('Ctrl Pts',(-24.3289474518143,19.6932281345803,5.67692239440037));
#63189=CARTESIAN_POINT('Ctrl Pts',(-24.4468796707661,19.7189211131666,5.67083489468246));
#63190=CARTESIAN_POINT('Ctrl Pts',(-24.5634385103922,19.749996859694,5.66474739496456));
#63191=CARTESIAN_POINT('Ctrl Pts',(-24.6754856920217,19.7798697533038,5.65889552488117));
#63192=CARTESIAN_POINT('Ctrl Pts',(-24.7862633998641,19.8147163437034,5.65304365479778));
#63193=CARTESIAN_POINT('Ctrl Pts',(-24.8953033067715,19.8543998002581,5.64719178471439));
#63194=CARTESIAN_POINT('Ctrl Pts',(-25.0043266113616,19.8940772146456,5.64134080563143));
#63195=CARTESIAN_POINT('Ctrl Pts',(-25.1116122527678,19.9385898895416,5.63548982654847));
#63196=CARTESIAN_POINT('Ctrl Pts',(-25.2167090186601,19.9877517559681,5.62963884746552));
#63197=CARTESIAN_POINT('Ctrl Pts',(-25.3218152337632,20.0369180425195,5.62378734232322));
#63198=CARTESIAN_POINT('Ctrl Pts',(-25.4247318076668,20.0907341763954,5.61793583718093));
#63199=CARTESIAN_POINT('Ctrl Pts',(-25.5250300452443,20.1489670729335,5.61208433203863));
#63200=CARTESIAN_POINT('Ctrl Pts',(-25.6253615896828,20.2072193073487,5.60623088373887));
#63201=CARTESIAN_POINT('Ctrl Pts',(-25.7230727115568,20.2698910134365,5.60037743543911));
#63202=CARTESIAN_POINT('Ctrl Pts',(-25.8177623434703,20.336704919864,5.59452398713936));
#63203=CARTESIAN_POINT('Ctrl Pts',(-25.9125596580567,20.4035948082116,5.58866388219782));
#63204=CARTESIAN_POINT('Ctrl Pts',(-26.0043282863861,20.4746360606059,5.58280377725629));
#63205=CARTESIAN_POINT('Ctrl Pts',(-26.092698926112,20.5495100683175,5.57694367231475));
#63206=CARTESIAN_POINT('Ctrl Pts',(-26.1811290779332,20.6244344989875,5.57107962095928));
#63207=CARTESIAN_POINT('Ctrl Pts',(-26.266156382102,20.7031965442662,5.56521556960381));
#63208=CARTESIAN_POINT('Ctrl Pts',(-26.3474484645022,20.7854407996801,5.55935151824835));
#63209=CARTESIAN_POINT('Ctrl Pts',(-26.4288603552039,20.8678062667086,5.55347882445179));
#63210=CARTESIAN_POINT('Ctrl Pts',(-26.5065257610035,20.9536638811046,5.54760613065524));
#63211=CARTESIAN_POINT('Ctrl Pts',(-26.5801525719743,21.0426252176958,5.54173343685868));
#63212=CARTESIAN_POINT('Ctrl Pts',(-26.6003103611928,21.0669813435141,5.54012559153529));
#63213=CARTESIAN_POINT('Ctrl Pts',(-26.6201656806579,21.0915699509017,5.5385177462119));
#63214=CARTESIAN_POINT('Ctrl Pts',(-26.6397131152008,21.1163827112315,5.5369099008885));
#63215=CARTESIAN_POINT('Ctrl Pts',(-26.7110486478897,21.206933288174,5.53104230213154));
#63216=CARTESIAN_POINT('Ctrl Pts',(-26.778524082213,21.300780476233,5.52517470337458));
#63217=CARTESIAN_POINT('Ctrl Pts',(-26.8418188622549,21.3975611716709,5.51930710461762));
#63218=CARTESIAN_POINT('Ctrl Pts',(-26.9050336190289,21.4942195077686,5.51344692423587));
#63219=CARTESIAN_POINT('Ctrl Pts',(-26.9640780044036,21.5938036364398,5.50758674385412));
#63220=CARTESIAN_POINT('Ctrl Pts',(-27.018671442544,21.6959172710525,5.50172656347237));
#63221=CARTESIAN_POINT('Ctrl Pts',(-27.0732091005547,21.7979265723976,5.4958723706531));
#63222=CARTESIAN_POINT('Ctrl Pts',(-27.1233046598979,21.9024598788128,5.49001817783384));
#63223=CARTESIAN_POINT('Ctrl Pts',(-27.1687210445858,22.0090923773909,5.48416398501457));
#63224=CARTESIAN_POINT('Ctrl Pts',(-27.2141020393429,22.1156417844424,5.4783143539736));
#63225=CARTESIAN_POINT('Ctrl Pts',(-27.2548109499471,22.2242867513825,5.47246472293264));
#63226=CARTESIAN_POINT('Ctrl Pts',(-27.2906571616852,22.3345789719167,5.46661509189167));
#63227=CARTESIAN_POINT('Ctrl Pts',(-27.3264865824959,22.4448195298464,5.46076820090955));
#63228=CARTESIAN_POINT('Ctrl Pts',(-27.3574577056136,22.5567054147355,5.45492130992742));
#63229=CARTESIAN_POINT('Ctrl Pts',(-27.3834287131429,22.6697700719174,5.4490744189453));
#63230=CARTESIAN_POINT('Ctrl Pts',(-27.4093924142585,22.7828029206627,5.44322917286677));
#63231=CARTESIAN_POINT('Ctrl Pts',(-27.4303587085588,22.8970134785583,5.43738392678824));
#63232=CARTESIAN_POINT('Ctrl Pts',(-27.4462363456635,23.0119225944907,5.43153868070971));
#63233=CARTESIAN_POINT('Ctrl Pts',(-27.4621171030454,23.1268542923917,5.42569228592195));
#63234=CARTESIAN_POINT('Ctrl Pts',(-27.4729071469972,23.2424844130739,5.41984589113418));
#63235=CARTESIAN_POINT('Ctrl Pts',(-27.4785668570434,23.3583266052125,5.41399949634641));
#63236=CARTESIAN_POINT('Ctrl Pts',(-27.4817408223472,23.4232909047189,5.41072083824254));
#63237=CARTESIAN_POINT('Ctrl Pts',(-27.4833022499328,23.4883218102957,5.40744218013866));
#63238=CARTESIAN_POINT('Ctrl Pts',(-27.4832513250676,23.5533333307847,5.40416352203479));
#63239=CARTESIAN_POINT('',(-27.4893522825259,23.5513991534028,4.15416352203478));
#63240=CARTESIAN_POINT('Ctrl Pts',(-27.4795712903284,23.553359068946,5.40416207728037));
#63241=CARTESIAN_POINT('Ctrl Pts',(-27.4827450664922,23.9901033867319,5.38211571469144));
#63242=CARTESIAN_POINT('Ctrl Pts',(-27.213804749291,25.7363791598107,5.29377371497752));
#63243=CARTESIAN_POINT('Ctrl Pts',(-24.6498133537127,28.0703981964695,5.13913607813869));
#63244=CARTESIAN_POINT('Ctrl Pts',(-20.3417373817907,26.9186618543491,4.9402491667638));
#63245=CARTESIAN_POINT('Ctrl Pts',(-18.9820147954062,22.6716429387221,4.74136225538889));
#63246=CARTESIAN_POINT('Ctrl Pts',(-21.8201153659821,19.2319917452288,4.54247534401407));
#63247=CARTESIAN_POINT('Ctrl Pts',(-26.1778457211819,19.7520755616869,4.34674243289589));
#63248=CARTESIAN_POINT('Ctrl Pts',(-27.484577323702,22.308533202287,4.2173051589029));
#63249=CARTESIAN_POINT('Ctrl Pts',(-27.4893522825259,23.5513991534028,4.15416352203478));
#63250=CARTESIAN_POINT('',(-27.4830612926269,23.5466160075057,2.90416352203478));
#63251=CARTESIAN_POINT('Ctrl Pts',(-27.4893522825259,23.5513991534028,4.15416352203478));
#63252=CARTESIAN_POINT('Ctrl Pts',(-27.4895907974283,23.6134817936935,4.15100952177793));
#63253=CARTESIAN_POINT('Ctrl Pts',(-27.4882507228628,23.6755539139368,4.14785552152109));
#63254=CARTESIAN_POINT('Ctrl Pts',(-27.4232753800365,25.0406653481724,4.07840588413927));
#63255=CARTESIAN_POINT('Ctrl Pts',(-25.8759180657365,27.5791519665122,3.94581460988933));
#63256=CARTESIAN_POINT('Ctrl Pts',(-21.4177926524215,27.6846649077641,3.74692769851445));
#63257=CARTESIAN_POINT('Ctrl Pts',(-18.9192170653763,23.9910034157703,3.54804078713955));
#63258=CARTESIAN_POINT('Ctrl Pts',(-20.6761704248198,19.8923292308246,3.34915387576474));
#63259=CARTESIAN_POINT('Ctrl Pts',(-25.0741615585053,19.1549764186241,3.15026696438971));
#63260=CARTESIAN_POINT('Ctrl Pts',(-27.3098113051133,21.6172642433357,3.00193684647982));
#63261=CARTESIAN_POINT('Ctrl Pts',(-27.4859294268932,23.2355262183984,2.91990236569482));
#63262=CARTESIAN_POINT('Ctrl Pts',(-27.4830612926269,23.5466160075057,2.90416352203478));
#63263=CARTESIAN_POINT('',(-27.4767827643537,23.550738941023,1.65416352203481));
#63264=CARTESIAN_POINT('Ctrl Pts',(-27.4830612926269,23.5466160075057,2.90416352203478));
#63265=CARTESIAN_POINT('Ctrl Pts',(-27.4738481842906,24.5459081128646,2.85360672856985));
#63266=CARTESIAN_POINT('Ctrl Pts',(-26.5783054564929,26.8702684537753,2.73675429797997));
#63267=CARTESIAN_POINT('Ctrl Pts',(-22.6657646993551,28.1173557828319,2.55360623026512));
#63268=CARTESIAN_POINT('Ctrl Pts',(-19.2297687690452,25.2748309986811,2.3547193188902));
#63269=CARTESIAN_POINT('Ctrl Pts',(-19.7639310999953,20.8475648235122,2.1558324075154));
#63270=CARTESIAN_POINT('Ctrl Pts',(-23.7774017995599,18.9038395020308,1.95694549614038));
#63271=CARTESIAN_POINT('Ctrl Pts',(-26.9764049458243,20.8594715760247,1.78972253431358));
#63272=CARTESIAN_POINT('Ctrl Pts',(-27.4760272010612,22.863454934077,1.68879520961172));
#63273=CARTESIAN_POINT('Ctrl Pts',(-27.4767827643537,23.550738941023,1.65416352203481));
#63274=CARTESIAN_POINT('',(-27.4832594378696,23.5537205931952,0.404163526210238));
#63275=CARTESIAN_POINT('Ctrl Pts',(-27.4767827643537,23.550738941023,1.65416352203481));
#63276=CARTESIAN_POINT('Ctrl Pts',(-27.477473580183,24.1791266299795,1.62249957248676));
#63277=CARTESIAN_POINT('Ctrl Pts',(-27.0381896343703,26.1222740522175,1.52453998581368));
#63278=CARTESIAN_POINT('Ctrl Pts',(-23.9850432680626,28.1818513752549,1.3602847620158));
#63279=CARTESIAN_POINT('Ctrl Pts',(-19.8886335395912,26.4196247955838,1.16139785064084));
#63280=CARTESIAN_POINT('Ctrl Pts',(-19.1569412107686,22.0206883880481,0.962510939266074));
#63281=CARTESIAN_POINT('Ctrl Pts',(-22.4623294945035,19.027291742867,0.763624027891007));
#63282=CARTESIAN_POINT('Ctrl Pts',(-26.4909783005602,20.1154429344271,0.577508486344934));
#63283=CARTESIAN_POINT('Ctrl Pts',(-27.4751100911716,22.4969944765995,0.457688581923687));
#63284=CARTESIAN_POINT('Ctrl Pts',(-27.4848522193952,23.5537064323839,0.404164314627433));
#63285=CARTESIAN_POINT('',(-27.4850143494599,23.5481581335268,-0.845837085113357));
#63286=CARTESIAN_POINT('Ctrl Pts',(-27.483251002585,23.5537206681901,0.404163522034823));
#63287=CARTESIAN_POINT('Ctrl Pts',(-27.4831014233451,23.7233492057095,0.395567971166493));
#63288=CARTESIAN_POINT('Ctrl Pts',(-27.471974586661,23.8925128226098,0.386972420298163));
#63289=CARTESIAN_POINT('Ctrl Pts',(-27.450069179886,24.0600751581893,0.378376869429831));
#63290=CARTESIAN_POINT('Ctrl Pts',(-27.439427950837,24.1414737467288,0.374201314666986));
#63291=CARTESIAN_POINT('Ctrl Pts',(-27.4262438101914,24.2224950106797,0.370025759904141));
#63292=CARTESIAN_POINT('Ctrl Pts',(-27.4105431465028,24.3030110382688,0.365850205141295));
#63293=CARTESIAN_POINT('Ctrl Pts',(-27.3884624973385,24.4162448602627,0.359977908172612));
#63294=CARTESIAN_POINT('Ctrl Pts',(-27.3613584050731,24.5286960190449,0.354105611203929));
#63295=CARTESIAN_POINT('Ctrl Pts',(-27.3292989305641,24.6398842654413,0.348233314235246));
#63296=CARTESIAN_POINT('Ctrl Pts',(-27.2972810025879,24.7509284207005,0.342368627297074));
#63297=CARTESIAN_POINT('Ctrl Pts',(-27.260320576457,24.8607125247166,0.336503940358903));
#63298=CARTESIAN_POINT('Ctrl Pts',(-27.2185369188538,24.9687653638256,0.33063925342073));
#63299=CARTESIAN_POINT('Ctrl Pts',(-27.1767962331267,25.0767070773538,0.324780597945935));
#63300=CARTESIAN_POINT('Ctrl Pts',(-27.1302423305995,25.1829206842347,0.318921942471139));
#63301=CARTESIAN_POINT('Ctrl Pts',(-27.0790444026469,25.2869496646158,0.313063286996343));
#63302=CARTESIAN_POINT('Ctrl Pts',(-27.0258466385337,25.3950421085986,0.306975787278432));
#63303=CARTESIAN_POINT('Ctrl Pts',(-26.9676347794541,25.5007753430996,0.300888287560521));
#63304=CARTESIAN_POINT('Ctrl Pts',(-26.9046540947007,25.6036592508074,0.294800787842609));
#63305=CARTESIAN_POINT('Ctrl Pts',(-26.8441112114125,25.702560817867,0.28894891775923));
#63306=CARTESIAN_POINT('Ctrl Pts',(-26.7791620489905,25.7988291497208,0.283097047675851));
#63307=CARTESIAN_POINT('Ctrl Pts',(-26.710071134818,25.8920542729509,0.277245177592472));
#63308=CARTESIAN_POINT('Ctrl Pts',(-26.6409907403654,25.9852652018083,0.271394198509522));
#63309=CARTESIAN_POINT('Ctrl Pts',(-26.5677700941059,26.075433511317,0.265543219426572));
#63310=CARTESIAN_POINT('Ctrl Pts',(-26.4907160495626,26.1621796555024,0.259692240343622));
#63311=CARTESIAN_POINT('Ctrl Pts',(-26.4136550771192,26.248933599001,0.253840735201346));
#63312=CARTESIAN_POINT('Ctrl Pts',(-26.3327602957871,26.3322644564463,0.247989230059069));
#63313=CARTESIAN_POINT('Ctrl Pts',(-26.2483772161981,26.4118276550958,0.242137724916793));
#63314=CARTESIAN_POINT('Ctrl Pts',(-26.1639661148251,26.4914172749517,0.236284276617029));
#63315=CARTESIAN_POINT('Ctrl Pts',(-26.0760647124238,26.5672364647243,0.230430828317265));
#63316=CARTESIAN_POINT('Ctrl Pts',(-25.9850530095633,26.6389797182499,0.224577380017501));
#63317=CARTESIAN_POINT('Ctrl Pts',(-25.8939378066339,26.7108045594335,0.218717275075979));
#63318=CARTESIAN_POINT('Ctrl Pts',(-25.7997055681635,26.7785439565373,0.212857170134457));
#63319=CARTESIAN_POINT('Ctrl Pts',(-25.7027668751975,26.8419346246388,0.206997065192935));
#63320=CARTESIAN_POINT('Ctrl Pts',(-25.6057629000891,26.9053679823878,0.20113301383751));
#63321=CARTESIAN_POINT('Ctrl Pts',(-25.5060491960494,26.9644465695172,0.195268962482086));
#63322=CARTESIAN_POINT('Ctrl Pts',(-25.4040611007033,27.0189529784708,0.189404911126661));
#63323=CARTESIAN_POINT('Ctrl Pts',(-25.3019226952632,27.0735397189908,0.183532217330108));
#63324=CARTESIAN_POINT('Ctrl Pts',(-25.1975035800155,27.1235406547688,0.177659523533554));
#63325=CARTESIAN_POINT('Ctrl Pts',(-25.0912592804576,27.1687863784705,0.171786829737001));
#63326=CARTESIAN_POINT('Ctrl Pts',(-25.062171368485,27.1811739007531,0.17017898441347));
#63327=CARTESIAN_POINT('Ctrl Pts',(-25.0329467319798,27.1932052741425,0.168571139089938));
#63328=CARTESIAN_POINT('Ctrl Pts',(-25.0035948967839,27.2048776793442,0.166963293766407));
#63329=CARTESIAN_POINT('Ctrl Pts',(-24.8963938555364,27.247508539838,0.161090996797697));
#63330=CARTESIAN_POINT('Ctrl Pts',(-24.7871358980256,27.2854900307209,0.155218699828987));
#63331=CARTESIAN_POINT('Ctrl Pts',(-24.6762618557182,27.3186198176963,0.149346402860276));
#63332=CARTESIAN_POINT('Ctrl Pts',(-24.5655314973643,27.3517066710989,0.143481715922072));
#63333=CARTESIAN_POINT('Ctrl Pts',(-24.4531896114827,27.3799542067631,0.137617028983867));
#63334=CARTESIAN_POINT('Ctrl Pts',(-24.3396971067328,27.4032080547884,0.131752342045662));
#63335=CARTESIAN_POINT('Ctrl Pts',(-24.2263213219194,27.4264379876867,0.125893686570838));
#63336=CARTESIAN_POINT('Ctrl Pts',(-24.1117976744959,27.4446843656312,0.120035031096014));
#63337=CARTESIAN_POINT('Ctrl Pts',(-23.9966016973842,27.4578427638306,0.114176375621191));
#63338=CARTESIAN_POINT('Ctrl Pts',(-23.8769060639434,27.4715151406535,0.108088875903287));
#63339=CARTESIAN_POINT('Ctrl Pts',(-23.756484942131,27.4796938225144,0.102001376185383));
#63340=CARTESIAN_POINT('Ctrl Pts',(-23.6358832543151,27.4823202294003,0.0959138764674789));
#63341=CARTESIAN_POINT('Ctrl Pts',(-23.5199497115402,27.484844975617,0.0900620063840775));
#63342=CARTESIAN_POINT('Ctrl Pts',(-23.4038497730578,27.4822392700093,0.0842101363006761));
#63343=CARTESIAN_POINT('Ctrl Pts',(-23.2880713446477,27.4745040558907,0.0783582662172749));
#63344=CARTESIAN_POINT('Ctrl Pts',(-23.1723105445562,27.4667700195288,0.0725072871343076));
#63345=CARTESIAN_POINT('Ctrl Pts',(-23.0568715695533,27.4539080551118,0.0666563080513403));
#63346=CARTESIAN_POINT('Ctrl Pts',(-22.9422396053731,27.4359711629678,0.0608053289683731));
#63347=CARTESIAN_POINT('Ctrl Pts',(-22.8275973346761,27.4180326581245,0.0549538238260758));
#63348=CARTESIAN_POINT('Ctrl Pts',(-22.7137626274781,27.3950183824119,0.0491023186837784));
#63349=CARTESIAN_POINT('Ctrl Pts',(-22.6012121417523,27.3670327635466,0.0432508135414812));
#63350=CARTESIAN_POINT('Ctrl Pts',(-22.4886242804604,27.3390378512664,0.0373973652417081));
#63351=CARTESIAN_POINT('Ctrl Pts',(-22.3773218895887,27.3060684128702,0.0315439169419352));
#63352=CARTESIAN_POINT('Ctrl Pts',(-22.2677674030154,27.2682790101795,0.0256904686421622));
#63353=CARTESIAN_POINT('Ctrl Pts',(-22.1580883292015,27.2304466327321,0.0198303637006198));
#63354=CARTESIAN_POINT('Ctrl Pts',(-22.0501615181881,27.1877834852662,0.0139702587590774));
#63355=CARTESIAN_POINT('Ctrl Pts',(-21.9444304124587,27.1404926798422,0.00811015381753506));
#63356=CARTESIAN_POINT('Ctrl Pts',(-21.838628103447,27.0931700270206,0.00224610246208278));
#63357=CARTESIAN_POINT('Ctrl Pts',(-21.7350248126622,27.0412136956528,-0.0036179488933695));
#63358=CARTESIAN_POINT('Ctrl Pts',(-21.6340387671704,26.9848724245862,-0.00948200024882183));
#63359=CARTESIAN_POINT('Ctrl Pts',(-21.5329038884063,26.9284481177328,-0.0153546940453922));
#63360=CARTESIAN_POINT('Ctrl Pts',(-21.4343943037761,26.8676261895828,-0.0212273878419625));
#63361=CARTESIAN_POINT('Ctrl Pts',(-21.3388987693554,26.8026983095343,-0.0271000816385329));
#63362=CARTESIAN_POINT('Ctrl Pts',(-21.3127536894765,26.784922142088,-0.028707926961845));
#63363=CARTESIAN_POINT('Ctrl Pts',(-21.2868343382308,26.7668384324236,-0.0303157722851571));
#63364=CARTESIAN_POINT('Ctrl Pts',(-21.2611482366596,26.7484536708432,-0.0319236176084692));
#63365=CARTESIAN_POINT('Ctrl Pts',(-21.167335471086,26.6813074235435,-0.0377959145771856));
#63366=CARTESIAN_POINT('Ctrl Pts',(-21.076322447735,26.6099174767044,-0.043668211545902));
#63367=CARTESIAN_POINT('Ctrl Pts',(-20.9885176819414,26.5345453389706,-0.0495405085146185));
#63368=CARTESIAN_POINT('Ctrl Pts',(-20.9008267041509,26.4592708775414,-0.0554051954528298));
#63369=CARTESIAN_POINT('Ctrl Pts',(-20.8163360266228,26.3800247545737,-0.0612698823910413));
#63370=CARTESIAN_POINT('Ctrl Pts',(-20.7354246640142,26.2971112967806,-0.0671345693292529));
#63371=CARTESIAN_POINT('Ctrl Pts',(-20.6545965136769,26.2142831102883,-0.0729932248040839));
#63372=CARTESIAN_POINT('Ctrl Pts',(-20.5773406433354,26.1277953850026,-0.078851880278915));
#63373=CARTESIAN_POINT('Ctrl Pts',(-20.5040019530224,26.0379917487227,-0.0847105357537462));
#63374=CARTESIAN_POINT('Ctrl Pts',(-20.42779858887,25.944680303312,-0.0907980354716464));
#63375=CARTESIAN_POINT('Ctrl Pts',(-20.3558250052433,25.8477889173408,-0.0968855351895468));
#63376=CARTESIAN_POINT('Ctrl Pts',(-20.2884250401308,25.7477443781594,-0.102973034907447));
#63377=CARTESIAN_POINT('Ctrl Pts',(-20.2236339341362,25.6515722758229,-0.108824904990857));
#63378=CARTESIAN_POINT('Ctrl Pts',(-20.1630692194076,25.5524869552794,-0.114676775074266));
#63379=CARTESIAN_POINT('Ctrl Pts',(-20.1069938360773,25.4508994097487,-0.120528645157676));
#63380=CARTESIAN_POINT('Ctrl Pts',(-20.0509269907339,25.3493273318455,-0.126379624240656));
#63381=CARTESIAN_POINT('Ctrl Pts',(-19.9993483174046,25.2452541482869,-0.132230603323635));
#63382=CARTESIAN_POINT('Ctrl Pts',(-19.9524754894816,25.1391167028958,-0.138081582406615));
#63383=CARTESIAN_POINT('Ctrl Pts',(-19.9055984472403,25.0329697147269,-0.143933087548922));
#63384=CARTESIAN_POINT('Ctrl Pts',(-19.8634282585003,24.9247584739471,-0.149784592691228));
#63385=CARTESIAN_POINT('Ctrl Pts',(-19.8261347203128,24.8149404485148,-0.155636097833535));
#63386=CARTESIAN_POINT('Ctrl Pts',(-19.7888287977531,24.7050859549068,-0.161489546133317));
#63387=CARTESIAN_POINT('Ctrl Pts',(-19.7564028787359,24.5936240068804,-0.1673429944331));
#63388=CARTESIAN_POINT('Ctrl Pts',(-19.7289768929224,24.481027205033,-0.173196442732883));
#63389=CARTESIAN_POINT('Ctrl Pts',(-19.7015197178075,24.3683023561719,-0.179056547674435));
#63390=CARTESIAN_POINT('Ctrl Pts',(-19.6790739228884,24.2544404794189,-0.184916652615988));
#63391=CARTESIAN_POINT('Ctrl Pts',(-19.661708326042,24.1399244410548,-0.19077675755754));
#63392=CARTESIAN_POINT('Ctrl Pts',(-19.6443310345531,24.0253312833061,-0.196640808912999));
#63393=CARTESIAN_POINT('Ctrl Pts',(-19.6320407971446,23.9100834967976,-0.202504860268458));
#63394=CARTESIAN_POINT('Ctrl Pts',(-19.6248544151101,23.7946673968688,-0.208368911623917));
#63395=CARTESIAN_POINT('Ctrl Pts',(-19.6176574417831,23.679081196648,-0.214241605420499));
#63396=CARTESIAN_POINT('Ctrl Pts',(-19.6155793438109,23.5633265996907,-0.22011429921708));
#63397=CARTESIAN_POINT('Ctrl Pts',(-19.6185848739744,23.4478883326802,-0.225986993013661));
#63398=CARTESIAN_POINT('Ctrl Pts',(-19.6194077378567,23.4162832662209,-0.227594838336907));
#63399=CARTESIAN_POINT('Ctrl Pts',(-19.6206113580627,23.3847018694414,-0.229202683660152));
#63400=CARTESIAN_POINT('Ctrl Pts',(-19.6221943396339,23.3531539782036,-0.230810528983397));
#63401=CARTESIAN_POINT('Ctrl Pts',(-19.6279758272855,23.2379323313163,-0.236682825952087));
#63402=CARTESIAN_POINT('Ctrl Pts',(-19.6388409899222,23.1227722550315,-0.242555122920777));
#63403=CARTESIAN_POINT('Ctrl Pts',(-19.6547906357902,23.0081587966629,-0.248427419889468));
#63404=CARTESIAN_POINT('Ctrl Pts',(-19.6707196121839,22.8936938682339,-0.254292106827657));
#63405=CARTESIAN_POINT('Ctrl Pts',(-19.6917199120295,22.7797745546788,-0.260156793765846));
#63406=CARTESIAN_POINT('Ctrl Pts',(-19.7177403736471,22.6668842288776,-0.266021480704035));
#63407=CARTESIAN_POINT('Ctrl Pts',(-19.7437340748488,22.5541100037094,-0.27188013617884));
#63408=CARTESIAN_POINT('Ctrl Pts',(-19.7747375762156,22.4423630617817,-0.277738791653646));
#63409=CARTESIAN_POINT('Ctrl Pts',(-19.8106482110032,22.3321193186715,-0.283597447128451));
#63410=CARTESIAN_POINT('Ctrl Pts',(-19.8479615468154,22.2175693578536,-0.289684946846359));
#63411=CARTESIAN_POINT('Ctrl Pts',(-19.8905731223735,22.1046428727228,-0.295772446564268));
#63412=CARTESIAN_POINT('Ctrl Pts',(-19.9383097333281,21.9938598366036,-0.301859946282177));
#63413=CARTESIAN_POINT('Ctrl Pts',(-19.9841985971429,21.8873648937118,-0.307711816365564));
#63414=CARTESIAN_POINT('Ctrl Pts',(-20.0348229439625,21.7828509667625,-0.313563686448951));
#63415=CARTESIAN_POINT('Ctrl Pts',(-20.0899791285838,21.6807614309593,-0.319415556532339));
#63416=CARTESIAN_POINT('Ctrl Pts',(-20.1451269151745,21.5786874392163,-0.325266535615292));
#63417=CARTESIAN_POINT('Ctrl Pts',(-20.2048049711578,21.4790374682561,-0.331117514698246));
#63418=CARTESIAN_POINT('Ctrl Pts',(-20.2687634341927,21.3822307829614,-0.336968493781199));
#63419=CARTESIAN_POINT('Ctrl Pts',(-20.3327276477089,21.2854153938139,-0.342819998923483));
#63420=CARTESIAN_POINT('Ctrl Pts',(-20.4009728054362,21.1914441434438,-0.348671504065767));
#63421=CARTESIAN_POINT('Ctrl Pts',(-20.4732058144103,21.1007071657839,-0.35452300920805));
#63422=CARTESIAN_POINT('Ctrl Pts',(-20.5454628103944,21.009940056349,-0.360376457507813));
#63423=CARTESIAN_POINT('Ctrl Pts',(-20.6217100335435,20.9224096785141,-0.366229905807576));
#63424=CARTESIAN_POINT('Ctrl Pts',(-20.701614704112,20.8384723917736,-0.372083354107339));
#63425=CARTESIAN_POINT('Ctrl Pts',(-20.7816102436418,20.7544396501115,-0.377943459048868));
#63426=CARTESIAN_POINT('Ctrl Pts',(-20.8652712472577,20.6740084549124,-0.383803563990396));
#63427=CARTESIAN_POINT('Ctrl Pts',(-20.9522286704359,20.5974977135062,-0.389663668931924));
#63428=CARTESIAN_POINT('Ctrl Pts',(-21.0392446539961,20.5209354469042,-0.395527720287355));
#63429=CARTESIAN_POINT('Ctrl Pts',(-21.1295611561015,20.4482991496557,-0.401391771642785));
#63430=CARTESIAN_POINT('Ctrl Pts',(-21.2227781133087,20.379865831028,-0.407255822998215));
#63431=CARTESIAN_POINT('Ctrl Pts',(-21.3161324537031,20.3113316553492,-0.413128516794771));
#63432=CARTESIAN_POINT('Ctrl Pts',(-21.4123954382311,20.2470130498172,-0.419001210591326));
#63433=CARTESIAN_POINT('Ctrl Pts',(-21.5111402055849,20.1871423756765,-0.424873904387882));
#63434=CARTESIAN_POINT('Ctrl Pts',(-21.5381748710902,20.1707507866097,-0.426481749711327));
#63435=CARTESIAN_POINT('Ctrl Pts',(-21.565395437831,20.1546923286918,-0.428089595034772));
#63436=CARTESIAN_POINT('Ctrl Pts',(-21.5927928766977,20.1389711450213,-0.429697440358217));
#63437=CARTESIAN_POINT('Ctrl Pts',(-21.6928559206118,20.0815530228508,-0.435569737326925));
#63438=CARTESIAN_POINT('Ctrl Pts',(-21.7956151059868,20.0284451632611,-0.441442034295634));
#63439=CARTESIAN_POINT('Ctrl Pts',(-21.9006627912706,19.9799104348792,-0.447314331264342));
#63440=CARTESIAN_POINT('Ctrl Pts',(-22.005574343097,19.9314386036507,-0.453179018202544));
#63441=CARTESIAN_POINT('Ctrl Pts',(-22.11276812529,19.8875282899,-0.459043705140747));
#63442=CARTESIAN_POINT('Ctrl Pts',(-22.2218098130786,19.8483977339803,-0.464908392078949));
#63443=CARTESIAN_POINT('Ctrl Pts',(-22.3307393583174,19.8093074213879,-0.470767047553771));
#63444=CARTESIAN_POINT('Ctrl Pts',(-22.4415126422997,19.774987227871,-0.476625703028593));
#63445=CARTESIAN_POINT('Ctrl Pts',(-22.553673773538,19.7456080307202,-0.482484358503414));
#63446=CARTESIAN_POINT('Ctrl Pts',(-22.6702160173526,19.7150812562518,-0.488571858221319));
#63447=CARTESIAN_POINT('Ctrl Pts',(-22.7882563270237,19.6898895372098,-0.494659357939225));
#63448=CARTESIAN_POINT('Ctrl Pts',(-22.9072636159754,19.6701682214939,-0.50074685765713));
#63449=CARTESIAN_POINT('Ctrl Pts',(-23.0216644744878,19.6512102612818,-0.506598727740525));
#63450=CARTESIAN_POINT('Ctrl Pts',(-23.1369584003652,19.6373071654731,-0.51245059782392));
#63451=CARTESIAN_POINT('Ctrl Pts',(-23.2526622957446,19.6285272670349,-0.518302467907315));
#63452=CARTESIAN_POINT('Ctrl Pts',(-23.3683485741538,19.619748705416,-0.524153446990283));
#63453=CARTESIAN_POINT('Ctrl Pts',(-23.4844442858662,19.6160918214419,-0.530004426073252));
#63454=CARTESIAN_POINT('Ctrl Pts',(-23.6004616351134,19.6175730321756,-0.53585540515622));
#63455=CARTESIAN_POINT('Ctrl Pts',(-23.7164894154368,19.6190543760844,-0.541706910298511));
#63456=CARTESIAN_POINT('Ctrl Pts',(-23.8324384059155,19.6256747277654,-0.547558415440801));
#63457=CARTESIAN_POINT('Ctrl Pts',(-23.9478219511535,19.6373983871201,-0.553409920583092));
#63458=CARTESIAN_POINT('Ctrl Pts',(-24.0632438127547,19.6491259396468,-0.559263368882843));
#63459=CARTESIAN_POINT('Ctrl Pts',(-24.1780994446946,19.6659601278811,-0.565116817182595));
#63460=CARTESIAN_POINT('Ctrl Pts',(-24.2919091541914,19.6878136060533,-0.570970265482346));
#63461=CARTESIAN_POINT('Ctrl Pts',(-24.4058482900415,19.7096919363756,-0.576830370423882));
#63462=CARTESIAN_POINT('Ctrl Pts',(-24.5187387231532,19.7366008716773,-0.582690475365417));
#63463=CARTESIAN_POINT('Ctrl Pts',(-24.6301126672292,19.7684023115397,-0.588550580306953));
#63464=CARTESIAN_POINT('Ctrl Pts',(-24.7415616146861,19.8002251676816,-0.594414631662402));
#63465=CARTESIAN_POINT('Ctrl Pts',(-24.8514916484476,19.8369469583216,-0.600278683017851));
#63466=CARTESIAN_POINT('Ctrl Pts',(-24.9594534647184,19.8783808386249,-0.6061427343733));
#63467=CARTESIAN_POINT('Ctrl Pts',(-25.0675743951551,19.9198757841968,-0.612015428169868));
#63468=CARTESIAN_POINT('Ctrl Pts',(-25.1737209411578,19.9660965152552,-0.617888121966435));
#63469=CARTESIAN_POINT('Ctrl Pts',(-25.27746687668,20.0168095073233,-0.623760815763002));
#63470=CARTESIAN_POINT('Ctrl Pts',(-25.3058707783694,20.0306938762273,-0.625368661086382));
#63471=CARTESIAN_POINT('Ctrl Pts',(-25.3340948987324,20.0449147184682,-0.626976506409762));
#63472=CARTESIAN_POINT('Ctrl Pts',(-25.3621308714945,20.059466677225,-0.628584351733142));
#63473=CARTESIAN_POINT('Ctrl Pts',(-25.4645260182614,20.1126144657925,-0.634456648701863));
#63474=CARTESIAN_POINT('Ctrl Pts',(-25.5647522475575,20.1703604430574,-0.640328945670583));
#63475=CARTESIAN_POINT('Ctrl Pts',(-25.6623680560565,20.2325037449793,-0.646201242639304));
#63476=CARTESIAN_POINT('Ctrl Pts',(-25.75985736222,20.2945665141172,-0.652065929577516));
#63477=CARTESIAN_POINT('Ctrl Pts',(-25.854742629459,20.3610150555275,-0.657930616515728));
#63478=CARTESIAN_POINT('Ctrl Pts',(-25.9466054775514,20.431601932656,-0.66379530345394));
#63479=CARTESIAN_POINT('Ctrl Pts',(-26.0383738504552,20.5021162156001,-0.669653958928763));
#63480=CARTESIAN_POINT('Ctrl Pts',(-26.1271256610989,20.5767601184639,-0.675512614403587));
#63481=CARTESIAN_POINT('Ctrl Pts',(-26.2124707188754,20.6552424585093,-0.681371269878411));
#63482=CARTESIAN_POINT('Ctrl Pts',(-26.3011494297795,20.7367903878832,-0.687458769596311));
#63483=CARTESIAN_POINT('Ctrl Pts',(-26.3861494371434,20.8224824888239,-0.693546269314211));
#63484=CARTESIAN_POINT('Ctrl Pts',(-26.4670697956996,20.9119451105623,-0.699633769032112));
#63485=CARTESIAN_POINT('Ctrl Pts',(-26.54485795953,20.9979448910952,-0.705485639115518));
#63486=CARTESIAN_POINT('Ctrl Pts',(-26.6188761218968,21.0874283926874,-0.711337509198923));
#63487=CARTESIAN_POINT('Ctrl Pts',(-26.688805658253,21.1800261138666,-0.717189379282329));
#63488=CARTESIAN_POINT('Ctrl Pts',(-26.7587245472015,21.2726097362008,-0.723040358365308));
#63489=CARTESIAN_POINT('Ctrl Pts',(-26.8245557988721,21.3683063055329,-0.728891337448287));
#63490=CARTESIAN_POINT('Ctrl Pts',(-26.8860219270224,21.4667143052171,-0.734742316531267));
#63491=CARTESIAN_POINT('Ctrl Pts',(-26.9474935815692,21.5651311527275,-0.740593821673573));
#63492=CARTESIAN_POINT('Ctrl Pts',(-27.0045991134024,21.6662595645785,-0.746445326815878));
#63493=CARTESIAN_POINT('Ctrl Pts',(-27.0571054997417,21.7696708120035,-0.752296831958184));
#63494=CARTESIAN_POINT('Ctrl Pts',(-27.1096293223089,21.8731164000528,-0.758150280257977));
#63495=CARTESIAN_POINT('Ctrl Pts',(-27.1575507754387,21.9788459626734,-0.76400372855777));
#63496=CARTESIAN_POINT('Ctrl Pts',(-27.2006840503086,22.086408712188,-0.769857176857563));
#63497=CARTESIAN_POINT('Ctrl Pts',(-27.2438663770781,22.1940937839054,-0.77571728179911));
#63498=CARTESIAN_POINT('Ctrl Pts',(-27.2822495031859,22.3036158196673,-0.781577386740657));
#63499=CARTESIAN_POINT('Ctrl Pts',(-27.3156967565068,22.4145066138827,-0.787437491682205));
#63500=CARTESIAN_POINT('Ctrl Pts',(-27.3491665344594,22.5254720861076,-0.793301543037662));
#63501=CARTESIAN_POINT('Ctrl Pts',(-27.3776937193796,22.6378077525327,-0.799165594393119));
#63502=CARTESIAN_POINT('Ctrl Pts',(-27.4011926392129,22.7510346087824,-0.805029645748576));
#63503=CARTESIAN_POINT('Ctrl Pts',(-27.4247261917633,22.8644283388157,-0.810902339545148));
#63504=CARTESIAN_POINT('Ctrl Pts',(-27.4432166232067,22.9787154734938,-0.816775033341719));
#63505=CARTESIAN_POINT('Ctrl Pts',(-27.4566300083566,23.0934111918128,-0.822647727138291));
#63506=CARTESIAN_POINT('Ctrl Pts',(-27.4603023688319,23.1248129608619,-0.824255572461539));
#63507=CARTESIAN_POINT('Ctrl Pts',(-27.4635944692151,23.1562453549675,-0.825863417784788));
#63508=CARTESIAN_POINT('Ctrl Pts',(-27.4665062939636,23.1876984398535,-0.827471263108036));
#63509=CARTESIAN_POINT('Ctrl Pts',(-27.477592826223,23.3074534630305,-0.833593001393755));
#63510=CARTESIAN_POINT('Ctrl Pts',(-27.4831875036166,23.4277246956559,-0.839714739679475));
#63511=CARTESIAN_POINT('Ctrl Pts',(-27.4832519681591,23.548147118064,-0.845836477965195));
#63512=CARTESIAN_POINT('',(-27.48156856957,23.5477950957604,-2.09583596348537));
#63513=CARTESIAN_POINT('Ctrl Pts',(-27.488361223027,23.5481790525876,-0.845838238126122));
#63514=CARTESIAN_POINT('Ctrl Pts',(-27.4806823124676,24.7334074016489,-0.906011550245059));
#63515=CARTESIAN_POINT('Ctrl Pts',(-26.2794691055314,27.2379105123852,-1.03248049948896));
#63516=CARTESIAN_POINT('Ctrl Pts',(-22.0150358044262,27.9415917844077,-1.22524508585781));
#63517=CARTESIAN_POINT('Ctrl Pts',(-19.0258954158673,24.6323539689758,-1.42413199723265));
#63518=CARTESIAN_POINT('Ctrl Pts',(-20.1942556145273,20.3287566797515,-1.62301890860764));
#63519=CARTESIAN_POINT('Ctrl Pts',(-24.4464924384507,18.9854409406596,-1.8219058199825));
#63520=CARTESIAN_POINT('Ctrl Pts',(-27.1634961703733,21.244963443143,-1.97951117201133));
#63521=CARTESIAN_POINT('Ctrl Pts',(-27.4811027227655,23.0518391628667,-2.07082088691515));
#63522=CARTESIAN_POINT('Ctrl Pts',(-27.478300869659,23.5477773275668,-2.09583496469404));
#63523=CARTESIAN_POINT('',(-27.482122854251,23.5532788466855,-3.34583691089324));
#63524=CARTESIAN_POINT('Ctrl Pts',(-27.4832517696687,23.5478042481997,-2.09583647796519));
#63525=CARTESIAN_POINT('Ctrl Pts',(-27.4833246542727,23.6648883574814,-2.10173454261193));
#63526=CARTESIAN_POINT('Ctrl Pts',(-27.4781648693244,23.7819916671266,-2.10763260725867));
#63527=CARTESIAN_POINT('Ctrl Pts',(-27.4677938782179,23.898618428816,-2.11353067190542));
#63528=CARTESIAN_POINT('Ctrl Pts',(-27.4574217011788,24.015258526885,-2.11942941100139));
#63529=CARTESIAN_POINT('Ctrl Pts',(-27.4418371675545,24.1314215660302,-2.12532815009736));
#63530=CARTESIAN_POINT('Ctrl Pts',(-27.4211136371411,24.2466168776645,-2.13122688919334));
#63531=CARTESIAN_POINT('Ctrl Pts',(-27.4003830219145,24.3618515714521,-2.13712764490825));
#63532=CARTESIAN_POINT('Ctrl Pts',(-27.3745099852318,24.4761174818321,-2.14302840062316));
#63533=CARTESIAN_POINT('Ctrl Pts',(-27.3436189016895,24.5889346693036,-2.14892915633808));
#63534=CARTESIAN_POINT('Ctrl Pts',(-27.3126878313712,24.7018978923003,-2.1548375502505));
#63535=CARTESIAN_POINT('Ctrl Pts',(-27.2767258456684,24.8134082559318,-2.16074594416292));
#63536=CARTESIAN_POINT('Ctrl Pts',(-27.2359072188032,24.9230010619762,-2.16665433807534));
#63537=CARTESIAN_POINT('Ctrl Pts',(-27.1950620589579,25.0326651056876,-2.17256657257013));
#63538=CARTESIAN_POINT('Ctrl Pts',(-27.1493541253973,25.1404087364141,-2.17847880706492));
#63539=CARTESIAN_POINT('Ctrl Pts',(-27.0990051098812,25.2457890658955,-2.18439104155971));
#63540=CARTESIAN_POINT('Ctrl Pts',(-27.0485626404997,25.3513649940202,-2.19031424987715));
#63541=CARTESIAN_POINT('Ctrl Pts',(-26.9934620634722,25.4545684973145,-2.19623745819458));
#63542=CARTESIAN_POINT('Ctrl Pts',(-26.9339705319384,25.554982312693,-2.20216066651202));
#63543=CARTESIAN_POINT('Ctrl Pts',(-26.8753181558165,25.6539797450261,-2.2080003252521));
#63544=CARTESIAN_POINT('Ctrl Pts',(-26.8123981750014,25.7502654222508,-2.21383998399218));
#63545=CARTESIAN_POINT('Ctrl Pts',(-26.7455051231394,25.8434707674631,-2.21967964273225));
#63546=CARTESIAN_POINT('Ctrl Pts',(-26.6782382017041,25.93719704335,-2.22555193970097));
#63547=CARTESIAN_POINT('Ctrl Pts',(-26.6067311872943,26.0281181180212,-2.23142423666969));
#63548=CARTESIAN_POINT('Ctrl Pts',(-26.5312461140655,26.1158258130217,-2.23729653363841));
#63549=CARTESIAN_POINT('Ctrl Pts',(-26.4558588634967,26.203419845815,-2.24316122057662));
#63550=CARTESIAN_POINT('Ctrl Pts',(-26.376504073216,26.2878084697762,-2.24902590751484));
#63551=CARTESIAN_POINT('Ctrl Pts',(-26.2934865574468,26.3686130622071,-2.25489059445305));
#63552=CARTESIAN_POINT('Ctrl Pts',(-26.2105544199956,26.4493345521732,-2.26074924992788));
#63553=CARTESIAN_POINT('Ctrl Pts',(-26.1239673440281,26.5264790555594,-2.26660790540271));
#63554=CARTESIAN_POINT('Ctrl Pts',(-26.0340694009186,26.5997021148413,-2.27246656087754));
#63555=CARTESIAN_POINT('Ctrl Pts',(-25.9406599649704,26.6757853313126,-2.27855406059544));
#63556=CARTESIAN_POINT('Ctrl Pts',(-25.843676034825,26.7476341636557,-2.28464156031334));
#63557=CARTESIAN_POINT('Ctrl Pts',(-25.7435448399721,26.8149053234086,-2.29072906003125));
#63558=CARTESIAN_POINT('Ctrl Pts',(-25.6472894361563,26.8795726097293,-2.29658093011465));
#63559=CARTESIAN_POINT('Ctrl Pts',(-25.5481262555831,26.9400097591984,-2.30243280019806));
#63560=CARTESIAN_POINT('Ctrl Pts',(-25.4464666295152,26.9959543608177,-2.30828467028146));
#63561=CARTESIAN_POINT('Ctrl Pts',(-25.3448224820499,27.0518904443626,-2.31413564936444));
#63562=CARTESIAN_POINT('Ctrl Pts',(-25.2406830069288,27.1033351408816,-2.31998662844741));
#63563=CARTESIAN_POINT('Ctrl Pts',(-25.1344853277419,27.1500713393465,-2.32583760753039));
#63564=CARTESIAN_POINT('Ctrl Pts',(-25.0282781003617,27.1968117398453,-2.33168911267268));
#63565=CARTESIAN_POINT('Ctrl Pts',(-24.9200126794348,27.2388426342079,-2.33754061781498));
#63566=CARTESIAN_POINT('Ctrl Pts',(-24.810146751056,27.2759948142493,-2.34339212295727));
#63567=CARTESIAN_POINT('Ctrl Pts',(-24.700244338594,27.3131593317209,-2.34924557125705));
#63568=CARTESIAN_POINT('Ctrl Pts',(-24.58874075323,27.3454417810223,-2.35509901955682));
#63569=CARTESIAN_POINT('Ctrl Pts',(-24.4761087495102,27.3727228407916,-2.3609524678566));
#63570=CARTESIAN_POINT('Ctrl Pts',(-24.3633486587444,27.4000349250499,-2.36681257279815));
#63571=CARTESIAN_POINT('Ctrl Pts',(-24.2494579902851,27.4223341699959,-2.3726726777397));
#63572=CARTESIAN_POINT('Ctrl Pts',(-24.1349196985764,27.4395523792207,-2.37853278268125));
#63573=CARTESIAN_POINT('Ctrl Pts',(-24.0203042724967,27.4567821838319,-2.38439683403673));
#63574=CARTESIAN_POINT('Ctrl Pts',(-23.9050407648425,27.4689240961187,-2.3902608853922));
#63575=CARTESIAN_POINT('Ctrl Pts',(-23.7896155121726,27.4759619406516,-2.39612493674767));
#63576=CARTESIAN_POINT('Ctrl Pts',(-23.6740201457215,27.4830101575624,-2.40199763054426));
#63577=CARTESIAN_POINT('Ctrl Pts',(-23.558262970268,27.4849392866438,-2.40787032434085));
#63578=CARTESIAN_POINT('Ctrl Pts',(-23.4428286667338,27.4817851988912,-2.41374301813744));
#63579=CARTESIAN_POINT('Ctrl Pts',(-23.411224685408,27.480921662426,-2.41535086346068));
#63580=CARTESIAN_POINT('Ctrl Pts',(-23.3796448637463,27.4796774004135,-2.41695870878393));
#63581=CARTESIAN_POINT('Ctrl Pts',(-23.348099035807,27.478053820469,-2.41856655410717));
#63582=CARTESIAN_POINT('Ctrl Pts',(-23.2328849246582,27.4721240563002,-2.42443885107587));
#63583=CARTESIAN_POINT('Ctrl Pts',(-23.1177389263555,27.4611107005926,-2.43031114804456));
#63584=CARTESIAN_POINT('Ctrl Pts',(-23.0031460888512,27.4450135693189,-2.43618344501325));
#63585=CARTESIAN_POINT('Ctrl Pts',(-22.8887017545635,27.428937298649,-2.44204813195144));
#63586=CARTESIAN_POINT('Ctrl Pts',(-22.774809561097,27.4077904108904,-2.44791281888963));
#63587=CARTESIAN_POINT('Ctrl Pts',(-22.6619528150904,27.3816246897443,-2.45377750582782));
#63588=CARTESIAN_POINT('Ctrl Pts',(-22.5492121351819,27.3554858784044,-2.45963616130264));
#63589=CARTESIAN_POINT('Ctrl Pts',(-22.4375051848865,27.3243385930816,-2.46549481677746));
#63590=CARTESIAN_POINT('Ctrl Pts',(-22.3273077472633,27.2882861129015,-2.47135347225228));
#63591=CARTESIAN_POINT('Ctrl Pts',(-22.2128059006658,27.2508253910909,-2.47744097197019));
#63592=CARTESIAN_POINT('Ctrl Pts',(-22.0999343468339,27.2080685232089,-2.48352847168809));
#63593=CARTESIAN_POINT('Ctrl Pts',(-21.9892128357608,27.1601893826267,-2.489615971406));
#63594=CARTESIAN_POINT('Ctrl Pts',(-21.8827770364571,27.1141635060968,-2.49546784148939));
#63595=CARTESIAN_POINT('Ctrl Pts',(-21.7783283456541,27.0634046998971,-2.50131971157278));
#63596=CARTESIAN_POINT('Ctrl Pts',(-21.6763098761126,27.0081171796514,-2.50717158165617));
#63597=CARTESIAN_POINT('Ctrl Pts',(-21.5743069398106,26.9528380774332,-2.51302256073914));
#63598=CARTESIAN_POINT('Ctrl Pts',(-21.4747338523888,26.8930318291002,-2.51887353982211));
#63599=CARTESIAN_POINT('Ctrl Pts',(-21.3780095568292,26.8289488363479,-2.52472451890508));
#63600=CARTESIAN_POINT('Ctrl Pts',(-21.2812765648244,26.7648600819177,-2.53057602404739));
#63601=CARTESIAN_POINT('Ctrl Pts',(-21.1873932184841,26.6964940470069,-2.53642752918969));
#63602=CARTESIAN_POINT('Ctrl Pts',(-21.0967492742306,26.6241443264091,-2.542279034332));
#63603=CARTESIAN_POINT('Ctrl Pts',(-21.0060752290967,26.5517705800443,-2.54813248263177));
#63604=CARTESIAN_POINT('Ctrl Pts',(-20.9186430479949,26.4754107752407,-2.55398593093153));
#63605=CARTESIAN_POINT('Ctrl Pts',(-20.8348086618625,26.3953981500754,-2.5598393792313));
#63606=CARTESIAN_POINT('Ctrl Pts',(-20.7508789378289,26.3152945331809,-2.56569948417284));
#63607=CARTESIAN_POINT('Ctrl Pts',(-20.6705554744434,26.231530090146,-2.57155958911437));
#63608=CARTESIAN_POINT('Ctrl Pts',(-20.59415670384,26.1444742755979,-2.5774196940559));
#63609=CARTESIAN_POINT('Ctrl Pts',(-20.5177064834463,26.0573598344074,-2.58328374541133));
#63610=CARTESIAN_POINT('Ctrl Pts',(-20.4451864766657,25.9669499298223,-2.58914779676677));
#63611=CARTESIAN_POINT('Ctrl Pts',(-20.3768731776859,25.8736449814439,-2.5950118481222));
#63612=CARTESIAN_POINT('Ctrl Pts',(-20.30845919854,25.780202520197,-2.60088454191876));
#63613=CARTESIAN_POINT('Ctrl Pts',(-20.244264529249,25.6838568423362,-2.60675723571532));
#63614=CARTESIAN_POINT('Ctrl Pts',(-20.1845209815277,25.5850351078467,-2.61262992951188));
#63615=CARTESIAN_POINT('Ctrl Pts',(-20.1681641975486,25.5579793700284,-2.61423777483526));
#63616=CARTESIAN_POINT('Ctrl Pts',(-20.1521407836831,25.5307381598423,-2.61584562015864));
#63617=CARTESIAN_POINT('Ctrl Pts',(-20.1364548714063,25.5033205117227,-2.61745346548201));
#63618=CARTESIAN_POINT('Ctrl Pts',(-20.0791655701436,25.4031836580085,-2.62332576245072));
#63619=CARTESIAN_POINT('Ctrl Pts',(-20.0261899976171,25.300356212039,-2.62919805941943));
#63620=CARTESIAN_POINT('Ctrl Pts',(-19.9777904976329,25.1952461533203,-2.63507035638813));
#63621=CARTESIAN_POINT('Ctrl Pts',(-19.9294537195569,25.0902723088901,-2.64093504332632));
#63622=CARTESIAN_POINT('Ctrl Pts',(-19.8856813922345,24.9830221063017,-2.64679973026451));
#63623=CARTESIAN_POINT('Ctrl Pts',(-19.8466911968959,24.8739301508248,-2.6526644172027));
#63624=CARTESIAN_POINT('Ctrl Pts',(-19.8077411005326,24.764950389595,-2.65852307267751));
#63625=CARTESIAN_POINT('Ctrl Pts',(-19.7735634920431,24.654133029921,-2.66438172815231));
#63626=CARTESIAN_POINT('Ctrl Pts',(-19.7443286618798,24.5419341828186,-2.67024038362711));
#63627=CARTESIAN_POINT('Ctrl Pts',(-19.7139518935004,24.4253527499244,-2.67632788334502));
#63628=CARTESIAN_POINT('Ctrl Pts',(-19.6889121040238,24.3072801182162,-2.68241538306293));
#63629=CARTESIAN_POINT('Ctrl Pts',(-19.6693439577706,24.1882475480119,-2.68850288278084));
#63630=CARTESIAN_POINT('Ctrl Pts',(-19.6505332382712,24.0738223868119,-2.69435475286423));
#63631=CARTESIAN_POINT('Ctrl Pts',(-19.6367785282974,23.9585106642039,-2.70020662294762));
#63632=CARTESIAN_POINT('Ctrl Pts',(-19.6281475390507,23.8427955655904,-2.706058493031));
#63633=CARTESIAN_POINT('Ctrl Pts',(-19.6195178639506,23.7270980856528,-2.71190947211396));
#63634=CARTESIAN_POINT('Ctrl Pts',(-19.6160103891629,23.6109977639522,-2.71776045119692));
#63635=CARTESIAN_POINT('Ctrl Pts',(-19.6176409039817,23.4949824169804,-2.72361143027989));
#63636=CARTESIAN_POINT('Ctrl Pts',(-19.6192715653995,23.3789566391125,-2.72946293542216));
#63637=CARTESIAN_POINT('Ctrl Pts',(-19.6260411289376,23.2630162645278,-2.73531444056444));
#63638=CARTESIAN_POINT('Ctrl Pts',(-19.6379132682393,23.1476479022758,-2.74116594570672));
#63639=CARTESIAN_POINT('Ctrl Pts',(-19.64978935002,23.032241228702,-2.74701939400649));
#63640=CARTESIAN_POINT('Ctrl Pts',(-19.6667713345861,22.9174073561639,-2.75287284230626));
#63641=CARTESIAN_POINT('Ctrl Pts',(-19.6887712589127,22.8036258646389,-2.75872629060602));
#63642=CARTESIAN_POINT('Ctrl Pts',(-19.7107962019305,22.6897149788509,-2.76458639554755));
#63643=CARTESIAN_POINT('Ctrl Pts',(-19.737850396163,22.5768592689307,-2.77044650048908));
#63644=CARTESIAN_POINT('Ctrl Pts',(-19.7697951393013,22.4655263430634,-2.77630660543061));
#63645=CARTESIAN_POINT('Ctrl Pts',(-19.8017613952247,22.3541184414384,-2.78217065678605));
#63646=CARTESIAN_POINT('Ctrl Pts',(-19.8386246268657,22.2442357567988,-2.7880347081415));
#63647=CARTESIAN_POINT('Ctrl Pts',(-19.8801974113251,22.1363273521134,-2.79389875949694));
#63648=CARTESIAN_POINT('Ctrl Pts',(-19.92183146577,22.0282599119802,-2.7997714532935));
#63649=CARTESIAN_POINT('Ctrl Pts',(-19.9681887609088,21.9221729363647,-2.80564414709005));
#63650=CARTESIAN_POINT('Ctrl Pts',(-20.0190352239381,21.8184923504325,-2.81151684088661));
#63651=CARTESIAN_POINT('Ctrl Pts',(-20.032956134959,21.7901063403666,-2.81312468621005));
#63652=CARTESIAN_POINT('Ctrl Pts',(-20.0472132876738,21.7619005444932,-2.81473253153349));
#63653=CARTESIAN_POINT('Ctrl Pts',(-20.0618013144989,21.7338833221862,-2.81634037685693));
#63654=CARTESIAN_POINT('Ctrl Pts',(-20.1150808336513,21.6315566572847,-2.82221267382564));
#63655=CARTESIAN_POINT('Ctrl Pts',(-20.1729557464653,21.5314048255695,-2.82808497079435));
#63656=CARTESIAN_POINT('Ctrl Pts',(-20.2352246208861,21.4338690715047,-2.83395726776306));
#63657=CARTESIAN_POINT('Ctrl Pts',(-20.297412799791,21.3364597160312,-2.83982195470126));
#63658=CARTESIAN_POINT('Ctrl Pts',(-20.3639833961407,21.2416600414739,-2.84568664163947));
#63659=CARTESIAN_POINT('Ctrl Pts',(-20.4346884351633,21.1498881092768,-2.85155132857767));
#63660=CARTESIAN_POINT('Ctrl Pts',(-20.5053207584793,21.058210558767,-2.85740998405249));
#63661=CARTESIAN_POINT('Ctrl Pts',(-20.5800788162142,20.9695548825192,-2.86326863952731));
#63662=CARTESIAN_POINT('Ctrl Pts',(-20.6586709237259,20.8843108960878,-2.86912729500212));
#63663=CARTESIAN_POINT('Ctrl Pts',(-20.7403329081801,20.7957372044645,-2.87521479472003));
#63664=CARTESIAN_POINT('Ctrl Pts',(-20.8261343265639,20.7108475465617,-2.88130229443793));
#63665=CARTESIAN_POINT('Ctrl Pts',(-20.9157010124322,20.6300423864557,-2.88738979415583));
#63666=CARTESIAN_POINT('Ctrl Pts',(-21.0018008290713,20.5523649620742,-2.89324166423924));
#63667=CARTESIAN_POINT('Ctrl Pts',(-21.091379512186,20.4784620193127,-2.89909353432265));
#63668=CARTESIAN_POINT('Ctrl Pts',(-21.1840671505649,20.4086517069346,-2.90494540440606));
#63669=CARTESIAN_POINT('Ctrl Pts',(-21.2767406764081,20.3388520238114,-2.91079638348904));
#63670=CARTESIAN_POINT('Ctrl Pts',(-21.3725218861999,20.2731439807019,-2.91664736257202));
#63671=CARTESIAN_POINT('Ctrl Pts',(-21.4710089065238,20.2118045468982,-2.922498341655));
#63672=CARTESIAN_POINT('Ctrl Pts',(-21.5695047817786,20.1504595980891,-2.92834984679731));
#63673=CARTESIAN_POINT('Ctrl Pts',(-21.6707066002681,20.0934842579507,-2.93420135193961));
#63674=CARTESIAN_POINT('Ctrl Pts',(-21.7741853336982,20.0411109973296,-2.94005285708192));
#63675=CARTESIAN_POINT('Ctrl Pts',(-21.877698430163,19.9887203446889,-2.94590630538169));
#63676=CARTESIAN_POINT('Ctrl Pts',(-21.9834895764158,19.9409349969722,-2.95175975368146));
#63677=CARTESIAN_POINT('Ctrl Pts',(-22.0911077460315,19.8979401827195,-2.95761320198123));
#63678=CARTESIAN_POINT('Ctrl Pts',(-22.1988483008749,19.8548964740267,-2.96347330692278));
#63679=CARTESIAN_POINT('Ctrl Pts',(-22.3084196420435,19.8166543260515,-2.96933341186432));
#63680=CARTESIAN_POINT('Ctrl Pts',(-22.4193533884474,19.7833498082616,-2.97519351680587));
#63681=CARTESIAN_POINT('Ctrl Pts',(-22.5303618417868,19.7500228619634,-2.98105756816135));
#63682=CARTESIAN_POINT('Ctrl Pts',(-22.6427341274588,19.7216402679381,-2.98692161951682));
#63683=CARTESIAN_POINT('Ctrl Pts',(-22.7559911312308,19.6982870817279,-2.9927856708723));
#63684=CARTESIAN_POINT('Ctrl Pts',(-22.8694150532178,19.6748994775831,-2.99865836466887));
#63685=CARTESIAN_POINT('Ctrl Pts',(-22.9837258890047,19.6565561401114,-3.00453105846545));
#63686=CARTESIAN_POINT('Ctrl Pts',(-23.0984387743304,19.6432903705443,-3.01040375226203));
#63687=CARTESIAN_POINT('Ctrl Pts',(-23.1298452434189,19.6396584247463,-3.0120115975853));
#63688=CARTESIAN_POINT('Ctrl Pts',(-23.1612818481735,19.6364067781375,-3.01361944290856));
#63689=CARTESIAN_POINT('Ctrl Pts',(-23.1927386543061,19.633535433476,-3.01522728823182));
#63690=CARTESIAN_POINT('Ctrl Pts',(-23.3076276331307,19.6230484865613,-3.02109958520052));
#63691=CARTESIAN_POINT('Ctrl Pts',(-23.4231708933924,19.6176033109717,-3.02697188216923));
#63692=CARTESIAN_POINT('Ctrl Pts',(-23.5388883261552,19.6172689498784,-3.03284417913793));
#63693=CARTESIAN_POINT('Ctrl Pts',(-23.6544557983154,19.6169350220905,-3.03870886607613));
#63694=CARTESIAN_POINT('Ctrl Pts',(-23.7701965845477,19.6216987387958,-3.04457355301433));
#63695=CARTESIAN_POINT('Ctrl Pts',(-23.8856249218682,19.6315774545911,-3.05043823995253));
#63696=CARTESIAN_POINT('Ctrl Pts',(-24.0009345483693,19.6414460107456,-3.05629689542733));
#63697=CARTESIAN_POINT('Ctrl Pts',(-24.1159319557078,19.6564190676342,-3.06215555090212));
#63698=CARTESIAN_POINT('Ctrl Pts',(-24.2301315176028,19.6764619379063,-3.06801420637692));
#63699=CARTESIAN_POINT('Ctrl Pts',(-24.3487918149717,19.6972877003448,-3.07410170609483));
#63700=CARTESIAN_POINT('Ctrl Pts',(-24.4665902124818,19.7235874144039,-3.08018920581274));
#63701=CARTESIAN_POINT('Ctrl Pts',(-24.5829875401612,19.7552627553856,-3.08627670553064));
#63702=CARTESIAN_POINT('Ctrl Pts',(-24.6948794615081,19.7857120348701,-3.09212857561405));
#63703=CARTESIAN_POINT('Ctrl Pts',(-24.8054763229485,19.821128410417,-3.09798044569746));
#63704=CARTESIAN_POINT('Ctrl Pts',(-24.9143105078985,19.8613726424116,-3.10383231578086));
#63705=CARTESIAN_POINT('Ctrl Pts',(-25.0231281218543,19.9016107468561,-3.10968329486384));
#63706=CARTESIAN_POINT('Ctrl Pts',(-25.1301832053341,19.9466751028323,-3.11553427394681));
#63707=CARTESIAN_POINT('Ctrl Pts',(-25.2350255098076,19.9963773211362,-3.12138525302979));
#63708=CARTESIAN_POINT('Ctrl Pts',(-25.3398772406127,20.0460840081476,-3.12723675817206));
#63709=CARTESIAN_POINT('Ctrl Pts',(-25.4425154233602,20.1004292093306,-3.13308826331434));
#63710=CARTESIAN_POINT('Ctrl Pts',(-25.5425125684457,20.1591776363309,-3.13893976845661));
#63711=CARTESIAN_POINT('Ctrl Pts',(-25.6425429204071,20.2179455724055,-3.14479321675641));
#63712=CARTESIAN_POINT('Ctrl Pts',(-25.7399301345507,20.2811194325328,-3.15064666505621));
#63713=CARTESIAN_POINT('Ctrl Pts',(-25.834274576095,20.3484198844918,-3.15650011335601));
#63714=CARTESIAN_POINT('Ctrl Pts',(-25.9287263077554,20.4157968716784,-3.16236021829756));
#63715=CARTESIAN_POINT('Ctrl Pts',(-26.0201280234437,20.4873095772382,-3.1682203232391));
#63716=CARTESIAN_POINT('Ctrl Pts',(-26.1081120657983,20.5626374956173,-3.17408042818064));
#63717=CARTESIAN_POINT('Ctrl Pts',(-26.1961553598988,20.6380161426349,-3.17994447953609));
#63718=CARTESIAN_POINT('Ctrl Pts',(-26.2807760966672,20.7172148366861,-3.18580853089154));
#63719=CARTESIAN_POINT('Ctrl Pts',(-26.361643735895,20.7998764670546,-3.19167258224699));
#63720=CARTESIAN_POINT('Ctrl Pts',(-26.4426305578804,20.8826599241655,-3.19754527604357));
#63721=CARTESIAN_POINT('Ctrl Pts',(-26.5198529681875,20.9689161967156,-3.20341796984014));
#63722=CARTESIAN_POINT('Ctrl Pts',(-26.5930208602435,21.0582553609942,-3.20929066363671));
#63723=CARTESIAN_POINT('Ctrl Pts',(-26.6130530051392,21.082714929712,-3.21089850896005));
#63724=CARTESIAN_POINT('Ctrl Pts',(-26.6327814875512,21.1074054199052,-3.21250635428339));
#63725=CARTESIAN_POINT('Ctrl Pts',(-26.6522009352553,21.1323184751813,-3.21411419960673));
#63726=CARTESIAN_POINT('Ctrl Pts',(-26.7231378177672,21.2233228385422,-3.21998746317924));
#63727=CARTESIAN_POINT('Ctrl Pts',(-26.7901893465413,21.3176091291791,-3.22586072675175));
#63728=CARTESIAN_POINT('Ctrl Pts',(-26.8530365008391,21.4148118153175,-3.23173399032427));
#63729=CARTESIAN_POINT('Ctrl Pts',(-26.9158037361498,21.5118908945829,-3.23759978521692));
#63730=CARTESIAN_POINT('Ctrl Pts',(-26.9743770037245,21.6118786541688,-3.24346558010956));
#63731=CARTESIAN_POINT('Ctrl Pts',(-27.0284774515868,21.714376608153,-3.24933137500221));
#63732=CARTESIAN_POINT('Ctrl Pts',(-27.0825221532819,21.8167689462264,-3.25519112566426));
#63733=CARTESIAN_POINT('Ctrl Pts',(-27.1321030083236,21.9216659732544,-3.26105087632632));
#63734=CARTESIAN_POINT('Ctrl Pts',(-27.1769848197709,22.0286409154721,-3.26691062698837));
#63735=CARTESIAN_POINT('Ctrl Pts',(-27.2218312081501,22.1355314274822,-3.27276575282937));
#63736=CARTESIAN_POINT('Ctrl Pts',(-27.261985770649,22.2444962138211,-3.27862087867038));
#63737=CARTESIAN_POINT('Ctrl Pts',(-27.297259893632,22.3550852506896,-3.28447600451138));
#63738=CARTESIAN_POINT('Ctrl Pts',(-27.3325166140797,22.4656197283104,-3.2903282417183));
#63739=CARTESIAN_POINT('Ctrl Pts',(-27.3628975582545,22.5777764705715,-3.29618047892522));
#63740=CARTESIAN_POINT('Ctrl Pts',(-27.3882630050007,22.6910874679318,-3.30203271613214));
#63741=CARTESIAN_POINT('Ctrl Pts',(-27.4136210567992,22.8043654310269,-3.30788324719967));
#63742=CARTESIAN_POINT('Ctrl Pts',(-27.4339664328418,22.9187965768231,-3.3137337782672));
#63743=CARTESIAN_POINT('Ctrl Pts',(-27.4492100355465,23.0339005362938,-3.31958430933472));
#63744=CARTESIAN_POINT('Ctrl Pts',(-27.464456042393,23.149022649363,-3.32543576311762));
#63745=CARTESIAN_POINT('Ctrl Pts',(-27.4745986124711,23.2648173792551,-3.33128721690051));
#63746=CARTESIAN_POINT('Ctrl Pts',(-27.4796003104943,23.3807974248407,-3.3371386706834));
#63747=CARTESIAN_POINT('Ctrl Pts',(-27.4820785439443,23.4382630349532,-3.34003793977733));
#63748=CARTESIAN_POINT('Ctrl Pts',(-27.4832955026874,23.4957740748039,-3.34293720887125));
#63749=CARTESIAN_POINT('Ctrl Pts',(-27.4832513732947,23.5532711355702,-3.34583647796518));
#63750=CARTESIAN_POINT('',(-27.4892650790848,23.551517445815,-4.59583647796518));
#63751=CARTESIAN_POINT('Ctrl Pts',(-27.4794097119894,23.5532973854538,-3.34583795172231));
#63752=CARTESIAN_POINT('Ctrl Pts',(-27.4825587700888,23.9968499807919,-3.36822567147541));
#63753=CARTESIAN_POINT('Ctrl Pts',(-27.2081891243134,25.7500858833574,-3.45690902835341));
#63754=CARTESIAN_POINT('Ctrl Pts',(-24.6265305769216,28.0759984814206,-3.61188802235648));
#63755=CARTESIAN_POINT('Ctrl Pts',(-20.3244404402133,26.9021008550186,-3.81077493373142));
#63756=CARTESIAN_POINT('Ctrl Pts',(-18.9865981118165,22.6481388093524,-4.0096618451063));
#63757=CARTESIAN_POINT('Ctrl Pts',(-21.8423672611993,19.2231427878892,-4.20854875648117));
#63758=CARTESIAN_POINT('Ctrl Pts',(-26.189767356571,19.7647057021154,-4.40394030076747));
#63759=CARTESIAN_POINT('Ctrl Pts',(-27.4840831004861,22.3152979151724,-4.5330362079288));
#63760=CARTESIAN_POINT('Ctrl Pts',(-27.4892650790848,23.551517445815,-4.59583647796518));
#63761=CARTESIAN_POINT('',(-27.4832669639411,23.5466206728664,-5.84583647796516));
#63762=CARTESIAN_POINT('Ctrl Pts',(-27.4892650790848,23.551517445815,-4.59583647796518));
#63763=CARTESIAN_POINT('Ctrl Pts',(-27.489553500097,23.6203235362853,-4.59933184505377));
#63764=CARTESIAN_POINT('Ctrl Pts',(-27.4879074477743,23.6891155407879,-4.60282721214237));
#63765=CARTESIAN_POINT('Ctrl Pts',(-27.4155519149962,25.0605826362573,-4.67261821635592));
#63766=CARTESIAN_POINT('Ctrl Pts',(-25.855147816285,27.5910703399071,-4.80520949060578));
#63767=CARTESIAN_POINT('Ctrl Pts',(-21.3965383245707,27.6736329344889,-5.0040964019808));
#63768=CARTESIAN_POINT('Ctrl Pts',(-18.9170095843528,23.967158543905,-5.20298331335561));
#63769=CARTESIAN_POINT('Ctrl Pts',(-20.6950382785201,19.8775828759019,-5.40187022473053));
#63770=CARTESIAN_POINT('Ctrl Pts',(-25.0967667891071,19.1628792305347,-5.6007571361054));
#63771=CARTESIAN_POINT('Ctrl Pts',(-27.3145959907761,21.6309496960074,-5.74874588718358));
#63772=CARTESIAN_POINT('Ctrl Pts',(-27.4860826067821,23.2423189068336,-5.83043900113687));
#63773=CARTESIAN_POINT('Ctrl Pts',(-27.4832669639411,23.5466206728664,-5.84583647796516));
#63774=CARTESIAN_POINT('',(-27.476760765631,23.5506274849305,-7.09583647796518));
#63775=CARTESIAN_POINT('Ctrl Pts',(-27.4832669639411,23.5466206728664,-5.84583647796516));
#63776=CARTESIAN_POINT('Ctrl Pts',(-27.473959527258,24.5525257467186,-5.89673463826183));
#63777=CARTESIAN_POINT('Ctrl Pts',(-26.5684793902742,26.8835250199973,-6.01392843568338));
#63778=CARTESIAN_POINT('Ctrl Pts',(-22.6422664878202,28.1127422222305,-6.19741787023015));
#63779=CARTESIAN_POINT('Ctrl Pts',(-19.2209484554937,25.2525677339697,-6.39630478160496));
#63780=CARTESIAN_POINT('Ctrl Pts',(-19.7778938047406,20.8281099073478,-6.59519169297986));
#63781=CARTESIAN_POINT('Ctrl Pts',(-23.8013169807825,18.9050703528649,-6.79407860435475));
#63782=CARTESIAN_POINT('Ctrl Pts',(-26.9837010307554,20.873118155621,-6.96096019934984));
#63783=CARTESIAN_POINT('Ctrl Pts',(-27.4761842519322,22.8701085782786,-7.06154615722));
#63784=CARTESIAN_POINT('Ctrl Pts',(-27.476760765631,23.5506274849305,-7.09583647796518));
#63785=CARTESIAN_POINT('',(-27.4832509725328,23.5537545826837,-8.34583647796518));
#63786=CARTESIAN_POINT('Ctrl Pts',(-27.476760765631,23.5506274849305,-7.09583647796518));
#63787=CARTESIAN_POINT('Ctrl Pts',(-27.4772988621821,24.1857986480022,-7.12784179434496));
#63788=CARTESIAN_POINT('Ctrl Pts',(-27.031270723818,26.1359470768735,-7.22614274784961));
#63789=CARTESIAN_POINT('Ctrl Pts',(-23.961195575086,28.1840281679555,-7.39073933847951));
#63790=CARTESIAN_POINT('Ctrl Pts',(-19.8739114783422,26.4007379800943,-7.5896262498543));
#63791=CARTESIAN_POINT('Ctrl Pts',(-19.1648731073088,21.9980933464675,-7.7885131612292));
#63792=CARTESIAN_POINT('Ctrl Pts',(-22.485626608426,19.0217514026655,-7.98740007260408));
#63793=CARTESIAN_POINT('Ctrl Pts',(-26.5012424661459,20.1285926572705,-8.173174280116));
#63794=CARTESIAN_POINT('Ctrl Pts',(-27.4749296595235,22.5036284115385,-8.29265285050309));
#63795=CARTESIAN_POINT('Ctrl Pts',(-27.4846475833386,23.5537421191806,-8.34583578376515));
#63796=CARTESIAN_POINT('',(-27.4850836380432,23.5482599068045,-9.59583708370669));
#63797=CARTESIAN_POINT('Ctrl Pts',(-27.4832509725328,23.5537545826837,-8.34583647796518));
#63798=CARTESIAN_POINT('Ctrl Pts',(-27.4831019658486,23.7210973936125,-8.35431462942859));
#63799=CARTESIAN_POINT('Ctrl Pts',(-27.4722693976411,23.8879836340533,-8.36279278089199));
#63800=CARTESIAN_POINT('Ctrl Pts',(-27.4509467894136,24.0533164518824,-8.3712709323554));
#63801=CARTESIAN_POINT('Ctrl Pts',(-27.4392914407801,24.1436905567658,-8.3759052533549));
#63802=CARTESIAN_POINT('Ctrl Pts',(-27.424502514206,24.2336011584677,-8.3805395743544));
#63803=CARTESIAN_POINT('Ctrl Pts',(-27.4066170495043,24.32287255847,-8.3851738953539));
#63804=CARTESIAN_POINT('Ctrl Pts',(-27.3839538027933,24.4359912163431,-8.3910461923225));
#63805=CARTESIAN_POINT('Ctrl Pts',(-27.3562712084288,24.5483013623581,-8.3969184892911));
#63806=CARTESIAN_POINT('Ctrl Pts',(-27.3236397985297,24.6593231040583,-8.40279078625971));
#63807=CARTESIAN_POINT('Ctrl Pts',(-27.2910506763462,24.7702009703983,-8.40865547319781));
#63808=CARTESIAN_POINT('Ctrl Pts',(-27.2535256078182,24.8797933598515,-8.41452016013591));
#63809=CARTESIAN_POINT('Ctrl Pts',(-27.2111862836991,24.9876296789424,-8.42038484707402));
#63810=CARTESIAN_POINT('Ctrl Pts',(-27.1688905029244,25.0953550951297,-8.42624350254875));
#63811=CARTESIAN_POINT('Ctrl Pts',(-27.1217904648406,25.2013276507248,-8.43210215802348));
#63812=CARTESIAN_POINT('Ctrl Pts',(-27.0700577085932,25.3050917028648,-8.43796081349821));
#63813=CARTESIAN_POINT('Ctrl Pts',(-27.0163042253202,25.4129088702777,-8.44404831321615));
#63814=CARTESIAN_POINT('Ctrl Pts',(-26.9575488579407,25.5183410485715,-8.45013581293408));
#63815=CARTESIAN_POINT('Ctrl Pts',(-26.8940393954591,25.6208993894933,-8.45622331265201));
#63816=CARTESIAN_POINT('Ctrl Pts',(-26.8329882019111,25.7194879915208,-8.46207518273532));
#63817=CARTESIAN_POINT('Ctrl Pts',(-26.7675443426298,25.8154207111699,-8.46792705281863));
#63818=CARTESIAN_POINT('Ctrl Pts',(-26.6979744519005,25.9082889421537,-8.47377892290194));
#63819=CARTESIAN_POINT('Ctrl Pts',(-26.6284151538198,26.0011430331048,-8.47962990198482));
#63820=CARTESIAN_POINT('Ctrl Pts',(-26.5547313211814,26.0909332323791,-8.4854808810677));
#63821=CARTESIAN_POINT('Ctrl Pts',(-26.4772317572196,26.1772815786106,-8.49133186015058));
#63822=CARTESIAN_POINT('Ctrl Pts',(-26.3997252253012,26.2636376883895,-8.49718336529279));
#63823=CARTESIAN_POINT('Ctrl Pts',(-26.3184025561994,26.3465510222942,-8.503034870435));
#63824=CARTESIAN_POINT('Ctrl Pts',(-26.2336110297142,26.4256787907215,-8.50888637557721));
#63825=CARTESIAN_POINT('Ctrl Pts',(-26.148791345809,26.5048328357581,-8.51473982387689));
#63826=CARTESIAN_POINT('Ctrl Pts',(-26.0605008160413,26.5801985337569,-8.52059327217658));
#63827=CARTESIAN_POINT('Ctrl Pts',(-25.9691210085896,26.6514723387188,-8.52644672047627));
#63828=CARTESIAN_POINT('Ctrl Pts',(-25.8776372824541,26.7228271974737,-8.53230682541771));
#63829=CARTESIAN_POINT('Ctrl Pts',(-25.7830575925853,26.7900806208148,-8.53816693035916));
#63830=CARTESIAN_POINT('Ctrl Pts',(-25.6857938698919,26.8529714408429,-8.54402703530061));
#63831=CARTESIAN_POINT('Ctrl Pts',(-25.5884646461688,26.9159046139021,-8.54989108665597));
#63832=CARTESIAN_POINT('Ctrl Pts',(-25.4884481463292,26.9744691252552,-8.55575513801134));
#63833=CARTESIAN_POINT('Ctrl Pts',(-25.3861808213717,27.0284498112001,-8.56161918936669));
#63834=CARTESIAN_POINT('Ctrl Pts',(-25.2837627747917,27.0825100539004,-8.56749188316317));
#63835=CARTESIAN_POINT('Ctrl Pts',(-25.1790876548214,27.1319728122813,-8.57336457695964));
#63836=CARTESIAN_POINT('Ctrl Pts',(-25.0726118529757,27.1766710261467,-8.57923727075612));
#63837=CARTESIAN_POINT('Ctrl Pts',(-25.0434605595363,27.1889086494003,-8.58084511608034));
#63838=CARTESIAN_POINT('Ctrl Pts',(-25.0141743767119,27.2007894246667,-8.58245296140456));
#63839=CARTESIAN_POINT('Ctrl Pts',(-24.9847628447309,27.2123105817244,-8.58406080672879));
#63840=CARTESIAN_POINT('Ctrl Pts',(-24.8773437743168,27.2543890420385,-8.58993310369751));
#63841=CARTESIAN_POINT('Ctrl Pts',(-24.7678917483023,27.291807606021,-8.59580540066624));
#63842=CARTESIAN_POINT('Ctrl Pts',(-24.6568486338633,27.3243662113101,-8.60167769763497));
#63843=CARTESIAN_POINT('Ctrl Pts',(-24.5459494224818,27.3568826232325,-8.60754238457319));
#63844=CARTESIAN_POINT('Ctrl Pts',(-24.4334636161244,27.3845514859259,-8.61340707151141));
#63845=CARTESIAN_POINT('Ctrl Pts',(-24.3198529119889,27.4072208041396,-8.61927175844964));
#63846=CARTESIAN_POINT('Ctrl Pts',(-24.2063590493505,27.4298668083786,-8.62513041392447));
#63847=CARTESIAN_POINT('Ctrl Pts',(-24.0917429929958,27.4475234148771,-8.63098906939931));
#63848=CARTESIAN_POINT('Ctrl Pts',(-23.9764808070906,27.460088648113,-8.63684772487415));
#63849=CARTESIAN_POINT('Ctrl Pts',(-23.8567163786826,27.4731446904263,-8.64293522459205));
#63850=CARTESIAN_POINT('Ctrl Pts',(-23.7362547512321,27.4807033759924,-8.64902272430995));
#63851=CARTESIAN_POINT('Ctrl Pts',(-23.6156411414375,27.4827089306535,-8.65511022402785));
#63852=CARTESIAN_POINT('Ctrl Pts',(-23.4996961381493,27.4846368560524,-8.66096209411126));
#63853=CARTESIAN_POINT('Ctrl Pts',(-23.3836111512199,27.4814335410521,-8.66681396419467));
#63854=CARTESIAN_POINT('Ctrl Pts',(-23.2678740751089,27.4731024405304,-8.67266583427808));
#63855=CARTESIAN_POINT('Ctrl Pts',(-23.1521546210202,27.4647726084946,-8.67851681336106));
#63856=CARTESIAN_POINT('Ctrl Pts',(-23.0367833846264,27.4513165729938,-8.68436779244404));
#63857=CARTESIAN_POINT('Ctrl Pts',(-22.922245272405,27.4327898312291,-8.69021877152701));
#63858=CARTESIAN_POINT('Ctrl Pts',(-22.807696862105,27.414261423732,-8.69607027666932));
#63859=CARTESIAN_POINT('Ctrl Pts',(-22.6939821329867,27.3906614696848,-8.70192178181162));
#63860=CARTESIAN_POINT('Ctrl Pts',(-22.5815771991487,27.3620968490972,-8.70777328695393));
#63861=CARTESIAN_POINT('Ctrl Pts',(-22.4691349380791,27.3335227428211,-8.71362673525371));
#63862=CARTESIAN_POINT('Ctrl Pts',(-22.3580037376061,27.2999807935126,-8.7194801835535));
#63863=CARTESIAN_POINT('Ctrl Pts',(-22.2486452298479,27.2616279414016,-8.72533363185328));
#63864=CARTESIAN_POINT('Ctrl Pts',(-22.1391623577198,27.2232314737696,-8.73119373679483));
#63865=CARTESIAN_POINT('Ctrl Pts',(-22.0314565923752,27.1800133201904,-8.73705384173637));
#63866=CARTESIAN_POINT('Ctrl Pts',(-21.9259703248689,27.1321788727279,-8.74291394667792));
#63867=CARTESIAN_POINT('Ctrl Pts',(-21.8204130189636,27.0843122117588,-8.74877799803338));
#63868=CARTESIAN_POINT('Ctrl Pts',(-21.7170785547875,27.0318232534521,-8.75464204938883));
#63869=CARTESIAN_POINT('Ctrl Pts',(-21.6163838734407,26.9749628862533,-8.76050610074429));
#63870=CARTESIAN_POINT('Ctrl Pts',(-21.5155407882341,26.9180187182238,-8.76637879454087));
#63871=CARTESIAN_POINT('Ctrl Pts',(-21.4173455998717,26.8566905013052,-8.77225148833744));
#63872=CARTESIAN_POINT('Ctrl Pts',(-21.322185557861,26.7912719022185,-8.77812418213402));
#63873=CARTESIAN_POINT('Ctrl Pts',(-21.2961323301937,26.7733613841095,-8.77973202745723));
#63874=CARTESIAN_POINT('Ctrl Pts',(-21.2703064112939,26.7551444898331,-8.78133987278043));
#63875=CARTESIAN_POINT('Ctrl Pts',(-21.2447152886934,26.7366277483215,-8.78294771810364));
#63876=CARTESIAN_POINT('Ctrl Pts',(-21.1512494126519,26.6689994737106,-8.78882001507236));
#63877=CARTESIAN_POINT('Ctrl Pts',(-21.0606050868939,26.5971419679294,-8.79469231204108));
#63878=CARTESIAN_POINT('Ctrl Pts',(-20.9731894751818,26.5213188390591,-8.8005646090098));
#63879=CARTESIAN_POINT('Ctrl Pts',(-20.8858871471601,26.445593970942,-8.80642929594803));
#63880=CARTESIAN_POINT('Ctrl Pts',(-20.8018055217932,26.3659139679909,-8.81229398288625));
#63881=CARTESIAN_POINT('Ctrl Pts',(-20.7213220421437,26.2825851039283,-8.81815866982447));
#63882=CARTESIAN_POINT('Ctrl Pts',(-20.6409213347147,26.199341938386,-8.82401732529931));
#63883=CARTESIAN_POINT('Ctrl Pts',(-20.5641116980415,26.1124576714474,-8.82987598077414));
#63884=CARTESIAN_POINT('Ctrl Pts',(-20.4912362587049,26.0222777017899,-8.83573463624898));
#63885=CARTESIAN_POINT('Ctrl Pts',(-20.4155142405203,25.9285752230884,-8.84182213596687));
#63886=CARTESIAN_POINT('Ctrl Pts',(-20.3440403751643,25.8313146247633,-8.84790963568477));
#63887=CARTESIAN_POINT('Ctrl Pts',(-20.2771562991104,25.7309244584741,-8.85399713540267));
#63888=CARTESIAN_POINT('Ctrl Pts',(-20.2128611135902,25.6344201072624,-8.85984900548609));
#63889=CARTESIAN_POINT('Ctrl Pts',(-20.1528072596188,25.5350243325003,-8.86570087556951));
#63890=CARTESIAN_POINT('Ctrl Pts',(-20.097255558188,25.4331494754904,-8.87155274565292));
#63891=CARTESIAN_POINT('Ctrl Pts',(-20.0417123150089,25.3312901298539,-8.87740372473591));
#63892=CARTESIAN_POINT('Ctrl Pts',(-19.9906700592396,25.2269528153186,-8.8832547038189));
#63893=CARTESIAN_POINT('Ctrl Pts',(-19.9443442126617,25.1205754904297,-8.88910568290189));
#63894=CARTESIAN_POINT('Ctrl Pts',(-19.8980142009442,25.0141886011957,-8.8949571880442));
#63895=CARTESIAN_POINT('Ctrl Pts',(-19.8564016064521,24.9057617160189,-8.90080869318652));
#63896=CARTESIAN_POINT('Ctrl Pts',(-19.8196738690939,24.7957531708555,-8.90666019832883));
#63897=CARTESIAN_POINT('Ctrl Pts',(-19.7829339352536,24.685708094249,-8.91251364662862));
#63898=CARTESIAN_POINT('Ctrl Pts',(-19.7510822149403,24.574080705159,-8.91836709492842));
#63899=CARTESIAN_POINT('Ctrl Pts',(-19.7242362034355,24.4613442152792,-8.92422054322821));
#63900=CARTESIAN_POINT('Ctrl Pts',(-19.6973596621861,24.3484795195302,-8.93008064816977));
#63901=CARTESIAN_POINT('Ctrl Pts',(-19.6755002877769,24.2345036078746,-8.93594075311132));
#63902=CARTESIAN_POINT('Ctrl Pts',(-19.6587244115379,24.1198996944472,-8.94180085805288));
#63903=CARTESIAN_POINT('Ctrl Pts',(-19.6419372377962,24.0052186024569,-8.94766490940835));
#63904=CARTESIAN_POINT('Ctrl Pts',(-19.6302404205463,23.8899090768447,-8.95352896076382));
#63905=CARTESIAN_POINT('Ctrl Pts',(-19.6236482574694,23.7744575129944,-8.95939301211929));
#63906=CARTESIAN_POINT('Ctrl Pts',(-19.6170463788601,23.6588357965852,-8.96526570591588));
#63907=CARTESIAN_POINT('Ctrl Pts',(-19.6155641746343,23.5430720359407,-8.97113839971246));
#63908=CARTESIAN_POINT('Ctrl Pts',(-19.6191639028281,23.4276507698807,-8.97701109350905));
#63909=CARTESIAN_POINT('Ctrl Pts',(-19.6201494481914,23.3960503579987,-8.97861893883222));
#63910=CARTESIAN_POINT('Ctrl Pts',(-19.6215156229899,23.3644755754901,-8.98022678415538));
#63911=CARTESIAN_POINT('Ctrl Pts',(-19.6232609816518,23.3329362509054,-8.98183462947855));
#63912=CARTESIAN_POINT('Ctrl Pts',(-19.6296355154656,23.2177458918056,-8.98770692644725));
#63913=CARTESIAN_POINT('Ctrl Pts',(-19.6410933399642,23.1026432715625,-8.99357922341594));
#63914=CARTESIAN_POINT('Ctrl Pts',(-19.6576327665207,22.988113435224,-8.99945152038464));
#63915=CARTESIAN_POINT('Ctrl Pts',(-19.6741507592938,22.8737320204576,-9.00531620732283));
#63916=CARTESIAN_POINT('Ctrl Pts',(-19.6957371996832,22.7599223188246,-9.01118089426103));
#63917=CARTESIAN_POINT('Ctrl Pts',(-19.7223384384437,22.6471674334372,-9.01704558119922));
#63918=CARTESIAN_POINT('Ctrl Pts',(-19.7489123194953,22.5345285093909,-9.02290423667403));
#63919=CARTESIAN_POINT('Ctrl Pts',(-19.7804906462226,22.4229426437613,-9.02876289214884));
#63920=CARTESIAN_POINT('Ctrl Pts',(-19.8169683033863,22.3128852173256,-9.03462154762364));
#63921=CARTESIAN_POINT('Ctrl Pts',(-19.8548708099681,22.1985288508756,-9.04070904734155));
#63922=CARTESIAN_POINT('Ctrl Pts',(-19.8980631289842,22.085823212181,-9.04679654705946));
#63923=CARTESIAN_POINT('Ctrl Pts',(-19.9463693817299,21.9752873760785,-9.05288404677736));
#63924=CARTESIAN_POINT('Ctrl Pts',(-19.9928058381377,21.8690300648006,-9.05873591686075));
#63925=CARTESIAN_POINT('Ctrl Pts',(-20.0439675171964,21.7647781199115,-9.06458778694414));
#63926=CARTESIAN_POINT('Ctrl Pts',(-20.0996484940528,21.6629738624424,-9.07043965702752));
#63927=CARTESIAN_POINT('Ctrl Pts',(-20.1553209929741,21.5611851055973,-9.07629063611048));
#63928=CARTESIAN_POINT('Ctrl Pts',(-20.2155112232113,21.4618436577402,-9.08214161519344));
#63929=CARTESIAN_POINT('Ctrl Pts',(-20.2799671674974,21.3653674919907,-9.08799259427639));
#63930=CARTESIAN_POINT('Ctrl Pts',(-20.3444289069932,21.2688826521053,-9.09384409941867));
#63931=CARTESIAN_POINT('Ctrl Pts',(-20.4131568932988,21.1752639501931,-9.09969560456095));
#63932=CARTESIAN_POINT('Ctrl Pts',(-20.4858560290533,21.0849000062727,-9.10554710970324));
#63933=CARTESIAN_POINT('Ctrl Pts',(-20.5585793066083,20.9945060544536,-9.11140055800299));
#63934=CARTESIAN_POINT('Ctrl Pts',(-20.6352760968414,20.9073693317141,-9.11725400630275));
#63935=CARTESIAN_POINT('Ctrl Pts',(-20.7156117899958,20.8238444797872,-9.12310745460251));
#63936=CARTESIAN_POINT('Ctrl Pts',(-20.7960388422778,20.7402246419666,-9.12896755954403));
#63937=CARTESIAN_POINT('Ctrl Pts',(-20.8801127705161,20.6602251714825,-9.13482766448555));
#63938=CARTESIAN_POINT('Ctrl Pts',(-20.9674628934476,20.5841630717207,-9.14068776942708));
#63939=CARTESIAN_POINT('Ctrl Pts',(-21.0548718412199,20.5080497488952,-9.14655182078251));
#63940=CARTESIAN_POINT('Ctrl Pts',(-21.1455610542217,20.4358793333796,-9.15241587213795));
#63941=CARTESIAN_POINT('Ctrl Pts',(-21.2391290483586,20.3679267713776,-9.15827992349339));
#63942=CARTESIAN_POINT('Ctrl Pts',(-21.3328349430408,20.2998740608639,-9.16415261728995));
#63943=CARTESIAN_POINT('Ctrl Pts',(-21.4294277429642,20.2360518373774,-9.1700253110865));
#63944=CARTESIAN_POINT('Ctrl Pts',(-21.5284793963583,20.1766902617436,-9.17589800488306));
#63945=CARTESIAN_POINT('Ctrl Pts',(-21.5555980821281,20.1604380553316,-9.17750585020651));
#63946=CARTESIAN_POINT('Ctrl Pts',(-21.5829009518218,20.1445199326127,-9.17911369552997));
#63947=CARTESIAN_POINT('Ctrl Pts',(-21.6103789551222,20.1289399901514,-9.18072154085343));
#63948=CARTESIAN_POINT('Ctrl Pts',(-21.7107362426876,20.0720377200429,-9.18659383782214));
#63949=CARTESIAN_POINT('Ctrl Pts',(-21.8137674481917,20.0194595342479,-9.19246613479085));
#63950=CARTESIAN_POINT('Ctrl Pts',(-21.9190635823233,19.971466199507,-9.19833843175956));
#63951=CARTESIAN_POINT('Ctrl Pts',(-22.0242232610274,19.9235350603164,-9.20420311869776));
#63952=CARTESIAN_POINT('Ctrl Pts',(-22.1316416586833,19.8801771263302,-9.21006780563596));
#63953=CARTESIAN_POINT('Ctrl Pts',(-22.2408833328458,19.8416083992508,-9.21593249257417));
#63954=CARTESIAN_POINT('Ctrl Pts',(-22.3500126587852,19.8030793376926,-9.22179114804899));
#63955=CARTESIAN_POINT('Ctrl Pts',(-22.4609611440514,19.7693298229638,-9.22764980352382));
#63956=CARTESIAN_POINT('Ctrl Pts',(-22.5732720235775,19.7405283833128,-9.23350845899865));
#63957=CARTESIAN_POINT('Ctrl Pts',(-22.6899698649799,19.7106019340612,-9.23959595871655));
#63958=CARTESIAN_POINT('Ctrl Pts',(-22.8081382892972,19.6860181810953,-9.24568345843445));
#63959=CARTESIAN_POINT('Ctrl Pts',(-22.9272455202642,19.6669097366645,-9.25177095815236));
#63960=CARTESIAN_POINT('Ctrl Pts',(-23.0417424523236,19.6485409252499,-9.25762282823576));
#63961=CARTESIAN_POINT('Ctrl Pts',(-23.1571064191528,19.6352315084791,-9.26347469831916));
#63962=CARTESIAN_POINT('Ctrl Pts',(-23.2728539775337,19.6270473315868,-9.26932656840257));
#63963=CARTESIAN_POINT('Ctrl Pts',(-23.3885839122965,19.6188644008099,-9.27517754748554));
#63964=CARTESIAN_POINT('Ctrl Pts',(-23.5046969102424,19.6158051874455,-9.28102852656851));
#63965=CARTESIAN_POINT('Ctrl Pts',(-23.6207050975568,19.6178835973286,-9.28687950565149));
#63966=CARTESIAN_POINT('Ctrl Pts',(-23.7367237151237,19.6199621940808,-9.29273101079379));
#63967=CARTESIAN_POINT('Ctrl Pts',(-23.8526370899848,19.627179324933,-9.29858251593608));
#63968=CARTESIAN_POINT('Ctrl Pts',(-23.9679587569643,19.639496785119,-9.30443402107838));
#63969=CARTESIAN_POINT('Ctrl Pts',(-24.0833187197589,19.6518183356655,-9.31028746937815));
#63970=CARTESIAN_POINT('Ctrl Pts',(-24.19808617313,19.669243539498,-9.31614091767792));
#63971=CARTESIAN_POINT('Ctrl Pts',(-24.3117818802786,19.6916825827047,-9.32199436597769));
#63972=CARTESIAN_POINT('Ctrl Pts',(-24.4256068841349,19.7141471439762,-9.32785447091923));
#63973=CARTESIAN_POINT('Ctrl Pts',(-24.5383573032639,19.7416368452016,-9.33371457586078));
#63974=CARTESIAN_POINT('Ctrl Pts',(-24.6495660684615,19.7740111797835,-9.33957468080232));
#63975=CARTESIAN_POINT('Ctrl Pts',(-24.7608497258022,19.8064073164536,-9.34543873215777));
#63976=CARTESIAN_POINT('Ctrl Pts',(-24.8705892714847,19.843694503851,-9.35130278351322));
#63977=CARTESIAN_POINT('Ctrl Pts',(-24.9783363694817,19.8856835867499,-9.35716683486867));
#63978=CARTESIAN_POINT('Ctrl Pts',(-25.0862422651928,19.9277345531752,-9.36303952866524));
#63979=CARTESIAN_POINT('Ctrl Pts',(-25.1921494758554,19.9745010789984,-9.36891222246181));
#63980=CARTESIAN_POINT('Ctrl Pts',(-25.2956329831765,20.0257474487665,-9.37478491625838));
#63981=CARTESIAN_POINT('Ctrl Pts',(-25.3239650364131,20.0397778475618,-9.3763927615817));
#63982=CARTESIAN_POINT('Ctrl Pts',(-25.3521155786525,20.0541437897815,-9.37800060690502));
#63983=CARTESIAN_POINT('Ctrl Pts',(-25.3800762713059,20.0688398756086,-9.37960845222834));
#63984=CARTESIAN_POINT('Ctrl Pts',(-25.4821964742451,20.1225140562046,-9.38548074919705));
#63985=CARTESIAN_POINT('Ctrl Pts',(-25.5821241185022,20.1807751997085,-9.39135304616576));
#63986=CARTESIAN_POINT('Ctrl Pts',(-25.6794187405819,20.2434201720287,-9.39722534313448));
#63987=CARTESIAN_POINT('Ctrl Pts',(-25.7765872765583,20.3059839614399,-9.40309003007268));
#63988=CARTESIAN_POINT('Ctrl Pts',(-25.8711292316133,20.3729200602875,-9.40895471701089));
#63989=CARTESIAN_POINT('Ctrl Pts',(-25.962627504789,20.4439788816135,-9.4148194039491));
#63990=CARTESIAN_POINT('Ctrl Pts',(-26.0540316777186,20.51496462339,-9.42067805942392));
#63991=CARTESIAN_POINT('Ctrl Pts',(-26.1423980704441,20.5900644021111,-9.42653671489874));
#63992=CARTESIAN_POINT('Ctrl Pts',(-26.22733799644,20.6689850303249,-9.43239537037356));
#63993=CARTESIAN_POINT('Ctrl Pts',(-26.3155957507595,20.7509883677892,-9.43848287009146));
#63994=CARTESIAN_POINT('Ctrl Pts',(-26.4001535174605,20.8371168851691,-9.44457036980937));
#63995=CARTESIAN_POINT('Ctrl Pts',(-26.4806122800179,20.9269948727129,-9.45065786952727));
#63996=CARTESIAN_POINT('Ctrl Pts',(-26.5579567149051,21.0133939414335,-9.45650973961067));
#63997=CARTESIAN_POINT('Ctrl Pts',(-26.6315132652398,21.1032572783412,-9.46236160969407));
#63998=CARTESIAN_POINT('Ctrl Pts',(-26.7009652127677,21.1962137466861,-9.46821347977748));
#63999=CARTESIAN_POINT('Ctrl Pts',(-26.770406585605,21.2891560615634,-9.47406445886045));
#64000=CARTESIAN_POINT('Ctrl Pts',(-26.8357443509059,21.3851902403952,-9.47991543794342));
#64001=CARTESIAN_POINT('Ctrl Pts',(-26.8967030929787,21.4839133434487,-9.48576641702639));
#64002=CARTESIAN_POINT('Ctrl Pts',(-26.957667315829,21.5826453226593,-9.49161792216869));
#64003=CARTESIAN_POINT('Ctrl Pts',(-27.0142515155815,21.6840663549347,-9.49746942731099));
#64004=CARTESIAN_POINT('Ctrl Pts',(-27.0662248794965,21.7877465176648,-9.50332093245328));
#64005=CARTESIAN_POINT('Ctrl Pts',(-27.1182155026342,21.8914611103199,-9.50917438075306));
#64006=CARTESIAN_POINT('Ctrl Pts',(-27.1655920601704,21.9974359558161,-9.51502782905283));
#64007=CARTESIAN_POINT('Ctrl Pts',(-27.2081710662497,22.1052193159667,-9.52088127735261));
#64008=CARTESIAN_POINT('Ctrl Pts',(-27.2507984939047,22.2131252492026,-9.52674138229415));
#64009=CARTESIAN_POINT('Ctrl Pts',(-27.2886173284035,22.3228434174537,-9.53260148723569));
#64010=CARTESIAN_POINT('Ctrl Pts',(-27.3214933095986,22.4339049177895,-9.53846159217723));
#64011=CARTESIAN_POINT('Ctrl Pts',(-27.3543914307095,22.5450412110949,-9.54432564353268));
#64012=CARTESIAN_POINT('Ctrl Pts',(-27.3823399709694,22.6575222376193,-9.55018969488814));
#64013=CARTESIAN_POINT('Ctrl Pts',(-27.4052557252144,22.7708685583222,-9.55605374624359));
#64014=CARTESIAN_POINT('Ctrl Pts',(-27.4282052527067,22.8843819288756,-9.56192644004016));
#64015=CARTESIAN_POINT('Ctrl Pts',(-27.4461071269598,22.9987627319246,-9.56779913383674));
#64016=CARTESIAN_POINT('Ctrl Pts',(-27.458929918934,23.1135259782533,-9.57367182763331));
#64017=CARTESIAN_POINT('Ctrl Pts',(-27.4624405848774,23.144946235343,-9.57527967295662));
#64018=CARTESIAN_POINT('Ctrl Pts',(-27.4655708381191,23.1763951596308,-9.57688751827993));
#64019=CARTESIAN_POINT('Ctrl Pts',(-27.4683207142553,23.2078628168923,-9.57849536360323));
#64020=CARTESIAN_POINT('Ctrl Pts',(-27.4782068054665,23.3209923232696,-9.5842757350572));
#64021=CARTESIAN_POINT('Ctrl Pts',(-27.4831941018349,23.4345561225121,-9.59005610651116));
#64022=CARTESIAN_POINT('Ctrl Pts',(-27.483252021333,23.5482489098093,-9.59583647796514));
#64023=CARTESIAN_POINT('',(-27.4816334182501,23.5477124661267,-10.8458359655833));
#64024=CARTESIAN_POINT('Ctrl Pts',(-27.4884997658551,23.5482804171771,-9.59583821346848));
#64025=CARTESIAN_POINT('Ctrl Pts',(-27.4810825272021,24.740122181211,-9.65635290063834));
#64026=CARTESIAN_POINT('Ctrl Pts',(-26.2680084891369,27.2507034664838,-9.78316322493322));
#64027=CARTESIAN_POINT('Ctrl Pts',(-21.9924509892916,27.9336308163729,-9.97626918635299));
#64028=CARTESIAN_POINT('Ctrl Pts',(-19.0203850618263,24.6090497443562,-10.1751560977279));
#64029=CARTESIAN_POINT('Ctrl Pts',(-20.2108832697441,20.3115238051025,-10.3740430091028));
#64030=CARTESIAN_POINT('Ctrl Pts',(-24.4699786975713,18.9901149666739,-10.5729299204777));
#64031=CARTESIAN_POINT('Ctrl Pts',(-27.1694554347631,21.2586694379709,-10.7301939012821));
#64032=CARTESIAN_POINT('Ctrl Pts',(-27.481293475824,23.0585648994137,-10.8211622449617));
#64033=CARTESIAN_POINT('Ctrl Pts',(-27.4784306046326,23.5476944236682,-10.8458349515162));
#64034=CARTESIAN_POINT('',(-27.4832514227223,23.5532060332972,-12.0958364780106));
#64035=CARTESIAN_POINT('Ctrl Pts',(-27.4832517173407,23.5477215825155,-10.8458364779652));
#64036=CARTESIAN_POINT('Ctrl Pts',(-27.4833269687236,23.6646593820601,-10.8517278562073));
#64037=CARTESIAN_POINT('Ctrl Pts',(-27.4781826122975,23.781621427634,-10.8576192344494));
#64038=CARTESIAN_POINT('Ctrl Pts',(-27.467838789277,23.8981130129192,-10.8635106126916));
#64039=CARTESIAN_POINT('Ctrl Pts',(-27.4574941529768,24.0146137573178,-10.8694024541414));
#64040=CARTESIAN_POINT('Ctrl Pts',(-27.4419492720751,24.13064356402,-10.8752942955912));
#64041=CARTESIAN_POINT('Ctrl Pts',(-27.4212761986332,24.2457126455741,-10.8811861370411));
#64042=CARTESIAN_POINT('Ctrl Pts',(-27.4005967517939,24.3608172023081,-10.887079794914));
#64043=CARTESIAN_POINT('Ctrl Pts',(-27.3747860381708,24.4749600456985,-10.8929734527869));
#64044=CARTESIAN_POINT('Ctrl Pts',(-27.3439671552581,24.5876619759145,-10.8988671106598));
#64045=CARTESIAN_POINT('Ctrl Pts',(-27.3126633818392,24.7021371078438,-10.9048534967071));
#64046=CARTESIAN_POINT('Ctrl Pts',(-27.2761926203301,24.8151251812877,-10.9108398827545));
#64047=CARTESIAN_POINT('Ctrl Pts',(-27.234735882171,24.9261418586604,-10.9168262688018));
#64048=CARTESIAN_POINT('Ctrl Pts',(-27.1938437091846,25.0356466913384,-10.9227311311879));
#64049=CARTESIAN_POINT('Ctrl Pts',(-27.1481007359123,25.14323313963,-10.9286359935741));
#64050=CARTESIAN_POINT('Ctrl Pts',(-27.0977281388904,25.2484591788217,-10.9345408559603));
#64051=CARTESIAN_POINT('Ctrl Pts',(-27.0463123612841,25.3558643742918,-10.9405680038381));
#64052=CARTESIAN_POINT('Ctrl Pts',(-26.9900733111427,25.4608099245802,-10.946595151716));
#64053=CARTESIAN_POINT('Ctrl Pts',(-26.9292934144627,25.5628557495638,-10.9526222995939));
#64054=CARTESIAN_POINT('Ctrl Pts',(-26.8685135177827,25.6649015745475,-10.9586494474718));
#64055=CARTESIAN_POINT('Ctrl Pts',(-26.803193074387,25.7640473432371,-10.9646765953496));
#64056=CARTESIAN_POINT('Ctrl Pts',(-26.7336580624837,25.8598884827781,-10.9707037432275));
#64057=CARTESIAN_POINT('Ctrl Pts',(-26.6659095605565,25.9532672490881,-10.9765760401962));
#64058=CARTESIAN_POINT('Ctrl Pts',(-26.5939354620773,26.0438190247594,-10.9824483371649));
#64059=CARTESIAN_POINT('Ctrl Pts',(-26.5179998988967,26.1311369856097,-10.9883206341336));
#64060=CARTESIAN_POINT('Ctrl Pts',(-26.4421627421755,26.2183417893172,-10.9941853210718));
#64061=CARTESIAN_POINT('Ctrl Pts',(-26.3623745986895,26.3023208030858,-11.00005000801));
#64062=CARTESIAN_POINT('Ctrl Pts',(-26.2789422276475,26.3826969783159,-11.0059146949482));
#64063=CARTESIAN_POINT('Ctrl Pts',(-26.195595661576,26.4629904916816,-11.011773350423));
#64064=CARTESIAN_POINT('Ctrl Pts',(-26.1086126185523,26.5396882514509,-11.0176320058978));
#64065=CARTESIAN_POINT('Ctrl Pts',(-26.018338938545,26.6124475758281,-11.0234906613727));
#64066=CARTESIAN_POINT('Ctrl Pts',(-25.9245390890847,26.688048943501,-11.0295781610906));
#64067=CARTESIAN_POINT('Ctrl Pts',(-25.8271865899897,26.7593975828396,-11.0356656608085));
#64068=CARTESIAN_POINT('Ctrl Pts',(-25.7267104322242,26.8261524091661,-11.0417531605264));
#64069=CARTESIAN_POINT('Ctrl Pts',(-25.6301234180198,26.8903233478445,-11.0476050306098));
#64070=CARTESIAN_POINT('Ctrl Pts',(-25.5306504409234,26.950249237449,-11.0534569006932));
#64071=CARTESIAN_POINT('Ctrl Pts',(-25.4287041775526,27.0056697878547,-11.0593087707766));
#64072=CARTESIAN_POINT('Ctrl Pts',(-25.3267734364273,27.0610818999778,-11.0651597498595));
#64073=CARTESIAN_POINT('Ctrl Pts',(-25.2223705208762,27.1119898394649,-11.0710107289425));
#64074=CARTESIAN_POINT('Ctrl Pts',(-25.115933666313,27.1581787483315,-11.0768617080255));
#64075=CARTESIAN_POINT('Ctrl Pts',(-25.0094872420524,27.2043718100255,-11.0827132131677));
#64076=CARTESIAN_POINT('Ctrl Pts',(-24.9010068944877,27.2458448330844,-11.08856471831));
#64077=CARTESIAN_POINT('Ctrl Pts',(-24.7909511746775,27.2824309675811,-11.0944162234523));
#64078=CARTESIAN_POINT('Ctrl Pts',(-24.6808589077582,27.3190292515368,-11.1002696717521));
#64079=CARTESIAN_POINT('Ctrl Pts',(-24.5691906204166,27.3507372897001,-11.1061231200519));
#64080=CARTESIAN_POINT('Ctrl Pts',(-24.4564196751618,27.3774381958735,-11.1119765683517));
#64081=CARTESIAN_POINT('Ctrl Pts',(-24.343520484855,27.4041694667752,-11.1178366732932));
#64082=CARTESIAN_POINT('Ctrl Pts',(-24.2295165362655,27.4258821449429,-11.1236967782348));
#64083=CARTESIAN_POINT('Ctrl Pts',(-24.1148911284914,27.4425105209604,-11.1295568831763));
#64084=CARTESIAN_POINT('Ctrl Pts',(-24.000188527679,27.4591500951486,-11.1354209345318));
#64085=CARTESIAN_POINT('Ctrl Pts',(-23.8848640446584,27.4706985083149,-11.1412849858872));
#64086=CARTESIAN_POINT('Ctrl Pts',(-23.7694040928103,27.4771420887432,-11.1471490372427));
#64087=CARTESIAN_POINT('Ctrl Pts',(-23.6537739760415,27.4835951657228,-11.1530217310392));
#64088=CARTESIAN_POINT('Ctrl Pts',(-23.5380084037779,27.4849283897584,-11.1588944248358));
#64089=CARTESIAN_POINT('Ctrl Pts',(-23.4225918658673,27.4811801263467,-11.1647671186324));
#64090=CARTESIAN_POINT('Ctrl Pts',(-23.3909927484701,27.4801539145254,-11.1663749639557));
#64091=CARTESIAN_POINT('Ctrl Pts',(-23.3594197502655,27.4787471065669,-11.167982809279));
#64092=CARTESIAN_POINT('Ctrl Pts',(-23.3278826979357,27.4769611606905,-11.1695906546024));
#64093=CARTESIAN_POINT('Ctrl Pts',(-23.2127006377526,27.4704383911156,-11.1754629515711));
#64094=CARTESIAN_POINT('Ctrl Pts',(-23.0976128581538,27.4588324479783,-11.1813352485398));
#64095=CARTESIAN_POINT('Ctrl Pts',(-22.9831044016121,27.4421456441196,-11.1872075455085));
#64096=CARTESIAN_POINT('Ctrl Pts',(-22.8687443389359,27.4254804650334,-11.1930722324467));
#64097=CARTESIAN_POINT('Ctrl Pts',(-22.7549625116179,27.4037475782785,-11.1989369193849));
#64098=CARTESIAN_POINT('Ctrl Pts',(-22.6422419533278,27.3770012547716,-11.2048016063231));
#64099=CARTESIAN_POINT('Ctrl Pts',(-22.5296373210751,27.3502824381841,-11.2106602617979));
#64100=CARTESIAN_POINT('Ctrl Pts',(-22.4180921866996,27.3185605352692,-11.2165189172728));
#64101=CARTESIAN_POINT('Ctrl Pts',(-22.30808179531,27.2819412729574,-11.2223775727476));
#64102=CARTESIAN_POINT('Ctrl Pts',(-22.1937743011372,27.243891630006,-11.2284650724655));
#64103=CARTESIAN_POINT('Ctrl Pts',(-22.0811243409304,27.2005543033591,-11.2345525721834));
#64104=CARTESIAN_POINT('Ctrl Pts',(-21.9706507627541,27.1521058395847,-11.2406400719013));
#64105=CARTESIAN_POINT('Ctrl Pts',(-21.8644532995766,27.1055326767285,-11.2464919419847));
#64106=CARTESIAN_POINT('Ctrl Pts',(-21.7602672821216,27.0542368758851,-11.2523438120681));
#64107=CARTESIAN_POINT('Ctrl Pts',(-21.6585347660448,26.9984249309699,-11.2581956821515));
#64108=CARTESIAN_POINT('Ctrl Pts',(-21.5568177396686,26.9426214839307,-11.2640466612345));
#64109=CARTESIAN_POINT('Ctrl Pts',(-21.457553834223,26.8823034588131,-11.2698976403174));
#64110=CARTESIAN_POINT('Ctrl Pts',(-21.3611606981547,26.8177234105745,-11.2757486194004));
#64111=CARTESIAN_POINT('Ctrl Pts',(-21.2647588954157,26.7531375559679,-11.2816001245427));
#64112=CARTESIAN_POINT('Ctrl Pts',(-21.1712287186044,26.6842891465812,-11.287451629685));
#64113=CARTESIAN_POINT('Ctrl Pts',(-21.0809584076506,26.6114737796545,-11.2933031348273));
#64114=CARTESIAN_POINT('Ctrl Pts',(-20.9906581198916,26.5386342323296,-11.2991565831271));
#64115=CARTESIAN_POINT('Ctrl Pts',(-20.9036201721168,26.4618253674175,-11.3050100314268));
#64116=CARTESIAN_POINT('Ctrl Pts',(-20.820198775149,26.3813822507946,-11.3108634797266));
#64117=CARTESIAN_POINT('Ctrl Pts',(-20.7366825099383,26.3008476528803,-11.3167235846682));
#64118=CARTESIAN_POINT('Ctrl Pts',(-20.6567913023122,26.2166708411609,-11.3225836896097));
#64119=CARTESIAN_POINT('Ctrl Pts',(-20.5808416783557,26.1292229045515,-11.3284437945512));
#64120=CARTESIAN_POINT('Ctrl Pts',(-20.5048409070811,26.04171607723,-11.3343078459067));
#64121=CARTESIAN_POINT('Ctrl Pts',(-20.4327872612978,25.9509340616106,-11.3401718972621));
#64122=CARTESIAN_POINT('Ctrl Pts',(-20.3649551703029,25.8572786952896,-11.3460359486175));
#64123=CARTESIAN_POINT('Ctrl Pts',(-20.2970231083467,25.7634852996543,-11.3519086424141));
#64124=CARTESIAN_POINT('Ctrl Pts',(-20.2333252451369,25.6668104454763,-11.3577813362107));
#64125=CARTESIAN_POINT('Ctrl Pts',(-20.1740911904395,25.5676824803709,-11.3636540300072));
#64126=CARTESIAN_POINT('Ctrl Pts',(-20.1578738971279,25.540542901733,-11.3652618753306));
#64127=CARTESIAN_POINT('Ctrl Pts',(-20.1419909242631,25.5132195692635,-11.3668697206539));
#64128=CARTESIAN_POINT('Ctrl Pts',(-20.1264463567591,25.485721538544,-11.3684775659772));
#64129=CARTESIAN_POINT('Ctrl Pts',(-20.0696732858,25.3852911052837,-11.374349862946));
#64130=CARTESIAN_POINT('Ctrl Pts',(-20.0172277366982,25.2821923210592,-11.3802221599147));
#64131=CARTESIAN_POINT('Ctrl Pts',(-19.9693699496409,25.1768345104299,-11.3860944568834));
#64132=CARTESIAN_POINT('Ctrl Pts',(-19.9215741824751,25.0716132351559,-11.3919591438216));
#64133=CARTESIAN_POINT('Ctrl Pts',(-19.8783545235224,24.9641391281602,-11.3978238307598));
#64134=CARTESIAN_POINT('Ctrl Pts',(-19.8399264139257,24.8548479095048,-11.403688517698));
#64135=CARTESIAN_POINT('Ctrl Pts',(-19.8015378252342,24.7456690900264,-11.4095471731728));
#64136=CARTESIAN_POINT('Ctrl Pts',(-19.7679311205307,24.6346772636328,-11.4154058286476));
#64137=CARTESIAN_POINT('Ctrl Pts',(-19.7392742401032,24.5223294118957,-11.4212644841224));
#64138=CARTESIAN_POINT('Ctrl Pts',(-19.7094979966855,24.4055931541146,-11.4273519838403));
#64139=CARTESIAN_POINT('Ctrl Pts',(-19.6850663376552,24.2873931902714,-11.4334394835582));
#64140=CARTESIAN_POINT('Ctrl Pts',(-19.6661111907973,24.1682614668524,-11.4395269832761));
#64141=CARTESIAN_POINT('Ctrl Pts',(-19.6478897432466,24.0537409903734,-11.4453788533595));
#64142=CARTESIAN_POINT('Ctrl Pts',(-19.6347288019565,23.9383599908905,-11.4512307234429));
#64143=CARTESIAN_POINT('Ctrl Pts',(-19.6266935899533,23.8226019959587,-11.4570825935263));
#64144=CARTESIAN_POINT('Ctrl Pts',(-19.6186596013842,23.7068616262343,-11.4629335726092));
#64145=CARTESIAN_POINT('Ctrl Pts',(-19.6157498189573,23.59074478747,-11.4687845516922));
#64146=CARTESIAN_POINT('Ctrl Pts',(-19.6179775206404,23.4747393709723,-11.4746355307752));
#64147=CARTESIAN_POINT('Ctrl Pts',(-19.6202054226154,23.3587235244714,-11.4804870359175));
#64148=CARTESIAN_POINT('Ctrl Pts',(-19.6275717189959,23.2428195334831,-11.4863385410597));
#64149=CARTESIAN_POINT('Ctrl Pts',(-19.6400375790048,23.1275138136139,-11.492190046202));
#64150=CARTESIAN_POINT('Ctrl Pts',(-19.6525075786544,23.0121698032251,-11.4980434945018));
#64151=CARTESIAN_POINT('Ctrl Pts',(-19.6700804648502,22.8974248697742,-11.5038969428016));
#64152=CARTESIAN_POINT('Ctrl Pts',(-19.6926658070144,22.78375813408,-11.5097503911013));
#64153=CARTESIAN_POINT('Ctrl Pts',(-19.7152768336169,22.6699621346249,-11.5156104960429));
#64154=CARTESIAN_POINT('Ctrl Pts',(-19.7429116131051,22.5572471859717,-11.5214706009844));
#64155=CARTESIAN_POINT('Ctrl Pts',(-19.7754290379162,22.4460801761168,-11.527330705926));
#64156=CARTESIAN_POINT('Ctrl Pts',(-19.8079683611775,22.3348383022388,-11.5331947572814));
#64157=CARTESIAN_POINT('Ctrl Pts',(-19.8453967439644,22.2251468331425,-11.5390588086368));
#64158=CARTESIAN_POINT('Ctrl Pts',(-19.8875244542338,22.1174538610558,-11.5449228599923));
#64159=CARTESIAN_POINT('Ctrl Pts',(-19.9297142523388,22.0096021710255,-11.5507955537888));
#64160=CARTESIAN_POINT('Ctrl Pts',(-19.9766170337844,21.9037552329472,-11.5566682475854));
#64161=CARTESIAN_POINT('Ctrl Pts',(-20.0279965363475,21.8003377614141,-11.562540941382));
#64162=CARTESIAN_POINT('Ctrl Pts',(-20.0420633846754,21.772023787671,-11.5641487867053));
#64163=CARTESIAN_POINT('Ctrl Pts',(-20.0564655425593,21.7438917565931,-11.5657566320287));
#64164=CARTESIAN_POINT('Ctrl Pts',(-20.0711975994555,21.715949999813,-11.5673644773521));
#64165=CARTESIAN_POINT('Ctrl Pts',(-20.1250031563694,21.613898955937,-11.5732367743208));
#64166=CARTESIAN_POINT('Ctrl Pts',(-20.1833928507401,21.5140463719922,-11.5791090712895));
#64167=CARTESIAN_POINT('Ctrl Pts',(-20.246162981802,21.4168324496913,-11.5849813682582));
#64168=CARTESIAN_POINT('Ctrl Pts',(-20.3088517677592,21.3197445089131,-11.5908460551964));
#64169=CARTESIAN_POINT('Ctrl Pts',(-20.3759094793266,21.2252887737039,-11.5967107421346));
#64170=CARTESIAN_POINT('Ctrl Pts',(-20.4470859929765,21.1338820234768,-11.6025754290728));
#64171=CARTESIAN_POINT('Ctrl Pts',(-20.5181893060374,21.0425692793706,-11.6084340845477));
#64172=CARTESIAN_POINT('Ctrl Pts',(-20.5934027432491,20.9542996073988,-11.6142927400225));
#64173=CARTESIAN_POINT('Ctrl Pts',(-20.6724326171932,20.8694613164554,-11.6201513954973));
#64174=CARTESIAN_POINT('Ctrl Pts',(-20.7545494676223,20.7813091671431,-11.6262388952152));
#64175=CARTESIAN_POINT('Ctrl Pts',(-20.8407867329545,20.6968623111711,-11.6323263949331));
#64176=CARTESIAN_POINT('Ctrl Pts',(-20.930768190246,20.6165192812252,-11.638413894651));
#64177=CARTESIAN_POINT('Ctrl Pts',(-21.0172667236974,20.5392860992724,-11.6442657647344));
#64178=CARTESIAN_POINT('Ctrl Pts',(-21.1072246477542,20.4658452569793,-11.6501176348178));
#64179=CARTESIAN_POINT('Ctrl Pts',(-21.200270418382,20.3965129947139,-11.6559695049012));
#64180=CARTESIAN_POINT('Ctrl Pts',(-21.2933020219452,20.3271912889158,-11.6618204839842));
#64181=CARTESIAN_POINT('Ctrl Pts',(-21.3894202058785,20.2619771662448,-11.6676714630671));
#64182=CARTESIAN_POINT('Ctrl Pts',(-21.4882216763444,20.201145523612,-11.6735224421501));
#64183=CARTESIAN_POINT('Ctrl Pts',(-21.5870320300134,20.1403084116291,-11.6793739472924));
#64184=CARTESIAN_POINT('Ctrl Pts',(-21.6885257977711,20.0838547797193,-11.6852254524347));
#64185=CARTESIAN_POINT('Ctrl Pts',(-21.7922727603254,20.0320148871542,-11.691076957577));
#64186=CARTESIAN_POINT('Ctrl Pts',(-21.8960541749875,19.9801577796893,-11.6969304058768));
#64187=CARTESIAN_POINT('Ctrl Pts',(-22.0020899026752,19.9329176427749,-11.7027838541766));
#64188=CARTESIAN_POINT('Ctrl Pts',(-22.1099279694438,19.8904773807623,-11.7086373024764));
#64189=CARTESIAN_POINT('Ctrl Pts',(-22.217888671511,19.8479888549562,-11.7144974074179));
#64190=CARTESIAN_POINT('Ctrl Pts',(-22.327655418807,19.81031125053,-11.7203575123595));
#64191=CARTESIAN_POINT('Ctrl Pts',(-22.4387591360074,19.7775782240784,-11.726217617301));
#64192=CARTESIAN_POINT('Ctrl Pts',(-22.5499376746075,19.7448231539821,-11.7320816686565));
#64193=CARTESIAN_POINT('Ctrl Pts',(-22.6624545755873,19.7170193912054,-11.7379457200119));
#64194=CARTESIAN_POINT('Ctrl Pts',(-22.7758302932245,19.6942495238422,-11.7438097713674));
#64195=CARTESIAN_POINT('Ctrl Pts',(-22.8893731040377,19.6714460982398,-11.749682465164));
#64196=CARTESIAN_POINT('Ctrl Pts',(-23.0037768506907,19.6536914380151,-11.7555551589606));
#64197=CARTESIAN_POINT('Ctrl Pts',(-23.1185565039226,19.6410163480381,-11.7614278527571));
#64198=CARTESIAN_POINT('Ctrl Pts',(-23.1499812529472,19.6375461204309,-11.7630356980804));
#64199=CARTESIAN_POINT('Ctrl Pts',(-23.1814341795848,19.6344563421027,-11.7646435434037));
#64200=CARTESIAN_POINT('Ctrl Pts',(-23.2129053496646,19.6317469646729,-11.766251388727));
#64201=CARTESIAN_POINT('Ctrl Pts',(-23.3278467896063,19.6218515670017,-11.7721236856957));
#64202=CARTESIAN_POINT('Ctrl Pts',(-23.4434165489523,19.6170012418788,-11.7779959826644));
#64203=CARTESIAN_POINT('Ctrl Pts',(-23.5591341697166,19.6172625601196,-11.7838682796331));
#64204=CARTESIAN_POINT('Ctrl Pts',(-23.6747018296348,19.6175235397128,-11.7897329665713));
#64205=CARTESIAN_POINT('Ctrl Pts',(-23.7904165603483,19.6228829884219,-11.7955976535095));
#64206=CARTESIAN_POINT('Ctrl Pts',(-23.9057925159736,19.6333557600676,-11.8014623404477));
#64207=CARTESIAN_POINT('Ctrl Pts',(-24.0210498146512,19.6438177611234,-11.8073209959226));
#64208=CARTESIAN_POINT('Ctrl Pts',(-24.1359686220287,19.6593825880814,-11.8131796513974));
#64209=CARTESIAN_POINT('Ctrl Pts',(-24.2500634968185,19.6800130542081,-11.8190383068722));
#64210=CARTESIAN_POINT('Ctrl Pts',(-24.3686150179109,19.7014493645127,-11.8251258065901));
#64211=CARTESIAN_POINT('Ctrl Pts',(-24.4862764724795,19.7283551171377,-11.831213306308));
#64212=CARTESIAN_POINT('Ctrl Pts',(-24.602509203839,19.7606292132196,-11.8373008060259));
#64213=CARTESIAN_POINT('Ctrl Pts',(-24.7142428999168,19.7916540717136,-11.8431526761093));
#64214=CARTESIAN_POINT('Ctrl Pts',(-24.8246559842864,19.8276392939211,-11.8490045461927));
#64215=CARTESIAN_POINT('Ctrl Pts',(-24.9332815633186,19.8684432349375,-11.8548564162761));
#64216=CARTESIAN_POINT('Ctrl Pts',(-25.0418906031188,19.9092409631829,-11.8607073953591));
#64217=CARTESIAN_POINT('Ctrl Pts',(-25.1487122918557,19.9548558060941,-11.8665583744421));
#64218=CARTESIAN_POINT('Ctrl Pts',(-25.2532973567295,20.0050970592332,-11.872409353525));
#64219=CARTESIAN_POINT('Ctrl Pts',(-25.357891824807,20.0553428295443,-11.8782608586673));
#64220=CARTESIAN_POINT('Ctrl Pts',(-25.4602488966248,20.1102156579598,-11.8841123638096));
#64221=CARTESIAN_POINT('Ctrl Pts',(-25.5599422994288,20.1694780586684,-11.8899638689519));
#64222=CARTESIAN_POINT('Ctrl Pts',(-25.6596688082408,20.2287601391297,-11.8958173172517));
#64223=CARTESIAN_POINT('Ctrl Pts',(-25.7567295340216,20.2924344792726,-11.9016707655514));
#64224=CARTESIAN_POINT('Ctrl Pts',(-25.8507262851938,20.3602196933899,-11.9075242138511));
#64225=CARTESIAN_POINT('Ctrl Pts',(-25.9448299310837,20.4280819940155,-11.9133843187927));
#64226=CARTESIAN_POINT('Ctrl Pts',(-26.0358623121079,20.5000642577497,-11.9192444237342));
#64227=CARTESIAN_POINT('Ctrl Pts',(-26.1234574256321,20.5758440907073,-11.9251045286757));
#64228=CARTESIAN_POINT('Ctrl Pts',(-26.2111115289827,20.6516749566393,-11.9309685800312));
#64229=CARTESIAN_POINT('Ctrl Pts',(-26.2953234560146,20.7313082008036,-11.9368326313866));
#64230=CARTESIAN_POINT('Ctrl Pts',(-26.3757645091863,20.8143850157043,-11.9426966827421));
#64231=CARTESIAN_POINT('Ctrl Pts',(-26.4563241164129,20.8975842692466,-11.9485693765386));
#64232=CARTESIAN_POINT('Ctrl Pts',(-26.533101484937,20.9842369142749,-11.9544420703352));
#64233=CARTESIAN_POINT('Ctrl Pts',(-26.6058085192272,21.0739515388722,-11.9603147641318));
#64234=CARTESIAN_POINT('Ctrl Pts',(-26.6257144889762,21.0985139023452,-11.9619226094551));
#64235=CARTESIAN_POINT('Ctrl Pts',(-26.6453156115578,21.1233056210805,-11.9635304547785));
#64236=CARTESIAN_POINT('Ctrl Pts',(-26.664606557835,21.1483183111418,-11.9651383001019));
#64237=CARTESIAN_POINT('Ctrl Pts',(-26.7351444391807,21.2397779076973,-11.9710174312245));
#64238=CARTESIAN_POINT('Ctrl Pts',(-26.8017714608122,21.3345047763228,-11.9768965623471));
#64239=CARTESIAN_POINT('Ctrl Pts',(-26.8641701381952,21.4321309352501,-11.9827756934698));
#64240=CARTESIAN_POINT('Ctrl Pts',(-26.9264889862588,21.5296321968215,-11.9886473031664));
#64241=CARTESIAN_POINT('Ctrl Pts',(-26.9845900250466,21.630025031603,-11.9945189128629));
#64242=CARTESIAN_POINT('Ctrl Pts',(-27.0381961265906,21.732908734054,-12.0003905225595));
#64243=CARTESIAN_POINT('Ctrl Pts',(-27.0917465023943,21.8356854846784,-12.0062560284771));
#64244=CARTESIAN_POINT('Ctrl Pts',(-27.1408110437252,21.9409475915276,-12.0121215343947));
#64245=CARTESIAN_POINT('Ctrl Pts',(-27.1851564316397,22.0482663006784,-12.0179870403123));
#64246=CARTESIAN_POINT('Ctrl Pts',(-27.2294663524372,22.1554991771106,-12.0238478550412));
#64247=CARTESIAN_POINT('Ctrl Pts',(-27.2690644708402,22.2647850052192,-12.02970866977));
#64248=CARTESIAN_POINT('Ctrl Pts',(-27.3037641718483,22.3756720247779,-12.0355694844989));
#64249=CARTESIAN_POINT('Ctrl Pts',(-27.338445871842,22.4865015199552,-12.0414272588381));
#64250=CARTESIAN_POINT('Ctrl Pts',(-27.3682340864401,22.5989301623155,-12.0472850331774));
#64251=CARTESIAN_POINT('Ctrl Pts',(-27.3929911871134,22.7124884681613,-12.0531428075167));
#64252=CARTESIAN_POINT('Ctrl Pts',(-27.417740802691,22.8260124406337,-12.0589988108084));
#64253=CARTESIAN_POINT('Ctrl Pts',(-27.437462245683,22.9406649946853,-12.0648548141001));
#64254=CARTESIAN_POINT('Ctrl Pts',(-27.4520685658512,23.0559645229432,-12.0707108173919));
#64255=CARTESIAN_POINT('Ctrl Pts',(-27.4666766293965,23.1712778130894,-12.0765675196428));
#64256=CARTESIAN_POINT('Ctrl Pts',(-27.4761682968273,23.287237823602,-12.0824242218937));
#64257=CARTESIAN_POINT('Ctrl Pts',(-27.4805083110525,23.4033562797998,-12.0882809241447));
#64258=CARTESIAN_POINT('Ctrl Pts',(-27.4823746179294,23.4532899118315,-12.0907994420848));
#64259=CARTESIAN_POINT('Ctrl Pts',(-27.483288935297,23.5032527983013,-12.093317960025));
#64260=CARTESIAN_POINT('Ctrl Pts',(-27.483251422723,23.5532060323939,-12.0958364779651));
#64261=CARTESIAN_POINT('',(-27.48469778642,23.5516324603682,-13.3458364779651));
#64262=CARTESIAN_POINT('Ctrl Pts',(-27.4832514227223,23.5532060332972,-12.0958364780106));
#64263=CARTESIAN_POINT('Ctrl Pts',(-27.4831507123894,23.6873158733359,-12.102597962912));
#64264=CARTESIAN_POINT('Ctrl Pts',(-27.4761866223843,23.8211447706251,-12.1093594478134));
#64265=CARTESIAN_POINT('Ctrl Pts',(-27.4624688174035,23.9540504190472,-12.1161209327148));
#64266=CARTESIAN_POINT('Ctrl Pts',(-27.4486733708594,24.0877083016881,-12.1229206870228));
#64267=CARTESIAN_POINT('Ctrl Pts',(-27.4280476574859,24.2204323263878,-12.1297204413309));
#64268=CARTESIAN_POINT('Ctrl Pts',(-27.4007524368963,24.3515885910592,-12.136520195639));
#64269=CARTESIAN_POINT('Ctrl Pts',(-27.3732778581082,24.4836066898115,-12.1433646314574));
#64270=CARTESIAN_POINT('Ctrl Pts',(-27.3390459221007,24.6140362322264,-12.1502090672759));
#64271=CARTESIAN_POINT('Ctrl Pts',(-27.2982687712955,24.7422522245149,-12.1570535030943));
#64272=CARTESIAN_POINT('Ctrl Pts',(-27.2844236367647,24.7857856158181,-12.1593774058885));
#64273=CARTESIAN_POINT('Ctrl Pts',(-27.2698243598901,24.8290640152035,-12.1617013086826));
#64274=CARTESIAN_POINT('Ctrl Pts',(-27.2544804696585,24.8720635558593,-12.1640252114768));
#64275=CARTESIAN_POINT('Ctrl Pts',(-27.2157078151732,24.9807195946939,-12.1698975084455));
#64276=CARTESIAN_POINT('Ctrl Pts',(-27.1720853447534,25.0878502392532,-12.1757698054142));
#64277=CARTESIAN_POINT('Ctrl Pts',(-27.1237522016443,25.1929908276094,-12.181642102383));
#64278=CARTESIAN_POINT('Ctrl Pts',(-27.0754816944502,25.2979951621133,-12.1875067893212));
#64279=CARTESIAN_POINT('Ctrl Pts',(-27.022512825608,25.4010141968992,-12.1933714762594));
#64280=CARTESIAN_POINT('Ctrl Pts',(-26.9650340161279,25.5015998645821,-12.1992361631976));
#64281=CARTESIAN_POINT('Ctrl Pts',(-26.9076143200052,25.6020820862025,-12.2050948186725));
#64282=CARTESIAN_POINT('Ctrl Pts',(-26.845694112712,25.7001355616948,-12.2109534741473));
#64283=CARTESIAN_POINT('Ctrl Pts',(-26.7795089797908,25.7953342211715,-12.2168121296222));
#64284=CARTESIAN_POINT('Ctrl Pts',(-26.7107385972829,25.8942514241368,-12.2228996293401));
#64285=CARTESIAN_POINT('Ctrl Pts',(-26.6373635032458,25.9900858281394,-12.228987129058));
#64286=CARTESIAN_POINT('Ctrl Pts',(-26.559699531327,26.0823895256978,-12.2350746287759));
#64287=CARTESIAN_POINT('Ctrl Pts',(-26.4850417087573,26.1711204121637,-12.2409264988593));
#64288=CARTESIAN_POINT('Ctrl Pts',(-26.4064211459179,26.256588491095,-12.2467783689427));
#64289=CARTESIAN_POINT('Ctrl Pts',(-26.324160727766,26.3384279780687,-12.2526302390261));
#64290=CARTESIAN_POINT('Ctrl Pts',(-26.2419128345107,26.4202550042363,-12.2584812181091));
#64291=CARTESIAN_POINT('Ctrl Pts',(-26.1560264808464,26.4984542454905,-12.2643321971921));
#64292=CARTESIAN_POINT('Ctrl Pts',(-26.0668618493745,26.572696334673,-12.2701831762751));
#64293=CARTESIAN_POINT('Ctrl Pts',(-25.9776892011441,26.6469450989337,-12.2760346814174));
#64294=CARTESIAN_POINT('Ctrl Pts',(-25.8852380068696,26.7172357393258,-12.2818861865597));
#64295=CARTESIAN_POINT('Ctrl Pts',(-25.7899014389786,26.7832792516735,-12.287737691702));
#64296=CARTESIAN_POINT('Ctrl Pts',(-25.694533211889,26.8493446956338,-12.2935911400018));
#64297=CARTESIAN_POINT('Ctrl Pts',(-25.5962780455541,26.9111599718238,-12.2994445883016));
#64298=CARTESIAN_POINT('Ctrl Pts',(-25.4955573695643,26.9684798628937,-12.3052980366013));
#64299=CARTESIAN_POINT('Ctrl Pts',(-25.3947221522947,27.0258649391266,-12.3111581415429));
#64300=CARTESIAN_POINT('Ctrl Pts',(-25.2914161885206,27.0787442217997,-12.3170182464845));
#64301=CARTESIAN_POINT('Ctrl Pts',(-25.1860848275753,27.1269188146667,-12.322878351426));
#64302=CARTESIAN_POINT('Ctrl Pts',(-25.080682532551,27.1751258501068,-12.3287424027815));
#64303=CARTESIAN_POINT('Ctrl Pts',(-24.9732525066363,27.2186217322415,-12.334606454137));
#64304=CARTESIAN_POINT('Ctrl Pts',(-24.8642577135746,27.2572566296136,-12.3404705054924));
#64305=CARTESIAN_POINT('Ctrl Pts',(-24.7551022839451,27.2959484671123,-12.346343199289));
#64306=CARTESIAN_POINT('Ctrl Pts',(-24.6443778784001,27.3297649013522,-12.3522158930856));
#64307=CARTESIAN_POINT('Ctrl Pts',(-24.5325602402114,27.3586065811213,-12.3580885868822));
#64308=CARTESIAN_POINT('Ctrl Pts',(-24.5019464413595,27.3665029505788,-12.3596964322053));
#64309=CARTESIAN_POINT('Ctrl Pts',(-24.4712507388927,27.3740267245054,-12.3613042775285));
#64310=CARTESIAN_POINT('Ctrl Pts',(-24.4404829732302,27.3811765404632,-12.3629121228517));
#64311=CARTESIAN_POINT('Ctrl Pts',(-24.3281105612624,27.4072896509539,-12.3687844198204));
#64312=CARTESIAN_POINT('Ctrl Pts',(-24.2143999579809,27.4284979896557,-12.3746567167891));
#64313=CARTESIAN_POINT('Ctrl Pts',(-24.0998173040847,27.4446674506451,-12.3805290137578));
#64314=CARTESIAN_POINT('Ctrl Pts',(-23.985383140208,27.4608159572972,-12.386393700696));
#64315=CARTESIAN_POINT('Ctrl Pts',(-23.8700795786453,27.4719385148041,-12.3922583876342));
#64316=CARTESIAN_POINT('Ctrl Pts',(-23.7543854355493,27.4779514455067,-12.3981230745724));
#64317=CARTESIAN_POINT('Ctrl Pts',(-23.6388102766371,27.4839581922864,-12.4039817300472));
#64318=CARTESIAN_POINT('Ctrl Pts',(-23.5228457455147,27.4848657432637,-12.409840385522));
#64319=CARTESIAN_POINT('Ctrl Pts',(-23.4069776459001,27.4806419916715,-12.4156990409968));
#64320=CARTESIAN_POINT('Ctrl Pts',(-23.2865836362589,27.4762532566219,-12.4217865407147));
#64321=CARTESIAN_POINT('Ctrl Pts',(-23.1662941953199,27.4663241169753,-12.4278740404326));
#64322=CARTESIAN_POINT('Ctrl Pts',(-23.046656876638,27.4508781758965,-12.4339615401505));
#64323=CARTESIAN_POINT('Ctrl Pts',(-22.9316503750372,27.4360301028456,-12.4398134102339));
#64324=CARTESIAN_POINT('Ctrl Pts',(-22.8172468990511,27.4160844241251,-12.4456652803173));
#64325=CARTESIAN_POINT('Ctrl Pts',(-22.7039287222596,27.3911150662799,-12.4515171504007));
#64326=CARTESIAN_POINT('Ctrl Pts',(-22.590627799191,27.3661495102465,-12.4573681294837));
#64327=CARTESIAN_POINT('Ctrl Pts',(-22.4784122503415,27.3361618848855,-12.4632191085667));
#64328=CARTESIAN_POINT('Ctrl Pts',(-22.3677538717931,27.301277180951,-12.4690700876496));
#64329=CARTESIAN_POINT('Ctrl Pts',(-22.2570855439913,27.2663893405458,-12.4749215927919));
#64330=CARTESIAN_POINT('Ctrl Pts',(-22.1479750590864,27.2266036705977,-12.4807730979342));
#64331=CARTESIAN_POINT('Ctrl Pts',(-22.0408780875052,27.182094734658,-12.4866246030765));
#64332=CARTESIAN_POINT('Ctrl Pts',(-21.9337455513511,27.1375710182696,-12.4924780513763));
#64333=CARTESIAN_POINT('Ctrl Pts',(-21.8286282396043,27.0883210755992,-12.4983314996761));
#64334=CARTESIAN_POINT('Ctrl Pts',(-21.725960258295,27.0345669120589,-12.5041849479758));
#64335=CARTESIAN_POINT('Ctrl Pts',(-21.6231755211971,26.9807516183621,-12.5100450529174));
#64336=CARTESIAN_POINT('Ctrl Pts',(-21.5228460405923,26.9224220717432,-12.5159051578589));
#64337=CARTESIAN_POINT('Ctrl Pts',(-21.425379881424,26.8598454402154,-12.5217652628004));
#64338=CARTESIAN_POINT('Ctrl Pts',(-21.3278480848978,26.7972266672428,-12.5276293141559));
#64339=CARTESIAN_POINT('Ctrl Pts',(-21.2331837861844,26.7303553521689,-12.5334933655113));
#64340=CARTESIAN_POINT('Ctrl Pts',(-21.1417632925323,26.6595400039041,-12.5393574168668));
#64341=CARTESIAN_POINT('Ctrl Pts',(-21.0502080633219,26.5886202879521,-12.5452301106633));
#64342=CARTESIAN_POINT('Ctrl Pts',(-20.9619064946779,26.5137452040934,-12.5511028044599));
#64343=CARTESIAN_POINT('Ctrl Pts',(-20.8771993318483,26.4352612995827,-12.5569754982565));
#64344=CARTESIAN_POINT('Ctrl Pts',(-20.8540079276428,26.4137737194026,-12.5585833435798));
#64345=CARTESIAN_POINT('Ctrl Pts',(-20.831085721933,26.3920158286571,-12.5601911889032));
#64346=CARTESIAN_POINT('Ctrl Pts',(-20.8084391801246,26.3699951698005,-12.5617990342266));
#64347=CARTESIAN_POINT('Ctrl Pts',(-20.7257277296633,26.2895696174335,-12.5676713311953));
#64348=CARTESIAN_POINT('Ctrl Pts',(-20.6464193968664,26.2053669851818,-12.573543628164));
#64349=CARTESIAN_POINT('Ctrl Pts',(-20.5708789761065,26.1177069550997,-12.5794159251327));
#64350=CARTESIAN_POINT('Ctrl Pts',(-20.4954364497325,26.0301605254548,-12.5852806120709));
#64351=CARTESIAN_POINT('Ctrl Pts',(-20.4237523923954,25.9391659183717,-12.5911452990091));
#64352=CARTESIAN_POINT('Ctrl Pts',(-20.3561560239427,25.8450807385911,-12.5970099859473));
#64353=CARTESIAN_POINT('Ctrl Pts',(-20.2886291741234,25.7510923195281,-12.6028686414221));
#64354=CARTESIAN_POINT('Ctrl Pts',(-20.2251818911019,25.6540199835902,-12.6087272968969));
#64355=CARTESIAN_POINT('Ctrl Pts',(-20.1661037843444,25.5542550905276,-12.6145859523717));
#64356=CARTESIAN_POINT('Ctrl Pts',(-20.1047180347016,25.4505932928701,-12.6206734520897));
#64357=CARTESIAN_POINT('Ctrl Pts',(-20.048050044221,25.3440246470571,-12.6267609518076));
#64358=CARTESIAN_POINT('Ctrl Pts',(-19.9963759310729,25.2350225775926,-12.6328484515255));
#64359=CARTESIAN_POINT('Ctrl Pts',(-19.9467019744684,25.1302396652499,-12.6387003216089));
#64360=CARTESIAN_POINT('Ctrl Pts',(-19.9016426799514,25.0232086165073,-12.6445521916922));
#64361=CARTESIAN_POINT('Ctrl Pts',(-19.8613965411944,24.9143751366508,-12.6504040617756));
#64362=CARTESIAN_POINT('Ctrl Pts',(-19.8211565302779,24.8055582276812,-12.6562550408586));
#64363=CARTESIAN_POINT('Ctrl Pts',(-19.785728361326,24.6949398208807,-12.6621060199416));
#64364=CARTESIAN_POINT('Ctrl Pts',(-19.7552619033032,24.58298440901,-12.6679569990245));
#64365=CARTESIAN_POINT('Ctrl Pts',(-19.7247927060526,24.4710189312705,-12.6738085041668));
#64366=CARTESIAN_POINT('Ctrl Pts',(-19.6992862151009,24.3577166083961,-12.6796600093091));
#64367=CARTESIAN_POINT('Ctrl Pts',(-19.6788418763863,24.2435551625623,-12.6855115144514));
#64368=CARTESIAN_POINT('Ctrl Pts',(-19.6583907485519,24.1293558061975,-12.6913649627512));
#64369=CARTESIAN_POINT('Ctrl Pts',(-19.64300518841,24.0142971662741,-12.6972184110509));
#64370=CARTESIAN_POINT('Ctrl Pts',(-19.6327330717947,23.8988644668155,-12.7030718593507));
#64371=CARTESIAN_POINT('Ctrl Pts',(-19.6224492735524,23.7833004953119,-12.7089319642922));
#64372=CARTESIAN_POINT('Ctrl Pts',(-19.6172905622549,23.6673620272137,-12.7147920692338));
#64373=CARTESIAN_POINT('Ctrl Pts',(-19.6172527413712,23.5515367900416,-12.7206521741753));
#64374=CARTESIAN_POINT('Ctrl Pts',(-19.6172148950175,23.4356335518215,-12.7265162255308));
#64375=CARTESIAN_POINT('Ctrl Pts',(-19.6223047878136,23.3198441083393,-12.7323802768862));
#64376=CARTESIAN_POINT('Ctrl Pts',(-19.6324662760574,23.2046518153413,-12.7382443282417));
#64377=CARTESIAN_POINT('Ctrl Pts',(-19.6426427403065,23.0892897518981,-12.7441170220382));
#64378=CARTESIAN_POINT('Ctrl Pts',(-19.6579056634082,22.9745270036465,-12.7499897158348));
#64379=CARTESIAN_POINT('Ctrl Pts',(-19.6781476765945,22.8608375687633,-12.7558624096314));
#64380=CARTESIAN_POINT('Ctrl Pts',(-19.6836896011975,22.8297113032836,-12.7574702549547));
#64381=CARTESIAN_POINT('Ctrl Pts',(-19.6896044558134,22.7986654046952,-12.7590781002781));
#64382=CARTESIAN_POINT('Ctrl Pts',(-19.6958893896751,22.7677093894686,-12.7606859456015));
#64383=CARTESIAN_POINT('Ctrl Pts',(-19.7188437109196,22.6546494379067,-12.7665582425702));
#64384=CARTESIAN_POINT('Ctrl Pts',(-19.74681528221,22.5424109145349,-12.7724305395389));
#64385=CARTESIAN_POINT('Ctrl Pts',(-19.7797323364932,22.4314735286818,-12.7783028365076));
#64386=CARTESIAN_POINT('Ctrl Pts',(-19.8126067328883,22.3206799088703,-12.7841675234458));
#64387=CARTESIAN_POINT('Ctrl Pts',(-19.8504137506637,22.2111844660361,-12.790032210384));
#64388=CARTESIAN_POINT('Ctrl Pts',(-19.8930304882355,22.1034574788828,-12.7958968973222));
#64389=CARTESIAN_POINT('Ctrl Pts',(-19.9356033971604,21.9958412821921,-12.801755552797));
#64390=CARTESIAN_POINT('Ctrl Pts',(-19.9829760358943,21.8899903056891,-12.8076142082718));
#64391=CARTESIAN_POINT('Ctrl Pts',(-20.0349756931068,21.7863597492125,-12.8134728637467));
#64392=CARTESIAN_POINT('Ctrl Pts',(-20.0890065027307,21.6786812919234,-12.8195603634646));
#64393=CARTESIAN_POINT('Ctrl Pts',(-20.1480330413069,21.573400689915,-12.8256478631825));
#64394=CARTESIAN_POINT('Ctrl Pts',(-20.2118062624334,21.4710061520512,-12.8317353629004));
#64395=CARTESIAN_POINT('Ctrl Pts',(-20.2731110052878,21.3725750127336,-12.8375872329838));
#64396=CARTESIAN_POINT('Ctrl Pts',(-20.3388015635028,21.2768110530268,-12.8434391030672));
#64397=CARTESIAN_POINT('Ctrl Pts',(-20.4086102519881,21.1841221915897,-12.8492909731506));
#64398=CARTESIAN_POINT('Ctrl Pts',(-20.4784083114659,21.0914474428744,-12.8551419522336));
#64399=CARTESIAN_POINT('Ctrl Pts',(-20.552323005865,21.0018471915897,-12.8609929313165));
#64400=CARTESIAN_POINT('Ctrl Pts',(-20.6300445601613,20.9156986030384,-12.8668439103995));
#64401=CARTESIAN_POINT('Ctrl Pts',(-20.7077731023733,20.8295422688999,-12.8726954155418));
#64402=CARTESIAN_POINT('Ctrl Pts',(-20.7893089079657,20.746838521368,-12.8785469206841));
#64403=CARTESIAN_POINT('Ctrl Pts',(-20.8743038160025,20.6679292550669,-12.8843984258264));
#64404=CARTESIAN_POINT('Ctrl Pts',(-20.959326948998,20.5889937847161,-12.8902518741262));
#64405=CARTESIAN_POINT('Ctrl Pts',(-21.0478111657511,20.5138555822654,-12.896105322426));
#64406=CARTESIAN_POINT('Ctrl Pts',(-21.1393741180676,20.442817210612,-12.9019587707257));
#64407=CARTESIAN_POINT('Ctrl Pts',(-21.2310411973434,20.3716980529044,-12.9078188756673));
#64408=CARTESIAN_POINT('Ctrl Pts',(-21.3257936736492,20.3046882855481,-12.9136789806088));
#64409=CARTESIAN_POINT('Ctrl Pts',(-21.4232189452357,20.2420480153323,-12.9195390855504));
#64410=CARTESIAN_POINT('Ctrl Pts',(-21.5207098266449,20.179365560815,-12.9254031369058));
#64411=CARTESIAN_POINT('Ctrl Pts',(-21.6208767310226,20.1210586701587,-12.9312671882613));
#64412=CARTESIAN_POINT('Ctrl Pts',(-21.7232826550185,20.0673413829969,-12.9371312396167));
#64413=CARTESIAN_POINT('Ctrl Pts',(-21.8258395049041,20.0135449272769,-12.9430039334133));
#64414=CARTESIAN_POINT('Ctrl Pts',(-21.9306415875036,19.9643517499993,-12.9488766272098));
#64415=CARTESIAN_POINT('Ctrl Pts',(-22.0372320828273,19.9199277361269,-12.9547493210064));
#64416=CARTESIAN_POINT('Ctrl Pts',(-22.0664147774055,19.9077651842517,-12.9563571663297));
#64417=CARTESIAN_POINT('Ctrl Pts',(-22.0957314424514,19.8959598263653,-12.9579650116531));
#64418=CARTESIAN_POINT('Ctrl Pts',(-22.1251725306378,19.8845144081249,-12.9595728569764));
#64419=CARTESIAN_POINT('Ctrl Pts',(-22.2326995485701,19.8427125669505,-12.9654451539451));
#64420=CARTESIAN_POINT('Ctrl Pts',(-22.34224752153,19.8055758391798,-12.9713174509138));
#64421=CARTESIAN_POINT('Ctrl Pts',(-22.4533740688761,19.7733031492155,-12.9771897478825));
#64422=CARTESIAN_POINT('Ctrl Pts',(-22.5643566050423,19.7410722820945,-12.9830544348207));
#64423=CARTESIAN_POINT('Ctrl Pts',(-22.6769132541011,19.7136930317912,-12.9889191217589));
#64424=CARTESIAN_POINT('Ctrl Pts',(-22.7905819291723,19.691316204717,-12.9947838086971));
#64425=CARTESIAN_POINT('Ctrl Pts',(-22.9041337031271,19.6689623908086,-13.0006424641719));
#64426=CARTESIAN_POINT('Ctrl Pts',(-23.0187948251574,19.651600846464,-13.0065011196468));
#64427=CARTESIAN_POINT('Ctrl Pts',(-23.1340889702056,19.6393323215532,-13.0123597751216));
#64428=CARTESIAN_POINT('Ctrl Pts',(-23.2538866061091,19.6265845772535,-13.0184472748395));
#64429=CARTESIAN_POINT('Ctrl Pts',(-23.3743672894156,19.6193359659724,-13.0245347745574));
#64430=CARTESIAN_POINT('Ctrl Pts',(-23.4949856616789,19.6176408583811,-13.0306222742753));
#64431=CARTESIAN_POINT('Ctrl Pts',(-23.610935243094,19.6160113635373,-13.0364741443587));
#64432=CARTESIAN_POINT('Ctrl Pts',(-23.7270116006823,19.6195134523921,-13.0423260144421));
#64433=CARTESIAN_POINT('Ctrl Pts',(-23.8427268504927,19.6281424143156,-13.0481778845255));
#64434=CARTESIAN_POINT('Ctrl Pts',(-23.9584244816041,19.6367700624013,-13.0540288636084));
#64435=CARTESIAN_POINT('Ctrl Pts',(-24.073760702134,19.6505230007146,-13.0598798426914));
#64436=CARTESIAN_POINT('Ctrl Pts',(-24.1882507500522,19.6693444841656,-13.0657308217744));
#64437=CARTESIAN_POINT('Ctrl Pts',(-24.3027510917275,19.6881676598491,-13.0715823269167));
#64438=CARTESIAN_POINT('Ctrl Pts',(-24.4164047016209,19.7120602195202,-13.077433832059));
#64439=CARTESIAN_POINT('Ctrl Pts',(-24.528735742303,19.7409140580801,-13.0832853372013));
#64440=CARTESIAN_POINT('Ctrl Pts',(-24.6411040856784,19.7697774783717,-13.0891387855011));
#64441=CARTESIAN_POINT('Ctrl Pts',(-24.7521485863547,19.8036053507769,-13.0949922338008));
#64442=CARTESIAN_POINT('Ctrl Pts',(-24.8614080176822,19.8422395474176,-13.1008456821006));
#64443=CARTESIAN_POINT('Ctrl Pts',(-24.9707917007082,19.8809176795292,-13.1067057870421));
#64444=CARTESIAN_POINT('Ctrl Pts',(-25.0783858725773,19.924412907624,-13.1125658919837));
#64445=CARTESIAN_POINT('Ctrl Pts',(-25.1837486723467,19.9725187016736,-13.1184259969252));
#64446=CARTESIAN_POINT('Ctrl Pts',(-25.2891824273672,20.0206568919648,-13.1242900482807));
#64447=CARTESIAN_POINT('Ctrl Pts',(-25.3923814509564,20.0734116430386,-13.1301540996361));
#64448=CARTESIAN_POINT('Ctrl Pts',(-25.4929294491425,20.1305309941398,-13.1360181509915));
#64449=CARTESIAN_POINT('Ctrl Pts',(-25.5936256350067,20.1877345277624,-13.1418908447881));
#64450=CARTESIAN_POINT('Ctrl Pts',(-25.6916626489464,20.2493152804833,-13.1477635385847));
#64451=CARTESIAN_POINT('Ctrl Pts',(-25.7866539985887,20.3149785898352,-13.1536362323813));
#64452=CARTESIAN_POINT('Ctrl Pts',(-25.8126610411095,20.3329561055227,-13.1552440777046));
#64453=CARTESIAN_POINT('Ctrl Pts',(-25.8384399870517,20.3512394113058,-13.1568519230279));
#64454=CARTESIAN_POINT('Ctrl Pts',(-25.8639833657127,20.3698219590025,-13.1584597683513));
#64455=CARTESIAN_POINT('Ctrl Pts',(-25.9564731617271,20.4371073431602,-13.1642816013966));
#64456=CARTESIAN_POINT('Ctrl Pts',(-26.0461934153803,20.5085530008612,-13.1701034344419));
#64457=CARTESIAN_POINT('Ctrl Pts',(-26.1327414871855,20.5839012721895,-13.1759252674872));
#64458=CARTESIAN_POINT('Ctrl Pts',(-26.2191770473706,20.6591515915252,-13.1817395322084));
#64459=CARTESIAN_POINT('Ctrl Pts',(-26.3024483088353,20.7382941652882,-13.1875537969295));
#64460=CARTESIAN_POINT('Ctrl Pts',(-26.3821821172197,20.8210284986355,-13.1933680616506));
#64461=CARTESIAN_POINT('Ctrl Pts',(-26.461834529825,20.9036783731357,-13.1991763909145));
#64462=CARTESIAN_POINT('Ctrl Pts',(-26.5379563791802,20.9899124152296,-13.2049847201784));
#64463=CARTESIAN_POINT('Ctrl Pts',(-26.6102086912381,21.0793908800291,-13.2107930494423));
#64464=CARTESIAN_POINT('Ctrl Pts',(-26.6824087585795,21.1688046441028,-13.2165971787781));
#64465=CARTESIAN_POINT('Ctrl Pts',(-26.7507445891201,21.2614578389486,-13.2224013081139));
#64466=CARTESIAN_POINT('Ctrl Pts',(-26.8149156222302,21.3569755529949,-13.2282054374497));
#64467=CARTESIAN_POINT('Ctrl Pts',(-26.8790624624768,21.4524572562917,-13.234007378594));
#64468=CARTESIAN_POINT('Ctrl Pts',(-26.9390473910909,21.550800983448,-13.2398093197383));
#64469=CARTESIAN_POINT('Ctrl Pts',(-26.9946119623445,21.6516011386021,-13.2456112608827));
#64470=CARTESIAN_POINT('Ctrl Pts',(-27.0501696158159,21.7523887441495,-13.251412479686));
#64471=CARTESIAN_POINT('Ctrl Pts',(-27.1013078028738,21.8556318007637,-13.2572136984894));
#64472=CARTESIAN_POINT('Ctrl Pts',(-27.1478134295246,21.9608990196015,-13.2630149172928));
#64473=CARTESIAN_POINT('Ctrl Pts',(-27.1943250094988,22.0661797140085,-13.2688168787274));
#64474=CARTESIAN_POINT('Ctrl Pts',(-27.2362026809513,22.1734847000118,-13.274618840162));
#64475=CARTESIAN_POINT('Ctrl Pts',(-27.2732813313051,22.2823623324783,-13.2804208015967));
#64476=CARTESIAN_POINT('Ctrl Pts',(-27.31039617053,22.391346229832,-13.2862284257626));
#64477=CARTESIAN_POINT('Ctrl Pts',(-27.3427024994715,22.5019054393114,-13.2920360499285));
#64478=CARTESIAN_POINT('Ctrl Pts',(-27.3700849821292,22.6135727301591,-13.2978436740944));
#64479=CARTESIAN_POINT('Ctrl Pts',(-27.39748145559,22.7252970762822,-13.3036542656073));
#64480=CARTESIAN_POINT('Ctrl Pts',(-27.4199489912256,22.8381302181769,-13.3094648571202));
#64481=CARTESIAN_POINT('Ctrl Pts',(-27.437423677328,22.9515961322864,-13.3152754486331));
#64482=CARTESIAN_POINT('Ctrl Pts',(-27.4549253614099,23.0652373485672,-13.3210950173733));
#64483=CARTESIAN_POINT('Ctrl Pts',(-27.4674187440957,23.1795128710186,-13.3269145861136));
#64484=CARTESIAN_POINT('Ctrl Pts',(-27.4748919119119,23.2939426894247,-13.3327341548538));
#64485=CARTESIAN_POINT('Ctrl Pts',(-27.4805003377686,23.379819411065,-13.3371015958909));
#64486=CARTESIAN_POINT('Ctrl Pts',(-27.4832823996245,23.4657829595106,-13.341469036928));
#64487=CARTESIAN_POINT('Ctrl Pts',(-27.4832522897918,23.5516319533889,-13.3458364779651));
#64488=CARTESIAN_POINT('',(-27.4832508627744,23.5466293120366,-14.5958364779651));
#64489=CARTESIAN_POINT('Ctrl Pts',(-27.4891703390607,23.5516340290274,-13.3458364779651));
#64490=CARTESIAN_POINT('Ctrl Pts',(-27.4895124260083,23.6271647418024,-13.3496732118855));
#64491=CARTESIAN_POINT('Ctrl Pts',(-27.4875288934805,23.702677131584,-13.3535099458058));
#64492=CARTESIAN_POINT('Ctrl Pts',(-27.4077260247039,25.0804599026187,-13.4236423168511));
#64493=CARTESIAN_POINT('Ctrl Pts',(-25.8343164901973,27.6028816370497,-13.5562335911011));
#64494=CARTESIAN_POINT('Ctrl Pts',(-21.3753410672612,27.6624916971593,-13.7551205024758));
#64495=CARTESIAN_POINT('Ctrl Pts',(-18.914924878056,23.9433026245908,-13.9540074138508));
#64496=CARTESIAN_POINT('Ctrl Pts',(-20.7139817915703,19.8629338418023,-14.1528943252257));
#64497=CARTESIAN_POINT('Ctrl Pts',(-25.1193310391543,19.1708983019559,-14.3517812366005));
#64498=CARTESIAN_POINT('Ctrl Pts',(-27.3193395389436,21.6446333378869,-14.4994286208471));
#64499=CARTESIAN_POINT('Ctrl Pts',(-27.4862333707757,23.2491136935675,-14.5807803679686));
#64500=CARTESIAN_POINT('Ctrl Pts',(-27.4834731626111,23.546629107246,-14.5958364779651));
#64501=CARTESIAN_POINT('',(-27.4832525228614,23.5505161199331,-15.8458364779913));
#64502=CARTESIAN_POINT('Ctrl Pts',(-27.4832508627744,23.5466293120366,-14.5958364779651));
#64503=CARTESIAN_POINT('Ctrl Pts',(-27.483356110635,23.6608756728268,-14.6016184276768));
#64504=CARTESIAN_POINT('Ctrl Pts',(-27.4784791878884,23.7752670552024,-14.6074003773886));
#64505=CARTESIAN_POINT('Ctrl Pts',(-27.4686089715413,23.8893274648705,-14.6131823271003));
#64506=CARTESIAN_POINT('Ctrl Pts',(-27.4587462040328,24.0033017956168,-14.6189599132998));
#64507=CARTESIAN_POINT('Ctrl Pts',(-27.4438976715182,24.116945228161,-14.6247374994993));
#64508=CARTESIAN_POINT('Ctrl Pts',(-27.4241043175623,24.2297827673178,-14.6305150856988));
#64509=CARTESIAN_POINT('Ctrl Pts',(-27.404318832571,24.342575447245,-14.6362903749848));
#64510=CARTESIAN_POINT('Ctrl Pts',(-27.3795925050751,24.4545624520454,-14.6420656642708));
#64511=CARTESIAN_POINT('Ctrl Pts',(-27.3500179328278,24.5652756330804,-14.6478409535568));
#64512=CARTESIAN_POINT('Ctrl Pts',(-27.3204475107449,24.6759732778671,-14.6536154324033));
#64513=CARTESIAN_POINT('Ctrl Pts',(-27.2860303059289,24.7853970433522,-14.6593899112499));
#64514=CARTESIAN_POINT('Ctrl Pts',(-27.24690945734,24.8930915295174,-14.6651643900964));
#64515=CARTESIAN_POINT('Ctrl Pts',(-27.2077840352198,25.0007986060054,-14.6709395440245));
#64516=CARTESIAN_POINT('Ctrl Pts',(-27.1639540226431,25.10677560197,-14.6767146979525));
#64517=CARTESIAN_POINT('Ctrl Pts',(-27.1156112958667,25.2105855954915,-14.6824898518805));
#64518=CARTESIAN_POINT('Ctrl Pts',(-27.0672201349842,25.3144995952322,-14.6882707918789));
#64519=CARTESIAN_POINT('Ctrl Pts',(-27.014307410922,25.4162418706406,-14.6940517318773));
#64520=CARTESIAN_POINT('Ctrl Pts',(-26.9571117307415,25.515398683477,-14.6998326718757));
#64521=CARTESIAN_POINT('Ctrl Pts',(-26.8998870056989,25.6146058496958,-14.7056165475259));
#64522=CARTESIAN_POINT('Ctrl Pts',(-26.8383752234161,25.7112245812216,-14.7114004231762));
#64523=CARTESIAN_POINT('Ctrl Pts',(-26.7728581599204,25.8048704516365,-14.7171842988264));
#64524=CARTESIAN_POINT('Ctrl Pts',(-26.7072344285476,25.8986687862441,-14.7229775911645));
#64525=CARTESIAN_POINT('Ctrl Pts',(-26.6375926502515,25.9894842550802,-14.7287708835027));
#64526=CARTESIAN_POINT('Ctrl Pts',(-26.5642548892321,26.0769655721394,-14.7345641758408));
#64527=CARTESIAN_POINT('Ctrl Pts',(-26.5009979495314,26.1524219307907,-14.7395611370107));
#64528=CARTESIAN_POINT('Ctrl Pts',(-26.4349920199945,26.2253982103105,-14.7445580981805));
#64529=CARTESIAN_POINT('Ctrl Pts',(-26.3664643341204,26.2956924024391,-14.7495550593504));
#64530=CARTESIAN_POINT('Ctrl Pts',(-26.2859324051439,26.378300282973,-14.7554273563191));
#64531=CARTESIAN_POINT('Ctrl Pts',(-26.2016277789585,26.4575001878523,-14.7612996532878));
#64532=CARTESIAN_POINT('Ctrl Pts',(-26.1138706068156,26.5329277344125,-14.7671719502566));
#64533=CARTESIAN_POINT('Ctrl Pts',(-26.0262271609984,26.6082575328626,-14.7730366371948));
#64534=CARTESIAN_POINT('Ctrl Pts',(-25.935140377456,26.6798244278518,-14.778901324133));
#64535=CARTESIAN_POINT('Ctrl Pts',(-25.8409682843132,26.7472996600148,-14.7847660110712));
#64536=CARTESIAN_POINT('Ctrl Pts',(-25.7468930412728,26.8147054981256,-14.790624666546));
#64537=CARTESIAN_POINT('Ctrl Pts',(-25.6497391339966,26.8780278040554,-14.7964833220208));
#64538=CARTESIAN_POINT('Ctrl Pts',(-25.5498982946156,26.9369774722275,-14.8023419774956));
#64539=CARTESIAN_POINT('Ctrl Pts',(-25.4461575841099,26.9982297663606,-14.8084294772135));
#64540=CARTESIAN_POINT('Ctrl Pts',(-25.3395160992451,27.0547605643504,-14.8145169769314));
#64541=CARTESIAN_POINT('Ctrl Pts',(-25.230447619476,27.106294357516,-14.8206044766493));
#64542=CARTESIAN_POINT('Ctrl Pts',(-25.1256008673807,27.1558334255216,-14.8264563467327));
#64543=CARTESIAN_POINT('Ctrl Pts',(-25.0185119194588,27.2007549420843,-14.8323082168161));
#64544=CARTESIAN_POINT('Ctrl Pts',(-24.9096267360728,27.2408609872839,-14.8381600868995));
#64545=CARTESIAN_POINT('Ctrl Pts',(-24.8007581314459,27.2809609259735,-14.8440110659825));
#64546=CARTESIAN_POINT('Ctrl Pts',(-24.6900942229466,27.3162467082954,-14.8498620450655));
#64547=CARTESIAN_POINT('Ctrl Pts',(-24.5780996958206,27.3465690631754,-14.8557130241484));
#64548=CARTESIAN_POINT('Ctrl Pts',(-24.4660950993092,27.3768941443267,-14.8615645292907));
#64549=CARTESIAN_POINT('Ctrl Pts',(-24.3527600453873,27.402254802873,-14.867416034433));
#64550=CARTESIAN_POINT('Ctrl Pts',(-24.2385723838139,27.4225522077495,-14.8732675395753));
#64551=CARTESIAN_POINT('Ctrl Pts',(-24.1243468030033,27.4428563529524,-14.8791209878751));
#64552=CARTESIAN_POINT('Ctrl Pts',(-24.0092684583377,27.4580938288264,-14.8849744361749));
#64553=CARTESIAN_POINT('Ctrl Pts',(-23.8938226350511,27.4682173840224,-14.8908278844746));
#64554=CARTESIAN_POINT('Ctrl Pts',(-23.7782455247951,27.478352451899,-14.8966879894162));
#64555=CARTESIAN_POINT('Ctrl Pts',(-23.6623005138431,27.4833619551266,-14.9025480943577));
#64556=CARTESIAN_POINT('Ctrl Pts',(-23.5464753239116,27.4832507179004,-14.9084081992993));
#64557=CARTESIAN_POINT('Ctrl Pts',(-23.4305721329638,27.4831394057629,-14.9142722506547));
#64558=CARTESIAN_POINT('Ctrl Pts',(-23.3147893356614,27.4779005051668,-14.9201363020102));
#64559=CARTESIAN_POINT('Ctrl Pts',(-23.199610215098,27.4675907818089,-14.9260003533656));
#64560=CARTESIAN_POINT('Ctrl Pts',(-23.0842613435028,27.4572658639769,-14.9318730471622));
#64561=CARTESIAN_POINT('Ctrl Pts',(-22.9695183324802,27.4418552627762,-14.9377457409587));
#64562=CARTESIAN_POINT('Ctrl Pts',(-22.8558550416392,27.421466956885,-14.9436184347553));
#64563=CARTESIAN_POINT('Ctrl Pts',(-22.824735933962,27.4158849797868,-14.9452262800786));
#64564=CARTESIAN_POINT('Ctrl Pts',(-22.7936976730415,27.4099301764103,-14.9468341254019));
#64565=CARTESIAN_POINT('Ctrl Pts',(-22.7627497716716,27.4036054097676,-14.9484419707252));
#64566=CARTESIAN_POINT('Ctrl Pts',(-22.6497194541605,27.3805056081604,-14.9543142676939));
#64567=CARTESIAN_POINT('Ctrl Pts',(-22.5375170209701,27.3523896177763,-14.9601865646626));
#64568=CARTESIAN_POINT('Ctrl Pts',(-22.4266220886732,27.3193298229575,-14.9660588616314));
#64569=CARTESIAN_POINT('Ctrl Pts',(-22.3158708674017,27.2863128710072,-14.9719235485695));
#64570=CARTESIAN_POINT('Ctrl Pts',(-22.2064241699327,27.2483649724142,-14.9777882355077));
#64571=CARTESIAN_POINT('Ctrl Pts',(-22.0987521164159,27.2056096338727,-14.9836529224459));
#64572=CARTESIAN_POINT('Ctrl Pts',(-21.9911907968657,27.1628982665204,-14.9895115779208));
#64573=CARTESIAN_POINT('Ctrl Pts',(-21.8854008729206,27.1153894450349,-14.9953702333956));
#64574=CARTESIAN_POINT('Ctrl Pts',(-21.7818373217765,27.0632564664104,-15.0012288888704));
#64575=CARTESIAN_POINT('Ctrl Pts',(-21.6742284871069,27.0090871277226,-15.0073163885883));
#64576=CARTESIAN_POINT('Ctrl Pts',(-21.5690239348475,26.9499251500729,-15.0134038883062));
#64577=CARTESIAN_POINT('Ctrl Pts',(-21.4667115529542,26.8860202079437,-15.0194913880241));
#64578=CARTESIAN_POINT('Ctrl Pts',(-21.3683593895854,26.8245888426284,-15.0253432581075));
#64579=CARTESIAN_POINT('Ctrl Pts',(-21.2726800478223,26.7587750980372,-15.0311951281909));
#64580=CARTESIAN_POINT('Ctrl Pts',(-21.1800811014959,26.6888471839983,-15.0370469982743));
#64581=CARTESIAN_POINT('Ctrl Pts',(-21.0874962542013,26.6189299171203,-15.0428979773573));
#64582=CARTESIAN_POINT('Ctrl Pts',(-20.9979911995804,26.5448999753691,-15.0487489564403));
#64583=CARTESIAN_POINT('Ctrl Pts',(-20.9119427039676,26.4670676188948,-15.0545999355232));
#64584=CARTESIAN_POINT('Ctrl Pts',(-20.8258864717669,26.3892282645427,-15.0604514406655));
#64585=CARTESIAN_POINT('Ctrl Pts',(-20.7432877229659,26.3075860931737,-15.0663029458078));
#64586=CARTESIAN_POINT('Ctrl Pts',(-20.6644879038494,26.2224897054271,-15.0721544509501));
#64587=CARTESIAN_POINT('Ctrl Pts',(-20.5856619170283,26.1373650590225,-15.0780078992499));
#64588=CARTESIAN_POINT('Ctrl Pts',(-20.5106376491086,26.0487842185151,-15.0838613475496));
#64589=CARTESIAN_POINT('Ctrl Pts',(-20.4397171706846,25.9571299211573,-15.0897147958494));
#64590=CARTESIAN_POINT('Ctrl Pts',(-20.3687160402766,25.8653713929611,-15.0955749007909));
#64591=CARTESIAN_POINT('Ctrl Pts',(-20.3018282674831,25.7705327587558,-15.1014350057325));
#64592=CARTESIAN_POINT('Ctrl Pts',(-20.2393134278915,25.6730269546865,-15.107295110674));
#64593=CARTESIAN_POINT('Ctrl Pts',(-20.176756488468,25.5754554865605,-15.1131591620295));
#64594=CARTESIAN_POINT('Ctrl Pts',(-20.1185785531158,25.4752136286926,-15.1190232133849));
#64595=CARTESIAN_POINT('Ctrl Pts',(-20.0649930989017,25.3727386595237,-15.1248872647404));
#64596=CARTESIAN_POINT('Ctrl Pts',(-20.0113286704249,25.2701126627063,-15.130759958537));
#64597=CARTESIAN_POINT('Ctrl Pts',(-19.9622704060186,25.1652473590959,-15.1366326523335));
#64598=CARTESIAN_POINT('Ctrl Pts',(-19.9179836026164,25.0585997817849,-15.1425053461301));
#64599=CARTESIAN_POINT('Ctrl Pts',(-19.9058586166724,25.0294014591127,-15.1441131914535));
#64600=CARTESIAN_POINT('Ctrl Pts',(-19.894090996831,25.0000696257647,-15.1457210367768));
#64601=CARTESIAN_POINT('Ctrl Pts',(-19.8826834764605,24.9706138325934,-15.1473288821002));
#64602=CARTESIAN_POINT('Ctrl Pts',(-19.8410200488168,24.8630331079819,-15.1532011790689));
#64603=CARTESIAN_POINT('Ctrl Pts',(-19.8040243315258,24.7534374336547,-15.1590734760376));
#64604=CARTESIAN_POINT('Ctrl Pts',(-19.771894679516,24.642269445887,-15.1649457730063));
#64605=CARTESIAN_POINT('Ctrl Pts',(-19.7398066649834,24.5312455230025,-15.1708104599445));
#64606=CARTESIAN_POINT('Ctrl Pts',(-19.7125722890121,24.4186537321826,-15.1766751468827));
#64607=CARTESIAN_POINT('Ctrl Pts',(-19.6903417632184,24.3049563540011,-15.1825398338209));
#64608=CARTESIAN_POINT('Ctrl Pts',(-19.6681341001289,24.1913759064559,-15.1883984892958));
#64609=CARTESIAN_POINT('Ctrl Pts',(-19.6509201301139,24.0766925364166,-15.1942571447706));
#64610=CARTESIAN_POINT('Ctrl Pts',(-19.6387999899668,23.9613826982038,-15.2001158002454));
#64611=CARTESIAN_POINT('Ctrl Pts',(-19.6262064264702,23.8415687561467,-15.2062032999633));
#64612=CARTESIAN_POINT('Ctrl Pts',(-19.6191128704675,23.721078844209,-15.2122907996812));
#64613=CARTESIAN_POINT('Ctrl Pts',(-19.6175729907506,23.6004583903563,-15.2183782993991));
#64614=CARTESIAN_POINT('Ctrl Pts',(-19.6160927153561,23.484506807924,-15.2242301694825));
#64615=CARTESIAN_POINT('Ctrl Pts',(-19.6197441825618,23.368435053373,-15.2300820395659));
#64616=CARTESIAN_POINT('Ctrl Pts',(-19.6285220538732,23.252731004188,-15.2359339096493));
#64617=CARTESIAN_POINT('Ctrl Pts',(-19.6372985886738,23.1370445719968,-15.2417848887322));
#64618=CARTESIAN_POINT('Ctrl Pts',(-19.6511999443506,23.0217261459378,-15.2476358678152));
#64619=CARTESIAN_POINT('Ctrl Pts',(-19.6701687520095,22.9072604146136,-15.2534868468982));
#64620=CARTESIAN_POINT('Ctrl Pts',(-19.6891392651468,22.7927843917183,-15.2593383520405));
#64621=CARTESIAN_POINT('Ctrl Pts',(-19.7131780683958,22.6791616238069,-15.2651898571828));
#64622=CARTESIAN_POINT('Ctrl Pts',(-19.7421764443815,22.5668678087919,-15.2710413623251));
#64623=CARTESIAN_POINT('Ctrl Pts',(-19.7711844500967,22.4545367034453,-15.2768948106249));
#64624=CARTESIAN_POINT('Ctrl Pts',(-19.805155200132,22.3435358285655,-15.2827482589247));
#64625=CARTESIAN_POINT('Ctrl Pts',(-19.8439299731772,22.2343262069221,-15.2886017072245));
#64626=CARTESIAN_POINT('Ctrl Pts',(-19.882748841559,22.1249923902251,-15.294461812166));
#64627=CARTESIAN_POINT('Ctrl Pts',(-19.9263824989732,22.0174542824313,-15.3003219171076));
#64628=CARTESIAN_POINT('Ctrl Pts',(-19.974623846922,21.9121534783296,-15.3061820220491));
#64629=CARTESIAN_POINT('Ctrl Pts',(-20.0228976823991,21.8067817607271,-15.3120460734045));
#64630=CARTESIAN_POINT('Ctrl Pts',(-20.0757851989103,21.7036507138604,-15.31791012476));
#64631=CARTESIAN_POINT('Ctrl Pts',(-20.1330339001709,21.6031763071025,-15.3237741761154));
#64632=CARTESIAN_POINT('Ctrl Pts',(-20.1903669745893,21.5025538211255,-15.329646869912));
#64633=CARTESIAN_POINT('Ctrl Pts',(-20.2520738423337,21.4045961380118,-15.3355195637085));
#64634=CARTESIAN_POINT('Ctrl Pts',(-20.3178593437951,21.3096893706065,-15.3413922575051));
#64635=CARTESIAN_POINT('Ctrl Pts',(-20.3358703136382,21.2837054852872,-15.3430001028284));
#64636=CARTESIAN_POINT('Ctrl Pts',(-20.3541867797811,21.2579500898859,-15.3446079481517));
#64637=CARTESIAN_POINT('Ctrl Pts',(-20.3728021844329,21.2324306466718,-15.3462157934751));
#64638=CARTESIAN_POINT('Ctrl Pts',(-20.4407908041852,21.1392265636325,-15.3520880904438));
#64639=CARTESIAN_POINT('Ctrl Pts',(-20.5129977302646,21.0488603378879,-15.3579603874125));
#64640=CARTESIAN_POINT('Ctrl Pts',(-20.5891577845937,20.9617381124386,-15.3638326843812));
#64641=CARTESIAN_POINT('Ctrl Pts',(-20.6652191415409,20.8747287904746,-15.3696973713194));
#64642=CARTESIAN_POINT('Ctrl Pts',(-20.7452231694908,20.790955416982,-15.3755620582576));
#64643=CARTESIAN_POINT('Ctrl Pts',(-20.8288621397872,20.7107942497615,-15.3814267451958));
#64644=CARTESIAN_POINT('Ctrl Pts',(-20.9124150926382,20.6307155232836,-15.3872854006706));
#64645=CARTESIAN_POINT('Ctrl Pts',(-20.9995952554929,20.5542418982105,-15.3931440561454));
#64646=CARTESIAN_POINT('Ctrl Pts',(-21.0900559075193,20.4817151650652,-15.3990027116203));
#64647=CARTESIAN_POINT('Ctrl Pts',(-21.1840500322909,20.4063554738422,-15.4050902113382));
#64648=CARTESIAN_POINT('Ctrl Pts',(-21.281585849077,20.3352576408274,-15.4111777110561));
#64649=CARTESIAN_POINT('Ctrl Pts',(-21.382233490436,20.2687616454137,-15.417265210774));
#64650=CARTESIAN_POINT('Ctrl Pts',(-21.4789853505966,20.2048395190466,-15.4231170808574));
#64651=CARTESIAN_POINT('Ctrl Pts',(-21.5786122380026,20.1451698557061,-15.4289689509408));
#64652=CARTESIAN_POINT('Ctrl Pts',(-21.6807008074574,20.0900118824903,-15.4348208210242));
#64653=CARTESIAN_POINT('Ctrl Pts',(-21.7827738329992,20.0348623075774,-15.4406718001072));
#64654=CARTESIAN_POINT('Ctrl Pts',(-21.8873074317477,19.9842232533686,-15.4465227791902));
#64655=CARTESIAN_POINT('Ctrl Pts',(-21.9938628167299,19.9383084491878,-15.4523737582732));
#64656=CARTESIAN_POINT('Ctrl Pts',(-22.1004277820665,19.8923895168242,-15.4582252634155));
#64657=CARTESIAN_POINT('Ctrl Pts',(-22.2090145153344,19.8511958424596,-15.4640767685578));
#64658=CARTESIAN_POINT('Ctrl Pts',(-22.3191640375484,19.81489309523,-15.4699282737001));
#64659=CARTESIAN_POINT('Ctrl Pts',(-22.4293501380207,19.7785782926485,-15.4757817219998));
#64660=CARTESIAN_POINT('Ctrl Pts',(-22.5410996669729,19.7471577760894,-15.4816351702996));
#64661=CARTESIAN_POINT('Ctrl Pts',(-22.6539389626171,19.7207472130025,-15.4874886185994));
#64662=CARTESIAN_POINT('Ctrl Pts',(-22.7669065810432,19.6943066153703,-15.4933487235409));
#64663=CARTESIAN_POINT('Ctrl Pts',(-22.8809660370256,19.6728874373227,-15.4992088284825));
#64664=CARTESIAN_POINT('Ctrl Pts',(-22.9956338639416,19.6565541441223,-15.505068933424));
#64665=CARTESIAN_POINT('Ctrl Pts',(-23.1103789124619,19.6402098514712,-15.5109329847794));
#64666=CARTESIAN_POINT('Ctrl Pts',(-23.2257327372844,19.628958303605,-15.5167970361349));
#64667=CARTESIAN_POINT('Ctrl Pts',(-23.3412088914505,19.6228119202433,-15.5226610874903));
#64668=CARTESIAN_POINT('Ctrl Pts',(-23.4568552344169,19.6166564783395,-15.5285337812869));
#64669=CARTESIAN_POINT('Ctrl Pts',(-23.5726238547347,19.615621221062,-15.5344064750835));
#64670=CARTESIAN_POINT('Ctrl Pts',(-23.6880303629076,19.6196665360409,-15.5402791688801));
#64671=CARTESIAN_POINT('Ctrl Pts',(-23.7196267343299,19.6207740756122,-15.5418870142034));
#64672=CARTESIAN_POINT('Ctrl Pts',(-23.7511960070516,19.6222621428333,-15.5434948595267));
#64673=CARTESIAN_POINT('Ctrl Pts',(-23.7827283581763,19.6241292541975,-15.54510270485));
#64674=CARTESIAN_POINT('Ctrl Pts',(-23.8978932482561,19.6309484626407,-15.5509750018187));
#64675=CARTESIAN_POINT('Ctrl Pts',(-24.0129507747762,19.6428505851457,-15.5568472987874));
#64676=CARTESIAN_POINT('Ctrl Pts',(-24.1274159028231,19.6598320604563,-15.5627195957561));
#64677=CARTESIAN_POINT('Ctrl Pts',(-24.2417326931544,19.6767915291235,-15.5685842826942));
#64678=CARTESIAN_POINT('Ctrl Pts',(-24.3554582065618,19.6988172003868,-15.5744489696324));
#64679=CARTESIAN_POINT('Ctrl Pts',(-24.4681095506604,19.7258535602564,-15.5803136565706));
#64680=CARTESIAN_POINT('Ctrl Pts',(-24.5806450399034,19.7528621149224,-15.5861723120454));
#64681=CARTESIAN_POINT('Ctrl Pts',(-24.6921081576227,19.784871012363,-15.5920309675201));
#64682=CARTESIAN_POINT('Ctrl Pts',(-24.8020239324085,19.8217733027922,-15.5978896229949));
#64683=CARTESIAN_POINT('Ctrl Pts',(-24.9162331141709,19.860117029189,-15.6039771227128));
#64684=CARTESIAN_POINT('Ctrl Pts',(-25.0287711577931,19.9037441555355,-15.6100646224307));
#64685=CARTESIAN_POINT('Ctrl Pts',(-25.139119671332,19.9524768004153,-15.6161521221487));
#64686=CARTESIAN_POINT('Ctrl Pts',(-25.2451969107647,19.999323144542,-15.622003992232));
#64687=CARTESIAN_POINT('Ctrl Pts',(-25.3492505558114,20.0508869338687,-15.6278558623154));
#64688=CARTESIAN_POINT('Ctrl Pts',(-25.4508390837635,20.1069605373822,-15.6337077323988));
#64689=CARTESIAN_POINT('Ctrl Pts',(-25.5524121439386,20.1630256031797,-15.6395587114817));
#64690=CARTESIAN_POINT('Ctrl Pts',(-25.6515204714959,20.2235989181551,-15.6454096905647));
#64691=CARTESIAN_POINT('Ctrl Pts',(-25.7477470694091,20.2884268532262,-15.6512606696476));
#64692=CARTESIAN_POINT('Ctrl Pts',(-25.8439823190194,20.3532606169526,-15.6571121747899));
#64693=CARTESIAN_POINT('Ctrl Pts',(-25.9373349810695,20.4223495302275,-15.6629636799322));
#64694=CARTESIAN_POINT('Ctrl Pts',(-26.0274175777364,20.4953969975213,-15.6688151850745));
#64695=CARTESIAN_POINT('Ctrl Pts',(-26.1175300888725,20.5684687222888,-15.6746686333742));
#64696=CARTESIAN_POINT('Ctrl Pts',(-26.2043700544324,20.6455013547467,-15.680522081674));
#64697=CARTESIAN_POINT('Ctrl Pts',(-26.2875841271733,20.7261589184456,-15.6863755299737));
#64698=CARTESIAN_POINT('Ctrl Pts',(-26.3708928323846,20.8069082073089,-15.6922356349153));
#64699=CARTESIAN_POINT('Ctrl Pts',(-26.4505671175344,20.891290367586,-15.6980957398568));
#64700=CARTESIAN_POINT('Ctrl Pts',(-26.5262914127103,20.9789334969028,-15.7039558447983));
#64701=CARTESIAN_POINT('Ctrl Pts',(-26.6020667034598,21.0666356483821,-15.7098198961538));
#64702=CARTESIAN_POINT('Ctrl Pts',(-26.6738864519735,21.1576028180315,-15.7156839475092));
#64703=CARTESIAN_POINT('Ctrl Pts',(-26.74147726413,21.2514324632482,-15.7215479988647));
#64704=CARTESIAN_POINT('Ctrl Pts',(-26.8091676916509,21.3454003946313,-15.7274206926612));
#64705=CARTESIAN_POINT('Ctrl Pts',(-26.8726165180301,21.4422388768522,-15.7332933864577));
#64706=CARTESIAN_POINT('Ctrl Pts',(-26.9315952367616,21.5415189727353,-15.7391660802543));
#64707=CARTESIAN_POINT('Ctrl Pts',(-26.9477426233586,21.5687002022379,-15.7407739255778));
#64708=CARTESIAN_POINT('Ctrl Pts',(-26.9635552176627,21.5960643244755,-15.7423817709013));
#64709=CARTESIAN_POINT('Ctrl Pts',(-26.9790289580811,21.6236022733822,-15.7439896162248));
#64710=CARTESIAN_POINT('Ctrl Pts',(-27.0381448271853,21.728808237742,-15.7501322275853));
#64711=CARTESIAN_POINT('Ctrl Pts',(-27.0924942057525,21.8368783305784,-15.7562748389458));
#64712=CARTESIAN_POINT('Ctrl Pts',(-27.1418029470715,21.9473630739327,-15.7624174503064));
#64713=CARTESIAN_POINT('Ctrl Pts',(-27.1910255695739,22.0576548532181,-15.7685493334592));
#64714=CARTESIAN_POINT('Ctrl Pts',(-27.2352249427918,22.1703525581504,-15.7746812166119));
#64715=CARTESIAN_POINT('Ctrl Pts',(-27.2741721621672,22.2849811830192,-15.7808130997647));
#64716=CARTESIAN_POINT('Ctrl Pts',(-27.3130334201259,22.3993568080807,-15.7869314490793));
#64717=CARTESIAN_POINT('Ctrl Pts',(-27.3466655169619,22.5156545194472,-15.793049798394));
#64718=CARTESIAN_POINT('Ctrl Pts',(-27.3748874772214,22.6333792942988,-15.7991681477086));
#64719=CARTESIAN_POINT('Ctrl Pts',(-27.4030721722485,22.7509486213695,-15.8052784181475));
#64720=CARTESIAN_POINT('Ctrl Pts',(-27.4258608715318,22.8699409127405,-15.8113886885864));
#64721=CARTESIAN_POINT('Ctrl Pts',(-27.4431219424024,22.989844866532,-15.8174989590254));
#64722=CARTESIAN_POINT('Ctrl Pts',(-27.4603550692174,23.1095547070631,-15.8235993375093));
#64723=CARTESIAN_POINT('Ctrl Pts',(-27.4720783532156,23.2301729141833,-15.8296997159932));
#64724=CARTESIAN_POINT('Ctrl Pts',(-27.4782110546695,23.3511775664535,-15.8358000944771));
#64725=CARTESIAN_POINT('Ctrl Pts',(-27.481574241821,23.4175367875645,-15.8391455556397));
#64726=CARTESIAN_POINT('Ctrl Pts',(-27.4832569799326,23.4840120305005,-15.8424910168024));
#64727=CARTESIAN_POINT('Ctrl Pts',(-27.4832525228614,23.5505161194119,-15.8458364779651));
#64728=CARTESIAN_POINT('',(-27.4832509455688,23.5537847349664,-17.0958364779651));
#64729=CARTESIAN_POINT('Ctrl Pts',(-27.4832525228614,23.550516119933,-15.8458364779913));
#64730=CARTESIAN_POINT('Ctrl Pts',(-27.48324431477,23.6729890476372,-15.8519974288415));
#64731=CARTESIAN_POINT('Ctrl Pts',(-27.477511140326,23.7953393043865,-15.8581583796916));
#64732=CARTESIAN_POINT('Ctrl Pts',(-27.4661129484295,23.9170306616928,-15.8643193305417));
#64733=CARTESIAN_POINT('Ctrl Pts',(-27.4546966094255,24.0389157643033,-15.8704900902668));
#64734=CARTESIAN_POINT('Ctrl Pts',(-27.4375972878388,24.1601395321258,-15.8766608499917));
#64735=CARTESIAN_POINT('Ctrl Pts',(-27.4149262183359,24.2801746479363,-15.8828316097167));
#64736=CARTESIAN_POINT('Ctrl Pts',(-27.3921961074326,24.4005223666145,-15.8890184397156));
#64737=CARTESIAN_POINT('Ctrl Pts',(-27.3638653041277,24.5196749056777,-15.8952052697145));
#64738=CARTESIAN_POINT('Ctrl Pts',(-27.3300956338617,24.6371173452736,-15.9013920997134));
#64739=CARTESIAN_POINT('Ctrl Pts',(-27.2962769719856,24.754730165396,-15.9075879053037));
#64740=CARTESIAN_POINT('Ctrl Pts',(-27.2570038069768,24.870627609844,-15.913783710894));
#64741=CARTESIAN_POINT('Ctrl Pts',(-27.2124864225242,24.9843138723824,-15.9199795164842));
#64742=CARTESIAN_POINT('Ctrl Pts',(-27.167867799437,25.0982586730654,-15.9261894121857));
#64743=CARTESIAN_POINT('Ctrl Pts',(-27.117981258964,25.2099819266785,-15.9323993078872));
#64744=CARTESIAN_POINT('Ctrl Pts',(-27.0630839286443,25.3190104508572,-15.9386092035887));
#64745=CARTESIAN_POINT('Ctrl Pts',(-27.0505091229324,25.343984570739,-15.9400316449257));
#64746=CARTESIAN_POINT('Ctrl Pts',(-27.0376715887623,25.3688174196986,-15.9414540862627));
#64747=CARTESIAN_POINT('Ctrl Pts',(-27.0245747344379,25.3935035269528,-15.9428765275997));
#64748=CARTESIAN_POINT('Ctrl Pts',(-26.9705066924393,25.495415745776,-15.9487488245684));
#64749=CARTESIAN_POINT('Ctrl Pts',(-26.9118601866573,25.5951177131025,-15.9546211215371));
#64750=CARTESIAN_POINT('Ctrl Pts',(-26.8488400501931,25.6921697529713,-15.9604934185059));
#64751=CARTESIAN_POINT('Ctrl Pts',(-26.7859015828207,25.7890960211042,-15.9663581054441));
#64752=CARTESIAN_POINT('Ctrl Pts',(-26.7186009791917,25.8833788474608,-15.9722227923823));
#64753=CARTESIAN_POINT('Ctrl Pts',(-26.6471894347301,25.974602097787,-15.9780874793205));
#64754=CARTESIAN_POINT('Ctrl Pts',(-26.5758513325716,26.0657315307109,-15.9839461347954));
#64755=CARTESIAN_POINT('Ctrl Pts',(-26.5004109522646,26.1538073227681,-15.9898047902702));
#64756=CARTESIAN_POINT('Ctrl Pts',(-26.4211629797005,26.2384419222559,-15.995663445745));
#64757=CARTESIAN_POINT('Ctrl Pts',(-26.3388195115278,26.3263824237444,-16.0017509454629));
#64758=CARTESIAN_POINT('Ctrl Pts',(-26.2523651789415,26.410607038867,-16.0078384451808));
#64759=CARTESIAN_POINT('Ctrl Pts',(-26.1621772293995,26.4907182045966,-16.0139259448987));
#64760=CARTESIAN_POINT('Ctrl Pts',(-26.0754801964193,26.5677284971313,-16.0197778149821));
#64761=CARTESIAN_POINT('Ctrl Pts',(-25.9853335451773,26.6409375586416,-16.0256296850655));
#64762=CARTESIAN_POINT('Ctrl Pts',(-25.8921096324298,26.7100301061026,-16.031481555149));
#64763=CARTESIAN_POINT('Ctrl Pts',(-25.7988999138706,26.7791121335951,-16.0373325342319));
#64764=CARTESIAN_POINT('Ctrl Pts',(-25.7026141974369,26.8440786471947,-16.0431835133149));
#64765=CARTESIAN_POINT('Ctrl Pts',(-25.6036564831716,26.9046557889155,-16.0490344923979));
#64766=CARTESIAN_POINT('Ctrl Pts',(-25.5046898716556,26.9652383771043,-16.0548859975402));
#64767=CARTESIAN_POINT('Ctrl Pts',(-25.4030511373262,27.0214305930544,-16.0607375026825));
#64768=CARTESIAN_POINT('Ctrl Pts',(-25.2991710907017,27.0730032855738,-16.0665890078248));
#64769=CARTESIAN_POINT('Ctrl Pts',(-25.1952565477747,27.1245931042618,-16.0724424561246));
#64770=CARTESIAN_POINT('Ctrl Pts',(-25.0890995826438,27.1715601654458,-16.0782959044244));
#64771=CARTESIAN_POINT('Ctrl Pts',(-24.9811526385236,27.2137227286899,-16.0841493527242));
#64772=CARTESIAN_POINT('Ctrl Pts',(-24.873082935288,27.2559332399236,-16.0900094576658));
#64773=CARTESIAN_POINT('Ctrl Pts',(-24.7632195753594,27.293328197237,-16.0958695626073));
#64774=CARTESIAN_POINT('Ctrl Pts',(-24.6520319765194,27.325775151804,-16.1017296675489));
#64775=CARTESIAN_POINT('Ctrl Pts',(-24.5407694997907,27.3582439573641,-16.1075937189043));
#64776=CARTESIAN_POINT('Ctrl Pts',(-24.4281814090004,27.3857580272712,-16.1134577702598));
#64777=CARTESIAN_POINT('Ctrl Pts',(-24.3147474608509,27.4082360079799,-16.1193218216153));
#64778=CARTESIAN_POINT('Ctrl Pts',(-24.2011463337053,27.4307471167452,-16.1251945154119));
#64779=CARTESIAN_POINT('Ctrl Pts',(-24.0866972682982,27.4482072609428,-16.1310672092084));
#64780=CARTESIAN_POINT('Ctrl Pts',(-23.9718853715709,27.4605868841937,-16.136939903005));
#64781=CARTESIAN_POINT('Ctrl Pts',(-23.9404517948184,27.4639762179536,-16.1385477483282));
#64782=CARTESIAN_POINT('Ctrl Pts',(-23.9089910197629,27.46698503117,-16.1401555936514));
#64783=CARTESIAN_POINT('Ctrl Pts',(-23.8775129804176,27.4696133977923,-16.1417634389746));
#64784=CARTESIAN_POINT('Ctrl Pts',(-23.7625464520062,27.4792129215314,-16.1476357359433));
#64785=CARTESIAN_POINT('Ctrl Pts',(-23.6469645914935,27.4837657722378,-16.153508032912));
#64786=CARTESIAN_POINT('Ctrl Pts',(-23.5312480266169,27.4832066159401,-16.1593803298807));
#64787=CARTESIAN_POINT('Ctrl Pts',(-23.4156814212184,27.4826481842646,-16.1652450168189));
#64788=CARTESIAN_POINT('Ctrl Pts',(-23.2999808681678,27.4769909218239,-16.1711097037571));
#64789=CARTESIAN_POINT('Ctrl Pts',(-23.1846322499708,27.4662212253373,-16.1769743906953));
#64790=CARTESIAN_POINT('Ctrl Pts',(-23.0694022606066,27.4554626048093,-16.1828330461701));
#64791=CARTESIAN_POINT('Ctrl Pts',(-22.9545238952912,27.4396020465045,-16.1886917016449));
#64792=CARTESIAN_POINT('Ctrl Pts',(-22.8404824979914,27.4186779864829,-16.1945503571198));
#64793=CARTESIAN_POINT('Ctrl Pts',(-22.7219865432668,27.3969366142473,-16.2006378568377));
#64794=CARTESIAN_POINT('Ctrl Pts',(-22.6043947296004,27.3697281086989,-16.2067253565556));
#64795=CARTESIAN_POINT('Ctrl Pts',(-22.4882454516809,27.3371549547838,-16.2128128562735));
#64796=CARTESIAN_POINT('Ctrl Pts',(-22.3765919788,27.3058426141265,-16.2186647263569));
#64797=CARTESIAN_POINT('Ctrl Pts',(-22.2662718804477,27.2695733252326,-16.2245165964403));
#64798=CARTESIAN_POINT('Ctrl Pts',(-22.1577516841349,27.2284899342481,-16.2303684665237));
#64799=CARTESIAN_POINT('Ctrl Pts',(-22.0492480110087,27.1874127985835,-16.2362194456067));
#64800=CARTESIAN_POINT('Ctrl Pts',(-21.9425440815196,27.141523164569,-16.2420704246896));
#64801=CARTESIAN_POINT('Ctrl Pts',(-21.8380886761361,27.0910128923682,-16.2479214037726));
#64802=CARTESIAN_POINT('Ctrl Pts',(-21.7336238792065,27.0404980788079,-16.2537729089149));
#64803=CARTESIAN_POINT('Ctrl Pts',(-21.631408380444,26.9853619811752,-16.2596244140572));
#64804=CARTESIAN_POINT('Ctrl Pts',(-21.5318678399399,26.9258431816534,-16.2654759191995));
#64805=CARTESIAN_POINT('Ctrl Pts',(-21.4322942441892,26.866304617234,-16.2713293674993));
#64806=CARTESIAN_POINT('Ctrl Pts',(-21.3353977276241,26.802380668987,-16.2771828157991));
#64807=CARTESIAN_POINT('Ctrl Pts',(-21.2415757562606,26.73435374657,-16.2830362640988));
#64808=CARTESIAN_POINT('Ctrl Pts',(-21.1476470889426,26.6662494627704,-16.2888963690404));
#64809=CARTESIAN_POINT('Ctrl Pts',(-21.0568002804533,26.5940331344607,-16.2947564739819));
#64810=CARTESIAN_POINT('Ctrl Pts',(-20.9694005024232,26.5180280964915,-16.3006165789235));
#64811=CARTESIAN_POINT('Ctrl Pts',(-20.8819418661128,26.4419718738861,-16.3064806302789));
#64812=CARTESIAN_POINT('Ctrl Pts',(-20.7979351814419,26.3621221452627,-16.3123446816344));
#64813=CARTESIAN_POINT('Ctrl Pts',(-20.7177082213493,26.2788385629443,-16.3182087329898));
#64814=CARTESIAN_POINT('Ctrl Pts',(-20.6373630227325,26.1954322372505,-16.3240814267864));
#64815=CARTESIAN_POINT('Ctrl Pts',(-20.5608089387756,26.1085822663961,-16.329954120583));
#64816=CARTESIAN_POINT('Ctrl Pts',(-20.4883330566234,26.0186808025139,-16.3358268143796));
#64817=CARTESIAN_POINT('Ctrl Pts',(-20.4684903724638,25.9940672855712,-16.3374346597029));
#64818=CARTESIAN_POINT('Ctrl Pts',(-20.4489531247863,25.9692251987545,-16.3390425050262));
#64819=CARTESIAN_POINT('Ctrl Pts',(-20.4297266211311,25.9441629396887,-16.3406503503495));
#64820=CARTESIAN_POINT('Ctrl Pts',(-20.3595060983629,25.8526286199332,-16.3465226473182));
#64821=CARTESIAN_POINT('Ctrl Pts',(-20.2931988132048,25.7578486702388,-16.3523949442869));
#64822=CARTESIAN_POINT('Ctrl Pts',(-20.2311195318906,25.6601921350039,-16.3582672412556));
#64823=CARTESIAN_POINT('Ctrl Pts',(-20.1691207003948,25.562662154883,-16.3641319281938));
#64824=CARTESIAN_POINT('Ctrl Pts',(-20.1113391963867,25.4622633481716,-16.369996615132));
#64825=CARTESIAN_POINT('Ctrl Pts',(-20.0580491046271,25.3593971428242,-16.3758613020702));
#64826=CARTESIAN_POINT('Ctrl Pts',(-20.0048138183908,25.2566367289294,-16.381719957545));
#64827=CARTESIAN_POINT('Ctrl Pts',(-19.9560609457124,25.1514143285916,-16.3875786130198));
#64828=CARTESIAN_POINT('Ctrl Pts',(-19.9120204986791,25.0441590461531,-16.3934372684946));
#64829=CARTESIAN_POINT('Ctrl Pts',(-19.8662597929943,24.9327142779133,-16.3995247682125));
#64830=CARTESIAN_POINT('Ctrl Pts',(-19.8255874048656,24.8190749613919,-16.4056122679304));
#64831=CARTESIAN_POINT('Ctrl Pts',(-19.7902081371419,24.7037494545317,-16.4116997676483));
#64832=CARTESIAN_POINT('Ctrl Pts',(-19.7561982992842,24.592887866898,-16.4175516377317));
#64833=CARTESIAN_POINT('Ctrl Pts',(-19.7270795706054,24.4804686289651,-16.4234035078151));
#64834=CARTESIAN_POINT('Ctrl Pts',(-19.7029839501431,24.3669614525529,-16.4292553778985));
#64835=CARTESIAN_POINT('Ctrl Pts',(-19.6788919984582,24.2534715586404,-16.4351063569815));
#64836=CARTESIAN_POINT('Ctrl Pts',(-19.6598217201127,24.1388944598719,-16.4409573360644));
#64837=CARTESIAN_POINT('Ctrl Pts',(-19.6458542848002,24.0237114313374,-16.4468083151474));
#64838=CARTESIAN_POINT('Ctrl Pts',(-19.631885593681,23.9085180467403,-16.4526598202897));
#64839=CARTESIAN_POINT('Ctrl Pts',(-19.6230207074027,23.7927190344791,-16.458511325432));
#64840=CARTESIAN_POINT('Ctrl Pts',(-19.6192889900959,23.6768014733149,-16.4643628305743));
#64841=CARTESIAN_POINT('Ctrl Pts',(-19.6155560335671,23.560845418452,-16.470216278874));
#64842=CARTESIAN_POINT('Ctrl Pts',(-19.6169596488206,23.4447711493564,-16.4760697271738));
#64843=CARTESIAN_POINT('Ctrl Pts',(-19.6234770871048,23.3290657152479,-16.4819231754736));
#64844=CARTESIAN_POINT('Ctrl Pts',(-19.6300019371315,23.2132286989359,-16.4877832804151));
#64845=CARTESIAN_POINT('Ctrl Pts',(-19.6416521945437,23.097761767785,-16.4936433853566));
#64846=CARTESIAN_POINT('Ctrl Pts',(-19.6583532230536,22.9831469230088,-16.4995034902982));
#64847=CARTESIAN_POINT('Ctrl Pts',(-19.6750654986609,22.8684548923081,-16.5053675416536));
#64848=CARTESIAN_POINT('Ctrl Pts',(-19.6968352407293,22.7546164956185,-16.511231593009));
#64849=CARTESIAN_POINT('Ctrl Pts',(-19.7235370428939,22.6421019011402,-16.5170956443645));
#64850=CARTESIAN_POINT('Ctrl Pts',(-19.7502781981846,22.5294214826098,-16.522968338161));
#64851=CARTESIAN_POINT('Ctrl Pts',(-19.7819658081179,22.4180691562552,-16.5288410319576));
#64852=CARTESIAN_POINT('Ctrl Pts',(-19.8184251312967,22.3084984281605,-16.5347137257542));
#64853=CARTESIAN_POINT('Ctrl Pts',(-19.8284070840936,22.2784997957013,-16.5363215710776));
#64854=CARTESIAN_POINT('Ctrl Pts',(-19.8387464379272,22.2486345803725,-16.537929416401));
#64855=CARTESIAN_POINT('Ctrl Pts',(-19.8494389966857,22.218911786769,-16.5395372617244));
#64856=CARTESIAN_POINT('Ctrl Pts',(-19.8884911862661,22.1103559025435,-16.5454095586931));
#64857=CARTESIAN_POINT('Ctrl Pts',(-19.9323892495922,22.0033378902027,-16.5512818556618));
#64858=CARTESIAN_POINT('Ctrl Pts',(-19.9809928479131,21.8983220520024,-16.5571541526305));
#64859=CARTESIAN_POINT('Ctrl Pts',(-20.0295334598306,21.7934423059883,-16.5630188395687));
#64860=CARTESIAN_POINT('Ctrl Pts',(-20.0827673079848,21.6905599459587,-16.5688835265069));
#64861=CARTESIAN_POINT('Ctrl Pts',(-20.140504818735,21.5901225528485,-16.5747482134451));
#64862=CARTESIAN_POINT('Ctrl Pts',(-20.1981829500698,21.4897884533097,-16.58060686892));
#64863=CARTESIAN_POINT('Ctrl Pts',(-20.260355326458,21.3918946754607,-16.5864655243948));
#64864=CARTESIAN_POINT('Ctrl Pts',(-20.3267852665007,21.2968666814178,-16.5923241798696));
#64865=CARTESIAN_POINT('Ctrl Pts',(-20.3958100185121,21.1981268102282,-16.5984116795875));
#64866=CARTESIAN_POINT('Ctrl Pts',(-20.4694315321615,21.1024815795919,-16.6044991793054));
#64867=CARTESIAN_POINT('Ctrl Pts',(-20.5473328220045,21.0103780826009,-16.6105866790233));
#64868=CARTESIAN_POINT('Ctrl Pts',(-20.6222187766026,20.9218396475133,-16.6164385491067));
#64869=CARTESIAN_POINT('Ctrl Pts',(-20.7010590603922,20.8365742086219,-16.6222904191902));
#64870=CARTESIAN_POINT('Ctrl Pts',(-20.7835298480138,20.7549467180831,-16.6281422892736));
#64871=CARTESIAN_POINT('Ctrl Pts',(-20.865988078708,20.6733316560719,-16.6339932683565));
#64872=CARTESIAN_POINT('Ctrl Pts',(-20.9520754204128,20.5953537317816,-16.6398442474395));
#64873=CARTESIAN_POINT('Ctrl Pts',(-21.0414308439804,20.521341384226,-16.6456952265225));
#64874=CARTESIAN_POINT('Ctrl Pts',(-21.1307943014606,20.4473223822481,-16.6515467316648));
#64875=CARTESIAN_POINT('Ctrl Pts',(-21.2234261065381,20.3772699294892,-16.6573982368071));
#64876=CARTESIAN_POINT('Ctrl Pts',(-21.3189323442364,20.3114720172037,-16.6632497419494));
#64877=CARTESIAN_POINT('Ctrl Pts',(-21.4144702974771,20.2456522548639,-16.6691031902492));
#64878=CARTESIAN_POINT('Ctrl Pts',(-21.5128842411385,20.1840900767431,-16.674956638549));
#64879=CARTESIAN_POINT('Ctrl Pts',(-21.6137521158751,20.1270296146856,-16.6808100868488));
#64880=CARTESIAN_POINT('Ctrl Pts',(-21.7147346992884,20.0699042624923,-16.6866701917903));
#64881=CARTESIAN_POINT('Ctrl Pts',(-21.8181764238196,20.0172910482463,-16.6925302967319));
#64882=CARTESIAN_POINT('Ctrl Pts',(-21.9236314296828,19.969387721276,-16.6983904016734));
#64883=CARTESIAN_POINT('Ctrl Pts',(-22.0291574528923,19.9214521344132,-16.7042544530289));
#64884=CARTESIAN_POINT('Ctrl Pts',(-22.1366990745092,19.8782329043107,-16.7101185043843));
#64885=CARTESIAN_POINT('Ctrl Pts',(-22.2457929466814,19.8398786703336,-16.7159825557398));
#64886=CARTESIAN_POINT('Ctrl Pts',(-22.355047601444,19.8014679098718,-16.7218552495364));
#64887=CARTESIAN_POINT('Ctrl Pts',(-22.4658586784054,19.7679365748165,-16.727727943333));
#64888=CARTESIAN_POINT('Ctrl Pts',(-22.5777501801553,19.7393827915625,-16.7336006371295));
#64889=CARTESIAN_POINT('Ctrl Pts',(-22.6083842016166,19.7315652433544,-16.7352084824528));
#64890=CARTESIAN_POINT('Ctrl Pts',(-22.6390991674193,19.7241205002501,-16.736816327776));
#64891=CARTESIAN_POINT('Ctrl Pts',(-22.6698852336702,19.7170498993553,-16.7384241730993));
#64892=CARTESIAN_POINT('Ctrl Pts',(-22.7823244844542,19.6912261042422,-16.744296470068));
#64893=CARTESIAN_POINT('Ctrl Pts',(-22.8960892980096,19.6703105089653,-16.7501687670367));
#64894=CARTESIAN_POINT('Ctrl Pts',(-23.010713190014,19.6544360192312,-16.7560410640054));
#64895=CARTESIAN_POINT('Ctrl Pts',(-23.1251885385575,19.6385821015751,-16.7619057509436));
#64896=CARTESIAN_POINT('Ctrl Pts',(-23.240520345906,19.6277563541092,-16.7677704378818));
#64897=CARTESIAN_POINT('Ctrl Pts',(-23.3562295821199,19.6220412218181,-16.77363512482));
#64898=CARTESIAN_POINT('Ctrl Pts',(-23.4718198186278,19.6163319671828,-16.7794937802948));
#64899=CARTESIAN_POINT('Ctrl Pts',(-23.5877863015297,19.6157228936424,-16.7853524357696));
#64900=CARTESIAN_POINT('Ctrl Pts',(-23.703643146079,19.6202448574754,-16.7912110912444));
#64901=CARTESIAN_POINT('Ctrl Pts',(-23.8240254610219,19.6249434531986,-16.7972985909623));
#64902=CARTESIAN_POINT('Ctrl Pts',(-23.9442889474807,19.6351821660237,-16.8033860906802));
#64903=CARTESIAN_POINT('Ctrl Pts',(-24.0638861144647,19.6509359835475,-16.8094735903981));
#64904=CARTESIAN_POINT('Ctrl Pts',(-24.1788540185246,19.6660800160304,-16.8153254604815));
#64905=CARTESIAN_POINT('Ctrl Pts',(-24.2932057785333,19.6863200852048,-16.8211773305649));
#64906=CARTESIAN_POINT('Ctrl Pts',(-24.4064593127839,19.7115810234747,-16.8270292006483));
#64907=CARTESIAN_POINT('Ctrl Pts',(-24.5196956031539,19.7368381155371,-16.8328801797312));
#64908=CARTESIAN_POINT('Ctrl Pts',(-24.6318335968848,19.76711446671,-16.8387311588142));
#64909=CARTESIAN_POINT('Ctrl Pts',(-24.7424018211641,19.8022838723246,-16.8445821378972));
#64910=CARTESIAN_POINT('Ctrl Pts',(-24.8529799865907,19.8374564400073,-16.8504336430394));
#64911=CARTESIAN_POINT('Ctrl Pts',(-24.9619877080391,19.8775228113676,-16.8562851481817));
#64912=CARTESIAN_POINT('Ctrl Pts',(-25.0689697658909,19.9223072506082,-16.862136653324));
#64913=CARTESIAN_POINT('Ctrl Pts',(-25.1759873501553,19.9671065617863,-16.8679901016238));
#64914=CARTESIAN_POINT('Ctrl Pts',(-25.2809775521256,20.0166268967214,-16.8738435499235));
#64915=CARTESIAN_POINT('Ctrl Pts',(-25.3835068386168,20.0706451334164,-16.8796969982233));
#64916=CARTESIAN_POINT('Ctrl Pts',(-25.4861527231704,20.1247248005762,-16.8855571031648));
#64917=CARTESIAN_POINT('Ctrl Pts',(-25.5863317403879,20.1833123862622,-16.8914172081063));
#64918=CARTESIAN_POINT('Ctrl Pts',(-25.6836365143257,20.246139673051,-16.8972773130479));
#64919=CARTESIAN_POINT('Ctrl Pts',(-25.7810068169388,20.3090092700853,-16.9031413644033));
#64920=CARTESIAN_POINT('Ctrl Pts',(-25.8754986858637,20.3761240146474,-16.9090054157587));
#64921=CARTESIAN_POINT('Ctrl Pts',(-25.9667366091519,20.4471744302934,-16.9148694671142));
#64922=CARTESIAN_POINT('Ctrl Pts',(-26.0581089989263,20.518329560069,-16.9207421609107));
#64923=CARTESIAN_POINT('Ctrl Pts',(-26.1462175584178,20.5934316702402,-16.9266148547073));
#64924=CARTESIAN_POINT('Ctrl Pts',(-26.2307224354649,20.6721333376754,-16.9324875485039));
#64925=CARTESIAN_POINT('Ctrl Pts',(-26.2538584572078,20.6936805377023,-16.9340953938273));
#64926=CARTESIAN_POINT('Ctrl Pts',(-26.2767245856099,20.7154973545247,-16.9357032391507));
#64927=CARTESIAN_POINT('Ctrl Pts',(-26.2993143747,20.7375762290725,-16.9373110844741));
#64928=CARTESIAN_POINT('Ctrl Pts',(-26.3806377699755,20.8170603285002,-16.9430993386388));
#64929=CARTESIAN_POINT('Ctrl Pts',(-26.4586662175932,20.900226228552,-16.9488875928034));
#64930=CARTESIAN_POINT('Ctrl Pts',(-26.5330404097928,20.9867655560557,-16.954675846968));
#64931=CARTESIAN_POINT('Ctrl Pts',(-26.6086152118127,21.0747018730712,-16.9605575399262));
#64932=CARTESIAN_POINT('Ctrl Pts',(-26.6804163740703,21.1661212422807,-16.9664392328845));
#64933=CARTESIAN_POINT('Ctrl Pts',(-26.7481028389295,21.2606581544048,-16.9723209258427));
#64934=CARTESIAN_POINT('Ctrl Pts',(-26.8145478422971,21.3534611314478,-16.9780947405814));
#64935=CARTESIAN_POINT('Ctrl Pts',(-26.8770275175112,21.449267917509,-16.9838685553201));
#64936=CARTESIAN_POINT('Ctrl Pts',(-26.9352579987848,21.5476974169054,-16.9896423700588));
#64937=CARTESIAN_POINT('Ctrl Pts',(-26.9934512704089,21.646064019223,-16.9954124952931));
#64938=CARTESIAN_POINT('Ctrl Pts',(-27.0474005270886,21.7470496392113,-17.0011826205273));
#64939=CARTESIAN_POINT('Ctrl Pts',(-27.0968649291307,21.8502438545547,-17.0069527457615));
#64940=CARTESIAN_POINT('Ctrl Pts',(-27.1463105048046,21.9533987937273,-17.0127206748608));
#64941=CARTESIAN_POINT('Ctrl Pts',(-27.1912744352322,22.0587602733001,-17.01848860396));
#64942=CARTESIAN_POINT('Ctrl Pts',(-27.2315620264637,22.1658936895872,-17.0242565330593));
#64943=CARTESIAN_POINT('Ctrl Pts',(-27.2732260782565,22.2766874121324,-17.0302215284681));
#64944=CARTESIAN_POINT('Ctrl Pts',(-27.3098883142778,22.389375888942,-17.0361865238769));
#64945=CARTESIAN_POINT('Ctrl Pts',(-27.3413880726729,22.5034572747656,-17.0421515192857));
#64946=CARTESIAN_POINT('Ctrl Pts',(-27.3718584508006,22.6138105962031,-17.0479215846735));
#64947=CARTESIAN_POINT('Ctrl Pts',(-27.3974984315432,22.7254667676748,-17.0536916500612));
#64948=CARTESIAN_POINT('Ctrl Pts',(-27.418214072793,22.8379586902349,-17.0594617154489));
#64949=CARTESIAN_POINT('Ctrl Pts',(-27.4399794682782,22.9561510818624,-17.0655241758682));
#64950=CARTESIAN_POINT('Ctrl Pts',(-27.4563082570169,23.0752656277984,-17.0715866362876));
#64951=CARTESIAN_POINT('Ctrl Pts',(-27.4671529931717,23.1947531999408,-17.077649096707));
#64952=CARTESIAN_POINT('Ctrl Pts',(-27.4779977293266,23.3142407720832,-17.0837115571264));
#64953=CARTESIAN_POINT('Ctrl Pts',(-27.4833584329987,23.434100826989,-17.0897740175457));
#64954=CARTESIAN_POINT('Ctrl Pts',(-27.4832509455688,23.5537847349664,-17.0958364779651));
#64955=CARTESIAN_POINT('',(-27.488632695345,23.5483506220125,-18.3458364779651));
#64956=CARTESIAN_POINT('Ctrl Pts',(-27.4844422471639,23.5537858048675,-17.0958364779651));
#64957=CARTESIAN_POINT('Ctrl Pts',(-27.4869069244524,23.8194717478141,-17.1092903172598));
#64958=CARTESIAN_POINT('Ctrl Pts',(-27.3410589034169,25.3916708787352,-17.1890397936792));
#64959=CARTESIAN_POINT('Ctrl Pts',(-25.2246752877004,27.8904206466729,-17.3350849072242));
#64960=CARTESIAN_POINT('Ctrl Pts',(-20.8038927595901,27.3050173491329,-17.5339718185988));
#64961=CARTESIAN_POINT('Ctrl Pts',(-18.9067820091341,23.2693035359248,-17.7328587299738));
#64962=CARTESIAN_POINT('Ctrl Pts',(-21.2766269675343,19.4917580292833,-17.9317456413486));
#64963=CARTESIAN_POINT('Ctrl Pts',(-25.735741047741,19.443624866767,-18.1306325527235));
#64964=CARTESIAN_POINT('Ctrl Pts',(-27.4366548782404,22.0291801880755,-18.2686628315957));
#64965=CARTESIAN_POINT('Ctrl Pts',(-27.489269671134,23.441238523299,-18.3403974733429));
#64966=CARTESIAN_POINT('Ctrl Pts',(-27.488632695345,23.5483506220125,-18.3458364779651));
#64967=CARTESIAN_POINT('',(-27.4785646527166,23.5476444295195,-19.5958364779651));
#64968=CARTESIAN_POINT('Ctrl Pts',(-27.488632695345,23.5483506220125,-18.3458364779651));
#64969=CARTESIAN_POINT('Ctrl Pts',(-27.4815056189417,24.7468202098731,-18.4066931104679));
#64970=CARTESIAN_POINT('Ctrl Pts',(-26.2565009221018,27.2634742278718,-18.5338453800956));
#64971=CARTESIAN_POINT('Ctrl Pts',(-21.9699074538095,27.92555369469,-18.7272932868482));
#64972=CARTESIAN_POINT('Ctrl Pts',(-19.0149947432021,24.5857174630311,-18.9261801982231));
#64973=CARTESIAN_POINT('Ctrl Pts',(-20.2275994137689,20.2943767524232,-19.1250671095979));
#64974=CARTESIAN_POINT('Ctrl Pts',(-24.4934405851835,18.99490983022,-19.3239540209729));
#64975=CARTESIAN_POINT('Ctrl Pts',(-27.1753782638637,21.2723832772041,-19.4808771437619));
#64976=CARTESIAN_POINT('Ctrl Pts',(-27.4814874096158,23.0653136103336,-19.571504629426));
#64977=CARTESIAN_POINT('Ctrl Pts',(-27.4785646527166,23.5476444295195,-19.5958364779651));
#64978=CARTESIAN_POINT('',(-27.4825985574987,23.5531384248387,-20.8458365189298));
#64979=CARTESIAN_POINT('Ctrl Pts',(-27.4785646527166,23.5476444295195,-19.5958364779651));
#64980=CARTESIAN_POINT('Ctrl Pts',(-27.4735239361261,24.3794936205995,-19.637800266551));
#64981=CARTESIAN_POINT('Ctrl Pts',(-26.8074519009194,26.5328992923714,-19.7460596922617));
#64982=CARTESIAN_POINT('Ctrl Pts',(-23.263327982895,28.1933576495441,-19.9206147550975));
#64983=CARTESIAN_POINT('Ctrl Pts',(-19.4888354106611,25.8186532460935,-20.1195016664724));
#64984=CARTESIAN_POINT('Ctrl Pts',(-19.4464408212713,21.3594809147753,-20.3183885778472));
#64985=CARTESIAN_POINT('Ctrl Pts',(-23.1751012479069,18.9134419526009,-20.5172754892222));
#64986=CARTESIAN_POINT('Ctrl Pts',(-26.7759790602274,20.517721770008,-20.6930914559281));
#64987=CARTESIAN_POINT('Ctrl Pts',(-27.4733101236253,22.6965827824429,-20.8026117855091));
#64988=CARTESIAN_POINT('Ctrl Pts',(-27.4790977446331,23.553135043743,-20.8458364779651));
#64989=CARTESIAN_POINT('',(-27.4847362990805,23.5517471200916,-22.0958364779651));
#64990=CARTESIAN_POINT('Ctrl Pts',(-27.4832514724493,23.553139055426,-20.8458365265699));
#64991=CARTESIAN_POINT('Ctrl Pts',(-27.483153468716,23.6866728888471,-20.852568041962));
#64992=CARTESIAN_POINT('Ctrl Pts',(-27.4762508629319,23.81993123264,-20.8592995573541));
#64993=CARTESIAN_POINT('Ctrl Pts',(-27.4626513953443,23.9522775703537,-20.8660310727461));
#64994=CARTESIAN_POINT('Ctrl Pts',(-27.4489790669834,24.0853329693935,-20.8727986530367));
#64995=CARTESIAN_POINT('Ctrl Pts',(-27.4285380422173,24.2174664225096,-20.8795662333272));
#64996=CARTESIAN_POINT('Ctrl Pts',(-27.4014871218311,24.3480502076328,-20.8863338136177));
#64997=CARTESIAN_POINT('Ctrl Pts',(-27.3742636811132,24.4794668057473,-20.8931445549238));
#64998=CARTESIAN_POINT('Ctrl Pts',(-27.3403458578836,24.6093137684927,-20.8999552962299));
#64999=CARTESIAN_POINT('Ctrl Pts',(-27.2999437608413,24.7369726697458,-20.906766037536));
#65000=CARTESIAN_POINT('Ctrl Pts',(-27.2835646501324,24.7887259060794,-20.9095271290147));
#65001=CARTESIAN_POINT('Ctrl Pts',(-27.2661203833671,24.8401197870983,-20.9122882204933));
#65002=CARTESIAN_POINT('Ctrl Pts',(-27.2476271470571,24.8911141776778,-20.9150493119719));
#65003=CARTESIAN_POINT('Ctrl Pts',(-27.2082956810897,24.999569188147,-20.9209216089406));
#65004=CARTESIAN_POINT('Ctrl Pts',(-27.1641223156677,25.1064738593099,-20.9267939059093));
#65005=CARTESIAN_POINT('Ctrl Pts',(-27.115248584118,25.2113642516585,-20.9326662028781));
#65006=CARTESIAN_POINT('Ctrl Pts',(-27.0664381890429,25.3161187143889,-20.9385308898163));
#65007=CARTESIAN_POINT('Ctrl Pts',(-27.0129397142333,25.4188637181002,-20.9443955767545));
#65008=CARTESIAN_POINT('Ctrl Pts',(-26.9549438847051,25.5191521712728,-20.9502602636927));
#65009=CARTESIAN_POINT('Ctrl Pts',(-26.897007700257,25.6193374840494,-20.9561189191675));
#65010=CARTESIAN_POINT('Ctrl Pts',(-26.8345835666454,25.7170709157408,-20.9619775746424));
#65011=CARTESIAN_POINT('Ctrl Pts',(-26.7679092595578,25.8119276148205,-20.9678362301172));
#65012=CARTESIAN_POINT('Ctrl Pts',(-26.6986305953095,25.9104895001147,-20.9739237298351));
#65013=CARTESIAN_POINT('Ctrl Pts',(-26.6247631497663,26.0059449237659,-20.980011229553));
#65014=CARTESIAN_POINT('Ctrl Pts',(-26.5466250580701,26.0978476100337,-20.9860987292709));
#65015=CARTESIAN_POINT('Ctrl Pts',(-26.4715114675385,26.1861930072046,-20.9919505993543));
#65016=CARTESIAN_POINT('Ctrl Pts',(-26.39245198509,26.2712552412002,-20.9978024694377));
#65017=CARTESIAN_POINT('Ctrl Pts',(-26.3097713743408,26.3526701945486,-21.0036543395211));
#65018=CARTESIAN_POINT('Ctrl Pts',(-26.2271033524663,26.4340727517301,-21.0095053186041));
#65019=CARTESIAN_POINT('Ctrl Pts',(-26.1408155930216,26.5118288424783,-21.0153562976871));
#65020=CARTESIAN_POINT('Ctrl Pts',(-26.0512699693086,26.5856109580993,-21.0212072767701));
#65021=CARTESIAN_POINT('Ctrl Pts',(-25.9617162945825,26.6593997074424,-21.0270587819124));
#65022=CARTESIAN_POINT('Ctrl Pts',(-25.8689044923576,26.7292135084934,-21.0329102870547));
#65023=CARTESIAN_POINT('Ctrl Pts',(-25.7732292175498,26.7947653848268,-21.038761792197));
#65024=CARTESIAN_POINT('Ctrl Pts',(-25.6775221710659,26.8603390295113,-21.0446152404968));
#65025=CARTESIAN_POINT('Ctrl Pts',(-25.5789501020386,26.9216477017333,-21.0504686887966));
#65026=CARTESIAN_POINT('Ctrl Pts',(-25.477935696772,26.9784483567712,-21.0563221370963));
#65027=CARTESIAN_POINT('Ctrl Pts',(-25.3768064161918,27.035313606488,-21.0621822420379));
#65028=CARTESIAN_POINT('Ctrl Pts',(-25.2732296161714,27.0876604037614,-21.0680423469794));
#65029=CARTESIAN_POINT('Ctrl Pts',(-25.1676516639953,27.1352921474909,-21.073902451921));
#65030=CARTESIAN_POINT('Ctrl Pts',(-25.0620026116764,27.1829559682186,-21.0797665032764));
#65031=CARTESIAN_POINT('Ctrl Pts',(-24.9543501067855,27.2258982599754,-21.0856305546319));
#65032=CARTESIAN_POINT('Ctrl Pts',(-24.8451578782144,27.2639715764731,-21.0914946059873));
#65033=CARTESIAN_POINT('Ctrl Pts',(-24.7358047220951,27.3021010054391,-21.0973672997839));
#65034=CARTESIAN_POINT('Ctrl Pts',(-24.6249077078045,27.3353470191755,-21.1032399935805));
#65035=CARTESIAN_POINT('Ctrl Pts',(-24.5129430837383,27.3636127167548,-21.1091126873771));
#65036=CARTESIAN_POINT('Ctrl Pts',(-24.4822890426096,27.3713513919243,-21.1107205327004));
#65037=CARTESIAN_POINT('Ctrl Pts',(-24.4515550169493,27.3787170548869,-21.1123283780236));
#65038=CARTESIAN_POINT('Ctrl Pts',(-24.4207508540594,27.3857083938779,-21.1139362233469));
#65039=CARTESIAN_POINT('Ctrl Pts',(-24.3082455093324,27.4112427025393,-21.1198085203156));
#65040=CARTESIAN_POINT('Ctrl Pts',(-24.1944272391577,27.4318654158323,-21.1256808172843));
#65041=CARTESIAN_POINT('Ctrl Pts',(-24.0797628683909,27.4474448291478,-21.131553114253));
#65042=CARTESIAN_POINT('Ctrl Pts',(-23.9652470935423,27.4630040527808,-21.1374178011912));
#65043=CARTESIAN_POINT('Ctrl Pts',(-23.8498878044433,27.4735329184888,-21.1432824881294));
#65044=CARTESIAN_POINT('Ctrl Pts',(-23.7341642416473,27.4789502145074,-21.1491471750676));
#65045=CARTESIAN_POINT('Ctrl Pts',(-23.6185596932913,27.4843619391763,-21.1550058305424));
#65046=CARTESIAN_POINT('Ctrl Pts',(-23.5025920268501,27.4846725312448,-21.1608644860173));
#65047=CARTESIAN_POINT('Ctrl Pts',(-23.3867472048801,27.4798523851276,-21.1667231414921));
#65048=CARTESIAN_POINT('Ctrl Pts',(-23.2663773821291,27.4748439598574,-21.17281064121));
#65049=CARTESIAN_POINT('Ctrl Pts',(-23.1461406468572,27.4642957416819,-21.1788981409279));
#65050=CARTESIAN_POINT('Ctrl Pts',(-23.0265844238634,27.4482341520768,-21.1849856406458));
#65051=CARTESIAN_POINT('Ctrl Pts',(-22.9116558789694,27.4327942604864,-21.1908375107292));
#65052=CARTESIAN_POINT('Ctrl Pts',(-22.797356592481,27.4122599349417,-21.1966893808126));
#65053=CARTESIAN_POINT('Ctrl Pts',(-22.6841684510391,27.3867075835925,-21.202541250896));
#65054=CARTESIAN_POINT('Ctrl Pts',(-22.5709975435209,27.361159122821,-21.2083922299789));
#65055=CARTESIAN_POINT('Ctrl Pts',(-22.458937847786,27.330594246407,-21.2142432090619));
#65056=CARTESIAN_POINT('Ctrl Pts',(-22.3484605102543,27.2951403720979,-21.2200941881449));
#65057=CARTESIAN_POINT('Ctrl Pts',(-22.2379732397468,27.2596833101443,-21.2259456932872));
#65058=CARTESIAN_POINT('Ctrl Pts',(-22.1290690038953,27.2193365027983,-21.2317971984295));
#65059=CARTESIAN_POINT('Ctrl Pts',(-22.022202568494,27.1742768569387,-21.2376487035718));
#65060=CARTESIAN_POINT('Ctrl Pts',(-21.9153006450761,27.1292022477517,-21.2435021518715));
#65061=CARTESIAN_POINT('Ctrl Pts',(-21.8104382484081,27.0794118486078,-21.2493556001713));
#65062=CARTESIAN_POINT('Ctrl Pts',(-21.7080483359584,27.0251298966113,-21.2552090484711));
#65063=CARTESIAN_POINT('Ctrl Pts',(-21.6055419839445,26.9707862142483,-21.2610691534126));
#65064=CARTESIAN_POINT('Ctrl Pts',(-21.5055140937677,26.9119409776187,-21.2669292583541));
#65065=CARTESIAN_POINT('Ctrl Pts',(-21.4083713496726,26.8488634517789,-21.2727893632957));
#65066=CARTESIAN_POINT('Ctrl Pts',(-21.3111631860194,26.7857434471733,-21.2786534146511));
#65067=CARTESIAN_POINT('Ctrl Pts',(-21.2168443728608,26.7183857177359,-21.2845174660066));
#65068=CARTESIAN_POINT('Ctrl Pts',(-21.1257896243579,26.6471007053944,-21.290381517362));
#65069=CARTESIAN_POINT('Ctrl Pts',(-21.034600679332,26.5757106331746,-21.2962542111586));
#65070=CARTESIAN_POINT('Ctrl Pts',(-20.9466857126837,26.5003819942177,-21.3021269049551));
#65071=CARTESIAN_POINT('Ctrl Pts',(-20.8623836812363,26.4214630852305,-21.3079995987517));
#65072=CARTESIAN_POINT('Ctrl Pts',(-20.8393031952265,26.3998564081016,-21.3096074440751));
#65073=CARTESIAN_POINT('Ctrl Pts',(-20.8164932956146,26.3779808097333,-21.3112152893984));
#65074=CARTESIAN_POINT('Ctrl Pts',(-20.7939604088947,26.3558438657615,-21.3128231347218));
#65075=CARTESIAN_POINT('Ctrl Pts',(-20.7116640583318,26.2749936079077,-21.3186954316905));
#65076=CARTESIAN_POINT('Ctrl Pts',(-20.6327902234969,26.1903838383324,-21.3245677286592));
#65077=CARTESIAN_POINT('Ctrl Pts',(-20.5577020483122,26.1023361126942,-21.3304400256279));
#65078=CARTESIAN_POINT('Ctrl Pts',(-20.4827111814391,26.014402489916,-21.3363047125661));
#65079=CARTESIAN_POINT('Ctrl Pts',(-20.4114964838776,25.9230400827357,-21.3421693995043));
#65080=CARTESIAN_POINT('Ctrl Pts',(-20.344385330283,25.8286081858703,-21.3480340864425));
#65081=CARTESIAN_POINT('Ctrl Pts',(-20.2773431963087,25.7342734062994,-21.3538927419173));
#65082=CARTESIAN_POINT('Ctrl Pts',(-20.2143964500605,25.6368757509681,-21.3597513973922));
#65083=CARTESIAN_POINT('Ctrl Pts',(-20.1558326825771,25.5368080652547,-21.365610052867));
#65084=CARTESIAN_POINT('Ctrl Pts',(-20.0949813627536,25.4328316475989,-21.3716975525849));
#65085=CARTESIAN_POINT('Ctrl Pts',(-20.0388627030738,25.3259727057584,-21.3777850523028));
#65086=CARTESIAN_POINT('Ctrl Pts',(-19.9877503810177,25.2167060793292,-21.3838725520207));
#65087=CARTESIAN_POINT('Ctrl Pts',(-19.938616470185,25.1116688502621,-21.3897244221041));
#65088=CARTESIAN_POINT('Ctrl Pts',(-19.8941087329581,25.004407269329,-21.3955762921875));
#65089=CARTESIAN_POINT('Ctrl Pts',(-19.8544233660366,24.8953680576899,-21.4014281622709));
#65090=CARTESIAN_POINT('Ctrl Pts',(-19.8147440415731,24.7863454482623,-21.4072791413539));
#65091=CARTESIAN_POINT('Ctrl Pts',(-19.7798857688329,24.6755461346364,-21.4131301204369));
#65092=CARTESIAN_POINT('Ctrl Pts',(-19.7499960237405,24.5634353748944,-21.4189810995198));
#65093=CARTESIAN_POINT('Ctrl Pts',(-19.7201035912723,24.4513145353162,-21.4248326046621));
#65094=CARTESIAN_POINT('Ctrl Pts',(-19.6951806809851,24.337882414679,-21.4306841098044));
#65095=CARTESIAN_POINT('Ctrl Pts',(-19.6753242783446,24.2236172407433,-21.4365356149467));
#65096=CARTESIAN_POINT('Ctrl Pts',(-19.655461281825,24.1093141218307,-21.4423890632465));
#65097=CARTESIAN_POINT('Ctrl Pts',(-19.6406682091888,23.9941778066043,-21.4482425115463));
#65098=CARTESIAN_POINT('Ctrl Pts',(-19.6309904378639,23.8786937591073,-21.4540959598461));
#65099=CARTESIAN_POINT('Ctrl Pts',(-19.6213016608115,23.7630783811716,-21.4599560647876));
#65100=CARTESIAN_POINT('Ctrl Pts',(-19.6167398305841,23.6471148938481,-21.4658161697292));
#65101=CARTESIAN_POINT('Ctrl Pts',(-19.6172982400469,23.5312909965933,-21.4716762746707));
#65102=CARTESIAN_POINT('Ctrl Pts',(-19.6178570255636,23.4153890991928,-21.4775403260262));
#65103=CARTESIAN_POINT('Ctrl Pts',(-19.6235428965134,23.2996273909202,-21.4834043773816));
#65104=CARTESIAN_POINT('Ctrl Pts',(-19.6342972217834,23.1844889321087,-21.4892684287371));
#65105=CARTESIAN_POINT('Ctrl Pts',(-19.6450673967821,23.0691807821928,-21.4951411225337));
#65106=CARTESIAN_POINT('Ctrl Pts',(-19.6609208781658,22.9544981229286,-21.5010138163302));
#65107=CARTESIAN_POINT('Ctrl Pts',(-19.6817478586037,22.8409143935139,-21.5068865101268));
#65108=CARTESIAN_POINT('Ctrl Pts',(-19.6874499374547,22.8098170684245,-21.5084943554501));
#65109=CARTESIAN_POINT('Ctrl Pts',(-19.6935245276755,22.7788020288813,-21.5101022007734));
#65110=CARTESIAN_POINT('Ctrl Pts',(-19.6999687295489,22.7478787765541,-21.5117100460967));
#65111=CARTESIAN_POINT('Ctrl Pts',(-19.7235047417377,22.6349384841817,-21.5175823430654));
#65112=CARTESIAN_POINT('Ctrl Pts',(-19.7520537090575,22.5228454362526,-21.5234546400341));
#65113=CARTESIAN_POINT('Ctrl Pts',(-19.7855413960222,22.4120789663066,-21.5293269370028));
#65114=CARTESIAN_POINT('Ctrl Pts',(-19.8189856856041,22.3014560409088,-21.535191623941));
#65115=CARTESIAN_POINT('Ctrl Pts',(-19.8573558486285,22.1921566667845,-21.5410563108792));
#65116=CARTESIAN_POINT('Ctrl Pts',(-19.9005265643013,22.0846504837501,-21.5469209978174));
#65117=CARTESIAN_POINT('Ctrl Pts',(-19.9436528815955,21.9772548640951,-21.5527796532922));
#65118=CARTESIAN_POINT('Ctrl Pts',(-19.9915697783382,21.8716491486544,-21.558638308767));
#65119=CARTESIAN_POINT('Ctrl Pts',(-20.04410220227,21.7682876421752,-21.5644969642418));
#65120=CARTESIAN_POINT('Ctrl Pts',(-20.0986865889506,21.660888744213,-21.5705844639597));
#65121=CARTESIAN_POINT('Ctrl Pts',(-20.158254295031,21.5559133861147,-21.5766719636776));
#65122=CARTESIAN_POINT('Ctrl Pts',(-20.2225537642718,21.4538484882676,-21.5827594633955));
#65123=CARTESIAN_POINT('Ctrl Pts',(-20.2843643856869,21.3557342295484,-21.5886113334789));
#65124=CARTESIAN_POINT('Ctrl Pts',(-20.3505470345989,21.2603096918223,-21.5944632035623));
#65125=CARTESIAN_POINT('Ctrl Pts',(-20.4208319296343,21.1679814103893,-21.6003150736457));
#65126=CARTESIAN_POINT('Ctrl Pts',(-20.4911061231554,21.0756671867768,-21.6061660527286));
#65127=CARTESIAN_POINT('Ctrl Pts',(-20.5654810705637,20.9864486109287,-21.6120170318116));
#65128=CARTESIAN_POINT('Ctrl Pts',(-20.6436450594176,20.9007012485321,-21.6178680108945));
#65129=CARTESIAN_POINT('Ctrl Pts',(-20.7218160759664,20.8149461766223,-21.6237195160368));
#65130=CARTESIAN_POINT('Ctrl Pts',(-20.8037765326829,20.7326632441018,-21.6295710211791));
#65131=CARTESIAN_POINT('Ctrl Pts',(-20.8891765132842,20.654192548848,-21.6354225263214));
#65132=CARTESIAN_POINT('Ctrl Pts',(-20.9746048533599,20.5756957951846,-21.6412759746211));
#65133=CARTESIAN_POINT('Ctrl Pts',(-21.0634746842623,20.5010140756193,-21.6471294229209));
#65134=CARTESIAN_POINT('Ctrl Pts',(-21.1554021053699,20.4304479808394,-21.6529828712207));
#65135=CARTESIAN_POINT('Ctrl Pts',(-21.2474340679171,20.3598016370865,-21.6588429761622));
#65136=CARTESIAN_POINT('Ctrl Pts',(-21.3425302328383,20.2932805118373,-21.6647030811037));
#65137=CARTESIAN_POINT('Ctrl Pts',(-21.4402766649077,20.2311425844977,-21.6705631860452));
#65138=CARTESIAN_POINT('Ctrl Pts',(-21.5380889230812,20.1689628111533,-21.6764272374007));
#65139=CARTESIAN_POINT('Ctrl Pts',(-21.6385546448185,20.1111723189739,-21.6822912887561));
#65140=CARTESIAN_POINT('Ctrl Pts',(-21.7412357307542,20.057982895209,-21.6881553401115));
#65141=CARTESIAN_POINT('Ctrl Pts',(-21.8440681481136,20.0047150808509,-21.6940280339081));
#65142=CARTESIAN_POINT('Ctrl Pts',(-21.9491220722908,19.9560620416572,-21.6999007277046));
#65143=CARTESIAN_POINT('Ctrl Pts',(-22.055939835428,19.912187308835,-21.7057734215012));
#65144=CARTESIAN_POINT('Ctrl Pts',(-22.085184752134,19.9001751409221,-21.7073812668246));
#65145=CARTESIAN_POINT('Ctrl Pts',(-22.1145617988165,19.8885208519009,-21.7089891121481));
#65146=CARTESIAN_POINT('Ctrl Pts',(-22.1440614141416,19.8772271382459,-21.7105969574715));
#65147=CARTESIAN_POINT('Ctrl Pts',(-22.2518021894051,19.8359793642871,-21.7164692544402));
#65148=CARTESIAN_POINT('Ctrl Pts',(-22.3615398784659,19.7994070451275,-21.7223415514089));
#65149=CARTESIAN_POINT('Ctrl Pts',(-22.472831082547,19.7677068253058,-21.7282138483776));
#65150=CARTESIAN_POINT('Ctrl Pts',(-22.5839780620662,19.7360476864513,-21.7340785353158));
#65151=CARTESIAN_POINT('Ctrl Pts',(-22.6966741591104,19.7092482031442,-21.739943222254));
#65152=CARTESIAN_POINT('Ctrl Pts',(-22.8104565166202,19.687456801128,-21.7458079091922));
#65153=CARTESIAN_POINT('Ctrl Pts',(-22.9241218560982,19.6656878102045,-21.751666564667));
#65154=CARTESIAN_POINT('Ctrl Pts',(-23.0388708304082,19.648916733256,-21.7575252201418));
#65155=CARTESIAN_POINT('Ctrl Pts',(-23.1542266021768,19.6372418668544,-21.7633838756166));
#65156=CARTESIAN_POINT('Ctrl Pts',(-23.274088271995,19.6251109698881,-21.7694713753345));
#65157=CARTESIAN_POINT('Ctrl Pts',(-23.3946046724564,19.6184826491818,-21.7755588750524));
#65158=CARTESIAN_POINT('Ctrl Pts',(-23.5152301724579,19.6174084673619,-21.7816463747703));
#65159=CARTESIAN_POINT('Ctrl Pts',(-23.6311866057169,19.616375864036,-21.7874982448537));
#65160=CARTESIAN_POINT('Ctrl Pts',(-23.747243397781,19.6204754290202,-21.7933501149371));
#65161=CARTESIAN_POINT('Ctrl Pts',(-23.8629126954122,19.6296999402826,-21.7992019850205));
#65162=CARTESIAN_POINT('Ctrl Pts',(-23.9785643813411,19.6389230470294,-21.8050529641035));
#65163=CARTESIAN_POINT('Ctrl Pts',(-24.0938282781855,19.6532695156755,-21.8109039431864));
#65164=CARTESIAN_POINT('Ctrl Pts',(-24.2082199224427,19.672680106489,-21.8167549222694));
#65165=CARTESIAN_POINT('Ctrl Pts',(-24.3226218516095,19.6920924425014,-21.8226064274117));
#65166=CARTESIAN_POINT('Ctrl Pts',(-24.4361509647081,19.7165697366414,-21.828457932554));
#65167=CARTESIAN_POINT('Ctrl Pts',(-24.548331987103,19.7460014357897,-21.8343094376963));
#65168=CARTESIAN_POINT('Ctrl Pts',(-24.6605502623735,19.7754429085646,-21.840162885996));
#65169=CARTESIAN_POINT('Ctrl Pts',(-24.7714191571347,19.809841952975,-21.8460163342958));
#65170=CARTESIAN_POINT('Ctrl Pts',(-24.8804782648373,19.8490380689963,-21.8518697825955));
#65171=CARTESIAN_POINT('Ctrl Pts',(-24.989661396427,19.8882787595128,-21.8577298875371));
#65172=CARTESIAN_POINT('Ctrl Pts',(-25.0970302437597,19.9323272703802,-21.8635899924786));
#65173=CARTESIAN_POINT('Ctrl Pts',(-25.2021440148948,19.9809747997533,-21.8694500974201));
#65174=CARTESIAN_POINT('Ctrl Pts',(-25.3073285735761,20.0296550901927,-21.8753141487756));
#65175=CARTESIAN_POINT('Ctrl Pts',(-25.4102546659133,20.0829403765934,-21.881178200131));
#65176=CARTESIAN_POINT('Ctrl Pts',(-25.5105073004607,20.1405765585953,-21.8870422514865));
#65177=CARTESIAN_POINT('Ctrl Pts',(-25.610907687379,20.1982976848241,-21.892914945283));
#65178=CARTESIAN_POINT('Ctrl Pts',(-25.7086264051352,20.2603822836222,-21.8987876390796));
#65179=CARTESIAN_POINT('Ctrl Pts',(-25.8032784833016,20.3265337068921,-21.9046603328761));
#65180=CARTESIAN_POINT('Ctrl Pts',(-25.8291926389689,20.344644860006,-21.9062681781995));
#65181=CARTESIAN_POINT('Ctrl Pts',(-25.8548771269737,20.3630606249987,-21.9078760235229));
#65182=CARTESIAN_POINT('Ctrl Pts',(-25.8803245104205,20.3817744153181,-21.9094838688464));
#65183=CARTESIAN_POINT('Ctrl Pts',(-25.9724125688686,20.4494951937751,-21.9153022805674));
#65184=CARTESIAN_POINT('Ctrl Pts',(-26.0617139492967,20.521357777344,-21.9211206922885));
#65185=CARTESIAN_POINT('Ctrl Pts',(-26.1478276033948,20.5971029000501,-21.9269391040095));
#65186=CARTESIAN_POINT('Ctrl Pts',(-26.2338292961867,20.672749542173,-21.9327499508794));
#65187=CARTESIAN_POINT('Ctrl Pts',(-26.3166511878312,20.7522684131351,-21.9385607977493));
#65188=CARTESIAN_POINT('Ctrl Pts',(-26.3959219135356,20.8353575485963,-21.9443716446192));
#65189=CARTESIAN_POINT('Ctrl Pts',(-26.4751117596737,20.9183619085847,-21.9501765627081));
#65190=CARTESIAN_POINT('Ctrl Pts',(-26.550757354672,21.0049289869369,-21.955981480797));
#65191=CARTESIAN_POINT('Ctrl Pts',(-26.6225217010584,21.0947177323126,-21.9617863988858));
#65192=CARTESIAN_POINT('Ctrl Pts',(-26.6942341937376,21.1844416003563,-21.9675871226005));
#65193=CARTESIAN_POINT('Ctrl Pts',(-26.762070752269,21.2773821779639,-21.9733878463151));
#65194=CARTESIAN_POINT('Ctrl Pts',(-26.8257329654358,21.3731634365545,-21.9791885700298));
#65195=CARTESIAN_POINT('Ctrl Pts',(-26.8893712767439,21.4689087342511,-21.9849871158736));
#65196=CARTESIAN_POINT('Ctrl Pts',(-26.9488381241163,21.567492242681,-21.9907856617174));
#65197=CARTESIAN_POINT('Ctrl Pts',(-27.0038773656675,21.6685074623071,-21.9965842075612));
#65198=CARTESIAN_POINT('Ctrl Pts',(-27.0589098750446,21.7695103261661,-22.0023820441507));
#65199=CARTESIAN_POINT('Ctrl Pts',(-27.1095156537141,21.8729439395001,-22.0081798807402));
#65200=CARTESIAN_POINT('Ctrl Pts',(-27.1554840438975,21.9783763459162,-22.0139777173297));
#65201=CARTESIAN_POINT('Ctrl Pts',(-27.2014584478216,22.0838225453569,-22.0197763124118));
#65202=CARTESIAN_POINT('Ctrl Pts',(-27.2427940897842,22.1912676706322,-22.0255749074939));
#65203=CARTESIAN_POINT('Ctrl Pts',(-27.2793284004151,22.3002596655853,-22.031373502576));
#65204=CARTESIAN_POINT('Ctrl Pts',(-27.3158981278116,22.4093573185858,-22.0371777188804));
#65205=CARTESIAN_POINT('Ctrl Pts',(-27.3476570957907,22.5200044350151,-22.0429819351848));
#65206=CARTESIAN_POINT('Ctrl Pts',(-27.3744925979449,22.6317336610754,-22.0487861514892));
#65207=CARTESIAN_POINT('Ctrl Pts',(-27.401341916976,22.7435204135032,-22.0545933562282));
#65208=CARTESIAN_POINT('Ctrl Pts',(-27.423262642645,22.8563899711206,-22.0604005609671));
#65209=CARTESIAN_POINT('Ctrl Pts',(-27.4401935372969,22.9698664766146,-22.0662077657061));
#65210=CARTESIAN_POINT('Ctrl Pts',(-27.4571501620944,23.0835154341303,-22.072023795745));
#65211=CARTESIAN_POINT('Ctrl Pts',(-27.4691017686041,23.1977727624032,-22.0778398257839));
#65212=CARTESIAN_POINT('Ctrl Pts',(-27.4760391345818,23.3121589606166,-22.0836558558228));
#65213=CARTESIAN_POINT('Ctrl Pts',(-27.4808821536785,23.3920126895583,-22.0877160632036));
#65214=CARTESIAN_POINT('Ctrl Pts',(-27.483282568071,23.4719291877988,-22.0917762705843));
#65215=CARTESIAN_POINT('Ctrl Pts',(-27.4832522479274,23.5517465563465,-22.0958364779651));
#65216=CARTESIAN_POINT('',(-27.4832508741802,23.5466417143109,-23.3458364779651));
#65217=CARTESIAN_POINT('Ctrl Pts',(-27.4890683231693,23.5517487656932,-22.0958364779651));
#65218=CARTESIAN_POINT('Ctrl Pts',(-27.4894675906155,23.6340053585404,-22.1000145787172));
#65219=CARTESIAN_POINT('Ctrl Pts',(-27.4871150503414,23.7162386824283,-22.1041926794693));
#65220=CARTESIAN_POINT('Ctrl Pts',(-27.3997979165351,25.1002966205361,-22.1746664173463));
#65221=CARTESIAN_POINT('Ctrl Pts',(-25.8134246394771,27.6145855449525,-22.3072576915961));
#65222=CARTESIAN_POINT('Ctrl Pts',(-21.3542014421887,27.6512414910049,-22.5061446029711));
#65223=CARTESIAN_POINT('Ctrl Pts',(-18.9129630017294,23.9194362899765,-22.7050315143459));
#65224=CARTESIAN_POINT('Ctrl Pts',(-20.7330004619926,19.8483825167044,-22.903918425721));
#65225=CARTESIAN_POINT('Ctrl Pts',(-25.1418537107282,19.1790334203933,-23.1028053370958));
#65226=CARTESIAN_POINT('Ctrl Pts',(-27.3240420942646,21.6583151087892,-23.2501113545105));
#65227=CARTESIAN_POINT('Ctrl Pts',(-27.4863816571791,23.2559105440861,-23.3311217348003));
#65228=CARTESIAN_POINT('Ctrl Pts',(-27.4836796968938,23.5466413206162,-23.3458364779651));
#65229=CARTESIAN_POINT('',(-27.4832525287817,23.5504038905352,-24.5958364779952));
#65230=CARTESIAN_POINT('Ctrl Pts',(-27.4832508741802,23.5466417143109,-23.3458364779651));
#65231=CARTESIAN_POINT('Ctrl Pts',(-27.4833557182763,23.6608406926443,-23.3516171098966));
#65232=CARTESIAN_POINT('Ctrl Pts',(-27.4784825236897,23.7751880197479,-23.3573977418282));
#65233=CARTESIAN_POINT('Ctrl Pts',(-27.4686193057639,23.889208021201,-23.3631783737597));
#65234=CARTESIAN_POINT('Ctrl Pts',(-27.4587638157106,24.003138687505,-23.3689544765419));
#65235=CARTESIAN_POINT('Ctrl Pts',(-27.4439261121891,24.1167421157918,-23.3747305793241));
#65236=CARTESIAN_POINT('Ctrl Pts',(-27.4241462761573,24.2295435272252,-23.3805066821063));
#65237=CARTESIAN_POINT('Ctrl Pts',(-27.4043746756592,24.3422979726569,-23.38628037995));
#65238=CARTESIAN_POINT('Ctrl Pts',(-27.379665103976,24.454250646175,-23.3920540777937));
#65239=CARTESIAN_POINT('Ctrl Pts',(-27.3501093088941,24.5649335026246,-23.3978277756374));
#65240=CARTESIAN_POINT('Ctrl Pts',(-27.3205582084652,24.6755987781697,-23.4036005563849));
#65241=CARTESIAN_POINT('Ctrl Pts',(-27.2861625243139,24.7849942264451,-23.4093733371324));
#65242=CARTESIAN_POINT('Ctrl Pts',(-27.2470645714314,24.8926644442061,-23.4151461178799));
#65243=CARTESIAN_POINT('Ctrl Pts',(-27.2079627601056,25.0003452875728,-23.4209194683233));
#65244=CARTESIAN_POINT('Ctrl Pts',(-27.164157904009,25.1063001623625,-23.4266928187668));
#65245=CARTESIAN_POINT('Ctrl Pts',(-27.1158410934982,25.210092044398,-23.4324661692103));
#65246=CARTESIAN_POINT('Ctrl Pts',(-27.0674764450961,25.3139866895237,-23.4382452357784));
#65247=CARTESIAN_POINT('Ctrl Pts',(-27.0145911004505,25.415713678327,-23.4440243023465));
#65248=CARTESIAN_POINT('Ctrl Pts',(-26.9574229325611,25.5148590723166,-23.4498033689146));
#65249=CARTESIAN_POINT('Ctrl Pts',(-26.9002266367599,25.6140532478746,-23.455585278902));
#65250=CARTESIAN_POINT('Ctrl Pts',(-26.838743551296,25.7106629410969,-23.4613671888895));
#65251=CARTESIAN_POINT('Ctrl Pts',(-26.7732547789132,25.8043034438124,-23.4671490988769));
#65252=CARTESIAN_POINT('Ctrl Pts',(-26.7076582898858,25.8980979674447,-23.4729405190127));
#65253=CARTESIAN_POINT('Ctrl Pts',(-26.6380432119247,25.9889132072198,-23.4787319391486));
#65254=CARTESIAN_POINT('Ctrl Pts',(-26.5647310345513,26.0763974910765,-23.4845233592844));
#65255=CARTESIAN_POINT('Ctrl Pts',(-26.4969822112343,26.1572429590788,-23.4898752928048));
#65256=CARTESIAN_POINT('Ctrl Pts',(-26.426076723758,26.2352440384564,-23.4952272263252));
#65257=CARTESIAN_POINT('Ctrl Pts',(-26.3522944087462,26.3101529500511,-23.5005791598455));
#65258=CARTESIAN_POINT('Ctrl Pts',(-26.2713383088362,26.3923451844673,-23.5064514568142));
#65259=CARTESIAN_POINT('Ctrl Pts',(-26.1866271048295,26.4711100677901,-23.512323753783));
#65260=CARTESIAN_POINT('Ctrl Pts',(-26.0984828194568,26.5460848702154,-23.5181960507517));
#65261=CARTESIAN_POINT('Ctrl Pts',(-26.0104527620777,26.6209625112511,-23.5240607376899));
#65262=CARTESIAN_POINT('Ctrl Pts',(-25.9189987827724,26.692059573523,-23.529925424628));
#65263=CARTESIAN_POINT('Ctrl Pts',(-25.824480597266,26.7590491450316,-23.5357901115662));
#65264=CARTESIAN_POINT('Ctrl Pts',(-25.7300596177961,26.8259698219597,-23.5416487670411));
#65265=CARTESIAN_POINT('Ctrl Pts',(-25.6325810355479,26.8887911728701,-23.5475074225159));
#65266=CARTESIAN_POINT('Ctrl Pts',(-25.5324380656816,26.9472261125234,-23.5533660779907));
#65267=CARTESIAN_POINT('Ctrl Pts',(-25.4283834232077,27.0079435723882,-23.5594535777086));
#65268=CARTESIAN_POINT('Ctrl Pts',(-25.3214523495019,27.0639246664437,-23.5655410774265));
#65269=CARTESIAN_POINT('Ctrl Pts',(-25.2121200359687,27.1148963285183,-23.5716285771445));
#65270=CARTESIAN_POINT('Ctrl Pts',(-25.1070196623568,27.1638950239134,-23.5774804472279));
#65271=CARTESIAN_POINT('Ctrl Pts',(-24.9997008922467,27.2082646869657,-23.5833323173113));
#65272=CARTESIAN_POINT('Ctrl Pts',(-24.8906106989184,27.2478096960333,-23.5891841873947));
#65273=CARTESIAN_POINT('Ctrl Pts',(-24.7815371155639,27.2873486840137,-23.5950351664776));
#65274=CARTESIAN_POINT('Ctrl Pts',(-24.6706930338013,27.3220643377828,-23.6008861455606));
#65275=CARTESIAN_POINT('Ctrl Pts',(-24.5585439011175,27.3518097802894,-23.6067371246436));
#65276=CARTESIAN_POINT('Ctrl Pts',(-24.4463846851479,27.3815578971973,-23.6125886297859));
#65277=CARTESIAN_POINT('Ctrl Pts',(-24.3329205845939,27.4063348085226,-23.6184401349282));
#65278=CARTESIAN_POINT('Ctrl Pts',(-24.2186299516329,27.426044144322,-23.6242916400704));
#65279=CARTESIAN_POINT('Ctrl Pts',(-24.1043013652403,27.4457600251628,-23.6301450883702));
#65280=CARTESIAN_POINT('Ctrl Pts',(-23.9891461078219,27.4604049140596,-23.63599853667));
#65281=CARTESIAN_POINT('Ctrl Pts',(-23.8736497014162,27.4699340583767,-23.6418519849698));
#65282=CARTESIAN_POINT('Ctrl Pts',(-23.7580219505167,27.4794740394,-23.6477120899113));
#65283=CARTESIAN_POINT('Ctrl Pts',(-23.6420526884998,27.4838866298542,-23.6535721948528));
#65284=CARTESIAN_POINT('Ctrl Pts',(-23.5262296057866,27.4831791644997,-23.6594322997944));
#65285=CARTESIAN_POINT('Ctrl Pts',(-23.4103285234763,27.4824712227116,-23.6652963511499));
#65286=CARTESIAN_POINT('Ctrl Pts',(-23.2945742283383,27.4766363801485,-23.6711604025053));
#65287=CARTESIAN_POINT('Ctrl Pts',(-23.179449704852,27.4657338895359,-23.6770244538608));
#65288=CARTESIAN_POINT('Ctrl Pts',(-23.0641555107995,27.4548153308285,-23.6828971476573));
#65289=CARTESIAN_POINT('Ctrl Pts',(-22.9494933487008,27.4388142749035,-23.6887698414539));
#65290=CARTESIAN_POINT('Ctrl Pts',(-22.8359365160484,27.41784113828,-23.6946425352505));
#65291=CARTESIAN_POINT('Ctrl Pts',(-22.8048465548419,27.4120990443101,-23.6962503805738));
#65292=CARTESIAN_POINT('Ctrl Pts',(-22.7738393585066,27.405984545174,-23.6978582258971));
#65293=CARTESIAN_POINT('Ctrl Pts',(-22.7429244249728,27.3995005528144,-23.6994660712205));
#65294=CARTESIAN_POINT('Ctrl Pts',(-22.6300145151427,27.3758192147366,-23.7053383681892));
#65295=CARTESIAN_POINT('Ctrl Pts',(-22.5179583003379,27.3471260160167,-23.7112106651579));
#65296=CARTESIAN_POINT('Ctrl Pts',(-22.4072350181661,27.3134958089443,-23.7170829621266));
#65297=CARTESIAN_POINT('Ctrl Pts',(-22.2966552245749,27.2799091839495,-23.7229476490648));
#65298=CARTESIAN_POINT('Ctrl Pts',(-22.1874053203775,27.2413983928989,-23.728812336003));
#65299=CARTESIAN_POINT('Ctrl Pts',(-22.0799547837233,27.1980893608728,-23.7346770229412));
#65300=CARTESIAN_POINT('Ctrl Pts',(-21.9726147532193,27.1548248694748,-23.740535678416));
#65301=CARTESIAN_POINT('Ctrl Pts',(-21.8670707905509,27.1067721060629,-23.7463943338908));
#65302=CARTESIAN_POINT('Ctrl Pts',(-21.7637769748103,27.0541067074065,-23.7522529893657));
#65303=CARTESIAN_POINT('Ctrl Pts',(-21.656448411647,26.9993841518915,-23.7583404890836));
#65304=CARTESIAN_POINT('Ctrl Pts',(-21.5515497994855,26.9396814000109,-23.7644279888015));
#65305=CARTESIAN_POINT('Ctrl Pts',(-21.4495677345764,26.8752506344242,-23.7705154885194));
#65306=CARTESIAN_POINT('Ctrl Pts',(-21.35153310257,26.8133137987677,-23.7763673586028));
#65307=CARTESIAN_POINT('Ctrl Pts',(-21.2561938157888,26.7470084006965,-23.7822192286862));
#65308=CARTESIAN_POINT('Ctrl Pts',(-21.1639560620088,26.6766047445402,-23.7880710987696));
#65309=CARTESIAN_POINT('Ctrl Pts',(-21.0717323522655,26.6062118079806,-23.7939220778525));
#65310=CARTESIAN_POINT('Ctrl Pts',(-20.9826095650749,26.5317221047876,-23.7997730569355));
#65311=CARTESIAN_POINT('Ctrl Pts',(-20.896962864663,26.4534478304686,-23.8056240360185));
#65312=CARTESIAN_POINT('Ctrl Pts',(-20.8113084637884,26.3751665185388,-23.8114755411608));
#65313=CARTESIAN_POINT('Ctrl Pts',(-20.7291310761429,26.2931002379528,-23.8173270463031));
#65314=CARTESIAN_POINT('Ctrl Pts',(-20.6507703490071,26.2075993423834,-23.8231785514454));
#65315=CARTESIAN_POINT('Ctrl Pts',(-20.5723835999794,26.1220700538275,-23.8290319997452));
#65316=CARTESIAN_POINT('Ctrl Pts',(-20.497816310822,26.033104186947,-23.834885448045));
#65317=CARTESIAN_POINT('Ctrl Pts',(-20.4273685779228,25.9410860288824,-23.8407388963448));
#65318=CARTESIAN_POINT('Ctrl Pts',(-20.3568407306543,25.8489632261913,-23.8465990012864));
#65319=CARTESIAN_POINT('Ctrl Pts',(-20.2904420418637,25.753781532499,-23.8524591062279));
#65320=CARTESIAN_POINT('Ctrl Pts',(-20.2284299580411,25.6559552146883,-23.8583192111694));
#65321=CARTESIAN_POINT('Ctrl Pts',(-20.1663761129612,25.5580630169754,-23.8641832625249));
#65322=CARTESIAN_POINT('Ctrl Pts',(-20.1087149602132,25.4575230065598,-23.8700473138803));
#65323=CARTESIAN_POINT('Ctrl Pts',(-20.0556577230711,25.3547735549977,-23.8759113652358));
#65324=CARTESIAN_POINT('Ctrl Pts',(-20.0025222901525,25.2518726712544,-23.8817840590324));
#65325=CARTESIAN_POINT('Ctrl Pts',(-19.9540044874834,25.1467562213898,-23.887656752829));
#65326=CARTESIAN_POINT('Ctrl Pts',(-19.9102672571527,25.0398820833349,-23.8935294466255));
#65327=CARTESIAN_POINT('Ctrl Pts',(-19.8982927351231,25.0106217321225,-23.8951372919488));
#65328=CARTESIAN_POINT('Ctrl Pts',(-19.8866762617299,24.9812297116053,-23.8967451372721));
#65329=CARTESIAN_POINT('Ctrl Pts',(-19.8754205211404,24.9517155865797,-23.8983529825954));
#65330=CARTESIAN_POINT('Ctrl Pts',(-19.8343114353426,24.8439218178553,-23.9042252795641));
#65331=CARTESIAN_POINT('Ctrl Pts',(-19.7978803703453,24.7341371539342,-23.9100975765328));
#65332=CARTESIAN_POINT('Ctrl Pts',(-19.7663233999043,24.6228052462924,-23.9159698735015));
#65333=CARTESIAN_POINT('Ctrl Pts',(-19.7348073247909,24.5116176159614,-23.9218345604396));
#65334=CARTESIAN_POINT('Ctrl Pts',(-19.7081528947946,24.3988871233872,-23.9276992473778));
#65335=CARTESIAN_POINT('Ctrl Pts',(-19.6865079398746,24.2850768162582,-23.933563934316));
#65336=CARTESIAN_POINT('Ctrl Pts',(-19.6648852454358,24.1713835559055,-23.9394225897908));
#65337=CARTESIAN_POINT('Ctrl Pts',(-19.648261855387,24.0566130935448,-23.9452812452656));
#65338=CARTESIAN_POINT('Ctrl Pts',(-19.6367354525663,23.941242392655,-23.9511399007404));
#65339=CARTESIAN_POINT('Ctrl Pts',(-19.624758818299,23.8213652105709,-23.9572274004583));
#65340=CARTESIAN_POINT('Ctrl Pts',(-19.6182855983226,23.7008403797738,-23.9633149001762));
#65341=CARTESIAN_POINT('Ctrl Pts',(-19.617366653036,23.580213597272,-23.9694023998941));
#65342=CARTESIAN_POINT('Ctrl Pts',(-19.6164832774827,23.4642559311546,-23.9752542699775));
#65343=CARTESIAN_POINT('Ctrl Pts',(-19.6207321951438,23.3482045110168,-23.9811061400609));
#65344=CARTESIAN_POINT('Ctrl Pts',(-19.630105556164,23.2325471803988,-23.9869580101443));
#65345=CARTESIAN_POINT('Ctrl Pts',(-19.6394774900048,23.116907459661,-23.9928089892272));
#65346=CARTESIAN_POINT('Ctrl Pts',(-19.6539722824479,23.0016621210552,-23.9986599683102));
#65347=CARTESIAN_POINT('Ctrl Pts',(-19.6735300703436,22.887295551446,-24.0045109473932));
#65348=CARTESIAN_POINT('Ctrl Pts',(-19.6930896166726,22.7729186991816,-24.0103624525354));
#65349=CARTESIAN_POINT('Ctrl Pts',(-19.7177129936886,22.65942118047,-24.0162139576777));
#65350=CARTESIAN_POINT('Ctrl Pts',(-19.7472890367221,22.54727812728,-24.02206546282));
#65351=CARTESIAN_POINT('Ctrl Pts',(-19.7768749013158,22.4350978338231,-24.0279189111198));
#65352=CARTESIAN_POINT('Ctrl Pts',(-19.8114165968919,22.3242732997676,-24.0337723594195));
#65353=CARTESIAN_POINT('Ctrl Pts',(-19.8507530310512,22.2152647247302,-24.0396258077193));
#65354=CARTESIAN_POINT('Ctrl Pts',(-19.8901341992779,22.1061321832724,-24.0454859126608));
#65355=CARTESIAN_POINT('Ctrl Pts',(-19.9343208490314,21.9988201118604,-24.0513460176024));
#65356=CARTESIAN_POINT('Ctrl Pts',(-19.9831036113743,21.8937690333578,-24.0572061225439));
#65357=CARTESIAN_POINT('Ctrl Pts',(-20.0319192258544,21.788647209529,-24.0630701738993));
#65358=CARTESIAN_POINT('Ctrl Pts',(-20.0853369260118,21.6857897764459,-24.0689342252548));
#65359=CARTESIAN_POINT('Ctrl Pts',(-20.1431020776351,21.5856113982032,-24.0747982766102));
#65360=CARTESIAN_POINT('Ctrl Pts',(-20.2009523635608,21.4852853770285,-24.0806709704068));
#65361=CARTESIAN_POINT('Ctrl Pts',(-20.2631626673428,21.3876466382453,-24.0865436642033));
#65362=CARTESIAN_POINT('Ctrl Pts',(-20.3294358457019,21.2930797701994,-24.0924163579999));
#65363=CARTESIAN_POINT('Ctrl Pts',(-20.3475803333228,21.2671889436375,-24.0940242033233));
#65364=CARTESIAN_POINT('Ctrl Pts',(-20.3660291370058,21.2415281765597,-24.0956320486467));
#65365=CARTESIAN_POINT('Ctrl Pts',(-20.3847756606335,21.216104897379,-24.0972398939701));
#65366=CARTESIAN_POINT('Ctrl Pts',(-20.4532431632402,21.1232520320611,-24.1031121909388));
#65367=CARTESIAN_POINT('Ctrl Pts',(-20.5259143079376,21.0332587008779,-24.1089844879075));
#65368=CARTESIAN_POINT('Ctrl Pts',(-20.6025218294725,20.9465296764003,-24.1148567848762));
#65369=CARTESIAN_POINT('Ctrl Pts',(-20.6790300737437,20.8599130458505,-24.1207214718144));
#65370=CARTESIAN_POINT('Ctrl Pts',(-20.7594642791921,20.7765526164585,-24.1265861587526));
#65371=CARTESIAN_POINT('Ctrl Pts',(-20.8435147843884,20.6968230569551,-24.1324508456908));
#65372=CARTESIAN_POINT('Ctrl Pts',(-20.9274788489016,20.6171754943126,-24.1383095011656));
#65373=CARTESIAN_POINT('Ctrl Pts',(-21.015051517496,20.5411516569819,-24.1441681566405));
#65374=CARTESIAN_POINT('Ctrl Pts',(-21.1058843145094,20.4690915461537,-24.1500268121153));
#65375=CARTESIAN_POINT('Ctrl Pts',(-21.2002651205788,20.3942167039267,-24.1561143118332));
#65376=CARTESIAN_POINT('Ctrl Pts',(-21.2981656331073,20.3236218948951,-24.1622018115511));
#65377=CARTESIAN_POINT('Ctrl Pts',(-21.3991542402479,20.2576448811326,-24.168289311269));
#65378=CARTESIAN_POINT('Ctrl Pts',(-21.4962338683834,20.1942216481273,-24.1741411813524));
#65379=CARTESIAN_POINT('Ctrl Pts',(-21.596166595405,20.1350656214916,-24.1799930514358));
#65380=CARTESIAN_POINT('Ctrl Pts',(-21.6985377471777,20.0804338971251,-24.1858449215192));
#65381=CARTESIAN_POINT('Ctrl Pts',(-21.800893312012,20.0258104909352,-24.1916959006022));
#65382=CARTESIAN_POINT('Ctrl Pts',(-21.9056861987896,19.9757102119016,-24.1975468796851));
#65383=CARTESIAN_POINT('Ctrl Pts',(-22.0124765261438,19.9303445277867,-24.2033978587681));
#65384=CARTESIAN_POINT('Ctrl Pts',(-22.1192764549758,19.8849747648604,-24.2092493639104));
#65385=CARTESIAN_POINT('Ctrl Pts',(-22.2280738008934,19.8443406047161,-24.2151008690527));
#65386=CARTESIAN_POINT('Ctrl Pts',(-22.3384087381831,19.8086053516238,-24.220952374195));
#65387=CARTESIAN_POINT('Ctrl Pts',(-22.4487803153041,19.7728582316317,-24.2268058224948));
#65388=CARTESIAN_POINT('Ctrl Pts',(-22.560690106032,19.7420133808265,-24.2326592707945));
#65389=CARTESIAN_POINT('Ctrl Pts',(-22.6736638594369,19.7161840268719,-24.2385127190943));
#65390=CARTESIAN_POINT('Ctrl Pts',(-22.786766088531,19.6903252993332,-24.2443728240359));
#65391=CARTESIAN_POINT('Ctrl Pts',(-22.9009342921154,19.6694935452655,-24.2502329289774));
#65392=CARTESIAN_POINT('Ctrl Pts',(-23.0156846781272,19.653750740352,-24.2560930339189));
#65393=CARTESIAN_POINT('Ctrl Pts',(-23.1305123413419,19.6379973336447,-24.2619570852744));
#65394=CARTESIAN_POINT('Ctrl Pts',(-23.2459225570346,19.627339738025,-24.2678211366298));
#65395=CARTESIAN_POINT('Ctrl Pts',(-23.361428820759,19.6217878689807,-24.2736851879853));
#65396=CARTESIAN_POINT('Ctrl Pts',(-23.4771053176591,19.6162278175896,-24.2795578817819));
#65397=CARTESIAN_POINT('Ctrl Pts',(-23.5928777332809,19.6157885124291,-24.2854305755784));
#65398=CARTESIAN_POINT('Ctrl Pts',(-23.7082618884572,19.6204278481777,-24.291303269375));
#65399=CARTESIAN_POINT('Ctrl Pts',(-23.7398521400037,19.6216980206991,-24.2929111146984));
#65400=CARTESIAN_POINT('Ctrl Pts',(-23.7714133343787,19.6233485763334,-24.2945189600217));
#65401=CARTESIAN_POINT('Ctrl Pts',(-23.8029356564525,19.6253779810286,-24.2961268053451));
#65402=CARTESIAN_POINT('Ctrl Pts',(-23.9180639176554,19.6327899297198,-24.3019991023138));
#65403=CARTESIAN_POINT('Ctrl Pts',(-24.0330586515679,19.6452841724555,-24.3078713992825));
#65404=CARTESIAN_POINT('Ctrl Pts',(-24.1474348480352,19.6628546512284,-24.3137436962512));
#65405=CARTESIAN_POINT('Ctrl Pts',(-24.2616628220351,19.6804023600562,-24.3196083831894));
#65406=CARTESIAN_POINT('Ctrl Pts',(-24.3752734478172,19.7030131606592,-24.3254730701276));
#65407=CARTESIAN_POINT('Ctrl Pts',(-24.487784125162,19.7306290540135,-24.3313377570658));
#65408=CARTESIAN_POINT('Ctrl Pts',(-24.6001790923184,19.7582165461502,-24.3371964125406));
#65409=CARTESIAN_POINT('Ctrl Pts',(-24.7114759620557,19.7907987945982,-24.3430550680155));
#65410=CARTESIAN_POINT('Ctrl Pts',(-24.8212003197991,19.8282664059931,-24.3489137234903));
#65411=CARTESIAN_POINT('Ctrl Pts',(-24.9352106076,19.8671975352902,-24.3550012232082));
#65412=CARTESIAN_POINT('Ctrl Pts',(-25.0475225822143,19.9114033920715,-24.3610887229261));
#65413=CARTESIAN_POINT('Ctrl Pts',(-25.1576187742416,19.9607034287679,-24.367176222644));
#65414=CARTESIAN_POINT('Ctrl Pts',(-25.2634534588044,20.0080952026033,-24.3730280927274));
#65415=CARTESIAN_POINT('Ctrl Pts',(-25.3672402919517,20.060193942344,-24.3788799628108));
#65416=CARTESIAN_POINT('Ctrl Pts',(-25.4685388256401,20.1167897469157,-24.3847318328942));
#65417=CARTESIAN_POINT('Ctrl Pts',(-25.5698219357058,20.1733769342615,-24.3905828119771));
#65418=CARTESIAN_POINT('Ctrl Pts',(-25.6686171388405,20.2344596234291,-24.3964337910601));
#65419=CARTESIAN_POINT('Ctrl Pts',(-25.7645087491411,20.2997820421346,-24.4022847701431));
#65420=CARTESIAN_POINT('Ctrl Pts',(-25.8604089810202,20.3651103339542,-24.4081362752854));
#65421=CARTESIAN_POINT('Ctrl Pts',(-25.953404759435,20.4346788803412,-24.4139877804276));
#65422=CARTESIAN_POINT('Ctrl Pts',(-26.0431101384716,20.5081890950887,-24.4198392855699));
#65423=CARTESIAN_POINT('Ctrl Pts',(-26.1328453067121,20.5817237209785,-24.4256927338697));
#65424=CARTESIAN_POINT('Ctrl Pts',(-26.2192875832983,20.6592023561018,-24.4315461821695));
#65425=CARTESIAN_POINT('Ctrl Pts',(-26.3020853551643,20.7402872095466,-24.4373996304693));
#65426=CARTESIAN_POINT('Ctrl Pts',(-26.3849772860759,20.8214642740766,-24.4432597354108));
#65427=CARTESIAN_POINT('Ctrl Pts',(-26.4642161442643,20.9062554531002,-24.4491198403524));
#65428=CARTESIAN_POINT('Ctrl Pts',(-26.5394882784282,20.9942872247216,-24.4549799452939));
#65429=CARTESIAN_POINT('Ctrl Pts',(-26.6148111036633,21.0823782802315,-24.4608439966494));
#65430=CARTESIAN_POINT('Ctrl Pts',(-26.6861616318421,21.1737139488348,-24.4667080480048));
#65431=CARTESIAN_POINT('Ctrl Pts',(-26.7532685446208,21.26789028592,-24.4725720993603));
#65432=CARTESIAN_POINT('Ctrl Pts',(-26.8204743595932,21.3622054201265,-24.4784447931568));
#65433=CARTESIAN_POINT('Ctrl Pts',(-26.88342385298,21.4593692327844,-24.4843174869534));
#65434=CARTESIAN_POINT('Ctrl Pts',(-26.9418907293289,21.5589516161254,-24.49019018075));
#65435=CARTESIAN_POINT('Ctrl Pts',(-26.9578979820419,21.5862156068744,-24.4917980260733));
#65436=CARTESIAN_POINT('Ctrl Pts',(-26.9735695054268,21.6136607645356,-24.4934058713966));
#65437=CARTESIAN_POINT('Ctrl Pts',(-26.9889012846137,21.6412780022556,-24.49501371672));
#65438=CARTESIAN_POINT('Ctrl Pts',(-27.0476041889497,21.7470199415403,-24.501169896577));
#65439=CARTESIAN_POINT('Ctrl Pts',(-27.1015037032677,21.8556120215365,-24.5073260764341));
#65440=CARTESIAN_POINT('Ctrl Pts',(-27.1503271994092,21.966601248464,-24.5134822562911));
#65441=CARTESIAN_POINT('Ctrl Pts',(-27.1990638964661,22.0773931572136,-24.5196274916067));
#65442=CARTESIAN_POINT('Ctrl Pts',(-27.2427424068359,22.1905734009645,-24.5257727269224));
#65443=CARTESIAN_POINT('Ctrl Pts',(-27.2811355030515,22.3056637425608,-24.531917962238));
#65444=CARTESIAN_POINT('Ctrl Pts',(-27.3194415615513,22.4204931726542,-24.5380492662145));
#65445=CARTESIAN_POINT('Ctrl Pts',(-27.3524859794983,22.537223732537,-24.5441805701909));
#65446=CARTESIAN_POINT('Ctrl Pts',(-27.3800895822657,22.655357473003,-24.5503118741674));
#65447=CARTESIAN_POINT('Ctrl Pts',(-27.4076555417525,22.773330113428,-24.5564348168297));
#65448=CARTESIAN_POINT('Ctrl Pts',(-27.4297953798824,22.8927017794769,-24.5625577594919));
#65449=CARTESIAN_POINT('Ctrl Pts',(-27.446379339963,23.0129584838122,-24.5686807021542));
#65450=CARTESIAN_POINT('Ctrl Pts',(-27.4629352965204,23.1330121237777,-24.5747933056715));
#65451=CARTESIAN_POINT('Ctrl Pts',(-27.4739540263127,23.253947471905,-24.5809059091889));
#65452=CARTESIAN_POINT('Ctrl Pts',(-27.4793567136677,23.3752401687067,-24.5870185127062));
#65453=CARTESIAN_POINT('Ctrl Pts',(-27.4819546633665,23.4335652770136,-24.5899578344592));
#65454=CARTESIAN_POINT('Ctrl Pts',(-27.4832547774517,23.4919728544158,-24.5928971562121));
#65455=CARTESIAN_POINT('Ctrl Pts',(-27.4832525287818,23.5504038899366,-24.5958364779651));
#65456=CARTESIAN_POINT('',(-27.4832509217898,23.5538111136364,-25.8458364779651));
#65457=CARTESIAN_POINT('Ctrl Pts',(-27.4832525287817,23.5504038905352,-24.5958364779952));
#65458=CARTESIAN_POINT('Ctrl Pts',(-27.4832478259376,23.6726054471124,-24.6019837196159));
#65459=CARTESIAN_POINT('Ctrl Pts',(-27.4775434726152,23.794689959441,-24.6081309612367));
#65460=CARTESIAN_POINT('Ctrl Pts',(-27.4661978260355,23.9161233445858,-24.6142782028574));
#65461=CARTESIAN_POINT('Ctrl Pts',(-27.4548350958917,24.0377395765178,-24.6204347006096));
#65462=CARTESIAN_POINT('Ctrl Pts',(-27.4378141573329,24.1587023794636,-24.6265911983618));
#65463=CARTESIAN_POINT('Ctrl Pts',(-27.415244682518,24.2784864735495,-24.632747696114));
#65464=CARTESIAN_POINT('Ctrl Pts',(-27.3926182231349,24.3985730046634,-24.6389197381077));
#65465=CARTESIAN_POINT('Ctrl Pts',(-27.3644152868304,24.5174745349927,-24.6450917801014));
#65466=CARTESIAN_POINT('Ctrl Pts',(-27.3307961618426,24.6346781218313,-24.651263822095));
#65467=CARTESIAN_POINT('Ctrl Pts',(-27.2971300334542,24.7520455727547,-24.6574444933128));
#65468=CARTESIAN_POINT('Ctrl Pts',(-27.2580327171207,24.8677100144452,-24.6636251645305));
#65469=CARTESIAN_POINT('Ctrl Pts',(-27.2137129937155,24.9811775622975,-24.6698058357483));
#65470=CARTESIAN_POINT('Ctrl Pts',(-27.1692929457998,25.0949019613957,-24.6760004978659));
#65471=CARTESIAN_POINT('Ctrl Pts',(-27.1196270025272,25.2064192089251,-24.6821951599836));
#65472=CARTESIAN_POINT('Ctrl Pts',(-27.0649708348363,25.3152579848183,-24.6883898221012));
#65473=CARTESIAN_POINT('Ctrl Pts',(-27.048763357561,25.3475325123143,-24.6902267574324));
#65474=CARTESIAN_POINT('Ctrl Pts',(-27.0321173672469,25.3795717027539,-24.6920636927636));
#65475=CARTESIAN_POINT('Ctrl Pts',(-27.0150402581779,25.4113637616877,-24.6939006280948));
#65476=CARTESIAN_POINT('Ctrl Pts',(-26.960448322296,25.5129963059227,-24.6997729250635));
#65477=CARTESIAN_POINT('Ctrl Pts',(-26.901289360933,25.6123950595346,-24.7056452220323));
#65478=CARTESIAN_POINT('Ctrl Pts',(-26.8377704677816,25.7091214068008,-24.711517519001));
#65479=CARTESIAN_POINT('Ctrl Pts',(-26.7743338900711,25.8057224044027,-24.7173822059392));
#65480=CARTESIAN_POINT('Ctrl Pts',(-26.7065488414596,25.8996575404238,-24.7232468928774));
#65481=CARTESIAN_POINT('Ctrl Pts',(-26.6346686561638,25.990511979194,-24.7291115798156));
#65482=CARTESIAN_POINT('Ctrl Pts',(-26.5628623951388,26.0812729798615,-24.7349702352904));
#65483=CARTESIAN_POINT('Ctrl Pts',(-26.4869696294465,26.1689592629559,-24.7408288907653));
#65484=CARTESIAN_POINT('Ctrl Pts',(-26.4072870360614,26.2531847988543,-24.7466875462401));
#65485=CARTESIAN_POINT('Ctrl Pts',(-26.3244919703955,26.3407002583695,-24.752775045958));
#65486=CARTESIAN_POINT('Ctrl Pts',(-26.2376052229308,26.4244787193873,-24.7588625456759));
#65487=CARTESIAN_POINT('Ctrl Pts',(-26.1470060826493,26.5041245660928,-24.7649500453938));
#65488=CARTESIAN_POINT('Ctrl Pts',(-26.0599137749427,26.5806875507666,-24.7708019154772));
#65489=CARTESIAN_POINT('Ctrl Pts',(-25.9693914621539,26.6534315972908,-24.7766537855606));
#65490=CARTESIAN_POINT('Ctrl Pts',(-25.8758131190781,26.7220433435868,-24.782505655644));
#65491=CARTESIAN_POINT('Ctrl Pts',(-25.782249024156,26.7906446431206,-24.788356634727));
#65492=CARTESIAN_POINT('Ctrl Pts',(-25.6856301574126,26.8551146490741,-24.79420761381));
#65493=CARTESIAN_POINT('Ctrl Pts',(-25.5863619232682,26.9151815867478,-24.800058592893));
#65494=CARTESIAN_POINT('Ctrl Pts',(-25.4870847639543,26.9752539250172,-24.8059100980353));
#65495=CARTESIAN_POINT('Ctrl Pts',(-25.3851581174088,27.0309221940169,-24.8117616031776));
#65496=CARTESIAN_POINT('Ctrl Pts',(-25.2810139680362,27.0819594632602,-24.8176131083199));
#65497=CARTESIAN_POINT('Ctrl Pts',(-25.1768352346587,27.1330136808696,-24.8234665566197));
#65498=CARTESIAN_POINT('Ctrl Pts',(-25.070437905208,27.1794336589788,-24.8293200049194));
#65499=CARTESIAN_POINT('Ctrl Pts',(-24.9622753524433,27.2210399885873,-24.8351734532192));
#65500=CARTESIAN_POINT('Ctrl Pts',(-24.853989795369,27.2626936336272,-24.8410335581608));
#65501=CARTESIAN_POINT('Ctrl Pts',(-24.7439353942383,27.2995225554008,-24.8468936631023));
#65502=CARTESIAN_POINT('Ctrl Pts',(-24.6325822424161,27.3313967232437,-24.8527537680438));
#65503=CARTESIAN_POINT('Ctrl Pts',(-24.5211541012155,27.3632923563437,-24.8586178193993));
#65504=CARTESIAN_POINT('Ctrl Pts',(-24.4084258688501,27.3902264956169,-24.8644818707548));
#65505=CARTESIAN_POINT('Ctrl Pts',(-24.2948777144468,27.4121202582238,-24.8703459221102));
#65506=CARTESIAN_POINT('Ctrl Pts',(-24.1811622127302,27.4340462878663,-24.8762186159068));
#65507=CARTESIAN_POINT('Ctrl Pts',(-24.0666247846745,27.4509170549587,-24.8820913097034));
#65508=CARTESIAN_POINT('Ctrl Pts',(-23.9517506829399,27.4627055006826,-24.8879640034999));
#65509=CARTESIAN_POINT('Ctrl Pts',(-23.920300075495,27.4659329799251,-24.8895718488232));
#65510=CARTESIAN_POINT('Ctrl Pts',(-23.8888242289008,27.4687798036578,-24.8911796941465));
#65511=CARTESIAN_POINT('Ctrl Pts',(-23.8573330766582,27.4712460969662,-24.8927875394698));
#65512=CARTESIAN_POINT('Ctrl Pts',(-23.7423186563169,27.4802536840202,-24.8986598364385));
#65513=CARTESIAN_POINT('Ctrl Pts',(-23.6267148906233,27.4842114973813,-24.9045321334072));
#65514=CARTESIAN_POINT('Ctrl Pts',(-23.5110027372644,27.4830566780556,-24.9104044303759));
#65515=CARTESIAN_POINT('Ctrl Pts',(-23.3954405376666,27.481903355284,-24.9162691173141));
#65516=CARTESIAN_POINT('Ctrl Pts',(-23.2797706392785,27.4756505797853,-24.9221338042523));
#65517=CARTESIAN_POINT('Ctrl Pts',(-23.1644789881933,27.4642872496208,-24.9279984911906));
#65518=CARTESIAN_POINT('Ctrl Pts',(-23.0493059073539,27.45293560593,-24.9338571466654));
#65519=CARTESIAN_POINT('Ctrl Pts',(-22.9345107089853,27.4364839021035,-24.9397158021402));
#65520=CARTESIAN_POINT('Ctrl Pts',(-22.8205785327678,27.4149730720814,-24.945574457615));
#65521=CARTESIAN_POINT('Ctrl Pts',(-22.7021960653973,27.3926220100922,-24.9516619573329));
#65522=CARTESIAN_POINT('Ctrl Pts',(-22.5847458700919,27.3648085414441,-24.9577494570508));
#65523=CARTESIAN_POINT('Ctrl Pts',(-22.4687658068485,27.3316379212019,-24.9638369567687));
#65524=CARTESIAN_POINT('Ctrl Pts',(-22.3572749988294,27.2997512404236,-24.9696888268521));
#65525=CARTESIAN_POINT('Ctrl Pts',(-22.2471430643954,27.262914540854,-24.9755406969355));
#65526=CARTESIAN_POINT('Ctrl Pts',(-22.1388357895518,27.2212730682753,-24.9813925670189));
#65527=CARTESIAN_POINT('Ctrl Pts',(-22.0305450054756,27.1796379359894,-24.9872435461019));
#65528=CARTESIAN_POINT('Ctrl Pts',(-21.9240787143339,27.1331996335984,-24.9930945251849));
#65529=CARTESIAN_POINT('Ctrl Pts',(-21.8198847030169,27.0821523288967,-24.9989455042679));
#65530=CARTESIAN_POINT('Ctrl Pts',(-21.7156813236557,27.031100434551,-25.0047970094102));
#65531=CARTESIAN_POINT('Ctrl Pts',(-21.6137510014951,26.9754388960015,-25.0106485145525));
#65532=CARTESIAN_POINT('Ctrl Pts',(-21.5145181628449,26.9154084834275,-25.0165000196948));
#65533=CARTESIAN_POINT('Ctrl Pts',(-21.4152523711293,26.8553581360602,-25.0223534679945));
#65534=CARTESIAN_POINT('Ctrl Pts',(-21.3186861976289,26.7909362436832,-25.0282069162943));
#65535=CARTESIAN_POINT('Ctrl Pts',(-21.2252156493426,26.7224272582351,-25.0340603645941));
#65536=CARTESIAN_POINT('Ctrl Pts',(-21.131638804746,26.653840363194,-25.0399204695356));
#65537=CARTESIAN_POINT('Ctrl Pts',(-21.0411649455847,26.5811573425102,-25.0457805744772));
#65538=CARTESIAN_POINT('Ctrl Pts',(-20.9541575742307,26.5047034065325,-25.0516406794187));
#65539=CARTESIAN_POINT('Ctrl Pts',(-20.8670916088577,26.4281979836139,-25.0575047307742));
#65540=CARTESIAN_POINT('Ctrl Pts',(-20.7834970770969,26.347916874439,-25.0633687821296));
#65541=CARTESIAN_POINT('Ctrl Pts',(-20.7036998961738,26.264221413832,-25.0692328334851));
#65542=CARTESIAN_POINT('Ctrl Pts',(-20.6237851101352,26.1804026028232,-25.0751055272817));
#65543=CARTESIAN_POINT('Ctrl Pts',(-20.5476791152681,26.0931597076787,-25.0809782210782));
#65544=CARTESIAN_POINT('Ctrl Pts',(-20.4756669762447,26.0028863531648,-25.0868509148748));
#65545=CARTESIAN_POINT('Ctrl Pts',(-20.4559512571966,25.9781710187883,-25.0884587601981));
#65546=CARTESIAN_POINT('Ctrl Pts',(-20.4365421471854,25.9532286898519,-25.0900666055214));
#65547=CARTESIAN_POINT('Ctrl Pts',(-20.417444910453,25.9280677911904,-25.0916744508447));
#65548=CARTESIAN_POINT('Ctrl Pts',(-20.3476965063314,25.8361732122785,-25.0975467478134));
#65549=CARTESIAN_POINT('Ctrl Pts',(-20.2818779953968,25.7410531904775,-25.1034190447821));
#65550=CARTESIAN_POINT('Ctrl Pts',(-20.2203022399947,25.6430783856081,-25.1092913417508));
#65551=CARTESIAN_POINT('Ctrl Pts',(-20.1588062818814,25.5452305483048,-25.115156028689));
#65552=CARTESIAN_POINT('Ctrl Pts',(-20.1015423631453,25.4445356318221,-25.1210207156272));
#65553=CARTESIAN_POINT('Ctrl Pts',(-20.0487824984981,25.3413964696929,-25.1268854025653));
#65554=CARTESIAN_POINT('Ctrl Pts',(-19.9960768940688,25.2383633797354,-25.1327440580401));
#65555=CARTESIAN_POINT('Ctrl Pts',(-19.9478663172968,25.1328914099305,-25.138602713515));
#65556=CARTESIAN_POINT('Ctrl Pts',(-19.9043785683351,25.0254108429612,-25.1444613689898));
#65557=CARTESIAN_POINT('Ctrl Pts',(-19.8591921495953,24.9137319903781,-25.1505488687077));
#65558=CARTESIAN_POINT('Ctrl Pts',(-19.8191052778004,24.7998848115582,-25.1566363684256));
#65559=CARTESIAN_POINT('Ctrl Pts',(-19.784320136228,24.6843787119661,-25.1627238681435));
#65560=CARTESIAN_POINT('Ctrl Pts',(-19.7508814276043,24.5733435218266,-25.1685757382269));
#65561=CARTESIAN_POINT('Ctrl Pts',(-19.7223417816217,24.460775879831,-25.1744276083103));
#65562=CARTESIAN_POINT('Ctrl Pts',(-19.6988307776489,24.347146171063,-25.1802794783937));
#65563=CARTESIAN_POINT('Ctrl Pts',(-19.6753233534402,24.2335337634515,-25.1861304574766));
#65564=CARTESIAN_POINT('Ctrl Pts',(-19.6568431326065,24.118860015295,-25.1919814365596));
#65565=CARTESIAN_POINT('Ctrl Pts',(-19.6434688063217,24.0036066131414,-25.1978324156425));
#65566=CARTESIAN_POINT('Ctrl Pts',(-19.6300932775564,23.8883428485979,-25.2036839207848));
#65567=CARTESIAN_POINT('Ctrl Pts',(-19.6218246035801,23.7724997371064,-25.2095354259271));
#65568=CARTESIAN_POINT('Ctrl Pts',(-19.6186896408146,23.6565645021312,-25.2153869310694));
#65569=CARTESIAN_POINT('Ctrl Pts',(-19.6155536369961,23.5405907675882,-25.2212403793691));
#65570=CARTESIAN_POINT('Ctrl Pts',(-19.6175547454316,23.424525261744,-25.2270938276689));
#65571=CARTESIAN_POINT('Ctrl Pts',(-19.624667710503,23.3088549102624,-25.2329472759687));
#65572=CARTESIAN_POINT('Ctrl Pts',(-19.6317887645602,23.1930530164737,-25.2388073809102));
#65573=CARTESIAN_POINT('Ctrl Pts',(-19.6440332530191,23.0776475868375,-25.2446674858517));
#65574=CARTESIAN_POINT('Ctrl Pts',(-19.6613240593988,22.9631202319782,-25.2505275907932));
#65575=CARTESIAN_POINT('Ctrl Pts',(-19.6786265100544,22.8485157501134,-25.2563916421487));
#65576=CARTESIAN_POINT('Ctrl Pts',(-19.7009819659387,22.7347909251069,-25.2622556935041));
#65577=CARTESIAN_POINT('Ctrl Pts',(-19.7282626020786,22.6224152733793,-25.2681197448595));
#65578=CARTESIAN_POINT('Ctrl Pts',(-19.7555834444305,22.5098740023734,-25.2739924386561));
#65579=CARTESIAN_POINT('Ctrl Pts',(-19.7878438393103,22.3986862686524,-25.2798651324526));
#65580=CARTESIAN_POINT('Ctrl Pts',(-19.8248667131377,22.2893046727808,-25.2857378262492));
#65581=CARTESIAN_POINT('Ctrl Pts',(-19.8350029566753,22.2593578215597,-25.2873456715727));
#65582=CARTESIAN_POINT('Ctrl Pts',(-19.8454959097274,22.2295462254831,-25.2889535168961));
#65583=CARTESIAN_POINT('Ctrl Pts',(-19.8563413298849,22.1998788674265,-25.2905613622195));
#65584=CARTESIAN_POINT('Ctrl Pts',(-19.895951811681,22.0915254491932,-25.2964336591882));
#65585=CARTESIAN_POINT('Ctrl Pts',(-19.9404001865646,21.9847348274171,-25.302305956157));
#65586=CARTESIAN_POINT('Ctrl Pts',(-19.9895437275704,21.8799705757852,-25.3081782531257));
#65587=CARTESIAN_POINT('Ctrl Pts',(-20.03862358245,21.7753420903031,-25.3140429400639));
#65588=CARTESIAN_POINT('Ctrl Pts',(-20.0923863295045,21.6727351235627,-25.3199076270021));
#65589=CARTESIAN_POINT('Ctrl Pts',(-20.150640093607,21.5725962747065,-25.3257723139403));
#65590=CARTESIAN_POINT('Ctrl Pts',(-20.2088339473598,21.4725604123875,-25.3316309694151));
#65591=CARTESIAN_POINT('Ctrl Pts',(-20.2715094246548,21.3749879743063,-25.3374896248899));
#65592=CARTESIAN_POINT('Ctrl Pts',(-20.3384276570915,21.2803031985849,-25.3433482803647));
#65593=CARTESIAN_POINT('Ctrl Pts',(-20.407959774628,21.1819199521265,-25.3494357800826));
#65594=CARTESIAN_POINT('Ctrl Pts',(-20.482072662717,21.0866549678214,-25.3555232798005));
#65595=CARTESIAN_POINT('Ctrl Pts',(-20.560447038627,20.9949537011021,-25.3616107795185));
#65596=CARTESIAN_POINT('Ctrl Pts',(-20.6357877674888,20.9068019271077,-25.3674626496019));
#65597=CARTESIAN_POINT('Ctrl Pts',(-20.7150659248526,20.8219434615175,-25.3733145196852));
#65598=CARTESIAN_POINT('Ctrl Pts',(-20.797955810997,20.7407415847072,-25.3791663897686));
#65599=CARTESIAN_POINT('Ctrl Pts',(-20.8808330764026,20.659552071621,-25.3850173688516));
#65600=CARTESIAN_POINT('Ctrl Pts',(-20.9673206819587,20.5820183295239,-25.3908683479346));
#65601=CARTESIAN_POINT('Ctrl Pts',(-21.0570559126059,20.5084669346202,-25.3967193270176));
#65602=CARTESIAN_POINT('Ctrl Pts',(-21.1467992113139,20.4349089267383,-25.4025708321598));
#65603=CARTESIAN_POINT('Ctrl Pts',(-21.2397903958381,20.3653342398889,-25.4084223373021));
#65604=CARTESIAN_POINT('Ctrl Pts',(-21.3356340739377,20.3000288337675,-25.4142738424444));
#65605=CARTESIAN_POINT('Ctrl Pts',(-21.4315095796365,20.2347017411422,-25.4201272907442));
#65606=CARTESIAN_POINT('Ctrl Pts',(-21.5302391210217,20.1736469809691,-25.425980739044));
#65607=CARTESIAN_POINT('Ctrl Pts',(-21.6313993876304,20.1171065092366,-25.4318341873438));
#65608=CARTESIAN_POINT('Ctrl Pts',(-21.7326746954286,20.0605017387102,-25.4376942922853));
#65609=CARTESIAN_POINT('Ctrl Pts',(-21.8363858847755,20.0084217051899,-25.4435543972268));
#65610=CARTESIAN_POINT('Ctrl Pts',(-21.9420860838447,19.961061860246,-25.4494145021684));
#65611=CARTESIAN_POINT('Ctrl Pts',(-22.0478574653824,19.9136701214106,-25.4552785535238));
#65612=CARTESIAN_POINT('Ctrl Pts',(-22.1556201403844,19.871005052478,-25.4611426048793));
#65613=CARTESIAN_POINT('Ctrl Pts',(-22.2649100019915,19.833212905683,-25.4670066562347));
#65614=CARTESIAN_POINT('Ctrl Pts',(-22.3743609350382,19.7953650608077,-25.4728793500313));
#65615=CARTESIAN_POINT('Ctrl Pts',(-22.4853431520009,19.7624045886343,-25.4787520438278));
#65616=CARTESIAN_POINT('Ctrl Pts',(-22.597380156654,19.7344271639808,-25.4846247376244));
#65617=CARTESIAN_POINT('Ctrl Pts',(-22.6280540143783,19.7267674131157,-25.4862325829477));
#65618=CARTESIAN_POINT('Ctrl Pts',(-22.6588068962948,19.7194808790895,-25.4878404282711));
#65619=CARTESIAN_POINT('Ctrl Pts',(-22.6896289517575,19.7125688483173,-25.4894482735945));
#65620=CARTESIAN_POINT('Ctrl Pts',(-22.8021996451161,19.6873241952643,-25.4953205705632));
#65621=CARTESIAN_POINT('Ctrl Pts',(-22.9160706179009,19.6669945005739,-25.5011928675319));
#65622=CARTESIAN_POINT('Ctrl Pts',(-23.0307747078158,19.6517102668856,-25.5070651645006));
#65623=CARTESIAN_POINT('Ctrl Pts',(-23.1453301503398,19.6364458403504,-25.5129298514388));
#65624=CARTESIAN_POINT('Ctrl Pts',(-23.2607161569714,19.6262139261508,-25.518794538377));
#65625=CARTESIAN_POINT('Ctrl Pts',(-23.3764532797184,19.6210945022924,-25.5246592253152));
#65626=CARTESIAN_POINT('Ctrl Pts',(-23.4920713740798,19.6159803434409,-25.5305178807901));
#65627=CARTESIAN_POINT('Ctrl Pts',(-23.6080394558122,19.6159682349018,-25.5363765362649));
#65628=CARTESIAN_POINT('Ctrl Pts',(-23.7238714877685,19.6210865313715,-25.5422351917397));
#65629=CARTESIAN_POINT('Ctrl Pts',(-23.8442280209165,19.6264047530094,-25.5483226914576));
#65630=CARTESIAN_POINT('Ctrl Pts',(-23.9644372084721,19.6372624066569,-25.5544101911755));
#65631=CARTESIAN_POINT('Ctrl Pts',(-24.0839516954544,19.6536316619403,-25.5604976908934));
#65632=CARTESIAN_POINT('Ctrl Pts',(-24.1988401198184,19.6693673103542,-25.5663495609768));
#65633=CARTESIAN_POINT('Ctrl Pts',(-24.3130861755907,19.6901957562358,-25.5722014310603));
#65634=CARTESIAN_POINT('Ctrl Pts',(-24.4262081743892,19.7160393513884,-25.5780533011437));
#65635=CARTESIAN_POINT('Ctrl Pts',(-24.5393129493348,19.7418790116186,-25.5839042802266));
#65636=CARTESIAN_POINT('Ctrl Pts',(-24.6512936047144,19.7727322107913,-25.5897552593096));
#65637=CARTESIAN_POINT('Ctrl Pts',(-24.7616793236217,19.8084703189244,-25.5956062383926));
#65638=CARTESIAN_POINT('Ctrl Pts',(-24.8720749672676,19.8442116402574,-25.6014577435349));
#65639=CARTESIAN_POINT('Ctrl Pts',(-24.9808749960669,19.8848386163045,-25.6073092486772));
#65640=CARTESIAN_POINT('Ctrl Pts',(-25.0876251010621,19.9301731702775,-25.6131607538195));
#65641=CARTESIAN_POINT('Ctrl Pts',(-25.1944106554432,19.975522778869,-25.6190142021193));
#65642=CARTESIAN_POINT('Ctrl Pts',(-25.2991445521298,20.0255829123766,-25.6248676504191));
#65643=CARTESIAN_POINT('Ctrl Pts',(-25.4013944122385,20.0801282200744,-25.6307210987189));
#65644=CARTESIAN_POINT('Ctrl Pts',(-25.5037605526413,20.1347355576314,-25.6365812036604));
#65645=CARTESIAN_POINT('Ctrl Pts',(-25.603636653125,20.193838055374,-25.642441308602));
#65646=CARTESIAN_POINT('Ctrl Pts',(-25.7006167238381,20.2571654023966,-25.6483014135435));
#65647=CARTESIAN_POINT('Ctrl Pts',(-25.797662104559,20.320535396424,-25.654165464899));
#65648=CARTESIAN_POINT('Ctrl Pts',(-25.8918072371198,20.3881356645135,-25.6600295162544));
#65649=CARTESIAN_POINT('Ctrl Pts',(-25.9826782076292,20.4596548013106,-25.6658935676099));
#65650=CARTESIAN_POINT('Ctrl Pts',(-26.0736831038095,20.5312793430387,-25.6717662614065));
#65651=CARTESIAN_POINT('Ctrl Pts',(-26.1614038952065,20.6068340117535,-25.677638955203));
#65652=CARTESIAN_POINT('Ctrl Pts',(-26.2455025225805,20.6859696394806,-25.6835116489996));
#65653=CARTESIAN_POINT('Ctrl Pts',(-26.2685273199561,20.7076356505738,-25.6851194943229));
#65654=CARTESIAN_POINT('Ctrl Pts',(-26.2912808396691,20.7295698855689,-25.6867273396461));
#65655=CARTESIAN_POINT('Ctrl Pts',(-26.3137566747453,20.7517647523142,-25.6883351849694));
#65656=CARTESIAN_POINT('Ctrl Pts',(-26.3946862692477,20.8316826534574,-25.6941246147989));
#65657=CARTESIAN_POINT('Ctrl Pts',(-26.4723004131786,20.9152665873004,-25.6999140446284));
#65658=CARTESIAN_POINT('Ctrl Pts',(-26.546241312436,21.0022061770002,-25.7057034744579));
#65659=CARTESIAN_POINT('Ctrl Pts',(-26.6208137127709,21.0898882846451,-25.711542349604));
#65660=CARTESIAN_POINT('Ctrl Pts',(-26.6916494610823,21.1809833960116,-25.7173812247501));
#65661=CARTESIAN_POINT('Ctrl Pts',(-26.7584167211044,21.2751324175494,-25.7232200998963));
#65662=CARTESIAN_POINT('Ctrl Pts',(-26.824453427439,21.3682512797722,-25.7289950872662));
#65663=CARTESIAN_POINT('Ctrl Pts',(-26.8865099624587,21.4643572122828,-25.7347700746361));
#65664=CARTESIAN_POINT('Ctrl Pts',(-26.94430404516,21.5630677582168,-25.7405450620059));
#65665=CARTESIAN_POINT('Ctrl Pts',(-27.0020609439112,21.6617147950882,-25.7463163338252));
#65666=CARTESIAN_POINT('Ctrl Pts',(-27.0555606251468,21.7629627491363,-25.7520876056444));
#65667=CARTESIAN_POINT('Ctrl Pts',(-27.1045639607166,21.8664000246375,-25.7578588774636));
#65668=CARTESIAN_POINT('Ctrl Pts',(-27.1535484216892,21.9697974592405,-25.7636279263642));
#65669=CARTESIAN_POINT('Ctrl Pts',(-27.1980397978055,22.0753821543431,-25.7693969752647));
#65670=CARTESIAN_POINT('Ctrl Pts',(-27.237845209806,22.182718531994,-25.7751660241652));
#65671=CARTESIAN_POINT('Ctrl Pts',(-27.2784796739708,22.2922904713871,-25.7810552286486));
#65672=CARTESIAN_POINT('Ctrl Pts',(-27.3142306032938,22.4036874607722,-25.7869444331319));
#65673=CARTESIAN_POINT('Ctrl Pts',(-27.3449451319187,22.5164261101894,-25.7928336376152));
#65674=CARTESIAN_POINT('Ctrl Pts',(-27.3750434035268,22.6269027687224,-25.7986046809628));
#65675=CARTESIAN_POINT('Ctrl Pts',(-27.4003054201884,22.7386673181903,-25.8043757243104));
#65676=CARTESIAN_POINT('Ctrl Pts',(-27.4206385093575,22.8512522570825,-25.810146767658));
#65677=CARTESIAN_POINT('Ctrl Pts',(-27.4415960733654,22.9672949323262,-25.8160950527092));
#65678=CARTESIAN_POINT('Ctrl Pts',(-27.4573169711912,23.0842087251304,-25.8220433377603));
#65679=CARTESIAN_POINT('Ctrl Pts',(-27.4677572464468,23.2014749379599,-25.8279916228115));
#65680=CARTESIAN_POINT('Ctrl Pts',(-27.4781975217024,23.3187411507893,-25.8339399078627));
#65681=CARTESIAN_POINT('Ctrl Pts',(-27.4833571923491,23.4363592900354,-25.8398881929139));
#65682=CARTESIAN_POINT('Ctrl Pts',(-27.4832509217898,23.5538111136364,-25.8458364779651));
#65683=CARTESIAN_POINT('',(-27.4887593445795,23.5484574312381,-27.0958364779651));
#65684=CARTESIAN_POINT('Ctrl Pts',(-27.4842361821344,23.5538120051012,-25.8458364779651));
#65685=CARTESIAN_POINT('Ctrl Pts',(-27.4867683033416,23.8262759091763,-25.8596316840915));
#65686=CARTESIAN_POINT('Ctrl Pts',(-27.3365065170297,25.4053452407083,-25.9397225273423));
#65687=CARTESIAN_POINT('Ctrl Pts',(-25.2023113590138,27.898982514481,-26.0861090077196));
#65688=CARTESIAN_POINT('Ctrl Pts',(-20.7846008650191,27.2908302532138,-26.2849959190938));
#65689=CARTESIAN_POINT('Ctrl Pts',(-18.908289764109,23.2454042145606,-26.483882830469));
#65690=CARTESIAN_POINT('Ctrl Pts',(-21.297548873069,19.4801079324787,-26.6827697418437));
#65691=CARTESIAN_POINT('Ctrl Pts',(-25.7568516465323,19.4549294457212,-26.8816566532187));
#65692=CARTESIAN_POINT('Ctrl Pts',(-27.4402597520929,22.0427902655866,-27.0193455652591));
#65693=CARTESIAN_POINT('Ctrl Pts',(-27.4893282421489,23.4480765207078,-27.0907388401746));
#65694=CARTESIAN_POINT('Ctrl Pts',(-27.4887593445795,23.5484574312381,-27.0958364779651));
#65695=CARTESIAN_POINT('',(-27.4787032760536,23.5475666446788,-28.3458364779651));
#65696=CARTESIAN_POINT('Ctrl Pts',(-27.4887593445795,23.5484574312381,-27.0958364779651));
#65697=CARTESIAN_POINT('Ctrl Pts',(-27.4819296335434,24.753547150884,-27.1570344772995));
#65698=CARTESIAN_POINT('Ctrl Pts',(-26.2449208629262,27.2762265169125,-27.2845281137589));
#65699=CARTESIAN_POINT('Ctrl Pts',(-21.9474057953528,27.9173606333923,-27.4783173873434));
#65700=CARTESIAN_POINT('Ctrl Pts',(-19.0097246028294,24.5623577432724,-27.6772042987183));
#65701=CARTESIAN_POINT('Ctrl Pts',(-20.244403603648,20.2773159760852,-27.8760912100932));
#65702=CARTESIAN_POINT('Ctrl Pts',(-24.5168774795743,18.9998254042427,-28.0749781214681));
#65703=CARTESIAN_POINT('Ctrl Pts',(-27.1812473048433,21.2860900718832,-28.2315598774252));
#65704=CARTESIAN_POINT('Ctrl Pts',(-27.4816774754266,23.0720448481154,-28.3218459962577));
#65705=CARTESIAN_POINT('Ctrl Pts',(-27.4787032760536,23.5475666446788,-28.3458364779651));
#65706=CARTESIAN_POINT('',(-27.482435324374,23.5530675880075,-29.5958365176789));
#65707=CARTESIAN_POINT('Ctrl Pts',(-27.4787032760536,23.5475666446788,-28.3458364779651));
#65708=CARTESIAN_POINT('Ctrl Pts',(-27.4734585307311,24.3861085194697,-28.3881416333826));
#65709=CARTESIAN_POINT('Ctrl Pts',(-26.7990027243226,26.5464152178334,-28.4967424259252));
#65710=CARTESIAN_POINT('Ctrl Pts',(-23.2394306216868,28.1918191392488,-28.6716388555926));
#65711=CARTESIAN_POINT('Ctrl Pts',(-19.4772122483696,25.7977163651147,-28.8705257669676));
#65712=CARTESIAN_POINT('Ctrl Pts',(-19.4577725585646,21.3383848815767,-29.0694126783425));
#65713=CARTESIAN_POINT('Ctrl Pts',(-23.1989749789817,18.9115722330461,-29.2682995897174));
#65714=CARTESIAN_POINT('Ctrl Pts',(-26.7845713929707,20.531216075928,-29.4437741895916));
#65715=CARTESIAN_POINT('Ctrl Pts',(-27.4733603952322,22.703195175,-29.5529531523408));
#65716=CARTESIAN_POINT('Ctrl Pts',(-27.4789478007187,23.5530643040686,-29.5958364779651));
#65717=CARTESIAN_POINT('',(-27.484770051487,23.5518598122456,-30.8458364779651));
#65718=CARTESIAN_POINT('Ctrl Pts',(-27.4832515237015,23.5530683565611,-29.5958365269733));
#65719=CARTESIAN_POINT('Ctrl Pts',(-27.4831563204269,23.6860433818375,-29.6025389720551));
#65720=CARTESIAN_POINT('Ctrl Pts',(-27.4763132956741,23.81874838759,-29.6092414171368));
#65721=CARTESIAN_POINT('Ctrl Pts',(-27.462828282249,23.950552414495,-29.6159438622185));
#65722=CARTESIAN_POINT('Ctrl Pts',(-27.4492748427458,24.0830252455284,-29.6226803170574));
#65723=CARTESIAN_POINT('Ctrl Pts',(-27.4290119542124,24.2145877774824,-29.6294167718962));
#65724=CARTESIAN_POINT('Ctrl Pts',(-27.4021964834553,24.344618185843,-29.6361532267351));
#65725=CARTESIAN_POINT('Ctrl Pts',(-27.3752149427135,24.4754538811259,-29.6429314008844));
#65726=CARTESIAN_POINT('Ctrl Pts',(-27.3415995030298,24.6047382666682,-29.6497095750338));
#65727=CARTESIAN_POINT('Ctrl Pts',(-27.3015582735726,24.7318591629173,-29.6564877491832));
#65728=CARTESIAN_POINT('Ctrl Pts',(-27.282682898258,24.7917837621254,-29.6596829702778));
#65729=CARTESIAN_POINT('Ctrl Pts',(-27.2623802904493,24.8512279175483,-29.6628781913724));
#65730=CARTESIAN_POINT('Ctrl Pts',(-27.240675848985,24.9101292684599,-29.6660734124671));
#65731=CARTESIAN_POINT('Ctrl Pts',(-27.200786613767,25.0183803766505,-29.6719457094357));
#65732=CARTESIAN_POINT('Ctrl Pts',(-27.156063523878,25.1250562415859,-29.6778180064044));
#65733=CARTESIAN_POINT('Ctrl Pts',(-27.1066504989764,25.2296936584715,-29.683690303373));
#65734=CARTESIAN_POINT('Ctrl Pts',(-27.0573015094307,25.3341954735751,-29.6895549903112));
#65735=CARTESIAN_POINT('Ctrl Pts',(-27.0032748462921,25.4366637236064,-29.6954196772494));
#65736=CARTESIAN_POINT('Ctrl Pts',(-26.9447635335279,25.5366523047585,-29.7012843641875));
#65737=CARTESIAN_POINT('Ctrl Pts',(-26.8863123959861,25.6365380539142,-29.7071430196623));
#65738=CARTESIAN_POINT('Ctrl Pts',(-26.8233859902127,25.733948851999,-29.7130016751371));
#65739=CARTESIAN_POINT('Ctrl Pts',(-26.756224275739,25.8284610771057,-29.7188603306119));
#65740=CARTESIAN_POINT('Ctrl Pts',(-26.6864391655421,25.9266650329714,-29.7249478303298));
#65741=CARTESIAN_POINT('Ctrl Pts',(-26.6120813258812,26.0217389468308,-29.7310353300477));
#65742=CARTESIAN_POINT('Ctrl Pts',(-26.5334711849622,26.1132381865104,-29.7371228297656));
#65743=CARTESIAN_POINT('Ctrl Pts',(-26.4579038168786,26.2011957533512,-29.742974699849));
#65744=CARTESIAN_POINT('Ctrl Pts',(-26.378407509792,26.2858498883758,-29.7488265699324));
#65745=CARTESIAN_POINT('Ctrl Pts',(-26.2953088973713,26.3668381507116,-29.7546784400158));
#65746=CARTESIAN_POINT('Ctrl Pts',(-26.2122229374701,26.447814081848,-29.7605294190987));
#65747=CARTESIAN_POINT('Ctrl Pts',(-26.1255360587556,26.5251249616578,-29.7663803981817));
#65748=CARTESIAN_POINT('Ctrl Pts',(-26.0356118156413,26.59844514859,-29.7722313772646));
#65749=CARTESIAN_POINT('Ctrl Pts',(-25.9456794874721,26.6717719277126,-29.7780828824069));
#65750=CARTESIAN_POINT('Ctrl Pts',(-25.8525095366855,26.7411070394505,-29.7839343875492));
#65751=CARTESIAN_POINT('Ctrl Pts',(-25.7564980902279,26.8061655427328,-29.7897858926914));
#65752=CARTESIAN_POINT('Ctrl Pts',(-25.660454760459,26.8712456505278,-29.7956393409912));
#65753=CARTESIAN_POINT('Ctrl Pts',(-25.5615684007677,26.9320460941839,-29.8014927892909));
#65754=CARTESIAN_POINT('Ctrl Pts',(-25.4602629429715,26.9883260080487,-29.8073462375907));
#65755=CARTESIAN_POINT('Ctrl Pts',(-25.3588422788718,27.0446699243964,-29.8132063425322));
#65756=CARTESIAN_POINT('Ctrl Pts',(-25.2549973872521,27.0964828491503,-29.8190664474737));
#65757=CARTESIAN_POINT('Ctrl Pts',(-25.14917564152,27.1435704815652,-29.8249265524152));
#65758=CARTESIAN_POINT('Ctrl Pts',(-25.0432826314653,27.1906898245533,-29.8307906037707));
#65759=CARTESIAN_POINT('Ctrl Pts',(-24.9354105002458,27.2330773880195,-29.8366546551261));
#65760=CARTESIAN_POINT('Ctrl Pts',(-24.8260237296135,27.2705881147511,-29.8425187064815));
#65761=CARTESIAN_POINT('Ctrl Pts',(-24.716475744717,27.3081541248061,-29.848391400278));
#65762=CARTESIAN_POINT('Ctrl Pts',(-24.6054090603038,27.3408288370644,-29.8542640940746));
#65763=CARTESIAN_POINT('Ctrl Pts',(-24.4933004172732,27.3685178034511,-29.8601367878711));
#65764=CARTESIAN_POINT('Ctrl Pts',(-24.4626069461535,27.3760985792696,-29.8617446331948));
#65765=CARTESIAN_POINT('Ctrl Pts',(-24.4318354117046,27.3833059360893,-29.8633524785185));
#65766=CARTESIAN_POINT('Ctrl Pts',(-24.400995667851,27.3901386128537,-29.8649603238421));
#65767=CARTESIAN_POINT('Ctrl Pts',(-24.2883603716054,27.4150934430608,-29.8708326208108));
#65768=CARTESIAN_POINT('Ctrl Pts',(-24.1744374505689,27.4351299844708,-29.8767049177795));
#65769=CARTESIAN_POINT('Ctrl Pts',(-24.0596944013836,27.4501189372788,-29.8825772147483));
#65770=CARTESIAN_POINT('Ctrl Pts',(-23.9451000500774,27.4650884655943,-29.8884419016865));
#65771=CARTESIAN_POINT('Ctrl Pts',(-23.8296880903085,27.4750233605025,-29.8943065886247));
#65772=CARTESIAN_POINT('Ctrl Pts',(-23.7139381743318,27.4798448782862,-29.9001712755629));
#65773=CARTESIAN_POINT('Ctrl Pts',(-23.5983072998975,27.4846614374407,-29.9060299310377));
#65774=CARTESIAN_POINT('Ctrl Pts',(-23.4823395711252,27.4843750623702,-29.9118885865125));
#65775=CARTESIAN_POINT('Ctrl Pts',(-23.3665210965324,27.4789586494553,-29.9177472419874));
#65776=CARTESIAN_POINT('Ctrl Pts',(-23.2461786503104,27.4733306666812,-29.9238347417053));
#65777=CARTESIAN_POINT('Ctrl Pts',(-23.1259978068178,27.4621636494904,-29.9299222414232));
#65778=CARTESIAN_POINT('Ctrl Pts',(-23.0065258475916,27.4454868369697,-29.9360097411411));
#65779=CARTESIAN_POINT('Ctrl Pts',(-22.8916783048566,27.429455535976,-29.9418616112245));
#65780=CARTESIAN_POINT('Ctrl Pts',(-22.7774862366438,27.4083331077393,-29.9477134813079));
#65781=CARTESIAN_POINT('Ctrl Pts',(-22.6644311298854,27.382198439989,-29.9535653513913));
#65782=CARTESIAN_POINT('Ctrl Pts',(-22.551393236795,27.3560677514795,-29.9594163304742));
#65783=CARTESIAN_POINT('Ctrl Pts',(-22.4394923636065,27.3249264339408,-29.9652673095572));
#65784=CARTESIAN_POINT('Ctrl Pts',(-22.3291989945931,27.2889043287372,-29.9711182886402));
#65785=CARTESIAN_POINT('Ctrl Pts',(-22.2188957091444,27.2528789847997,-29.9769697937825));
#65786=CARTESIAN_POINT('Ctrl Pts',(-22.1102006081625,27.2119721091923,-29.9828212989247));
#65787=CARTESIAN_POINT('Ctrl Pts',(-22.0035675407585,27.1663629474329,-29.988672804067));
#65788=CARTESIAN_POINT('Ctrl Pts',(-21.896899062834,27.1207386398638,-29.9945262523668));
#65789=CARTESIAN_POINT('Ctrl Pts',(-21.7922943599572,27.070409103625,-30.0003797006666));
#65790=CARTESIAN_POINT('Ctrl Pts',(-21.690185229562,27.0156008015711,-30.0062331489663));
#65791=CARTESIAN_POINT('Ctrl Pts',(-21.5879599789131,26.9607301705764,-30.0120932539079));
#65792=CARTESIAN_POINT('Ctrl Pts',(-21.4882363297693,26.901370803256,-30.0179533588494));
#65793=CARTESIAN_POINT('Ctrl Pts',(-21.3914195749,26.837794054574,-30.023813463791));
#65794=CARTESIAN_POINT('Ctrl Pts',(-21.2945376200058,26.7741744909309,-30.0296775151464));
#65795=CARTESIAN_POINT('Ctrl Pts',(-21.200566791724,26.7063321320196,-30.0355415665018));
#65796=CARTESIAN_POINT('Ctrl Pts',(-21.1098802011991,26.6345793445585,-30.0414056178573));
#65797=CARTESIAN_POINT('Ctrl Pts',(-21.0190599567425,26.5627208078119,-30.0472783116538));
#65798=CARTESIAN_POINT('Ctrl Pts',(-20.9315339217186,26.4869406098649,-30.0531510054504));
#65799=CARTESIAN_POINT('Ctrl Pts',(-20.8476392555443,26.4075887876463,-30.059023699247));
#65800=CARTESIAN_POINT('Ctrl Pts',(-20.8246702993324,26.385863586117,-30.0606315445703));
#65801=CARTESIAN_POINT('Ctrl Pts',(-20.8019733102506,26.3638708598002,-30.0622393898936));
#65802=CARTESIAN_POINT('Ctrl Pts',(-20.7795546757109,26.3416182173129,-30.0638472352169));
#65803=CARTESIAN_POINT('Ctrl Pts',(-20.6976756057894,26.2603453963959,-30.0697195321856));
#65804=CARTESIAN_POINT('Ctrl Pts',(-20.6192383589675,26.1753307315423,-30.0755918291543));
#65805=CARTESIAN_POINT('Ctrl Pts',(-20.5446044190939,26.0868976434949,-30.0814641261231));
#65806=CARTESIAN_POINT('Ctrl Pts',(-20.4700671988791,25.9985791577064,-30.0873288130613));
#65807=CARTESIAN_POINT('Ctrl Pts',(-20.3993237481874,25.9068513714101,-30.0931934999995));
#65808=CARTESIAN_POINT('Ctrl Pts',(-20.3326995878065,25.8120752597787,-30.0990581869377));
#65809=CARTESIAN_POINT('Ctrl Pts',(-20.266143946204,25.7173966194451,-30.1049168424125));
#65810=CARTESIAN_POINT('Ctrl Pts',(-20.2036994047332,25.6196762256278,-30.1107754978873));
#65811=CARTESIAN_POINT('Ctrl Pts',(-20.1456515283854,25.5193083989232,-30.1166341533622));
#65812=CARTESIAN_POINT('Ctrl Pts',(-20.0853362508596,25.4150201165048,-30.1227216530801));
#65813=CARTESIAN_POINT('Ctrl Pts',(-20.02976840905,25.3078737102556,-30.128809152798));
#65814=CARTESIAN_POINT('Ctrl Pts',(-19.9792192324939,25.1983454222809,-30.1348966525159));
#65815=CARTESIAN_POINT('Ctrl Pts',(-19.9306266694158,25.0930566598353,-30.1407485225993));
#65816=CARTESIAN_POINT('Ctrl Pts',(-19.8866716688742,24.9855673889998,-30.1466003926827));
#65817=CARTESIAN_POINT('Ctrl Pts',(-19.8475481253974,24.876325334971,-30.1524522627661));
#65818=CARTESIAN_POINT('Ctrl Pts',(-19.8084305388359,24.7670999140384,-30.1583032418491));
#65819=CARTESIAN_POINT('Ctrl Pts',(-19.7741430860048,24.6561226296204,-30.1641542209321));
#65820=CARTESIAN_POINT('Ctrl Pts',(-19.7448308458809,24.5438594927919,-30.170005200015));
#65821=CARTESIAN_POINT('Ctrl Pts',(-19.7155159703045,24.4315862624271,-30.1758567051573));
#65822=CARTESIAN_POINT('Ctrl Pts',(-19.6911773011056,24.3180273498262,-30.1817082102996));
#65823=CARTESIAN_POINT('Ctrl Pts',(-19.6719093607071,24.2036614756626,-30.1875597154419));
#65824=CARTESIAN_POINT('Ctrl Pts',(-19.6526350218451,24.0892576230818,-30.1934131637417));
#65825=CARTESIAN_POINT('Ctrl Pts',(-19.6384348287113,23.9740466835105,-30.1992666120415));
#65826=CARTESIAN_POINT('Ctrl Pts',(-19.6293516591246,23.8585143481477,-30.2051200603413));
#65827=CARTESIAN_POINT('Ctrl Pts',(-19.6202581600018,23.7428506274324,-30.2109801652829));
#65828=CARTESIAN_POINT('Ctrl Pts',(-19.6162933317269,23.6268651937607,-30.2168402702244));
#65829=CARTESIAN_POINT('Ctrl Pts',(-19.6174479567391,23.5110457056012,-30.222700375166));
#65830=CARTESIAN_POINT('Ctrl Pts',(-19.618603359319,23.3951482202654,-30.2285644265214));
#65831=CARTESIAN_POINT('Ctrl Pts',(-19.6248850577546,23.2794173147327,-30.2344284778769));
#65832=CARTESIAN_POINT('Ctrl Pts',(-19.6362319350756,23.1643357411226,-30.2402925292323));
#65833=CARTESIAN_POINT('Ctrl Pts',(-19.6475955354286,23.0490845602455,-30.2461652230289));
#65834=CARTESIAN_POINT('Ctrl Pts',(-19.6640391549982,22.9344850289054,-30.2520379168255));
#65835=CARTESIAN_POINT('Ctrl Pts',(-19.6854505508007,22.8210100147757,-30.2579106106221));
#65836=CARTESIAN_POINT('Ctrl Pts',(-19.6913126328021,22.7899424541141,-30.2595184559453));
#65837=CARTESIAN_POINT('Ctrl Pts',(-19.6975467976592,22.7589590954733,-30.2611263012686));
#65838=CARTESIAN_POINT('Ctrl Pts',(-19.7041500967817,22.7280694254704,-30.2627341465918));
#65839=CARTESIAN_POINT('Ctrl Pts',(-19.7282671762418,22.6152517850535,-30.2686064435605));
#65840=CARTESIAN_POINT('Ctrl Pts',(-19.7573927830819,22.5033071828822,-30.2744787405292));
#65841=CARTESIAN_POINT('Ctrl Pts',(-19.7914502153492,22.392714564006,-30.2803510374979));
#65842=CARTESIAN_POINT('Ctrl Pts',(-19.8254635118892,22.2822652643807,-30.2862157244361));
#65843=CARTESIAN_POINT('Ctrl Pts',(-19.8643958034048,22.1731648552529,-30.2920804113743));
#65844=CARTESIAN_POINT('Ctrl Pts',(-19.9081193532127,22.0658823251069,-30.2979450983125));
#65845=CARTESIAN_POINT('Ctrl Pts',(-19.9517979360866,21.9587101283272,-30.3038037537873));
#65846=CARTESIAN_POINT('Ctrl Pts',(-20.0002578211049,21.8533524723583,-30.3096624092621));
#65847=CARTESIAN_POINT('Ctrl Pts',(-20.0533216197173,21.7502627548175,-30.315521064737));
#65848=CARTESIAN_POINT('Ctrl Pts',(-20.1084581370416,21.6431462621091,-30.3216085644549));
#65849=CARTESIAN_POINT('Ctrl Pts',(-20.1685654321618,21.5384789296272,-30.3276960641728));
#65850=CARTESIAN_POINT('Ctrl Pts',(-20.2333894456673,21.4367463763798,-30.3337835638907));
#65851=CARTESIAN_POINT('Ctrl Pts',(-20.2957043077447,21.338951598155,-30.3396354339741));
#65852=CARTESIAN_POINT('Ctrl Pts',(-20.3623772936025,21.2438690110315,-30.3454873040575));
#65853=CARTESIAN_POINT('Ctrl Pts',(-20.4331365327328,21.1519037561783,-30.3513391741409));
#65854=CARTESIAN_POINT('Ctrl Pts',(-20.5038849981255,21.0599525038713,-30.3571901532238));
#65855=CARTESIAN_POINT('Ctrl Pts',(-20.5787182277069,20.9711179676324,-30.3630411323068));
#65856=CARTESIAN_POINT('Ctrl Pts',(-20.6573225798779,20.8857741035803,-30.3688921113898));
#65857=CARTESIAN_POINT('Ctrl Pts',(-20.7359339993367,20.8004225662935,-30.374743616532));
#65858=CARTESIAN_POINT('Ctrl Pts',(-20.8183169353355,20.7185626291716,-30.3805951216743));
#65859=CARTESIAN_POINT('Ctrl Pts',(-20.9041197255165,20.6405325843333,-30.3864466268166));
#65860=CARTESIAN_POINT('Ctrl Pts',(-20.9899510089364,20.5624766274156,-30.3923000751164));
#65861=CARTESIAN_POINT('Ctrl Pts',(-21.0792040990572,20.4882533697011,-30.3981535234162));
#65862=CARTESIAN_POINT('Ctrl Pts',(-21.1714935530031,20.4181614217013,-30.4040069717159));
#65863=CARTESIAN_POINT('Ctrl Pts',(-21.2638879600984,20.3479897639365,-30.4098670766575));
#65864=CARTESIAN_POINT('Ctrl Pts',(-21.3593252937146,20.2819590435148,-30.415727181599));
#65865=CARTESIAN_POINT('Ctrl Pts',(-21.4573902961179,20.2203251056234,-30.4215872865405));
#65866=CARTESIAN_POINT('Ctrl Pts',(-21.5555213391625,20.1586496611323,-30.427451337896));
#65867=CARTESIAN_POINT('Ctrl Pts',(-21.656283216053,20.1013770988003,-30.4333153892514));
#65868=CARTESIAN_POINT('Ctrl Pts',(-21.759236743018,20.0487169478806,-30.4391794406068));
#65869=CARTESIAN_POINT('Ctrl Pts',(-21.8623420029303,19.9959791864105,-30.4450521344034));
#65870=CARTESIAN_POINT('Ctrl Pts',(-21.9676449848974,19.947867574541,-30.4509248282));
#65871=CARTESIAN_POINT('Ctrl Pts',(-22.0746871853209,19.9045432853908,-30.4567975219965));
#65872=CARTESIAN_POINT('Ctrl Pts',(-22.103993549201,19.8926818197477,-30.4584053673199));
#65873=CARTESIAN_POINT('Ctrl Pts',(-22.1334301990654,19.8811789084159,-30.4600132126433));
#65874=CARTESIAN_POINT('Ctrl Pts',(-22.1629875598261,19.8700371986155,-30.4616210579668));
#65875=CARTESIAN_POINT('Ctrl Pts',(-22.2709392374352,19.8293445848829,-30.4674933549355));
#65876=CARTESIAN_POINT('Ctrl Pts',(-22.3808637346955,19.7933376434519,-30.4733656519042));
#65877=CARTESIAN_POINT('Ctrl Pts',(-22.4923166464442,19.7622107337859,-30.4792379488729));
#65878=CARTESIAN_POINT('Ctrl Pts',(-22.6036251240706,19.7311241621228,-30.4851026358111));
#65879=CARTESIAN_POINT('Ctrl Pts',(-22.7164576828048,19.7049051559623,-30.4909673227493));
#65880=CARTESIAN_POINT('Ctrl Pts',(-22.8303507076736,19.683699756447,-30.4968320096875));
#65881=CARTESIAN_POINT('Ctrl Pts',(-22.9441266006961,19.6625161653576,-30.5026906651623));
#65882=CARTESIAN_POINT('Ctrl Pts',(-23.0589603865923,19.6463360002162,-30.5085493206371));
#65883=CARTESIAN_POINT('Ctrl Pts',(-23.1743747283084,19.6352551016922,-30.5144079761119));
#65884=CARTESIAN_POINT('Ctrl Pts',(-23.2942972558676,19.623741373512,-30.5204954758298));
#65885=CARTESIAN_POINT('Ctrl Pts',(-23.4148461799605,19.6177335190221,-30.5265829755478));
#65886=CARTESIAN_POINT('Ctrl Pts',(-23.5354756112862,19.6172802914383,-30.5326704752657));
#65887=CARTESIAN_POINT('Ctrl Pts',(-23.6514358236992,19.6168446069929,-30.5385223453491));
#65888=CARTESIAN_POINT('Ctrl Pts',(-23.7674699748903,19.6215415394737,-30.5443742154325));
#65889=CARTESIAN_POINT('Ctrl Pts',(-23.8830902552613,19.6313613556381,-30.5502260855159));
#65890=CARTESIAN_POINT('Ctrl Pts',(-23.9986929313934,19.6411796766461,-30.5560770645988));
#65891=CARTESIAN_POINT('Ctrl Pts',(-24.1138814502137,19.656119295463,-30.5619280436818));
#65892=CARTESIAN_POINT('Ctrl Pts',(-24.2281716595849,19.6761184792846,-30.5677790227648));
#65893=CARTESIAN_POINT('Ctrl Pts',(-24.3424721447459,19.6961194612252,-30.5736305279071));
#65894=CARTESIAN_POINT('Ctrl Pts',(-24.455873752681,19.721180841219,-30.5794820330494));
#65895=CARTESIAN_POINT('Ctrl Pts',(-24.5679017841425,19.7511896210554,-30.5853335381917));
#65896=CARTESIAN_POINT('Ctrl Pts',(-24.6799670176746,19.7812083661544,-30.5911869864915));
#65897=CARTESIAN_POINT('Ctrl Pts',(-24.7906573686438,19.8161776710418,-30.5970404347913));
#65898=CARTESIAN_POINT('Ctrl Pts',(-24.8995132628018,19.8559346677996,-30.602893883091));
#65899=CARTESIAN_POINT('Ctrl Pts',(-25.0084929497488,19.8957368768956,-30.6087539880326));
#65900=CARTESIAN_POINT('Ctrl Pts',(-25.1156336274148,19.9403375033096,-30.6146140929741));
#65901=CARTESIAN_POINT('Ctrl Pts',(-25.220495584542,19.9895254789122,-30.6204741979157));
#65902=CARTESIAN_POINT('Ctrl Pts',(-25.3254281596342,20.0387465795378,-30.6263382492711));
#65903=CARTESIAN_POINT('Ctrl Pts',(-25.428078593316,20.092560989277,-30.6322023006266));
#65904=CARTESIAN_POINT('Ctrl Pts',(-25.5280332076643,20.1507124748984,-30.638066351982));
#65905=CARTESIAN_POINT('Ctrl Pts',(-25.6281351351613,20.2089496642014,-30.6439390457786));
#65906=CARTESIAN_POINT('Ctrl Pts',(-25.7255329673192,20.2715364639187,-30.6498117395752));
#65907=CARTESIAN_POINT('Ctrl Pts',(-25.8198432658568,20.3381742481832,-30.6556844333718));
#65908=CARTESIAN_POINT('Ctrl Pts',(-25.8456638479769,20.3564185588002,-30.657292278695));
#65909=CARTESIAN_POINT('Ctrl Pts',(-25.8712531974368,20.3749662950071,-30.6589001240183));
#65910=CARTESIAN_POINT('Ctrl Pts',(-25.8966039113448,20.3938108320565,-30.6605079693416));
#65911=CARTESIAN_POINT('Ctrl Pts',(-25.9882908702291,20.4619666362644,-30.6663231289692));
#65912=CARTESIAN_POINT('Ctrl Pts',(-26.0771739154361,20.534245915364,-30.6721382885967));
#65913=CARTESIAN_POINT('Ctrl Pts',(-26.1628535832494,20.610387782184,-30.6779534482243));
#65914=CARTESIAN_POINT('Ctrl Pts',(-26.2484218402025,20.6864306403232,-30.683761046292));
#65915=CARTESIAN_POINT('Ctrl Pts',(-26.3307946872854,20.7663258245341,-30.6895686443597));
#65916=CARTESIAN_POINT('Ctrl Pts',(-26.4096025433909,20.8497698876822,-30.6953762424275));
#65917=CARTESIAN_POINT('Ctrl Pts',(-26.4883300325188,20.9331288559236,-30.7011779180006));
#65918=CARTESIAN_POINT('Ctrl Pts',(-26.5634994709374,21.0200292023037,-30.7069795935737));
#65919=CARTESIAN_POINT('Ctrl Pts',(-26.6347758320368,21.1101285574577,-30.7127812691468));
#65920=CARTESIAN_POINT('Ctrl Pts',(-26.7060007161387,21.2001628413286,-30.7185787546513));
#65921=CARTESIAN_POINT('Ctrl Pts',(-26.7733378530381,21.2933912095816,-30.7243762401559));
#65922=CARTESIAN_POINT('Ctrl Pts',(-26.8364909749819,21.3894365067031,-30.7301737256604));
#65923=CARTESIAN_POINT('Ctrl Pts',(-26.8996204763624,21.485445880913,-30.7359690427865));
#65924=CARTESIAN_POINT('Ctrl Pts',(-26.958568840997,21.5842697379139,-30.7417643599125));
#65925=CARTESIAN_POINT('Ctrl Pts',(-27.0130822241071,21.6855006658033,-30.7475596770385));
#65926=CARTESIAN_POINT('Ctrl Pts',(-27.0675890491965,21.7867194154993,-30.7533542969815));
#65927=CARTESIAN_POINT('Ctrl Pts',(-27.1176617535317,21.8903442885566,-30.7591489169244));
#65928=CARTESIAN_POINT('Ctrl Pts',(-27.1630921076474,21.9959426531866,-30.7649435368673));
#65929=CARTESIAN_POINT('Ctrl Pts',(-27.2085285233355,22.1015551073422,-30.7707389299609));
#65930=CARTESIAN_POINT('Ctrl Pts',(-27.2493211918264,22.2091411881512,-30.7765343230545));
#65931=CARTESIAN_POINT('Ctrl Pts',(-27.2853100775913,22.3182484209717,-30.7823297161481));
#65932=CARTESIAN_POINT('Ctrl Pts',(-27.3213335965694,22.4274606510428,-30.7881306863269));
#65933=CARTESIAN_POINT('Ctrl Pts',(-27.3525439703304,22.5381965543137,-30.7939316565058));
#65934=CARTESIAN_POINT('Ctrl Pts',(-27.3788311109258,22.6499886466868,-30.7997326266846));
#65935=CARTESIAN_POINT('Ctrl Pts',(-27.4051318832004,22.7618387109008,-30.805536605063));
#65936=CARTESIAN_POINT('Ctrl Pts',(-27.4265042609705,22.8747456401159,-30.8113405834414));
#65937=CARTESIAN_POINT('Ctrl Pts',(-27.4428896676765,22.9882337352369,-30.8171445618198));
#65938=CARTESIAN_POINT('Ctrl Pts',(-27.459299555236,23.1018913888848,-30.8229572117159));
#65939=CARTESIAN_POINT('Ctrl Pts',(-27.4707075521564,23.2161315225773,-30.828769861612));
#65940=CARTESIAN_POINT('Ctrl Pts',(-27.4771071121635,23.3304751355696,-30.8345825115081));
#65941=CARTESIAN_POINT('Ctrl Pts',(-27.481237209735,23.4042693148278,-30.8383338336604));
#65942=CARTESIAN_POINT('Ctrl Pts',(-27.4832823320317,23.478106587533,-30.8420851558128));
#65943=CARTESIAN_POINT('Ctrl Pts',(-27.4832522035277,23.5518591921931,-30.8458364779651));
#65944=CARTESIAN_POINT('',(-27.4838863721737,23.5466573194615,-32.0958364779651));
#65945=CARTESIAN_POINT('Ctrl Pts',(-27.4889592910419,23.5518615235821,-30.8458364779651));
#65946=CARTESIAN_POINT('Ctrl Pts',(-27.4894190108028,23.6408453350039,-30.8503559455489));
#65947=CARTESIAN_POINT('Ctrl Pts',(-27.4866659078226,23.7298001893193,-30.8548754131327));
#65948=CARTESIAN_POINT('Ctrl Pts',(-27.3917678005741,25.1200922643632,-30.9256905178415));
#65949=CARTESIAN_POINT('Ctrl Pts',(-25.7924728177291,27.6261817534798,-31.0582817920914));
#65950=CARTESIAN_POINT('Ctrl Pts',(-21.3331200095261,27.6398826141405,-31.2571687034663));
#65951=CARTESIAN_POINT('Ctrl Pts',(-18.9111240073572,23.8955601724853,-31.4560556148412));
#65952=CARTESIAN_POINT('Ctrl Pts',(-20.7520937858179,19.8339292862019,-31.6549425262161));
#65953=CARTESIAN_POINT('Ctrl Pts',(-25.1643342070015,19.1872843702764,-31.853829437591));
#65954=CARTESIAN_POINT('Ctrl Pts',(-27.3287038009197,21.6719949499706,-32.000794088174));
#65955=CARTESIAN_POINT('Ctrl Pts',(-27.4865274055665,23.262709423076,-32.081463101632));
#65956=CARTESIAN_POINT('Ctrl Pts',(-27.4838863721737,23.5466573194615,-32.0958364779651));
#65957=CARTESIAN_POINT('',(-27.4767290463135,23.5502914556789,-33.3458364779651));
#65958=CARTESIAN_POINT('Ctrl Pts',(-27.4838863721737,23.5466573194615,-32.0958364779651));
#65959=CARTESIAN_POINT('Ctrl Pts',(-27.4743459259068,24.5723882532228,-32.147758738757));
#65960=CARTESIAN_POINT('Ctrl Pts',(-26.5386620802302,26.923215037617,-32.2659766366737));
#65961=CARTESIAN_POINT('Ctrl Pts',(-22.5719187031782,28.098176646286,-32.4504901717156));
#65962=CARTESIAN_POINT('Ctrl Pts',(-19.1951767590657,25.1855096511627,-32.6493770830904));
#65963=CARTESIAN_POINT('Ctrl Pts',(-19.8203802004651,20.7701800101868,-32.8482639944654));
#65964=CARTESIAN_POINT('Ctrl Pts',(-23.8730200732411,18.9095013051974,-33.0471509058403));
#65965=CARTESIAN_POINT('Ctrl Pts',(-27.0052926844262,20.9140808275611,-33.2130084003402));
#65966=CARTESIAN_POINT('Ctrl Pts',(-27.4766710115324,22.8900833516303,-33.3125702577151));
#65967=CARTESIAN_POINT('Ctrl Pts',(-27.4767290463135,23.5502914556789,-33.3458364779651));
#65968=CARTESIAN_POINT('',(-27.4840297199183,23.553834420186,-34.5958364779651));
#65969=CARTESIAN_POINT('Ctrl Pts',(-27.4767290463135,23.5502914556789,-33.3458364779651));
#65970=CARTESIAN_POINT('Ctrl Pts',(-27.4767866679778,24.2057999122759,-33.3788658948401));
#65971=CARTESIAN_POINT('Ctrl Pts',(-27.0102223100593,26.1769478082497,-33.4781909488402));
#65972=CARTESIAN_POINT('Ctrl Pts',(-23.889589688675,28.1898215985353,-33.6438116399649));
#65973=CARTESIAN_POINT('Ctrl Pts',(-19.8303313507955,26.3436263412674,-33.8426985513399));
#65974=CARTESIAN_POINT('Ctrl Pts',(-19.1893651808564,21.9305573920422,-34.0415854627147));
#65975=CARTESIAN_POINT('Ctrl Pts',(-22.5556847440637,19.0058509486566,-34.2404723740897));
#65976=CARTESIAN_POINT('Ctrl Pts',(-26.531694747342,20.168129958384,-34.4252227125063));
#65977=CARTESIAN_POINT('Ctrl Pts',(-27.4744466997929,22.5235216847793,-34.5436774137982));
#65978=CARTESIAN_POINT('Ctrl Pts',(-27.4840297199183,23.553834420186,-34.5958364779651));
#65979=CARTESIAN_POINT('',(-27.4847809928552,23.5485683047834,-35.8458364779651));
#65980=CARTESIAN_POINT('Ctrl Pts',(-27.4840297199183,23.553834420186,-34.5958364779651));
#65981=CARTESIAN_POINT('Ctrl Pts',(-27.4866269878204,23.8330781410309,-34.6099730509232));
#65982=CARTESIAN_POINT('Ctrl Pts',(-27.3319136679028,25.4190216835505,-34.6904052610063));
#65983=CARTESIAN_POINT('Ctrl Pts',(-25.1799036529807,27.9074291467727,-34.8371331082142));
#65984=CARTESIAN_POINT('Ctrl Pts',(-20.765382256512,27.2765440370006,-35.0360200195892));
#65985=CARTESIAN_POINT('Ctrl Pts',(-18.9099205248741,23.2215129712688,-35.2349069309641));
#65986=CARTESIAN_POINT('Ctrl Pts',(-21.3185304722301,19.468565689051,-35.433793842339));
#65987=CARTESIAN_POINT('Ctrl Pts',(-25.7779037734052,19.4663425452466,-35.6326807537138));
#65988=CARTESIAN_POINT('Ctrl Pts',(-27.4438276006778,22.0563973201223,-35.7700282989226));
#65989=CARTESIAN_POINT('Ctrl Pts',(-27.4893831213271,23.4549152959221,-35.8410802070063));
#65990=CARTESIAN_POINT('Ctrl Pts',(-27.48887967105,23.54856655029,-35.8458364779651));
#65991=CARTESIAN_POINT('',(-27.4823337739288,23.5474881844497,-37.0958364389384));
#65992=CARTESIAN_POINT('Ctrl Pts',(-27.4832521713565,23.5485689592156,-35.8458364779651));
#65993=CARTESIAN_POINT('Ctrl Pts',(-27.4833010804302,23.6628256197236,-35.8516475539864));
#65994=CARTESIAN_POINT('Ctrl Pts',(-27.4783669067839,23.7772857692739,-35.8574586300076));
#65995=CARTESIAN_POINT('Ctrl Pts',(-27.4684227067072,23.8914731049878,-35.8632697060289));
#65996=CARTESIAN_POINT('Ctrl Pts',(-27.4584907720493,24.0055195992575,-35.8690736145273));
#65997=CARTESIAN_POINT('Ctrl Pts',(-27.4435611311356,24.1192935314233,-35.8748775230257));
#65998=CARTESIAN_POINT('Ctrl Pts',(-27.4236588403682,24.2323174610992,-35.8806814315241));
#65999=CARTESIAN_POINT('Ctrl Pts',(-27.4037755068557,24.3452337336485,-35.8864798117056));
#66000=CARTESIAN_POINT('Ctrl Pts',(-27.3789290140938,24.4574010102805,-35.892278191887));
#66001=CARTESIAN_POINT('Ctrl Pts',(-27.3491962524981,24.5683466364628,-35.8980765720684));
#66002=CARTESIAN_POINT('Ctrl Pts',(-27.3194819609759,24.6792233429163,-35.90387135028));
#66003=CARTESIAN_POINT('Ctrl Pts',(-27.2848875439982,24.7888795006092,-35.9096661284917));
#66004=CARTESIAN_POINT('Ctrl Pts',(-27.245540894086,24.8968530362135,-35.9154609067034));
#66005=CARTESIAN_POINT('Ctrl Pts',(-27.2062064694983,25.0047930235612,-35.9212538844303));
#66006=CARTESIAN_POINT('Ctrl Pts',(-27.1621228906993,25.1110510310645,-35.9270468621571));
#66007=CARTESIAN_POINT('Ctrl Pts',(-27.1134675588383,25.2151812599989,-35.932839839884));
#66008=CARTESIAN_POINT('Ctrl Pts',(-27.0648149810358,25.3193055948056,-35.9386324897085));
#66009=CARTESIAN_POINT('Ctrl Pts',(-27.0115913437918,25.4213020077496,-35.944425139533));
#66010=CARTESIAN_POINT('Ctrl Pts',(-26.9540213827635,25.5207465328245,-35.9502177893575));
#66011=CARTESIAN_POINT('Ctrl Pts',(-26.8964400508042,25.620210699685,-35.9560115833173));
#66012=CARTESIAN_POINT('Ctrl Pts',(-26.8345109012256,25.7171216116196,-35.961805377277));
#66013=CARTESIAN_POINT('Ctrl Pts',(-26.7685031915193,25.8110823993612,-35.9675991712368));
#66014=CARTESIAN_POINT('Ctrl Pts',(-26.7024260487529,25.9051420238152,-35.9733990596489));
#66015=CARTESIAN_POINT('Ctrl Pts',(-26.6322620242447,25.9962449826675,-35.9791989480611));
#66016=CARTESIAN_POINT('Ctrl Pts',(-26.5583220564273,26.0840257524802,-35.9849988364732));
#66017=CARTESIAN_POINT('Ctrl Pts',(-26.4843396080464,26.1718569547812,-35.9908020570822));
#66018=CARTESIAN_POINT('Ctrl Pts',(-26.4065771839923,26.2563618583141,-35.9966052776912));
#66019=CARTESIAN_POINT('Ctrl Pts',(-26.3253828185495,26.3372116076367,-36.0024084983002));
#66020=CARTESIAN_POINT('Ctrl Pts',(-26.2440619203749,26.4181873526437,-36.0082207626077));
#66021=CARTESIAN_POINT('Ctrl Pts',(-26.1592987145201,26.4954962868289,-36.0140330269151));
#66022=CARTESIAN_POINT('Ctrl Pts',(-26.0714746767591,26.5688495394504,-36.0198452912225));
#66023=CARTESIAN_POINT('Ctrl Pts',(-26.0180388028701,26.6134807731804,-36.0233817196362));
#66024=CARTESIAN_POINT('Ctrl Pts',(-25.9634703998983,26.6566484310142,-36.0269181480499));
#66025=CARTESIAN_POINT('Ctrl Pts',(-25.9078602994194,26.6982955132244,-36.0304545764636));
#66026=CARTESIAN_POINT('Ctrl Pts',(-25.81551882201,26.7674511714226,-36.0363268734323));
#66027=CARTESIAN_POINT('Ctrl Pts',(-25.7199772556527,26.8326562634563,-36.042199170401));
#66028=CARTESIAN_POINT('Ctrl Pts',(-25.6216082656292,26.8936003184933,-36.0480714673697));
#66029=CARTESIAN_POINT('Ctrl Pts',(-25.5233667540044,26.9544653948751,-36.0539361543079));
#66030=CARTESIAN_POINT('Ctrl Pts',(-25.422305453489,27.0110801997646,-36.0598008412462));
#66031=CARTESIAN_POINT('Ctrl Pts',(-25.318828939574,27.0631753161418,-36.0656655281844));
#66032=CARTESIAN_POINT('Ctrl Pts',(-25.2154588447757,27.115216855953,-36.0715241836592));
#66033=CARTESIAN_POINT('Ctrl Pts',(-25.1096788441844,27.1627477680231,-36.077382839134));
#66034=CARTESIAN_POINT('Ctrl Pts',(-25.0019206773712,27.2055430255984,-36.0832414946088));
#66035=CARTESIAN_POINT('Ctrl Pts',(-24.8899533816501,27.2500099036282,-36.0893289943267));
#66036=CARTESIAN_POINT('Ctrl Pts',(-24.7758506179667,27.2893633880399,-36.0954164940446));
#66037=CARTESIAN_POINT('Ctrl Pts',(-24.6601230822019,27.323404577546,-36.1015039937625));
#66038=CARTESIAN_POINT('Ctrl Pts',(-24.5488750270478,27.3561281303518,-36.107355863846));
#66039=CARTESIAN_POINT('Ctrl Pts',(-24.436126075118,27.3839428612702,-36.1132077339294));
#66040=CARTESIAN_POINT('Ctrl Pts',(-24.3223474355458,27.4067222203403,-36.1190596040128));
#66041=CARTESIAN_POINT('Ctrl Pts',(-24.2085861198059,27.429498111046,-36.1249105830957));
#66042=CARTESIAN_POINT('Ctrl Pts',(-24.0937958333789,27.4472400731813,-36.1307615621787));
#66043=CARTESIAN_POINT('Ctrl Pts',(-23.9784587591846,27.4598725166465,-36.1366125412617));
#66044=CARTESIAN_POINT('Ctrl Pts',(-23.8631113150775,27.47250609589,-36.142464046404));
#66045=CARTESIAN_POINT('Ctrl Pts',(-23.7472173964247,27.4800291982189,-36.1483155515463));
#66046=CARTESIAN_POINT('Ctrl Pts',(-23.6312643894131,27.4824181028406,-36.1541670566886));
#66047=CARTESIAN_POINT('Ctrl Pts',(-23.5152728769322,27.4848078007655,-36.1600205049883));
#66048=CARTESIAN_POINT('Ctrl Pts',(-23.399222650152,27.4820599022765,-36.1658739532881));
#66049=CARTESIAN_POINT('Ctrl Pts',(-23.283600462147,27.4742027956255,-36.1717274015878));
#66050=CARTESIAN_POINT('Ctrl Pts',(-23.1678467866071,27.466336753738,-36.1775875065294));
#66051=CARTESIAN_POINT('Ctrl Pts',(-23.052522534103,27.4533499345903,-36.1834476114709));
#66052=CARTESIAN_POINT('Ctrl Pts',(-22.9381088090778,27.4353225520235,-36.1893077164124));
#66053=CARTESIAN_POINT('Ctrl Pts',(-22.8236180335695,27.4172830291428,-36.1951717677679));
#66054=CARTESIAN_POINT('Ctrl Pts',(-22.7100394106186,27.3941962658534,-36.2010358191233));
#66055=CARTESIAN_POINT('Ctrl Pts',(-22.597841624427,27.3661931056181,-36.2068998704788));
#66056=CARTESIAN_POINT('Ctrl Pts',(-22.4854784810952,27.3381486743145,-36.2127725642754));
#66057=CARTESIAN_POINT('Ctrl Pts',(-22.3745006309178,27.3051735021705,-36.2186452580719));
#66058=CARTESIAN_POINT('Ctrl Pts',(-22.2653595256975,27.2674475713902,-36.2245179518685));
#66059=CARTESIAN_POINT('Ctrl Pts',(-22.2354785167956,27.2571188426202,-36.2261257971919));
#66060=CARTESIAN_POINT('Ctrl Pts',(-22.20573505551,27.2464342820289,-36.2277336425152));
#66061=CARTESIAN_POINT('Ctrl Pts',(-22.1761380972322,27.2353981897386,-36.2293414878386));
#66062=CARTESIAN_POINT('Ctrl Pts',(-22.0680417985066,27.1950913204384,-36.2352137848073));
#66063=CARTESIAN_POINT('Ctrl Pts',(-21.9615393936409,27.1499567141263,-36.241086081776));
#66064=CARTESIAN_POINT('Ctrl Pts',(-21.8570935283387,27.1001400777097,-36.2469583787447));
#66065=CARTESIAN_POINT('Ctrl Pts',(-21.752783016583,27.0503879996976,-36.2528230656829));
#66066=CARTESIAN_POINT('Ctrl Pts',(-21.6505241141111,26.9959661340572,-36.2586877526211));
#66067=CARTESIAN_POINT('Ctrl Pts',(-21.5507621761864,26.9370692256166,-36.2645524395593));
#66068=CARTESIAN_POINT('Ctrl Pts',(-21.4511028371693,26.8782328889591,-36.2704110950341));
#66069=CARTESIAN_POINT('Ctrl Pts',(-21.3539357087071,26.8149308726108,-36.2762697505089));
#66070=CARTESIAN_POINT('Ctrl Pts',(-21.2596834831239,26.7474047698167,-36.2821284059838));
#66071=CARTESIAN_POINT('Ctrl Pts',(-21.1617496825934,26.6772410379715,-36.2882159057017));
#66072=CARTESIAN_POINT('Ctrl Pts',(-21.0669635549451,26.6025166950774,-36.2943034054196));
#66073=CARTESIAN_POINT('Ctrl Pts',(-20.9757684919428,26.5235538835698,-36.3003909051375));
#66074=CARTESIAN_POINT('Ctrl Pts',(-20.888103327973,26.4476474957629,-36.3062427752209));
#66075=CARTESIAN_POINT('Ctrl Pts',(-20.8037567398837,26.3678249519861,-36.3120946453042));
#66076=CARTESIAN_POINT('Ctrl Pts',(-20.7230899047927,26.284414282771,-36.3179465153876));
#66077=CARTESIAN_POINT('Ctrl Pts',(-20.6424353519607,26.2010163135886,-36.3237974944706));
#66078=CARTESIAN_POINT('Ctrl Pts',(-20.5654597254178,26.114031602307,-36.3296484735536));
#66079=CARTESIAN_POINT('Ctrl Pts',(-20.4924872606926,26.0238249578536,-36.3354994526366));
#66080=CARTESIAN_POINT('Ctrl Pts',(-20.4195082350406,25.933610202955,-36.3413509577788));
#66081=CARTESIAN_POINT('Ctrl Pts',(-20.350533346703,25.8401732604312,-36.3472024629211));
#66082=CARTESIAN_POINT('Ctrl Pts',(-20.2858460052765,25.7439113543651,-36.3530539680634));
#66083=CARTESIAN_POINT('Ctrl Pts',(-20.2211371825919,25.647617481815,-36.3589074163632));
#66084=CARTESIAN_POINT('Ctrl Pts',(-20.1607189684023,25.54849712328,-36.364760864663));
#66085=CARTESIAN_POINT('Ctrl Pts',(-20.1048305898669,25.4469751373419,-36.3706143129627));
#66086=CARTESIAN_POINT('Ctrl Pts',(-20.0488786541094,25.3453376988611,-36.3764744179043));
#66087=CARTESIAN_POINT('Ctrl Pts',(-19.9974670355339,25.2412935439909,-36.3823345228458));
#66088=CARTESIAN_POINT('Ctrl Pts',(-19.950788306237,25.1352907929529,-36.3881946277874));
#66089=CARTESIAN_POINT('Ctrl Pts',(-19.9040781417375,25.0292166556966,-36.3940586791428));
#66090=CARTESIAN_POINT('Ctrl Pts',(-19.8621073624037,24.9211816802824,-36.3999227304983));
#66091=CARTESIAN_POINT('Ctrl Pts',(-19.8250192311154,24.8116509050318,-36.4057867818537));
#66092=CARTESIAN_POINT('Ctrl Pts',(-19.787876439325,24.7019587032828,-36.4116594756503));
#66093=CARTESIAN_POINT('Ctrl Pts',(-19.7556307722095,24.5907666974543,-36.4175321694469));
#66094=CARTESIAN_POINT('Ctrl Pts',(-19.7283748365586,24.4785519895337,-36.4234048632434));
#66095=CARTESIAN_POINT('Ctrl Pts',(-19.7209126173136,24.4478294796281,-36.4250127085667));
#66096=CARTESIAN_POINT('Ctrl Pts',(-19.7138241156677,24.4170303486559,-36.4266205538901));
#66097=CARTESIAN_POINT('Ctrl Pts',(-19.7071105546248,24.3861644553363,-36.4282283992134));
#66098=CARTESIAN_POINT('Ctrl Pts',(-19.682590768057,24.2734336539658,-36.4341006961821));
#66099=CARTESIAN_POINT('Ctrl Pts',(-19.6629942048396,24.1594342257253,-36.4399729931508));
#66100=CARTESIAN_POINT('Ctrl Pts',(-19.6484483589224,24.0446341629677,-36.4458452901195));
#66101=CARTESIAN_POINT('Ctrl Pts',(-19.6339213632663,23.9299828719743,-36.4517099770577));
#66102=CARTESIAN_POINT('Ctrl Pts',(-19.6244321200844,23.8145334161144,-36.4575746639959));
#66103=CARTESIAN_POINT('Ctrl Pts',(-19.6200575206853,23.6987657480786,-36.4634393509341));
#66104=CARTESIAN_POINT('Ctrl Pts',(-19.6156874202879,23.583117139842,-36.4692980064089));
#66105=CARTESIAN_POINT('Ctrl Pts',(-19.6164215165977,23.4671513809737,-36.4751566618838));
#66106=CARTESIAN_POINT('Ctrl Pts',(-19.6222850362848,23.3513546810087,-36.4810153173586));
#66107=CARTESIAN_POINT('Ctrl Pts',(-19.6283775902154,23.2310348599508,-36.4871028170765));
#66108=CARTESIAN_POINT('Ctrl Pts',(-19.6400085133725,23.1108980252912,-36.4931903167944));
#66109=CARTESIAN_POINT('Ctrl Pts',(-19.6571464539655,22.991491341603,-36.4992778165123));
#66110=CARTESIAN_POINT('Ctrl Pts',(-19.6736210340879,22.8767065477774,-36.5051296865957));
#66111=CARTESIAN_POINT('Ctrl Pts',(-19.6951841728816,22.7625968792008,-36.5109815566791));
#66112=CARTESIAN_POINT('Ctrl Pts',(-19.7217551243006,22.6496435146504,-36.5168334267625));
#66113=CARTESIAN_POINT('Ctrl Pts',(-19.7483220300506,22.5367073482771,-36.5226844058455));
#66114=CARTESIAN_POINT('Ctrl Pts',(-19.7798951377277,22.4249275381594,-36.5285353849285));
#66115=CARTESIAN_POINT('Ctrl Pts',(-19.8163427905093,22.3147740637781,-36.5343863640114));
#66116=CARTESIAN_POINT('Ctrl Pts',(-19.8527937202857,22.204610685539,-36.5402378691537));
#66117=CARTESIAN_POINT('Ctrl Pts',(-19.8941199365396,22.0960743261952,-36.546089374296));
#66118=CARTESIAN_POINT('Ctrl Pts',(-19.9401404428872,21.9896181394519,-36.5519408794383));
#66119=CARTESIAN_POINT('Ctrl Pts',(-19.9861762316429,21.883126600927,-36.5577943277381));
#66120=CARTESIAN_POINT('Ctrl Pts',(-20.0369092462645,21.7787169878198,-36.5636477760379));
#66121=CARTESIAN_POINT('Ctrl Pts',(-20.0921113585199,21.6768202200276,-36.5695012243376));
#66122=CARTESIAN_POINT('Ctrl Pts',(-20.1473762475639,21.5748075734836,-36.5753613292791));
#66123=CARTESIAN_POINT('Ctrl Pts',(-20.2071201814014,21.4753138397271,-36.5812214342207));
#66124=CARTESIAN_POINT('Ctrl Pts',(-20.2710702423531,21.3787432608708,-36.5870815391622));
#66125=CARTESIAN_POINT('Ctrl Pts',(-20.3350633696686,21.2821076477736,-36.5929455905177));
#66126=CARTESIAN_POINT('Ctrl Pts',(-20.4032680216245,21.1883994427848,-36.5988096418731));
#66127=CARTESIAN_POINT('Ctrl Pts',(-20.4753703933385,21.0979905482959,-36.6046736932286));
#66128=CARTESIAN_POINT('Ctrl Pts',(-20.5475790295552,21.0074484091439,-36.6105463870251));
#66129=CARTESIAN_POINT('Ctrl Pts',(-20.6236965795987,20.92021559546,-36.6164190808217));
#66130=CARTESIAN_POINT('Ctrl Pts',(-20.7033717074578,20.8366279127399,-36.6222917746183));
#66131=CARTESIAN_POINT('Ctrl Pts',(-20.7251854246639,20.8137430034618,-36.6238996199416));
#66132=CARTESIAN_POINT('Ctrl Pts',(-20.7472656146644,20.7911310921355,-36.625507465265));
#66133=CARTESIAN_POINT('Ctrl Pts',(-20.7696046442387,20.7687985367503,-36.6271153105884));
#66134=CARTESIAN_POINT('Ctrl Pts',(-20.8511929747496,20.6872338517731,-36.6329876075571));
#66135=CARTESIAN_POINT('Ctrl Pts',(-20.9365098332629,20.6091254105994,-36.6388599045258));
#66136=CARTESIAN_POINT('Ctrl Pts',(-21.0252304058443,20.5348334457348,-36.6447322014945));
#66137=CARTESIAN_POINT('Ctrl Pts',(-21.1138360036096,20.4606377573565,-36.6505968884327));
#66138=CARTESIAN_POINT('Ctrl Pts',(-21.2058362296468,20.3902489727126,-36.6564615753709));
#66139=CARTESIAN_POINT('Ctrl Pts',(-21.3008688547163,20.3239912165269,-36.6623262623091));
#66140=CARTESIAN_POINT('Ctrl Pts',(-21.3958037446802,20.2578016022955,-36.6681849177839));
#66141=CARTESIAN_POINT('Ctrl Pts',(-21.4937644934943,20.1957348010321,-36.6740435732588));
#66142=CARTESIAN_POINT('Ctrl Pts',(-21.5943556810036,20.1380748532228,-36.6799022287336));
#66143=CARTESIAN_POINT('Ctrl Pts',(-21.6988760488965,20.0781626570659,-36.6859897284515));
#66144=CARTESIAN_POINT('Ctrl Pts',(-21.8062361906173,20.0230088957691,-36.6920772281694));
#66145=CARTESIAN_POINT('Ctrl Pts',(-21.9159588204585,19.9728829581926,-36.6981647278873));
#66146=CARTESIAN_POINT('Ctrl Pts',(-22.0214344023548,19.9246972517285,-36.7040165979707));
#66147=CARTESIAN_POINT('Ctrl Pts',(-22.1290925717329,19.8811575688695,-36.7098684680541));
#66148=CARTESIAN_POINT('Ctrl Pts',(-22.2384848581532,19.8424560741398,-36.7157203381375));
#66149=CARTESIAN_POINT('Ctrl Pts',(-22.3478604886033,19.8037604720645,-36.7215713172205));
#66150=CARTESIAN_POINT('Ctrl Pts',(-22.4589693215036,19.7699017312436,-36.7274222963034));
#66151=CARTESIAN_POINT('Ctrl Pts',(-22.5713447891374,19.741023130416,-36.7332732753864));
#66152=CARTESIAN_POINT('Ctrl Pts',(-22.6837303604072,19.7121419331243,-36.7391247805287));
#66153=CARTESIAN_POINT('Ctrl Pts',(-22.7973823924009,19.688241868832,-36.744976285671));
#66154=CARTESIAN_POINT('Ctrl Pts',(-22.911821803085,19.6694156110329,-36.7508277908133));
#66155=CARTESIAN_POINT('Ctrl Pts',(-23.0262992166063,19.6505831014434,-36.7566812391131));
#66156=CARTESIAN_POINT('Ctrl Pts',(-23.1415641210529,19.6368278157336,-36.7625346874129));
#66157=CARTESIAN_POINT('Ctrl Pts',(-23.2571306633043,19.6281907562664,-36.7683881357127));
#66158=CARTESIAN_POINT('Ctrl Pts',(-23.3728286298086,19.6195438745872,-36.7742482406543));
#66159=CARTESIAN_POINT('Ctrl Pts',(-23.4888285063129,19.6160268675892,-36.7801083455958));
#66160=CARTESIAN_POINT('Ctrl Pts',(-23.6046426735698,19.6176286350488,-36.7859684505373));
#66161=CARTESIAN_POINT('Ctrl Pts',(-23.7205348344199,19.6192314811984,-36.7918325018928));
#66162=CARTESIAN_POINT('Ctrl Pts',(-23.836240625319,19.6259599418744,-36.7976965532482));
#66163=CARTESIAN_POINT('Ctrl Pts',(-23.9512775337031,19.6377510367726,-36.8035606046037));
#66164=CARTESIAN_POINT('Ctrl Pts',(-24.0664839835267,19.6495595093909,-36.8094332984003));
#66165=CARTESIAN_POINT('Ctrl Pts',(-24.1810191759434,19.6664454475042,-36.8153059921968));
#66166=CARTESIAN_POINT('Ctrl Pts',(-24.294410680147,19.6882947833376,-36.8211786859934));
#66167=CARTESIAN_POINT('Ctrl Pts',(-24.3254553771884,19.6942767659938,-36.8227865313166));
#66168=CARTESIAN_POINT('Ctrl Pts',(-24.3564144363144,19.7006305036489,-36.8243943766399));
#66169=CARTESIAN_POINT('Ctrl Pts',(-24.3872783823627,19.7073530111092,-36.8260022219632));
#66170=CARTESIAN_POINT('Ctrl Pts',(-24.5000020717623,19.7319054724746,-36.8318745189319));
#66171=CARTESIAN_POINT('Ctrl Pts',(-24.611833392709,19.7614630533028,-36.8377468159006));
#66172=CARTESIAN_POINT('Ctrl Pts',(-24.7222936998507,19.7959472031219,-36.8436191128693));
#66173=CARTESIAN_POINT('Ctrl Pts',(-24.8326108592068,19.8303866642215,-36.8494837998075));
#66174=CARTESIAN_POINT('Ctrl Pts',(-24.9415601470675,19.8697398758966,-36.8553484867457));
#66175=CARTESIAN_POINT('Ctrl Pts',(-25.0486730716044,19.9138772917643,-36.8612131736839));
#66176=CARTESIAN_POINT('Ctrl Pts',(-25.1556758372039,19.9579693150629,-36.8670718291587));
#66177=CARTESIAN_POINT('Ctrl Pts',(-25.2608456160637,20.0068355993684,-36.8729304846335));
#66178=CARTESIAN_POINT('Ctrl Pts',(-25.3637296988003,20.0602970069941,-36.8787891401083));
#66179=CARTESIAN_POINT('Ctrl Pts',(-25.4706325244276,20.1158466642898,-36.8848766398262));
#66180=CARTESIAN_POINT('Ctrl Pts',(-25.5750670171097,20.1763576067197,-36.8909641395441));
#66181=CARTESIAN_POINT('Ctrl Pts',(-25.6765485423198,20.2415739019089,-36.897051639262));
#66182=CARTESIAN_POINT('Ctrl Pts',(-25.7741020090817,20.3042658615726,-36.9029035093454));
#66183=CARTESIAN_POINT('Ctrl Pts',(-25.868926479293,20.3713054414222,-36.9087553794288));
#66184=CARTESIAN_POINT('Ctrl Pts',(-25.9606178644304,20.4424192088239,-36.9146072495122));
#66185=CARTESIAN_POINT('Ctrl Pts',(-26.0522952887209,20.5135221485079,-36.9204582285952));
#66186=CARTESIAN_POINT('Ctrl Pts',(-26.140840249884,20.5886977890504,-36.9263092076781));
#66187=CARTESIAN_POINT('Ctrl Pts',(-26.2258800054825,20.6676310474356,-36.9321601867611));
#66188=CARTESIAN_POINT('Ctrl Pts',(-26.3109274069734,20.7465714026803,-36.9380116919034));
#66189=CARTESIAN_POINT('Ctrl Pts',(-26.3924686734077,20.8292697661325,-36.9438631970457));
#66190=CARTESIAN_POINT('Ctrl Pts',(-26.4701668728711,20.9153731719911,-36.9497147021879));
#66191=CARTESIAN_POINT('Ctrl Pts',(-26.5478908742153,21.0015051709165,-36.9555681504877));
#66192=CARTESIAN_POINT('Ctrl Pts',(-26.6217689941519,21.0910441539158,-36.9614215987875));
#66193=CARTESIAN_POINT('Ctrl Pts',(-26.6915041124965,21.1836035281224,-36.9672750470873));
#66194=CARTESIAN_POINT('Ctrl Pts',(-26.7613185348132,21.2762681624363,-36.9731351520288));
#66195=CARTESIAN_POINT('Ctrl Pts',(-26.8269803026443,21.3719597134348,-36.9789952569703));
#66196=CARTESIAN_POINT('Ctrl Pts',(-26.8882351759192,21.4702619387221,-36.9848553619119));
#66197=CARTESIAN_POINT('Ctrl Pts',(-26.9495313005174,21.5686303644055,-36.9907194132673));
#66198=CARTESIAN_POINT('Ctrl Pts',(-27.0064144187566,21.6696126058639,-36.9965834646228));
#66199=CARTESIAN_POINT('Ctrl Pts',(-27.0586766985272,21.7727686736572,-37.0024475159782));
#66200=CARTESIAN_POINT('Ctrl Pts',(-27.1110160024657,21.8760767729025,-37.0083202097748));
#66201=CARTESIAN_POINT('Ctrl Pts',(-27.1587207064073,21.9815647173778,-37.0141929035713));
#66202=CARTESIAN_POINT('Ctrl Pts',(-27.2016314086062,22.0887733846515,-37.0200655973679));
#66203=CARTESIAN_POINT('Ctrl Pts',(-27.2133796410605,22.1181253243704,-37.0216734426913));
#66204=CARTESIAN_POINT('Ctrl Pts',(-27.224768818873,22.1476061648111,-37.0232812880147));
#66205=CARTESIAN_POINT('Ctrl Pts',(-27.2357963318104,22.1772063207366,-37.024889133338));
#66206=CARTESIAN_POINT('Ctrl Pts',(-27.2821080378936,22.3015166461033,-37.031641522609));
#66207=CARTESIAN_POINT('Ctrl Pts',(-27.322165586825,22.4282767091552,-37.03839391188));
#66208=CARTESIAN_POINT('Ctrl Pts',(-27.355738366958,22.5568912894431,-37.045146301151));
#66209=CARTESIAN_POINT('Ctrl Pts',(-27.3891788643623,22.6849991053951,-37.0518720848066));
#66210=CARTESIAN_POINT('Ctrl Pts',(-27.4161854879993,22.8149467075672,-37.0585978684621));
#66211=CARTESIAN_POINT('Ctrl Pts',(-27.4365769699211,22.9461239354163,-37.0653236521177));
#66212=CARTESIAN_POINT('Ctrl Pts',(-27.4568208581286,23.076351701409,-37.0720007544957));
#66213=CARTESIAN_POINT('Ctrl Pts',(-27.4705449288546,23.2077911962808,-37.0786778568737));
#66214=CARTESIAN_POINT('Ctrl Pts',(-27.4776192945278,23.3398260357622,-37.0853549592517));
#66215=CARTESIAN_POINT('Ctrl Pts',(-27.4813209874302,23.4089138452932,-37.0888487823905));
#66216=CARTESIAN_POINT('Ctrl Pts',(-27.483202820316,23.4781643496993,-37.0923426055294));
#66217=CARTESIAN_POINT('Ctrl Pts',(-27.4832515596232,23.547487335628,-37.0958364286682));
#66218=CARTESIAN_POINT('',(-27.4822753988055,23.5529940695056,-38.3458365164865));
#66219=CARTESIAN_POINT('Ctrl Pts',(-27.4788461937177,23.5474914099673,-37.0958364779651));
#66220=CARTESIAN_POINT('Ctrl Pts',(-27.4733986381108,24.3927224225629,-37.1384830002144));
#66221=CARTESIAN_POINT('Ctrl Pts',(-26.7905005240498,26.5599232774312,-37.2474251595887));
#66222=CARTESIAN_POINT('Ctrl Pts',(-23.2155414968396,28.1901576336606,-37.4226629560879));
#66223=CARTESIAN_POINT('Ctrl Pts',(-19.4656970161889,25.7767199293586,-37.6215498674628));
#66224=CARTESIAN_POINT('Ctrl Pts',(-19.4692127410894,21.3173474599079,-37.8204367788377));
#66225=CARTESIAN_POINT('Ctrl Pts',(-23.222858018441,18.9098254322999,-38.0193236902125));
#66226=CARTESIAN_POINT('Ctrl Pts',(-26.7931104595749,20.5447185682919,-38.1944569232551));
#66227=CARTESIAN_POINT('Ctrl Pts',(-27.4734163905603,22.7098084322925,-38.3032945191725));
#66228=CARTESIAN_POINT('Ctrl Pts',(-27.4788019670004,23.5529908840325,-38.3458364779651));
#66229=CARTESIAN_POINT('',(-27.4847991704008,23.5519704097288,-39.5958364779651));
#66230=CARTESIAN_POINT('Ctrl Pts',(-27.4832515755615,23.5529949647541,-38.3458365273125));
#66231=CARTESIAN_POINT('Ctrl Pts',(-27.4831592318539,23.6854276278161,-38.3525107634145));
#66232=CARTESIAN_POINT('Ctrl Pts',(-27.4763739482618,23.8175957568385,-38.3591849995164));
#66233=CARTESIAN_POINT('Ctrl Pts',(-27.4629996664109,23.9488737300342,-38.3658592356183));
#66234=CARTESIAN_POINT('Ctrl Pts',(-27.449561077883,24.0807829184477,-38.3725655630094));
#66235=CARTESIAN_POINT('Ctrl Pts',(-27.4294700928455,24.2117932052308,-38.3792718904004));
#66236=CARTESIAN_POINT('Ctrl Pts',(-27.4028816673861,24.3412883986546,-38.3859782177915));
#66237=CARTESIAN_POINT('Ctrl Pts',(-27.3761332597264,24.4715627629248,-38.3927248970648));
#66238=CARTESIAN_POINT('Ctrl Pts',(-27.3428090848831,24.6003035844075,-38.3994715763381));
#66239=CARTESIAN_POINT('Ctrl Pts',(-27.3031152843816,24.7269046295938,-38.4062182556113));
#66240=CARTESIAN_POINT('Ctrl Pts',(-27.281779401774,24.7949541739549,-38.4098446747283));
#66241=CARTESIAN_POINT('Ctrl Pts',(-27.2586040313723,24.8623858726676,-38.4134710938453));
#66242=CARTESIAN_POINT('Ctrl Pts',(-27.2336267596423,24.929108324331,-38.4170975129623));
#66243=CARTESIAN_POINT('Ctrl Pts',(-27.1931808121841,25.0371526617359,-38.422969809931));
#66244=CARTESIAN_POINT('Ctrl Pts',(-27.1479091829293,25.1435968936783,-38.4288421068997));
#66245=CARTESIAN_POINT('Ctrl Pts',(-27.0979581740536,25.2479785623515,-38.4347144038685));
#66246=CARTESIAN_POINT('Ctrl Pts',(-27.0480718977184,25.3522249606718,-38.4405790908067));
#66247=CARTESIAN_POINT('Ctrl Pts',(-26.9935184778837,25.4544137417535,-38.4464437777449));
#66248=CARTESIAN_POINT('Ctrl Pts',(-26.9344932323536,25.5540998013233,-38.4523084646831));
#66249=CARTESIAN_POINT('Ctrl Pts',(-26.8755286905936,25.6536833400213,-38.458167120158));
#66250=CARTESIAN_POINT('Ctrl Pts',(-26.8121016801221,25.7507689232456,-38.4640257756328));
#66251=CARTESIAN_POINT('Ctrl Pts',(-26.7444543379561,25.8449341699337,-38.4698844311076));
#66252=CARTESIAN_POINT('Ctrl Pts',(-26.6741646310224,25.9427775940967,-38.4759719308255));
#66253=CARTESIAN_POINT('Ctrl Pts',(-26.5993183676267,26.0374674788321,-38.4820594305434));
#66254=CARTESIAN_POINT('Ctrl Pts',(-26.5202382605485,26.1285608473155,-38.4881469302613));
#66255=CARTESIAN_POINT('Ctrl Pts',(-26.4442191173452,26.2161282530697,-38.4939988003447));
#66256=CARTESIAN_POINT('Ctrl Pts',(-26.3642880921644,26.3003720459029,-38.4998506704282));
#66257=CARTESIAN_POINT('Ctrl Pts',(-26.2807736800725,26.3809314711465,-38.5057025405116));
#66258=CARTESIAN_POINT('Ctrl Pts',(-26.1972719838092,26.461478630485,-38.5115535195945));
#66259=CARTESIAN_POINT('Ctrl Pts',(-26.1101882829092,26.5383422507226,-38.5174044986775));
#66260=CARTESIAN_POINT('Ctrl Pts',(-26.0198878032634,26.6111985660798,-38.5232554777605));
#66261=CARTESIAN_POINT('Ctrl Pts',(-25.9295792047356,26.6840614319209,-38.5291069829028));
#66262=CARTESIAN_POINT('Ctrl Pts',(-25.8360535742644,26.7529160170584,-38.5349584880451));
#66263=CARTESIAN_POINT('Ctrl Pts',(-25.7397085003297,26.8174794233267,-38.5408099931875));
#66264=CARTESIAN_POINT('Ctrl Pts',(-25.6433314322933,26.8820642696967,-38.5466634414872));
#66265=CARTESIAN_POINT('Ctrl Pts',(-25.5441334022921,26.9423548736568,-38.552516889787));
#66266=CARTESIAN_POINT('Ctrl Pts',(-25.4425395764231,26.9981125550059,-38.5583703380868));
#66267=CARTESIAN_POINT('Ctrl Pts',(-25.3408302163134,27.0539336449463,-38.5642304430284));
#66268=CARTESIAN_POINT('Ctrl Pts',(-25.2367199848427,27.1052113242074,-38.5700905479699));
#66269=CARTESIAN_POINT('Ctrl Pts',(-25.1306572496868,27.1517535975481,-38.5759506529115));
#66270=CARTESIAN_POINT('Ctrl Pts',(-25.024523087917,27.1983272141968,-38.581814704267));
#66271=CARTESIAN_POINT('Ctrl Pts',(-24.9164341888335,27.2401589261581,-38.5876787556224));
#66272=CARTESIAN_POINT('Ctrl Pts',(-24.8068557747408,27.277106069139,-38.5935428069779));
#66273=CARTESIAN_POINT('Ctrl Pts',(-24.6971158639395,27.3141076648333,-38.5994155007745));
#66274=CARTESIAN_POINT('Ctrl Pts',(-24.5858824525196,27.3462102097767,-38.605288194571));
#66275=CARTESIAN_POINT('Ctrl Pts',(-24.4736327612511,27.3733217112492,-38.6111608883676));
#66276=CARTESIAN_POINT('Ctrl Pts',(-24.4429006734929,27.3807443868316,-38.6127687336908));
#66277=CARTESIAN_POINT('Ctrl Pts',(-24.412092445677,27.387793246519,-38.614376579014));
#66278=CARTESIAN_POINT('Ctrl Pts',(-24.3812179380884,27.3944670799961,-38.6159844243371));
#66279=CARTESIAN_POINT('Ctrl Pts',(-24.2684556750089,27.4188417704793,-38.6218567213059));
#66280=CARTESIAN_POINT('Ctrl Pts',(-24.1544311219155,27.4382916090648,-38.6277290182746));
#66281=CARTESIAN_POINT('Ctrl Pts',(-24.0396124348488,27.4526897041781,-38.6336013152433));
#66282=CARTESIAN_POINT('Ctrl Pts',(-23.9249425436819,27.4670691405037,-38.6394660021815));
#66283=CARTESIAN_POINT('Ctrl Pts',(-23.8094809715053,27.4764098013506,-38.6453306891197));
#66284=CARTESIAN_POINT('Ctrl Pts',(-23.6937077695654,27.4806354131356,-38.6511953760579));
#66285=CARTESIAN_POINT('Ctrl Pts',(-23.5780536331161,27.4848566791434,-38.6570540315327));
#66286=CARTESIAN_POINT('Ctrl Pts',(-23.4620889150022,27.4839733445224,-38.6629126870076));
#66287=CARTESIAN_POINT('Ctrl Pts',(-23.3462998568208,27.4779608083375,-38.6687713424824));
#66288=CARTESIAN_POINT('Ctrl Pts',(-23.2259879760414,27.4717134171934,-38.6748588422003));
#66289=CARTESIAN_POINT('Ctrl Pts',(-23.1058662089595,27.4599278968983,-38.6809463419182));
#66290=CARTESIAN_POINT('Ctrl Pts',(-22.9864816793478,27.4426363033751,-38.6870338416361));
#66291=CARTESIAN_POINT('Ctrl Pts',(-22.8717181820779,27.4260140177863,-38.6928857117195));
#66292=CARTESIAN_POINT('Ctrl Pts',(-22.7576363580775,27.4043040465735,-38.6987375818029));
#66293=CARTESIAN_POINT('Ctrl Pts',(-22.6447172818115,27.3775877549559,-38.7045894518863));
#66294=CARTESIAN_POINT('Ctrl Pts',(-22.5318153985016,27.3508755311366,-38.7104404309693));
#66295=CARTESIAN_POINT('Ctrl Pts',(-22.4200763130827,27.3191585976763,-38.7162914100522));
#66296=CARTESIAN_POINT('Ctrl Pts',(-22.3099698352141,27.2825692161158,-38.7221423891352));
#66297=CARTESIAN_POINT('Ctrl Pts',(-22.1998534577134,27.2459765448178,-38.7279938942775));
#66298=CARTESIAN_POINT('Ctrl Pts',(-22.0913703718756,27.2045106849263,-38.7338453994198));
#66299=CARTESIAN_POINT('Ctrl Pts',(-21.9849734981023,27.1583532158489,-38.7396969045621));
#66300=CARTESIAN_POINT('Ctrl Pts',(-21.8785412922432,27.1121804188807,-38.7455503528619));
#66301=CARTESIAN_POINT('Ctrl Pts',(-21.7741970550425,27.0613130792125,-38.7514038011617));
#66302=CARTESIAN_POINT('Ctrl Pts',(-21.6723714124572,27.005979879448,-38.7572572494615));
#66303=CARTESIAN_POINT('Ctrl Pts',(-21.5704299720054,26.95058375382,-38.763117354403));
#66304=CARTESIAN_POINT('Ctrl Pts',(-21.4710132064377,26.8907118287525,-38.7689774593445));
#66305=CARTESIAN_POINT('Ctrl Pts',(-21.3745250063084,26.8266375419271,-38.7748375642861));
#66306=CARTESIAN_POINT('Ctrl Pts',(-21.2779718274152,26.7625201050797,-38.7807016156415));
#66307=CARTESIAN_POINT('Ctrl Pts',(-21.1843514741112,26.694194914426,-38.786565666997));
#66308=CARTESIAN_POINT('Ctrl Pts',(-21.0940354446374,26.6219762531982,-38.7924297183524));
#66309=CARTESIAN_POINT('Ctrl Pts',(-21.0035863073649,26.5496511560799,-38.798302412149));
#66310=CARTESIAN_POINT('Ctrl Pts',(-20.9164515232883,26.4734214072164,-38.8041751059456));
#66311=CARTESIAN_POINT('Ctrl Pts',(-20.8329664454832,26.3936387744836,-38.8100477997422));
#66312=CARTESIAN_POINT('Ctrl Pts',(-20.8101096277153,26.3717956242421,-38.8116556450655));
#66313=CARTESIAN_POINT('Ctrl Pts',(-20.7875261506028,26.349686352754,-38.8132634903888));
#66314=CARTESIAN_POINT('Ctrl Pts',(-20.7652223623064,26.327318601416,-38.8148713357121));
#66315=CARTESIAN_POINT('Ctrl Pts',(-20.6837627427124,26.2456253710568,-38.8207436326808));
#66316=CARTESIAN_POINT('Ctrl Pts',(-20.6057641623855,26.1602080637001,-38.8266159296495));
#66317=CARTESIAN_POINT('Ctrl Pts',(-20.5315864355227,26.0713919566021,-38.8324882266182));
#66318=CARTESIAN_POINT('Ctrl Pts',(-20.4575048371029,25.9826909481253,-38.8383529135564));
#66319=CARTESIAN_POINT('Ctrl Pts',(-20.3872345078877,25.8906002133769,-38.8442176004946));
#66320=CARTESIAN_POINT('Ctrl Pts',(-20.3210991061718,25.7954823984199,-38.8500822874328));
#66321=CARTESIAN_POINT('Ctrl Pts',(-20.2550317205764,25.700462406181,-38.8559409429076));
#66322=CARTESIAN_POINT('Ctrl Pts',(-20.19309103858,25.6024218633374,-38.8617995983824));
#66323=CARTESIAN_POINT('Ctrl Pts',(-20.1355605915586,25.5017565552548,-38.8676582538572));
#66324=CARTESIAN_POINT('Ctrl Pts',(-20.0757829546044,25.3971591715735,-38.8737457535751));
#66325=CARTESIAN_POINT('Ctrl Pts',(-20.020767403138,25.2897281401515,-38.879833253293));
#66326=CARTESIAN_POINT('Ctrl Pts',(-19.9707827115671,25.179941092984,-38.8859207530109));
#66327=CARTESIAN_POINT('Ctrl Pts',(-19.9227327838814,25.0744035871713,-38.8917726230943));
#66328=CARTESIAN_POINT('Ctrl Pts',(-19.8793316847739,24.9666894747554,-38.8976244931777));
#66329=CARTESIAN_POINT('Ctrl Pts',(-19.8407710014632,24.8572474731055,-38.9034763632611));
#66330=CARTESIAN_POINT('Ctrl Pts',(-19.8022161893671,24.7478221349955,-38.9093273423441));
#66331=CARTESIAN_POINT('Ctrl Pts',(-19.7685004650167,24.6366698205351,-38.915178321427));
#66332=CARTESIAN_POINT('Ctrl Pts',(-19.7397665065963,24.5242572814432,-38.92102930051));
#66333=CARTESIAN_POINT('Ctrl Pts',(-19.7110299647165,24.4118346353824,-38.9268808056523));
#66334=CARTESIAN_POINT('Ctrl Pts',(-19.6872761815478,24.2981519399773,-38.9327323107946));
#66335=CARTESIAN_POINT('Ctrl Pts',(-19.6685972139659,24.1836883961286,-38.9385838159369));
#66336=CARTESIAN_POINT('Ctrl Pts',(-19.6499120435055,24.0691868414287,-38.9444372642366));
#66337=CARTESIAN_POINT('Ctrl Pts',(-19.6363051061599,23.9539043304483,-38.9502907125364));
#66338=CARTESIAN_POINT('Ctrl Pts',(-19.6278167790031,23.8383267686721,-38.9561441608362));
#66339=CARTESIAN_POINT('Ctrl Pts',(-19.6193187987751,23.7226177701111,-38.9620042657777));
#66340=CARTESIAN_POINT('Ctrl Pts',(-19.615951077515,23.6066134635501,-38.9678643707192));
#66341=CARTESIAN_POINT('Ctrl Pts',(-19.6177018874803,23.4908014535475,-38.9737244756608));
#66342=CARTESIAN_POINT('Ctrl Pts',(-19.6194538765065,23.3749114514046,-38.9795885270162));
#66343=CARTESIAN_POINT('Ctrl Pts',(-19.626331235971,23.2592144153259,-38.9854525783717));
#66344=CARTESIAN_POINT('Ctrl Pts',(-19.6382703646655,23.144192776425,-38.9913166297271));
#66345=CARTESIAN_POINT('Ctrl Pts',(-19.6502270892524,23.0290016185889,-38.9971893235237));
#66346=CARTESIAN_POINT('Ctrl Pts',(-19.6672604112736,22.9144882519072,-39.0030620173202));
#66347=CARTESIAN_POINT('Ctrl Pts',(-19.6892556550669,22.8011249599986,-39.0089347111168));
#66348=CARTESIAN_POINT('Ctrl Pts',(-19.6952775848823,22.7700879870091,-39.0105425564402));
#66349=CARTESIAN_POINT('Ctrl Pts',(-19.7016711591795,22.7391371302837,-39.0121504017636));
#66350=CARTESIAN_POINT('Ctrl Pts',(-19.7084333805734,22.7082818611354,-39.013758247087));
#66351=CARTESIAN_POINT('Ctrl Pts',(-19.7331308882348,22.5955898621899,-39.0196305440557));
#66352=CARTESIAN_POINT('Ctrl Pts',(-19.7628323628056,22.4837966721581,-39.0255028410244));
#66353=CARTESIAN_POINT('Ctrl Pts',(-19.7974586378996,22.3733808349075,-39.0313751379931));
#66354=CARTESIAN_POINT('Ctrl Pts',(-19.8320400400909,22.2631080878129,-39.0372398249313));
#66355=CARTESIAN_POINT('Ctrl Pts',(-19.8715334284444,22.1542095346961,-39.0431045118695));
#66356=CARTESIAN_POINT('Ctrl Pts',(-19.915808653772,22.0471535002815,-39.0489691988077));
#66357=CARTESIAN_POINT('Ctrl Pts',(-19.960038344802,21.9402075662965,-39.0548278542826));
#66358=CARTESIAN_POINT('Ctrl Pts',(-20.009039933974,21.8351007616361,-39.0606865097574));
#66359=CARTESIAN_POINT('Ctrl Pts',(-20.0626337011476,21.7322855647729,-39.0665451652322));
#66360=CARTESIAN_POINT('Ctrl Pts',(-20.1183208880718,21.6254543157619,-39.0726326649501));
#66361=CARTESIAN_POINT('Ctrl Pts',(-20.1789661794692,21.5210977824406,-39.078720164668));
#66362=CARTESIAN_POINT('Ctrl Pts',(-20.2443130194898,21.4197002695693,-39.0848076643859));
#66363=CARTESIAN_POINT('Ctrl Pts',(-20.3071304709695,21.3222275632694,-39.0906595344693));
#66364=CARTESIAN_POINT('Ctrl Pts',(-20.3742920270284,21.2274894463095,-39.0965114045527));
#66365=CARTESIAN_POINT('Ctrl Pts',(-20.4455237352288,21.1358896549918,-39.1023632746362));
#66366=CARTESIAN_POINT('Ctrl Pts',(-20.5167445977539,21.0443038105753,-39.1082142537191));
#66367=CARTESIAN_POINT('Ctrl Pts',(-20.5920341265283,20.9558556679415,-39.1140652328021));
#66368=CARTESIAN_POINT('Ctrl Pts',(-20.6710767591067,20.8709175637319,-39.1199162118851));
#66369=CARTESIAN_POINT('Ctrl Pts',(-20.7501264983784,20.7859718227694,-39.1257677170274));
#66370=CARTESIAN_POINT('Ctrl Pts',(-20.8329297306223,20.7045370502247,-39.1316192221697));
#66371=CARTESIAN_POINT('Ctrl Pts',(-20.9191330567245,20.6269497234933,-39.137470727312));
#66372=CARTESIAN_POINT('Ctrl Pts',(-21.0053650090748,20.5493366316997,-39.1433241756118));
#66373=CARTESIAN_POINT('Ctrl Pts',(-21.0949989933271,20.4755738026527,-39.1491776239116));
#66374=CARTESIAN_POINT('Ctrl Pts',(-21.1876480345647,20.4059578587758,-39.1550310722114));
#66375=CARTESIAN_POINT('Ctrl Pts',(-21.2804024378804,20.3362627464538,-39.1608911771529));
#66376=CARTESIAN_POINT('Ctrl Pts',(-21.3761784112305,20.2707241805854,-39.1667512820945));
#66377=CARTESIAN_POINT('Ctrl Pts',(-21.4745593853769,20.2095958653588,-39.172611387036));
#66378=CARTESIAN_POINT('Ctrl Pts',(-21.5730066129518,20.1484263840378,-39.1784754383915));
#66379=CARTESIAN_POINT('Ctrl Pts',(-21.6740619749411,20.0916732691993,-39.1843394897469));
#66380=CARTESIAN_POINT('Ctrl Pts',(-21.7772852148052,20.0395437865484,-39.1902035411024));
#66381=CARTESIAN_POINT('Ctrl Pts',(-21.8806605851196,19.987337475446,-39.196076234899));
#66382=CARTESIAN_POINT('Ctrl Pts',(-21.9862098344891,19.9397685657942,-39.2019489286955));
#66383=CARTESIAN_POINT('Ctrl Pts',(-22.0934736357243,19.8969958683516,-39.2078216224921));
#66384=CARTESIAN_POINT('Ctrl Pts',(-22.122840670197,19.8852854192923,-39.2094294678154));
#66385=CARTESIAN_POINT('Ctrl Pts',(-22.1523361432092,19.8739341904624,-39.2110373131386));
#66386=CARTESIAN_POINT('Ctrl Pts',(-22.1819504661728,19.8629447797578,-39.2126451584619));
#66387=CARTESIAN_POINT('Ctrl Pts',(-22.2901101855521,19.8228084045515,-39.2185174554306));
#66388=CARTESIAN_POINT('Ctrl Pts',(-22.4002185781596,19.7873677949848,-39.2243897523993));
#66389=CARTESIAN_POINT('Ctrl Pts',(-22.5118302442226,19.7568150202961,-39.230262049368));
#66390=CARTESIAN_POINT('Ctrl Pts',(-22.6232972704304,19.7263018395769,-39.2361267363062));
#66391=CARTESIAN_POINT('Ctrl Pts',(-22.7362633009426,19.7006640053316,-39.2419914232444));
#66392=CARTESIAN_POINT('Ctrl Pts',(-22.8502639751575,19.6800451702318,-39.2478561101826));
#66393=CARTESIAN_POINT('Ctrl Pts',(-22.9641474068155,19.6594475403132,-39.2537147656574));
#66394=CARTESIAN_POINT('Ctrl Pts',(-23.0790629613562,19.6438587157316,-39.2595734211322));
#66395=CARTESIAN_POINT('Ctrl Pts',(-23.1945328146942,19.6333720787141,-39.265432076607));
#66396=CARTESIAN_POINT('Ctrl Pts',(-23.3145130222083,19.6224758244182,-39.2715195763249));
#66397=CARTESIAN_POINT('Ctrl Pts',(-23.4350912755479,19.6170885953447,-39.2776070760428));
#66398=CARTESIAN_POINT('Ctrl Pts',(-23.5557214416796,19.6172563340068,-39.2836945757607));
#66399=CARTESIAN_POINT('Ctrl Pts',(-23.671682360456,19.6174175799869,-39.2895464458441));
#66400=CARTESIAN_POINT('Ctrl Pts',(-23.7876907960239,19.6227117555017,-39.2953983159275));
#66401=CARTESIAN_POINT('Ctrl Pts',(-23.9032589953519,19.6331266163558,-39.3012501860109));
#66402=CARTESIAN_POINT('Ctrl Pts',(-24.0188095983706,19.6435398914526,-39.3071011650939));
#66403=CARTESIAN_POINT('Ctrl Pts',(-24.1339196868251,19.6590722645602,-39.3129521441768));
#66404=CARTESIAN_POINT('Ctrl Pts',(-24.2481054327725,19.6796595114379,-39.3188031232598));
#66405=CARTESIAN_POINT('Ctrl Pts',(-24.3623014451173,19.7002486093073,-39.3246546284021));
#66406=CARTESIAN_POINT('Ctrl Pts',(-24.4755725428977,19.7258934110615,-39.3305061335443));
#66407=CARTESIAN_POINT('Ctrl Pts',(-24.5874446148324,19.7564784763931,-39.3363576386866));
#66408=CARTESIAN_POINT('Ctrl Pts',(-24.699353837047,19.7870736983592,-39.3422110869864));
#66409=CARTESIAN_POINT('Ctrl Pts',(-24.8098627110775,19.8226123370834,-39.3480645352862));
#66410=CARTESIAN_POINT('Ctrl Pts',(-24.918512507155,19.8629291610699,-39.3539179835859));
#66411=CARTESIAN_POINT('Ctrl Pts',(-25.0272858616434,19.9032918340399,-39.3597780885275));
#66412=CARTESIAN_POINT('Ctrl Pts',(-25.1341955305579,19.9484433941431,-39.365638193469));
#66413=CARTESIAN_POINT('Ctrl Pts',(-25.2388028949754,19.9981705125591,-39.3714982984105));
#66414=CARTESIAN_POINT('Ctrl Pts',(-25.3434807059058,20.0479311190771,-39.377362349766));
#66415=CARTESIAN_POINT('Ctrl Pts',(-25.4458527608331,20.1022732261446,-39.3832264011214));
#66416=CARTESIAN_POINT('Ctrl Pts',(-25.5455067063187,20.1609384744485,-39.3890904524768));
#66417=CARTESIAN_POINT('Ctrl Pts',(-25.6453075218272,20.2196901836176,-39.3949631462734));
#66418=CARTESIAN_POINT('Ctrl Pts',(-25.7423818874744,20.282777525787,-39.40083584007));
#66419=CARTESIAN_POINT('Ctrl Pts',(-25.8363479072864,20.3498999052332,-39.4067085338665));
#66420=CARTESIAN_POINT('Ctrl Pts',(-25.8620742316527,20.3682768899062,-39.4083163791899));
#66421=CARTESIAN_POINT('Ctrl Pts',(-25.8875677644883,20.3869561058402,-39.4099242245133));
#66422=CARTESIAN_POINT('Ctrl Pts',(-25.9128211371016,20.4059308902676,-39.4115320698367));
#66423=CARTESIAN_POINT('Ctrl Pts',(-26.0041076019299,20.4745213719348,-39.4173441456261));
#66424=CARTESIAN_POINT('Ctrl Pts',(-26.0925728163968,20.5472171325677,-39.4231562214154));
#66425=CARTESIAN_POINT('Ctrl Pts',(-26.1778188951763,20.6237556488157,-39.4289682972048));
#66426=CARTESIAN_POINT('Ctrl Pts',(-26.2629541132975,20.7001946283997,-39.4347728145169));
#66427=CARTESIAN_POINT('Ctrl Pts',(-26.3448782059138,20.7804661503196,-39.440577331829));
#66428=CARTESIAN_POINT('Ctrl Pts',(-26.423223370057,20.8642652715016,-39.446381849141));
#66429=CARTESIAN_POINT('Ctrl Pts',(-26.5014886760188,20.9479789752173,-39.4521804498378));
#66430=CARTESIAN_POINT('Ctrl Pts',(-26.5761820197674,21.0352128222047,-39.4579790505346));
#66431=CARTESIAN_POINT('Ctrl Pts',(-26.6469703401396,21.1256231136476,-39.4637776512314));
#66432=CARTESIAN_POINT('Ctrl Pts',(-26.7177075464019,21.2159681225474,-39.4695720649337));
#66433=CARTESIAN_POINT('Ctrl Pts',(-26.7845450767361,21.3094846832181,-39.4753664786359));
#66434=CARTESIAN_POINT('Ctrl Pts',(-26.8471888011666,21.4057945034182,-39.4811608923381));
#66435=CARTESIAN_POINT('Ctrl Pts',(-26.9098091768905,21.5020684268105,-39.4869531463337));
#66436=CARTESIAN_POINT('Ctrl Pts',(-26.9682386228485,21.601133186934,-39.4927454003293));
#66437=CARTESIAN_POINT('Ctrl Pts',(-27.0222255848724,21.7025804509383,-39.4985376543249));
#66438=CARTESIAN_POINT('Ctrl Pts',(-27.0762061519759,21.8040156982047,-39.5043292222104));
#66439=CARTESIAN_POINT('Ctrl Pts',(-27.125745083046,21.9078325150411,-39.5101207900959));
#66440=CARTESIAN_POINT('Ctrl Pts',(-27.1706365692537,22.0135975865017,-39.5159123579813));
#66441=CARTESIAN_POINT('Ctrl Pts',(-27.215534152786,22.1193770233584,-39.5217047124986));
#66442=CARTESIAN_POINT('Ctrl Pts',(-27.2557828728013,22.227104851244,-39.5274970670158));
#66443=CARTESIAN_POINT('Ctrl Pts',(-27.2912252184687,22.3363281696325,-39.533289421533));
#66444=CARTESIAN_POINT('Ctrl Pts',(-27.3267014039581,22.4456557728131,-39.5390873065038));
#66445=CARTESIAN_POINT('Ctrl Pts',(-27.3573619224923,22.5564813146062,-39.5448851914746));
#66446=CARTESIAN_POINT('Ctrl Pts',(-27.3830992936658,22.6683371733724,-39.5506830764454));
#66447=CARTESIAN_POINT('Ctrl Pts',(-27.4088501005704,22.7802514244751,-39.5564839880976));
#66448=CARTESIAN_POINT('Ctrl Pts',(-27.4296725671037,22.893196648022,-39.5622848997498));
#66449=CARTESIAN_POINT('Ctrl Pts',(-27.4455107650829,23.0066972951108,-39.568085811402));
#66450=CARTESIAN_POINT('Ctrl Pts',(-27.4613722147019,23.1203645694989,-39.5738952392192));
#66451=CARTESIAN_POINT('Ctrl Pts',(-27.4722347465043,23.2345884752599,-39.5797046670364));
#66452=CARTESIAN_POINT('Ctrl Pts',(-27.4780944751955,23.3488905023242,-39.5855140948537));
#66453=CARTESIAN_POINT('Ctrl Pts',(-27.4815650616504,23.4165890405674,-39.5889548892241));
#66454=CARTESIAN_POINT('Ctrl Pts',(-27.4832816958199,23.4843149981474,-39.5923956835946));
#66455=CARTESIAN_POINT('Ctrl Pts',(-27.4832521568169,23.551969734281,-39.5958364779651));
#66456=CARTESIAN_POINT('',(-27.4832509072098,23.5466778720844,-40.8458364779651));
#66457=CARTESIAN_POINT('Ctrl Pts',(-27.4888435011611,23.5519721755401,-39.5958364779651));
#66458=CARTESIAN_POINT('Ctrl Pts',(-27.4893667048836,23.6476846199245,-39.6006973123806));
#66459=CARTESIAN_POINT('Ctrl Pts',(-27.4427386655007,25.0482753731377,-39.6718537839204));
#66460=CARTESIAN_POINT('Ctrl Pts',(-25.771461580151,27.6376699553484,-39.8093058925872));
#66461=CARTESIAN_POINT('Ctrl Pts',(-21.3120973279039,27.6284153675602,-40.0081928039611));
#66462=CARTESIAN_POINT('Ctrl Pts',(-18.9094079436724,23.8716749048059,-40.2070797153365));
#66463=CARTESIAN_POINT('Ctrl Pts',(-20.771261257099,19.8195745332832,-40.4059666267111));
#66464=CARTESIAN_POINT('Ctrl Pts',(-25.1867719322757,19.1956509329671,-40.6048535380861));
#66465=CARTESIAN_POINT('Ctrl Pts',(-27.333324802602,21.6856728041178,-40.7514768218375));
#66466=CARTESIAN_POINT('Ctrl Pts',(-27.4866705567893,23.2695102944433,-40.8318044684637));
#66467=CARTESIAN_POINT('Ctrl Pts',(-27.4840929910064,23.5466771067236,-40.8458364779651));
#66468=CARTESIAN_POINT('',(-27.483252531009,23.5501791140891,-42.0958364779359));
#66469=CARTESIAN_POINT('Ctrl Pts',(-27.4832509072098,23.5466778720844,-40.8458364779651));
#66470=CARTESIAN_POINT('Ctrl Pts',(-27.4833546239329,23.6607915913766,-40.8516149565601));
#66471=CARTESIAN_POINT('Ctrl Pts',(-27.4784877326466,23.7750600714861,-40.8573934351551));
#66472=CARTESIAN_POINT('Ctrl Pts',(-27.46863658494,23.8890082124863,-40.8631719137501));
#66473=CARTESIAN_POINT('Ctrl Pts',(-27.4587306022987,24.0035906287068,-40.8689825573786));
#66474=CARTESIAN_POINT('Ctrl Pts',(-27.4437846550542,24.1178486950974,-40.8747932010072));
#66475=CARTESIAN_POINT('Ctrl Pts',(-27.4238380713898,24.2312988345701,-40.8806038446358));
#66476=CARTESIAN_POINT('Ctrl Pts',(-27.4040275805656,24.3439749190992,-40.8863748430295));
#66477=CARTESIAN_POINT('Ctrl Pts',(-27.3792845583178,24.4558536426567,-40.8921458414232));
#66478=CARTESIAN_POINT('Ctrl Pts',(-27.3496994383711,24.5664671760205,-40.8979168398169));
#66479=CARTESIAN_POINT('Ctrl Pts',(-27.3201200368547,24.6770593291845,-40.9036867227494));
#66480=CARTESIAN_POINT('Ctrl Pts',(-27.2857005075728,24.7863863667189,-40.909456605682));
#66481=CARTESIAN_POINT('Ctrl Pts',(-27.2465818921875,24.8939929302666,-40.9152264886145));
#66482=CARTESIAN_POINT('Ctrl Pts',(-27.2074607445555,25.0016064594586,-40.9209967450461));
#66483=CARTESIAN_POINT('Ctrl Pts',(-27.163640052765,25.1074988932365,-40.9267670014778));
#66484=CARTESIAN_POINT('Ctrl Pts',(-27.1153096941662,25.2112330939848,-40.9325372579094));
#66485=CARTESIAN_POINT('Ctrl Pts',(-27.0663881276119,25.3162362380332,-40.9383780998199));
#66486=CARTESIAN_POINT('Ctrl Pts',(-27.0128460033438,25.4190275828371,-40.9442189417305));
#66487=CARTESIAN_POINT('Ctrl Pts',(-26.9549284064541,25.5191789365728,-40.950059783641));
#66488=CARTESIAN_POINT('Ctrl Pts',(-26.8976284850674,25.6182622032136,-40.9558383345526));
#66489=CARTESIAN_POINT('Ctrl Pts',(-26.836046253187,25.7147611904133,-40.9616168854642));
#66490=CARTESIAN_POINT('Ctrl Pts',(-26.7704622490776,25.8082911443112,-40.9673954363758));
#66491=CARTESIAN_POINT('Ctrl Pts',(-26.7038177819236,25.90333343435,-40.9732674237858));
#66492=CARTESIAN_POINT('Ctrl Pts',(-26.6330412851277,25.995309476246,-40.9791394111958));
#66493=CARTESIAN_POINT('Ctrl Pts',(-26.5584682167693,26.0838522222665,-40.9850113986058));
#66494=CARTESIAN_POINT('Ctrl Pts',(-26.4838951484109,26.172394968287,-40.9908833860158));
#66495=CARTESIAN_POINT('Ctrl Pts',(-26.4055258673103,26.2575041323493,-40.9967553734258));
#66496=CARTESIAN_POINT('Ctrl Pts',(-26.3237321843897,26.3388542630434,-41.0026273608358));
#66497=CARTESIAN_POINT('Ctrl Pts',(-26.2419341894797,26.4202086823439,-41.0084996578045));
#66498=CARTESIAN_POINT('Ctrl Pts',(-26.1564165747446,26.4980972726454,-41.0143719547732));
#66499=CARTESIAN_POINT('Ctrl Pts',(-26.0675050802241,26.5721606386557,-41.0202442517419));
#66500=CARTESIAN_POINT('Ctrl Pts',(-25.9787088079395,26.6461280244254,-41.0261089386801));
#66501=CARTESIAN_POINT('Ctrl Pts',(-25.8865277169977,26.7162797818324,-41.0319736256183));
#66502=CARTESIAN_POINT('Ctrl Pts',(-25.791324869684,26.7822927195472,-41.0378383125565));
#66503=CARTESIAN_POINT('Ctrl Pts',(-25.6962199325391,26.848237767088,-41.0436969680313));
#66504=CARTESIAN_POINT('Ctrl Pts',(-25.5980997580374,26.9100522272332,-41.0495556235062));
#66505=CARTESIAN_POINT('Ctrl Pts',(-25.4973604961,26.9674530781866,-41.055414278981));
#66506=CARTESIAN_POINT('Ctrl Pts',(-25.3926862698612,27.0270960569361,-41.0615017786989));
#66507=CARTESIAN_POINT('Ctrl Pts',(-25.2851845266623,27.0819733074568,-41.0675892784168));
#66508=CARTESIAN_POINT('Ctrl Pts',(-25.1753332439945,27.1318166702389,-41.0736767781347));
#66509=CARTESIAN_POINT('Ctrl Pts',(-25.069733989053,27.1797307395674,-41.0795286482181));
#66510=CARTESIAN_POINT('Ctrl Pts',(-24.9619641119919,27.2229931830438,-41.0853805183015));
#66511=CARTESIAN_POINT('Ctrl Pts',(-24.8524725763665,27.2614129910726,-41.0912323883849));
#66512=CARTESIAN_POINT('Ctrl Pts',(-24.7429977118231,27.2998269493362,-41.0970833674679));
#66513=CARTESIAN_POINT('Ctrl Pts',(-24.6318020998893,27.3333996013769,-41.1029343465509));
#66514=CARTESIAN_POINT('Ctrl Pts',(-24.5193526755131,27.3619888698018,-41.1087853256338));
#66515=CARTESIAN_POINT('Ctrl Pts',(-24.4068931408517,27.3905807086771,-41.1146368307761));
#66516=CARTESIAN_POINT('Ctrl Pts',(-24.2931799703128,27.4141881713818,-41.1204883359184));
#66517=CARTESIAN_POINT('Ctrl Pts',(-24.1786924828701,27.4327198178108,-41.1263398410607));
#66518=CARTESIAN_POINT('Ctrl Pts',(-24.064166976625,27.4512576181963,-41.1321932893605));
#66519=CARTESIAN_POINT('Ctrl Pts',(-23.9488670500374,27.4647161846421,-41.1380467376603));
#66520=CARTESIAN_POINT('Ctrl Pts',(-23.8332786601519,27.4730557654303,-41.14390018596));
#66521=CARTESIAN_POINT('Ctrl Pts',(-23.7175588211674,27.4814048301327,-41.1497602909016));
#66522=CARTESIAN_POINT('Ctrl Pts',(-23.6015502766721,27.4846232600771,-41.1556203958431));
#66523=CARTESIAN_POINT('Ctrl Pts',(-23.4857406157279,27.4827234105054,-41.1614805007847));
#66524=CARTESIAN_POINT('Ctrl Pts',(-23.3698529642249,27.4808222815039,-41.1673445521402));
#66525=CARTESIAN_POINT('Ctrl Pts',(-23.2541648745799,27.4737960346408,-41.1732086034956));
#66526=CARTESIAN_POINT('Ctrl Pts',(-23.1391586956569,27.4617088919227,-41.1790726548511));
#66527=CARTESIAN_POINT('Ctrl Pts',(-23.023983020584,27.4496039351692,-41.1849453486477));
#66528=CARTESIAN_POINT('Ctrl Pts',(-22.9094916692907,27.4324232574498,-41.1908180424442));
#66529=CARTESIAN_POINT('Ctrl Pts',(-22.7961567774259,27.410282142124,-41.1966907362408));
#66530=CARTESIAN_POINT('Ctrl Pts',(-22.7651275798946,27.4042202751234,-41.1982985815641));
#66531=CARTESIAN_POINT('Ctrl Pts',(-22.7341849768338,27.3977868747737,-41.1999064268875));
#66532=CARTESIAN_POINT('Ctrl Pts',(-22.703338435691,27.3909849506465,-41.2015142722108));
#66533=CARTESIAN_POINT('Ctrl Pts',(-22.5906783138372,27.3661424375923,-41.2073865691795));
#66534=CARTESIAN_POINT('Ctrl Pts',(-22.4789234398692,27.3362971184697,-41.2132588661482));
#66535=CARTESIAN_POINT('Ctrl Pts',(-22.3685522553774,27.3015287754482,-41.2191311631169));
#66536=CARTESIAN_POINT('Ctrl Pts',(-22.2583241031752,27.2668054894379,-41.2249958500551));
#66537=CARTESIAN_POINT('Ctrl Pts',(-22.1494764651573,27.227171989814,-41.2308605369933));
#66538=CARTESIAN_POINT('Ctrl Pts',(-22.0424774981683,27.182759028354,-41.2367252239315));
#66539=CARTESIAN_POINT('Ctrl Pts',(-21.9355885729184,27.1383917428446,-41.2425838794063));
#66540=CARTESIAN_POINT('Ctrl Pts',(-21.8305449165322,27.0892549299612,-41.2484425348812));
#66541=CARTESIAN_POINT('Ctrl Pts',(-21.7277987758217,27.035528892,-41.254301190356));
#66542=CARTESIAN_POINT('Ctrl Pts',(-21.6210392803576,26.9797042676748,-41.2603886900739));
#66543=CARTESIAN_POINT('Ctrl Pts',(-21.5167608792292,26.9189247277489,-41.2664761897918));
#66544=CARTESIAN_POINT('Ctrl Pts',(-21.415447546628,26.8534474511224,-41.2725636895097));
#66545=CARTESIAN_POINT('Ctrl Pts',(-21.3180557622218,26.7905046118634,-41.2784155595931));
#66546=CARTESIAN_POINT('Ctrl Pts',(-21.2234041554162,26.7232211908264,-41.2842674296765));
#66547=CARTESIAN_POINT('Ctrl Pts',(-21.1318961096235,26.6518716597996,-41.2901192997599));
#66548=CARTESIAN_POINT('Ctrl Pts',(-21.0404019967627,26.5805329923876,-41.2959702788429));
#66549=CARTESIAN_POINT('Ctrl Pts',(-20.9520508191438,26.5051297000739,-41.3018212579259));
#66550=CARTESIAN_POINT('Ctrl Pts',(-20.8672145069952,26.4259778242108,-41.3076722370088));
#66551=CARTESIAN_POINT('Ctrl Pts',(-20.782370567246,26.3468188318324,-41.3135237421511));
#66552=CARTESIAN_POINT('Ctrl Pts',(-20.7010424234609,26.2639108679335,-41.3193752472934));
#66553=CARTESIAN_POINT('Ctrl Pts',(-20.6235660979596,26.1776077643558,-41.3252267524357));
#66554=CARTESIAN_POINT('Ctrl Pts',(-20.5460640442569,26.0912760013956,-41.3310802007355));
#66555=CARTESIAN_POINT('Ctrl Pts',(-20.4724166282632,26.0015471643394,-41.3369336490353));
#66556=CARTESIAN_POINT('Ctrl Pts',(-20.4029199741495,25.9088086095136,-41.3427870973351));
#66557=CARTESIAN_POINT('Ctrl Pts',(-20.3333442872495,25.8159645908137,-41.3486472022766));
#66558=CARTESIAN_POINT('Ctrl Pts',(-20.2679290318867,25.7201043537337,-41.3545073072181));
#66559=CARTESIAN_POINT('Ctrl Pts',(-20.2069273759473,25.6216447936644,-41.3603674121597));
#66560=CARTESIAN_POINT('Ctrl Pts',(-20.1458846392107,25.5231189272441,-41.3662314635151));
#66561=CARTESIAN_POINT('Ctrl Pts',(-20.0892616217658,25.4219906120896,-41.3720955148705));
#66562=CARTESIAN_POINT('Ctrl Pts',(-20.03726502257,25.3187003711108,-41.377959566226));
#66563=CARTESIAN_POINT('Ctrl Pts',(-19.9851917907664,25.2152579009354,-41.3838322600225));
#66564=CARTESIAN_POINT('Ctrl Pts',(-19.9377587541865,25.1096475214803,-41.3897049538191));
#66565=CARTESIAN_POINT('Ctrl Pts',(-19.8951241323392,25.0023287639316,-41.3955776476156));
#66566=CARTESIAN_POINT('Ctrl Pts',(-19.8834514860675,24.9729466833382,-41.397185492939));
#66567=CARTESIAN_POINT('Ctrl Pts',(-19.8721382250183,24.9434366266,-41.3987933382623));
#66568=CARTESIAN_POINT('Ctrl Pts',(-19.8611869347455,24.9138081856406,-41.4004011835857));
#66569=CARTESIAN_POINT('Ctrl Pts',(-19.8211897859282,24.8055969034308,-41.4062734805544));
#66570=CARTESIAN_POINT('Ctrl Pts',(-19.785890906653,24.6954429926919,-41.4121457775231));
#66571=CARTESIAN_POINT('Ctrl Pts',(-19.7554817928044,24.5837921000058,-41.4180180744918));
#66572=CARTESIAN_POINT('Ctrl Pts',(-19.7251120867523,24.4722858980096,-41.42388276143));
#66573=CARTESIAN_POINT('Ctrl Pts',(-19.699619652239,24.3592869671422,-41.4297474483682));
#66574=CARTESIAN_POINT('Ctrl Pts',(-19.6791475442211,24.2452598524908,-41.4356121353064));
#66575=CARTESIAN_POINT('Ctrl Pts',(-19.6586964904848,24.1313500075889,-41.4414707907813));
#66576=CARTESIAN_POINT('Ctrl Pts',(-19.6432555661998,24.0164144866021,-41.4473294462561));
#66577=CARTESIAN_POINT('Ctrl Pts',(-19.6329175385933,23.900931233396,-41.4531881017309));
#66578=CARTESIAN_POINT('Ctrl Pts',(-19.6221756985229,23.7809371026034,-41.4592756014488));
#66579=CARTESIAN_POINT('Ctrl Pts',(-19.6169436487515,23.6603520161677,-41.4653631011667));
#66580=CARTESIAN_POINT('Ctrl Pts',(-19.6172666289234,23.5397221657949,-41.4714506008846));
#66581=CARTESIAN_POINT('Ctrl Pts',(-19.6175771074602,23.4237615505545,-41.477302470968));
#66582=CARTESIAN_POINT('Ctrl Pts',(-19.6230205724317,23.3077600242436,-41.4831543410514));
#66583=CARTESIAN_POINT('Ctrl Pts',(-19.6335841519522,23.192205323732,-41.4890062111348));
#66584=CARTESIAN_POINT('Ctrl Pts',(-19.6441461230718,23.0766682174745,-41.4948571902178));
#66585=CARTESIAN_POINT('Ctrl Pts',(-19.6598266210551,22.9615782132978,-41.5007081693008));
#66586=CARTESIAN_POINT('Ctrl Pts',(-19.6805607990657,22.8474190560924,-41.5065591483838));
#66587=CARTESIAN_POINT('Ctrl Pts',(-19.7012968412784,22.73324963488,-41.5124106535261));
#66588=CARTESIAN_POINT('Ctrl Pts',(-19.7270873928964,22.6200116337642,-41.5182621586684));
#66589=CARTESIAN_POINT('Ctrl Pts',(-19.7578164035634,22.5081790150707,-41.5241136638107));
#66590=CARTESIAN_POINT('Ctrl Pts',(-19.7885556186658,22.3963092591992,-41.5299671121105));
#66591=CARTESIAN_POINT('Ctrl Pts',(-19.8242364442935,22.2858462121451,-41.5358205604103));
#66592=CARTESIAN_POINT('Ctrl Pts',(-19.864693058738,22.1772483906579,-41.54167400871));
#66593=CARTESIAN_POINT('Ctrl Pts',(-19.9051956811382,22.0685270698657,-41.5475341136516));
#66594=CARTESIAN_POINT('Ctrl Pts',(-19.9504847882875,21.9616755960297,-41.5533942185932));
#66595=CARTESIAN_POINT('Ctrl Pts',(-20.0003464870739,21.8571323131722,-41.5592543235347));
#66596=CARTESIAN_POINT('Ctrl Pts',(-20.0502417645936,21.7525186269568,-41.5651183748902));
#66597=CARTESIAN_POINT('Ctrl Pts',(-20.1047155715402,21.6502165908703,-41.5709824262457));
#66598=CARTESIAN_POINT('Ctrl Pts',(-20.1635090181477,21.5506382255214,-41.5768464776011));
#66599=CARTESIAN_POINT('Ctrl Pts',(-20.2223891145591,21.4509131015399,-41.5827191713977));
#66600=CARTESIAN_POINT('Ctrl Pts',(-20.2856013316514,21.3539200047846,-41.5885918651943));
#66601=CARTESIAN_POINT('Ctrl Pts',(-20.3528445824797,21.26004044407,-41.5944645589909));
#66602=CARTESIAN_POINT('Ctrl Pts',(-20.3712546597133,21.234337790761,-41.5960724043141));
#66603=CARTESIAN_POINT('Ctrl Pts',(-20.3899666683729,21.2088683177379,-41.5976802496373));
#66604=CARTESIAN_POINT('Ctrl Pts',(-20.4089739362136,21.183639385112,-41.5992880949606));
#66605=CARTESIAN_POINT('Ctrl Pts',(-20.4783937489969,21.091496327294,-41.6051603919293));
#66606=CARTESIAN_POINT('Ctrl Pts',(-20.5519875416169,21.0022559293968,-41.611032688898));
#66607=CARTESIAN_POINT('Ctrl Pts',(-20.6294838957706,20.9163201909905,-41.6169049858667));
#66608=CARTESIAN_POINT('Ctrl Pts',(-20.7068798208039,20.8304958184764,-41.6227696728049));
#66609=CARTESIAN_POINT('Ctrl Pts',(-20.7881679757107,20.7479678931038,-41.6286343597431));
#66610=CARTESIAN_POINT('Ctrl Pts',(-20.8730348581837,20.669107875721,-41.6344990466813));
#66611=CARTESIAN_POINT('Ctrl Pts',(-20.9578144603808,20.5903289609293,-41.6403577021561));
#66612=CARTESIAN_POINT('Ctrl Pts',(-21.0461651684401,20.5152107307009,-41.6462163576309));
#66613=CARTESIAN_POINT('Ctrl Pts',(-21.1377350247873,20.4440895805811,-41.6520750131057));
#66614=CARTESIAN_POINT('Ctrl Pts',(-21.2328816803773,20.3701903756948,-41.6581625128236));
#66615=CARTESIAN_POINT('Ctrl Pts',(-21.3315037920983,20.3006072132542,-41.6642500125415));
#66616=CARTESIAN_POINT('Ctrl Pts',(-21.4331662936495,20.2356733939028,-41.6703375122594));
#66617=CARTESIAN_POINT('Ctrl Pts',(-21.530893731678,20.1732529762484,-41.6761893823428));
#66618=CARTESIAN_POINT('Ctrl Pts',(-21.6314301856473,20.115128912036,-41.6820412524262));
#66619=CARTESIAN_POINT('Ctrl Pts',(-21.7343583565453,20.0615540143871,-41.6878931225096));
#66620=CARTESIAN_POINT('Ctrl Pts',(-21.8372708556935,20.0079872740036,-41.6937441015925));
#66621=CARTESIAN_POINT('Ctrl Pts',(-21.9425739811191,19.9589685137791,-41.6995950806755));
#66622=CARTESIAN_POINT('Ctrl Pts',(-22.0498256976651,19.9147046616029,-41.7054460597585));
#66623=CARTESIAN_POINT('Ctrl Pts',(-22.1570870571728,19.8704368296803,-41.7112975649008));
#66624=CARTESIAN_POINT('Ctrl Pts',(-22.2662969739351,19.8309249133739,-41.717149070043));
#66625=CARTESIAN_POINT('Ctrl Pts',(-22.3769939653576,19.7963274743019,-41.7230005751853));
#66626=CARTESIAN_POINT('Ctrl Pts',(-22.4877277168412,19.7617185461735,-41.7288540234851));
#66627=CARTESIAN_POINT('Ctrl Pts',(-22.5999491305731,19.7320274636421,-41.7347074717849));
#66628=CARTESIAN_POINT('Ctrl Pts',(-22.7131828150561,19.7073625658628,-41.7405609200846));
#66629=CARTESIAN_POINT('Ctrl Pts',(-22.8265452708263,19.682669618739,-41.7464210250262));
#66630=CARTESIAN_POINT('Ctrl Pts',(-22.9409218909,19.6630143530916,-41.7522811299677));
#66631=CARTESIAN_POINT('Ctrl Pts',(-23.0558282708018,19.6484537605835,-41.7581412349092));
#66632=CARTESIAN_POINT('Ctrl Pts',(-23.1708120329589,19.6338833624276,-41.7640052862647));
#66633=CARTESIAN_POINT('Ctrl Pts',(-23.28632585433,19.6244145027907,-41.7698693376201));
#66634=CARTESIAN_POINT('Ctrl Pts',(-23.4018831541704,19.6200520879747,-41.7757333889756));
#66635=CARTESIAN_POINT('Ctrl Pts',(-23.5176107624034,19.61568324383,-41.7816060827721));
#66636=CARTESIAN_POINT('Ctrl Pts',(-23.633381565172,19.6164358620342,-41.7874787765687));
#66637=CARTESIAN_POINT('Ctrl Pts',(-23.7487118424519,19.6222628547763,-41.7933514703652));
#66638=CARTESIAN_POINT('Ctrl Pts',(-23.7802873431325,19.6238581879155,-41.7949593156886));
#66639=CARTESIAN_POINT('Ctrl Pts',(-23.8118298720617,19.6258335848591,-41.796567161012));
#66640=CARTESIAN_POINT('Ctrl Pts',(-23.8433296304232,19.6281874105876,-41.7981750063354));
#66641=CARTESIAN_POINT('Ctrl Pts',(-23.9583754826885,19.6367842348528,-41.8040473033041));
#66642=CARTESIAN_POINT('Ctrl Pts',(-24.0732354915104,19.6504617091263,-41.8099196002728));
#66643=CARTESIAN_POINT('Ctrl Pts',(-24.1874247348063,19.6692087824456,-41.8157918972415));
#66644=CARTESIAN_POINT('Ctrl Pts',(-24.3014659979123,19.6879315610469,-41.8216565841797));
#66645=CARTESIAN_POINT('Ctrl Pts',(-24.4148378199795,19.7117108073719,-41.827521271118));
#66646=CARTESIAN_POINT('Ctrl Pts',(-24.5270582234763,19.7404835570053,-41.8333859580562));
#66647=CARTESIAN_POINT('Ctrl Pts',(-24.6391632153123,19.7692267156667,-41.839244613531));
#66648=CARTESIAN_POINT('Ctrl Pts',(-24.7501187459138,19.8029530608005,-41.8451032690058));
#66649=CARTESIAN_POINT('Ctrl Pts',(-24.859451552075,19.8415483206477,-41.8509619244806));
#66650=CARTESIAN_POINT('Ctrl Pts',(-24.9730549939445,19.881651145339,-41.8570494241985));
#66651=CARTESIAN_POINT('Ctrl Pts',(-25.0849059082626,19.9270109334973,-41.8631369239164));
#66652=CARTESIAN_POINT('Ctrl Pts',(-25.1944887118264,19.9774418196715,-41.8692244236343));
#66653=CARTESIAN_POINT('Ctrl Pts',(-25.2998298797188,20.0259206710484,-41.8750762937177));
#66654=CARTESIAN_POINT('Ctrl Pts',(-25.403074845574,20.0790851558375,-41.8809281638011));
#66655=CARTESIAN_POINT('Ctrl Pts',(-25.5037853456642,20.1367208495881,-41.8867800338845));
#66656=CARTESIAN_POINT('Ctrl Pts',(-25.604480511665,20.1943477677801,-41.8926310129675));
#66657=CARTESIAN_POINT('Ctrl Pts',(-25.7026416204997,20.2564443360485,-41.8984819920504));
#66658=CARTESIAN_POINT('Ctrl Pts',(-25.7978556415216,20.3227505160954,-41.9043329711334));
#66659=CARTESIAN_POINT('Ctrl Pts',(-25.8930782232,20.3890626577058,-41.9101844762757));
#66660=CARTESIAN_POINT('Ctrl Pts',(-25.9853528510759,20.459584927236,-41.9160359814179));
#66661=CARTESIAN_POINT('Ctrl Pts',(-26.0742966736938,20.534014780913,-41.9218874865602));
#66662=CARTESIAN_POINT('Ctrl Pts',(-26.1632700326189,20.6084693511241,-41.9277409348599));
#66663=CARTESIAN_POINT('Ctrl Pts',(-26.2489100700422,20.6868338205726,-41.9335943831597));
#66664=CARTESIAN_POINT('Ctrl Pts',(-26.330868669157,20.7687667963216,-41.9394478314594));
#66665=CARTESIAN_POINT('Ctrl Pts',(-26.412920472996,20.8507929476554,-41.945307936401));
#66666=CARTESIAN_POINT('Ctrl Pts',(-26.4912821896849,20.9363954128342,-41.9511680413425));
#66667=CARTESIAN_POINT('Ctrl Pts',(-26.5656440300273,21.0251974606551,-41.957028146284));
#66668=CARTESIAN_POINT('Ctrl Pts',(-26.640055948415,21.1140593110972,-41.9628921976394));
#66669=CARTESIAN_POINT('Ctrl Pts',(-26.7104623763278,21.2061247070886,-41.9687562489948));
#66670=CARTESIAN_POINT('Ctrl Pts',(-26.7765961684914,21.3009869321489,-41.9746203003502));
#66671=CARTESIAN_POINT('Ctrl Pts',(-26.8428274286634,21.395988965193,-41.9804929941468));
#66672=CARTESIAN_POINT('Ctrl Pts',(-26.9047732651099,21.4937957060384,-41.9863656879434));
#66673=CARTESIAN_POINT('Ctrl Pts',(-26.9622118224166,21.5939747399547,-41.9922383817399));
#66674=CARTESIAN_POINT('Ctrl Pts',(-26.9779375385788,21.6214020836527,-41.9938462270634));
#66675=CARTESIAN_POINT('Ctrl Pts',(-26.993325678056,21.6490071282614,-41.9954540723869));
#66676=CARTESIAN_POINT('Ctrl Pts',(-27.0083723197421,21.6767807460749,-41.9970619177103));
#66677=CARTESIAN_POINT('Ctrl Pts',(-27.0662475677887,21.7836089043874,-42.0032463174493));
#66678=CARTESIAN_POINT('Ctrl Pts',(-27.1192437917329,21.8932593022833,-42.0094307171883));
#66679=CARTESIAN_POINT('Ctrl Pts',(-27.167091389344,22.0052717299383,-42.0156151169273));
#66680=CARTESIAN_POINT('Ctrl Pts',(-27.2148506879968,22.1170774475144,-42.0217881038456));
#66681=CARTESIAN_POINT('Ctrl Pts',(-27.2574801505841,22.2312361925119,-42.0279610907638));
#66682=CARTESIAN_POINT('Ctrl Pts',(-27.294755889838,22.3472630883283,-42.0341340776821));
#66683=CARTESIAN_POINT('Ctrl Pts',(-27.331942379294,22.463012179406,-42.0402922845357));
#66684=CARTESIAN_POINT('Ctrl Pts',(-27.3638005933607,22.5806201732055,-42.0464504913893));
#66685=CARTESIAN_POINT('Ctrl Pts',(-27.3901549413329,22.6995830985704,-42.052608698243));
#66686=CARTESIAN_POINT('Ctrl Pts',(-27.4164708538347,22.8183725270991,-42.0587579239001));
#66687=CARTESIAN_POINT('Ctrl Pts',(-27.4372988102862,22.9385126128449,-42.0649071495573));
#66688=CARTESIAN_POINT('Ctrl Pts',(-27.4525127845195,23.0594838293304,-42.0710563752145));
#66689=CARTESIAN_POINT('Ctrl Pts',(-27.4676988927091,23.1802334739147,-42.077194337898));
#66690=CARTESIAN_POINT('Ctrl Pts',(-27.4772914712536,23.3018108695333,-42.0833323005816));
#66691=CARTESIAN_POINT('Ctrl Pts',(-27.4812155263533,23.4236866017564,-42.0894702632651));
#66692=CARTESIAN_POINT('Ctrl Pts',(-27.4825721859069,23.4658225739292,-42.0915923348221));
#66693=CARTESIAN_POINT('Ctrl Pts',(-27.4832517435385,23.507994117478,-42.093714406379));
#66694=CARTESIAN_POINT('Ctrl Pts',(-27.483252531009,23.5501791140891,-42.095836477936));
#66695=CARTESIAN_POINT('',(-27.4832508841044,23.5538525231951,-43.3458364779651));
#66696=CARTESIAN_POINT('Ctrl Pts',(-27.483252531009,23.5501791146685,-42.0958364779651));
#66697=CARTESIAN_POINT('Ctrl Pts',(-27.4832548023492,23.6718563556103,-42.1019573226462));
#66698=CARTESIAN_POINT('Ctrl Pts',(-27.4776061777862,23.7934277859455,-42.1080781673273));
#66699=CARTESIAN_POINT('Ctrl Pts',(-27.4663618573772,23.914363434166,-42.1141990120083));
#66700=CARTESIAN_POINT('Ctrl Pts',(-27.4551024321348,24.0354615388757,-42.120328079004));
#66701=CARTESIAN_POINT('Ctrl Pts',(-27.4382323502158,24.1559218053875,-42.1264571459996));
#66702=CARTESIAN_POINT('Ctrl Pts',(-27.4158581845192,24.2752228323601,-42.1325862129952));
#66703=CARTESIAN_POINT('Ctrl Pts',(-27.3934308955725,24.3948071171923,-42.1387298323081));
#66704=CARTESIAN_POINT('Ctrl Pts',(-27.3654734665504,24.5132263115375,-42.144873451621));
#66705=CARTESIAN_POINT('Ctrl Pts',(-27.3321431398045,24.6299712118543,-42.1510170709339));
#66706=CARTESIAN_POINT('Ctrl Pts',(-27.2987695721189,24.7468675706085,-42.1571686606419));
#66707=CARTESIAN_POINT('Ctrl Pts',(-27.2600093126576,24.8620849663055,-42.1633202503499));
#66708=CARTESIAN_POINT('Ctrl Pts',(-27.2160681697929,24.9751331258042,-42.1694718400579));
#66709=CARTESIAN_POINT('Ctrl Pts',(-27.172028412201,25.0884349931647,-42.1756372354455));
#66710=CARTESIAN_POINT('Ctrl Pts',(-27.1227846735459,25.1995575690667,-42.1818026308332));
#66711=CARTESIAN_POINT('Ctrl Pts',(-27.0685897512435,25.3080330098923,-42.1879680262208));
#66712=CARTESIAN_POINT('Ctrl Pts',(-27.0452055255798,25.3548383945937,-42.1906282938423));
#66713=CARTESIAN_POINT('Ctrl Pts',(-27.0209000560249,25.4011512922844,-42.1932885614637));
#66714=CARTESIAN_POINT('Ctrl Pts',(-26.9956961240515,25.4469358083337,-42.1959488290852));
#66715=CARTESIAN_POINT('Ctrl Pts',(-26.9400607540866,25.5480009314964,-42.2018211260539));
#66716=CARTESIAN_POINT('Ctrl Pts',(-26.8798815979984,25.646785363983,-42.2076934230227));
#66717=CARTESIAN_POINT('Ctrl Pts',(-26.8153702541408,25.7428526453869,-42.2135657199914));
#66718=CARTESIAN_POINT('Ctrl Pts',(-26.7509425118614,25.8387954312236,-42.2194304069296));
#66719=CARTESIAN_POINT('Ctrl Pts',(-26.6821939747129,25.9320277283877,-42.2252950938678));
#66720=CARTESIAN_POINT('Ctrl Pts',(-26.6093822343018,26.0221373313206,-42.231159780806));
#66721=CARTESIAN_POINT('Ctrl Pts',(-26.5366453762077,26.1121542621677,-42.2370184362808));
#66722=CARTESIAN_POINT('Ctrl Pts',(-26.4598538848487,26.1990545670127,-42.2428770917557));
#66723=CARTESIAN_POINT('Ctrl Pts',(-26.3793083957282,26.2824552910397,-42.2487357472305));
#66724=CARTESIAN_POINT('Ctrl Pts',(-26.2956167288591,26.3691137208055,-42.2548232469484));
#66725=CARTESIAN_POINT('Ctrl Pts',(-26.2078720701821,26.4519932254442,-42.2609107466663));
#66726=CARTESIAN_POINT('Ctrl Pts',(-26.1164577615215,26.530702114963,-42.2669982463842));
#66727=CARTESIAN_POINT('Ctrl Pts',(-26.0285818382629,26.6063644093725,-42.2728501164676));
#66728=CARTESIAN_POINT('Ctrl Pts',(-25.937315408431,26.678172655439,-42.278701986551));
#66729=CARTESIAN_POINT('Ctrl Pts',(-25.8430356531267,26.7458173578359,-42.2845538566345));
#66730=CARTESIAN_POINT('Ctrl Pts',(-25.7487702527725,26.8134517607118,-42.2904048357174));
#66731=CARTESIAN_POINT('Ctrl Pts',(-25.651492774981,26.876923639469,-42.2962558148004));
#66732=CARTESIAN_POINT('Ctrl Pts',(-25.5516114006621,26.9359654075305,-42.3021067938834));
#66733=CARTESIAN_POINT('Ctrl Pts',(-25.4517210460465,26.995012484015,-42.3079582990257));
#66734=CARTESIAN_POINT('Ctrl Pts',(-25.3492266853846,27.0496284476332,-42.313809804168));
#66735=CARTESIAN_POINT('Ctrl Pts',(-25.2445626164815,27.0995908272907,-42.3196613093103));
#66736=CARTESIAN_POINT('Ctrl Pts',(-25.1398637909194,27.1495697983669,-42.3255147576101));
#66737=CARTESIAN_POINT('Ctrl Pts',(-25.0329941972818,27.194891934655,-42.3313682059099));
#66738=CARTESIAN_POINT('Ctrl Pts',(-24.924409031352,27.2353825042255,-42.3372216542097));
#66739=CARTESIAN_POINT('Ctrl Pts',(-24.8157003805099,27.2759191203658,-42.3430817591512));
#66740=CARTESIAN_POINT('Ctrl Pts',(-24.7052726508419,27.3116130583335,-42.3489418640928));
#66741=CARTESIAN_POINT('Ctrl Pts',(-24.5935972494911,27.3423391340604,-42.3548019690343));
#66742=CARTESIAN_POINT('Ctrl Pts',(-24.4818466417466,27.3730859018763,-42.3606660203898));
#66743=CARTESIAN_POINT('Ctrl Pts',(-24.3688470913055,27.3988580541119,-42.3665300717453));
#66744=CARTESIAN_POINT('Ctrl Pts',(-24.2550795539619,27.4195816555452,-42.3723941231008));
#66745=CARTESIAN_POINT('Ctrl Pts',(-24.1411443459788,27.44033579943,-42.3782668168973));
#66746=CARTESIAN_POINT('Ctrl Pts',(-24.0264393001511,27.4560264867828,-42.3841395106939));
#66747=CARTESIAN_POINT('Ctrl Pts',(-23.9114499219983,27.4666316559922,-42.3900122044905));
#66748=CARTESIAN_POINT('Ctrl Pts',(-23.8799677537996,27.4695351739188,-42.3916200498137));
#66749=CARTESIAN_POINT('Ctrl Pts',(-23.8484642667136,27.4720577966671,-42.3932278951369));
#66750=CARTESIAN_POINT('Ctrl Pts',(-23.8169493924268,27.4741997515833,-42.3948357404602));
#66751=CARTESIAN_POINT('Ctrl Pts',(-23.7018483325979,27.4820227648919,-42.4007080374289));
#66752=CARTESIAN_POINT('Ctrl Pts',(-23.5862099470765,27.4847902047025,-42.4065803343976));
#66753=CARTESIAN_POINT('Ctrl Pts',(-23.470515815206,27.4824441669078,-42.4124526313663));
#66754=CARTESIAN_POINT('Ctrl Pts',(-23.354971613742,27.4801011693917,-42.4183173183045));
#66755=CARTESIAN_POINT('Ctrl Pts',(-23.2393722190771,27.4726578806235,-42.4241820052427));
#66756=CARTESIAN_POINT('Ctrl Pts',(-23.1242036658475,27.4601082021648,-42.4300466921809));
#66757=CARTESIAN_POINT('Ctrl Pts',(-23.0091535562656,27.4475714302647,-42.4359053476557));
#66758=CARTESIAN_POINT('Ctrl Pts',(-22.8945338152629,27.4299387588919,-42.4417640031305));
#66759=CARTESIAN_POINT('Ctrl Pts',(-22.7808291353859,27.407256114427,-42.4476226586053));
#66760=CARTESIAN_POINT('Ctrl Pts',(-22.6626830505631,27.3836874658906,-42.4537101583232));
#66761=CARTESIAN_POINT('Ctrl Pts',(-22.5455254249626,27.3546662981129,-42.4597976580411));
#66762=CARTESIAN_POINT('Ctrl Pts',(-22.4298930064545,27.3203033979565,-42.465885157759));
#66763=CARTESIAN_POINT('Ctrl Pts',(-22.3187363868413,27.2872705869959,-42.4717370278424));
#66764=CARTESIAN_POINT('Ctrl Pts',(-22.2089895302267,27.2493020094543,-42.4775888979258));
#66765=CARTESIAN_POINT('Ctrl Pts',(-22.1011167025963,27.2065476987759,-42.4834407680092));
#66766=CARTESIAN_POINT('Ctrl Pts',(-21.9932602995848,27.16379989783,-42.4892917470922));
#66767=CARTESIAN_POINT('Ctrl Pts',(-21.8872777424082,27.1162679648508,-42.4951427261752));
#66768=CARTESIAN_POINT('Ctrl Pts',(-21.7836147952294,27.0641506673974,-42.5009937052582));
#66769=CARTESIAN_POINT('Ctrl Pts',(-21.6799425277543,27.0120286840976,-42.5068452104004));
#66770=CARTESIAN_POINT('Ctrl Pts',(-21.5785906542202,26.9553207024679,-42.5126967155427));
#66771=CARTESIAN_POINT('Ctrl Pts',(-21.4799810996665,26.8942718494808,-42.518548220685));
#66772=CARTESIAN_POINT('Ctrl Pts',(-21.3813387990259,26.8332027234983,-42.5244016689848));
#66773=CARTESIAN_POINT('Ctrl Pts',(-21.2854409794558,26.767790077292,-42.5302551172846));
#66774=CARTESIAN_POINT('Ctrl Pts',(-21.1926806984784,26.6983224246965,-42.5361085655844));
#66775=CARTESIAN_POINT('Ctrl Pts',(-21.0998149289194,26.6287757722956,-42.5419686705259));
#66776=CARTESIAN_POINT('Ctrl Pts',(-21.0100941507763,26.5551651571875,-42.5478287754674));
#66777=CARTESIAN_POINT('Ctrl Pts',(-20.9238784990514,26.4778195148151,-42.553688880409));
#66778=CARTESIAN_POINT('Ctrl Pts',(-20.8376047864811,26.4004217849935,-42.5595529317644));
#66779=CARTESIAN_POINT('Ctrl Pts',(-20.7548411949899,26.3192843081161,-42.5654169831198));
#66780=CARTESIAN_POINT('Ctrl Pts',(-20.6759099045163,26.2347717552402,-42.5712810344753));
#66781=CARTESIAN_POINT('Ctrl Pts',(-20.5968622850767,26.1501346477316,-42.5771537282718));
#66782=CARTESIAN_POINT('Ctrl Pts',(-20.5216585065826,26.062112849817,-42.5830264220684));
#66783=CARTESIAN_POINT('Ctrl Pts',(-20.4505795661531,25.9711029001998,-42.588899115865));
#66784=CARTESIAN_POINT('Ctrl Pts',(-20.4311193412691,25.9461858984053,-42.5905069611883));
#66785=CARTESIAN_POINT('Ctrl Pts',(-20.4119680461269,25.9210450706819,-42.5921148065117));
#66786=CARTESIAN_POINT('Ctrl Pts',(-20.393130857954,25.8956888956146,-42.593722651835));
#66787=CARTESIAN_POINT('Ctrl Pts',(-20.3243322232833,25.8030811131209,-42.5995949488037));
#66788=CARTESIAN_POINT('Ctrl Pts',(-20.2594964801044,25.7072885177101,-42.6054672457724));
#66789=CARTESIAN_POINT('Ctrl Pts',(-20.1989326581651,25.6086849705391,-42.6113395427411));
#66790=CARTESIAN_POINT('Ctrl Pts',(-20.1384473221291,25.5102092057341,-42.6172042296793));
#66791=CARTESIAN_POINT('Ctrl Pts',(-20.0822231124325,25.4089300823247,-42.6230689166175));
#66792=CARTESIAN_POINT('Ctrl Pts',(-20.0305278821194,25.3052532129406,-42.6289336035557));
#66793=CARTESIAN_POINT('Ctrl Pts',(-19.9788858171146,25.2016829687268,-42.6347922590306));
#66794=CARTESIAN_POINT('Ctrl Pts',(-19.9317636502982,25.095720251124,-42.6406509145054));
#66795=CARTESIAN_POINT('Ctrl Pts',(-19.8893847399046,24.9877976652596,-42.6465095699802));
#66796=CARTESIAN_POINT('Ctrl Pts',(-19.845350471944,24.8756595281341,-42.6525970696981));
#66797=CARTESIAN_POINT('Ctrl Pts',(-19.8064378040184,24.7614056805383,-42.658684569416));
#66798=CARTESIAN_POINT('Ctrl Pts',(-19.7728436642594,24.6455475824569,-42.6647720691339));
#66799=CARTESIAN_POINT('Ctrl Pts',(-19.7405498571887,24.5341740186785,-42.6706239392173));
#66800=CARTESIAN_POINT('Ctrl Pts',(-19.7131706300209,24.4213185210852,-42.6764758093007));
#66801=CARTESIAN_POINT('Ctrl Pts',(-19.690830712549,24.3074527838771,-42.6823276793841));
#66802=CARTESIAN_POINT('Ctrl Pts',(-19.6684941965327,24.193604383763,-42.6881786584671));
#66803=CARTESIAN_POINT('Ctrl Pts',(-19.6511955441772,24.0787464554119,-42.6940296375501));
#66804=CARTESIAN_POINT('Ctrl Pts',(-19.6390084834272,23.9633614699852,-42.6998806166331));
#66805=CARTESIAN_POINT('Ctrl Pts',(-19.6268203269432,23.8479661103381,-42.7057321217754));
#66806=CARTESIAN_POINT('Ctrl Pts',(-19.6197447190927,23.732044010534,-42.7115836269177));
#66807=CARTESIAN_POINT('Ctrl Pts',(-19.6178034988114,23.6160826447082,-42.71743513206));
#66808=CARTESIAN_POINT('Ctrl Pts',(-19.6158616338932,23.500082770637,-42.7232885803598));
#66809=CARTESIAN_POINT('Ctrl Pts',(-19.6190575537813,23.3840440177222,-42.7291420286595));
#66810=CARTESIAN_POINT('Ctrl Pts',(-19.6273609911997,23.2684530258104,-42.7349954769593));
#66811=CARTESIAN_POINT('Ctrl Pts',(-19.6356738714294,23.152730581841,-42.7408555819009));
#66812=CARTESIAN_POINT('Ctrl Pts',(-19.6491058328568,23.0374573277903,-42.7467156868424));
#66813=CARTESIAN_POINT('Ctrl Pts',(-19.6675748048108,22.9231140548297,-42.752575791784));
#66814=CARTESIAN_POINT('Ctrl Pts',(-19.6860562144616,22.808693778831,-42.7584398431394));
#66815=CARTESIAN_POINT('Ctrl Pts',(-19.7095813053045,22.695205134767,-42.7643038944949));
#66816=CARTESIAN_POINT('Ctrl Pts',(-19.7380174253758,22.5831162981918,-42.7701679458503));
#66817=CARTESIAN_POINT('Ctrl Pts',(-19.7664954546116,22.4708622650464,-42.7760406396469));
#66818=CARTESIAN_POINT('Ctrl Pts',(-19.7998988396582,22.3600125511299,-42.7819133334435));
#66819=CARTESIAN_POINT('Ctrl Pts',(-19.8380458567064,22.2510179100126,-42.7877860272401));
#66820=CARTESIAN_POINT('Ctrl Pts',(-19.8484898718523,22.221177000533,-42.7893938725634));
#66821=CARTESIAN_POINT('Ctrl Pts',(-19.8592891851295,22.1914750114253,-42.7910017178867));
#66822=CARTESIAN_POINT('Ctrl Pts',(-19.8704394618732,22.1619208814124,-42.79260956321));
#66823=CARTESIAN_POINT('Ctrl Pts',(-19.9111633644607,22.0539810033831,-42.7984818601787));
#66824=CARTESIAN_POINT('Ctrl Pts',(-19.9567088144411,21.9476536460607,-42.8043541571474));
#66825=CARTESIAN_POINT('Ctrl Pts',(-20.0069283198299,21.8434008891616,-42.8102264541161));
#66826=CARTESIAN_POINT('Ctrl Pts',(-20.057082744728,21.7392832355559,-42.8160911410543));
#66827=CARTESIAN_POINT('Ctrl Pts',(-20.1118990016838,21.6372352048653,-42.8219558279925));
#66828=CARTESIAN_POINT('Ctrl Pts',(-20.1711806279119,21.5377013971714,-42.8278205149307));
#66829=CARTESIAN_POINT('Ctrl Pts',(-20.2304012866987,21.4382699537674,-42.8336791704055));
#66830=CARTESIAN_POINT('Ctrl Pts',(-20.2940779700719,21.3413479432545,-42.8395378258803));
#66831=CARTESIAN_POINT('Ctrl Pts',(-20.3619674546744,21.2473571220733,-42.8453964813551));
#66832=CARTESIAN_POINT('Ctrl Pts',(-20.4325087623416,21.1496949366309,-42.851483981073));
#66833=CARTESIAN_POINT('Ctrl Pts',(-20.5075984946643,21.0551980080289,-42.8575714807909));
#66834=CARTESIAN_POINT('Ctrl Pts',(-20.5869127997796,20.9643084810125,-42.8636589805088));
#66835=CARTESIAN_POINT('Ctrl Pts',(-20.6631570758859,20.8769370266079,-42.8695108505922));
#66836=CARTESIAN_POINT('Ctrl Pts',(-20.7433046665563,20.7928992426831,-42.8753627206756));
#66837=CARTESIAN_POINT('Ctrl Pts',(-20.8270261492867,20.7125550372174,-42.881214590759));
#66838=CARTESIAN_POINT('Ctrl Pts',(-20.9107348846602,20.6322230648875,-42.8870655698419));
#66839=CARTESIAN_POINT('Ctrl Pts',(-20.9980161319563,20.555583838973,-42.8929165489249));
#66840=CARTESIAN_POINT('Ctrl Pts',(-21.0885038331717,20.4829601841468,-42.8987675280078));
#66841=CARTESIAN_POINT('Ctrl Pts',(-21.1789996701022,20.4103299997552,-42.9046190331501));
#66842=CARTESIAN_POINT('Ctrl Pts',(-21.2727022116373,20.3417163629236,-42.9104705382924));
#66843=CARTESIAN_POINT('Ctrl Pts',(-21.3692131424786,20.2774011475507,-42.9163220434347));
#66844=CARTESIAN_POINT('Ctrl Pts',(-21.4657561224994,20.2130645744946,-42.9221754917345));
#66845=CARTESIAN_POINT('Ctrl Pts',(-21.5651090024377,20.153029490336,-42.9280289400342));
#66846=CARTESIAN_POINT('Ctrl Pts',(-21.6668460032796,20.0975334801748,-42.933882388334));
#66847=CARTESIAN_POINT('Ctrl Pts',(-21.7686987011828,20.0419743589995,-42.9397424932755));
#66848=CARTESIAN_POINT('Ctrl Pts',(-21.8729405684713,19.9909648129188,-42.9456025982171));
#66849=CARTESIAN_POINT('Ctrl Pts',(-21.979122744789,19.94469568251,-42.9514627031586));
#66850=CARTESIAN_POINT('Ctrl Pts',(-22.0853764281566,19.8983953927378,-42.957326754514));
#66851=CARTESIAN_POINT('Ctrl Pts',(-22.1935726374476,19.8568420231322,-42.9631908058694));
#66852=CARTESIAN_POINT('Ctrl Pts',(-22.3032457847031,19.8201770401044,-42.9690548572249));
#66853=CARTESIAN_POINT('Ctrl Pts',(-22.413080568285,19.7834580202107,-42.9749275510214));
#66854=CARTESIAN_POINT('Ctrl Pts',(-22.5243962381538,19.7516418788758,-42.980800244818));
#66855=CARTESIAN_POINT('Ctrl Pts',(-22.6367153383455,19.7248193802238,-42.9866729386145));
#66856=CARTESIAN_POINT('Ctrl Pts',(-22.6674664291102,19.7174758287782,-42.9882807839379));
#66857=CARTESIAN_POINT('Ctrl Pts',(-22.6982926975374,19.710506287962,-42.9898886292613));
#66858=CARTESIAN_POINT('Ctrl Pts',(-22.7291842802592,19.7039119427076,-42.9914964745847));
#66859=CARTESIAN_POINT('Ctrl Pts',(-22.8420089064447,19.6798275652591,-42.9973687715534));
#66860=CARTESIAN_POINT('Ctrl Pts',(-22.95608314267,19.660671272331,-43.0032410685221));
#66861=CARTESIAN_POINT('Ctrl Pts',(-23.0709385078465,19.6465687501178,-43.0091133654908));
#66862=CARTESIAN_POINT('Ctrl Pts',(-23.1856450295913,19.6324845036533,-43.014978052429));
#66863=CARTESIAN_POINT('Ctrl Pts',(-23.3011302607094,19.6234410536395,-43.0208427393672));
#66864=CARTESIAN_POINT('Ctrl Pts',(-23.4169139552282,19.6195134378308,-43.0267074263054));
#66865=CARTESIAN_POINT('Ctrl Pts',(-23.5325785734653,19.615589861329,-43.0325660817803));
#66866=CARTESIAN_POINT('Ctrl Pts',(-23.6485406339005,19.6167716679362,-43.0384247372551));
#66867=CARTESIAN_POINT('Ctrl Pts',(-23.7643138332285,19.6230822069966,-43.0442833927299));
#66868=CARTESIAN_POINT('Ctrl Pts',(-23.8846092356939,19.629639241271,-43.0503708924478));
#66869=CARTESIAN_POINT('Ctrl Pts',(-24.0047002708198,19.6417338970295,-43.0564583921657));
#66870=CARTESIAN_POINT('Ctrl Pts',(-24.1240398991526,19.6593327102451,-43.0625458918836));
#66871=CARTESIAN_POINT('Ctrl Pts',(-24.2387602331429,19.6762503239342,-43.068397761967));
#66872=CARTESIAN_POINT('Ctrl Pts',(-24.3527858012207,19.6982538518754,-43.0742496320504));
#66873=CARTESIAN_POINT('Ctrl Pts',(-24.4656357399355,19.7252606909094,-43.0801015021338));
#66874=CARTESIAN_POINT('Ctrl Pts',(-24.578468496221,19.7522634179067,-43.0859524812168));
#66875=CARTESIAN_POINT('Ctrl Pts',(-24.6901255771332,19.7842678451091,-43.0918034602998));
#66876=CARTESIAN_POINT('Ctrl Pts',(-24.8001375149892,19.8211405021979,-43.0976544393827));
#66877=CARTESIAN_POINT('Ctrl Pts',(-24.910159343977,19.8580164744934,-43.103505944525));
#66878=CARTESIAN_POINT('Ctrl Pts',(-25.0185353438925,19.8997614154054,-43.1093574496673));
#66879=CARTESIAN_POINT('Ctrl Pts',(-25.1248130631909,19.946192580382,-43.1152089548096));
#66880=CARTESIAN_POINT('Ctrl Pts',(-25.2311260750058,19.9926391641374,-43.1210624031094));
#66881=CARTESIAN_POINT('Ctrl Pts',(-25.3353390420653,20.0437749009407,-43.1269158514091));
#66882=CARTESIAN_POINT('Ctrl Pts',(-25.4370219284316,20.099370000582,-43.1327692997088));
#66883=CARTESIAN_POINT('Ctrl Pts',(-25.5388204503202,20.1550283239242,-43.1386294046504));
#66884=CARTESIAN_POINT('Ctrl Pts',(-25.6380827856848,20.2151559337651,-43.1444895095919));
#66885=CARTESIAN_POINT('Ctrl Pts',(-25.7344057490944,20.2794783537784,-43.1503496145335));
#66886=CARTESIAN_POINT('Ctrl Pts',(-25.8307935799914,20.343844090916,-43.1562136658889));
#66887=CARTESIAN_POINT('Ctrl Pts',(-25.9242377649184,20.4124100192913,-43.1620777172444));
#66888=CARTESIAN_POINT('Ctrl Pts',(-26.0143676157806,20.4848609005355,-43.1679417685998));
#66889=CARTESIAN_POINT('Ctrl Pts',(-26.1046303000512,20.5574185599159,-43.1738144623964));
#66890=CARTESIAN_POINT('Ctrl Pts',(-26.1915685921458,20.6338723274852,-43.179687156193));
#66891=CARTESIAN_POINT('Ctrl Pts',(-26.2748480454947,20.7138695733865,-43.1855598499895));
#66892=CARTESIAN_POINT('Ctrl Pts',(-26.2976485667273,20.7357714811245,-43.1871676953129));
#66893=CARTESIAN_POINT('Ctrl Pts',(-26.3201750632556,20.7579388056919,-43.1887755406363));
#66894=CARTESIAN_POINT('Ctrl Pts',(-26.3424212066077,20.7803638893781,-43.1903833859597));
#66895=CARTESIAN_POINT('Ctrl Pts',(-26.4225631173301,20.8611504340963,-43.1961756616958));
#66896=CARTESIAN_POINT('Ctrl Pts',(-26.4993481242919,20.9455716560126,-43.201967937432));
#66897=CARTESIAN_POINT('Ctrl Pts',(-26.5724214610187,21.0333131278496,-43.2077602131682));
#66898=CARTESIAN_POINT('Ctrl Pts',(-26.645378490056,21.1209149453568,-43.213543269588));
#66899=CARTESIAN_POINT('Ctrl Pts',(-26.7146353328247,21.2118261747569,-43.2193263260078));
#66900=CARTESIAN_POINT('Ctrl Pts',(-26.7798732943023,21.3056949517399,-43.2251093824277));
#66901=CARTESIAN_POINT('Ctrl Pts',(-26.8450519405058,21.3994783819078,-43.2308871808111));
#66902=CARTESIAN_POINT('Ctrl Pts',(-26.9062187231756,21.4962136705681,-43.2366649791945));
#66903=CARTESIAN_POINT('Ctrl Pts',(-26.9630947331139,21.595515437298,-43.2424427775779));
#66904=CARTESIAN_POINT('Ctrl Pts',(-27.0199336962467,21.6947525227457,-43.2482168125297));
#66905=CARTESIAN_POINT('Ctrl Pts',(-27.0724872296379,21.7965523962866,-43.2539908474816));
#66906=CARTESIAN_POINT('Ctrl Pts',(-27.1205198455029,21.900500941924,-43.2597648824334));
#66907=CARTESIAN_POINT('Ctrl Pts',(-27.1685335558155,22.0044085735983,-43.2655366447353));
#66908=CARTESIAN_POINT('Ctrl Pts',(-27.2120297080586,22.1104628101103,-43.2713084070372));
#66909=CARTESIAN_POINT('Ctrl Pts',(-27.2508192808952,22.2182259798914,-43.2770801693391));
#66910=CARTESIAN_POINT('Ctrl Pts',(-27.2896177420185,22.3260138426474,-43.2828532541891));
#66911=CARTESIAN_POINT('Ctrl Pts',(-27.3237073141794,22.4355110240529,-43.2886263390392));
#66912=CARTESIAN_POINT('Ctrl Pts',(-27.3529477084147,22.5462613001855,-43.2943994238892));
#66913=CARTESIAN_POINT('Ctrl Pts',(-27.3821901415692,22.6570192988831,-43.3001729112938));
#66914=CARTESIAN_POINT('Ctrl Pts',(-27.4065826235527,22.7690301520469,-43.3059463986984));
#66915=CARTESIAN_POINT('Ctrl Pts',(-27.4260355702733,22.8818253944067,-43.3117198861029));
#66916=CARTESIAN_POINT('Ctrl Pts',(-27.4455074752284,22.9947305634875,-43.3174990001681));
#66917=CARTESIAN_POINT('Ctrl Pts',(-27.4600301634214,23.1084212272737,-43.3232781142332));
#66918=CARTESIAN_POINT('Ctrl Pts',(-27.4695657285762,23.2224216839291,-43.3290572282983));
#66919=CARTESIAN_POINT('Ctrl Pts',(-27.4787943419729,23.3327524429809,-43.3346503115206));
#66920=CARTESIAN_POINT('Ctrl Pts',(-27.4833520093356,23.4433729935048,-43.3402433947428));
#66921=CARTESIAN_POINT('Ctrl Pts',(-27.4832508841044,23.5538525231951,-43.3458364779651));
#66922=CARTESIAN_POINT('',(-27.4847506190423,23.5486795567491,-44.5958364779651));
#66923=CARTESIAN_POINT('Ctrl Pts',(-27.4838230626506,23.5538530469273,-43.3458364779651));
#66924=CARTESIAN_POINT('Ctrl Pts',(-27.4864830348576,23.8398784059976,-43.3603144177549));
#66925=CARTESIAN_POINT('Ctrl Pts',(-27.3272802131915,25.4327001523438,-43.4410879946694));
#66926=CARTESIAN_POINT('Ctrl Pts',(-25.1574527633787,27.9157603197276,-43.5881572087097));
#66927=CARTESIAN_POINT('Ctrl Pts',(-20.7462374433328,27.2621590790564,-43.7870441200843));
#66928=CARTESIAN_POINT('Ctrl Pts',(-18.9116742482175,23.1976304391361,-43.9859310314592));
#66929=CARTESIAN_POINT('Ctrl Pts',(-21.3395712090345,19.4571316048511,-44.1848179428342));
#66930=CARTESIAN_POINT('Ctrl Pts',(-25.79889687051,19.477863862913,-44.3837048542089));
#66931=CARTESIAN_POINT('Ctrl Pts',(-27.4473585497634,22.0700013317081,-44.5207110325861));
#66932=CARTESIAN_POINT('Ctrl Pts',(-27.4894342879407,23.4617547981006,-44.591421573838));
#66933=CARTESIAN_POINT('Ctrl Pts',(-27.4889934183657,23.5486778605183,-44.5958364779651));
#66934=CARTESIAN_POINT('',(-27.482494567136,23.5474154798039,-45.8458364377547));
#66935=CARTESIAN_POINT('Ctrl Pts',(-27.4832522173837,23.5486801557959,-44.5958364779651));
#66936=CARTESIAN_POINT('Ctrl Pts',(-27.4832979178416,23.6629911717324,-44.6016509300033));
#66937=CARTESIAN_POINT('Ctrl Pts',(-27.4783557921311,23.7775058598441,-44.6074653820416));
#66938=CARTESIAN_POINT('Ctrl Pts',(-27.4683987986737,23.8917475251493,-44.6132798340798));
#66939=CARTESIAN_POINT('Ctrl Pts',(-27.4584541714557,24.0058473062807,-44.6190870647709));
#66940=CARTESIAN_POINT('Ctrl Pts',(-27.4435070938817,24.1196743220027,-44.624894295462));
#66941=CARTESIAN_POINT('Ctrl Pts',(-27.4235825224486,24.2327507241623,-44.6307015261531));
#66942=CARTESIAN_POINT('Ctrl Pts',(-27.4036771122677,24.3457183819277,-44.6365031720911));
#66943=CARTESIAN_POINT('Ctrl Pts',(-27.3788037988945,24.4579364480779,-44.6423048180292));
#66944=CARTESIAN_POINT('Ctrl Pts',(-27.3490393736304,24.5689318382143,-44.6481064639672));
#66945=CARTESIAN_POINT('Ctrl Pts',(-27.319293827833,24.6798568243785,-44.6539044299423));
#66946=CARTESIAN_POINT('Ctrl Pts',(-27.2846634470628,24.7895602698918,-44.6597023959174));
#66947=CARTESIAN_POINT('Ctrl Pts',(-27.245276028477,24.8975796479591,-44.6655003618925));
#66948=CARTESIAN_POINT('Ctrl Pts',(-27.2059012195097,25.0055644443453,-44.6712964716876));
#66949=CARTESIAN_POINT('Ctrl Pts',(-27.1617725435547,25.1118658485073,-44.6770925814827));
#66950=CARTESIAN_POINT('Ctrl Pts',(-27.1130673171308,25.2160375732509,-44.6828886912778));
#66951=CARTESIAN_POINT('Ctrl Pts',(-27.0643653344555,25.3202023601995,-44.6886844150543));
#66952=CARTESIAN_POINT('Ctrl Pts',(-27.011087586258,25.4222373674284,-44.6944801388308));
#66953=CARTESIAN_POINT('Ctrl Pts',(-26.9534587417486,25.5217181012254,-44.7002758626073));
#66954=CARTESIAN_POINT('Ctrl Pts',(-26.895819123162,25.6212174335753,-44.7060726699311));
#66955=CARTESIAN_POINT('Ctrl Pts',(-26.833827003668,25.7181611785204,-44.7118694772548));
#66956=CARTESIAN_POINT('Ctrl Pts',(-26.7677516010664,25.8121518969598,-44.7176662845786));
#66957=CARTESIAN_POINT('Ctrl Pts',(-26.7016069900243,25.906241062791,-44.7234691635717));
#66958=CARTESIAN_POINT('Ctrl Pts',(-26.6313708000516,25.9973706809659,-44.7292720425648));
#66959=CARTESIAN_POINT('Ctrl Pts',(-26.5573539724366,26.0851746064501,-44.7350749215578));
#66960=CARTESIAN_POINT('Ctrl Pts',(-26.483295396102,26.1730280571786,-44.7408810736278));
#66961=CARTESIAN_POINT('Ctrl Pts',(-26.4054522228431,26.2575517709989,-44.7466872256978));
#66962=CARTESIAN_POINT('Ctrl Pts',(-26.3241725384107,26.33841622781,-44.7524933777678));
#66963=CARTESIAN_POINT('Ctrl Pts',(-26.2427648856999,26.4194079991572,-44.7583086711538));
#66964=CARTESIAN_POINT('Ctrl Pts',(-26.1579102299989,26.4967287260163,-44.7641239645399));
#66965=CARTESIAN_POINT('Ctrl Pts',(-26.069990189229,26.5700888082497,-44.7699392579259));
#66966=CARTESIAN_POINT('Ctrl Pts',(-26.0118362765209,26.6186121685794,-44.7737857309369));
#66967=CARTESIAN_POINT('Ctrl Pts',(-25.9523418936925,26.6654035933763,-44.7776322039478));
#66968=CARTESIAN_POINT('Ctrl Pts',(-25.8916239831666,26.7103899853867,-44.7814786769588));
#66969=CARTESIAN_POINT('Ctrl Pts',(-25.798927738864,26.7790693840677,-44.7873509739275));
#66970=CARTESIAN_POINT('Ctrl Pts',(-25.7030517842149,26.8437817959317,-44.7932232708962));
#66971=CARTESIAN_POINT('Ctrl Pts',(-25.604370377764,26.9042186726172,-44.7990955678649));
#66972=CARTESIAN_POINT('Ctrl Pts',(-25.5058168545787,26.9645772279102,-44.8049602548031));
#66973=CARTESIAN_POINT('Ctrl Pts',(-25.4044654588489,27.0206710526877,-44.8108249417413));
#66974=CARTESIAN_POINT('Ctrl Pts',(-25.3007221475745,27.0722328161194,-44.8166896286795));
#66975=CARTESIAN_POINT('Ctrl Pts',(-25.1970855298013,27.1237415515053,-44.8225482841544));
#66976=CARTESIAN_POINT('Ctrl Pts',(-25.091062257378,27.1707273135183,-44.8284069396292));
#66977=CARTESIAN_POINT('Ctrl Pts',(-24.9830852225184,27.2129673008382,-44.834265595104));
#66978=CARTESIAN_POINT('Ctrl Pts',(-24.8708905095722,27.2568572192673,-44.8403530948219));
#66979=CARTESIAN_POINT('Ctrl Pts',(-24.7565866790089,27.2956228191477,-44.8464405945398));
#66980=CARTESIAN_POINT('Ctrl Pts',(-24.6406854438209,27.3290678307199,-44.8525280942577));
#66981=CARTESIAN_POINT('Ctrl Pts',(-24.5292704126494,27.3612182819278,-44.8583799643411));
#66982=CARTESIAN_POINT('Ctrl Pts',(-24.4163797735725,27.3884522501689,-44.8642318344245));
#66983=CARTESIAN_POINT('Ctrl Pts',(-24.3024853809174,27.4106456127871,-44.8700837045079));
#66984=CARTESIAN_POINT('Ctrl Pts',(-24.1886083297191,27.432835596264,-44.8759346835909));
#66985=CARTESIAN_POINT('Ctrl Pts',(-24.0737282344589,27.4499864210675,-44.8817856626739));
#66986=CARTESIAN_POINT('Ctrl Pts',(-23.9583276607807,27.4620249802169,-44.8876366417569));
#66987=CARTESIAN_POINT('Ctrl Pts',(-23.8429167114804,27.4740646217485,-44.8934881468992));
#66988=CARTESIAN_POINT('Ctrl Pts',(-23.7269856019121,27.4809910410066,-44.8993396520415));
#66989=CARTESIAN_POINT('Ctrl Pts',(-23.6110218339123,27.4827830264149,-44.9051911571838));
#66990=CARTESIAN_POINT('Ctrl Pts',(-23.4950195568699,27.4845756069024,-44.9110446054835));
#66991=CARTESIAN_POINT('Ctrl Pts',(-23.3789850129459,27.4812303568041,-44.9168980537833));
#66992=CARTESIAN_POINT('Ctrl Pts',(-23.2634048026322,27.4727781696387,-44.9227515020831));
#66993=CARTESIAN_POINT('Ctrl Pts',(-23.1476931525214,27.4643163705011,-44.9286116070246));
#66994=CARTESIAN_POINT('Ctrl Pts',(-23.032437279817,27.4507360724773,-44.9344717119662));
#66995=CARTESIAN_POINT('Ctrl Pts',(-22.9181178696736,27.4321199649114,-44.9403318169077));
#66996=CARTESIAN_POINT('Ctrl Pts',(-22.8037214725622,27.4134913205621,-44.9461958682632));
#66997=CARTESIAN_POINT('Ctrl Pts',(-22.6902631974396,27.389820198135,-44.9520599196187));
#66998=CARTESIAN_POINT('Ctrl Pts',(-22.5782110487595,27.3612398519898,-44.9579239709741));
#66999=CARTESIAN_POINT('Ctrl Pts',(-22.4659937575806,27.3326173841197,-44.9637966647707));
#67000=CARTESIAN_POINT('Ctrl Pts',(-22.3551871230178,27.2990713717673,-44.9696693585673));
#67001=CARTESIAN_POINT('Ctrl Pts',(-22.2462416644037,27.2607841186758,-44.9755420523638));
#67002=CARTESIAN_POINT('Ctrl Pts',(-22.2164142202711,27.2503017092472,-44.9771498976871));
#67003=CARTESIAN_POINT('Ctrl Pts',(-22.1867261536364,27.2394641807614,-44.9787577430104));
#67004=CARTESIAN_POINT('Ctrl Pts',(-22.1571863976369,27.2282758793828,-44.9803655883337));
#67005=CARTESIAN_POINT('Ctrl Pts',(-22.0492990174886,27.1874131002841,-44.9862378853024));
#67006=CARTESIAN_POINT('Ctrl Pts',(-21.9430303616688,27.1417308529738,-44.9921101822711));
#67007=CARTESIAN_POINT('Ctrl Pts',(-21.8388423197003,27.0913772239753,-44.9979824792398));
#67008=CARTESIAN_POINT('Ctrl Pts',(-21.7347892971598,27.041088849281,-45.003847166178));
#67009=CARTESIAN_POINT('Ctrl Pts',(-21.6328118952361,26.9861413098332,-45.0097118531162));
#67010=CARTESIAN_POINT('Ctrl Pts',(-21.5333544608102,26.9267316404204,-45.0155765400544));
#67011=CARTESIAN_POINT('Ctrl Pts',(-21.4339993121295,26.8673830701335,-45.0214351955292));
#67012=CARTESIAN_POINT('Ctrl Pts',(-21.337159328819,26.8035817083951,-45.027293851004));
#67013=CARTESIAN_POINT('Ctrl Pts',(-21.2432559539608,26.735571321129,-45.0331525064788));
#67014=CARTESIAN_POINT('Ctrl Pts',(-21.1456846305716,26.6649043882335,-45.0392400061967));
#67015=CARTESIAN_POINT('Ctrl Pts',(-21.0512844148706,26.5896931078885,-45.0453275059146));
#67016=CARTESIAN_POINT('Ctrl Pts',(-20.9604970344649,26.5102619006947,-45.0514150056325));
#67017=CARTESIAN_POINT('Ctrl Pts',(-20.873223772869,26.4339052474536,-45.0572668757159));
#67018=CARTESIAN_POINT('Ctrl Pts',(-20.7892892022547,26.3536495730555,-45.0631187457993));
#67019=CARTESIAN_POINT('Ctrl Pts',(-20.7090528063624,26.2698247629052,-45.0689706158827));
#67020=CARTESIAN_POINT('Ctrl Pts',(-20.6288286271908,26.1860127158445,-45.0748215949657));
#67021=CARTESIAN_POINT('Ctrl Pts',(-20.5523017889219,26.0986329120971,-45.0806725740486));
#67022=CARTESIAN_POINT('Ctrl Pts',(-20.4797946448731,26.0080518248136,-45.0865235531316));
#67023=CARTESIAN_POINT('Ctrl Pts',(-20.4072809817341,25.9174625934184,-45.0923750582739));
#67024=CARTESIAN_POINT('Ctrl Pts',(-20.3387879896089,25.8236718290587,-45.0982265634162));
#67025=CARTESIAN_POINT('Ctrl Pts',(-20.2745970295616,25.7270782094527,-45.1040780685585));
#67026=CARTESIAN_POINT('Ctrl Pts',(-20.2103847530942,25.6304525132088,-45.1099315168582));
#67027=CARTESIAN_POINT('Ctrl Pts',(-20.150477578085,25.5310224550563,-45.115784965158));
#67028=CARTESIAN_POINT('Ctrl Pts',(-20.0951125414928,25.4292141194099,-45.1216384134577));
#67029=CARTESIAN_POINT('Ctrl Pts',(-20.0396845428315,25.3272900055784,-45.1274985183993));
#67030=CARTESIAN_POINT('Ctrl Pts',(-19.9888091901727,25.2229825792895,-45.1333586233408));
#67031=CARTESIAN_POINT('Ctrl Pts',(-19.9426767462872,25.1167409461248,-45.1392187282823));
#67032=CARTESIAN_POINT('Ctrl Pts',(-19.8965132350882,25.0104277658695,-45.1450827796378));
#67033=CARTESIAN_POINT('Ctrl Pts',(-19.8550991400046,24.9021781702167,-45.1509468309932));
#67034=CARTESIAN_POINT('Ctrl Pts',(-19.8185753281554,24.7924579287959,-45.1568108823487));
#67035=CARTESIAN_POINT('Ctrl Pts',(-19.7819976874983,24.6825759816416,-45.1626835761452));
#67036=CARTESIAN_POINT('Ctrl Pts',(-19.7503248271257,24.5712194590503,-45.1685562699418));
#67037=CARTESIAN_POINT('Ctrl Pts',(-19.7236468966377,24.458865933397,-45.1744289637384));
#67038=CARTESIAN_POINT('Ctrl Pts',(-19.7163429255371,24.4281054175168,-45.1760368090617));
#67039=CARTESIAN_POINT('Ctrl Pts',(-19.7094130615039,24.397270205359,-45.1776446543851));
#67040=CARTESIAN_POINT('Ctrl Pts',(-19.7028584767764,24.3663701618082,-45.1792524997085));
#67041=CARTESIAN_POINT('Ctrl Pts',(-19.6789193157971,24.2535146343293,-45.1851247966772));
#67042=CARTESIAN_POINT('Ctrl Pts',(-19.6599098434085,24.1394158399071,-45.1909970936459));
#67043=CARTESIAN_POINT('Ctrl Pts',(-19.6459551428019,24.0245424209907,-45.1968693906147));
#67044=CARTESIAN_POINT('Ctrl Pts',(-19.6320185263791,23.9098178689022,-45.2027340775528));
#67045=CARTESIAN_POINT('Ctrl Pts',(-19.6231237043712,23.7943210951986,-45.208598764491));
#67046=CARTESIAN_POINT('Ctrl Pts',(-19.6193450964312,23.6785324420225,-45.2144634514292));
#67047=CARTESIAN_POINT('Ctrl Pts',(-19.6155703745528,23.5628628702274,-45.220322106904));
#67048=CARTESIAN_POINT('Ctrl Pts',(-19.6169014143407,23.4469024267117,-45.2261807623789));
#67049=CARTESIAN_POINT('Ctrl Pts',(-19.6233609392853,23.3311374444271,-45.2320394178537));
#67050=CARTESIAN_POINT('Ctrl Pts',(-19.6300727789637,23.2108505799699,-45.2381269175716));
#67051=CARTESIAN_POINT('Ctrl Pts',(-19.6423219725357,23.0907752091715,-45.2442144172895));
#67052=CARTESIAN_POINT('Ctrl Pts',(-19.6600743520048,22.9714583279669,-45.2503019170074));
#67053=CARTESIAN_POINT('Ctrl Pts',(-19.6771395878385,22.8567598606287,-45.2561537870908));
#67054=CARTESIAN_POINT('Ctrl Pts',(-19.6992898396032,22.7427627038041,-45.2620056571742));
#67055=CARTESIAN_POINT('Ctrl Pts',(-19.7264418853739,22.6299476142415,-45.2678575272576));
#67056=CARTESIAN_POINT('Ctrl Pts',(-19.7535897969987,22.5171497018023,-45.2737085063406));
#67057=CARTESIAN_POINT('Ctrl Pts',(-19.785737891684,22.4055339005623,-45.2795594854235));
#67058=CARTESIAN_POINT('Ctrl Pts',(-19.8227520950531,22.2955695060498,-45.2854104645065));
#67059=CARTESIAN_POINT('Ctrl Pts',(-19.8597696263553,22.1855952246798,-45.2912619696488));
#67060=CARTESIAN_POINT('Ctrl Pts',(-19.9016540041879,22.0772730370034,-45.2971134747911));
#67061=CARTESIAN_POINT('Ctrl Pts',(-19.9482219018805,21.9710551590127,-45.3029649799334));
#67062=CARTESIAN_POINT('Ctrl Pts',(-19.9948052637582,21.8648020083769,-45.3088184282331));
#67063=CARTESIAN_POINT('Ctrl Pts',(-20.0460750722064,21.760654935333,-45.3146718765329));
#67064=CARTESIAN_POINT('Ctrl Pts',(-20.1018009837828,21.6590436797407,-45.3205253248327));
#67065=CARTESIAN_POINT('Ctrl Pts',(-20.1575902678212,21.5573168700864,-45.3263854297742));
#67066=CARTESIAN_POINT('Ctrl Pts',(-20.2178455707824,21.4581319964804,-45.3322455347157));
#67067=CARTESIAN_POINT('Ctrl Pts',(-20.2822918976991,21.36189189079,-45.3381056396573));
#67068=CARTESIAN_POINT('Ctrl Pts',(-20.3467816251835,21.2655869734118,-45.3439696910127));
#67069=CARTESIAN_POINT('Ctrl Pts',(-20.415467752184,21.1722311048856,-45.3498337423682));
#67070=CARTESIAN_POINT('Ctrl Pts',(-20.4880345635459,21.0821945673122,-45.3556977937236));
#67071=CARTESIAN_POINT('Ctrl Pts',(-20.560708323902,20.9920253338553,-45.3615704875202));
#67072=CARTESIAN_POINT('Ctrl Pts',(-20.6372739109862,20.90518550381,-45.3674431813167));
#67073=CARTESIAN_POINT('Ctrl Pts',(-20.7173782648272,20.8220090696618,-45.3733158751133));
#67074=CARTESIAN_POINT('Ctrl Pts',(-20.7393094969274,20.799236753363,-45.3749237204367));
#67075=CARTESIAN_POINT('Ctrl Pts',(-20.7615057929887,20.7767388031124,-45.3765315657601));
#67076=CARTESIAN_POINT('Ctrl Pts',(-20.7839594871627,20.7545215375217,-45.3781394110835));
#67077=CARTESIAN_POINT('Ctrl Pts',(-20.8659666045865,20.6733779228448,-45.3840117080522));
#67078=CARTESIAN_POINT('Ctrl Pts',(-20.9516844090171,20.595709699402,-45.3898840050209));
#67079=CARTESIAN_POINT('Ctrl Pts',(-21.0407862364668,20.5218754228919,-45.3957563019896));
#67080=CARTESIAN_POINT('Ctrl Pts',(-21.1297725950243,20.4481368297405,-45.4016209889278));
#67081=CARTESIAN_POINT('Ctrl Pts',(-21.2221339402012,20.3782225643031,-45.407485675866));
#67082=CARTESIAN_POINT('Ctrl Pts',(-21.317506379071,20.3124548823735,-45.4133503628042));
#67083=CARTESIAN_POINT('Ctrl Pts',(-21.4127807333576,20.2467548383879,-45.419209018279));
#67084=CARTESIAN_POINT('Ctrl Pts',(-21.5110596835321,20.1851931288619,-45.4250676737538));
#67085=CARTESIAN_POINT('Ctrl Pts',(-21.6119463525326,20.1280517550267,-45.4309263292286));
#67086=CARTESIAN_POINT('Ctrl Pts',(-21.7167737436844,20.0686783887998,-45.4370138289465));
#67087=CARTESIAN_POINT('Ctrl Pts',(-21.8244163761972,20.0140780125992,-45.4431013286644));
#67088=CARTESIAN_POINT('Ctrl Pts',(-21.9343955839625,19.9645175548077,-45.4491888283824));
#67089=CARTESIAN_POINT('Ctrl Pts',(-22.0401178123885,19.9168754400298,-45.4550406984658));
#67090=CARTESIAN_POINT('Ctrl Pts',(-22.1479986831924,19.8738905225356,-45.4608925685492));
#67091=CARTESIAN_POINT('Ctrl Pts',(-22.2575887426771,19.8357526557265,-45.4667444386326));
#67092=CARTESIAN_POINT('Ctrl Pts',(-22.3671621160788,19.7976205957544,-45.4725954177156));
#67093=CARTESIAN_POINT('Ctrl Pts',(-22.4784437704118,19.7643342549019,-45.4784463967986));
#67094=CARTESIAN_POINT('Ctrl Pts',(-22.5909664065899,19.7360345082742,-45.4842973758815));
#67095=CARTESIAN_POINT('Ctrl Pts',(-22.7034991596359,19.7077322172268,-45.4901488810238));
#67096=CARTESIAN_POINT('Ctrl Pts',(-22.8172727154081,19.6844175125014,-45.4960003861662));
#67097=CARTESIAN_POINT('Ctrl Pts',(-22.931807521168,19.6661806002085,-45.5018518913085));
#67098=CARTESIAN_POINT('Ctrl Pts',(-23.0463803614432,19.6479376318341,-45.5077053396083));
#67099=CARTESIAN_POINT('Ctrl Pts',(-23.161714546348,19.6347758738111,-45.513558787908));
#67100=CARTESIAN_POINT('Ctrl Pts',(-23.2773240181326,19.6267338269491,-45.5194122362078));
#67101=CARTESIAN_POINT('Ctrl Pts',(-23.3930649629909,19.6186826345334,-45.5252723411494));
#67102=CARTESIAN_POINT('Ctrl Pts',(-23.5090814069584,19.6157628029639,-45.5311324460909));
#67103=CARTESIAN_POINT('Ctrl Pts',(-23.6248857943885,19.6179607220621,-45.5369925510324));
#67104=CARTESIAN_POINT('Ctrl Pts',(-23.7407681688258,19.6201601213213,-45.5428566023879));
#67105=CARTESIAN_POINT('Ctrl Pts',(-23.8564377908205,19.6274841078252,-45.5487206537434));
#67106=CARTESIAN_POINT('Ctrl Pts',(-23.9714124784033,19.6398672182899,-45.5545847050988));
#67107=CARTESIAN_POINT('Ctrl Pts',(-24.0865566157241,19.6522685789875,-45.5604573988954));
#67108=CARTESIAN_POINT('Ctrl Pts',(-24.2010033674262,19.6697438824968,-45.566330092692));
#67109=CARTESIAN_POINT('Ctrl Pts',(-24.3142808961455,19.6921766306376,-45.5722027864886));
#67110=CARTESIAN_POINT('Ctrl Pts',(-24.345294388606,19.6983183418242,-45.5738106318118));
#67111=CARTESIAN_POINT('Ctrl Pts',(-24.3762203306147,19.7048313622488,-45.5754184771351));
#67112=CARTESIAN_POINT('Ctrl Pts',(-24.4070492625013,19.711712657982,-45.5770263224584));
#67113=CARTESIAN_POINT('Ctrl Pts',(-24.5196450704724,19.7368450581514,-45.5828986194271));
#67114=CARTESIAN_POINT('Ctrl Pts',(-24.6313227571216,19.7669779178528,-45.5887709163958));
#67115=CARTESIAN_POINT('Ctrl Pts',(-24.7416040877902,19.8020302237477,-45.5946432133645));
#67116=CARTESIAN_POINT('Ctrl Pts',(-24.851742502613,19.8370371046381,-45.6005079003027));
#67117=CARTESIAN_POINT('Ctrl Pts',(-24.960487769708,19.876950629652,-45.6063725872409));
#67118=CARTESIAN_POINT('Ctrl Pts',(-25.0673720703158,19.9216388424828,-45.6122372741791));
#67119=CARTESIAN_POINT('Ctrl Pts',(-25.1741464471114,19.9662810962841,-45.618095929654));
#67120=CARTESIAN_POINT('Ctrl Pts',(-25.2790632851435,20.0156881122298,-45.6239545851288));
#67121=CARTESIAN_POINT('Ctrl Pts',(-25.3816708031678,20.0696784246089,-45.6298132406036));
#67122=CARTESIAN_POINT('Ctrl Pts',(-25.4882862612215,20.1257776461435,-45.6359007403215));
#67123=CARTESIAN_POINT('Ctrl Pts',(-25.5924078799858,20.1868253809205,-45.6419882400394));
#67124=CARTESIAN_POINT('Ctrl Pts',(-25.69355234881,20.2525632052186,-45.6480757397573));
#67125=CARTESIAN_POINT('Ctrl Pts',(-25.7907818056711,20.3157565070968,-45.6539276098407));
#67126=CARTESIAN_POINT('Ctrl Pts',(-25.8852599220345,20.3832833235902,-45.6597794799241));
#67127=CARTESIAN_POINT('Ctrl Pts',(-25.9765840222712,20.4548681455744,-45.6656313500075));
#67128=CARTESIAN_POINT('Ctrl Pts',(-26.0678942175833,20.5264420681185,-45.6714823290905));
#67129=CARTESIAN_POINT('Ctrl Pts',(-26.1560510263601,20.602072512681,-45.6773333081735));
#67130=CARTESIAN_POINT('Ctrl Pts',(-26.2406833330455,20.6814424816665,-45.6831842872565));
#67131=CARTESIAN_POINT('Ctrl Pts',(-26.3253232489896,20.7608195867758,-45.6890357923987));
#67132=CARTESIAN_POINT('Ctrl Pts',(-26.406437731353,20.8439366018829,-45.694887297541));
#67133=CARTESIAN_POINT('Ctrl Pts',(-26.4836916696365,20.9304388314498,-45.7007388026833));
#67134=CARTESIAN_POINT('Ctrl Pts',(-26.5609712622708,21.0169697865237,-45.7065922509831));
#67135=CARTESIAN_POINT('Ctrl Pts',(-26.6343874864306,21.1068878832111,-45.7124456992828));
#67136=CARTESIAN_POINT('Ctrl Pts',(-26.7036452159199,21.1998050042919,-45.7182991475826));
#67137=CARTESIAN_POINT('Ctrl Pts',(-26.772981706487,21.2928277923163,-45.7241592525241));
#67138=CARTESIAN_POINT('Ctrl Pts',(-26.8381500160266,21.3888560804348,-45.7300193574656));
#67139=CARTESIAN_POINT('Ctrl Pts',(-26.8988980505145,21.4874723230232,-45.7358794624072));
#67140=CARTESIAN_POINT('Ctrl Pts',(-26.9596869950014,21.5861549774786,-45.7417435137626));
#67141=CARTESIAN_POINT('Ctrl Pts',(-27.0160495365432,21.6874286963868,-45.747607565118));
#67142=CARTESIAN_POINT('Ctrl Pts',(-27.0677801107037,21.7908524262868,-45.7534716164735));
#67143=CARTESIAN_POINT('Ctrl Pts',(-27.1195869254044,21.8944285821198,-45.7593443102701));
#67144=CARTESIAN_POINT('Ctrl Pts',(-27.1667479803943,22.0001606969201,-45.7652170040666));
#67145=CARTESIAN_POINT('Ctrl Pts',(-27.2091062394496,22.107588833792,-45.7710896978632));
#67146=CARTESIAN_POINT('Ctrl Pts',(-27.2207032222119,22.1370008606145,-45.7726975431866));
#67147=CARTESIAN_POINT('Ctrl Pts',(-27.2319404915516,22.166539938157,-45.7743053885099));
#67148=CARTESIAN_POINT('Ctrl Pts',(-27.2428154866116,22.1961964678728,-45.7759132338333));
#67149=CARTESIAN_POINT('Ctrl Pts',(-27.288696711522,22.3213163325201,-45.7826966771815));
#67150=CARTESIAN_POINT('Ctrl Pts',(-27.3282525808161,22.448873430684,-45.7894801205297));
#67151=CARTESIAN_POINT('Ctrl Pts',(-27.3612536578878,22.5782651777892,-45.7962635638779));
#67152=CARTESIAN_POINT('Ctrl Pts',(-27.3941183897617,22.7071223379985,-45.8030189811734));
#67153=CARTESIAN_POINT('Ctrl Pts',(-27.420482277308,22.8377988841297,-45.8097743984689));
#67154=CARTESIAN_POINT('Ctrl Pts',(-27.4401653876646,22.9696778397244,-45.8165298157645));
#67155=CARTESIAN_POINT('Ctrl Pts',(-27.4596999042476,23.1005612010595,-45.8232342343646));
#67156=CARTESIAN_POINT('Ctrl Pts',(-27.4726540447025,23.2326287353507,-45.8299386529647));
#67157=CARTESIAN_POINT('Ctrl Pts',(-27.4788993718126,23.365257921968,-45.8366430715649));
#67158=CARTESIAN_POINT('Ctrl Pts',(-27.4817539829892,23.4258800081761,-45.8397075240638));
#67159=CARTESIAN_POINT('Ctrl Pts',(-27.4832076421927,23.4866191808702,-45.8427719765627));
#67160=CARTESIAN_POINT('Ctrl Pts',(-27.4832515079284,23.5474147613741,-45.8458364290615));
#67161=CARTESIAN_POINT('',(-27.4786603534827,23.5529148598696,-47.095836477965));
#67162=CARTESIAN_POINT('Ctrl Pts',(-27.4789932982812,23.5474188029378,-45.845836477965));
#67163=CARTESIAN_POINT('Ctrl Pts',(-27.4733443827607,24.3993354066055,-45.8888243670461));
#67164=CARTESIAN_POINT('Ctrl Pts',(-26.7819451567561,26.5734232824688,-45.998107893252));
#67165=CARTESIAN_POINT('Ctrl Pts',(-23.1916612413879,28.1883731768075,-46.1736870565831));
#67166=CARTESIAN_POINT('Ctrl Pts',(-19.454290019253,25.7556644952009,-46.3725739679577));
#67167=CARTESIAN_POINT('Ctrl Pts',(-19.4807610656983,21.2963692072287,-46.571460879333));
#67168=CARTESIAN_POINT('Ctrl Pts',(-23.2467497334191,18.9082015966501,-46.7703477907076));
#67169=CARTESIAN_POINT('Ctrl Pts',(-26.8015964030055,20.5582290572362,-46.9451396569184));
#67170=CARTESIAN_POINT('Ctrl Pts',(-27.4734779850077,22.7164226323347,-47.0536358860042));
#67171=CARTESIAN_POINT('Ctrl Pts',(-27.4786603534827,23.5529148598696,-47.095836477965));
#67172=CARTESIAN_POINT('',(-27.4887212107966,23.5520805994482,-48.345836477965));
#67173=CARTESIAN_POINT('Ctrl Pts',(-27.4786603534827,23.5529148598696,-47.095836477965));
#67174=CARTESIAN_POINT('Ctrl Pts',(-27.4816193025558,24.0305223308889,-47.1199315231292));
#67175=CARTESIAN_POINT('Ctrl Pts',(-27.1794543469686,25.8186135203327,-47.2103222054181));
#67176=CARTESIAN_POINT('Ctrl Pts',(-24.5097012594312,28.1021981564742,-47.3670085248325));
#67177=CARTESIAN_POINT('Ctrl Pts',(-20.2392470151605,26.817972425073,-47.5658954362071));
#67178=CARTESIAN_POINT('Ctrl Pts',(-19.0113261136081,22.530989168614,-47.7647823475823));
#67179=CARTESIAN_POINT('Ctrl Pts',(-21.9542937527826,19.1806225235446,-47.963669258957));
#67180=CARTESIAN_POINT('Ctrl Pts',(-26.2484742764648,19.8281824805853,-48.1573539690847));
#67181=CARTESIAN_POINT('Ctrl Pts',(-27.4817984742678,22.3490190787578,-48.2847430420873));
#67182=CARTESIAN_POINT('Ctrl Pts',(-27.4887212107966,23.5520805994482,-48.345836477965));
#67183=CARTESIAN_POINT('',(-27.4832509287299,23.5467016283086,-49.595836477965));
#67184=CARTESIAN_POINT('Ctrl Pts',(-27.4887212107966,23.5520805994482,-48.345836477965));
#67185=CARTESIAN_POINT('Ctrl Pts',(-27.4893106925975,23.6545231622795,-48.3510386792123));
#67186=CARTESIAN_POINT('Ctrl Pts',(-27.4856616780405,23.7569230546521,-48.3562408804595));
#67187=CARTESIAN_POINT('Ctrl Pts',(-27.3754023991223,25.1595582326159,-48.4277387188318));
#67188=CARTESIAN_POINT('Ctrl Pts',(-25.7503914835099,27.6490498461281,-48.5603299930818));
#67189=CARTESIAN_POINT('Ctrl Pts',(-21.2911339543954,27.6168400551349,-48.7592169044564));
#67190=CARTESIAN_POINT('Ctrl Pts',(-18.9078148561469,23.8477811198626,-48.9581038158317));
#67191=CARTESIAN_POINT('Ctrl Pts',(-20.7905023679254,19.8053186383279,-49.1569907272063));
#67192=CARTESIAN_POINT('Ctrl Pts',(-25.2091662919772,19.204132886764,-49.3558776385813));
#67193=CARTESIAN_POINT('Ctrl Pts',(-27.337905242507,21.6993486153379,-49.5021595555008));
#67194=CARTESIAN_POINT('Ctrl Pts',(-27.4868110529832,23.2763131213276,-49.5821458352954));
#67195=CARTESIAN_POINT('Ctrl Pts',(-27.4842993531624,23.5467006817397,-49.595836477965));
#67196=CARTESIAN_POINT('',(-27.4832525273076,23.5500667762137,-50.845836477928));
#67197=CARTESIAN_POINT('Ctrl Pts',(-27.4832509287299,23.5467016283086,-49.595836477965));
#67198=CARTESIAN_POINT('Ctrl Pts',(-27.483353921989,23.6607774786029,-49.6016141195103));
#67199=CARTESIAN_POINT('Ctrl Pts',(-27.478489605921,23.7750111715627,-49.6073917610556));
#67200=CARTESIAN_POINT('Ctrl Pts',(-27.4686435306552,23.8889278618572,-49.6131694026009));
#67201=CARTESIAN_POINT('Ctrl Pts',(-27.4586683176372,24.0043386444607,-49.6190228217147));
#67202=CARTESIAN_POINT('Ctrl Pts',(-27.4435796743107,24.1194236090951,-49.6248762408284));
#67203=CARTESIAN_POINT('Ctrl Pts',(-27.4234171929912,24.2336883417597,-49.6307296599422));
#67204=CARTESIAN_POINT('Ctrl Pts',(-27.4035424495562,24.3463224074482,-49.6364995451691));
#67205=CARTESIAN_POINT('Ctrl Pts',(-27.3787378179568,24.4581590660768,-49.642269430396));
#67206=CARTESIAN_POINT('Ctrl Pts',(-27.3490933288047,24.5687306110897,-49.648039315623));
#67207=CARTESIAN_POINT('Ctrl Pts',(-27.3194550330856,24.6792790550987,-49.6538079953848));
#67208=CARTESIAN_POINT('Ctrl Pts',(-27.284978999474,24.7885624992263,-49.6595766751466));
#67209=CARTESIAN_POINT('Ctrl Pts',(-27.2458058797152,24.8961256505024,-49.6653453549084));
#67210=CARTESIAN_POINT('Ctrl Pts',(-27.2066308287074,25.0036941046812,-49.6711143190682));
#67211=CARTESIAN_POINT('Ctrl Pts',(-27.1627583780813,25.1095416972608,-49.676883283228));
#67212=CARTESIAN_POINT('Ctrl Pts',(-27.1143780351475,25.2132313035472,-49.6826522473879));
#67213=CARTESIAN_POINT('Ctrl Pts',(-27.0647595620063,25.319574492383,-49.6885688485498));
#67214=CARTESIAN_POINT('Ctrl Pts',(-27.0103995267252,25.4236473098046,-49.6944854497117));
#67215=CARTESIAN_POINT('Ctrl Pts',(-26.9515528064239,25.525004526534,-49.7004020508737));
#67216=CARTESIAN_POINT('Ctrl Pts',(-26.8940929348259,25.6239730438783,-49.706179214687));
#67217=CARTESIAN_POINT('Ctrl Pts',(-26.8323557985413,25.7203522122916,-49.7119563785004));
#67218=CARTESIAN_POINT('Ctrl Pts',(-26.766622182131,25.8137576171201,-49.7177335423138));
#67219=CARTESIAN_POINT('Ctrl Pts',(-26.698508750604,25.9105446645012,-49.72371986215));
#67220=CARTESIAN_POINT('Ctrl Pts',(-26.6261043021226,26.0041381491129,-49.7297061819862));
#67221=CARTESIAN_POINT('Ctrl Pts',(-26.5497651972763,26.0941496933366,-49.7356925018224));
#67222=CARTESIAN_POINT('Ctrl Pts',(-26.4734260924301,26.1841612375603,-49.7416788216586));
#67223=CARTESIAN_POINT('Ctrl Pts',(-26.3931527277981,26.2705905268623,-49.7476651414949));
#67224=CARTESIAN_POINT('Ctrl Pts',(-26.309340642267,26.3530942678784,-49.7536514613311));
#67225=CARTESIAN_POINT('Ctrl Pts',(-26.2271249456003,26.4340265403813,-49.7595237582998));
#67226=CARTESIAN_POINT('Ctrl Pts',(-26.1412075193273,26.5114738824381,-49.7653960552685));
#67227=CARTESIAN_POINT('Ctrl Pts',(-26.0519159492196,26.5850785803196,-49.7712683522372));
#67228=CARTESIAN_POINT('Ctrl Pts',(-25.9627400938953,26.6585878923582,-49.7771330391753));
#67229=CARTESIAN_POINT('Ctrl Pts',(-25.8701991063477,26.7282642026664,-49.7829977261135));
#67230=CARTESIAN_POINT('Ctrl Pts',(-25.7746577077335,26.7937861931211,-49.7888624130517));
#67231=CARTESIAN_POINT('Ctrl Pts',(-25.6792145674669,26.8592407983103,-49.7947210685265));
#67232=CARTESIAN_POINT('Ctrl Pts',(-25.5807774926853,26.9205493493911,-49.8005797240013));
#67233=CARTESIAN_POINT('Ctrl Pts',(-25.4797440849629,26.9774308675654,-49.8064383794761));
#67234=CARTESIAN_POINT('Ctrl Pts',(-25.3747642233455,27.0365342279403,-49.812525879194));
#67235=CARTESIAN_POINT('Ctrl Pts',(-25.2669814146164,27.090857368111,-49.8186133789119));
#67236=CARTESIAN_POINT('Ctrl Pts',(-25.1568750103301,27.14013459259,-49.8247008786299));
#67237=CARTESIAN_POINT('Ctrl Pts',(-25.0510305087958,27.1875044372034,-49.8305527487132));
#67238=CARTESIAN_POINT('Ctrl Pts',(-24.9430393589257,27.2302115439541,-49.8364046187966));
#67239=CARTESIAN_POINT('Ctrl Pts',(-24.8333515015809,27.2680672168924,-49.84225648888));
#67240=CARTESIAN_POINT('Ctrl Pts',(-24.7236803452098,27.3059171259603,-49.848107467963));
#67241=CARTESIAN_POINT('Ctrl Pts',(-24.6123133856832,27.3389169351134,-49.8539584470459));
#67242=CARTESIAN_POINT('Ctrl Pts',(-24.4997182831299,27.3669269724673,-49.8598094261289));
#67243=CARTESIAN_POINT('Ctrl Pts',(-24.3871130571933,27.3949395281931,-49.8656609312712));
#67244=CARTESIAN_POINT('Ctrl Pts',(-24.2732798699017,27.417961320487,-49.8715124364135));
#67245=CARTESIAN_POINT('Ctrl Pts',(-24.1586985045816,27.4359033778302,-49.8773639415558));
#67246=CARTESIAN_POINT('Ctrl Pts',(-24.0440790892849,27.4538513933399,-49.8832173898555));
#67247=CARTESIAN_POINT('Ctrl Pts',(-23.9287114101153,27.4667162557479,-49.8890708381553));
#67248=CARTESIAN_POINT('Ctrl Pts',(-23.8130816223074,27.4744607154081,-49.894924286455));
#67249=CARTESIAN_POINT('Ctrl Pts',(-23.6973203383219,27.4822139822008,-49.9007843913965));
#67250=CARTESIAN_POINT('Ctrl Pts',(-23.5812967634541,27.4848351960527,-49.9066444963381));
#67251=CARTESIAN_POINT('Ctrl Pts',(-23.465498416705,27.4823392219889,-49.9125046012796));
#67252=CARTESIAN_POINT('Ctrl Pts',(-23.3496220870172,27.4798415670427,-49.918368652635));
#67253=CARTESIAN_POINT('Ctrl Pts',(-23.2339716989474,27.4722198894174,-49.9242327039905));
#67254=CARTESIAN_POINT('Ctrl Pts',(-23.1190292643755,27.4595408932407,-49.9300967553459));
#67255=CARTESIAN_POINT('Ctrl Pts',(-23.0039174275996,27.4468432107546,-49.9359694491424));
#67256=CARTESIAN_POINT('Ctrl Pts',(-22.8895160336619,27.4290733972241,-49.941842142939));
#67257=CARTESIAN_POINT('Ctrl Pts',(-22.7762966185154,27.4063491648785,-49.9477148367355));
#67258=CARTESIAN_POINT('Ctrl Pts',(-22.7452990365751,27.4001276501918,-49.949322682059));
#67259=CARTESIAN_POINT('Ctrl Pts',(-22.7143899604881,27.393535052838,-49.9509305273825));
#67260=CARTESIAN_POINT('Ctrl Pts',(-22.6835788420845,27.3865744310841,-49.952538372706));
#67261=CARTESIAN_POINT('Ctrl Pts',(-22.5710480939066,27.3611523102935,-49.9584106696747));
#67262=CARTESIAN_POINT('Ctrl Pts',(-22.4594483344045,27.3307321096337,-49.9642829666434));
#67263=CARTESIAN_POINT('Ctrl Pts',(-22.3492575881372,27.2953960730756,-49.9701552636121));
#67264=CARTESIAN_POINT('Ctrl Pts',(-22.2392096403258,27.2601058292144,-49.9760199505503));
#67265=CARTESIAN_POINT('Ctrl Pts',(-22.1305674645564,27.219912543225,-49.9818846374885));
#67266=CARTESIAN_POINT('Ctrl Pts',(-22.0237985384041,27.1749493750687,-49.9877493244267));
#67267=CARTESIAN_POINT('Ctrl Pts',(-21.9171394174088,27.1300324487161,-49.9936079799015));
#67268=CARTESIAN_POINT('Ctrl Pts',(-21.8123500927711,27.0803555570138,-49.9994666353763));
#67269=CARTESIAN_POINT('Ctrl Pts',(-21.7098818771748,27.0261013278854,-50.0053252908511));
#67270=CARTESIAN_POINT('Ctrl Pts',(-21.6034111628242,26.9697278807805,-50.011412790569));
#67271=CARTESIAN_POINT('Ctrl Pts',(-21.4994470161958,26.9084123555737,-50.017500290287));
#67272=CARTESIAN_POINT('Ctrl Pts',(-21.3984720811977,26.842414419096,-50.0235877900049));
#67273=CARTESIAN_POINT('Ctrl Pts',(-21.301405595995,26.7789710732336,-50.0294396600883));
#67274=CARTESIAN_POINT('Ctrl Pts',(-21.2071015959606,26.711201308627,-50.0352915301717));
#67275=CARTESIAN_POINT('Ctrl Pts',(-21.1159620462723,26.6393816699117,-50.0411434002551));
#67276=CARTESIAN_POINT('Ctrl Pts',(-21.0248363734094,26.5675729663895,-50.046994379338));
#67277=CARTESIAN_POINT('Ctrl Pts',(-20.9368745174852,26.4917158706057,-50.052845358421));
#67278=CARTESIAN_POINT('Ctrl Pts',(-20.8524467769247,26.4121283342986,-50.0586963375039));
#67279=CARTESIAN_POINT('Ctrl Pts',(-20.7680114454979,26.3325336423061,-50.0645478426462));
#67280=CARTESIAN_POINT('Ctrl Pts',(-20.6871111619133,26.2492081266141,-50.0703993477885));
#67281=CARTESIAN_POINT('Ctrl Pts',(-20.6100801226299,26.1625073441076,-50.0762508529308));
#67282=CARTESIAN_POINT('Ctrl Pts',(-20.5330235030151,26.0757777701585,-50.0821043012306));
#67283=CARTESIAN_POINT('Ctrl Pts',(-20.4598389570468,25.9856710095167,-50.0879577495303));
#67284=CARTESIAN_POINT('Ctrl Pts',(-20.3908206109911,25.8925759377256,-50.0938111978301));
#67285=CARTESIAN_POINT('Ctrl Pts',(-20.3217237760889,25.7993749966227,-50.0996713027717));
#67286=CARTESIAN_POINT('Ctrl Pts',(-20.2568028440914,25.7031792936221,-50.1055314077132));
#67287=CARTESIAN_POINT('Ctrl Pts',(-20.1963088334912,25.6044070218152,-50.1113915126547));
#67288=CARTESIAN_POINT('Ctrl Pts',(-20.1357740839611,25.5055682330654,-50.1172555640102));
#67289=CARTESIAN_POINT('Ctrl Pts',(-20.079672391706,25.4041497813089,-50.1231196153656));
#67290=CARTESIAN_POINT('Ctrl Pts',(-20.028208185279,25.3005932476364,-50.128983666721));
#67291=CARTESIAN_POINT('Ctrl Pts',(-19.9766681308849,25.1968840923049,-50.1348563605176));
#67292=CARTESIAN_POINT('Ctrl Pts',(-19.9297793699119,25.0910309426008,-50.1407290543142));
#67293=CARTESIAN_POINT('Ctrl Pts',(-19.8876977542586,24.9834941380829,-50.1466017481107));
#67294=CARTESIAN_POINT('Ctrl Pts',(-19.8761765118319,24.9540523598762,-50.1482095934341));
#67295=CARTESIAN_POINT('Ctrl Pts',(-19.8650153086448,24.924484457216,-50.1498174387575));
#67296=CARTESIAN_POINT('Ctrl Pts',(-19.8542166808408,24.8948000352085,-50.1514252840809));
#67297=CARTESIAN_POINT('Ctrl Pts',(-19.8147770976934,24.7863842946901,-50.1572975810496));
#67298=CARTESIAN_POINT('Ctrl Pts',(-19.7800457218456,24.6760501365121,-50.1631698780183));
#67299=CARTESIAN_POINT('Ctrl Pts',(-19.7502117526039,24.5642441871091,-50.169042174987));
#67300=CARTESIAN_POINT('Ctrl Pts',(-19.720416445817,24.4525831293368,-50.1749068619252));
#67301=CARTESIAN_POINT('Ctrl Pts',(-19.6955060300206,24.3394544690448,-50.1807715488634));
#67302=CARTESIAN_POINT('Ctrl Pts',(-19.6756211669524,24.2253234815646,-50.1866362358017));
#67303=CARTESIAN_POINT('Ctrl Pts',(-19.6557567542211,24.1113098706608,-50.1924948912765));
#67304=CARTESIAN_POINT('Ctrl Pts',(-19.6409076843999,23.9962963877439,-50.1983535467513));
#67305=CARTESIAN_POINT('Ctrl Pts',(-19.6311642631908,23.8807614478816,-50.2042122022261));
#67306=CARTESIAN_POINT('Ctrl Pts',(-19.6210402553674,23.7607136115064,-50.210299701944));
#67307=CARTESIAN_POINT('Ctrl Pts',(-19.6164290068854,23.6401031898881,-50.2163872016619));
#67308=CARTESIAN_POINT('Ctrl Pts',(-19.617372945176,23.5194766003745,-50.2224747013798));
#67309=CARTESIAN_POINT('Ctrl Pts',(-19.6182803463258,23.4035191197751,-50.2283265714632));
#67310=CARTESIAN_POINT('Ctrl Pts',(-19.6243208764983,23.2875471515561,-50.2341784415466));
#67311=CARTESIAN_POINT('Ctrl Pts',(-19.635479153271,23.1720483598653,-50.24003031163));
#67312=CARTESIAN_POINT('Ctrl Pts',(-19.6466357310945,23.0565671539158,-50.245881290713));
#67313=CARTESIAN_POINT('Ctrl Pts',(-19.6629084664319,22.9415593925992,-50.251732269796));
#67314=CARTESIAN_POINT('Ctrl Pts',(-19.6842300231476,22.8275084805869,-50.257583248879));
#67315=CARTESIAN_POINT('Ctrl Pts',(-19.7055534968766,22.7134473142993,-50.2634347540213));
#67316=CARTESIAN_POINT('Ctrl Pts',(-19.7319266184007,22.600343574703,-50.2692862591636));
#67317=CARTESIAN_POINT('Ctrl Pts',(-19.7632308991008,22.4886706204554,-50.275137764306));
#67318=CARTESIAN_POINT('Ctrl Pts',(-19.7945455752707,22.3769605820517,-50.2809912126057));
#67319=CARTESIAN_POINT('Ctrl Pts',(-19.8307945552232,22.266682671597,-50.2868446609055));
#67320=CARTESIAN_POINT('Ctrl Pts',(-19.8718096591547,22.1582945461705,-50.2926981092052));
#67321=CARTESIAN_POINT('Ctrl Pts',(-19.9128714061658,22.0497831599088,-50.2985582141468));
#67322=CARTESIAN_POINT('Ctrl Pts',(-19.9587099491574,21.9431662350625,-50.3044183190883));
#67323=CARTESIAN_POINT('Ctrl Pts',(-20.0091091414018,21.8388810087955,-50.3102784240299));
#67324=CARTESIAN_POINT('Ctrl Pts',(-20.0595422743478,21.7345255529556,-50.3161424753854));
#67325=CARTESIAN_POINT('Ctrl Pts',(-20.1145419764513,21.6325052853654,-50.3220065267408));
#67326=CARTESIAN_POINT('Ctrl Pts',(-20.1738472404311,21.5332308884959,-50.3278705780963));
#67327=CARTESIAN_POINT('Ctrl Pts',(-20.2332399085315,21.4338101809826,-50.3337432718928));
#67328=CARTESIAN_POINT('Ctrl Pts',(-20.2969505763465,21.3371437648161,-50.3396159656894));
#67329=CARTESIAN_POINT('Ctrl Pts',(-20.3646761970398,21.2436115938606,-50.345488659486));
#67330=CARTESIAN_POINT('Ctrl Pts',(-20.3832183390734,21.2180040500564,-50.3470965048093));
#67331=CARTESIAN_POINT('Ctrl Pts',(-20.4020612081979,21.1926312376915,-50.3487043501325));
#67332=CARTESIAN_POINT('Ctrl Pts',(-20.4211980943696,21.1675004824328,-50.3503121954558));
#67333=CARTESIAN_POINT('Ctrl Pts',(-20.4910913092399,21.0757159955843,-50.3561844924245));
#67334=CARTESIAN_POINT('Ctrl Pts',(-20.5651435067155,20.9868556164598,-50.3620567893932));
#67335=CARTESIAN_POINT('Ctrl Pts',(-20.6430812027292,20.9013199421322,-50.3679290863619));
#67336=CARTESIAN_POINT('Ctrl Pts',(-20.7209178976786,20.8158951152453,-50.3737937733001));
#67337=CARTESIAN_POINT('Ctrl Pts',(-20.8026298019172,20.7337867277308,-50.3796584602383));
#67338=CARTESIAN_POINT('Ctrl Pts',(-20.8879015051344,20.6553646217094,-50.3855231471765));
#67339=CARTESIAN_POINT('Ctrl Pts',(-20.9730855117428,20.5770231679149,-50.3913818026513));
#67340=CARTESIAN_POINT('Ctrl Pts',(-21.0618217329104,20.5023607330488,-50.3972404581262));
#67341=CARTESIAN_POINT('Ctrl Pts',(-21.1537564840738,20.4317118964387,-50.403099113601));
#67342=CARTESIAN_POINT('Ctrl Pts',(-21.2492822875929,20.3583034540438,-50.4091866133189));
#67343=CARTESIAN_POINT('Ctrl Pts',(-21.3482612836426,20.2892288874038,-50.4152741130368));
#67344=CARTESIAN_POINT('Ctrl Pts',(-21.4502566959656,20.2248192531691,-50.4213616127547));
#67345=CARTESIAN_POINT('Ctrl Pts',(-21.5483041587459,20.1629027309306,-50.4272134828381));
#67346=CARTESIAN_POINT('Ctrl Pts',(-21.6491384840492,20.1052969650911,-50.4330653529215));
#67347=CARTESIAN_POINT('Ctrl Pts',(-21.7523410769943,20.0522526173061,-50.4389172230049));
#67348=CARTESIAN_POINT('Ctrl Pts',(-21.8555279564064,19.9992163460053,-50.4447682020879));
#67349=CARTESIAN_POINT('Ctrl Pts',(-21.9610820189306,19.9507403007559,-50.4506191811708));
#67350=CARTESIAN_POINT('Ctrl Pts',(-22.0685601700707,19.9070291312552,-50.4564701602538));
#67351=CARTESIAN_POINT('Ctrl Pts',(-22.1760479845304,19.8633140316998,-50.462321665396));
#67352=CARTESIAN_POINT('Ctrl Pts',(-22.2854598485538,19.8243648152735,-50.4681731705383));
#67353=CARTESIAN_POINT('Ctrl Pts',(-22.3963334694385,19.7903376659342,-50.4740246756806));
#67354=CARTESIAN_POINT('Ctrl Pts',(-22.5072439090401,19.7562992169191,-50.4798781239804));
#67355=CARTESIAN_POINT('Ctrl Pts',(-22.619616675744,19.7271862063339,-50.4857315722802));
#67356=CARTESIAN_POINT('Ctrl Pts',(-22.7329758266575,19.703104524741,-50.49158502058));
#67357=CARTESIAN_POINT('Ctrl Pts',(-22.8464638915404,19.678995457047,-50.4974451255215));
#67358=CARTESIAN_POINT('Ctrl Pts',(-22.960940174979,19.6599292246644,-50.503305230463));
#67359=CARTESIAN_POINT('Ctrl Pts',(-23.0759199855418,19.6459603249478,-50.5091653354046));
#67360=CARTESIAN_POINT('Ctrl Pts',(-23.1909772278111,19.6319820180515,-50.51502938676));
#67361=CARTESIAN_POINT('Ctrl Pts',(-23.3065382612459,19.6231079106509,-50.5208934381155));
#67362=CARTESIAN_POINT('Ctrl Pts',(-23.4221164862923,19.619340404227,-50.526757489471));
#67363=CARTESIAN_POINT('Ctrl Pts',(-23.5378650505702,19.6155673452507,-50.5326301832675));
#67364=CARTESIAN_POINT('Ctrl Pts',(-23.6536304452246,19.6169159031184,-50.538502877064));
#67365=CARTESIAN_POINT('Ctrl Pts',(-23.7689291990324,19.6233365006131,-50.5443755708606));
#67366=CARTESIAN_POINT('Ctrl Pts',(-23.8004960691129,19.6250943528037,-50.545983416184));
#67367=CARTESIAN_POINT('Ctrl Pts',(-23.8320280114364,19.6272320940354,-50.5475912615073));
#67368=CARTESIAN_POINT('Ctrl Pts',(-23.8635152357334,19.6297480388696,-50.5491991068306));
#67369=CARTESIAN_POINT('Ctrl Pts',(-23.9785153101229,19.6389369670634,-50.5550714037994));
#67370=CARTESIAN_POINT('Ctrl Pts',(-24.0933033900328,19.65320552129,-50.5609437007681));
#67371=CARTESIAN_POINT('Ctrl Pts',(-24.2073946166921,19.6725401545155,-50.5668159977368));
#67372=CARTESIAN_POINT('Ctrl Pts',(-24.3213379901826,19.6918497315919,-50.572680684675));
#67373=CARTESIAN_POINT('Ctrl Pts',(-24.4345859024878,19.7162122633372,-50.5785453716132));
#67374=CARTESIAN_POINT('Ctrl Pts',(-24.546656706582,19.7455623051099,-50.5844100585514));
#67375=CARTESIAN_POINT('Ctrl Pts',(-24.6586122528693,19.7748821622018,-50.5902687140261));
#67376=CARTESIAN_POINT('Ctrl Pts',(-24.769392701363,19.8091792226978,-50.5961273695009));
#67377=CARTESIAN_POINT('Ctrl Pts',(-24.8785253833609,19.8483367801508,-50.6019860249757));
#67378=CARTESIAN_POINT('Ctrl Pts',(-24.9919208840411,19.8890238662877,-50.6080735246936));
#67379=CARTESIAN_POINT('Ctrl Pts',(-25.1035368192879,19.9349588248107,-50.6141610244115));
#67380=CARTESIAN_POINT('Ctrl Pts',(-25.2128585695035,19.9859531386802,-50.6202485241294));
#67381=CARTESIAN_POINT('Ctrl Pts',(-25.3179487886732,20.0349736090842,-50.6261003942128));
#67382=CARTESIAN_POINT('Ctrl Pts',(-25.4209187134945,20.088668860267,-50.6319522642962));
#67383=CARTESIAN_POINT('Ctrl Pts',(-25.5213311898325,20.146822214583,-50.6378041343796));
#67384=CARTESIAN_POINT('Ctrl Pts',(-25.6217283774579,20.2049667145219,-50.6436551134626));
#67385=CARTESIAN_POINT('Ctrl Pts',(-25.7195685332179,20.2675677608329,-50.6495060925455));
#67386=CARTESIAN_POINT('Ctrl Pts',(-25.814439970529,20.3343631925187,-50.6553570716285));
#67387=CARTESIAN_POINT('Ctrl Pts',(-25.9093199376955,20.4011646297567,-50.6612085767708));
#67388=CARTESIAN_POINT('Ctrl Pts',(-26.0012303177777,20.4721609640463,-50.6670600819131));
#67389=CARTESIAN_POINT('Ctrl Pts',(-26.0897898217878,20.5470476848308,-50.6729115870554));
#67390=CARTESIAN_POINT('Ctrl Pts',(-26.1783787344812,20.621959273865,-50.6787650353551));
#67391=CARTESIAN_POINT('Ctrl Pts',(-26.2636142429747,20.7007635515012,-50.6846184836549));
#67392=CARTESIAN_POINT('Ctrl Pts',(-26.3451499924511,20.7831173373363,-50.6904719319547));
#67393=CARTESIAN_POINT('Ctrl Pts',(-26.42677846578,20.8655647773087,-50.6963320368962));
#67394=CARTESIAN_POINT('Ctrl Pts',(-26.5046984911743,20.9515694883994,-50.7021921418378));
#67395=CARTESIAN_POINT('Ctrl Pts',(-26.5786022228291,21.0407531497052,-50.7080522467793));
#67396=CARTESIAN_POINT('Ctrl Pts',(-26.6525557240218,21.1299968706252,-50.7139162981348));
#67397=CARTESIAN_POINT('Ctrl Pts',(-26.7224872970213,21.2224234757153,-50.7197803494902));
#67398=CARTESIAN_POINT('Ctrl Pts',(-26.7881318937342,21.3176248787088,-50.7256444008457));
#67399=CARTESIAN_POINT('Ctrl Pts',(-26.8538732374787,21.412966589566,-50.7315170946423));
#67400=CARTESIAN_POINT('Ctrl Pts',(-26.9153147765724,21.5110909111264,-50.7373897884388));
#67401=CARTESIAN_POINT('Ctrl Pts',(-26.9722368844682,21.6115642923505,-50.7432624822354));
#67402=CARTESIAN_POINT('Ctrl Pts',(-26.9878212054197,21.6390722234156,-50.7448703275588));
#67403=CARTESIAN_POINT('Ctrl Pts',(-27.0030670394137,21.6667561153043,-50.7464781728821));
#67404=CARTESIAN_POINT('Ctrl Pts',(-27.0179705123824,21.6946068202471,-50.7480860182055));
#67405=CARTESIAN_POINT('Ctrl Pts',(-27.0754310621943,21.8019856051811,-50.7542850884817));
#67406=CARTESIAN_POINT('Ctrl Pts',(-27.1279738091353,21.9121727179392,-50.7604841587579));
#67407=CARTESIAN_POINT('Ctrl Pts',(-27.1753306576848,22.0247042432207,-50.7666832290342));
#67408=CARTESIAN_POINT('Ctrl Pts',(-27.2225983833257,22.1370239905409,-50.772870633011));
#67409=CARTESIAN_POINT('Ctrl Pts',(-27.264699519378,22.2516790441243,-50.7790580369878));
#67410=CARTESIAN_POINT('Ctrl Pts',(-27.30141184107,22.368181114358,-50.7852454409647));
#67411=CARTESIAN_POINT('Ctrl Pts',(-27.3380337747153,22.4843963491621,-50.7914176111635));
#67412=CARTESIAN_POINT('Ctrl Pts',(-27.3692932407326,22.6024492064155,-50.7975897813623));
#67413=CARTESIAN_POINT('Ctrl Pts',(-27.3950164309745,22.7218326147495,-50.8037619515611));
#67414=CARTESIAN_POINT('Ctrl Pts',(-27.4207007736102,22.8410357281977,-50.8099248004418));
#67415=CARTESIAN_POINT('Ctrl Pts',(-27.4408654193857,22.9615650546885,-50.8160876493226));
#67416=CARTESIAN_POINT('Ctrl Pts',(-27.4553861962024,23.0828982096596,-50.8222504982033));
#67417=CARTESIAN_POINT('Ctrl Pts',(-27.4698793086307,23.2040002056798,-50.8284016058771));
#67418=CARTESIAN_POINT('Ctrl Pts',(-27.4787499437123,23.3259026354998,-50.8345527135509));
#67419=CARTESIAN_POINT('Ctrl Pts',(-27.4819250050777,23.4480734632001,-50.8407038212247));
#67420=CARTESIAN_POINT('Ctrl Pts',(-27.4828081251522,23.4820543845235,-50.8424147067925));
#67421=CARTESIAN_POINT('Ctrl Pts',(-27.4832509209801,23.5160560114756,-50.8441255923602));
#67422=CARTESIAN_POINT('Ctrl Pts',(-27.4832525273076,23.5500667762137,-50.845836477928));
#67423=CARTESIAN_POINT('',(-27.4832508703214,23.5538675497877,-52.095836477965));
#67424=CARTESIAN_POINT('Ctrl Pts',(-27.4832525273076,23.5500667769491,-50.845836477965));
#67425=CARTESIAN_POINT('Ctrl Pts',(-27.4832582621366,23.6714907668338,-50.8519446191219));
#67426=CARTESIAN_POINT('Ctrl Pts',(-27.4776365755207,23.7928145505648,-50.8580527602788));
#67427=CARTESIAN_POINT('Ctrl Pts',(-27.4664411021963,23.913510126616,-50.8641609014358));
#67428=CARTESIAN_POINT('Ctrl Pts',(-27.4552314451803,24.0343586134725,-50.8702767810767));
#67429=CARTESIAN_POINT('Ctrl Pts',(-27.4384339508407,24.154576949595,-50.8763926607176));
#67430=CARTESIAN_POINT('Ctrl Pts',(-27.4161536553574,24.273645579808,-50.8825085403585));
#67431=CARTESIAN_POINT('Ctrl Pts',(-27.3938220497938,24.3929884173797,-50.8886385044749));
#67432=CARTESIAN_POINT('Ctrl Pts',(-27.365982471607,24.5111759044408,-50.8947684685913));
#67433=CARTESIAN_POINT('Ctrl Pts',(-27.3327906542758,24.6277006052536,-50.9008984327076));
#67434=CARTESIAN_POINT('Ctrl Pts',(-27.2995573770958,24.7443708568941,-50.9070360537529));
#67435=CARTESIAN_POINT('Ctrl Pts',(-27.2609586372413,24.8593738402802,-50.9131736747982));
#67436=CARTESIAN_POINT('Ctrl Pts',(-27.2171987729359,24.9722209785464,-50.9193112958435));
#67437=CARTESIAN_POINT('Ctrl Pts',(-27.1733410876714,25.0853203757138,-50.9254626369491));
#67438=CARTESIAN_POINT('Ctrl Pts',(-27.1242993608469,25.1962539673951,-50.9316139780547));
#67439=CARTESIAN_POINT('Ctrl Pts',(-27.0703249722303,25.3045555310014,-50.9377653191603));
#67440=CARTESIAN_POINT('Ctrl Pts',(-27.0433945227279,25.3585924522985,-50.9408345226337));
#67441=CARTESIAN_POINT('Ctrl Pts',(-27.0152367819953,25.4119745593238,-50.9439037261071));
#67442=CARTESIAN_POINT('Ctrl Pts',(-26.9858869787784,25.464646677634,-50.9469729295805));
#67443=CARTESIAN_POINT('Ctrl Pts',(-26.9297320962635,25.5654240693478,-50.9528452265492));
#67444=CARTESIAN_POINT('Ctrl Pts',(-26.8690452280656,25.6638974107016,-50.9587175235178));
#67445=CARTESIAN_POINT('Ctrl Pts',(-26.804040216488,25.7596313363097,-50.9645898204865));
#67446=CARTESIAN_POINT('Ctrl Pts',(-26.7391194462429,25.855241198353,-50.9704545074247));
#67447=CARTESIAN_POINT('Ctrl Pts',(-26.6698918910716,25.9481183656194,-50.9763191943629));
#67448=CARTESIAN_POINT('Ctrl Pts',(-26.5966172610651,26.0378519640074,-50.9821838813011));
#67449=CARTESIAN_POINT('Ctrl Pts',(-26.5234179894285,26.1274932770068,-50.9880425367759));
#67450=CARTESIAN_POINT('Ctrl Pts',(-26.4461801816037,26.2139971333922,-50.9939011922507));
#67451=CARTESIAN_POINT('Ctrl Pts',(-26.3652064404348,26.2969821309933,-50.9997598477255));
#67452=CARTESIAN_POINT('Ctrl Pts',(-26.2810697936146,26.3832085956935,-51.0058473474434));
#67453=CARTESIAN_POINT('Ctrl Pts',(-26.1928996613371,26.4656353218793,-51.0119348471613));
#67454=CARTESIAN_POINT('Ctrl Pts',(-26.1010813966376,26.543872598064,-51.0180223468792));
#67455=CARTESIAN_POINT('Ctrl Pts',(-26.012817153319,26.6190815339368,-51.0238742169625));
#67456=CARTESIAN_POINT('Ctrl Pts',(-25.9211822877098,26.6904190193286,-51.0297260870459));
#67457=CARTESIAN_POINT('Ctrl Pts',(-25.8265555690924,26.7575775046166,-51.0355779571293));
#67458=CARTESIAN_POINT('Ctrl Pts',(-25.7319432582533,26.8247257644146,-51.0414289362123));
#67459=CARTESIAN_POINT('Ctrl Pts',(-25.6343403371765,26.8876960500704,-51.0472799152952));
#67460=CARTESIAN_POINT('Ctrl Pts',(-25.5341563588103,26.9462228797323,-51.0531308943781));
#67461=CARTESIAN_POINT('Ctrl Pts',(-25.4339633729406,27.0047549715193,-51.0589823995204));
#67462=CARTESIAN_POINT('Ctrl Pts',(-25.3311892254228,27.0588426045912,-51.0648339046627));
#67463=CARTESIAN_POINT('Ctrl Pts',(-25.2262693535155,27.1082655464219,-51.0706854098049));
#67464=CARTESIAN_POINT('Ctrl Pts',(-25.1213146400026,27.1577049005359,-51.0765388581047));
#67465=CARTESIAN_POINT('Ctrl Pts',(-25.0142131590139,27.2024763071687,-51.0823923064045));
#67466=CARTESIAN_POINT('Ctrl Pts',(-24.9054209997638,27.2424073799027,-51.0882457547042));
#67467=CARTESIAN_POINT('Ctrl Pts',(-24.7965051202049,27.2823838629373,-51.0941058596457));
#67468=CARTESIAN_POINT('Ctrl Pts',(-24.6858951130954,27.3175088827148,-51.0999659645872));
#67469=CARTESIAN_POINT('Ctrl Pts',(-24.5740630237384,27.3476596834729,-51.1058260695288));
#67470=CARTESIAN_POINT('Ctrl Pts',(-24.4621556224685,27.3778307889083,-51.1116901208842));
#67471=CARTESIAN_POINT('Ctrl Pts',(-24.3490249027182,27.4030209155317,-51.1175541722396));
#67472=CARTESIAN_POINT('Ctrl Pts',(-24.2351521945031,27.4231586049013,-51.123418223595));
#67473=CARTESIAN_POINT('Ctrl Pts',(-24.1211116606473,27.4433259732051,-51.1292909173916));
#67474=CARTESIAN_POINT('Ctrl Pts',(-24.006327364139,27.4584259891948,-51.1351636111881));
#67475=CARTESIAN_POINT('Ctrl Pts',(-23.8912849176308,27.4684390907726,-51.1410363049847));
#67476=CARTESIAN_POINT('Ctrl Pts',(-23.8597882201984,27.4711805104861,-51.1426441503082));
#67477=CARTESIAN_POINT('Ctrl Pts',(-23.8282721648829,27.4735409303254,-51.1442519956317));
#67478=CARTESIAN_POINT('Ctrl Pts',(-23.7967466820691,27.4755206287585,-51.1458598409552));
#67479=CARTESIAN_POINT('Ctrl Pts',(-23.6816068769783,27.4827510363965,-51.1517321379239));
#67480=CARTESIAN_POINT('Ctrl Pts',(-23.565955777727,27.4849231715453,-51.1576044348926));
#67481=CARTESIAN_POINT('Ctrl Pts',(-23.4502752553495,27.4819816098753,-51.1634767318613));
#67482=CARTESIAN_POINT('Ctrl Pts',(-23.3347446457418,27.4790438602355,-51.1693414187995));
#67483=CARTESIAN_POINT('Ctrl Pts',(-23.2191850982695,27.4710056028029,-51.1752061057377));
#67484=CARTESIAN_POINT('Ctrl Pts',(-23.1040826725221,27.4578632411644,-51.1810707926759));
#67485=CARTESIAN_POINT('Ctrl Pts',(-22.9890986224141,27.4447343956222,-51.1869294481508));
#67486=CARTESIAN_POINT('Ctrl Pts',(-22.8745711671811,27.426511933519,-51.1927881036256));
#67487=CARTESIAN_POINT('Ctrl Pts',(-22.7609847565337,27.4032442756632,-51.1986467591004));
#67488=CARTESIAN_POINT('Ctrl Pts',(-22.6429615606407,27.3790677625976,-51.2047342588183));
#67489=CARTESIAN_POINT('Ctrl Pts',(-22.5259548786314,27.3494438907925,-51.2108217585362));
#67490=CARTESIAN_POINT('Ctrl Pts',(-22.4105008809704,27.3144862086426,-51.2169092582541));
#67491=CARTESIAN_POINT('Ctrl Pts',(-22.2995157760456,27.2808816379916,-51.2227611283376));
#67492=CARTESIAN_POINT('Ctrl Pts',(-22.1899658231277,27.2423486231468,-51.228612998421));
#67493=CARTESIAN_POINT('Ctrl Pts',(-22.0823145097288,27.1990395854517,-51.2344648685044));
#67494=CARTESIAN_POINT('Ctrl Pts',(-21.9746795872214,27.1557371419514,-51.2403158475873));
#67495=CARTESIAN_POINT('Ctrl Pts',(-21.8689431128443,27.1076602757401,-51.2461668266703));
#67496=CARTESIAN_POINT('Ctrl Pts',(-21.7655498216647,27.0550100463895,-51.2520178057533));
#67497=CARTESIAN_POINT('Ctrl Pts',(-21.6621472344333,27.0023550832766,-51.2578693108956));
#67498=CARTESIAN_POINT('Ctrl Pts',(-21.5610886175952,26.9451261272124,-51.2637208160379));
#67499=CARTESIAN_POINT('Ctrl Pts',(-21.4627946287674,26.8835704738516,-51.2695723211802));
#67500=CARTESIAN_POINT('Ctrl Pts',(-21.364467998646,26.8219943791985,-51.2754257694799));
#67501=CARTESIAN_POINT('Ctrl Pts',(-21.2689081722319,26.7560889495473,-51.2812792177797));
#67502=CARTESIAN_POINT('Ctrl Pts',(-21.1765067166659,26.6861447182394,-51.2871326660794));
#67503=CARTESIAN_POINT('Ctrl Pts',(-21.0840001805799,26.6161209451522,-51.292992771021));
#67504=CARTESIAN_POINT('Ctrl Pts',(-20.994659514171,26.5420494525735,-51.2988528759625));
#67505=CARTESIAN_POINT('Ctrl Pts',(-20.9088431544191,26.4642610254436,-51.3047129809041));
#67506=CARTESIAN_POINT('Ctrl Pts',(-20.8229690027202,26.3864202126767,-51.3105770322595));
#67507=CARTESIAN_POINT('Ctrl Pts',(-20.7406241765691,26.3048577713405,-51.3164410836149));
#67508=CARTESIAN_POINT('Ctrl Pts',(-20.6621289744305,26.2199400261359,-51.3223051349704));
#67509=CARTESIAN_POINT('Ctrl Pts',(-20.5835180860329,26.134897129126,-51.3281778287669));
#67510=CARTESIAN_POINT('Ctrl Pts',(-20.5087684109145,26.0464893733715,-51.3340505225635));
#67511=CARTESIAN_POINT('Ctrl Pts',(-20.4381589012217,25.9551147388014,-51.3399232163601));
#67512=CARTESIAN_POINT('Ctrl Pts',(-20.4188271986202,25.9300978923664,-51.3415310616835));
#67513=CARTESIAN_POINT('Ctrl Pts',(-20.3998055738489,25.9048588132359,-51.3431389070068));
#67514=CARTESIAN_POINT('Ctrl Pts',(-20.3810991604219,25.8794060065329,-51.3447467523302));
#67515=CARTESIAN_POINT('Ctrl Pts',(-20.312778151388,25.7864452985128,-51.3506190492989));
#67516=CARTESIAN_POINT('Ctrl Pts',(-20.2484363756992,25.6903202194212,-51.3564913462677));
#67517=CARTESIAN_POINT('Ctrl Pts',(-20.188380934496,25.5914062162441,-51.3623636432364));
#67518=CARTESIAN_POINT('Ctrl Pts',(-20.1284033203751,25.4926203977597,-51.3682283301746));
#67519=CARTESIAN_POINT('Ctrl Pts',(-20.0727012068954,25.3910531926764,-51.3740930171128));
#67520=CARTESIAN_POINT('Ctrl Pts',(-20.021540355593,25.2871115870683,-51.379957704051));
#67521=CARTESIAN_POINT('Ctrl Pts',(-19.9704321200234,25.1832768788948,-51.3858163595258));
#67522=CARTESIAN_POINT('Ctrl Pts',(-19.9238560384149,25.0770729959655,-51.3916750150006));
#67523=CARTESIAN_POINT('Ctrl Pts',(-19.882033239135,24.9689336874498,-51.3975336704755));
#67524=CARTESIAN_POINT('Ctrl Pts',(-19.8385768044781,24.8565703622957,-51.4036211701934));
#67525=CARTESIAN_POINT('Ctrl Pts',(-19.800252792973,24.7421177189986,-51.4097086699113));
#67526=CARTESIAN_POINT('Ctrl Pts',(-19.7672554973163,24.6260882244875,-51.4157961696292));
#67527=CARTESIAN_POINT('Ctrl Pts',(-19.7355354322263,24.5145498985429,-51.4216480397126));
#67528=CARTESIAN_POINT('Ctrl Pts',(-19.7087375104274,24.4015549570428,-51.427499909796));
#67529=CARTESIAN_POINT('Ctrl Pts',(-19.6869840319349,24.2875757300053,-51.4333517798794));
#67530=CARTESIAN_POINT('Ctrl Pts',(-19.6652338656073,24.1736138573415,-51.4392027589624));
#67531=CARTESIAN_POINT('Ctrl Pts',(-19.6485266929083,24.058668403065,-51.4450537380454));
#67532=CARTESIAN_POINT('Ctrl Pts',(-19.6369337572042,23.9432222114717,-51.4509047171283));
#67533=CARTESIAN_POINT('Ctrl Pts',(-19.6253397791837,23.8277656401547,-51.4567562222706));
#67534=CARTESIAN_POINT('Ctrl Pts',(-19.6188609935423,23.7118086533619,-51.462607727413));
#67535=CARTESIAN_POINT('Ctrl Pts',(-19.6175167295714,23.5958388311891,-51.4684592325553));
#67536=CARTESIAN_POINT('Ctrl Pts',(-19.6161720191997,23.4798304979626,-51.4743126808551));
#67537=CARTESIAN_POINT('Ctrl Pts',(-19.6199652256975,23.3638097340171,-51.4801661291549));
#67538=CARTESIAN_POINT('Ctrl Pts',(-19.6288635771295,23.2482630169458,-51.4860195774547));
#67539=CARTESIAN_POINT('Ctrl Pts',(-19.6377720479193,23.132584898167,-51.4918796823962));
#67540=CARTESIAN_POINT('Ctrl Pts',(-19.6517972198019,23.017382314685,-51.4977397873378));
#67541=CARTESIAN_POINT('Ctrl Pts',(-19.6708545482404,22.9031356288285,-51.5035998922793));
#67542=CARTESIAN_POINT('Ctrl Pts',(-19.6899247105968,22.7888120049794,-51.5094639436348));
#67543=CARTESIAN_POINT('Ctrl Pts',(-19.7140336915884,22.6754459639168,-51.5153279949902));
#67544=CARTESIAN_POINT('Ctrl Pts',(-19.7430464309964,22.5635049921435,-51.5211920463457));
#67545=CARTESIAN_POINT('Ctrl Pts',(-19.7721019293908,22.4513990417234,-51.5270647401423));
#67546=CARTESIAN_POINT('Ctrl Pts',(-19.8060754893694,22.3407227460215,-51.5329374339388));
#67547=CARTESIAN_POINT('Ctrl Pts',(-19.8447830692011,22.2319259171821,-51.5388101277354));
#67548=CARTESIAN_POINT('Ctrl Pts',(-19.8553805570597,22.2021391653961,-51.5404179730587));
#67549=CARTESIAN_POINT('Ctrl Pts',(-19.8663326232262,22.1724931610982,-51.5420258183819));
#67550=CARTESIAN_POINT('Ctrl Pts',(-19.8776348870796,22.1429968205794,-51.5436336637052));
#67551=CARTESIAN_POINT('Ctrl Pts',(-19.9189138887385,22.0352680058037,-51.5495059606738));
#67552=CARTESIAN_POINT('Ctrl Pts',(-19.9650060731872,21.9291765100944,-51.5553782576425));
#67553=CARTESIAN_POINT('Ctrl Pts',(-20.0157615717623,21.8251836478059,-51.5612505546112));
#67554=CARTESIAN_POINT('Ctrl Pts',(-20.0664512952421,21.721325552008,-51.5671152415494));
#67555=CARTESIAN_POINT('Ctrl Pts',(-20.1217921352823,21.6195610492669,-51.5729799284876));
#67556=CARTESIAN_POINT('Ctrl Pts',(-20.1815853430468,21.5203337224483,-51.5788446154258));
#67557=CARTESIAN_POINT('Ctrl Pts',(-20.2413170572404,21.4212084447233,-51.5847032709007));
#67558=CARTESIAN_POINT('Ctrl Pts',(-20.3054918192543,21.3246155047753,-51.5905619263755));
#67559=CARTESIAN_POINT('Ctrl Pts',(-20.3738642378916,21.2309754014241,-51.5964205818503));
#67560=CARTESIAN_POINT('Ctrl Pts',(-20.4449073434223,21.1336776331592,-51.6025080815682));
#67561=CARTESIAN_POINT('Ctrl Pts',(-20.5204825196542,21.0395684935762,-51.6085955812861));
#67562=CARTESIAN_POINT('Ctrl Pts',(-20.6002636430009,20.9490884544807,-51.614683081004));
#67563=CARTESIAN_POINT('Ctrl Pts',(-20.6769566681454,20.8621106378952,-51.6205349510874));
#67564=CARTESIAN_POINT('Ctrl Pts',(-20.7575357955095,20.7784865405874,-51.6263868211708));
#67565=CARTESIAN_POINT('Ctrl Pts',(-20.841669754267,20.6985743700103,-51.6322386912542));
#67566=CARTESIAN_POINT('Ctrl Pts',(-20.9257909028643,20.6186743667879,-51.6380896703372));
#67567=CARTESIAN_POINT('Ctrl Pts',(-21.013465507019,20.542485451159,-51.6439406494201));
#67568=CARTESIAN_POINT('Ctrl Pts',(-21.1043258517836,20.4703285591745,-51.6497916285031));
#67569=CARTESIAN_POINT('Ctrl Pts',(-21.1951943657672,20.3981651795913,-51.6556431336454));
#67570=CARTESIAN_POINT('Ctrl Pts',(-21.289248866016,20.3300348014017,-51.6614946387876));
#67571=CARTESIAN_POINT('Ctrl Pts',(-21.386089591516,20.2662172443748,-51.6673461439299));
#67572=CARTESIAN_POINT('Ctrl Pts',(-21.4829624757136,20.2023784949259,-51.6731995922297));
#67573=CARTESIAN_POINT('Ctrl Pts',(-21.5826230799634,20.1428556418139,-51.6790530405295));
#67574=CARTESIAN_POINT('Ctrl Pts',(-21.6846444078837,20.0878840752222,-51.6849064888293));
#67575=CARTESIAN_POINT('Ctrl Pts',(-21.7867817562068,20.0328499940227,-51.6907665937708));
#67576=CARTESIAN_POINT('Ctrl Pts',(-21.891284822559,19.9823777262893,-51.6966266987124));
#67577=CARTESIAN_POINT('Ctrl Pts',(-21.9977037701475,19.9366557994868,-51.7024868036539));
#67578=CARTESIAN_POINT('Ctrl Pts',(-22.104194384237,19.8909030818281,-51.7083508550093));
#67579=CARTESIAN_POINT('Ctrl Pts',(-22.2126030629448,19.8499072209206,-51.7142149063648));
#67580=CARTESIAN_POINT('Ctrl Pts',(-22.3224634962584,19.8138072846093,-51.7200789577203));
#67581=CARTESIAN_POINT('Ctrl Pts',(-22.4324858419203,19.7776541441981,-51.7259516515168));
#67582=CARTESIAN_POINT('Ctrl Pts',(-22.5439638158583,19.7464114404966,-51.7318243453134));
#67583=CARTESIAN_POINT('Ctrl Pts',(-22.6564195012106,19.7201674786416,-51.73769703911));
#67584=CARTESIAN_POINT('Ctrl Pts',(-22.6872079867061,19.7129823208937,-51.7393048844333));
#67585=CARTESIAN_POINT('Ctrl Pts',(-22.7180697235853,19.7061715558093,-51.7409127297566));
#67586=CARTESIAN_POINT('Ctrl Pts',(-22.7489948425118,19.699736317532,-51.74252057508));
#67587=CARTESIAN_POINT('Ctrl Pts',(-22.8619419522212,19.676233042882,-51.7483928720487));
#67588=CARTESIAN_POINT('Ctrl Pts',(-22.9761132872718,19.6576642200362,-51.7542651690174));
#67589=CARTESIAN_POINT('Ctrl Pts',(-23.0910397257914,19.6441531219384,-51.7601374659861));
#67590=CARTESIAN_POINT('Ctrl Pts',(-23.2058172287738,19.6306595331507,-51.7660021529243));
#67591=CARTESIAN_POINT('Ctrl Pts',(-23.3213474824664,19.6222106825637,-51.7718668398625));
#67592=CARTESIAN_POINT('Ctrl Pts',(-23.4371498609902,19.6188791347908,-51.7777315268007));
#67593=CARTESIAN_POINT('Ctrl Pts',(-23.5528331440167,19.6155510133062,-51.7835901822755));
#67594=CARTESIAN_POINT('Ctrl Pts',(-23.6687875844842,19.6173297384213,-51.7894488377503));
#67595=CARTESIAN_POINT('Ctrl Pts',(-23.7845267653356,19.624236155843,-51.7953074932251));
#67596=CARTESIAN_POINT('Ctrl Pts',(-23.9047868205333,19.6314123440124,-51.801394992943));
#67597=CARTESIAN_POINT('Ctrl Pts',(-24.0248140052634,19.644125028281,-51.8074824926609));
#67598=CARTESIAN_POINT('Ctrl Pts',(-24.1440614595818,19.6623379290877,-51.8135699923788));
#67599=CARTESIAN_POINT('Ctrl Pts',(-24.2586931873493,19.6798458608005,-51.8194218624622));
#67600=CARTESIAN_POINT('Ctrl Pts',(-24.3726039778124,19.7024360629564,-51.8252737325456));
#67601=CARTESIAN_POINT('Ctrl Pts',(-24.4853133991054,19.7300234581652,-51.831125602629));
#67602=CARTESIAN_POINT('Ctrl Pts',(-24.598005659364,19.7576066529422,-51.836976581712));
#67603=CARTESIAN_POINT('Ctrl Pts',(-24.7094965127351,19.790185429669,-51.842827560795));
#67604=CARTESIAN_POINT('Ctrl Pts',(-24.8193171848167,19.8276239031314,-51.848678539878));
#67605=CARTESIAN_POINT('Ctrl Pts',(-24.929147730833,19.8650657426727,-51.8545300450202));
#67606=CARTESIAN_POINT('Ctrl Pts',(-25.0373074057501,19.9073680141385,-51.8603815501625));
#67607=CARTESIAN_POINT('Ctrl Pts',(-25.1433447047262,19.954345646328,-51.8662330553048));
#67608=CARTESIAN_POINT('Ctrl Pts',(-25.2494172163824,20.0013388787671,-51.8720865036046));
#67609=CARTESIAN_POINT('Ctrl Pts',(-25.3533655729051,20.0530103917931,-51.8779399519045));
#67610=CARTESIAN_POINT('Ctrl Pts',(-25.4547609269378,20.109128184559,-51.8837934002043));
#67611=CARTESIAN_POINT('Ctrl Pts',(-25.5562715895045,20.1653097954403,-51.8896535051458));
#67612=CARTESIAN_POINT('Ctrl Pts',(-25.6552230927477,20.2259475781596,-51.8955136100874));
#67613=CARTESIAN_POINT('Ctrl Pts',(-25.7512136694914,20.2907649845625,-51.9013737150289));
#67614=CARTESIAN_POINT('Ctrl Pts',(-25.8472688898812,20.3556260414322,-51.9072377663844));
#67615=CARTESIAN_POINT('Ctrl Pts',(-25.940358882113,20.4246720809784,-51.9131018177399));
#67616=CARTESIAN_POINT('Ctrl Pts',(-26.0301145857459,20.4975859608296,-51.9189658690953));
#67617=CARTESIAN_POINT('Ctrl Pts',(-26.1200025713687,20.5706073011844,-51.9248385628919));
#67618=CARTESIAN_POINT('Ctrl Pts',(-26.2065461529907,20.6475075852407,-51.9307112566885));
#67619=CARTESIAN_POINT('Ctrl Pts',(-26.2894127036948,20.7279324661939,-51.9365839504851));
#67620=CARTESIAN_POINT('Ctrl Pts',(-26.3121001790887,20.7499514532541,-51.9381917958083));
#67621=CARTESIAN_POINT('Ctrl Pts',(-26.3345122671313,20.7722344430389,-51.9397996411316));
#67622=CARTESIAN_POINT('Ctrl Pts',(-26.356642678854,20.7947737453624,-51.9414074864549));
#67623=CARTESIAN_POINT('Ctrl Pts',(-26.4363906743046,20.8759951976191,-51.9472014338578));
#67624=CARTESIAN_POINT('Ctrl Pts',(-26.5127608102905,20.9608357359645,-51.9529953812607));
#67625=CARTESIAN_POINT('Ctrl Pts',(-26.5853998345252,21.0489788861053,-51.9587893286636));
#67626=CARTESIAN_POINT('Ctrl Pts',(-26.6579229415245,21.136981377552,-51.9645740300948));
#67627=CARTESIAN_POINT('Ctrl Pts',(-26.7267265150926,21.2282756699981,-51.9703587315259));
#67628=CARTESIAN_POINT('Ctrl Pts',(-26.7914935773824,21.3225080481983,-51.9761434329571));
#67629=CARTESIAN_POINT('Ctrl Pts',(-26.8562015787308,21.4166544961007,-51.9819228593317));
#67630=CARTESIAN_POINT('Ctrl Pts',(-26.9168801420518,21.5137333589691,-51.9877022857064));
#67631=CARTESIAN_POINT('Ctrl Pts',(-26.973252252748,21.6133576172331,-51.9934817120811));
#67632=CARTESIAN_POINT('Ctrl Pts',(-27.0295874781854,21.7129166896009,-51.9992573568759));
#67633=CARTESIAN_POINT('Ctrl Pts',(-27.0816216417915,21.8150174787474,-52.0050330016708));
#67634=CARTESIAN_POINT('Ctrl Pts',(-27.1291213003051,21.9192444578142,-52.0108086464656));
#67635=CARTESIAN_POINT('Ctrl Pts',(-27.1766021097159,22.0234300768986,-52.016581999334));
#67636=CARTESIAN_POINT('Ctrl Pts',(-27.2195518154751,22.1297398218363,-52.0223553522024));
#67637=CARTESIAN_POINT('Ctrl Pts',(-27.2577835617444,22.2377348513505,-52.0281287050708));
#67638=CARTESIAN_POINT('Ctrl Pts',(-27.2960234093541,22.3457527651056,-52.0339032813177));
#67639=CARTESIAN_POINT('Ctrl Pts',(-27.3295431476156,22.4554562793153,-52.0396778575646));
#67640=CARTESIAN_POINT('Ctrl Pts',(-27.3582047519617,22.5663882686172,-52.0454524338115));
#67641=CARTESIAN_POINT('Ctrl Pts',(-27.3868682813938,22.6773277087797,-52.0512273979138));
#67642=CARTESIAN_POINT('Ctrl Pts',(-27.4106729294253,22.7894953738474,-52.057002362016));
#67643=CARTESIAN_POINT('Ctrl Pts',(-27.4295314336681,22.9024221521192,-52.0627773261183));
#67644=CARTESIAN_POINT('Ctrl Pts',(-27.4484075946599,23.0154546609279,-52.0685576971759));
#67645=CARTESIAN_POINT('Ctrl Pts',(-27.4623282990379,23.1292472810354,-52.0743380682336));
#67646=CARTESIAN_POINT('Ctrl Pts',(-27.4712579968975,23.2433239702244,-52.0801184392912));
#67647=CARTESIAN_POINT('Ctrl Pts',(-27.4793519026867,23.3467234345241,-52.0853577855158));
#67648=CARTESIAN_POINT('Ctrl Pts',(-27.4833460130466,23.4503559848456,-52.0905971317404));
#67649=CARTESIAN_POINT('Ctrl Pts',(-27.4832508703214,23.5538675497877,-52.095836477965));
#67650=CARTESIAN_POINT('',(-27.4847156486848,23.548792864961,-53.345836477965));
#67651=CARTESIAN_POINT('Ctrl Pts',(-27.4836164097124,23.5538678857735,-52.095836477965));
#67652=CARTESIAN_POINT('Ctrl Pts',(-27.4863365027118,23.8466766674494,-52.1106557845866));
#67653=CARTESIAN_POINT('Ctrl Pts',(-27.3226060095439,25.4463805907666,-52.1917707283331));
#67654=CARTESIAN_POINT('Ctrl Pts',(-25.1349592851244,27.9239758125807,-52.3391813092048));
#67655=CARTESIAN_POINT('Ctrl Pts',(-20.7271669327941,27.2476757605631,-52.5380682205796));
#67656=CARTESIAN_POINT('Ctrl Pts',(-18.9135508876664,23.1737572510144,-52.7369551319543));
#67657=CARTESIAN_POINT('Ctrl Pts',(-21.3606705259297,19.4458059828712,-52.9358420433294));
#67658=CARTESIAN_POINT('Ctrl Pts',(-25.8198303815515,19.4894930934187,-53.1347289547041));
#67659=CARTESIAN_POINT('Ctrl Pts',(-27.4508527243426,22.083602281584,-53.2713937662495));
#67660=CARTESIAN_POINT('Ctrl Pts',(-27.4894817226864,23.4685949761432,-53.3417629406697));
#67661=CARTESIAN_POINT('Ctrl Pts',(-27.4891003288786,23.5487912382659,-53.345836477965));
#67662=CARTESIAN_POINT('',(-27.4826585752767,23.5473454798973,-54.5958364365128));
#67663=CARTESIAN_POINT('Ctrl Pts',(-27.4832522610303,23.5487934078707,-53.345836477965));
#67664=CARTESIAN_POINT('Ctrl Pts',(-27.4832946914238,23.663162540572,-53.3516544617535));
#67665=CARTESIAN_POINT('Ctrl Pts',(-27.4783442215885,23.7777353956967,-53.3574724455419));
#67666=CARTESIAN_POINT('Ctrl Pts',(-27.4683737448524,23.8920348586218,-53.3632904293304));
#67667=CARTESIAN_POINT('Ctrl Pts',(-27.4584157308707,24.006191451132,-53.3691011408383));
#67668=CARTESIAN_POINT('Ctrl Pts',(-27.4434502201329,24.1200749146401,-53.3749118523463));
#67669=CARTESIAN_POINT('Ctrl Pts',(-27.4235021021631,24.2332069700445,-53.3807225638542));
#67670=CARTESIAN_POINT('Ctrl Pts',(-27.4035733411655,24.3462292459676,-53.3865276368462));
#67671=CARTESIAN_POINT('Ctrl Pts',(-27.3786716594561,24.4585011507698,-53.3923327098383));
#67672=CARTESIAN_POINT('Ctrl Pts',(-27.3488737818166,24.5695491509951,-53.3981377828303));
#67673=CARTESIAN_POINT('Ctrl Pts',(-27.3190951784397,24.6805253216648,-53.4039391009072));
#67674=CARTESIAN_POINT('Ctrl Pts',(-27.2844267847394,24.7902787557818,-53.4097404189842));
#67675=CARTESIAN_POINT('Ctrl Pts',(-27.2449963344048,24.8983464573282,-53.4155417370611));
#67676=CARTESIAN_POINT('Ctrl Pts',(-27.2055788649269,25.0063785820212,-53.4213411452922));
#67677=CARTESIAN_POINT('Ctrl Pts',(-27.1614025985756,25.1127256813328,-53.4271405535234));
#67678=CARTESIAN_POINT('Ctrl Pts',(-27.1126447980758,25.2169409670127,-53.4329399617545));
#67679=CARTESIAN_POINT('Ctrl Pts',(-27.063890716047,25.3211483048052,-53.4387389276989));
#67680=CARTESIAN_POINT('Ctrl Pts',(-27.0105559733405,25.4232237703927,-53.4445378936432));
#67681=CARTESIAN_POINT('Ctrl Pts',(-26.9528652022628,25.52274233245,-53.4503368595876));
#67682=CARTESIAN_POINT('Ctrl Pts',(-26.8951642377128,25.6222784785972,-53.4561368501603));
#67683=CARTESIAN_POINT('Ctrl Pts',(-26.833105927028,25.7192564588746,-53.461936840733));
#67684=CARTESIAN_POINT('Ctrl Pts',(-26.7669594764301,25.8132782566226,-53.4677368313057));
#67685=CARTESIAN_POINT('Ctrl Pts',(-26.70074402803,25.9073981291327,-53.4735428718871));
#67686=CARTESIAN_POINT('Ctrl Pts',(-26.6304321681201,25.9985553167895,-53.4793489124685));
#67687=CARTESIAN_POINT('Ctrl Pts',(-26.5563348674562,26.086383046991,-53.4851549530499));
#67688=CARTESIAN_POINT('Ctrl Pts',(-26.4821965350304,26.1742594122506,-53.4909642087561));
#67689=CARTESIAN_POINT('Ctrl Pts',(-26.404268874238,26.2588023399374,-53.4967734644624));
#67690=CARTESIAN_POINT('Ctrl Pts',(-26.3229000474504,26.339681640557,-53.5025827201687));
#67691=CARTESIAN_POINT('Ctrl Pts',(-26.241401802324,26.4206895809166,-53.5084012155832));
#67692=CARTESIAN_POINT('Ctrl Pts',(-26.1564517727988,26.4980219742657,-53.5142197109978));
#67693=CARTESIAN_POINT('Ctrl Pts',(-26.0684317427574,26.5713884870873,-53.5200382064123));
#67694=CARTESIAN_POINT('Ctrl Pts',(-26.0055786143933,26.6237778676163,-53.5241930634262));
#67695=CARTESIAN_POINT('Ctrl Pts',(-25.9411607548155,26.6741458817202,-53.52834792044));
#67696=CARTESIAN_POINT('Ctrl Pts',(-25.8753256237094,26.7224007181424,-53.5325027774539));
#67697=CARTESIAN_POINT('Ctrl Pts',(-25.7822770688398,26.7906020373943,-53.5383750744226));
#67698=CARTESIAN_POINT('Ctrl Pts',(-25.686069266483,26.8548200542966,-53.5442473713914));
#67699=CARTESIAN_POINT('Ctrl Pts',(-25.5870780585296,26.9147481511343,-53.5501196683601));
#67700=CARTESIAN_POINT('Ctrl Pts',(-25.4882151353203,26.9745985859177,-53.5559843552983));
#67701=CARTESIAN_POINT('Ctrl Pts',(-25.3865763300523,27.030169944172,-53.5618490422365));
#67702=CARTESIAN_POINT('Ctrl Pts',(-25.2825689704772,27.0811969883406,-53.5677137291747));
#67703=CARTESIAN_POINT('Ctrl Pts',(-25.1786685759603,27.1321715543888,-53.5735723846495));
#67704=CARTESIAN_POINT('Ctrl Pts',(-25.0724048411793,27.1786109212852,-53.5794310401243));
#67705=CARTESIAN_POINT('Ctrl Pts',(-24.9642117995196,27.2202945190468,-53.5852896955992));
#67706=CARTESIAN_POINT('Ctrl Pts',(-24.8517926423577,27.2636063148512,-53.5913771953171));
#67707=CARTESIAN_POINT('Ctrl Pts',(-24.7372907738129,27.3017830029639,-53.597464695035));
#67708=CARTESIAN_POINT('Ctrl Pts',(-24.6212189104289,27.3346309503542,-53.6035521947529));
#67709=CARTESIAN_POINT('Ctrl Pts',(-24.5096398555892,27.3662074480203,-53.6094040648363));
#67710=CARTESIAN_POINT('Ctrl Pts',(-24.3966105208159,27.3928599319203,-53.6152559349197));
#67711=CARTESIAN_POINT('Ctrl Pts',(-24.2826033931268,27.4144667099921,-53.6211078050031));
#67712=CARTESIAN_POINT('Ctrl Pts',(-24.1686136240595,27.4360701982356,-53.6269587840861));
#67713=CARTESIAN_POINT('Ctrl Pts',(-24.0536467641348,27.4526294312334,-53.6328097631691));
#67714=CARTESIAN_POINT('Ctrl Pts',(-23.9381857489335,27.4640737870612,-53.638660742252));
#67715=CARTESIAN_POINT('Ctrl Pts',(-23.8227143526758,27.4755191718467,-53.6445122473944));
#67716=CARTESIAN_POINT('Ctrl Pts',(-23.7067491242115,27.4818487244931,-53.6503637525366));
#67717=CARTESIAN_POINT('Ctrl Pts',(-23.5907776681084,27.4830437432027,-53.6562152576789));
#67718=CARTESIAN_POINT('Ctrl Pts',(-23.4747677004092,27.484239158752,-53.6620687059787));
#67719=CARTESIAN_POINT('Ctrl Pts',(-23.3587519141009,27.480296645689,-53.6679221542785));
#67720=CARTESIAN_POINT('Ctrl Pts',(-23.243216744199,27.4712496019809,-53.6737756025783));
#67721=CARTESIAN_POINT('Ctrl Pts',(-23.1275501857212,27.4621922698196,-53.6796357075199));
#67722=CARTESIAN_POINT('Ctrl Pts',(-23.0123657469431,27.4480188527795,-53.6854958124614));
#67723=CARTESIAN_POINT('Ctrl Pts',(-22.8981436809932,27.4288145135165,-53.691355917403));
#67724=CARTESIAN_POINT('Ctrl Pts',(-22.7838446936306,27.409597241333,-53.6972199687584));
#67725=CARTESIAN_POINT('Ctrl Pts',(-22.6705097728295,27.3853423870215,-53.7030840201139));
#67726=CARTESIAN_POINT('Ctrl Pts',(-22.5586062308937,27.3561856123078,-53.7089480714693));
#67727=CARTESIAN_POINT('Ctrl Pts',(-22.4465377654753,27.3269858663284,-53.7148207652659));
#67728=CARTESIAN_POINT('Ctrl Pts',(-22.3359052827544,27.292869902692,-53.7206934590625));
#67729=CARTESIAN_POINT('Ctrl Pts',(-22.2271583576552,27.2540223418503,-53.726566152859));
#67730=CARTESIAN_POINT('Ctrl Pts',(-22.1973852686777,27.2433865295325,-53.7281739981823));
#67731=CARTESIAN_POINT('Ctrl Pts',(-22.1677533833864,27.2323963203315,-53.7297818435056));
#67732=CARTESIAN_POINT('Ctrl Pts',(-22.1382716124275,27.2210561063393,-53.7313896888289));
#67733=CARTESIAN_POINT('Ctrl Pts',(-22.0305960097272,27.1796385002506,-53.7372619857976));
#67734=CARTESIAN_POINT('Ctrl Pts',(-21.9245639189295,27.1334098224602,-53.7431342827663));
#67735=CARTESIAN_POINT('Ctrl Pts',(-21.8206364611377,27.0825205351833,-53.749006579735));
#67736=CARTESIAN_POINT('Ctrl Pts',(-21.7168436850777,27.0316971963812,-53.7548712666732));
#67737=CARTESIAN_POINT('Ctrl Pts',(-21.6151504859665,26.9762254391619,-53.7607359536114));
#67738=CARTESIAN_POINT('Ctrl Pts',(-21.516000190528,26.9163045830534,-53.7666006405496));
#67739=CARTESIAN_POINT('Ctrl Pts',(-21.4169518649613,26.8564453517943,-53.7724592960244));
#67740=CARTESIAN_POINT('Ctrl Pts',(-21.3204415929319,26.7921463353161,-53.7783179514993));
#67741=CARTESIAN_POINT('Ctrl Pts',(-21.226889557112,26.7236534657617,-53.7841766069741));
#67742=CARTESIAN_POINT('Ctrl Pts',(-21.1296832963733,26.6524852043947,-53.790264106692));
#67743=CARTESIAN_POINT('Ctrl Pts',(-21.0356714940989,26.5767889795969,-53.7963516064099));
#67744=CARTESIAN_POINT('Ctrl Pts',(-20.9452942020338,26.4968914815374,-53.8024391061278));
#67745=CARTESIAN_POINT('Ctrl Pts',(-20.8584151554361,26.4200865862109,-53.8082909762112));
#67746=CARTESIAN_POINT('Ctrl Pts',(-20.7748948264504,26.3393999078589,-53.8141428462946));
#67747=CARTESIAN_POINT('Ctrl Pts',(-20.6950909959134,26.2551631780184,-53.819994716378));
#67748=CARTESIAN_POINT('Ctrl Pts',(-20.6152993162354,26.1709392739861,-53.825845695461));
#67749=CARTESIAN_POINT('Ctrl Pts',(-20.5392232940991,26.0831666932203,-53.8316966745439));
#67750=CARTESIAN_POINT('Ctrl Pts',(-20.4671833920689,25.9922135633837,-53.8375476536269));
#67751=CARTESIAN_POINT('Ctrl Pts',(-20.3951370129583,25.9012522559856,-53.8433991587692));
#67752=CARTESIAN_POINT('Ctrl Pts',(-20.3271277320184,25.80711015512,-53.8492506639115));
#67753=CARTESIAN_POINT('Ctrl Pts',(-20.2634348543251,25.7101873815761,-53.8551021690538));
#67754=CARTESIAN_POINT('Ctrl Pts',(-20.1997208256133,25.6132324220884,-53.8609556173536));
#67755=CARTESIAN_POINT('Ctrl Pts',(-20.1403262772436,25.5134952990801,-53.8668090656534));
#67756=CARTESIAN_POINT('Ctrl Pts',(-20.0854860496932,25.4114033115082,-53.8726625139532));
#67757=CARTESIAN_POINT('Ctrl Pts',(-20.0305834568958,25.3091952231778,-53.8785226188947));
#67758=CARTESIAN_POINT('Ctrl Pts',(-19.9802457182821,25.2046272894767,-53.8843827238362));
#67759=CARTESIAN_POINT('Ctrl Pts',(-19.9346607822561,25.0981495894455,-53.8902428287778));
#67760=CARTESIAN_POINT('Ctrl Pts',(-19.8890451476287,24.9916001833476,-53.8961068801332));
#67761=CARTESIAN_POINT('Ctrl Pts',(-19.8481888342136,24.8831388359249,-53.9019709314887));
#67762=CARTESIAN_POINT('Ctrl Pts',(-19.8122303096357,24.7732320357729,-53.9078349828442));
#67763=CARTESIAN_POINT('Ctrl Pts',(-19.7762187893704,24.6631632549366,-53.9137076766408));
#67764=CARTESIAN_POINT('Ctrl Pts',(-19.7451195750291,24.55164516638,-53.9195803704373));
#67765=CARTESIAN_POINT('Ctrl Pts',(-19.7190203566335,24.4391558002109,-53.9254530642339));
#67766=CARTESIAN_POINT('Ctrl Pts',(-19.7118748272236,24.4083580934721,-53.9270609095572));
#67767=CARTESIAN_POINT('Ctrl Pts',(-19.7051037844361,24.3774876172243,-53.9286687548805));
#67768=CARTESIAN_POINT('Ctrl Pts',(-19.6987083497125,24.3465542422555,-53.9302766002038));
#67769=CARTESIAN_POINT('Ctrl Pts',(-19.6753504486774,24.2335769791884,-53.9361488971725));
#67770=CARTESIAN_POINT('Ctrl Pts',(-19.6569285708432,24.1193818420497,-53.9420211941412));
#67771=CARTESIAN_POINT('Ctrl Pts',(-19.6435653853282,24.004438110966,-53.9478934911099));
#67772=CARTESIAN_POINT('Ctrl Pts',(-19.6302195174403,23.8896433378291,-53.9537581780481));
#67773=CARTESIAN_POINT('Ctrl Pts',(-19.6219193523074,23.7741023067914,-53.9596228649863));
#67774=CARTESIAN_POINT('Ctrl Pts',(-19.6187368359544,23.6582957367187,-53.9654875519245));
#67775=CARTESIAN_POINT('Ctrl Pts',(-19.6155575926203,23.5426082664538,-53.9713462073993));
#67776=CARTESIAN_POINT('Ctrl Pts',(-19.6174855406155,23.4266562110871,-53.9772048628741));
#67777=CARTESIAN_POINT('Ctrl Pts',(-19.6245408996489,23.3109260140997,-53.9830635183489));
#67778=CARTESIAN_POINT('Ctrl Pts',(-19.6318718472204,23.1906752936839,-53.9891510180668));
#67779=CARTESIAN_POINT('Ctrl Pts',(-19.6447389866202,23.0706645685832,-53.9952385177847));
#67780=CARTESIAN_POINT('Ctrl Pts',(-19.6631053345511,22.9514406515997,-54.0013260175026));
#67781=CARTESIAN_POINT('Ctrl Pts',(-19.6807607738904,22.8368315501046,-54.007177887586));
#67782=CARTESIAN_POINT('Ctrl Pts',(-19.703497551674,22.7229499258041,-54.0130297576694));
#67783=CARTESIAN_POINT('Ctrl Pts',(-19.7312299723037,22.6102761006779,-54.0188816277528));
#67784=CARTESIAN_POINT('Ctrl Pts',(-19.7589581704201,22.4976194311662,-54.0247326068358));
#67785=CARTESIAN_POINT('Ctrl Pts',(-19.7916804002322,22.3861705964729,-54.0305835859187));
#67786=CARTESIAN_POINT('Ctrl Pts',(-19.8292601733621,22.2763981957381,-54.0364345650017));
#67787=CARTESIAN_POINT('Ctrl Pts',(-19.8668433252753,22.1666159254079,-54.042286070144));
#67788=CARTESIAN_POINT('Ctrl Pts',(-19.909284754807,22.0585107797916,-54.0481375752863));
#67789=CARTESIAN_POINT('Ctrl Pts',(-19.9563988098579,21.9525340251846,-54.0539890804286));
#67790=CARTESIAN_POINT('Ctrl Pts',(-20.0035285104608,21.8465220780046,-54.0598425287283));
#67791=CARTESIAN_POINT('Ctrl Pts',(-20.055333754154,21.7426403047825,-54.0656959770281));
#67792=CARTESIAN_POINT('Ctrl Pts',(-20.1115819883891,21.6413172539527,-54.0715494253279));
#67793=CARTESIAN_POINT('Ctrl Pts',(-20.1678941890807,21.5398789768122,-54.0774095302694));
#67794=CARTESIAN_POINT('Ctrl Pts',(-20.228659264481,21.4410055916228,-54.083269635211));
#67795=CARTESIAN_POINT('Ctrl Pts',(-20.2936001496216,21.3450985093319,-54.0891297401525));
#67796=CARTESIAN_POINT('Ctrl Pts',(-20.3585847683837,21.2491268396237,-54.0949937915079));
#67797=CARTESIAN_POINT('Ctrl Pts',(-20.4277505503387,21.1561257813653,-54.1008578428634));
#67798=CARTESIAN_POINT('Ctrl Pts',(-20.5007798784254,21.0664639865547,-54.1067218942188));
#67799=CARTESIAN_POINT('Ctrl Pts',(-20.5739168371637,20.9766700481569,-54.1125945880154));
#67800=CARTESIAN_POINT('Ctrl Pts',(-20.6509284324033,20.8902255028893,-54.118467281812));
#67801=CARTESIAN_POINT('Ctrl Pts',(-20.7314598895681,20.807462521377,-54.1243399756085));
#67802=CARTESIAN_POINT('Ctrl Pts',(-20.7535080554138,20.7848034014938,-54.1259478209319));
#67803=CARTESIAN_POINT('Ctrl Pts',(-20.7758198693633,20.7624200084848,-54.1275556662553));
#67804=CARTESIAN_POINT('Ctrl Pts',(-20.7983876331438,20.7403186214169,-54.1291635115787));
#67805=CARTESIAN_POINT('Ctrl Pts',(-20.8808113644017,20.6595982272373,-54.1350358085474));
#67806=CARTESIAN_POINT('Ctrl Pts',(-20.9669278433428,20.5823722796293,-54.1409081055161));
#67807=CARTESIAN_POINT('Ctrl Pts',(-21.0564085645817,20.5089976479831,-54.1467804024848));
#67808=CARTESIAN_POINT('Ctrl Pts',(-21.1457733259119,20.4357181040326,-54.152645089423));
#67809=CARTESIAN_POINT('Ctrl Pts',(-21.2384933427765,20.3662802104363,-54.1585097763612));
#67810=CARTESIAN_POINT('Ctrl Pts',(-21.3342030682045,20.3010043455183,-54.1643744632994));
#67811=CARTESIAN_POINT('Ctrl Pts',(-21.4298143621718,20.235795612741,-54.1702331187742));
#67812=CARTESIAN_POINT('Ctrl Pts',(-21.5284089094472,20.1747406262545,-54.176091774249));
#67813=CARTESIAN_POINT('Ctrl Pts',(-21.6295883865782,20.1181193405628,-54.1819504297239));
#67814=CARTESIAN_POINT('Ctrl Pts',(-21.7347200232035,20.0592863775806,-54.1880379294418));
#67815=CARTESIAN_POINT('Ctrl Pts',(-21.8426422941227,20.0052408333132,-54.1941254291597));
#67816=CARTESIAN_POINT('Ctrl Pts',(-21.9528751655106,19.9562471685924,-54.2002129288776));
#67817=CARTESIAN_POINT('Ctrl Pts',(-22.0588412389685,19.9091499079531,-54.206064798961));
#67818=CARTESIAN_POINT('Ctrl Pts',(-22.1669419524992,19.8667208948666,-54.2119166690444));
#67819=CARTESIAN_POINT('Ctrl Pts',(-22.2767268810583,19.8291476665806,-54.2177685391278));
#67820=CARTESIAN_POINT('Ctrl Pts',(-22.3864950938636,19.7915801591602,-54.2236195182108));
#67821=CARTESIAN_POINT('Ctrl Pts',(-22.4979466208144,19.7588671003197,-54.2294704972937));
#67822=CARTESIAN_POINT('Ctrl Pts',(-22.6106134438374,19.7311469577971,-54.2353214763767));
#67823=CARTESIAN_POINT('Ctrl Pts',(-22.7232903966919,19.703424322967,-54.241172981519));
#67824=CARTESIAN_POINT('Ctrl Pts',(-22.8371824613953,19.6806955956169,-54.2470244866612));
#67825=CARTESIAN_POINT('Ctrl Pts',(-22.9518096272116,19.6630485120839,-54.2528759918035));
#67826=CARTESIAN_POINT('Ctrl Pts',(-23.0664748582145,19.6453955683386,-54.2587294401033));
#67827=CARTESIAN_POINT('Ctrl Pts',(-23.1818752673766,19.6328276867715,-54.264582888403));
#67828=CARTESIAN_POINT('Ctrl Pts',(-23.2975246051989,19.6253808656178,-54.2704363367028));
#67829=CARTESIAN_POINT('Ctrl Pts',(-23.4133054614312,19.6179255758114,-54.2762964416444));
#67830=CARTESIAN_POINT('Ctrl Pts',(-23.5293353985815,19.615602997042,-54.2821565465859));
#67831=CARTESIAN_POINT('Ctrl Pts',(-23.6451269375236,19.6183970095369,-54.2880166515274));
#67832=CARTESIAN_POINT('Ctrl Pts',(-23.7609964548192,19.6211929036244,-54.2938807028829));
#67833=CARTESIAN_POINT('Ctrl Pts',(-23.8766268428183,19.6291122218803,-54.2997447542383));
#67834=CARTESIAN_POINT('Ctrl Pts',(-23.9915362629233,19.6420870197753,-54.3056088055937));
#67835=CARTESIAN_POINT('Ctrl Pts',(-24.1066150365761,19.6550809399324,-54.3114814993902));
#67836=CARTESIAN_POINT('Ctrl Pts',(-24.220970314878,19.6731451457655,-54.3173541931868));
#67837=CARTESIAN_POINT('Ctrl Pts',(-24.3341308664104,19.6961607117757,-54.3232268869834));
#67838=CARTESIAN_POINT('Ctrl Pts',(-24.3651123324764,19.7024619887462,-54.3248347323068));
#67839=CARTESIAN_POINT('Ctrl Pts',(-24.3960043378739,19.7091341193543,-54.3264425776302));
#67840=CARTESIAN_POINT('Ctrl Pts',(-24.4267974386757,19.7161740210159,-54.3280504229536));
#67841=CARTESIAN_POINT('Ctrl Pts',(-24.5392623815807,19.7418856940145,-54.3339227199223));
#67842=CARTESIAN_POINT('Ctrl Pts',(-24.6507834746237,19.7725930341088,-54.339795016891));
#67843=CARTESIAN_POINT('Ctrl Pts',(-24.7608829065119,19.8082125672405,-54.3456673138597));
#67844=CARTESIAN_POINT('Ctrl Pts',(-24.8708396582798,19.843785940286,-54.3515320007979));
#67845=CARTESIAN_POINT('Ctrl Pts',(-24.9793780230043,19.8842587209834,-54.3573966877361));
#67846=CARTESIAN_POINT('Ctrl Pts',(-25.0860308673914,19.9294965465989,-54.3632613746743));
#67847=CARTESIAN_POINT('Ctrl Pts',(-25.1925740260051,19.974687847943,-54.3691200301491));
#67848=CARTESIAN_POINT('Ctrl Pts',(-25.2972351430538,20.024634286309,-54.3749786856239));
#67849=CARTESIAN_POINT('Ctrl Pts',(-25.3995633774041,20.0791520727706,-54.3808373410988));
#67850=CARTESIAN_POINT('Ctrl Pts',(-25.5058886427174,20.1357993719899,-54.3869248408167));
#67851=CARTESIAN_POINT('Ctrl Pts',(-25.6096946284807,20.1973822814309,-54.3930123405346));
#67852=CARTESIAN_POINT('Ctrl Pts',(-25.7104993607264,20.2636398928734,-54.3990998402525));
#67853=CARTESIAN_POINT('Ctrl Pts',(-25.8074022312365,20.3273328624284,-54.4049517103359));
#67854=CARTESIAN_POINT('Ctrl Pts',(-25.9015314902085,20.3953451261955,-54.4108035804193));
#67855=CARTESIAN_POINT('Ctrl Pts',(-25.9924858855782,20.4673991058602,-54.4166554505027));
#67856=CARTESIAN_POINT('Ctrl Pts',(-26.0834264323143,20.5394421146514,-54.4225064295857));
#67857=CARTESIAN_POINT('Ctrl Pts',(-26.1711927526675,20.6155253591283,-54.4283574086687));
#67858=CARTESIAN_POINT('Ctrl Pts',(-26.255415367797,20.6953299355161,-54.4342083877517));
#67859=CARTESIAN_POINT('Ctrl Pts',(-26.3396455553504,20.7751416871035,-54.440059892894));
#67860=CARTESIAN_POINT('Ctrl Pts',(-26.4203311042185,20.8586751513766,-54.4459113980363));
#67861=CARTESIAN_POINT('Ctrl Pts',(-26.4971387341967,20.9455739124591,-54.4517629031787));
#67862=CARTESIAN_POINT('Ctrl Pts',(-26.5739718703161,21.0325015307277,-54.4576163514784));
#67863=CARTESIAN_POINT('Ctrl Pts',(-26.6469242532682,21.1227963583951,-54.4634697997782));
#67864=CARTESIAN_POINT('Ctrl Pts',(-26.7157027586656,21.2160687641715,-54.4693232480779));
#67865=CARTESIAN_POINT('Ctrl Pts',(-26.7845594801588,21.3094472409272,-54.4751833530195));
#67866=CARTESIAN_POINT('Ctrl Pts',(-26.8492326045341,21.4058097215448,-54.481043457961));
#67867=CARTESIAN_POINT('Ctrl Pts',(-26.9094721904934,21.504737368236,-54.4869035629026));
#67868=CARTESIAN_POINT('Ctrl Pts',(-26.9697523440433,21.6037316365053,-54.492767614258));
#67869=CARTESIAN_POINT('Ctrl Pts',(-27.0255928153559,21.7052941492456,-54.4986316656134));
#67870=CARTESIAN_POINT('Ctrl Pts',(-27.0767903131154,21.8089828006621,-54.5044957169689));
#67871=CARTESIAN_POINT('Ctrl Pts',(-27.128063265767,21.9128242684532,-54.5103684107655));
#67872=CARTESIAN_POINT('Ctrl Pts',(-27.1746794221004,22.0187977518191,-54.5162411045621));
#67873=CARTESIAN_POINT('Ctrl Pts',(-27.2164841155747,22.1264425115873,-54.5221137983587));
#67874=CARTESIAN_POINT('Ctrl Pts',(-27.2279295413405,22.1559138461338,-54.5237216436819));
#67875=CARTESIAN_POINT('Ctrl Pts',(-27.2390146044347,22.1855103780317,-54.5253294890052));
#67876=CARTESIAN_POINT('Ctrl Pts',(-27.2497367934444,22.2152224956791,-54.5269373343285));
#67877=CARTESIAN_POINT('Ctrl Pts',(-27.2951872236293,22.3411695879713,-54.5337528513416));
#67878=CARTESIAN_POINT('Ctrl Pts',(-27.3342388739079,22.469541534013,-54.5405683683548));
#67879=CARTESIAN_POINT('Ctrl Pts',(-27.3666634540376,22.5997281123246,-54.547383885368));
#67880=CARTESIAN_POINT('Ctrl Pts',(-27.3989473711172,22.7293499202949,-54.5541698355708));
#67881=CARTESIAN_POINT('Ctrl Pts',(-27.4246614926118,22.8607705276024,-54.5609557857736));
#67882=CARTESIAN_POINT('Ctrl Pts',(-27.4436271962016,22.9933658989116,-54.5677417359765));
#67883=CARTESIAN_POINT('Ctrl Pts',(-27.4624434598956,23.1249164875493,-54.5744742164155));
#67884=CARTESIAN_POINT('Ctrl Pts',(-27.4746171475041,23.2576232611374,-54.5812066968546));
#67885=CARTESIAN_POINT('Ctrl Pts',(-27.4800212497374,23.3908573539461,-54.5879391772936));
#67886=CARTESIAN_POINT('Ctrl Pts',(-27.4821342678033,23.4429522316802,-54.5905715947022));
#67887=CARTESIAN_POINT('Ctrl Pts',(-27.4832128530943,23.4951275274992,-54.5932040121107));
#67888=CARTESIAN_POINT('Ctrl Pts',(-27.4832514569032,23.5473449030032,-54.5958364295193));
#67889=CARTESIAN_POINT('',(-27.4785230664524,23.5528363097046,-55.8458364779651));
#67890=CARTESIAN_POINT('Ctrl Pts',(-27.4791444786054,23.5473488992339,-54.595836477965));
#67891=CARTESIAN_POINT('Ctrl Pts',(-27.4732958893268,24.4059475501821,-54.6391657338778));
#67892=CARTESIAN_POINT('Ctrl Pts',(-26.7733364796375,26.5869150425722,-54.7487906269156));
#67893=CARTESIAN_POINT('Ctrl Pts',(-23.1677904881242,28.1864658159741,-54.9247111570782));
#67894=CARTESIAN_POINT('Ctrl Pts',(-19.4429915598308,25.7345506205814,-55.123598068453));
#67895=CARTESIAN_POINT('Ctrl Pts',(-19.4924172263766,21.2754506794386,-55.3224849798281));
#67896=CARTESIAN_POINT('Ctrl Pts',(-23.2706494908114,18.9067007691274,-55.5213718912028));
#67897=CARTESIAN_POINT('Ctrl Pts',(-26.810029366777,20.5717473545874,-55.6958223905819));
#67898=CARTESIAN_POINT('Ctrl Pts',(-27.4735450541292,22.7230378512852,-55.803977252836));
#67899=CARTESIAN_POINT('Ctrl Pts',(-27.4785230664524,23.5528363097046,-55.8458364779651));
#67900=CARTESIAN_POINT('',(-27.4885926759417,23.5521866781829,-57.095836477965));
#67901=CARTESIAN_POINT('Ctrl Pts',(-27.4785230664524,23.5528363097046,-55.8458364779651));
#67902=CARTESIAN_POINT('Ctrl Pts',(-27.4814291106918,24.0372527541313,-55.8702728899609));
#67903=CARTESIAN_POINT('Ctrl Pts',(-27.1735715217939,25.832320235274,-55.9610049390818));
#67904=CARTESIAN_POINT('Ctrl Pts',(-24.4862566433993,28.1070767695796,-56.1180326253275));
#67905=CARTESIAN_POINT('Ctrl Pts',(-20.2224697472459,26.8008851734482,-56.3169195367025));
#67906=CARTESIAN_POINT('Ctrl Pts',(-19.0166330805488,22.5076377877433,-56.5158064480773));
#67907=CARTESIAN_POINT('Ctrl Pts',(-21.9768083019133,19.1724649525765,-56.7146933594523));
#67908=CARTESIAN_POINT('Ctrl Pts',(-26.2600360440162,19.840941083895,-56.9080367027482));
#67909=CARTESIAN_POINT('Ctrl Pts',(-27.4813781435483,22.3557441605591,-57.035084408919));
#67910=CARTESIAN_POINT('Ctrl Pts',(-27.4885926759417,23.5521866781829,-57.095836477965));
#67911=CARTESIAN_POINT('',(-27.4832509534939,23.5467291638537,-58.345836477965));
#67912=CARTESIAN_POINT('Ctrl Pts',(-27.4885926759417,23.5521866781829,-57.095836477965));
#67913=CARTESIAN_POINT('Ctrl Pts',(-27.4892509951086,23.6613609113114,-57.101380046044));
#67914=CARTESIAN_POINT('Ctrl Pts',(-27.435543248894,25.0754943551076,-57.1732192512479));
#67915=CARTESIAN_POINT('Ctrl Pts',(-25.7292630861362,27.6603211242788,-57.3113540935769));
#67916=CARTESIAN_POINT('Ctrl Pts',(-21.2702304444974,27.6051569835892,-57.5102410049518));
#67917=CARTESIAN_POINT('Ctrl Pts',(-18.9063447869989,23.8238794508129,-57.7091279163267));
#67918=CARTESIAN_POINT('Ctrl Pts',(-20.8098166084289,19.7911619791023,-57.9080148277016));
#67919=CARTESIAN_POINT('Ctrl Pts',(-25.23151669269,19.2127300069044,-58.1069017390765));
#67920=CARTESIAN_POINT('Ctrl Pts',(-27.3424452633267,21.7130223291607,-58.2528422891643));
#67921=CARTESIAN_POINT('Ctrl Pts',(-27.4869488375757,23.2831178661222,-58.3324872021271));
#67922=CARTESIAN_POINT('Ctrl Pts',(-27.4845052556721,23.5467280401899,-58.345836477965));
#67923=CARTESIAN_POINT('',(-27.4832525204106,23.5499546106029,-59.5958364779354));
#67924=CARTESIAN_POINT('Ctrl Pts',(-27.4832509534939,23.5467291638537,-58.345836477965));
#67925=CARTESIAN_POINT('Ctrl Pts',(-27.4833531170139,23.6607703259115,-58.3516134412877));
#67926=CARTESIAN_POINT('Ctrl Pts',(-27.4784909918628,23.7749723276717,-58.3573904046104));
#67927=CARTESIAN_POINT('Ctrl Pts',(-27.4686493474181,23.8888605565914,-58.363167367933));
#67928=CARTESIAN_POINT('Ctrl Pts',(-27.4586046141927,24.0050989437275,-58.3690635426786));
#67929=CARTESIAN_POINT('Ctrl Pts',(-27.4433725210574,24.1210100185658,-58.3749597174241));
#67930=CARTESIAN_POINT('Ctrl Pts',(-27.4229929270286,24.2360883942338,-58.3808558921697));
#67931=CARTESIAN_POINT('Ctrl Pts',(-27.4030531299606,24.3486833485048,-58.3866248259246));
#67932=CARTESIAN_POINT('Ctrl Pts',(-27.3781858356613,24.4604807384687,-58.3923937596795));
#67933=CARTESIAN_POINT('Ctrl Pts',(-27.3484806902701,24.5710129616683,-58.3981626934344));
#67934=CARTESIAN_POINT('Ctrl Pts',(-27.3187822067082,24.681520396341,-58.4039303334184));
#67935=CARTESIAN_POINT('Ctrl Pts',(-27.2842481385667,24.790762816491,-58.4096979734024));
#67936=CARTESIAN_POINT('Ctrl Pts',(-27.2450187657923,24.8982849776571,-58.4154656133865));
#67937=CARTESIAN_POINT('Ctrl Pts',(-27.2057880539103,25.0058108091275,-58.4212334502508));
#67938=CARTESIAN_POINT('Ctrl Pts',(-27.1618618658653,25.111615864635,-58.4270012871151));
#67939=CARTESIAN_POINT('Ctrl Pts',(-27.113429356445,25.215263016814,-58.4327691239794));
#67940=CARTESIAN_POINT('Ctrl Pts',(-27.0631128439418,25.3229419971303,-58.4387613271333));
#67941=CARTESIAN_POINT('Ctrl Pts',(-27.0079325042467,25.4282913250685,-58.4447535302872));
#67942=CARTESIAN_POINT('Ctrl Pts',(-26.9481532417051,25.5308483422793,-58.4507457334411));
#67943=CARTESIAN_POINT('Ctrl Pts',(-26.8905314358294,25.6297040371419,-58.4565216756696));
#67944=CARTESIAN_POINT('Ctrl Pts',(-26.8286372096835,25.7259651579475,-58.4622976178982));
#67945=CARTESIAN_POINT('Ctrl Pts',(-26.7627516086389,25.8192476133614,-58.4680735601267));
#67946=CARTESIAN_POINT('Ctrl Pts',(-26.6968214320502,25.9125931799275,-58.473853410125));
#67947=CARTESIAN_POINT('Ctrl Pts',(-26.6268947686452,26.0029557362783,-58.4796332601234));
#67948=CARTESIAN_POINT('Ctrl Pts',(-26.5532921780326,26.0899851716624,-58.4854131101218));
#67949=CARTESIAN_POINT('Ctrl Pts',(-26.4795853896802,26.1771378129063,-58.4912011425402));
#67950=CARTESIAN_POINT('Ctrl Pts',(-26.4021925845177,26.2609476126844,-58.4969891749585));
#67951=CARTESIAN_POINT('Ctrl Pts',(-26.3214700984561,26.3411022585104,-58.5027772073768));
#67952=CARTESIAN_POINT('Ctrl Pts',(-26.3126449986922,26.3498652783388,-58.5034099921933));
#67953=CARTESIAN_POINT('Ctrl Pts',(-26.3037801325963,26.3585846517521,-58.5040427770098));
#67954=CARTESIAN_POINT('Ctrl Pts',(-26.294875988009,26.3672600011636,-58.5046755618263));
#67955=CARTESIAN_POINT('Ctrl Pts',(-26.2122447681908,26.447767982273,-58.510547858795));
#67956=CARTESIAN_POINT('Ctrl Pts',(-26.125929807076,26.5247720238348,-58.5164201557637));
#67957=CARTESIAN_POINT('Ctrl Pts',(-26.0362605274874,26.5979161031621,-58.5222924527324));
#67958=CARTESIAN_POINT('Ctrl Pts',(-25.9467074521637,26.6709653935715,-58.5281571396706));
#67959=CARTESIAN_POINT('Ctrl Pts',(-25.8538090202221,26.7401644104525,-58.5340218266088));
#67960=CARTESIAN_POINT('Ctrl Pts',(-25.7579316020259,26.8051937174024,-58.539886513547));
#67961=CARTESIAN_POINT('Ctrl Pts',(-25.6621527877523,26.8701561457809,-58.5457451690218));
#67962=CARTESIAN_POINT('Ctrl Pts',(-25.5634014211407,26.9309571632031,-58.5516038244966));
#67963=CARTESIAN_POINT('Ctrl Pts',(-25.4620765448829,26.9873178413145,-58.5574624799714));
#67964=CARTESIAN_POINT('Ctrl Pts',(-25.3567938297124,27.0458800171548,-58.5635499796894));
#67965=CARTESIAN_POINT('Ctrl Pts',(-25.2487328115532,27.0996476074849,-58.5696374794073));
#67966=CARTESIAN_POINT('Ctrl Pts',(-25.1383742033206,27.1483573878804,-58.5757249791252));
#67967=CARTESIAN_POINT('Ctrl Pts',(-25.0322872599303,27.1951817525414,-58.5815768492086));
#67968=CARTESIAN_POINT('Ctrl Pts',(-24.9240776988716,27.2373323908853,-58.587428719292));
#67969=CARTESIAN_POINT('Ctrl Pts',(-24.814196426388,27.2746229256086,-58.5932805893754));
#67970=CARTESIAN_POINT('Ctrl Pts',(-24.7043318843272,27.311907782509,-58.5991315684583));
#67971=CARTESIAN_POINT('Ctrl Pts',(-24.5927965282824,27.3443338743237,-58.6049825475413));
#67972=CARTESIAN_POINT('Ctrl Pts',(-24.4800587311707,27.3717639383781,-58.6108335266243));
#67973=CARTESIAN_POINT('Ctrl Pts',(-24.3673107978464,27.3991964686591,-58.6166850317666));
#67974=CARTESIAN_POINT('Ctrl Pts',(-24.2533606102291,27.4216319804953,-58.6225365369089));
#67975=CARTESIAN_POINT('Ctrl Pts',(-24.1386884032842,27.4389839733119,-58.6283880420511));
#67976=CARTESIAN_POINT('Ctrl Pts',(-24.0239781161958,27.4563417283476,-58.6342414903509));
#67977=CARTESIAN_POINT('Ctrl Pts',(-23.908545741532,27.4686125458159,-58.6400949386507));
#67978=CARTESIAN_POINT('Ctrl Pts',(-23.7928776198352,27.4757616791303,-58.6459483869504));
#67979=CARTESIAN_POINT('Ctrl Pts',(-23.6770779583671,27.4829189425617,-58.6518084918919));
#67980=CARTESIAN_POINT('Ctrl Pts',(-23.5610424275956,27.4849428708623,-58.6576685968335));
#67981=CARTESIAN_POINT('Ctrl Pts',(-23.4452584635423,27.4818508384459,-58.663528701775));
#67982=CARTESIAN_POINT('Ctrl Pts',(-23.329396526236,27.4787567237392,-58.6693927531304));
#67983=CARTESIAN_POINT('Ctrl Pts',(-23.2137869043208,27.4705398173157,-58.6752568044859));
#67984=CARTESIAN_POINT('Ctrl Pts',(-23.0989112599195,27.4572693036563,-58.6811208558413));
#67985=CARTESIAN_POINT('Ctrl Pts',(-22.9838663117496,27.4439792319087,-58.6869935496379));
#67986=CARTESIAN_POINT('Ctrl Pts',(-22.8695579066507,27.4256207534428,-58.6928662434344));
#67987=CARTESIAN_POINT('Ctrl Pts',(-22.7564569683847,27.4023140062387,-58.698738937231));
#67988=CARTESIAN_POINT('Ctrl Pts',(-22.725491823434,27.3959330087283,-58.7003467825544));
#67989=CARTESIAN_POINT('Ctrl Pts',(-22.6946170933743,27.3891813890662,-58.7019546278778));
#67990=CARTESIAN_POINT('Ctrl Pts',(-22.6638422141674,27.3820622541337,-58.7035624732012));
#67991=CARTESIAN_POINT('Ctrl Pts',(-22.5514438215795,27.3560611992588,-58.7094347701699));
#67992=CARTESIAN_POINT('Ctrl Pts',(-22.4400021337872,27.3250669231564,-58.7153070671386));
#67993=CARTESIAN_POINT('Ctrl Pts',(-22.3299947456515,27.2891641294191,-58.7211793641073));
#67994=CARTESIAN_POINT('Ctrl Pts',(-22.2201299183543,27.2533078628513,-58.7270440510455));
#67995=CARTESIAN_POINT('Ctrl Pts',(-22.1116960837057,27.2125558555647,-58.7329087379837));
#67996=CARTESIAN_POINT('Ctrl Pts',(-22.0051600276238,27.1670436721757,-58.7387734249219));
#67997=CARTESIAN_POINT('Ctrl Pts',(-21.8987335372064,27.1215782952182,-58.7446320803967));
#67998=CARTESIAN_POINT('Ctrl Pts',(-21.7942013210934,27.0713626410679,-58.7504907358715));
#67999=CARTESIAN_POINT('Ctrl Pts',(-21.6920137458813,27.0165816584363,-58.7563493913463));
#68000=CARTESIAN_POINT('Ctrl Pts',(-21.5858346339755,26.9596608823725,-58.7624368910642));
#68001=CARTESIAN_POINT('Ctrl Pts',(-21.4821874967579,26.897810996664,-58.7685243907821));
#68002=CARTESIAN_POINT('Ctrl Pts',(-21.3815536350633,26.8312941491919,-58.7746118905));
#68003=CARTESIAN_POINT('Ctrl Pts',(-21.284815021196,26.7673519778897,-58.7804637605834));
#68004=CARTESIAN_POINT('Ctrl Pts',(-21.1908611268622,26.6990976655215,-58.7863156306668));
#68005=CARTESIAN_POINT('Ctrl Pts',(-21.1000924883545,26.6268098222418,-58.7921675007502));
#68006=CARTESIAN_POINT('Ctrl Pts',(-21.0093376701973,26.5545329854436,-58.7980184798332));
#68007=CARTESIAN_POINT('Ctrl Pts',(-20.9217674668391,26.4782240963009,-58.8038694589162));
#68008=CARTESIAN_POINT('Ctrl Pts',(-20.8377505350885,26.3982030085125,-58.8097204379991));
#68009=CARTESIAN_POINT('Ctrl Pts',(-20.7537260494073,26.3181747260585,-58.8155719431414));
#68010=CARTESIAN_POINT('Ctrl Pts',(-20.6732557697725,26.234433866588,-58.8214234482837));
#68011=CARTESIAN_POINT('Ctrl Pts',(-20.5966720579262,26.1473377026072,-58.827274953426));
#68012=CARTESIAN_POINT('Ctrl Pts',(-20.5200629142958,26.0602126158858,-58.8331284017258));
#68013=CARTESIAN_POINT('Ctrl Pts',(-20.4473431776449,25.969730319366,-58.8389818500256));
#68014=CARTESIAN_POINT('Ctrl Pts',(-20.3788049685402,25.8762811975031,-58.8448352983254));
#68015=CARTESIAN_POINT('Ctrl Pts',(-20.3101888166095,25.7827258036972,-58.850695403267));
#68016=CARTESIAN_POINT('Ctrl Pts',(-20.2457639282949,25.6861971838331,-58.8565555082085));
#68017=CARTESIAN_POINT('Ctrl Pts',(-20.1857791660443,25.5871148176213,-58.86241561315));
#68018=CARTESIAN_POINT('Ctrl Pts',(-20.1257540078105,25.4879657256372,-58.8682796645055));
#68019=CARTESIAN_POINT('Ctrl Pts',(-20.0701751273649,25.3862598247315,-58.8741437158609));
#68020=CARTESIAN_POINT('Ctrl Pts',(-20.0192446774394,25.2824397424745,-58.8800077672164));
#68021=CARTESIAN_POINT('Ctrl Pts',(-19.9682391661974,25.1784666501408,-58.8858804610129));
#68022=CARTESIAN_POINT('Ctrl Pts',(-19.9218959233207,25.0723735351543,-58.8917531548095));
#68023=CARTESIAN_POINT('Ctrl Pts',(-19.8803684289681,24.9646215332487,-58.8976258486061));
#68024=CARTESIAN_POINT('Ctrl Pts',(-19.8689988956845,24.9351208375979,-58.8992336939294));
#68025=CARTESIAN_POINT('Ctrl Pts',(-19.8579900461171,24.9054958725272,-58.9008415392527));
#68026=CARTESIAN_POINT('Ctrl Pts',(-19.8473443669317,24.8757562560705,-58.902449384576));
#68027=CARTESIAN_POINT('Ctrl Pts',(-19.8084633945502,24.7671389301154,-58.9083216815447));
#68028=CARTESIAN_POINT('Ctrl Pts',(-19.7743004424646,24.6566274482055,-58.9141939785134));
#68029=CARTESIAN_POINT('Ctrl Pts',(-19.7450424083901,24.5446694047933,-58.9200662754821));
#68030=CARTESIAN_POINT('Ctrl Pts',(-19.7158222904042,24.432856450114,-58.9259309624203));
#68031=CARTESIAN_POINT('Ctrl Pts',(-19.6914945534176,24.3196010581559,-58.9317956493585));
#68032=CARTESIAN_POINT('Ctrl Pts',(-19.6721974622212,24.2053692221658,-58.9376603362967));
#68033=CARTESIAN_POINT('Ctrl Pts',(-19.652920216875,24.0912548664679,-58.9435189917715));
#68034=CARTESIAN_POINT('Ctrl Pts',(-19.6386633949981,23.9761664693238,-58.9493776472463));
#68035=CARTESIAN_POINT('Ctrl Pts',(-19.629514838374,23.8605829043263,-58.9552363027212));
#68036=CARTESIAN_POINT('Ctrl Pts',(-19.6200089310701,23.7404845434751,-58.9613238024391));
#68037=CARTESIAN_POINT('Ctrl Pts',(-19.6160186060692,23.6198519826886,-58.967411302157));
#68038=CARTESIAN_POINT('Ctrl Pts',(-19.6175834774655,23.4992318504771,-58.9734988018749));
#68039=CARTESIAN_POINT('Ctrl Pts',(-19.6190877771834,23.3832805772363,-58.9793506719583));
#68040=CARTESIAN_POINT('Ctrl Pts',(-19.6257252124908,23.2673412402109,-58.9852025420417));
#68041=CARTESIAN_POINT('Ctrl Pts',(-19.6374778908361,23.1519014179038,-58.9910544121251));
#68042=CARTESIAN_POINT('Ctrl Pts',(-19.6492287797293,23.0364791723595,-58.996905391208));
#68043=CARTESIAN_POINT('Ctrl Pts',(-19.6660933212149,22.9215567014546,-59.002756370291));
#68044=CARTESIAN_POINT('Ctrl Pts',(-19.6880016916431,22.8076170568317,-59.008607349374));
#68045=CARTESIAN_POINT('Ctrl Pts',(-19.7099120318445,22.6936671679382,-59.0144588545163));
#68046=CARTESIAN_POINT('Ctrl Pts',(-19.7368670244221,22.5807006869601,-59.0203103596586));
#68047=CARTESIAN_POINT('Ctrl Pts',(-19.7687457456332,22.4691903563431,-59.0261618648009));
#68048=CARTESIAN_POINT('Ctrl Pts',(-19.8006350530737,22.3576429955728,-59.0320153131006));
#68049=CARTESIAN_POINT('Ctrl Pts',(-19.8374512268016,22.2475531439335,-59.0378687614004));
#68050=CARTESIAN_POINT('Ctrl Pts',(-19.8790237333752,22.1393775867069,-59.0437222097002));
#68051=CARTESIAN_POINT('Ctrl Pts',(-19.9206435169159,22.031079010382,-59.0495823146417));
#68052=CARTESIAN_POINT('Ctrl Pts',(-19.9670302810896,21.924699459731,-59.0554424195833));
#68053=CARTESIAN_POINT('Ctrl Pts',(-20.017965631281,21.8206750534733,-59.0613025245248));
#68054=CARTESIAN_POINT('Ctrl Pts',(-20.0689352832428,21.7165805932883,-59.0671665758803));
#68055=CARTESIAN_POINT('Ctrl Pts',(-20.1244594230848,21.6148447975942,-59.0730306272357));
#68056=CARTESIAN_POINT('Ctrl Pts',(-20.184274932927,21.5158769998424,-59.0788946785912));
#68057=CARTESIAN_POINT('Ctrl Pts',(-20.2441785988902,21.4167633433127,-59.0847673723878));
#68058=CARTESIAN_POINT('Ctrl Pts',(-20.3083860291805,21.3204261692656,-59.0906400661843));
#68059=CARTESIAN_POINT('Ctrl Pts',(-20.3765922251004,21.2272438665465,-59.0965127599809));
#68060=CARTESIAN_POINT('Ctrl Pts',(-20.3952659405929,21.2017321108117,-59.0981206053042));
#68061=CARTESIAN_POINT('Ctrl Pts',(-20.4142391708724,21.1764566314493,-59.0997284506276));
#68062=CARTESIAN_POINT('Ctrl Pts',(-20.433505168274,21.1514247194882,-59.1013362959509));
#68063=CARTESIAN_POINT('Ctrl Pts',(-20.5038699331547,21.0600012357751,-59.1072085929196));
#68064=CARTESIAN_POINT('Ctrl Pts',(-20.5783785732018,20.9715232301045,-59.1130808898883));
#68065=CARTESIAN_POINT('Ctrl Pts',(-20.6567555458308,20.8863898864365,-59.118953186857));
#68066=CARTESIAN_POINT('Ctrl Pts',(-20.7350309481279,20.8013668688207,-59.1248178737952));
#68067=CARTESIAN_POINT('Ctrl Pts',(-20.817164436442,20.7196801949267,-59.1306825607334));
#68068=CARTESIAN_POINT('Ctrl Pts',(-20.9028387008172,20.6416980783478,-59.1365472476716));
#68069=CARTESIAN_POINT('Ctrl Pts',(-20.9884248545749,20.5637961614939,-59.1424059031464));
#68070=CARTESIAN_POINT('Ctrl Pts',(-21.07754423746,20.4895915004444,-59.1482645586213));
#68071=CARTESIAN_POINT('Ctrl Pts',(-21.1698414472921,20.4194168494433,-59.1541232140961));
#68072=CARTESIAN_POINT('Ctrl Pts',(-21.2657438674344,20.3465011147652,-59.160210713814));
#68073=CARTESIAN_POINT('Ctrl Pts',(-21.3650771250021,20.277936974309,-59.1662982135319));
#68074=CARTESIAN_POINT('Ctrl Pts',(-21.4674027453553,20.2140532319599,-59.1723857132498));
#68075=CARTESIAN_POINT('Ctrl Pts',(-21.5657676347611,20.1526422458421,-59.1782375833332));
#68076=CARTESIAN_POINT('Ctrl Pts',(-21.6668971594238,20.0955563048513,-59.1840894534166));
#68077=CARTESIAN_POINT('Ctrl Pts',(-21.7703714396855,20.0430439125343,-59.1899413235));
#68078=CARTESIAN_POINT('Ctrl Pts',(-21.8738299650472,19.9905395157064,-59.195792302583));
#68079=CARTESIAN_POINT('Ctrl Pts',(-21.9796321676288,19.9426074699822,-59.201643281666));
#68080=CARTESIAN_POINT('Ctrl Pts',(-22.0873339053358,19.8994501414444,-59.207494260749));
#68081=CARTESIAN_POINT('Ctrl Pts',(-22.1950453264651,19.8562889326476,-59.2133457658912));
#68082=CARTESIAN_POINT('Ctrl Pts',(-22.3046562384826,19.817903448203,-59.2191972710335));
#68083=CARTESIAN_POINT('Ctrl Pts',(-22.4157035508278,19.7844474902701,-59.2250487761758));
#68084=CARTESIAN_POINT('Ctrl Pts',(-22.5267877395681,19.7509804223419,-59.2309022244756));
#68085=CARTESIAN_POINT('Ctrl Pts',(-22.6393088815149,19.722446255159,-59.2367556727753));
#68086=CARTESIAN_POINT('Ctrl Pts',(-22.7527904949922,19.6989484278848,-59.2426091210751));
#68087=CARTESIAN_POINT('Ctrl Pts',(-22.8664011617061,19.6754238784785,-59.2484692260166));
#68088=CARTESIAN_POINT('Ctrl Pts',(-22.9809740750415,19.6569471845903,-59.2543293309582));
#68089=CARTESIAN_POINT('Ctrl Pts',(-23.0960242694544,19.6435703478222,-59.2601894358997));
#68090=CARTESIAN_POINT('Ctrl Pts',(-23.2111519429727,19.6301845025918,-59.2660534872552));
#68091=CARTESIAN_POINT('Ctrl Pts',(-23.3267571262581,19.6219053825794,-59.2719175386106));
#68092=CARTESIAN_POINT('Ctrl Pts',(-23.4423532138419,19.6187328843813,-59.2777815899661));
#68093=CARTESIAN_POINT('Ctrl Pts',(-23.5581196669834,19.6155557105542,-59.2836542837626));
#68094=CARTESIAN_POINT('Ctrl Pts',(-23.6738765858963,19.6175001723504,-59.2895269775592));
#68095=CARTESIAN_POINT('Ctrl Pts',(-23.7891407609701,19.6245142044603,-59.2953996713558));
#68096=CARTESIAN_POINT('Ctrl Pts',(-23.8206981639717,19.6264345291216,-59.2970075166791));
#68097=CARTESIAN_POINT('Ctrl Pts',(-23.8522186841367,19.6287345579943,-59.2986153620025));
#68098=CARTESIAN_POINT('Ctrl Pts',(-23.883692540001,19.6314125552649,-59.3002232073259));
#68099=CARTESIAN_POINT('Ctrl Pts',(-23.9986437891668,19.641193343893,-59.3060955042946));
#68100=CARTESIAN_POINT('Ctrl Pts',(-24.1133568984343,19.6560525999751,-59.3119678012633));
#68101=CARTESIAN_POINT('Ctrl Pts',(-24.2273470851922,19.675974280765,-59.317840098232));
#68102=CARTESIAN_POINT('Ctrl Pts',(-24.341189549721,19.6958701446386,-59.3237047851702));
#68103=CARTESIAN_POINT('Ctrl Pts',(-24.4543105513467,19.7208153162297,-59.3295694721084));
#68104=CARTESIAN_POINT('Ctrl Pts',(-24.5662287863124,19.750741872405,-59.3354341590466));
#68105=CARTESIAN_POINT('Ctrl Pts',(-24.6780319203796,19.7806376509907,-59.3412928145214));
#68106=CARTESIAN_POINT('Ctrl Pts',(-24.7886343512326,19.8155045180228,-59.3471514699962));
#68107=CARTESIAN_POINT('Ctrl Pts',(-24.8975640171979,19.8552233354591,-59.353010125471));
#68108=CARTESIAN_POINT('Ctrl Pts',(-25.0107485718599,19.8964936048884,-59.3590976251889));
#68109=CARTESIAN_POINT('Ctrl Pts',(-25.1221265703629,19.9430025165613,-59.3651851249068));
#68110=CARTESIAN_POINT('Ctrl Pts',(-25.2311843703503,19.9945589068451,-59.3712726246247));
#68111=CARTESIAN_POINT('Ctrl Pts',(-25.3360208560475,20.0441196972996,-59.3771244947081));
#68112=CARTESIAN_POINT('Ctrl Pts',(-25.4387130112703,20.0983442920242,-59.3829763647915));
#68113=CARTESIAN_POINT('Ctrl Pts',(-25.5388248030602,20.1570137659198,-59.3888282348749));
#68114=CARTESIAN_POINT('Ctrl Pts',(-25.6389213519195,20.2156743068545,-59.3946792139579));
#68115=CARTESIAN_POINT('Ctrl Pts',(-25.7364379619719,20.2787781723643,-59.4005301930409));
#68116=CARTESIAN_POINT('Ctrl Pts',(-25.8309643016064,20.3460610856998,-59.4063811721238));
#68117=CARTESIAN_POINT('Ctrl Pts',(-25.9254991400683,20.4133500484165,-59.4122326772661));
#68118=CARTESIAN_POINT('Ctrl Pts',(-26.0170428368545,20.4848185661572,-59.4180841824084));
#68119=CARTESIAN_POINT('Ctrl Pts',(-26.105215675548,20.560160169651,-59.4239356875507));
#68120=CARTESIAN_POINT('Ctrl Pts',(-26.1934177945225,20.6355267924519,-59.4297891358505));
#68121=CARTESIAN_POINT('Ctrl Pts',(-26.2782465154595,20.7147687900684,-59.4356425841503));
#68122=CARTESIAN_POINT('Ctrl Pts',(-26.3593572547097,20.7975412037247,-59.4414960324501));
#68123=CARTESIAN_POINT('Ctrl Pts',(-26.4405602344828,20.8804077475884,-59.4473561373916));
#68124=CARTESIAN_POINT('Ctrl Pts',(-26.5180365038056,20.9668124255809,-59.4532162423331));
#68125=CARTESIAN_POINT('Ctrl Pts',(-26.5914801684225,21.0563753371235,-59.4590763472746));
#68126=CARTESIAN_POINT('Ctrl Pts',(-26.6649732927511,21.1459985636818,-59.4649403986301));
#68127=CARTESIAN_POINT('Ctrl Pts',(-26.7344281577441,21.2387839286889,-59.4708044499856));
#68128=CARTESIAN_POINT('Ctrl Pts',(-26.7995818195121,21.3343219869053,-59.476668501341));
#68129=CARTESIAN_POINT('Ctrl Pts',(-26.8648315047715,21.4300008491479,-59.4825411951376));
#68130=CARTESIAN_POINT('Ctrl Pts',(-26.9257671183942,21.5284401512598,-59.4884138889341));
#68131=CARTESIAN_POINT('Ctrl Pts',(-26.9821712685195,21.6292052173816,-59.4942865827307));
#68132=CARTESIAN_POINT('Ctrl Pts',(-26.9976137812974,21.6567930068918,-59.495894428054));
#68133=CARTESIAN_POINT('Ctrl Pts',(-27.0127169058148,21.6845550124757,-59.4975022733773));
#68134=CARTESIAN_POINT('Ctrl Pts',(-27.0274768151446,21.7124820665429,-59.4991101187007));
#68135=CARTESIAN_POINT('Ctrl Pts',(-27.0845220828676,21.8204167591193,-59.5053242467739));
#68136=CARTESIAN_POINT('Ctrl Pts',(-27.1366100965118,21.9311458948516,-59.5115383748472));
#68137=CARTESIAN_POINT('Ctrl Pts',(-27.1834742626248,22.0442017842446,-59.5177525029205));
#68138=CARTESIAN_POINT('Ctrl Pts',(-27.2325471217173,22.1625859611095,-59.5242595008384));
#68139=CARTESIAN_POINT('Ctrl Pts',(-27.2758914982486,22.2835212836231,-59.5307664987563));
#68140=CARTESIAN_POINT('Ctrl Pts',(-27.3132539937852,22.4064391744103,-59.5372734966742));
#68141=CARTESIAN_POINT('Ctrl Pts',(-27.3487733347603,22.5232933195125,-59.5434594934726));
#68142=CARTESIAN_POINT('Ctrl Pts',(-27.3788866604174,22.6419387339928,-59.549645490271));
#68143=CARTESIAN_POINT('Ctrl Pts',(-27.4034243477068,22.7618643301806,-59.5558314870695));
#68144=CARTESIAN_POINT('Ctrl Pts',(-27.4279237226215,22.8816026783065,-59.5620078252467));
#68145=CARTESIAN_POINT('Ctrl Pts',(-27.4468647295695,23.00261689376,-59.5681841634239));
#68146=CARTESIAN_POINT('Ctrl Pts',(-27.4601275277268,23.1243810541338,-59.574360501601));
#68147=CARTESIAN_POINT('Ctrl Pts',(-27.4733643544789,23.2459067741507,-59.5805247451826));
#68148=CARTESIAN_POINT('Ctrl Pts',(-27.4809450984992,23.3681791729121,-59.5866889887642));
#68149=CARTESIAN_POINT('Ctrl Pts',(-27.482801082237,23.4906631230373,-59.5928532323458));
#68150=CARTESIAN_POINT('Ctrl Pts',(-27.4831004893595,23.5104222223859,-59.5938476475423));
#68151=CARTESIAN_POINT('Ctrl Pts',(-27.4832510230179,23.5301868073856,-59.5948420627388));
#68152=CARTESIAN_POINT('Ctrl Pts',(-27.4832525204106,23.5499546106029,-59.5958364779354));
#68153=CARTESIAN_POINT('',(-27.4832508599701,23.5538787940674,-60.8458364779651));
#68154=CARTESIAN_POINT('Ctrl Pts',(-27.4832525204106,23.5499546111917,-59.595836477965));
#68155=CARTESIAN_POINT('Ctrl Pts',(-27.4832616993984,23.6711310949174,-59.6019322355743));
#68156=CARTESIAN_POINT('Ctrl Pts',(-27.477666351959,23.7922129670324,-59.6080279931836));
#68157=CARTESIAN_POINT('Ctrl Pts',(-27.4665185564701,23.9126741414055,-59.6141237507928));
#68158=CARTESIAN_POINT('Ctrl Pts',(-27.4553574565759,24.0332790809115,-59.6202267834217));
#68159=CARTESIAN_POINT('Ctrl Pts',(-27.4386307271698,24.153261486616,-59.6263298160506));
#68160=CARTESIAN_POINT('Ctrl Pts',(-27.4164418763637,24.2721035905451,-59.6324328486795));
#68161=CARTESIAN_POINT('Ctrl Pts',(-27.3942034556774,24.391211187667,-59.6385495154798));
#68162=CARTESIAN_POINT('Ctrl Pts',(-27.366478591319,24.5091730359776,-59.6446661822801));
#68163=CARTESIAN_POINT('Ctrl Pts',(-27.333421517184,24.6254834032879,-59.6507828490804));
#68164=CARTESIAN_POINT('Ctrl Pts',(-27.3003247017988,24.7419335990474,-59.6569068693442));
#68165=CARTESIAN_POINT('Ctrl Pts',(-27.2618830036239,24.8567280117497,-59.6630308896079));
#68166=CARTESIAN_POINT('Ctrl Pts',(-27.2182993012072,24.9693796918406,-59.6691549098717));
#68167=CARTESIAN_POINT('Ctrl Pts',(-27.1746185298994,25.0822822678641,-59.6752925694507));
#68168=CARTESIAN_POINT('Ctrl Pts',(-27.1257730077416,25.19303224151,-59.6814302290296));
#68169=CARTESIAN_POINT('Ctrl Pts',(-27.0720127091686,25.3011649373717,-59.6875678886086));
#68170=CARTESIAN_POINT('Ctrl Pts',(-27.0415627875594,25.3624114743103,-59.6910442690976));
#68171=CARTESIAN_POINT('Ctrl Pts',(-27.0095369683429,25.4228188506372,-59.6945206495867));
#68172=CARTESIAN_POINT('Ctrl Pts',(-26.9759867937984,25.4823068180551,-59.6979970300757));
#68173=CARTESIAN_POINT('Ctrl Pts',(-26.9193138867624,25.582793807855,-59.7038693270444));
#68174=CARTESIAN_POINT('Ctrl Pts',(-26.8581209145749,25.6809534486651,-59.7097416240131));
#68175=CARTESIAN_POINT('Ctrl Pts',(-26.7926239578226,25.7763514816572,-59.7156139209819));
#68176=CARTESIAN_POINT('Ctrl Pts',(-26.7272118799245,25.8716258863749,-59.7214786079201));
#68177=CARTESIAN_POINT('Ctrl Pts',(-26.6575071411671,25.9641454626237,-59.7273432948583));
#68178=CARTESIAN_POINT('Ctrl Pts',(-26.5837715632439,26.0535006786476,-59.7332079817964));
#68179=CARTESIAN_POINT('Ctrl Pts',(-26.5101118177467,26.1427639984255,-59.7390666372713));
#68180=CARTESIAN_POINT('Ctrl Pts',(-26.4324297401534,26.2288691141159,-59.7449252927461));
#68181=CARTESIAN_POINT('Ctrl Pts',(-26.3510298926307,26.3114361863006,-59.7507839482209));
#68182=CARTESIAN_POINT('Ctrl Pts',(-26.2664504953678,26.3972284010489,-59.7568714479388));
#68183=CARTESIAN_POINT('Ctrl Pts',(-26.1778572258801,26.4792001645838,-59.7629589476567));
#68184=CARTESIAN_POINT('Ctrl Pts',(-26.0856374382027,26.556963754251,-59.7690464473746));
#68185=CARTESIAN_POINT('Ctrl Pts',(-25.9969872137074,26.6317173386517,-59.774898317458));
#68186=CARTESIAN_POINT('Ctrl Pts',(-25.9049863405209,26.7025821730215,-59.7807501875414));
#68187=CARTESIAN_POINT('Ctrl Pts',(-25.8100151660706,26.7692526615911,-59.7866020576248));
#68188=CARTESIAN_POINT('Ctrl Pts',(-25.7150584518453,26.8359129989724,-59.7924530367077));
#68189=CARTESIAN_POINT('Ctrl Pts',(-25.6171326738288,26.898380022899,-59.7983040157907));
#68190=CARTESIAN_POINT('Ctrl Pts',(-25.5166487461557,26.9563903632788,-59.8041549948736));
#68191=CARTESIAN_POINT('Ctrl Pts',(-25.4161557840106,27.0144059193463,-59.8100065000159));
#68192=CARTESIAN_POINT('Ctrl Pts',(-25.3131045730134,27.0679637886221,-59.8158580051582));
#68193=CARTESIAN_POINT('Ctrl Pts',(-25.2079316783369,27.1168459829844,-59.8217095103005));
#68194=CARTESIAN_POINT('Ctrl Pts',(-25.1027238580312,27.1657444100595,-59.8275629586003));
#68195=CARTESIAN_POINT('Ctrl Pts',(-24.9953933277361,27.2099639006548,-59.8334164069));
#68196=CARTESIAN_POINT('Ctrl Pts',(-24.8863970580109,27.2493344184323,-59.8392698551998));
#68197=CARTESIAN_POINT('Ctrl Pts',(-24.7772768358591,27.2887497090376,-59.8451299601413));
#68198=CARTESIAN_POINT('Ctrl Pts',(-24.6664874823241,27.3233048798586,-59.8509900650828));
#68199=CARTESIAN_POINT('Ctrl Pts',(-24.5545016683604,27.3528796066918,-59.8568501700244));
#68200=CARTESIAN_POINT('Ctrl Pts',(-24.4424404389601,27.3824742502526,-59.8627142213798));
#68201=CARTESIAN_POINT('Ctrl Pts',(-24.3291815477118,27.4070816837588,-59.8685782727352));
#68202=CARTESIAN_POINT('Ctrl Pts',(-24.2152066860982,27.4266329274424,-59.8744423240906));
#68203=CARTESIAN_POINT('Ctrl Pts',(-24.1010638482899,27.4462129857564,-59.8803150178872));
#68204=CARTESIAN_POINT('Ctrl Pts',(-23.9862033427299,27.4607219302523,-59.8861877116838));
#68205=CARTESIAN_POINT('Ctrl Pts',(-23.8711108763358,27.4701426988639,-59.8920604054803));
#68206=CARTESIAN_POINT('Ctrl Pts',(-23.8396004842983,27.4727219477196,-59.8936682508037));
#68207=CARTESIAN_POINT('Ctrl Pts',(-23.808072695895,27.4749201021011,-59.8952760961271));
#68208=CARTESIAN_POINT('Ctrl Pts',(-23.7765374399455,27.4767374915912,-59.8968839414504));
#68209=CARTESIAN_POINT('Ctrl Pts',(-23.6613619406432,27.4833751019625,-59.9027562384191));
#68210=CARTESIAN_POINT('Ctrl Pts',(-23.5457011922613,27.4849518748908,-59.9086285353878));
#68211=CARTESIAN_POINT('Ctrl Pts',(-23.4300373447555,27.4814148672928,-59.9145008323565));
#68212=CARTESIAN_POINT('Ctrl Pts',(-23.3145233884103,27.4778824433758,-59.9203655192947));
#68213=CARTESIAN_POINT('Ctrl Pts',(-23.1990067503038,27.4692494302816,-59.9262302062329));
#68214=CARTESIAN_POINT('Ctrl Pts',(-23.0839735020986,27.4555147337185,-59.9320948931711));
#68215=CARTESIAN_POINT('Ctrl Pts',(-22.9690585583877,27.4417941624309,-59.937953548646));
#68216=CARTESIAN_POINT('Ctrl Pts',(-22.8546264237481,27.4229823924681,-59.9438122041208));
#68217=CARTESIAN_POINT('Ctrl Pts',(-22.7411612922178,27.3991303377829,-59.9496708595956));
#68218=CARTESIAN_POINT('Ctrl Pts',(-22.6232641127112,27.3743466008332,-59.9557583593135));
#68219=CARTESIAN_POINT('Ctrl Pts',(-22.5064114748136,27.3441208099937,-59.9618458590314));
#68220=CARTESIAN_POINT('Ctrl Pts',(-22.3911389573759,27.308569272182,-59.9679333587493));
#68221=CARTESIAN_POINT('Ctrl Pts',(-22.2803283080962,27.2743938323168,-59.9737852288327));
#68222=CARTESIAN_POINT('Ctrl Pts',(-22.1709781618021,27.2352974012421,-59.9796370989161));
#68223=CARTESIAN_POINT('Ctrl Pts',(-22.0635512152505,27.1914347841617,-59.9854889689995));
#68224=CARTESIAN_POINT('Ctrl Pts',(-21.9561406254283,27.1475788455636,-59.9913399480825));
#68225=CARTESIAN_POINT('Ctrl Pts',(-21.8506530357254,27.0989583200929,-59.9971909271655));
#68226=CARTESIAN_POINT('Ctrl Pts',(-21.7475321403287,27.0457765540054,-60.0030419062484));
#68227=CARTESIAN_POINT('Ctrl Pts',(-21.6444019733711,26.9925900063655,-60.0088934113907));
#68228=CARTESIAN_POINT('Ctrl Pts',(-21.5436392911471,26.9348415923575,-60.014744916533));
#68229=CARTESIAN_POINT('Ctrl Pts',(-21.4456634727043,26.8727807697653,-60.0205964216753));
#68230=CARTESIAN_POINT('Ctrl Pts',(-21.3476551186254,26.8106993381252,-60.0264498699751));
#68231=CARTESIAN_POINT('Ctrl Pts',(-21.2524358175739,26.7443028714342,-60.0323033182748));
#68232=CARTESIAN_POINT('Ctrl Pts',(-21.1603956359335,26.6738839148418,-60.0381567665746));
#68233=CARTESIAN_POINT('Ctrl Pts',(-21.0682507846201,26.6033848766044,-60.0440168715161));
#68234=CARTESIAN_POINT('Ctrl Pts',(-20.9792925973534,26.5288544693506,-60.0498769764577));
#68235=CARTESIAN_POINT('Ctrl Pts',(-20.8938778035935,26.4506253187524,-60.0557370813992));
#68236=CARTESIAN_POINT('Ctrl Pts',(-20.8084054883159,26.3723434857175,-60.0616011327547));
#68237=CARTESIAN_POINT('Ctrl Pts',(-20.7264816095325,26.2903582412178,-60.0674651841101));
#68238=CARTESIAN_POINT('Ctrl Pts',(-20.6484245757464,26.2050375538908,-60.0733292354656));
#68239=CARTESIAN_POINT('Ctrl Pts',(-20.570252501474,26.1195911209024,-60.0792019292621));
#68240=CARTESIAN_POINT('Ctrl Pts',(-20.4959589104974,26.0307997499948,-60.0850746230587));
#68241=CARTESIAN_POINT('Ctrl Pts',(-20.4258207025986,25.939062851777,-60.0909473168553));
#68242=CARTESIAN_POINT('Ctrl Pts',(-20.4066180345442,25.9139468236151,-60.0925551621787));
#68243=CARTESIAN_POINT('Ctrl Pts',(-20.3877265841919,25.8886101618797,-60.094163007502));
#68244=CARTESIAN_POINT('Ctrl Pts',(-20.369151441206,25.863061398007,-60.0957708528254));
#68245=CARTESIAN_POINT('Ctrl Pts',(-20.3013098682243,25.7697502277949,-60.1016431497941));
#68246=CARTESIAN_POINT('Ctrl Pts',(-20.2374637649966,25.6732952122084,-60.1075154467628));
#68247=CARTESIAN_POINT('Ctrl Pts',(-20.1779182959182,25.574073374114,-60.1133877437315));
#68248=CARTESIAN_POINT('Ctrl Pts',(-20.1184499930387,25.4749801196419,-60.1192524306697));
#68249=CARTESIAN_POINT('Ctrl Pts',(-20.0632714518072,25.3731275242794,-60.1251171176079));
#68250=CARTESIAN_POINT('Ctrl Pts',(-20.0126463352094,25.2689239367605,-60.1309818045461));
#68251=CARTESIAN_POINT('Ctrl Pts',(-19.9620732833747,25.1648275161077,-60.136840460021));
#68252=CARTESIAN_POINT('Ctrl Pts',(-19.9160445211776,25.0583852821121,-60.1426991154958));
#68253=CARTESIAN_POINT('Ctrl Pts',(-19.8747789412593,24.9500321164916,-60.1485577709707));
#68254=CARTESIAN_POINT('Ctrl Pts',(-19.8319014914433,24.8374465807862,-60.1546452706886));
#68255=CARTESIAN_POINT('Ctrl Pts',(-19.7941671518938,24.7227981746295,-60.1607327704065));
#68256=CARTESIAN_POINT('Ctrl Pts',(-19.7617675747234,24.6066003583146,-60.1668202701244));
#68257=CARTESIAN_POINT('Ctrl Pts',(-19.7306220921535,24.4949002258202,-60.1726721402078));
#68258=CARTESIAN_POINT('Ctrl Pts',(-19.7044061858325,24.381768834628,-60.1785240102912));
#68259=CARTESIAN_POINT('Ctrl Pts',(-19.6832397227574,24.267679138058,-60.1843758803746));
#68260=CARTESIAN_POINT('Ctrl Pts',(-19.6620764824688,24.1536068126817,-60.1902268594575));
#68261=CARTESIAN_POINT('Ctrl Pts',(-19.6459612321438,24.0385768783805,-60.1960778385405));
#68262=CARTESIAN_POINT('Ctrl Pts',(-19.634962728683,23.9230725397902,-60.2019288176235));
#68263=CARTESIAN_POINT('Ctrl Pts',(-19.6239632363509,23.8075578162481,-60.2077803227658));
#68264=CARTESIAN_POINT('Ctrl Pts',(-19.6180814445977,23.6915690151714,-60.213631827908));
#68265=CARTESIAN_POINT('Ctrl Pts',(-19.6173341725582,23.5755938096969,-60.2194833330503));
#68266=CARTESIAN_POINT('Ctrl Pts',(-19.6165866523659,23.4595800913813,-60.2253367813501));
#68267=CARTESIAN_POINT('Ctrl Pts',(-19.6209770449584,23.3435803908008,-60.2311902296499));
#68268=CARTESIAN_POINT('Ctrl Pts',(-19.6304700746094,23.2280810104037,-60.2370436779496));
#68269=CARTESIAN_POINT('Ctrl Pts',(-19.6399738998965,23.112450282131,-60.2429037828912));
#68270=CARTESIAN_POINT('Ctrl Pts',(-19.6545919105859,22.9973214219321,-60.2487638878327));
#68271=CARTESIAN_POINT('Ctrl Pts',(-19.6742370905149,22.8831743505639,-60.2546239927742));
#68272=CARTESIAN_POINT('Ctrl Pts',(-19.6938955002431,22.7689504082874,-60.2604880441297));
#68273=CARTESIAN_POINT('Ctrl Pts',(-19.7185877325273,22.6557099742744,-60.2663520954851));
#68274=CARTESIAN_POINT('Ctrl Pts',(-19.7481763224732,22.543919833589,-60.2722161468406));
#68275=CARTESIAN_POINT('Ctrl Pts',(-19.7778085200942,22.4319649365515,-60.2780888406371));
#68276=CARTESIAN_POINT('Ctrl Pts',(-19.8123513547508,22.3214649918376,-60.2839615344337));
#68277=CARTESIAN_POINT('Ctrl Pts',(-19.8516184716668,22.2128688582461,-60.2898342282303));
#68278=CARTESIAN_POINT('Ctrl Pts',(-19.8623691514197,22.1831370534604,-60.2914420735536));
#68279=CARTESIAN_POINT('Ctrl Pts',(-19.8734736802612,22.1535478195493,-60.2930499188769));
#68280=CARTESIAN_POINT('Ctrl Pts',(-19.8849276317304,22.1241100501358,-60.2946577642002));
#68281=CARTESIAN_POINT('Ctrl Pts',(-19.9267606386227,22.0165951532827,-60.300530061169));
#68282=CARTESIAN_POINT('Ctrl Pts',(-19.9733983361586,21.9107423304688,-60.3064023581377));
#68283=CARTESIAN_POINT('Ctrl Pts',(-20.0246884829674,21.8070121184622,-60.3122746551064));
#68284=CARTESIAN_POINT('Ctrl Pts',(-20.0759121618193,21.7034163325723,-60.3181393420446));
#68285=CARTESIAN_POINT('Ctrl Pts',(-20.1317761184858,21.6019380544036,-60.3240040289828));
#68286=CARTESIAN_POINT('Ctrl Pts',(-20.1920793233468,21.5030198378516,-60.329868715921));
#68287=CARTESIAN_POINT('Ctrl Pts',(-20.2523205101368,21.4042033524929,-60.3357273713958));
#68288=CARTESIAN_POINT('Ctrl Pts',(-20.3169916502459,21.3079420426936,-60.3415860268706));
#68289=CARTESIAN_POINT('Ctrl Pts',(-20.3858451911404,21.2146551385099,-60.3474446823455));
#68290=CARTESIAN_POINT('Ctrl Pts',(-20.4573882119876,21.1177243656829,-60.3535321820634));
#68291=CARTESIAN_POINT('Ctrl Pts',(-20.5334468294877,21.0240055088851,-60.3596196817813));
#68292=CARTESIAN_POINT('Ctrl Pts',(-20.613692656973,20.9339373553102,-60.3657071814992));
#68293=CARTESIAN_POINT('Ctrl Pts',(-20.6908323988932,20.8473554813395,-60.3715590515826));
#68294=CARTESIAN_POINT('Ctrl Pts',(-20.771840927712,20.7641472865752,-60.3774109216659));
#68295=CARTESIAN_POINT('Ctrl Pts',(-20.8563851330593,20.6846692684523,-60.3832627917494));
#68296=CARTESIAN_POINT('Ctrl Pts',(-20.9409164657827,20.6052033515803,-60.3891137708323));
#68297=CARTESIAN_POINT('Ctrl Pts',(-21.0289821035365,20.5294667651412,-60.3949647499153));
#68298=CARTESIAN_POINT('Ctrl Pts',(-21.1202126841728,20.4577785480594,-60.4008157289983));
#68299=CARTESIAN_POINT('Ctrl Pts',(-21.2114514673163,20.3860838855169,-60.4066672341406));
#68300=CARTESIAN_POINT('Ctrl Pts',(-21.3058554339614,20.3184385713325,-60.4125187392829));
#68301=CARTESIAN_POINT('Ctrl Pts',(-21.4030233879713,20.2551203637308,-60.4183702444252));
#68302=CARTESIAN_POINT('Ctrl Pts',(-21.5002236093435,20.1917811295308,-60.424223692725));
#68303=CARTESIAN_POINT('Ctrl Pts',(-21.6001892970318,20.1327720847418,-60.4300771410247));
#68304=CARTESIAN_POINT('Ctrl Pts',(-21.7024922486014,20.0783264183927,-60.4359305893245));
#68305=CARTESIAN_POINT('Ctrl Pts',(-21.8049115408417,20.0238188354983,-60.4417906942661));
#68306=CARTESIAN_POINT('Ctrl Pts',(-21.9096730370667,19.9738851835595,-60.4476507992076));
#68307=CARTESIAN_POINT('Ctrl Pts',(-22.0163259359665,19.9287116719331,-60.4535109041491));
#68308=CARTESIAN_POINT('Ctrl Pts',(-22.1230506589182,19.8835077387741,-60.4593749555046));
#68309=CARTESIAN_POINT('Ctrl Pts',(-22.2316689343565,19.8430704729006,-60.46523900686));
#68310=CARTESIAN_POINT('Ctrl Pts',(-22.3417137425724,19.8075365399059,-60.4711030582154));
#68311=CARTESIAN_POINT('Ctrl Pts',(-22.4519207348692,19.771950236987,-60.476975752012));
#68312=CARTESIAN_POINT('Ctrl Pts',(-22.5635580588591,19.7412817988087,-60.4828484458086));
#68313=CARTESIAN_POINT('Ctrl Pts',(-22.6761473494468,19.7156170691804,-60.4887211396052));
#68314=CARTESIAN_POINT('Ctrl Pts',(-22.706972413821,19.7085904955267,-60.4903289849285));
#68315=CARTESIAN_POINT('Ctrl Pts',(-22.7378688013595,19.7019386866499,-60.4919368302518));
#68316=CARTESIAN_POINT('Ctrl Pts',(-22.7688266370183,19.6956627258744,-60.4935446755752));
#68317=CARTESIAN_POINT('Ctrl Pts',(-22.8818932373045,19.6727411768283,-60.4994169725439));
#68318=CARTESIAN_POINT('Ctrl Pts',(-22.9961586457932,19.6547603161135,-60.5052892695126));
#68319=CARTESIAN_POINT('Ctrl Pts',(-23.1111531122592,19.6418410001571,-60.5111615664813));
#68320=CARTESIAN_POINT('Ctrl Pts',(-23.2259985550296,19.6289384266082,-60.5170262534195));
#68321=CARTESIAN_POINT('Ctrl Pts',(-23.3415707699003,19.6210843993312,-60.5228909403577));
#68322=CARTESIAN_POINT('Ctrl Pts',(-23.4573887638217,19.6183490078757,-60.5287556272959));
#68323=CARTESIAN_POINT('Ctrl Pts',(-23.5730876461862,19.615616429599,-60.5346142827707));
#68324=CARTESIAN_POINT('Ctrl Pts',(-23.6890313940491,19.6179920260881,-60.5404729382455));
#68325=CARTESIAN_POINT('Ctrl Pts',(-23.8047334894914,19.6254941388605,-60.5463315937203));
#68326=CARTESIAN_POINT('Ctrl Pts',(-23.9249550106912,19.6332892907655,-60.5524190934382));
#68327=CARTESIAN_POINT('Ctrl Pts',(-24.0449151644658,19.6466196666752,-60.5585065931562));
#68328=CARTESIAN_POINT('Ctrl Pts',(-24.164067284872,19.6654461724555,-60.5645940928741));
#68329=CARTESIAN_POINT('Ctrl Pts',(-24.2786073688293,19.6835439582553,-60.5704459629575));
#68330=CARTESIAN_POINT('Ctrl Pts',(-24.3924003631941,19.7067202360158,-60.5762978330409));
#68331=CARTESIAN_POINT('Ctrl Pts',(-24.5049662804162,19.7348874563703,-60.5821497031243));
#68332=CARTESIAN_POINT('Ctrl Pts',(-24.6175150584538,19.7630503880094,-60.5880006822072));
#68333=CARTESIAN_POINT('Ctrl Pts',(-24.7288367299253,19.7962026509665,-60.5938516612902));
#68334=CARTESIAN_POINT('Ctrl Pts',(-24.8384632261315,19.834205948733,-60.5997026403732));
#68335=CARTESIAN_POINT('Ctrl Pts',(-24.9480995788145,19.8722126633617,-60.6055541455154));
#68336=CARTESIAN_POINT('Ctrl Pts',(-25.0560400626472,19.915071144428,-60.6114056506577));
#68337=CARTESIAN_POINT('Ctrl Pts',(-25.161834131455,19.9625939989862,-60.6172571558));
#68338=CARTESIAN_POINT('Ctrl Pts',(-25.2676633321701,20.0101326348499,-60.6231106040998));
#68339=CARTESIAN_POINT('Ctrl Pts',(-25.3713443236609,20.0623385548715,-60.6289640523995));
#68340=CARTESIAN_POINT('Ctrl Pts',(-25.4724494585164,20.1189775537137,-60.6348175006993));
#68341=CARTESIAN_POINT('Ctrl Pts',(-25.5736695718648,20.1756809633965,-60.6406776056408));
#68342=CARTESIAN_POINT('Ctrl Pts',(-25.6723076209045,20.2368273121739,-60.6465377105823));
#68343=CARTESIAN_POINT('Ctrl Pts',(-25.7679632673607,20.3021379873917,-60.6523978155238));
#68344=CARTESIAN_POINT('Ctrl Pts',(-25.8636833319078,20.3674926452615,-60.6582618668793));
#68345=CARTESIAN_POINT('Ctrl Pts',(-25.9564166646838,20.43701696635,-60.6641259182347));
#68346=CARTESIAN_POINT('Ctrl Pts',(-26.0457958426808,20.5103919126871,-60.6699899695902));
#68347=CARTESIAN_POINT('Ctrl Pts',(-26.1353067477447,20.5838749990484,-60.6758626633867));
#68348=CARTESIAN_POINT('Ctrl Pts',(-26.2214533256054,20.6612197618368,-60.6817353571833));
#68349=CARTESIAN_POINT('Ctrl Pts',(-26.3039047778123,20.7420701466899,-60.6876080509799));
#68350=CARTESIAN_POINT('Ctrl Pts',(-26.3264786061831,20.7642056296018,-60.6892158963033));
#68351=CARTESIAN_POINT('Ctrl Pts',(-26.348775691853,20.7866036941377,-60.6908237416267));
#68352=CARTESIAN_POINT('Ctrl Pts',(-26.3707897855231,20.8092566178404,-60.6924315869501));
#68353=CARTESIAN_POINT('Ctrl Pts',(-26.4501437958303,20.890913413161,-60.6982273728805));
#68354=CARTESIAN_POINT('Ctrl Pts',(-26.52609883446,20.9761737589497,-60.704023158811));
#68355=CARTESIAN_POINT('Ctrl Pts',(-26.5983031636978,21.0647191191764,-60.7098189447415));
#68356=CARTESIAN_POINT('Ctrl Pts',(-26.6703919570342,21.1531227958209,-60.7156054566941));
#68357=CARTESIAN_POINT('Ctrl Pts',(-26.7387417158845,21.2448007023129,-60.7213919686466));
#68358=CARTESIAN_POINT('Ctrl Pts',(-26.8030371795997,21.339397259554,-60.7271784805992));
#68359=CARTESIAN_POINT('Ctrl Pts',(-26.8672738292152,21.4339072848529,-60.7329596993558));
#68360=CARTESIAN_POINT('Ctrl Pts',(-26.9274633142762,21.5313303076372,-60.7387409181124));
#68361=CARTESIAN_POINT('Ctrl Pts',(-26.9833305140211,21.6312776576371,-60.744522136869));
#68362=CARTESIAN_POINT('Ctrl Pts',(-27.0391609827443,21.731159295228,-60.7502995546463));
#68363=CARTESIAN_POINT('Ctrl Pts',(-27.0906746068446,21.8335615920512,-60.7560769724236));
#68364=CARTESIAN_POINT('Ctrl Pts',(-27.1376399857211,21.9380675997803,-60.7618543902008));
#68365=CARTESIAN_POINT('Ctrl Pts',(-27.1845865652934,22.0425317758393,-60.767629495393));
#68366=CARTESIAN_POINT('Ctrl Pts',(-27.2269883454295,22.1490976013021,-60.7734046005852));
#68367=CARTESIAN_POINT('Ctrl Pts',(-27.2646606326085,22.2573250550497,-60.7791797057774));
#68368=CARTESIAN_POINT('Ctrl Pts',(-27.3023402449164,22.3655735529152,-60.7849559339008));
#68369=CARTESIAN_POINT('Ctrl Pts',(-27.3352883768845,22.4754839263879,-60.7907321620243));
#68370=CARTESIAN_POINT('Ctrl Pts',(-27.3633692635136,22.5865981385018,-60.7965083901478));
#68371=CARTESIAN_POINT('Ctrl Pts',(-27.3914519574842,22.6977195021466,-60.8022849900408));
#68372=CARTESIAN_POINT('Ctrl Pts',(-27.4146666867965,22.8100444440291,-60.8080615899338));
#68373=CARTESIAN_POINT('Ctrl Pts',(-27.4329285044896,22.9231031951903,-60.8138381898267));
#68374=CARTESIAN_POINT('Ctrl Pts',(-27.4512067275791,23.0362635120149,-60.8196199790942));
#68375=CARTESIAN_POINT('Ctrl Pts',(-27.4645230919947,23.1501585331982,-60.8254017683616));
#68376=CARTESIAN_POINT('Ctrl Pts',(-27.4728443960287,23.264311863273,-60.8311835576291));
#68377=CARTESIAN_POINT('Ctrl Pts',(-27.4798740195275,23.3607456587816,-60.8360678644078));
#68378=CARTESIAN_POINT('Ctrl Pts',(-27.4833398479381,23.457363568906,-60.8409521711864));
#68379=CARTESIAN_POINT('Ctrl Pts',(-27.4832508599701,23.5538787940674,-60.8458364779651));
#68380=CARTESIAN_POINT('',(-27.4892001437474,23.5489065548291,-62.095836477965));
#68381=CARTESIAN_POINT('Ctrl Pts',(-27.4834099576864,23.553878940757,-60.8458364779651));
#68382=CARTESIAN_POINT('Ctrl Pts',(-27.4861874509236,23.8534728895291,-60.8609971514184));
#68383=CARTESIAN_POINT('Ctrl Pts',(-27.3178909131174,25.4600629410759,-60.9424534619966));
#68384=CARTESIAN_POINT('Ctrl Pts',(-25.1124238142668,27.9320754076231,-61.0902054096999));
#68385=CARTESIAN_POINT('Ctrl Pts',(-20.7081712302401,27.2330944653146,-61.2890923210748));
#68386=CARTESIAN_POINT('Ctrl Pts',(-18.9155503934932,23.1498940395121,-61.4879792324495));
#68387=CARTESIAN_POINT('Ctrl Pts',(-21.3818278638133,19.4345891232223,-61.6868661438245));
#68388=CARTESIAN_POINT('Ctrl Pts',(-25.8407037518232,19.5012299286061,-61.8857530551994));
#68389=CARTESIAN_POINT('Ctrl Pts',(-27.4543102486202,22.0972001521906,-62.0220764999129));
#68390=CARTESIAN_POINT('Ctrl Pts',(-27.4895254076886,23.4754357787105,-62.0921043075015));
#68391=CARTESIAN_POINT('Ctrl Pts',(-27.4892001437474,23.5489065548291,-62.095836477965));
#68392=CARTESIAN_POINT('',(-27.4820679227229,23.5472708336066,-63.3458360315144));
#68393=CARTESIAN_POINT('Ctrl Pts',(-27.4892001437474,23.5489065548291,-62.095836477965));
#68394=CARTESIAN_POINT('Ctrl Pts',(-27.4837476490292,24.7805186950384,-62.1583999446264));
#68395=CARTESIAN_POINT('Ctrl Pts',(-26.1980019261252,27.3270249273693,-62.2872590484128));
#68396=CARTESIAN_POINT('Ctrl Pts',(-21.8578298400895,27.8834333801068,-62.4824137893241));
#68397=CARTESIAN_POINT('Ctrl Pts',(-18.9898485690431,24.4686568705032,-62.681300700699));
#68398=CARTESIAN_POINT('Ctrl Pts',(-20.3124918811797,20.209944641381,-62.8801876120739));
#68399=CARTESIAN_POINT('Ctrl Pts',(-24.6103627143063,19.0206921520514,-63.0790745234488));
#68400=CARTESIAN_POINT('Ctrl Pts',(-27.2042676807139,21.3409108015181,-63.2342903151889));
#68401=CARTESIAN_POINT('Ctrl Pts',(-27.4824290166878,23.0989765952615,-63.3232104698041));
#68402=CARTESIAN_POINT('Ctrl Pts',(-27.4792998261461,23.5472522368032,-63.3458349872944));
#68403=CARTESIAN_POINT('',(-27.4816133133806,23.5527675431246,-64.5958369912555));
#68404=CARTESIAN_POINT('Ctrl Pts',(-27.4832514074667,23.5472787845695,-63.3458364779651));
#68405=CARTESIAN_POINT('Ctrl Pts',(-27.48333921894,23.6634159041666,-63.3516920745539));
#68406=CARTESIAN_POINT('Ctrl Pts',(-27.4782786202806,23.7796066600921,-63.3575476711427));
#68407=CARTESIAN_POINT('Ctrl Pts',(-27.4680820905473,23.8953620038579,-63.3634032677314));
#68408=CARTESIAN_POINT('Ctrl Pts',(-27.4578867609682,24.011103722962,-63.3692581751035));
#68409=CARTESIAN_POINT('Ctrl Pts',(-27.4425567381748,24.1264097214561,-63.3751130824755));
#68410=CARTESIAN_POINT('Ctrl Pts',(-27.4221564839496,24.2407949159899,-63.3809679898475));
#68411=CARTESIAN_POINT('Ctrl Pts',(-27.401753732463,24.3551941127874,-63.3868236139378));
#68412=CARTESIAN_POINT('Ctrl Pts',(-27.3762795874776,24.4686718758199,-63.3926792380281));
#68413=CARTESIAN_POINT('Ctrl Pts',(-27.3458497277285,24.5807528594265,-63.3985348621183));
#68414=CARTESIAN_POINT('Ctrl Pts',(-27.3154088362872,24.6928744755873,-63.4043926090394));
#68415=CARTESIAN_POINT('Ctrl Pts',(-27.2800087648194,24.8035979078446,-63.4102503559605));
#68416=CARTESIAN_POINT('Ctrl Pts',(-27.239814986766,24.9124631945965,-63.4161081028815));
#68417=CARTESIAN_POINT('Ctrl Pts',(-27.1995721439576,25.0214613737729,-63.4219730003849));
#68418=CARTESIAN_POINT('Ctrl Pts',(-27.1545240553449,25.128596492421,-63.4278378978882));
#68419=CARTESIAN_POINT('Ctrl Pts',(-27.1048843389936,25.2334286111748,-63.4337027953915));
#68420=CARTESIAN_POINT('Ctrl Pts',(-27.0552101520406,25.3383335270047,-63.4395717655722));
#68421=CARTESIAN_POINT('Ctrl Pts',(-27.0009381802215,25.4409318949764,-63.4454407357528));
#68422=CARTESIAN_POINT('Ctrl Pts',(-26.9423270985381,25.5408100247023,-63.4513097059334));
#68423=CARTESIAN_POINT('Ctrl Pts',(-26.8836219472568,25.6408484568017,-63.4571880956922));
#68424=CARTESIAN_POINT('Ctrl Pts',(-26.8205640056903,25.738157589445,-63.4630664854511));
#68425=CARTESIAN_POINT('Ctrl Pts',(-26.7534543272939,25.8323540317741,-63.4689448752099));
#68426=CARTESIAN_POINT('Ctrl Pts',(-26.7233780979169,25.874569608926,-63.4715793655394));
#68427=CARTESIAN_POINT('Ctrl Pts',(-26.6924885943787,25.9161604565012,-63.4742138558689));
#68428=CARTESIAN_POINT('Ctrl Pts',(-26.660815366584,25.9570944147855,-63.4768483461985));
#68429=CARTESIAN_POINT('Ctrl Pts',(-26.5902155251335,26.0483364878555,-63.4827206431672));
#68430=CARTESIAN_POINT('Ctrl Pts',(-26.5154794034389,26.1366224269578,-63.4885929401359));
#68431=CARTESIAN_POINT('Ctrl Pts',(-26.4368835706086,26.2215537586576,-63.4944652371046));
#68432=CARTESIAN_POINT('Ctrl Pts',(-26.3583895917357,26.3063750260966,-63.5003299240428));
#68433=CARTESIAN_POINT('Ctrl Pts',(-26.276046126848,26.3878500307594,-63.506194610981));
#68434=CARTESIAN_POINT('Ctrl Pts',(-26.1901714325743,26.4656113769782,-63.5120592979192));
#68435=CARTESIAN_POINT('Ctrl Pts',(-26.1043850550479,26.5432927505205,-63.517917953394));
#68436=CARTESIAN_POINT('Ctrl Pts',(-26.0150749762511,26.6172677865298,-63.5237766088688));
#68437=CARTESIAN_POINT('Ctrl Pts',(-25.9225974536442,26.6872046466137,-63.5296352643436));
#68438=CARTESIAN_POINT('Ctrl Pts',(-25.8265076775513,26.7598733020519,-63.5357227640615));
#68439=CARTESIAN_POINT('Ctrl Pts',(-25.7269982757149,26.8281815472473,-63.5418102637794));
#68440=CARTESIAN_POINT('Ctrl Pts',(-25.624508567612,26.8918017079684,-63.5478977634973));
#68441=CARTESIAN_POINT('Ctrl Pts',(-25.525985941822,26.9529593149461,-63.5537496335807));
#68442=CARTESIAN_POINT('Ctrl Pts',(-25.4247098219172,27.0097847753873,-63.5596015036641));
#68443=CARTESIAN_POINT('Ctrl Pts',(-25.3211007257736,27.0620306672725,-63.5654533737475));
#68444=CARTESIAN_POINT('Ctrl Pts',(-25.2175074050572,27.1142686042455,-63.5713043528305));
#68445=CARTESIAN_POINT('Ctrl Pts',(-25.1115821833953,27.161928173004,-63.5771553319135));
#68446=CARTESIAN_POINT('Ctrl Pts',(-25.0037697222696,27.2048081512876,-63.5830063109964));
#68447=CARTESIAN_POINT('Ctrl Pts',(-24.895947567766,27.247691984894,-63.5888578161387));
#68448=CARTESIAN_POINT('Ctrl Pts',(-24.786238220628,27.2857952209766,-63.594709321281));
#68449=CARTESIAN_POINT('Ctrl Pts',(-24.6751051657447,27.3189652498076,-63.6005608264233));
#68450=CARTESIAN_POINT('Ctrl Pts',(-24.5639352059935,27.352146293683,-63.6064142747231));
#68451=CARTESIAN_POINT('Ctrl Pts',(-24.4513409943046,27.3803907546614,-63.6122677230228));
#68452=CARTESIAN_POINT('Ctrl Pts',(-24.3377992770121,27.4035964203108,-63.6181211713226));
#68453=CARTESIAN_POINT('Ctrl Pts',(-24.2241284381315,27.4268284758412,-63.6239812762641));
#68454=CARTESIAN_POINT('Ctrl Pts',(-24.1095083482015,27.4450102159024,-63.6298413812057));
#68455=CARTESIAN_POINT('Ctrl Pts',(-23.9944241050035,27.4580908872898,-63.6357014861472));
#68456=CARTESIAN_POINT('Ctrl Pts',(-23.8792623597704,27.4711803676906,-63.6415655375027));
#68457=CARTESIAN_POINT('Ctrl Pts',(-23.7636362502579,27.4791619107537,-63.6474295888582));
#68458=CARTESIAN_POINT('Ctrl Pts',(-23.6480323800569,27.4820368723281,-63.6532936402136));
#68459=CARTESIAN_POINT('Ctrl Pts',(-23.5322581328281,27.484916071022,-63.6591663340102));
#68460=CARTESIAN_POINT('Ctrl Pts',(-23.4165066020795,27.4826736755969,-63.6650390278068));
#68461=CARTESIAN_POINT('Ctrl Pts',(-23.301260861813,27.4753629948952,-63.6709117216034));
#68462=CARTESIAN_POINT('Ctrl Pts',(-23.2697085059534,27.4733614528118,-63.6725195669267));
#68463=CARTESIAN_POINT('Ctrl Pts',(-23.2381940101071,27.4709803027052,-63.6741274122501));
#68464=CARTESIAN_POINT('Ctrl Pts',(-23.206727151238,27.4682213055594,-63.6757352575734));
#68465=CARTESIAN_POINT('Ctrl Pts',(-23.0918014570385,27.4581446829259,-63.6816075545421));
#68466=CARTESIAN_POINT('Ctrl Pts',(-22.9771269731236,27.4429902225945,-63.6874798515108));
#68467=CARTESIAN_POINT('Ctrl Pts',(-22.8631884392071,27.4227752150125,-63.6933521484795));
#68468=CARTESIAN_POINT('Ctrl Pts',(-22.7493975605817,27.4025864044749,-63.6992168354177));
#68469=CARTESIAN_POINT('Ctrl Pts',(-22.636341138592,27.3773501598767,-63.7050815223559));
#68470=CARTESIAN_POINT('Ctrl Pts',(-22.5245003005774,27.3471356429262,-63.7109462092941));
#68471=CARTESIAN_POINT('Ctrl Pts',(-22.4127744838634,27.3169521997149,-63.716804864769));
#68472=CARTESIAN_POINT('Ctrl Pts',(-22.3022621611847,27.2818007749441,-63.7226635202438));
#68473=CARTESIAN_POINT('Ctrl Pts',(-22.1934350860089,27.2418017212736,-63.7285221757186));
#68474=CARTESIAN_POINT('Ctrl Pts',(-22.0803571294231,27.2002402693359,-63.7346096754365));
#68475=CARTESIAN_POINT('Ctrl Pts',(-21.969099206452,27.1534448422978,-63.7406971751544));
#68476=CARTESIAN_POINT('Ctrl Pts',(-21.8601744657258,27.1016079251929,-63.7467846748723));
#68477=CARTESIAN_POINT('Ctrl Pts',(-21.755465888948,27.0517774663053,-63.7526365449557));
#68478=CARTESIAN_POINT('Ctrl Pts',(-21.6529136394392,26.9972887377645,-63.7584884150391));
#68479=CARTESIAN_POINT('Ctrl Pts',(-21.5529531852349,26.9383617862244,-63.7643402851225));
#68480=CARTESIAN_POINT('Ctrl Pts',(-21.4530079509187,26.8794438068486,-63.7701912642055));
#68481=CARTESIAN_POINT('Ctrl Pts',(-21.3556540832809,26.8160891579714,-63.7760422432885));
#68482=CARTESIAN_POINT('Ctrl Pts',(-21.2613012323669,26.7485631715958,-63.7818932223714));
#68483=CARTESIAN_POINT('Ctrl Pts',(-21.1669398982235,26.6810311139842,-63.7877447275137));
#68484=CARTESIAN_POINT('Ctrl Pts',(-21.0755804533642,26.6093272139199,-63.793596232656));
#68485=CARTESIAN_POINT('Ctrl Pts',(-20.9876018241446,26.5337589169891,-63.7994477377983));
#68486=CARTESIAN_POINT('Ctrl Pts',(-20.8995939791375,26.458165525472,-63.8053011860981));
#68487=CARTESIAN_POINT('Ctrl Pts',(-20.8149694955982,26.3787054545708,-63.8111546343979));
#68488=CARTESIAN_POINT('Ctrl Pts',(-20.734072068165,26.2957245488229,-63.8170080826977));
#68489=CARTESIAN_POINT('Ctrl Pts',(-20.6530826427903,26.2126492757661,-63.8228681876392));
#68490=CARTESIAN_POINT('Ctrl Pts',(-20.5758290221214,26.1260454722655,-63.8287282925807));
#68491=CARTESIAN_POINT('Ctrl Pts',(-20.5026161215967,26.036293824965,-63.8345883975223));
#68492=CARTESIAN_POINT('Ctrl Pts',(-20.4293539167658,25.9464817355477,-63.8404524488777));
#68493=CARTESIAN_POINT('Ctrl Pts',(-20.3601380967407,25.853517911999,-63.8463165002331));
#68494=CARTESIAN_POINT('Ctrl Pts',(-20.2952305506919,25.7578124749782,-63.8521805515886));
#68495=CARTESIAN_POINT('Ctrl Pts',(-20.230227343877,25.6619659872478,-63.8580532453851));
#68496=CARTESIAN_POINT('Ctrl Pts',(-20.1695452993464,25.5633701725322,-63.8639259391817));
#68497=CARTESIAN_POINT('Ctrl Pts',(-20.1134006894535,25.4624602647835,-63.8697986329783));
#68498=CARTESIAN_POINT('Ctrl Pts',(-20.0980292344491,25.434832820058,-63.8714064783016));
#68499=CARTESIAN_POINT('Ctrl Pts',(-20.0829976149859,25.4070320333676,-63.873014323625));
#68500=CARTESIAN_POINT('Ctrl Pts',(-20.0683096343822,25.3790670821226,-63.8746221689483));
#68501=CARTESIAN_POINT('Ctrl Pts',(-20.014665056311,25.2769313256291,-63.880494465917));
#68502=CARTESIAN_POINT('Ctrl Pts',(-19.9654283381006,25.1722621300223,-63.8863667628857));
#68503=CARTESIAN_POINT('Ctrl Pts',(-19.9208469553725,25.0654766611764,-63.8922390598544));
#68504=CARTESIAN_POINT('Ctrl Pts',(-19.8763233465758,24.9588295778171,-63.8981037467927));
#68505=CARTESIAN_POINT('Ctrl Pts',(-19.8364432336887,24.8500720530627,-63.9039684337309));
#68506=CARTESIAN_POINT('Ctrl Pts',(-19.8014084995292,24.7396462522514,-63.9098331206691));
#68507=CARTESIAN_POINT('Ctrl Pts',(-19.7664097964007,24.6293340174638,-63.9156917761439));
#68508=CARTESIAN_POINT('Ctrl Pts',(-19.7362466844819,24.5173573109278,-63.9215504316187));
#68509=CARTESIAN_POINT('Ctrl Pts',(-19.7110729118093,24.4041780824656,-63.9274090870936));
#68510=CARTESIAN_POINT('Ctrl Pts',(-19.6849158294033,24.2865779736527,-63.9334965868115));
#68511=CARTESIAN_POINT('Ctrl Pts',(-19.6641459833917,24.1676799042311,-63.9395840865293));
#68512=CARTESIAN_POINT('Ctrl Pts',(-19.6488788114747,24.048019641074,-63.9456715862472));
#68513=CARTESIAN_POINT('Ctrl Pts',(-19.6342025879445,23.9329910831126,-63.9515234563306));
#68514=CARTESIAN_POINT('Ctrl Pts',(-19.6246110311334,23.8172586872364,-63.9573753264141));
#68515=CARTESIAN_POINT('Ctrl Pts',(-19.6201544010332,23.7013077645549,-63.9632271964974));
#68516=CARTESIAN_POINT('Ctrl Pts',(-19.6156984494954,23.5853744964557,-63.9690781755804));
#68517=CARTESIAN_POINT('Ctrl Pts',(-19.6163758859941,23.4692231806724,-63.9749291546634));
#68518=CARTESIAN_POINT('Ctrl Pts',(-19.6221849154793,23.3533418858573,-63.9807801337463));
#68519=CARTESIAN_POINT('Ctrl Pts',(-19.6279944672522,23.2374501721985,-63.9866316388886));
#68520=CARTESIAN_POINT('Ctrl Pts',(-19.6389365084938,23.1218289406583,-63.9924831440309));
#68521=CARTESIAN_POINT('Ctrl Pts',(-19.6549572058332,23.0069631757101,-63.9983346491732));
#68522=CARTESIAN_POINT('Ctrl Pts',(-19.6709832232975,22.892059266342,-64.004188097473));
#68523=CARTESIAN_POINT('Ctrl Pts',(-19.6920911933078,22.7779117316164,-64.0100415457727));
#68524=CARTESIAN_POINT('Ctrl Pts',(-19.7181759325748,22.6649966712328,-64.0158949940725));
#68525=CARTESIAN_POINT('Ctrl Pts',(-19.7442903358544,22.5519532019065,-64.021755099014));
#68526=CARTESIAN_POINT('Ctrl Pts',(-19.7753927118145,22.4401454074695,-64.0276152039556));
#68527=CARTESIAN_POINT('Ctrl Pts',(-19.811327602115,22.3300355956655,-64.0334753088971));
#68528=CARTESIAN_POINT('Ctrl Pts',(-19.847286692315,22.2198516317948,-64.0393393602526));
#68529=CARTESIAN_POINT('Ctrl Pts',(-19.8880846318463,22.1113683134429,-64.045203411608));
#68530=CARTESIAN_POINT('Ctrl Pts',(-19.933517941516,22.0050276599657,-64.0510674629635));
#68531=CARTESIAN_POINT('Ctrl Pts',(-19.9790182108148,21.898530281593,-64.0569401567601));
#68532=CARTESIAN_POINT('Ctrl Pts',(-20.0291673064368,21.7941822417638,-64.0628128505566));
#68533=CARTESIAN_POINT('Ctrl Pts',(-20.0837159631312,21.6924007564398,-64.0686855443532));
#68534=CARTESIAN_POINT('Ctrl Pts',(-20.0986504728465,21.6645346883547,-64.0702933896765));
#68535=CARTESIAN_POINT('Ctrl Pts',(-20.1139145135817,21.6368608309317,-64.0719012349999));
#68536=CARTESIAN_POINT('Ctrl Pts',(-20.1295024200826,21.6093873447456,-64.0735090803232));
#68537=CARTESIAN_POINT('Ctrl Pts',(-20.186433777077,21.5090465549255,-64.0793813772919));
#68538=CARTESIAN_POINT('Ctrl Pts',(-20.2478791940212,21.4110447403216,-64.0852536742606));
#68539=CARTESIAN_POINT('Ctrl Pts',(-20.3136214733308,21.3158156021665,-64.0911259712293));
#68540=CARTESIAN_POINT('Ctrl Pts',(-20.3792785558675,21.2207098734114,-64.0969906581675));
#68541=CARTESIAN_POINT('Ctrl Pts',(-20.4492211945505,21.1283700126328,-64.1028553451057));
#68542=CARTESIAN_POINT('Ctrl Pts',(-20.5231865144831,21.0392048763428,-64.1087200320439));
#68543=CARTESIAN_POINT('Ctrl Pts',(-20.5970757657147,20.9501314408134,-64.1145786875187));
#68544=CARTESIAN_POINT('Ctrl Pts',(-20.6749792069993,20.8642265517596,-64.1204373429936));
#68545=CARTESIAN_POINT('Ctrl Pts',(-20.7565912995322,20.7818692634463,-64.1262959984684));
#68546=CARTESIAN_POINT('Ctrl Pts',(-20.8413912322822,20.6962950269123,-64.1323834981863));
#68547=CARTESIAN_POINT('Ctrl Pts',(-20.9301951907223,20.6145515600119,-64.1384709979042));
#68548=CARTESIAN_POINT('Ctrl Pts',(-21.0226148241633,20.5370255871266,-64.1445584976221));
#68549=CARTESIAN_POINT('Ctrl Pts',(-21.1114571589664,20.4625004220446,-64.1504103677055));
#68550=CARTESIAN_POINT('Ctrl Pts',(-21.2036401223324,20.3918726181543,-64.1562622377889));
#68551=CARTESIAN_POINT('Ctrl Pts',(-21.2987825815385,20.3254467912587,-64.1621141078723));
#68552=CARTESIAN_POINT('Ctrl Pts',(-21.39391055444,20.2590310782992,-64.1679650869553));
#68553=CARTESIAN_POINT('Ctrl Pts',(-21.49199678837,20.1968163068072,-64.1738160660383));
#68554=CARTESIAN_POINT('Ctrl Pts',(-21.592629692682,20.139064788374,-64.1796670451212));
#68555=CARTESIAN_POINT('Ctrl Pts',(-21.6932716448603,20.0813080775237,-64.1855185502635));
#68556=CARTESIAN_POINT('Ctrl Pts',(-21.7964603640337,20.0280156232292,-64.1913700554058));
#68557=CARTESIAN_POINT('Ctrl Pts',(-21.901758725408,19.9794042892403,-64.1972215605481));
#68558=CARTESIAN_POINT('Ctrl Pts',(-22.0070920540762,19.9307768124854,-64.2030750088479));
#68559=CARTESIAN_POINT('Ctrl Pts',(-22.1145360428575,19.8868337202332,-64.2089284571477));
#68560=CARTESIAN_POINT('Ctrl Pts',(-22.2236332850595,19.8477438720881,-64.2147819054474));
#68561=CARTESIAN_POINT('Ctrl Pts',(-22.3328545945158,19.8086095702975,-64.220642010389));
#68562=CARTESIAN_POINT('Ctrl Pts',(-22.4437325206441,19.774339668274,-64.2265021153305));
#68563=CARTESIAN_POINT('Ctrl Pts',(-22.5557940843599,19.745053273242,-64.2323622202721));
#68564=CARTESIAN_POINT('Ctrl Pts',(-22.667931114525,19.7157471556559,-64.2382262716275));
#68565=CARTESIAN_POINT('Ctrl Pts',(-22.7812529662782,19.6914313141979,-64.244090322983));
#68566=CARTESIAN_POINT('Ctrl Pts',(-22.8952777721892,19.6721734886097,-64.2499543743384));
#68567=CARTESIAN_POINT('Ctrl Pts',(-23.0094706279027,19.6528872808307,-64.255827068135));
#68568=CARTESIAN_POINT('Ctrl Pts',(-23.1243680967429,19.6386740172364,-64.2616997619315));
#68569=CARTESIAN_POINT('Ctrl Pts',(-23.2394844294858,19.6295495097031,-64.2675724557281));
#68570=CARTESIAN_POINT('Ctrl Pts',(-23.27100135573,19.6270513721749,-64.2691803010514));
#68571=CARTESIAN_POINT('Ctrl Pts',(-23.3025346974053,19.624934372634,-64.2707881463748));
#68572=CARTESIAN_POINT('Ctrl Pts',(-23.3340745265731,19.6231981559436,-64.2723959916981));
#68573=CARTESIAN_POINT('Ctrl Pts',(-23.4492667285384,19.6168570111456,-64.2782682886669));
#68574=CARTESIAN_POINT('Ctrl Pts',(-23.564931152178,19.615577935982,-64.2841405856356));
#68575=CARTESIAN_POINT('Ctrl Pts',(-23.6805855128659,19.6194126323827,-64.2900128826043));
#68576=CARTESIAN_POINT('Ctrl Pts',(-23.796089994687,19.6232423593215,-64.2958775695425));
#68577=CARTESIAN_POINT('Ctrl Pts',(-23.9115840301476,19.632172665445,-64.3017422564807));
#68578=CARTESIAN_POINT('Ctrl Pts',(-24.0265815463789,19.6462033939694,-64.3076069434188));
#68579=CARTESIAN_POINT('Ctrl Pts',(-24.141460794864,19.660219692768,-64.3134655988937));
#68580=CARTESIAN_POINT('Ctrl Pts',(-24.2558441319339,19.6793259307035,-64.3193242543685));
#68581=CARTESIAN_POINT('Ctrl Pts',(-24.3692474961989,19.7034699477527,-64.3251829098433));
#68582=CARTESIAN_POINT('Ctrl Pts',(-24.4870804957564,19.7285570513735,-64.3312704095612));
#68583=CARTESIAN_POINT('Ctrl Pts',(-24.6038549501757,19.7590835023726,-64.3373579092791));
#68584=CARTESIAN_POINT('Ctrl Pts',(-24.7190355817353,19.7949316157222,-64.343445408997));
#68585=CARTESIAN_POINT('Ctrl Pts',(-24.8297579017756,19.8293921515379,-64.3492972790804));
#68586=CARTESIAN_POINT('Ctrl Pts',(-24.9390070578119,19.8687699031585,-64.3551491491638));
#68587=CARTESIAN_POINT('Ctrl Pts',(-25.0463207530643,19.9129088749844,-64.3610010192472));
#68588=CARTESIAN_POINT('Ctrl Pts',(-25.1536181088305,19.9570411262505,-64.3668519983302));
#68589=CARTESIAN_POINT('Ctrl Pts',(-25.2589802075513,20.0059329991081,-64.3727029774131));
#68590=CARTESIAN_POINT('Ctrl Pts',(-25.3619638798905,20.0593800059756,-64.3785539564961));
#68591=CARTESIAN_POINT('Ctrl Pts',(-25.4649568114528,20.1128318182434,-64.3844054616384));
#68592=CARTESIAN_POINT('Ctrl Pts',(-25.5655705245983,20.1708393882361,-64.3902569667807));
#68593=CARTESIAN_POINT('Ctrl Pts',(-25.6633862837334,20.2331521795805,-64.396108471923));
#68594=CARTESIAN_POINT('Ctrl Pts',(-25.7612345253536,20.295485663647,-64.4019619202228));
#68595=CARTESIAN_POINT('Ctrl Pts',(-25.8562826169643,20.3621269898886,-64.4078153685225));
#68596=CARTESIAN_POINT('Ctrl Pts',(-25.9481412464389,20.4327826101553,-64.4136688168223));
#68597=CARTESIAN_POINT('Ctrl Pts',(-26.0401043391214,20.5035185812043,-64.4195289217639));
#68598=CARTESIAN_POINT('Ctrl Pts',(-26.1288704022038,20.5782777059454,-64.4253890267054));
#68599=CARTESIAN_POINT('Ctrl Pts',(-26.2140835635339,20.6567264416428,-64.431249131647));
#68600=CARTESIAN_POINT('Ctrl Pts',(-26.2993541105949,20.7352280076539,-64.4371131830024));
#68601=CARTESIAN_POINT('Ctrl Pts',(-26.3810667009177,20.8174238397464,-64.4429772343579));
#68602=CARTESIAN_POINT('Ctrl Pts',(-26.4589038741473,20.9029451509683,-64.4488412857133));
#68603=CARTESIAN_POINT('Ctrl Pts',(-26.5368557638323,20.9885925035311,-64.4547139795099));
#68604=CARTESIAN_POINT('Ctrl Pts',(-26.6109205737252,21.0775748003285,-64.4605866733064));
#68605=CARTESIAN_POINT('Ctrl Pts',(-26.6808224329813,21.1694919193782,-64.466459367103));
#68606=CARTESIAN_POINT('Ctrl Pts',(-26.6999603927303,21.1946572889883,-64.4680672124263));
#68607=CARTESIAN_POINT('Ctrl Pts',(-26.718786567932,21.2200424904158,-64.4696750577496));
#68608=CARTESIAN_POINT('Ctrl Pts',(-26.7372958908976,21.2456389791528,-64.471282903073));
#68609=CARTESIAN_POINT('Ctrl Pts',(-26.8054318389887,21.339863983014,-64.4772016536233));
#68610=CARTESIAN_POINT('Ctrl Pts',(-26.8694982636535,21.4372688892917,-64.4831204041736));
#68611=CARTESIAN_POINT('Ctrl Pts',(-26.9291869163797,21.5374705206483,-64.4890391547239));
#68612=CARTESIAN_POINT('Ctrl Pts',(-26.988795941757,21.6375384785194,-64.4949500093947));
#68613=CARTESIAN_POINT('Ctrl Pts',(-27.0440386046206,21.7403953974653,-64.5008608640654));
#68614=CARTESIAN_POINT('Ctrl Pts',(-27.0946481205995,21.8456267929032,-64.5067717187361));
#68615=CARTESIAN_POINT('Ctrl Pts',(-27.1452017244463,21.9507419313177,-64.5126760432419));
#68616=CARTESIAN_POINT('Ctrl Pts',(-27.1911321889275,22.0582259658421,-64.5185803677477));
#68617=CARTESIAN_POINT('Ctrl Pts',(-27.2322174367539,22.1676378211156,-64.5244846922535));
#68618=CARTESIAN_POINT('Ctrl Pts',(-27.273592559287,22.2778216257168,-64.5304306743961));
#68619=CARTESIAN_POINT('Ctrl Pts',(-27.3100536038442,22.3899602092726,-64.5363766565388));
#68620=CARTESIAN_POINT('Ctrl Pts',(-27.3414218951241,22.5035797758673,-64.5423226386814));
#68621=CARTESIAN_POINT('Ctrl Pts',(-27.3725217740672,22.6162271220402,-64.5482177422171));
#68622=CARTESIAN_POINT('Ctrl Pts',(-27.3986156100069,22.7303298065523,-64.5541128457528));
#68623=CARTESIAN_POINT('Ctrl Pts',(-27.4195786389942,22.8454089494954,-64.5600079492885));
#68624=CARTESIAN_POINT('Ctrl Pts',(-27.4408130549991,22.9619779050709,-64.5659793707346));
#68625=CARTESIAN_POINT('Ctrl Pts',(-27.456782747268,23.0795483776637,-64.5719507921807));
#68626=CARTESIAN_POINT('Ctrl Pts',(-27.4674113082267,23.1976109013743,-64.5779222136267));
#68627=CARTESIAN_POINT('Ctrl Pts',(-27.4780398691853,23.315673425085,-64.5838936350728));
#68628=CARTESIAN_POINT('Ctrl Pts',(-27.4833272543798,23.4342275698376,-64.5898650565189));
#68629=CARTESIAN_POINT('Ctrl Pts',(-27.4832517333937,23.5527584109668,-64.595836477965));
#68630=CARTESIAN_POINT('',(-27.4850627174193,23.5522765954312,-65.8458358713706));
#68631=CARTESIAN_POINT('Ctrl Pts',(-27.478390383421,23.5527855069586,-64.5958380009472));
#68632=CARTESIAN_POINT('Ctrl Pts',(-27.4812350713865,24.0440006034334,-64.6206152721141));
#68633=CARTESIAN_POINT('Ctrl Pts',(-27.1676348699015,25.8460339334477,-64.7116881804063));
#68634=CARTESIAN_POINT('Ctrl Pts',(-24.4627872245136,28.1118346329514,-64.8690567258226));
#68635=CARTESIAN_POINT('Ctrl Pts',(-20.2057806611153,26.7837117844163,-65.0679436371978));
#68636=CARTESIAN_POINT('Ctrl Pts',(-19.0220601823267,22.4843140347648,-65.2668305485724));
#68637=CARTESIAN_POINT('Ctrl Pts',(-21.999364545208,19.1644233871103,-65.4657174599474));
#68638=CARTESIAN_POINT('Ctrl Pts',(-26.2715252890564,19.8537180446844,-65.6587188550772));
#68639=CARTESIAN_POINT('Ctrl Pts',(-27.4809586739053,22.3624402719865,-65.7854246130821));
#68640=CARTESIAN_POINT('Ctrl Pts',(-27.4884579349096,23.5522559503263,-65.845834733962));
#68641=CARTESIAN_POINT('',(-27.4832509814148,23.5467604699193,-67.0958364779651));
#68642=CARTESIAN_POINT('Ctrl Pts',(-27.4832520051843,23.5522876057256,-65.845836477965));
#68643=CARTESIAN_POINT('Ctrl Pts',(-27.4831921100013,23.6680414897683,-65.8517214128757));
#68644=CARTESIAN_POINT('Ctrl Pts',(-27.4780224898854,23.7836598109612,-65.8576063477865));
#68645=CARTESIAN_POINT('Ctrl Pts',(-27.4677759706825,23.8988197489962,-65.8634912826973));
#68646=CARTESIAN_POINT('Ctrl Pts',(-27.4575514559566,24.0137323801976,-65.8693635796661));
#68647=CARTESIAN_POINT('Ctrl Pts',(-27.4422494310259,24.1283872665401,-65.8752358766348));
#68648=CARTESIAN_POINT('Ctrl Pts',(-27.4218878101455,24.2422996909625,-65.8811081736036));
#68649=CARTESIAN_POINT('Ctrl Pts',(-27.4015525763087,24.3560644939294,-65.8869728605419));
#68650=CARTESIAN_POINT('Ctrl Pts',(-27.3761708577797,24.4690883452134,-65.8928375474801));
#68651=CARTESIAN_POINT('Ctrl Pts',(-27.3458124353828,24.5808902068794,-65.8987022344183));
#68652=CARTESIAN_POINT('Ctrl Pts',(-27.3154852347229,24.6925770873298,-65.9045608898932));
#68653=CARTESIAN_POINT('Ctrl Pts',(-27.2801916182897,24.8030440813435,-65.910419545368));
#68654=CARTESIAN_POINT('Ctrl Pts',(-27.2400525457537,24.9118195907283,-65.9162782008429));
#68655=CARTESIAN_POINT('Ctrl Pts',(-27.1983456056905,25.0248439673173,-65.9223657005608));
#68656=CARTESIAN_POINT('Ctrl Pts',(-27.1514070371028,25.1360415760795,-65.9284532002787));
#68657=CARTESIAN_POINT('Ctrl Pts',(-27.0994299852475,25.244899516523,-65.9345406999966));
#68658=CARTESIAN_POINT('Ctrl Pts',(-27.049464815823,25.3495438786655,-65.94039257008));
#68659=CARTESIAN_POINT('Ctrl Pts',(-26.9948441556283,25.4520259204937,-65.9462444401634));
#68660=CARTESIAN_POINT('Ctrl Pts',(-26.9357886115487,25.5519104575155,-65.9520963102468));
#68661=CARTESIAN_POINT('Ctrl Pts',(-26.8767420592127,25.6517797862084,-65.9579472893297));
#68662=CARTESIAN_POINT('Ctrl Pts',(-26.8132621759368,25.7490520407199,-65.9637982684127));
#68663=CARTESIAN_POINT('Ctrl Pts',(-26.745614820692,25.8433179128055,-65.9696492474957));
#68664=CARTESIAN_POINT('Ctrl Pts',(-26.6779613832989,25.9375922603001,-65.9755007526379));
#68665=CARTESIAN_POINT('Ctrl Pts',(-26.6061399701061,26.0288593521594,-65.9813522577802));
#68666=CARTESIAN_POINT('Ctrl Pts',(-26.5304585140938,26.1167406580002,-65.9872037629225));
#68667=CARTESIAN_POINT('Ctrl Pts',(-26.4547519259174,26.2046511473096,-65.9930572112223));
#68668=CARTESIAN_POINT('Ctrl Pts',(-26.3751830156822,26.289173301837,-65.998910659522));
#68669=CARTESIAN_POINT('Ctrl Pts',(-26.2920980699472,26.3699638723038,-66.0047641078218));
#68670=CARTESIAN_POINT('Ctrl Pts',(-26.2089186385874,26.4508463191924,-66.0106242127633));
#68671=CARTESIAN_POINT('Ctrl Pts',(-26.122215487396,26.5279884235244,-66.0164843177048));
#68672=CARTESIAN_POINT('Ctrl Pts',(-26.0323696951043,26.6010857600279,-66.0223444226463));
#68673=CARTESIAN_POINT('Ctrl Pts',(-25.9424633972947,26.6742323230125,-66.0282084740017));
#68674=CARTESIAN_POINT('Ctrl Pts',(-25.8494105753464,26.7433284485053,-66.0340725253572));
#68675=CARTESIAN_POINT('Ctrl Pts',(-25.7536216866102,26.8081127753457,-66.0399365767126));
#68676=CARTESIAN_POINT('Ctrl Pts',(-25.6576916241731,26.8729925813517,-66.0458092705091));
#68677=CARTESIAN_POINT('Ctrl Pts',(-25.5590177980276,26.9335476904816,-66.0516819643057));
#68678=CARTESIAN_POINT('Ctrl Pts',(-25.458035720091,26.9895623906733,-66.0575546581023));
#68679=CARTESIAN_POINT('Ctrl Pts',(-25.430388516378,27.004898278573,-66.0591625034255));
#68680=CARTESIAN_POINT('Ctrl Pts',(-25.4025684081857,27.0198941081355,-66.0607703487487));
#68681=CARTESIAN_POINT('Ctrl Pts',(-25.3745845778111,27.034546087856,-66.0623781940719));
#68682=CARTESIAN_POINT('Ctrl Pts',(-25.2723798694919,27.0880591807242,-66.0682504910406));
#68683=CARTESIAN_POINT('Ctrl Pts',(-25.1676473967304,27.1371611570424,-66.0741227880092));
#68684=CARTESIAN_POINT('Ctrl Pts',(-25.0608046435372,27.181605078254,-66.0799950849779));
#68685=CARTESIAN_POINT('Ctrl Pts',(-24.9541003500669,27.2259914036735,-66.0858597719161));
#68686=CARTESIAN_POINT('Ctrl Pts',(-24.8452915927674,27.2657315210544,-66.0917244588543));
#68687=CARTESIAN_POINT('Ctrl Pts',(-24.7348207964185,27.3006241167786,-66.0975891457925));
#68688=CARTESIAN_POINT('Ctrl Pts',(-24.6244636123681,27.3354808276523,-66.1034478012673));
#68689=CARTESIAN_POINT('Ctrl Pts',(-24.5124481809777,27.3654998092747,-66.1093064567421));
#68690=CARTESIAN_POINT('Ctrl Pts',(-24.3992366495488,27.3905279082305,-66.1151651122169));
#68691=CARTESIAN_POINT('Ctrl Pts',(-24.2816029759865,27.4165336267759,-66.1212526119348));
#68692=CARTESIAN_POINT('Ctrl Pts',(-24.162678275845,27.4371504430135,-66.1273401116528));
#68693=CARTESIAN_POINT('Ctrl Pts',(-24.0429984641129,27.4522636088293,-66.1334276113707));
#68694=CARTESIAN_POINT('Ctrl Pts',(-23.9279511142459,27.466791787392,-66.1392794814541));
#68695=CARTESIAN_POINT('Ctrl Pts',(-23.8122064706178,27.4762343976616,-66.1451313515375));
#68696=CARTESIAN_POINT('Ctrl Pts',(-23.696249908617,27.4805418042455,-66.1509832216209));
#68697=CARTESIAN_POINT('Ctrl Pts',(-23.5803110020571,27.4848485549875,-66.1568342007039));
#68698=CARTESIAN_POINT('Ctrl Pts',(-23.4641606542651,27.4840216413335,-66.1626851797869));
#68699=CARTESIAN_POINT('Ctrl Pts',(-23.348286931179,27.4780634864384,-66.1685361588699));
#68700=CARTESIAN_POINT('Ctrl Pts',(-23.2324027899302,27.4721047958478,-66.1743876640122));
#68701=CARTESIAN_POINT('Ctrl Pts',(-23.1167957356909,27.4610139681281,-66.1802391691545));
#68702=CARTESIAN_POINT('Ctrl Pts',(-23.0019506832539,27.444845460743,-66.1860906742968));
#68703=CARTESIAN_POINT('Ctrl Pts',(-22.887067493275,27.4286715841485,-66.1919441225965));
#68704=CARTESIAN_POINT('Ctrl Pts',(-22.7729472173903,27.4074167326116,-66.1977975708963));
#68705=CARTESIAN_POINT('Ctrl Pts',(-22.6600658195423,27.3811867020381,-66.2036510191961));
#68706=CARTESIAN_POINT('Ctrl Pts',(-22.5470560510331,27.354926842224,-66.2095111241376));
#68707=CARTESIAN_POINT('Ctrl Pts',(-22.4352883755231,27.3236806040775,-66.2153712290792));
#68708=CARTESIAN_POINT('Ctrl Pts',(-22.3252249003106,27.287604040764,-66.2212313340208));
#68709=CARTESIAN_POINT('Ctrl Pts',(-22.2150873042362,27.2515031821432,-66.2270953853762));
#68710=CARTESIAN_POINT('Ctrl Pts',(-22.1066565794953,27.2105656667968,-66.2329594367317));
#68711=CARTESIAN_POINT('Ctrl Pts',(-22.000374483216,27.1649955425935,-66.2388234880871));
#68712=CARTESIAN_POINT('Ctrl Pts',(-21.8939357483426,27.1193582571238,-66.2446961818837));
#68713=CARTESIAN_POINT('Ctrl Pts',(-21.7896523329111,27.0690749152121,-66.2505688756803));
#68714=CARTESIAN_POINT('Ctrl Pts',(-21.6879411317527,27.0143953188275,-66.2564415694769));
#68715=CARTESIAN_POINT('Ctrl Pts',(-21.6600943062949,26.9994249600147,-66.2580494148003));
#68716=CARTESIAN_POINT('Ctrl Pts',(-21.632440115421,26.984125317815,-66.2596572601237));
#68717=CARTESIAN_POINT('Ctrl Pts',(-21.6049867124081,26.9685020679799,-66.2612651054471));
#68718=CARTESIAN_POINT('Ctrl Pts',(-21.5047192719105,26.9114416273313,-66.2671374024158));
#68719=CARTESIAN_POINT('Ctrl Pts',(-21.4067966139366,26.8498701405502,-66.2730096993845));
#68720=CARTESIAN_POINT('Ctrl Pts',(-21.3116521598433,26.784005363181,-66.2788819963532));
#68721=CARTESIAN_POINT('Ctrl Pts',(-21.2166310054064,26.7182259413325,-66.2847466832914));
#68722=CARTESIAN_POINT('Ctrl Pts',(-21.1243812318333,26.6481645263437,-66.2906113702296));
#68723=CARTESIAN_POINT('Ctrl Pts',(-21.0353113569978,26.57408451906,-66.2964760571678));
#68724=CARTESIAN_POINT('Ctrl Pts',(-20.9463330849527,26.5000806984263,-66.3023347126426));
#68725=CARTESIAN_POINT('Ctrl Pts',(-20.86052852271,26.4220667687367,-66.3081933681175));
#68726=CARTESIAN_POINT('Ctrl Pts',(-20.778276331016,26.3403487563563,-66.3140520235923));
#68727=CARTESIAN_POINT('Ctrl Pts',(-20.6928112962676,26.2554387664361,-66.3201395233102));
#68728=CARTESIAN_POINT('Ctrl Pts',(-20.6111821808506,26.1665296840443,-66.3262270230281));
#68729=CARTESIAN_POINT('Ctrl Pts',(-20.5337752090489,26.0740103572326,-66.332314522746));
#68730=CARTESIAN_POINT('Ctrl Pts',(-20.4593644388601,25.9850721879029,-66.3381663928294));
#68731=CARTESIAN_POINT('Ctrl Pts',(-20.3888553257652,25.8927984083777,-66.3440182629128));
#68732=CARTESIAN_POINT('Ctrl Pts',(-20.3225519948264,25.7975705430809,-66.3498701329962));
#68733=CARTESIAN_POINT('Ctrl Pts',(-20.2562587591726,25.7023571770926,-66.3557211120791));
#68734=CARTESIAN_POINT('Ctrl Pts',(-20.1941702685596,25.6041909588105,-66.3615720911621));
#68735=CARTESIAN_POINT('Ctrl Pts',(-20.1365483046765,25.5034838161153,-66.367423070245));
#68736=CARTESIAN_POINT('Ctrl Pts',(-20.0789211600242,25.4027676188787,-66.3732745753873));
#68737=CARTESIAN_POINT('Ctrl Pts',(-20.0257615457222,25.2995104019073,-66.3791260805296));
#68738=CARTESIAN_POINT('Ctrl Pts',(-19.9772857627949,25.1941495687198,-66.3849775856719));
#68739=CARTESIAN_POINT('Ctrl Pts',(-19.9287938821155,25.0887537474933,-66.3908310339717));
#68740=CARTESIAN_POINT('Ctrl Pts',(-19.884989098315,24.9812532963402,-66.3966844822715));
#68741=CARTESIAN_POINT('Ctrl Pts',(-19.8460396822115,24.8721058388836,-66.4025379305712));
#68742=CARTESIAN_POINT('Ctrl Pts',(-19.8070459721642,24.7628342570669,-66.4083980355127));
#68743=CARTESIAN_POINT('Ctrl Pts',(-19.7729187897928,24.6519123200544,-66.4142581404543));
#68744=CARTESIAN_POINT('Ctrl Pts',(-19.7437766335357,24.5398131598208,-66.4201182453958));
#68745=CARTESIAN_POINT('Ctrl Pts',(-19.7146148518602,24.4276385078188,-66.4259822967512));
#68746=CARTESIAN_POINT('Ctrl Pts',(-19.6904448669539,24.3142854573075,-66.4318463481067));
#68747=CARTESIAN_POINT('Ctrl Pts',(-19.6713337983761,24.2002359624937,-66.4377103994621));
#68748=CARTESIAN_POINT('Ctrl Pts',(-19.6521945638982,24.086018381491,-66.4435830932587));
#68749=CARTESIAN_POINT('Ctrl Pts',(-19.6381291761864,23.9711027164301,-66.4494557870552));
#68750=CARTESIAN_POINT('Ctrl Pts',(-19.6291528219826,23.8559747364813,-66.4553284808518));
#68751=CARTESIAN_POINT('Ctrl Pts',(-19.6266952463577,23.8244546214269,-66.4569363261751));
#68752=CARTESIAN_POINT('Ctrl Pts',(-19.6246188295299,23.7929185814501,-66.4585441714985));
#68753=CARTESIAN_POINT('Ctrl Pts',(-19.6229232035861,23.7613765440241,-66.4601520168218));
#68754=CARTESIAN_POINT('Ctrl Pts',(-19.6167303074505,23.6461762768871,-66.4660243137905));
#68755=CARTESIAN_POINT('Ctrl Pts',(-19.61560008447,23.5305103029573,-66.4718966107592));
#68756=CARTESIAN_POINT('Ctrl Pts',(-19.6195836158691,23.4148609729973,-66.4777689077279));
#68757=CARTESIAN_POINT('Ctrl Pts',(-19.6235619849278,23.2993615153842,-66.4836335946661));
#68758=CARTESIAN_POINT('Ctrl Pts',(-19.6326409155039,23.183879068172,-66.4894982816044));
#68759=CARTESIAN_POINT('Ctrl Pts',(-19.6468196252758,23.0688997036252,-66.4953629685426));
#68760=CARTESIAN_POINT('Ctrl Pts',(-19.6609837531323,22.9540385881571,-66.5012216240174));
#68761=CARTESIAN_POINT('Ctrl Pts',(-19.6802371777114,22.8396799340498,-66.5070802794922));
#68762=CARTESIAN_POINT('Ctrl Pts',(-19.7045271160835,22.7263077351659,-66.512938934967));
#68763=CARTESIAN_POINT('Ctrl Pts',(-19.7297658408427,22.6085071183368,-66.5190264346849));
#68764=CARTESIAN_POINT('Ctrl Pts',(-19.7604425462107,22.4917720457867,-66.5251139344028));
#68765=CARTESIAN_POINT('Ctrl Pts',(-19.7964388583962,22.3766376433423,-66.5312014341207));
#68766=CARTESIAN_POINT('Ctrl Pts',(-19.8310418566964,22.2659597630209,-66.5370533042041));
#68767=CARTESIAN_POINT('Ctrl Pts',(-19.870560170882,22.1567613735582,-66.5429051742875));
#68768=CARTESIAN_POINT('Ctrl Pts',(-19.9148372105427,22.0495045705971,-66.5487570443709));
#68769=CARTESIAN_POINT('Ctrl Pts',(-19.9591075086215,21.9422640984595,-66.5546080234539));
#68770=CARTESIAN_POINT('Ctrl Pts',(-20.008134933825,21.8369650070279,-66.5604590025369));
#68771=CARTESIAN_POINT('Ctrl Pts',(-20.0617144284166,21.7340502021118,-66.5663099816199));
#68772=CARTESIAN_POINT('Ctrl Pts',(-20.1152987403204,21.6311261441644,-66.5721614867622));
#68773=CARTESIAN_POINT('Ctrl Pts',(-20.1734357443073,21.5305871655698,-66.5780129919045));
#68774=CARTESIAN_POINT('Ctrl Pts',(-20.2358743653315,21.4328516791539,-66.5838644970468));
#68775=CARTESIAN_POINT('Ctrl Pts',(-20.2983337208625,21.3350837369106,-66.5897179453465));
#68776=CARTESIAN_POINT('Ctrl Pts',(-20.365097311426,21.240121486216,-66.5955713936463));
#68777=CARTESIAN_POINT('Ctrl Pts',(-20.4358710881004,21.1483538611007,-66.6014248419461));
#68778=CARTESIAN_POINT('Ctrl Pts',(-20.5067253499271,21.0564818762688,-66.6072849468876));
#68779=CARTESIAN_POINT('Ctrl Pts',(-20.5815986477857,20.9678120958755,-66.6131450518292));
#68780=CARTESIAN_POINT('Ctrl Pts',(-20.660156981237,20.8826999625351,-66.6190051567707));
#68781=CARTESIAN_POINT('Ctrl Pts',(-20.738768218809,20.7975305114998,-66.6248692081262));
#68782=CARTESIAN_POINT('Ctrl Pts',(-20.8210691405895,20.7159237684898,-66.6307332594816));
#68783=CARTESIAN_POINT('Ctrl Pts',(-20.906690551385,20.638196718997,-66.6365973108371));
#68784=CARTESIAN_POINT('Ctrl Pts',(-20.9924381510483,20.560355115349,-66.6424700046337));
#68785=CARTESIAN_POINT('Ctrl Pts',(-21.0815156898151,20.4864048800883,-66.6483426984303));
#68786=CARTESIAN_POINT('Ctrl Pts',(-21.17352269101,20.4166213689054,-66.6542153922268));
#68787=CARTESIAN_POINT('Ctrl Pts',(-21.198712668848,20.3975158108791,-66.6558232375502));
#68788=CARTESIAN_POINT('Ctrl Pts',(-21.2241220770787,20.3787223200483,-66.6574310828735));
#68789=CARTESIAN_POINT('Ctrl Pts',(-21.2497423646799,20.3602459531016,-66.6590389281968));
#68790=CARTESIAN_POINT('Ctrl Pts',(-21.3433147593839,20.2927651376033,-66.6649112251655));
#68791=CARTESIAN_POINT('Ctrl Pts',(-21.4400155504888,20.229291899709,-66.6707835221342));
#68792=CARTESIAN_POINT('Ctrl Pts',(-21.5394665397721,20.1701299459453,-66.6766558191029));
#68793=CARTESIAN_POINT('Ctrl Pts',(-21.6387886484716,20.1110446613751,-66.6825205060411));
#68794=CARTESIAN_POINT('Ctrl Pts',(-21.7408535157637,20.0562597596307,-66.6883851929793));
#68795=CARTESIAN_POINT('Ctrl Pts',(-21.8452517780188,20.0060373251969,-66.6942498799175));
#68796=CARTESIAN_POINT('Ctrl Pts',(-21.9495426731966,19.9558665413931,-66.7001085353923));
#68797=CARTESIAN_POINT('Ctrl Pts',(-22.0561618198304,19.9102490699777,-66.7059671908672));
#68798=CARTESIAN_POINT('Ctrl Pts',(-22.1646734943517,19.8694021229874,-66.711825846342));
#68799=CARTESIAN_POINT('Ctrl Pts',(-22.2774237304557,19.8269596582701,-66.7179133460599));
#68800=CARTESIAN_POINT('Ctrl Pts',(-22.3922169653313,19.7896682297332,-66.7240008457778));
#68801=CARTESIAN_POINT('Ctrl Pts',(-22.5085390025895,19.7577175057148,-66.7300883454957));
#68802=CARTESIAN_POINT('Ctrl Pts',(-22.6203585477911,19.7270035024803,-66.7359402155791));
#68803=CARTESIAN_POINT('Ctrl Pts',(-22.7335903091212,19.7012245644998,-66.7417920856625));
#68804=CARTESIAN_POINT('Ctrl Pts',(-22.847760874007,19.6804987319183,-66.7476439557459));
#68805=CARTESIAN_POINT('Ctrl Pts',(-22.9619140553862,19.6597760550333,-66.7534949348288));
#68806=CARTESIAN_POINT('Ctrl Pts',(-23.0770053494842,19.6441050275871,-66.7593459139118));
#68807=CARTESIAN_POINT('Ctrl Pts',(-23.1925512898128,19.6335525404316,-66.7651968929947));
#68808=CARTESIAN_POINT('Ctrl Pts',(-23.3081076188334,19.6229991045059,-66.771048398137));
#68809=CARTESIAN_POINT('Ctrl Pts',(-23.4241182636503,19.6175651613169,-66.7768999032793));
#68810=CARTESIAN_POINT('Ctrl Pts',(-23.5400954898268,19.617265647086,-66.7827514084216));
#68811=CARTESIAN_POINT('Ctrl Pts',(-23.6561112295153,19.6169660333929,-66.7886048567214));
#68812=CARTESIAN_POINT('Ctrl Pts',(-23.7720931153339,19.6218042400739,-66.7944583050212));
#68813=CARTESIAN_POINT('Ctrl Pts',(-23.8875549846491,19.6317431141694,-66.8003117533209));
#68814=CARTESIAN_POINT('Ctrl Pts',(-24.0031481591818,19.6416932909229,-66.8061718582625));
#68815=CARTESIAN_POINT('Ctrl Pts',(-24.1182197247471,19.6567556773726,-66.812031963204));
#68816=CARTESIAN_POINT('Ctrl Pts',(-24.2322901001133,19.6768414051463,-66.8178920681455));
#68817=CARTESIAN_POINT('Ctrl Pts',(-24.3464372947379,19.6969406594005,-66.823756119501));
#68818=CARTESIAN_POINT('Ctrl Pts',(-24.4595815540564,19.7220699016073,-66.8296201708564));
#68819=CARTESIAN_POINT('Ctrl Pts',(-24.5712566272026,19.7520898657523,-66.8354842222119));
#68820=CARTESIAN_POINT('Ctrl Pts',(-24.683096287114,19.7821540733318,-66.8413569160084));
#68821=CARTESIAN_POINT('Ctrl Pts',(-24.7934620467624,19.8171232641298,-66.847229609805));
#68822=CARTESIAN_POINT('Ctrl Pts',(-24.901905770165,19.8568093518238,-66.8531023036016));
#68823=CARTESIAN_POINT('Ctrl Pts',(-24.9315958475913,19.8676747387674,-66.8547101489249));
#68824=CARTESIAN_POINT('Ctrl Pts',(-24.9611419890797,19.8788934217309,-66.8563179942483));
#68825=CARTESIAN_POINT('Ctrl Pts',(-24.9905353181631,19.89046093995,-66.8579258395717));
#68826=CARTESIAN_POINT('Ctrl Pts',(-25.0978879066045,19.9327087241036,-66.8637981365404));
#68827=CARTESIAN_POINT('Ctrl Pts',(-25.2035598836444,19.9797547462265,-66.869670433509));
#68828=CARTESIAN_POINT('Ctrl Pts',(-25.3070913037141,20.0314449880613,-66.8755427304777));
#68829=CARTESIAN_POINT('Ctrl Pts',(-25.4104885552857,20.0830682434479,-66.8814074174159));
#68830=CARTESIAN_POINT('Ctrl Pts',(-25.5117503999262,20.1393235668807,-66.8872721043542));
#68831=CARTESIAN_POINT('Ctrl Pts',(-25.6104350631652,20.2000082216443,-66.8931367912924));
#68832=CARTESIAN_POINT('Ctrl Pts',(-25.7090182354057,20.2606304660393,-66.8989954467672));
#68833=CARTESIAN_POINT('Ctrl Pts',(-25.8050291481507,20.3256727658229,-66.904854102242));
#68834=CARTESIAN_POINT('Ctrl Pts',(-25.8980495302091,20.3948859517602,-66.9107127577169));
#68835=CARTESIAN_POINT('Ctrl Pts',(-25.9947033703219,20.4668026657023,-66.9168002574348));
#68836=CARTESIAN_POINT('Ctrl Pts',(-26.0881278847157,20.5432225422124,-66.9228877571526));
#68837=CARTESIAN_POINT('Ctrl Pts',(-26.1778855572887,20.6238155030183,-66.9289752568705));
#68838=CARTESIAN_POINT('Ctrl Pts',(-26.2641689680855,20.7012889417252,-66.9348271269539));
#68839=CARTESIAN_POINT('Ctrl Pts',(-26.3470637883679,20.7826181135374,-66.9406789970374));
#68840=CARTESIAN_POINT('Ctrl Pts',(-26.4262148094164,20.8674685342172,-66.9465308671208));
#68841=CARTESIAN_POINT('Ctrl Pts',(-26.5053537790023,20.9523060356488,-66.9523818462037));
#68842=CARTESIAN_POINT('Ctrl Pts',(-26.5807498008514,21.040663417727,-66.9582328252867));
#68843=CARTESIAN_POINT('Ctrl Pts',(-26.6520852644353,21.1321700893246,-66.9640838043697));
#68844=CARTESIAN_POINT('Ctrl Pts',(-26.7234271417638,21.2236849882525,-66.969935309512));
#68845=CARTESIAN_POINT('Ctrl Pts',(-26.7907074809046,21.3183494135374,-66.9757868146542));
#68846=CARTESIAN_POINT('Ctrl Pts',(-26.8536500746243,21.415761099675,-66.9816383197965));
#68847=CARTESIAN_POINT('Ctrl Pts',(-26.9166135702093,21.5132051341132,-66.9874917680963));
#68848=CARTESIAN_POINT('Ctrl Pts',(-26.975236231858,21.6133978964424,-66.9933452163961));
#68849=CARTESIAN_POINT('Ctrl Pts',(-27.0292865254656,21.7159102871326,-66.9991986646959));
#68850=CARTESIAN_POINT('Ctrl Pts',(-27.0833982859936,21.818539256671,-67.0050587696374));
#68851=CARTESIAN_POINT('Ctrl Pts',(-27.132927106971,21.9234927538961,-67.0109188745789));
#68852=CARTESIAN_POINT('Ctrl Pts',(-27.1776885208635,22.0303192619487,-67.0167789795205));
#68853=CARTESIAN_POINT('Ctrl Pts',(-27.2224800787668,22.1372177109685,-67.0226430308759));
#68854=CARTESIAN_POINT('Ctrl Pts',(-27.2624976943609,22.2459912954124,-67.0285070822314));
#68855=CARTESIAN_POINT('Ctrl Pts',(-27.2976065061211,22.3561724714191,-67.0343711335868));
#68856=CARTESIAN_POINT('Ctrl Pts',(-27.3327670612616,22.4665160324851,-67.0402438273834));
#68857=CARTESIAN_POINT('Ctrl Pts',(-27.3630042661482,22.578270927897,-67.04611652118));
#68858=CARTESIAN_POINT('Ctrl Pts',(-27.3882341244631,22.6909584647025,-67.0519892149766));
#68859=CARTESIAN_POINT('Ctrl Pts',(-27.3951416376258,22.7218104272479,-67.0535970602999));
#68860=CARTESIAN_POINT('Ctrl Pts',(-27.4016741134431,22.7527322655498,-67.0552049056232));
#68861=CARTESIAN_POINT('Ctrl Pts',(-27.4078305067238,22.7837141004552,-67.0568127509466));
#68862=CARTESIAN_POINT('Ctrl Pts',(-27.440427587772,22.9477577762541,-67.065326025185));
#68863=CARTESIAN_POINT('Ctrl Pts',(-27.4625690874079,23.1139424991538,-67.0738392994233));
#68864=CARTESIAN_POINT('Ctrl Pts',(-27.4740372302633,23.2811751464035,-67.0823525736617));
#68865=CARTESIAN_POINT('Ctrl Pts',(-27.480091905839,23.3694666367974,-67.0868472084295));
#68866=CARTESIAN_POINT('Ctrl Pts',(-27.4831722163398,23.4580498634429,-67.0913418431973));
#68867=CARTESIAN_POINT('Ctrl Pts',(-27.4832509814148,23.5467604699193,-67.0958364779651));
#68868=CARTESIAN_POINT('',(-27.4767668984626,23.5498433970659,-68.3458364779651));
#68869=CARTESIAN_POINT('Ctrl Pts',(-27.4847103606465,23.5467734800025,-67.0958372025195));
#68870=CARTESIAN_POINT('Ctrl Pts',(-27.4749839165426,24.5989084225538,-67.1491246891201));
#68871=CARTESIAN_POINT('Ctrl Pts',(-26.4981045555357,26.9759418482296,-67.2687078128457));
#68872=CARTESIAN_POINT('Ctrl Pts',(-22.4784874858222,28.077069351332,-67.4545865736964));
#68873=CARTESIAN_POINT('Ctrl Pts',(-19.1624311466427,25.0954950126635,-67.6534734850713));
#68874=CARTESIAN_POINT('Ctrl Pts',(-19.8784106344222,20.6939738489423,-67.852360396446));
#68875=CARTESIAN_POINT('Ctrl Pts',(-23.968501504941,18.9171306221722,-68.051247307821));
#68876=CARTESIAN_POINT('Ctrl Pts',(-27.0333951896357,20.9687458373182,-68.215739334994));
#68877=CARTESIAN_POINT('Ctrl Pts',(-27.4773521810207,22.9167498443613,-68.313935725042));
#68878=CARTESIAN_POINT('Ctrl Pts',(-27.4767668984626,23.5498433970659,-68.3458364779651));
#68879=CARTESIAN_POINT('',(-27.4832039003184,23.5538862193999,-69.5958364779651));
#68880=CARTESIAN_POINT('Ctrl Pts',(-27.4767668984626,23.5498433970659,-68.3458364779651));
#68881=CARTESIAN_POINT('Ctrl Pts',(-27.4761358561213,24.2324347919078,-68.380231362167));
#68882=CARTESIAN_POINT('Ctrl Pts',(-26.9814714499248,26.231567390239,-68.4809218834938));
#68883=CARTESIAN_POINT('Ctrl Pts',(-23.7939922423769,28.1958248092063,-68.6479080419455));
#68884=CARTESIAN_POINT('Ctrl Pts',(-19.7736062765533,26.2664435955882,-68.8467949533207));
#68885=CARTESIAN_POINT('Ctrl Pts',(-19.2236380124017,21.8411130893086,-69.0456818646953));
#68886=CARTESIAN_POINT('Ctrl Pts',(-22.649461655072,18.9863368193928,-69.2445687760705));
#68887=CARTESIAN_POINT('Ctrl Pts',(-26.5714951847596,20.2210392543588,-69.4279536471601));
#68888=CARTESIAN_POINT('Ctrl Pts',(-27.4739245090166,22.5500065074999,-69.5450428811251));
#68889=CARTESIAN_POINT('Ctrl Pts',(-27.4832039003184,23.5538862193999,-69.5958364779651));
#68890=CARTESIAN_POINT('',(-27.4892926031819,23.5490236752345,-70.845836477965));
#68891=CARTESIAN_POINT('Ctrl Pts',(-27.4832039003184,23.5538862193999,-69.5958364779651));
#68892=CARTESIAN_POINT('Ctrl Pts',(-27.4860359403141,23.8602670371284,-69.6113385182501));
#68893=CARTESIAN_POINT('Ctrl Pts',(-27.313134779593,25.4737471440459,-69.6931361956599));
#68894=CARTESIAN_POINT('Ctrl Pts',(-25.08984694793,27.9400588904566,-69.841229510195));
#68895=CARTESIAN_POINT('Ctrl Pts',(-20.6892508390938,27.2184155792749,-70.0401164215698));
#68896=CARTESIAN_POINT('Ctrl Pts',(-18.9176727125942,23.1260414377581,-70.2390033329449));
#68897=CARTESIAN_POINT('Ctrl Pts',(-21.4030426622697,19.4234813216558,-70.4378902443196));
#68898=CARTESIAN_POINT('Ctrl Pts',(-25.8615164277807,19.51307406026,-70.6367771556946));
#68899=CARTESIAN_POINT('Ctrl Pts',(-27.4577312464195,22.110794924436,-70.7727592335762));
#68900=CARTESIAN_POINT('Ctrl Pts',(-27.4895653266935,23.4822771529814,-70.8424456743331));
#68901=CARTESIAN_POINT('Ctrl Pts',(-27.4892926031819,23.5490236752345,-70.845836477965));
#68902=CARTESIAN_POINT('',(-27.4821474792635,23.5472069989156,-72.0958360514227));
#68903=CARTESIAN_POINT('Ctrl Pts',(-27.4892926031819,23.5490236752345,-70.845836477965));
#68904=CARTESIAN_POINT('Ctrl Pts',(-27.4842331456164,24.7872784739266,-70.9087413114581));
#68905=CARTESIAN_POINT('Ctrl Pts',(-26.1861220606148,27.3396704490119,-71.0379417820763));
#68906=CARTESIAN_POINT('Ctrl Pts',(-21.835546490849,27.8746639197317,-71.2334378898192));
#68907=CARTESIAN_POINT('Ctrl Pts',(-18.9851813454571,24.4451692930999,-71.4323248011941));
#68908=CARTESIAN_POINT('Ctrl Pts',(-20.3297295849991,20.1933219148442,-71.6312117125691));
#68909=CARTESIAN_POINT('Ctrl Pts',(-24.6336653213793,19.0262093874363,-71.8300986239438));
#68910=CARTESIAN_POINT('Ctrl Pts',(-27.2099139446467,21.3546175314318,-71.9849730572581));
#68911=CARTESIAN_POINT('Ctrl Pts',(-27.4826159325481,23.1057213294587,-72.0735518534471));
#68912=CARTESIAN_POINT('Ctrl Pts',(-27.4794588064285,23.5471884932199,-72.0958350125112));
#68913=CARTESIAN_POINT('',(-27.481501086808,23.5526898751615,-73.3458370071997));
#68914=CARTESIAN_POINT('Ctrl Pts',(-27.4832513584104,23.5472145967353,-72.095836477965));
#68915=CARTESIAN_POINT('Ctrl Pts',(-27.4833409718037,23.6632306982906,-72.1016868061657));
#68916=CARTESIAN_POINT('Ctrl Pts',(-27.4782928946537,23.7793051745592,-72.1075371343664));
#68917=CARTESIAN_POINT('Ctrl Pts',(-27.4681183761652,23.8949498260379,-72.113387462567));
#68918=CARTESIAN_POINT('Ctrl Pts',(-27.457945360829,24.0105773925284,-72.119236926458));
#68919=CARTESIAN_POINT('Ctrl Pts',(-27.4426474459296,24.1257748492107,-72.1250863903491));
#68920=CARTESIAN_POINT('Ctrl Pts',(-27.4222878729755,24.2400578055713,-72.1309358542401));
#68921=CARTESIAN_POINT('Ctrl Pts',(-27.4019263907767,24.3543514789602,-72.136785866672));
#68922=CARTESIAN_POINT('Ctrl Pts',(-27.3765023790015,24.4677300748901,-72.1426358791038));
#68923=CARTESIAN_POINT('Ctrl Pts',(-27.346130322552,24.5797187996565,-72.1484858915357));
#68924=CARTESIAN_POINT('Ctrl Pts',(-27.3157480826565,24.6917450731197,-72.1543378654181));
#68925=CARTESIAN_POINT('Ctrl Pts',(-27.2804146068323,24.8023801502962,-72.1601898393005));
#68926=CARTESIAN_POINT('Ctrl Pts',(-27.2402942145768,24.9111644974689,-72.1660418131829));
#68927=CARTESIAN_POINT('Ctrl Pts',(-27.2001256652783,25.0200794199474,-72.1719008112678));
#68928=CARTESIAN_POINT('Ctrl Pts',(-27.1551588714224,25.1271387895848,-72.1777598093527));
#68929=CARTESIAN_POINT('Ctrl Pts',(-27.1056063485421,25.2319029820035,-72.1836188074376));
#68930=CARTESIAN_POINT('Ctrl Pts',(-27.0560204868967,25.3367376594064,-72.1894817474359));
#68931=CARTESIAN_POINT('Ctrl Pts',(-27.0018429450793,25.4392737202483,-72.1953446874343));
#68932=CARTESIAN_POINT('Ctrl Pts',(-26.9433313556434,25.5390976977309,-72.2012076274327));
#68933=CARTESIAN_POINT('Ctrl Pts',(-26.8847251742034,25.6390830543552,-72.2070800456772));
#68934=CARTESIAN_POINT('Ctrl Pts',(-26.8217711792399,25.7363472275307,-72.2129524639217));
#68935=CARTESIAN_POINT('Ctrl Pts',(-26.7547694728672,25.830506941565,-72.2188248821662));
#68936=CARTESIAN_POINT('Ctrl Pts',(-26.7203598970834,25.8788638565042,-72.2218407370087));
#68937=CARTESIAN_POINT('Ctrl Pts',(-26.6848833939656,25.9264025322493,-72.2248565918512));
#68938=CARTESIAN_POINT('Ctrl Pts',(-26.6483844666265,25.9730747525252,-72.2278724466937));
#68939=CARTESIAN_POINT('Ctrl Pts',(-26.5773158620215,26.0639522059367,-72.2337447451685));
#68940=CARTESIAN_POINT('Ctrl Pts',(-26.5021262477415,26.1518522713299,-72.2396170436432));
#68941=CARTESIAN_POINT('Ctrl Pts',(-26.4230942404892,26.2363779040862,-72.2454893421181));
#68942=CARTESIAN_POINT('Ctrl Pts',(-26.3441646528039,26.3207939979479,-72.2513540305335));
#68943=CARTESIAN_POINT('Ctrl Pts',(-26.261402854215,26.401844056358,-72.257218718949));
#68944=CARTESIAN_POINT('Ctrl Pts',(-26.1751289884192,26.4791623266402,-72.2630834073644));
#68945=CARTESIAN_POINT('Ctrl Pts',(-26.0889438503148,26.5564010795442,-72.2689420642863));
#68946=CARTESIAN_POINT('Ctrl Pts',(-25.9992541353705,26.6299154039258,-72.2748007212082));
#68947=CARTESIAN_POINT('Ctrl Pts',(-25.9064178045803,26.6993752995211,-72.2806593781302));
#68948=CARTESIAN_POINT('Ctrl Pts',(-25.8099552375422,26.7715483354251,-72.2867468772942));
#68949=CARTESIAN_POINT('Ctrl Pts',(-25.7100955370243,26.8393434171954,-72.2928343764584));
#68950=CARTESIAN_POINT('Ctrl Pts',(-25.6072797030729,26.9024351365369,-72.2989218756225));
#68951=CARTESIAN_POINT('Ctrl Pts',(-25.5084435428034,26.9630847762359,-72.3047737470697));
#68952=CARTESIAN_POINT('Ctrl Pts',(-25.4068762241754,27.0193881513439,-72.3106256185169));
#68953=CARTESIAN_POINT('Ctrl Pts',(-25.3029995332083,27.0711000076129,-72.3164774899641));
#68954=CARTESIAN_POINT('Ctrl Pts',(-25.1991386589906,27.1228039899936,-72.3223284703781));
#68955=CARTESIAN_POINT('Ctrl Pts',(-25.0929694815596,27.1699176594476,-72.3281794507921));
#68956=CARTESIAN_POINT('Ctrl Pts',(-24.984937692417,27.2122420851476,-72.3340304312061));
#68957=CARTESIAN_POINT('Ctrl Pts',(-24.8768961908077,27.2545703159736,-72.3398819376454));
#68958=CARTESIAN_POINT('Ctrl Pts',(-24.7669921295208,27.2921082963066,-72.3457334440847));
#68959=CARTESIAN_POINT('Ctrl Pts',(-24.6556897729954,27.324705804096,-72.3515849505239));
#68960=CARTESIAN_POINT('Ctrl Pts',(-24.5443504560599,27.357314136609,-72.3574384000854));
#68961=CARTESIAN_POINT('Ctrl Pts',(-24.4316123170939,27.3849786182353,-72.3632918496468));
#68962=CARTESIAN_POINT('Ctrl Pts',(-24.3179526224015,27.4075994918117,-72.3691452992083));
#68963=CARTESIAN_POINT('Ctrl Pts',(-24.2041636731156,27.4302460900025,-72.3750054053532));
#68964=CARTESIAN_POINT('Ctrl Pts',(-24.0894514819994,27.4478375512691,-72.3808655114981));
#68965=CARTESIAN_POINT('Ctrl Pts',(-23.9743014018211,27.4603256199809,-72.386725617643));
#68966=CARTESIAN_POINT('Ctrl Pts',(-23.8590737759236,27.4728220985546,-72.3925896701694));
#68967=CARTESIAN_POINT('Ctrl Pts',(-23.7434080853169,27.480208314969,-72.3984537226958));
#68968=CARTESIAN_POINT('Ctrl Pts',(-23.6277909203501,27.4824881297077,-72.4043177752222));
#68969=CARTESIAN_POINT('Ctrl Pts',(-23.5120033599067,27.4847713044157,-72.4101904701333));
#68970=CARTESIAN_POINT('Ctrl Pts',(-23.3962648795434,27.4819330675668,-72.4160631650445));
#68971=CARTESIAN_POINT('Ctrl Pts',(-23.2810582726591,27.4740292137828,-72.4219358599556));
#68972=CARTESIAN_POINT('Ctrl Pts',(-23.2495168844031,27.4718652882263,-72.4235436926599));
#68973=CARTESIAN_POINT('Ctrl Pts',(-23.2180153091037,27.4693219604832,-72.4251515253643));
#68974=CARTESIAN_POINT('Ctrl Pts',(-23.1865633142998,27.4664010417933,-72.4267593580686));
#68975=CARTESIAN_POINT('Ctrl Pts',(-23.0716907827328,27.4557329322979,-72.4326316664621));
#68976=CARTESIAN_POINT('Ctrl Pts',(-22.9570956039099,27.4399883256425,-72.4385039748556));
#68977=CARTESIAN_POINT('Ctrl Pts',(-22.8432624237119,27.4191870086807,-72.4443762832492));
#68978=CARTESIAN_POINT('Ctrl Pts',(-22.7295767608545,27.3984126483142,-72.4502409816707));
#68979=CARTESIAN_POINT('Ctrl Pts',(-22.6166515357721,27.3725946828935,-72.4561056800922));
#68980=CARTESIAN_POINT('Ctrl Pts',(-22.5049675148465,27.3418047512415,-72.4619703785137));
#68981=CARTESIAN_POINT('Ctrl Pts',(-22.3933983528712,27.3110464848107,-72.4678290455164));
#68982=CARTESIAN_POINT('Ctrl Pts',(-22.2830682521687,27.2753265319876,-72.4736877125191));
#68983=CARTESIAN_POINT('Ctrl Pts',(-22.1744483417286,27.2347676735918,-72.4795463795218));
#68984=CARTESIAN_POINT('Ctrl Pts',(-22.0615859437967,27.1926246631864,-72.4856338749352));
#68985=CARTESIAN_POINT('Ctrl Pts',(-21.9505705002284,27.1452571266615,-72.4917213703486));
#68986=CARTESIAN_POINT('Ctrl Pts',(-21.8419141592654,27.0928601878265,-72.497808865762));
#68987=CARTESIAN_POINT('Ctrl Pts',(-21.7374633129529,27.0424912488673,-72.5036607474122));
#68988=CARTESIAN_POINT('Ctrl Pts',(-21.635192755677,26.9874751867753,-72.5095126290623));
#68989=CARTESIAN_POINT('Ctrl Pts',(-21.5355368181626,26.9280342880617,-72.5153645107125));
#68990=CARTESIAN_POINT('Ctrl Pts',(-21.4358960542298,26.8686024398005,-72.521215501357));
#68991=CARTESIAN_POINT('Ctrl Pts',(-21.3388694734326,26.8047473061974,-72.5270664920015));
#68992=CARTESIAN_POINT('Ctrl Pts',(-21.2448653556963,26.7367363255875,-72.532917482646));
#68993=CARTESIAN_POINT('Ctrl Pts',(-21.1508527863816,26.6687192303504,-72.5387689993324));
#68994=CARTESIAN_POINT('Ctrl Pts',(-21.0598635552576,26.5965457876734,-72.5446205160188));
#68995=CARTESIAN_POINT('Ctrl Pts',(-20.972275002165,26.5205253907498,-72.5504720327052));
#68996=CARTESIAN_POINT('Ctrl Pts',(-20.884657363322,26.4444797495425,-72.5563254925194));
#68997=CARTESIAN_POINT('Ctrl Pts',(-20.8004429600238,26.364584884741,-72.5621789523336));
#68998=CARTESIAN_POINT('Ctrl Pts',(-20.7199737031995,26.2811884066232,-72.5680324121478));
#68999=CARTESIAN_POINT('Ctrl Pts',(-20.6394129369394,26.197697090241,-72.5738925285018));
#69000=CARTESIAN_POINT('Ctrl Pts',(-20.5626061051385,26.1106965101942,-72.5797526448558));
#69001=CARTESIAN_POINT('Ctrl Pts',(-20.4898561606954,26.0205689187948,-72.5856127612097));
#69002=CARTESIAN_POINT('Ctrl Pts',(-20.4170572243753,25.9303806329176,-72.5914768239323));
#69003=CARTESIAN_POINT('Ctrl Pts',(-20.3483208599742,25.8370614746095,-72.597340886655));
#69004=CARTESIAN_POINT('Ctrl Pts',(-20.2839068432094,25.7410229083692,-72.6032049493776));
#69005=CARTESIAN_POINT('Ctrl Pts',(-20.2193978949256,25.6448428032615,-72.6090776543866));
#69006=CARTESIAN_POINT('Ctrl Pts',(-20.159224221921,25.5459356432879,-72.6149503593956));
#69007=CARTESIAN_POINT('Ctrl Pts',(-20.1035998544535,25.4447377711377,-72.6208230644046));
#69008=CARTESIAN_POINT('Ctrl Pts',(-20.0883719070233,25.4170334403325,-72.6224307994176));
#69009=CARTESIAN_POINT('Ctrl Pts',(-20.0734846362955,25.389157542895,-72.6240385344305));
#69010=CARTESIAN_POINT('Ctrl Pts',(-20.0589417975363,25.3611192737694,-72.6256462694435));
#69011=CARTESIAN_POINT('Ctrl Pts',(-20.005823932946,25.2587092142599,-72.6315185377213));
#69012=CARTESIAN_POINT('Ctrl Pts',(-19.9571268640713,25.1537884528487,-72.6373908059991));
#69013=CARTESIAN_POINT('Ctrl Pts',(-19.913095915983,25.0467754191864,-72.6432630742769));
#69014=CARTESIAN_POINT('Ctrl Pts',(-19.8691220289086,24.9399010668942,-72.6491277325077));
#69015=CARTESIAN_POINT('Ctrl Pts',(-19.8298023932249,24.8309402131891,-72.6549923907386));
#69016=CARTESIAN_POINT('Ctrl Pts',(-19.7953366132564,24.720336052415,-72.6608570489695));
#69017=CARTESIAN_POINT('Ctrl Pts',(-19.7609062792614,24.6098456413412,-72.6667156757535));
#69018=CARTESIAN_POINT('Ctrl Pts',(-19.7313199940879,24.4977156770748,-72.6725743025375));
#69019=CARTESIAN_POINT('Ctrl Pts',(-19.7067291261628,24.3844088906175,-72.6784329293215));
#69020=CARTESIAN_POINT('Ctrl Pts',(-19.6811775469786,24.2666754566009,-72.6845204398005));
#69021=CARTESIAN_POINT('Ctrl Pts',(-19.6610198365035,24.1476717943016,-72.6906079502796));
#69022=CARTESIAN_POINT('Ctrl Pts',(-19.6463686755074,24.0279342640268,-72.6966954607586));
#69023=CARTESIAN_POINT('Ctrl Pts',(-19.6322847123097,23.9128321932603,-72.7025473023687));
#69024=CARTESIAN_POINT('Ctrl Pts',(-19.6232889269094,23.7970524675998,-72.7083991439788));
#69025=CARTESIAN_POINT('Ctrl Pts',(-19.6194290805156,23.6810806466566,-72.7142509855889));
#69026=CARTESIAN_POINT('Ctrl Pts',(-19.6155698217372,23.5651264810349,-72.7201019363261));
#69027=CARTESIAN_POINT('Ctrl Pts',(-19.6168449610749,23.4489806913225,-72.7259528870634));
#69028=CARTESIAN_POINT('Ctrl Pts',(-19.6232501911883,23.3331313266936,-72.7318038378006));
#69029=CARTESIAN_POINT('Ctrl Pts',(-19.6296559973681,23.2172715429345,-72.7376553147541));
#69030=CARTESIAN_POINT('Ctrl Pts',(-19.6411927886908,23.1017086500372,-72.7435067917076));
#69031=CARTESIAN_POINT('Ctrl Pts',(-19.6578042360617,22.9869273451213,-72.7493582686611));
#69032=CARTESIAN_POINT('Ctrl Pts',(-19.6744212002883,22.8721079199931,-72.7552116889584));
#69033=CARTESIAN_POINT('Ctrl Pts',(-19.6961161126017,22.7580710079023,-72.7610651092558));
#69034=CARTESIAN_POINT('Ctrl Pts',(-19.722781340422,22.6452921568815,-72.7669185295531));
#69035=CARTESIAN_POINT('Ctrl Pts',(-19.7494768944375,22.5323850431853,-72.7727786069084));
#69036=CARTESIAN_POINT('Ctrl Pts',(-19.7811539514199,22.4207392488964,-72.7786386842637));
#69037=CARTESIAN_POINT('Ctrl Pts',(-19.8176546754305,22.3108162713663,-72.784498761619));
#69038=CARTESIAN_POINT('Ctrl Pts',(-19.8541799818049,22.2008192633424,-72.7903627855961));
#69039=CARTESIAN_POINT('Ctrl Pts',(-19.8955352767182,22.0925477676481,-72.7962268095732));
#69040=CARTESIAN_POINT('Ctrl Pts',(-19.9415148085408,21.9864427461097,-72.8020908335503));
#69041=CARTESIAN_POINT('Ctrl Pts',(-19.987562109383,21.8801813368702,-72.8079635004853));
#69042=CARTESIAN_POINT('Ctrl Pts',(-20.0382470695384,21.7760931449798,-72.8138361674203));
#69043=CARTESIAN_POINT('Ctrl Pts',(-20.0933182797116,21.6745940933134,-72.8197088343552));
#69044=CARTESIAN_POINT('Ctrl Pts',(-20.1083984582723,21.6468005544015,-72.821316949843));
#69045=CARTESIAN_POINT('Ctrl Pts',(-20.1238072844074,21.6192009847867,-72.8229250653307));
#69046=CARTESIAN_POINT('Ctrl Pts',(-20.1395390479644,21.5918035198729,-72.8245331808184));
#69047=CARTESIAN_POINT('Ctrl Pts',(-20.1969863325208,21.4917568876362,-72.8304054956219));
#69048=CARTESIAN_POINT('Ctrl Pts',(-20.2589355974952,21.3940724510578,-72.8362778104255));
#69049=CARTESIAN_POINT('Ctrl Pts',(-20.3251674142848,21.299182789224,-72.8421501252291));
#69050=CARTESIAN_POINT('Ctrl Pts',(-20.3913133981876,21.2044160993093,-72.8480148298272));
#69051=CARTESIAN_POINT('Ctrl Pts',(-20.4617306626143,21.1124373173681,-72.8538795344253));
#69052=CARTESIAN_POINT('Ctrl Pts',(-20.5361542301702,21.0236539429291,-72.8597442390235));
#69053=CARTESIAN_POINT('Ctrl Pts',(-20.610501255532,20.9349618792737,-72.8656029119656));
#69054=CARTESIAN_POINT('Ctrl Pts',(-20.6888461244686,20.8494590012516,-72.8714615849077));
#69055=CARTESIAN_POINT('Ctrl Pts',(-20.7708813496616,20.7675227869136,-72.8773202578498));
#69056=CARTESIAN_POINT('Ctrl Pts',(-20.8561205961699,20.682386418293,-72.8834077509475));
#69057=CARTESIAN_POINT('Ctrl Pts',(-20.945344080629,20.6011013691313,-72.8894952440452));
#69058=CARTESIAN_POINT('Ctrl Pts',(-21.038161470082,20.5240523568597,-72.8955827371428));
#69059=CARTESIAN_POINT('Ctrl Pts',(-21.1273865193826,20.4499853963579,-72.9014346241109));
#69060=CARTESIAN_POINT('Ctrl Pts',(-21.219932106138,20.3798329604736,-72.907286511079));
#69061=CARTESIAN_POINT('Ctrl Pts',(-21.3154155334049,20.3138977008579,-72.9131383980471));
#69062=CARTESIAN_POINT('Ctrl Pts',(-21.4108844185471,20.2479724831814,-72.9189893937729));
#69063=CARTESIAN_POINT('Ctrl Pts',(-21.5092899144949,20.1862633995526,-72.9248403894987));
#69064=CARTESIAN_POINT('Ctrl Pts',(-21.6102190844596,20.1290306412563,-72.9306913852245));
#69065=CARTESIAN_POINT('Ctrl Pts',(-21.7111573244478,20.0717927397249,-72.9365429067514));
#69066=CARTESIAN_POINT('Ctrl Pts',(-21.8146193296805,20.0190321671141,-72.9423944282783));
#69067=CARTESIAN_POINT('Ctrl Pts',(-21.9201668633793,19.9709635361038,-72.9482459498052));
#69068=CARTESIAN_POINT('Ctrl Pts',(-22.025749442061,19.9228789448499,-72.9540994142148));
#69069=CARTESIAN_POINT('Ctrl Pts',(-22.133418550115,19.8794895641573,-72.9599528786243));
#69070=CARTESIAN_POINT('Ctrl Pts',(-22.2427159160716,19.8409618988634,-72.9658063430339));
#69071=CARTESIAN_POINT('Ctrl Pts',(-22.3521375674535,19.8023904225662,-72.9716664635994));
#69072=CARTESIAN_POINT('Ctrl Pts',(-22.4631907822626,19.7686918337133,-72.9775265841649));
#69073=CARTESIAN_POINT('Ctrl Pts',(-22.575401972787,19.7399828053102,-72.9833867047304));
#69074=CARTESIAN_POINT('Ctrl Pts',(-22.6876887252861,19.7112544445137,-72.9892507714467));
#69075=CARTESIAN_POINT('Ctrl Pts',(-22.8011346025448,19.6875224188809,-72.9951148381631));
#69076=CARTESIAN_POINT('Ctrl Pts',(-22.9152573927853,19.6688519889053,-73.0009789048794));
#69077=CARTESIAN_POINT('Ctrl Pts',(-23.0295483670025,19.6501540441173,-73.0068516135336));
#69078=CARTESIAN_POINT('Ctrl Pts',(-23.1445178361985,19.6365326308205,-73.0127243221878));
#69079=CARTESIAN_POINT('Ctrl Pts',(-23.2596799739163,19.6280010623636,-73.0185970308419));
#69080=CARTESIAN_POINT('Ctrl Pts',(-23.2912062586497,19.625665497379,-73.020204717959));
#69081=CARTESIAN_POINT('Ctrl Pts',(-23.3227469939116,19.6237110750981,-73.0218124050761));
#69082=CARTESIAN_POINT('Ctrl Pts',(-23.3542922566749,19.6221373894645,-73.0234200921933));
#69083=CARTESIAN_POINT('Ctrl Pts',(-23.4695169340422,19.616389223067,-73.0292924550506));
#69084=CARTESIAN_POINT('Ctrl Pts',(-23.5851877451827,19.6157056112334,-73.035164817908));
#69085=CARTESIAN_POINT('Ctrl Pts',(-23.7008221353131,19.6201357656851,-73.0410371807653));
#69086=CARTESIAN_POINT('Ctrl Pts',(-23.8163066823252,19.6245601793865,-73.0469019340079));
#69087=CARTESIAN_POINT('Ctrl Pts',(-23.9317544929248,19.6340851657604,-73.0527666872505));
#69088=CARTESIAN_POINT('Ctrl Pts',(-24.0466794920465,19.6487080589199,-73.0586314404931));
#69089=CARTESIAN_POINT('Ctrl Pts',(-24.1614863058885,19.6633159143528,-73.0644901626067));
#69090=CARTESIAN_POINT('Ctrl Pts',(-24.2757709700512,19.6830111970448,-73.0703488847202));
#69091=CARTESIAN_POINT('Ctrl Pts',(-24.3890496894398,19.707739248938,-73.0762076068337));
#69092=CARTESIAN_POINT('Ctrl Pts',(-24.5067513560378,19.7334328031665,-73.0822950816976));
#69093=CARTESIAN_POINT('Ctrl Pts',(-24.6233664689073,19.7645601250094,-73.0883825565616));
#69094=CARTESIAN_POINT('Ctrl Pts',(-24.7383603790814,19.8010007739461,-73.0944700314255));
#69095=CARTESIAN_POINT('Ctrl Pts',(-24.848904923149,19.8360314544069,-73.1003219685615));
#69096=CARTESIAN_POINT('Ctrl Pts',(-24.9579509576739,19.8759717992191,-73.1061739056974));
#69097=CARTESIAN_POINT('Ctrl Pts',(-25.0650369873523,19.9206634292066,-73.1120258428334));
#69098=CARTESIAN_POINT('Ctrl Pts',(-25.1721067131054,19.9653482548612,-73.1178768890077));
#69099=CARTESIAN_POINT('Ctrl Pts',(-25.2772166459731,20.0147827682002,-73.123727935182));
#69100=CARTESIAN_POINT('Ctrl Pts',(-25.3799246677479,20.0687601972852,-73.1295789813563));
#69101=CARTESIAN_POINT('Ctrl Pts',(-25.4826419232885,20.1227424791064,-73.1354305535576));
#69102=CARTESIAN_POINT('Ctrl Pts',(-25.5829564725298,20.1812682962628,-73.1412821257589));
#69103=CARTESIAN_POINT('Ctrl Pts',(-25.6804508678707,20.2440849544908,-73.1471336979602));
#69104=CARTESIAN_POINT('Ctrl Pts',(-25.7779776368804,20.3069224714121,-73.1529872132153));
#69105=CARTESIAN_POINT('Ctrl Pts',(-25.8726820426087,20.3740534387639,-73.1588407284705));
#69106=CARTESIAN_POINT('Ctrl Pts',(-25.9641762819582,20.445182302551,-73.1646942437256));
#69107=CARTESIAN_POINT('Ctrl Pts',(-26.0557745612392,20.5163920483933,-73.1705544151301));
#69108=CARTESIAN_POINT('Ctrl Pts',(-26.1441550616155,20.5916085106643,-73.1764145865347));
#69109=CARTESIAN_POINT('Ctrl Pts',(-26.2289636253595,20.6704963134225,-73.1822747579392));
#69110=CARTESIAN_POINT('Ctrl Pts',(-26.3138292987582,20.7494372388252,-73.1881388755533));
#69111=CARTESIAN_POINT('Ctrl Pts',(-26.3951179568315,20.8320541335458,-73.1940029931674));
#69112=CARTESIAN_POINT('Ctrl Pts',(-26.4725140343758,20.9179765754265,-73.1998671107815));
#69113=CARTESIAN_POINT('Ctrl Pts',(-26.5500241662413,21.0040256364601,-73.2057398700216));
#69114=CARTESIAN_POINT('Ctrl Pts',(-26.6236300072429,21.0933896487596,-73.2116126292616));
#69115=CARTESIAN_POINT('Ctrl Pts',(-26.6930577422606,21.1856670694119,-73.2174853885017));
#69116=CARTESIAN_POINT('Ctrl Pts',(-26.7120581132677,21.2109207411257,-73.2190925935239));
#69117=CARTESIAN_POINT('Ctrl Pts',(-26.7307458206822,21.236392462215,-73.220699798546));
#69118=CARTESIAN_POINT('Ctrl Pts',(-26.7491158468198,21.2620736726136,-73.2223070035682));
#69119=CARTESIAN_POINT('Ctrl Pts',(-26.8168479191964,21.3567627921826,-73.2282329247437));
#69120=CARTESIAN_POINT('Ctrl Pts',(-26.8804833326209,21.4546172015587,-73.2341588459192));
#69121=CARTESIAN_POINT('Ctrl Pts',(-26.9397153837474,21.5552511345641,-73.2400847670947));
#69122=CARTESIAN_POINT('Ctrl Pts',(-26.9988677778658,21.6557497320901,-73.2460027189167));
#69123=CARTESIAN_POINT('Ctrl Pts',(-27.0536283845837,21.7590200748152,-73.2519206707387));
#69124=CARTESIAN_POINT('Ctrl Pts',(-27.1037321446487,21.8646453294325,-73.2578386225608));
#69125=CARTESIAN_POINT('Ctrl Pts',(-27.1537799057791,21.970152530999,-73.2637499601288));
#69126=CARTESIAN_POINT('Ctrl Pts',(-27.1991810022792,22.0780090466331,-73.2696612976968));
#69127=CARTESIAN_POINT('Ctrl Pts',(-27.2397152263503,22.1877716970617,-73.2755726352648));
#69128=CARTESIAN_POINT('Ctrl Pts',(-27.2802088669413,22.2974244514591,-73.2814780543119));
#69129=CARTESIAN_POINT('Ctrl Pts',(-27.3158451972843,22.4089791642609,-73.287383473359));
#69130=CARTESIAN_POINT('Ctrl Pts',(-27.3464515726025,22.5219715186406,-73.2932888924061));
#69131=CARTESIAN_POINT('Ctrl Pts',(-27.3770395349175,22.6348958960523,-73.299190758713));
#69132=CARTESIAN_POINT('Ctrl Pts',(-27.4026034574628,22.7492558059355,-73.30509262502));
#69133=CARTESIAN_POINT('Ctrl Pts',(-27.423020232726,22.8645708753517,-73.3109944913269));
#69134=CARTESIAN_POINT('Ctrl Pts',(-27.4434322422425,22.9798590275683,-73.3168949800019));
#69135=CARTESIAN_POINT('Ctrl Pts',(-27.4586994176279,23.0961015000886,-73.3227954686769));
#69136=CARTESIAN_POINT('Ctrl Pts',(-27.468749644824,23.2128071666449,-73.328695957352));
#69137=CARTESIAN_POINT('Ctrl Pts',(-27.4784813882952,23.3258145232347,-73.334409464223));
#69138=CARTESIAN_POINT('Ctrl Pts',(-27.4833218019471,23.4392557983426,-73.340122971094));
#69139=CARTESIAN_POINT('Ctrl Pts',(-27.4832517822853,23.5526804628563,-73.345836477965));
#69140=CARTESIAN_POINT('Ctrl Pts',(-27.4782612161635,23.552707293754,-73.3458379866115));
#69141=CARTESIAN_POINT('Ctrl Pts',(-27.4810432214932,24.0507322526134,-73.3709566293887));
#69142=CARTESIAN_POINT('Ctrl Pts',(-27.1616604773278,25.8597480102053,-73.4623709092908));
#69143=CARTESIAN_POINT('Ctrl Pts',(-24.4392995286466,28.1164329704807,-73.620080826318));
#69144=CARTESIAN_POINT('Ctrl Pts',(-20.1891690511146,26.7665256923699,-73.8189677376927));
#69145=CARTESIAN_POINT('Ctrl Pts',(-19.0276283246582,22.4608807262844,-74.0178546490677));
#69146=CARTESIAN_POINT('Ctrl Pts',(-22.0219221388387,19.1567582508198,-74.2167415604425));
#69147=CARTESIAN_POINT('Ctrl Pts',(-26.2830391088016,19.8660492331889,-74.4094015795675));
#69148=CARTESIAN_POINT('Ctrl Pts',(-27.4805056762975,22.3695229369242,-74.5357659615675));
#69149=CARTESIAN_POINT('Ctrl Pts',(-27.4882738925428,23.5526426182486,-74.5958347064426));
#69150=CARTESIAN_POINT('Origin',(-23.5502525316942,23.5502525316942,-77.3107734492734));
#69151=CARTESIAN_POINT('',(-21.7179950055095,20.8990358449182,30.));
#69152=CARTESIAN_POINT('Ctrl Pts',(-21.7179950055095,20.8990358449182,30.));
#69153=CARTESIAN_POINT('Ctrl Pts',(-21.9298629608487,20.7526137672118,29.9831668988443));
#69154=CARTESIAN_POINT('Ctrl Pts',(-22.1585744966718,20.6320761596675,29.9653743087997));
#69155=CARTESIAN_POINT('Ctrl Pts',(-22.5126273183095,20.4967004425218,29.9400899248691));
#69156=CARTESIAN_POINT('Ctrl Pts',(-22.628353293357,20.459790786396,29.9321326957846));
#69157=CARTESIAN_POINT('Ctrl Pts',(-22.8159383538087,20.4114419441816,29.9197544699574));
#69158=CARTESIAN_POINT('Ctrl Pts',(-22.8865714104851,20.3957513134557,29.9152061722286));
#69159=CARTESIAN_POINT('Ctrl Pts',(-22.9662854811856,20.3808398517232,29.910191053069));
#69160=CARTESIAN_POINT('Ctrl Pts',(-22.9749000208742,20.3792647135659,29.9096506001298));
#69161=CARTESIAN_POINT('Ctrl Pts',(-22.9877931533489,20.3769615200717,29.9088439626519));
#69162=CARTESIAN_POINT('Ctrl Pts',(-22.9920669189485,20.3762069714118,29.908576949571));
#69163=CARTESIAN_POINT('Ctrl Pts',(-22.9993978136246,20.3749279399407,29.9081195617715));
#69164=CARTESIAN_POINT('Ctrl Pts',(-23.0024541910024,20.3743992351063,29.9079290553469));
#69165=CARTESIAN_POINT('Ctrl Pts',(-23.008730027137,20.3733229441465,29.9075382582219));
#69166=CARTESIAN_POINT('Ctrl Pts',(-23.0119495648089,20.3727758373445,29.9073379827214));
#69167=CARTESIAN_POINT('Ctrl Pts',(-23.0196698025262,20.3714759820123,29.9068582250794));
#69168=CARTESIAN_POINT('Ctrl Pts',(-23.024171289719,20.3707278954502,29.9065788885492));
#69169=CARTESIAN_POINT('Ctrl Pts',(-23.037887446517,20.3684783810228,29.90572894625));
#69170=CARTESIAN_POINT('Ctrl Pts',(-23.0471071202861,20.3670074226602,29.9051592892992));
#69171=CARTESIAN_POINT('Ctrl Pts',(-23.1489625406978,20.3512104096274,29.8988838468123));
#69172=CARTESIAN_POINT('Ctrl Pts',(-23.242180281236,20.3408915091698,29.8933059483484));
#69173=CARTESIAN_POINT('Ctrl Pts',(-23.4963027679233,20.3239376477752,29.8784264564005));
#69174=CARTESIAN_POINT('Ctrl Pts',(-23.657468210975,20.3252674899317,29.8693523304162));
#69175=CARTESIAN_POINT('Ctrl Pts',(-23.9685073654848,20.3511853595039,29.8518110266293));
#69176=CARTESIAN_POINT('Ctrl Pts',(-24.1180692247852,20.3743201719093,29.8433583321896));
#69177=CARTESIAN_POINT('Ctrl Pts',(-24.3429114255277,20.4254931187756,29.8299590348898));
#69178=CARTESIAN_POINT('Ctrl Pts',(-24.4196929418666,20.4459811791637,29.825254310171));
#69179=CARTESIAN_POINT('Ctrl Pts',(-24.5042521220368,20.471927719796,29.8198491575605));
#69180=CARTESIAN_POINT('Ctrl Pts',(-24.5128610275461,20.4746089006265,29.8192962413981));
#69181=CARTESIAN_POINT('Ctrl Pts',(-24.5277058470465,20.4793006422308,29.8183381027039));
#69182=CARTESIAN_POINT('Ctrl Pts',(-24.5339471418504,20.4812941736653,29.8179338232026));
#69183=CARTESIAN_POINT('Ctrl Pts',(-24.5427974175166,20.4841508106583,29.8173584387305));
#69184=CARTESIAN_POINT('Ctrl Pts',(-24.5454114917559,20.4849982586869,29.8171882279141));
#69185=CARTESIAN_POINT('Ctrl Pts',(-24.5497496339647,20.4864107608489,29.8169053180814));
#69186=CARTESIAN_POINT('Ctrl Pts',(-24.5514743207105,20.4869739313406,29.8167927280635));
#69187=CARTESIAN_POINT('Ctrl Pts',(-24.555053082414,20.4881458673242,29.8165588599876));
#69188=CARTESIAN_POINT('Ctrl Pts',(-24.5569070810166,20.4887548607843,29.8164375686648));
#69189=CARTESIAN_POINT('Ctrl Pts',(-24.5613881423805,20.4902312910431,29.8161440829554));
#69190=CARTESIAN_POINT('Ctrl Pts',(-24.5640146348641,20.4911004245828,29.8159717886689));
#69191=CARTESIAN_POINT('Ctrl Pts',(-24.5729614638971,20.4940738102851,29.8153839660973));
#69192=CARTESIAN_POINT('Ctrl Pts',(-24.579276341819,20.4961942589145,29.8149674966045));
#69193=CARTESIAN_POINT('Ctrl Pts',(-24.6842763549335,20.5318144373344,29.808017049784));
#69194=CARTESIAN_POINT('Ctrl Pts',(-24.7812749973739,20.5700583880627,29.8012202361129));
#69195=CARTESIAN_POINT('Ctrl Pts',(-24.9538128011945,20.6479465189471,29.788642057707));
#69196=CARTESIAN_POINT('Ctrl Pts',(-25.0299664674638,20.6860236182878,29.7829071454149));
#69197=CARTESIAN_POINT('Ctrl Pts',(-25.2441722546298,20.8039519091449,29.7663844271414));
#69198=CARTESIAN_POINT('Ctrl Pts',(-25.3779362146065,20.8910966595255,29.7555900994215));
#69199=CARTESIAN_POINT('Ctrl Pts',(-25.5816319379943,21.0464603735282,29.7386684696809));
#69200=CARTESIAN_POINT('Ctrl Pts',(-25.6558812309435,21.1085711046002,29.7323797290813));
#69201=CARTESIAN_POINT('Ctrl Pts',(-25.7738526902579,21.2166463129568,29.7221948715367));
#69202=CARTESIAN_POINT('Ctrl Pts',(-25.8192114163984,21.2607237288694,29.7182264821787));
#69203=CARTESIAN_POINT('Ctrl Pts',(-25.869111756015,21.3121550350113,29.7137950129729));
#69204=CARTESIAN_POINT('Ctrl Pts',(-25.8749532783229,21.3182231977364,29.7132751809532));
#69205=CARTESIAN_POINT('Ctrl Pts',(-25.8836989401452,21.3273797526832,29.7124952759405));
#69206=CARTESIAN_POINT('Ctrl Pts',(-25.8866208517964,21.3304510527603,29.7122344340904));
#69207=CARTESIAN_POINT('Ctrl Pts',(-25.8916383313928,21.3357459421734,29.7117860376474));
#69208=CARTESIAN_POINT('Ctrl Pts',(-25.89373680711,21.3379667569721,29.7115983578546));
#69209=CARTESIAN_POINT('Ctrl Pts',(-25.8980544223111,21.3425491217386,29.7112119042922));
#69210=CARTESIAN_POINT('Ctrl Pts',(-25.9002731648341,21.3449110416195,29.7110131477093));
#69211=CARTESIAN_POINT('Ctrl Pts',(-25.9056100235284,21.3506094917643,29.7105346666166));
#69212=CARTESIAN_POINT('Ctrl Pts',(-25.9087246241701,21.3539493179254,29.7102550927863));
#69213=CARTESIAN_POINT('Ctrl Pts',(-25.9182743178774,21.3642333153892,29.7093968596217));
#69214=CARTESIAN_POINT('Ctrl Pts',(-25.9246859591711,21.3711992750332,29.7088191998655));
#69215=CARTESIAN_POINT('Ctrl Pts',(-25.9999572425682,21.4537048346496,29.7020201299799));
#69216=CARTESIAN_POINT('Ctrl Pts',(-26.0652208138656,21.5324558916646,29.6959543552564));
#69217=CARTESIAN_POINT('Ctrl Pts',(-26.1283647047898,21.6164832940963,29.6898427359488));
#69218=CARTESIAN_POINT('Ctrl Pts',(-26.1300901657968,21.6187858291399,29.6896755296771));
#69219=CARTESIAN_POINT('Ctrl Pts',(-26.2775093540809,21.8160587953789,29.6753724565649));
#69220=CARTESIAN_POINT('Ctrl Pts',(-26.4006468986361,22.0268970767938,29.6620447908319));
#69221=CARTESIAN_POINT('Ctrl Pts',(-26.5374445743441,22.3370203294724,29.6429444056442));
#69222=CARTESIAN_POINT('Ctrl Pts',(-26.5721000086692,22.4261155195152,29.6375000200887));
#69223=CARTESIAN_POINT('Ctrl Pts',(-26.6227336822201,22.5756441265718,29.6282375515535));
#69224=CARTESIAN_POINT('Ctrl Pts',(-26.641005119485,22.6352393168289,29.6245139306103));
#69225=CARTESIAN_POINT('Ctrl Pts',(-26.6602931856184,22.7053426477049,29.6200565536783));
#69226=CARTESIAN_POINT('Ctrl Pts',(-26.6630017569354,22.7153765918689,29.6194167394031));
#69227=CARTESIAN_POINT('Ctrl Pts',(-26.6664892658084,22.7285490361741,29.6185741966033));
#69228=CARTESIAN_POINT('Ctrl Pts',(-26.6673121204535,22.7316760004533,29.6183739962105));
#69229=CARTESIAN_POINT('Ctrl Pts',(-26.668637508965,22.7367436412484,29.6180492276507));
#69230=CARTESIAN_POINT('Ctrl Pts',(-26.6691429429946,22.7386835675589,29.6179248285545));
#69231=CARTESIAN_POINT('Ctrl Pts',(-26.6701092461706,22.742406608542,29.6176859388827));
#69232=CARTESIAN_POINT('Ctrl Pts',(-26.6705703955044,22.7441896413548,29.6175714653879));
#69233=CARTESIAN_POINT('Ctrl Pts',(-26.6716269330408,22.7482892345219,29.6173081150987));
#69234=CARTESIAN_POINT('Ctrl Pts',(-26.6722212667572,22.7506060469319,29.617159177712));
#69235=CARTESIAN_POINT('Ctrl Pts',(-26.6740222972519,22.7576593793744,29.6167054219028));
#69236=CARTESIAN_POINT('Ctrl Pts',(-26.6752207909294,22.7623979567029,29.616400127919));
#69237=CARTESIAN_POINT('Ctrl Pts',(-26.6843034179204,22.7986554273766,29.6140608048123));
#69238=CARTESIAN_POINT('Ctrl Pts',(-26.6917209266959,22.830287750922,29.612000558304));
#69239=CARTESIAN_POINT('Ctrl Pts',(-26.7374078438757,23.0392898786938,29.5982856506814));
#69240=CARTESIAN_POINT('Ctrl Pts',(-26.761113384066,23.2194933337451,29.5859957193082));
#69241=CARTESIAN_POINT('Ctrl Pts',(-26.7787621559303,23.5994356026406,29.5602348194704));
#69242=CARTESIAN_POINT('Ctrl Pts',(-26.7695740247474,23.7986108341445,29.5468310377809));
#69243=CARTESIAN_POINT('Ctrl Pts',(-26.734137425529,24.0525367763684,29.5302452816274));
#69244=CARTESIAN_POINT('Ctrl Pts',(-26.7246858508568,24.1091677791813,29.5265760112754));
#69245=CARTESIAN_POINT('Ctrl Pts',(-26.7052298986207,24.2092031009733,29.5201461968322));
#69246=CARTESIAN_POINT('Ctrl Pts',(-26.6958295123921,24.2527080960775,29.5173674241366));
#69247=CARTESIAN_POINT('Ctrl Pts',(-26.6837606698719,24.3034476038151,29.5141451243775));
#69248=CARTESIAN_POINT('Ctrl Pts',(-26.6819641855773,24.3108826568239,29.5136734155555));
#69249=CARTESIAN_POINT('Ctrl Pts',(-26.6791771645141,24.3222399463337,29.5129535599061));
#69250=CARTESIAN_POINT('Ctrl Pts',(-26.6782056940745,24.3261667926946,29.5127047930568));
#69251=CARTESIAN_POINT('Ctrl Pts',(-26.6764238668061,24.3333115059672,29.5122524015377));
#69252=CARTESIAN_POINT('Ctrl Pts',(-26.6756159299215,24.3365299654396,29.5120486983328));
#69253=CARTESIAN_POINT('Ctrl Pts',(-26.6739843471008,24.3429872136368,29.5116401723345));
#69254=CARTESIAN_POINT('Ctrl Pts',(-26.6731606314016,24.346225980658,29.5114353520998));
#69255=CARTESIAN_POINT('Ctrl Pts',(-26.670810230119,24.3554077109653,29.5108549339681));
#69256=CARTESIAN_POINT('Ctrl Pts',(-26.6692716019104,24.3613476262194,29.510479726348));
#69257=CARTESIAN_POINT('Ctrl Pts',(-26.6627322324901,24.3862992559835,29.508904751374));
#69258=CARTESIAN_POINT('Ctrl Pts',(-26.6575744813119,24.405269690207,29.5077101267986));
#69259=CARTESIAN_POINT('Ctrl Pts',(-26.5464090093256,24.7998442096166,29.4829153174042));
#69260=CARTESIAN_POINT('Ctrl Pts',(-26.3732515597564,25.1530847453112,29.4622281856888));
#69261=CARTESIAN_POINT('Ctrl Pts',(-26.0938334325533,25.5308215645426,29.4352713542118));
#69262=CARTESIAN_POINT('Ctrl Pts',(-26.0441292729003,25.5930531111164,29.4306229963969));
#69263=CARTESIAN_POINT('Ctrl Pts',(-25.9715330284493,25.6773442045163,29.4239293092894));
#69264=CARTESIAN_POINT('Ctrl Pts',(-25.9505387300426,25.7010068666755,29.4220038356843));
#69265=CARTESIAN_POINT('Ctrl Pts',(-25.9261417111635,25.7277025835267,29.4197726191509));
#69266=CARTESIAN_POINT('Ctrl Pts',(-25.9230758609738,25.7310431151222,29.4194923454347));
#69267=CARTESIAN_POINT('Ctrl Pts',(-25.9184602189465,25.7360510344415,29.4190705405192));
#69268=CARTESIAN_POINT('Ctrl Pts',(-25.9169156766902,25.7377232863818,29.4189294157396));
#69269=CARTESIAN_POINT('Ctrl Pts',(-25.9141315261297,25.7407312425984,29.418675069353));
#69270=CARTESIAN_POINT('Ctrl Pts',(-25.9128925546058,25.7420675342282,29.4185618975494));
#69271=CARTESIAN_POINT('Ctrl Pts',(-25.9102477594258,25.744915227483,29.4183203454948));
#69272=CARTESIAN_POINT('Ctrl Pts',(-25.9088416153029,25.7464263312435,29.4181919402884));
#69273=CARTESIAN_POINT('Ctrl Pts',(-25.9051152991176,25.7504230866298,29.4178517174421));
#69274=CARTESIAN_POINT('Ctrl Pts',(-25.9027926512932,25.7529064104562,29.4176397087285));
#69275=CARTESIAN_POINT('Ctrl Pts',(-25.8927703168508,25.7635881339019,29.4167251378481));
#69276=CARTESIAN_POINT('Ctrl Pts',(-25.8850317935019,25.7717497411225,29.4160196231809));
#69277=CARTESIAN_POINT('Ctrl Pts',(-25.7439877023938,25.9189540435713,29.4031752896231));
#69278=CARTESIAN_POINT('Ctrl Pts',(-25.5985400038457,26.0457926234618,29.3901856923264));
#69279=CARTESIAN_POINT('Ctrl Pts',(-25.284738071636,26.2734388172624,29.3639477691765));
#69280=CARTESIAN_POINT('Ctrl Pts',(-25.1167166413429,26.3734404623235,29.3507596549073));
#69281=CARTESIAN_POINT('Ctrl Pts',(-24.8691366058195,26.4918420723846,29.3328907835062));
#69282=CARTESIAN_POINT('Ctrl Pts',(-24.7963645604632,26.5234008258716,29.3278086661774));
#69283=CARTESIAN_POINT('Ctrl Pts',(-24.6850391244419,26.5668721624575,29.3202846481387));
#69284=CARTESIAN_POINT('Ctrl Pts',(-24.6473093960438,26.5807972154086,29.3177765632291));
#69285=CARTESIAN_POINT('Ctrl Pts',(-24.6022491107101,26.5964759197372,29.3148289069903));
#69286=CARTESIAN_POINT('Ctrl Pts',(-24.5951621016848,26.5989141600452,29.3143666899971));
#69287=CARTESIAN_POINT('Ctrl Pts',(-24.5842436404484,26.602628041936,29.3136566954193));
#69288=CARTESIAN_POINT('Ctrl Pts',(-24.5804182230257,26.6039212296944,29.3134083378077));
#69289=CARTESIAN_POINT('Ctrl Pts',(-24.5734430567413,26.6062645957357,29.3129562096452));
#69290=CARTESIAN_POINT('Ctrl Pts',(-24.5702941008127,26.6073171014268,29.3127523624552));
#69291=CARTESIAN_POINT('Ctrl Pts',(-24.5639168131349,26.6094376927881,29.3123400678684));
#69292=CARTESIAN_POINT('Ctrl Pts',(-24.560688405787,26.6105055391778,29.3121316285793));
#69293=CARTESIAN_POINT('Ctrl Pts',(-24.5514601976808,26.6135417187981,29.311536609632));
#69294=CARTESIAN_POINT('Ctrl Pts',(-24.5454562705332,26.6154975387618,29.3111504424672));
#69295=CARTESIAN_POINT('Ctrl Pts',(-24.5196478806968,26.6238209758197,29.3094945332828));
#69296=CARTESIAN_POINT('Ctrl Pts',(-24.4997874516919,26.6300145014779,29.3082305186263));
#69297=CARTESIAN_POINT('Ctrl Pts',(-24.1430899814698,26.737473022109,29.2857055377371));
#69298=CARTESIAN_POINT('Ctrl Pts',(-23.7920122253475,26.7831121845741,29.2666957835297));
#69299=CARTESIAN_POINT('Ctrl Pts',(-23.3608145853837,26.7684175824128,29.2422175577395));
#69300=CARTESIAN_POINT('Ctrl Pts',(-23.2812726767628,26.7627470871028,29.2376389056326));
#69301=CARTESIAN_POINT('Ctrl Pts',(-23.145452268188,26.7479850030291,29.2295929228964));
#69302=CARTESIAN_POINT('Ctrl Pts',(-23.0890532080488,26.7403388081765,29.2261837029241));
#69303=CARTESIAN_POINT('Ctrl Pts',(-23.0231748368864,26.7296240976667,29.2220903805206));
#69304=CARTESIAN_POINT('Ctrl Pts',(-23.013466750109,26.7279994488734,29.2214843259563));
#69305=CARTESIAN_POINT('Ctrl Pts',(-23.0006365140691,26.7257918373753,29.2206794125919));
#69306=CARTESIAN_POINT('Ctrl Pts',(-22.9975074346999,26.725248674416,29.2204827965758));
#69307=CARTESIAN_POINT('Ctrl Pts',(-22.9924120988614,26.7243564370587,29.2201621162081));
#69308=CARTESIAN_POINT('Ctrl Pts',(-22.9904453454084,26.7240101570783,29.2200382115792));
#69309=CARTESIAN_POINT('Ctrl Pts',(-22.9866502114488,26.7233383225442,29.219798876431));
#69310=CARTESIAN_POINT('Ctrl Pts',(-22.9848217963528,26.7230130166587,29.2196834605371));
#69311=CARTESIAN_POINT('Ctrl Pts',(-22.9805850507495,26.7222554494987,29.2194157695822));
#69312=CARTESIAN_POINT('Ctrl Pts',(-22.9781769379555,26.7218220271269,29.2192634282119));
#69313=CARTESIAN_POINT('Ctrl Pts',(-22.9707491959713,26.7204764157812,29.2187929575582));
#69314=CARTESIAN_POINT('Ctrl Pts',(-22.9657312688389,26.7195550549269,29.2184743078043));
#69315=CARTESIAN_POINT('Ctrl Pts',(-22.9244925907579,26.7118817939853,29.2158489660614));
#69316=CARTESIAN_POINT('Ctrl Pts',(-22.888389731073,26.7045214549152,29.2135087623178));
#69317=CARTESIAN_POINT('Ctrl Pts',(-22.844730689279,26.6948381282827,29.2106343371644));
#69318=CARTESIAN_POINT('Ctrl Pts',(-22.8370447730954,26.6931038382261,29.2101266303812));
#69319=CARTESIAN_POINT('Ctrl Pts',(-22.8256244546952,26.6904828487402,29.2093698145893));
#69320=CARTESIAN_POINT('Ctrl Pts',(-22.8218850916567,26.6896176213396,29.2091216223243));
#69321=CARTESIAN_POINT('Ctrl Pts',(-22.5605843704022,26.6286649241888,29.191751648993));
#69322=CARTESIAN_POINT('Ctrl Pts',(-22.3114045873123,26.5371106962531,29.1734720195285));
#69323=CARTESIAN_POINT('Ctrl Pts',(-22.075820670606,26.4159406592144,29.1557691003147));
#69324=CARTESIAN_POINT('Ctrl Pts',(-22.0754283214049,26.4157387567432,29.1557396157498));
#69325=CARTESIAN_POINT('Ctrl Pts',(-22.0750360153802,26.4155367745738,29.1557101328919));
#69326=CARTESIAN_POINT('',(-25.421839063434,20.9266516823442,30.));
#69327=CARTESIAN_POINT('Origin',(-23.5502525316942,23.5502525316942,30.));
#69328=CARTESIAN_POINT('',(-26.7730025235471,23.5504816865032,29.8107734493065));
#69329=CARTESIAN_POINT('Ctrl Pts',(-26.7730025235471,23.5504816865032,29.8107734493065));
#69330=CARTESIAN_POINT('Ctrl Pts',(-26.7730097124841,23.4493790882664,29.8170642445203));
#69331=CARTESIAN_POINT('Ctrl Pts',(-26.7682549907641,23.3481129961194,29.8233550397341));
#69332=CARTESIAN_POINT('Ctrl Pts',(-26.7587181907666,23.2471590196342,29.8296458349478));
#69333=CARTESIAN_POINT('Ctrl Pts',(-26.7491960906962,23.1463606525867,29.8359269335934));
#69334=CARTESIAN_POINT('Ctrl Pts',(-26.7349066139694,23.0458738538775,29.8422080322391));
#69335=CARTESIAN_POINT('Ctrl Pts',(-26.7158815845527,22.9461745051131,29.8484891308848));
#69336=CARTESIAN_POINT('Ctrl Pts',(-26.6967600707826,22.8459695367783,29.8548020837646));
#69337=CARTESIAN_POINT('Ctrl Pts',(-26.6728548173153,22.7465604534429,29.8611150366444));
#69338=CARTESIAN_POINT('Ctrl Pts',(-26.6442511577937,22.6484265705495,29.8674279895242));
#69339=CARTESIAN_POINT('Ctrl Pts',(-26.6158621770808,22.5510292110741,29.873693561851));
#69340=CARTESIAN_POINT('Ctrl Pts',(-26.5828451813618,22.454888383564,29.8799591341779));
#69341=CARTESIAN_POINT('Ctrl Pts',(-26.5453347984475,22.3604627276196,29.8862247065047));
#69342=CARTESIAN_POINT('Ctrl Pts',(-26.5078496538264,22.266100604548,29.8924860631362));
#69343=CARTESIAN_POINT('Ctrl Pts',(-26.4658772891907,22.1734517418654,29.8987474197676));
#69344=CARTESIAN_POINT('Ctrl Pts',(-26.4196015840391,22.0829578856508,29.905008776399));
#69345=CARTESIAN_POINT('Ctrl Pts',(-26.3733462169056,21.9925038011844,29.911267381185));
#69346=CARTESIAN_POINT('Ctrl Pts',(-26.3227914617942,21.9042032072897,29.917525985971));
#69347=CARTESIAN_POINT('Ctrl Pts',(-26.2681682537503,21.8184754991925,29.9237845907571));
#69348=CARTESIAN_POINT('Ctrl Pts',(-26.2127361686776,21.7314783091976,29.9301358748606));
#69349=CARTESIAN_POINT('Ctrl Pts',(-26.1531143575681,21.6471312129612,29.9364871589642));
#69350=CARTESIAN_POINT('Ctrl Pts',(-26.0895909161889,21.565843770493,29.9428384430678));
#69351=CARTESIAN_POINT('Ctrl Pts',(-26.0269887177682,21.4857351918013,29.9490976182486));
#69352=CARTESIAN_POINT('Ctrl Pts',(-25.9605976006371,21.4085984170733,29.9553567934293));
#69353=CARTESIAN_POINT('Ctrl Pts',(-25.8907344422317,21.3347927624936,29.9616159686101));
#69354=CARTESIAN_POINT('Ctrl Pts',(-25.8193291428703,21.2593579413358,29.9680133071751));
#69355=CARTESIAN_POINT('Ctrl Pts',(-25.744297009417,21.1874033784249,29.9744106457401));
#69356=CARTESIAN_POINT('Ctrl Pts',(-25.6660158720703,21.1192726778039,29.980807984305));
#69357=CARTESIAN_POINT('Ctrl Pts',(-25.5877347347236,21.0511419771829,29.98720532287));
#69358=CARTESIAN_POINT('Ctrl Pts',(-25.5062049653236,20.9868354125613,29.993602661435));
#69359=CARTESIAN_POINT('Ctrl Pts',(-25.421839063434,20.9266516823442,30.));
#69360=CARTESIAN_POINT('Ctrl Pts',(-22.0750360153459,26.4155367745562,29.4036987823186));
#69361=CARTESIAN_POINT('Ctrl Pts',(-22.163538723818,26.4611031638611,29.4098802346134));
#69362=CARTESIAN_POINT('Ctrl Pts',(-22.2543048787986,26.5026426058483,29.4160616869082));
#69363=CARTESIAN_POINT('Ctrl Pts',(-22.3469329220167,26.5399246674752,29.422243139203));
#69364=CARTESIAN_POINT('Ctrl Pts',(-22.4394383465509,26.5771573760426,29.4284164086461));
#69365=CARTESIAN_POINT('Ctrl Pts',(-22.533800361804,26.6101437469483,29.4345896780891));
#69366=CARTESIAN_POINT('Ctrl Pts',(-22.6295932389525,26.6386993952793,29.4407629475322));
#69367=CARTESIAN_POINT('Ctrl Pts',(-22.7252873456082,26.6672256003411,29.4469298518165));
#69368=CARTESIAN_POINT('Ctrl Pts',(-22.8224089681871,26.6913300432624,29.4530967561009));
#69369=CARTESIAN_POINT('Ctrl Pts',(-22.9205137248114,26.7108769316516,29.4592636603853));
#69370=CARTESIAN_POINT('Ctrl Pts',(-23.0185500479327,26.7304101850031,29.4654262629123));
#69371=CARTESIAN_POINT('Ctrl Pts',(-23.1175677183753,26.7453921203669,29.4715888654392));
#69372=CARTESIAN_POINT('Ctrl Pts',(-23.2171094256828,26.755737398827,29.4777514679662));
#69373=CARTESIAN_POINT('Ctrl Pts',(-23.3166154028359,26.7660789638848,29.4839118584481));
#69374=CARTESIAN_POINT('Ctrl Pts',(-23.416644613055,26.7717871346705,29.49007224893));
#69375=CARTESIAN_POINT('Ctrl Pts',(-23.5167327130705,26.7728282071841,29.4962326394119));
#69376=CARTESIAN_POINT('Ctrl Pts',(-23.6168114130105,26.7738691819223,29.5023924513222));
#69377=CARTESIAN_POINT('Ctrl Pts',(-23.7169485590095,26.7702439254885,29.5085522632325));
#69378=CARTESIAN_POINT('Ctrl Pts',(-23.8166788722726,26.7619708517755,29.5147120751428));
#69379=CARTESIAN_POINT('Ctrl Pts',(-23.9164262500222,26.7536963624874,29.5208729410358));
#69380=CARTESIAN_POINT('Ctrl Pts',(-24.0157662254474,26.7407725118116,29.5270338069288));
#69381=CARTESIAN_POINT('Ctrl Pts',(-24.1142386955665,26.7232695769463,29.5331946728219));
#69382=CARTESIAN_POINT('Ctrl Pts',(-24.2128171516534,26.7057478036637,29.5393621696578));
#69383=CARTESIAN_POINT('Ctrl Pts',(-24.3105258111033,26.6836371806377,29.5455296664938));
#69384=CARTESIAN_POINT('Ctrl Pts',(-24.4069149246519,26.6570591087105,29.5516971633298));
#69385=CARTESIAN_POINT('Ctrl Pts',(-24.5033587057452,26.6304659629034,29.557868158091));
#69386=CARTESIAN_POINT('Ctrl Pts',(-24.5984810390793,26.5994004562953,29.5640391528522));
#69387=CARTESIAN_POINT('Ctrl Pts',(-24.6918494769263,26.5640332100344,29.5702101476134));
#69388=CARTESIAN_POINT('Ctrl Pts',(-24.7853725540406,26.5286073876082,29.5763913629387));
#69389=CARTESIAN_POINT('Ctrl Pts',(-24.8771355361964,26.4888657665696,29.5825725782641));
#69390=CARTESIAN_POINT('Ctrl Pts',(-24.9667278895851,26.4450262919366,29.5887537935894));
#69391=CARTESIAN_POINT('Ctrl Pts',(-25.0318187870004,26.4131759091958,29.593244588143));
#69392=CARTESIAN_POINT('Ctrl Pts',(-25.0957644355923,26.3791635199644,29.5977353826967));
#69393=CARTESIAN_POINT('Ctrl Pts',(-25.1584170365697,26.3430870215554,29.6022261772503));
#69394=CARTESIAN_POINT('Ctrl Pts',(-25.243559258323,26.2940605936067,29.6083289761727));
#69395=CARTESIAN_POINT('Ctrl Pts',(-25.32662678499,26.241039450202,29.6144317750951));
#69396=CARTESIAN_POINT('Ctrl Pts',(-25.4072140012169,26.1842251327681,29.6205345740176));
#69397=CARTESIAN_POINT('Ctrl Pts',(-25.4876901347248,26.127489129106,29.6266289607435));
#69398=CARTESIAN_POINT('Ctrl Pts',(-25.5656923893407,26.0669705912239,29.6327233474695));
#69399=CARTESIAN_POINT('Ctrl Pts',(-25.6408399464524,26.0029167614156,29.6388177341954));
#69400=CARTESIAN_POINT('Ctrl Pts',(-25.7159073224964,25.938931275871,29.6449056183223));
#69401=CARTESIAN_POINT('Ctrl Pts',(-25.788125716647,25.8714182800427,29.6509935024491));
#69402=CARTESIAN_POINT('Ctrl Pts',(-25.8571444259622,25.8006674602486,29.657081386576));
#69403=CARTESIAN_POINT('Ctrl Pts',(-25.9261154992051,25.7299654720134,29.6631650689018));
#69404=CARTESIAN_POINT('Ctrl Pts',(-25.9918909646655,25.6560304161728,29.6692487512276));
#69405=CARTESIAN_POINT('Ctrl Pts',(-26.054155056627,25.5791906056963,29.6753324335534));
#69406=CARTESIAN_POINT('Ctrl Pts',(-26.116397200168,25.5023778816577,29.6814139713491));
#69407=CARTESIAN_POINT('Ctrl Pts',(-26.1751301479751,25.4226627812701,29.6874955091447));
#69408=CARTESIAN_POINT('Ctrl Pts',(-26.2300774405538,25.3404078379053,29.6935770469404));
#69409=CARTESIAN_POINT('Ctrl Pts',(-26.2850208376939,25.2581587259301,29.6996581535911));
#69410=CARTESIAN_POINT('Ctrl Pts',(-26.3361788655351,25.173370498625,29.7057392602417));
#69411=CARTESIAN_POINT('Ctrl Pts',(-26.383318215777,25.0864349401901,29.7118203668923));
#69412=CARTESIAN_POINT('Ctrl Pts',(-26.4304675000564,24.9994810611572,29.7179027550612));
#69413=CARTESIAN_POINT('Ctrl Pts',(-26.4735962130561,24.9103793435768,29.7239851432301));
#69414=CARTESIAN_POINT('Ctrl Pts',(-26.5125173981894,24.8195454148493,29.730067531399));
#69415=CARTESIAN_POINT('Ctrl Pts',(-26.5514865212595,24.7285996089753,29.7361574110443));
#69416=CARTESIAN_POINT('Ctrl Pts',(-26.5862375940756,24.6359177420117,29.7422472906897));
#69417=CARTESIAN_POINT('Ctrl Pts',(-26.6166322300379,24.5419344908351,29.748337170335));
#69418=CARTESIAN_POINT('Ctrl Pts',(-26.6470459155989,24.4478923363959,29.7544308667644));
#69419=CARTESIAN_POINT('Ctrl Pts',(-26.6730976151406,24.3525476038542,29.7605245631938));
#69420=CARTESIAN_POINT('Ctrl Pts',(-26.6946997582596,24.2563468609769,29.7666182596232));
#69421=CARTESIAN_POINT('Ctrl Pts',(-26.7163432303414,24.1599620679845,29.7727236144401));
#69422=CARTESIAN_POINT('Ctrl Pts',(-26.7335200676174,24.0627184319362,29.7788289692569));
#69423=CARTESIAN_POINT('Ctrl Pts',(-26.7461943958854,23.9650695554648,29.7849343240737));
#69424=CARTESIAN_POINT('Ctrl Pts',(-26.7573897579376,23.8788153175311,29.7903272455908));
#69425=CARTESIAN_POINT('Ctrl Pts',(-26.7650728676828,23.7922451571525,29.7957201671079));
#69426=CARTESIAN_POINT('Ctrl Pts',(-26.76925281896,23.705670397728,29.801113088625));
#69427=CARTESIAN_POINT('Ctrl Pts',(-26.7717486731212,23.6539765000638,29.8043332088409));
#69428=CARTESIAN_POINT('Ctrl Pts',(-26.7729988436791,23.6022338915603,29.8075533290569));
#69429=CARTESIAN_POINT('Ctrl Pts',(-26.7730025235471,23.5504816870455,29.8107734492728));
#69430=CARTESIAN_POINT('Ctrl Pts',(-24.9806647809486,26.4319136911417,-75.413296538515));
#69431=CARTESIAN_POINT('Ctrl Pts',(-25.9409444120173,25.9552456614925,-75.3470009013901));
#69432=CARTESIAN_POINT('Ctrl Pts',(-27.3306922290377,23.9746675204515,-75.2144096271402));
#69433=CARTESIAN_POINT('Ctrl Pts',(-25.9479925434464,20.5921055094508,-75.0155227157653));
#69434=CARTESIAN_POINT('Ctrl Pts',(-22.358936684886,19.9375333945402,-74.8166358043905));
#69435=CARTESIAN_POINT('Ctrl Pts',(-19.8661618148865,22.5978429125412,-74.6177488930155));
#69436=CARTESIAN_POINT('Ctrl Pts',(-20.7579317754914,26.1359023573449,-74.4188619816407));
#69437=CARTESIAN_POINT('Ctrl Pts',(-24.2160425247577,27.2966133380363,-74.2199750702657));
#69438=CARTESIAN_POINT('Ctrl Pts',(-27.0621185490293,25.0154538166582,-74.0210881588908));
#69439=CARTESIAN_POINT('Ctrl Pts',(-26.6812093500516,21.3875186376235,-73.822201247516));
#69440=CARTESIAN_POINT('Ctrl Pts',(-23.4231517443953,19.7471537304636,-73.623314336141));
#69441=CARTESIAN_POINT('Ctrl Pts',(-20.2819231727274,21.6014076203184,-73.4244274247662));
#69442=CARTESIAN_POINT('Ctrl Pts',(-20.1439940678548,25.2465411790391,-73.2255405133912));
#69443=CARTESIAN_POINT('Ctrl Pts',(-23.1361372768816,27.3328994068108,-73.0266536020164));
#69444=CARTESIAN_POINT('Ctrl Pts',(-26.5088122156722,25.9433416994471,-72.8277666906415));
#69445=CARTESIAN_POINT('Ctrl Pts',(-27.1628243388303,22.3547295650974,-72.6288797792667));
#69446=CARTESIAN_POINT('Ctrl Pts',(-24.4971878424663,19.8647061127295,-72.4299928678917));
#69447=CARTESIAN_POINT('Ctrl Pts',(-20.9613988367147,20.7613849855078,-72.2311059565169));
#69448=CARTESIAN_POINT('Ctrl Pts',(-19.8045464785528,24.2207979213969,-72.0322190451419));
#69449=CARTESIAN_POINT('Ctrl Pts',(-22.0896806113034,27.0640358375917,-71.833332133767));
#69450=CARTESIAN_POINT('Ctrl Pts',(-25.7169563907639,26.678405164599,-71.6344452223922));
#69451=CARTESIAN_POINT('Ctrl Pts',(-27.3532150892751,23.4182672606151,-71.4355583110172));
#69452=CARTESIAN_POINT('Ctrl Pts',(-25.4948736039934,20.2794127282015,-71.2366713996424));
#69453=CARTESIAN_POINT('Ctrl Pts',(-21.8495902465907,20.1461826018379,-71.0377844882675));
#69454=CARTESIAN_POINT('Ctrl Pts',(-19.7670713279998,23.1410041509518,-70.8388975768926));
#69455=CARTESIAN_POINT('Ctrl Pts',(-21.1609751794025,26.5118902488768,-70.6400106655177));
#69456=CARTESIAN_POINT('Ctrl Pts',(-24.7504223377759,27.1612823978862,-70.4411237541428));
#69457=CARTESIAN_POINT('Ctrl Pts',(-27.2370152032886,24.4924442606275,-70.2422368427679));
#69458=CARTESIAN_POINT('Ctrl Pts',(-26.3357857588391,20.9578118113256,-70.0433499313931));
#69459=CARTESIAN_POINT('Ctrl Pts',(-22.8748874532814,19.8054125801717,-69.8444630200181));
#69460=CARTESIAN_POINT('Ctrl Pts',(-20.0345923930747,22.0942037550054,-69.6455761086433));
#69461=CARTESIAN_POINT('Ctrl Pts',(-20.4248909215382,25.7209803027169,-69.4466891972683));
#69462=CARTESIAN_POINT('Ctrl Pts',(-23.6871317827143,27.3530420763928,-69.2478022858935));
#69463=CARTESIAN_POINT('Ctrl Pts',(-26.8235922176786,25.4906626817836,-69.0489153745184));
#69464=CARTESIAN_POINT('Ctrl Pts',(-26.9521310146457,21.8452108789403,-68.8500284631438));
#69465=CARTESIAN_POINT('Ctrl Pts',(-23.9546319175192,19.7665477912599,-68.6511415517687));
#69466=CARTESIAN_POINT('Ctrl Pts',(-20.5855424505331,21.1647885547934,-68.452254640394));
#69467=CARTESIAN_POINT('Ctrl Pts',(-19.9407701821737,24.7550684590997,-68.2533677290189));
#69468=CARTESIAN_POINT('Ctrl Pts',(-22.6128061593865,27.2382246776691,-68.0544808176442));
#69469=CARTESIAN_POINT('Ctrl Pts',(-26.1462758704056,26.3324471825587,-67.8555939062692));
#69470=CARTESIAN_POINT('Ctrl Pts',(-27.2942202396304,22.8700686945109,-67.6567069948944));
#69471=CARTESIAN_POINT('Ctrl Pts',(-25.0017757213758,20.0327214827548,-67.4578200835195));
#69472=CARTESIAN_POINT('Ctrl Pts',(-21.3755044606752,20.4276870675231,-67.2589331721445));
#69473=CARTESIAN_POINT('Ctrl Pts',(-19.7476422890117,23.6920255639724,-67.0600462607698));
#69474=CARTESIAN_POINT('Ctrl Pts',(-21.6140565221925,26.826086664129,-66.8611593493947));
#69475=CARTESIAN_POINT('Ctrl Pts',(-25.2596707257554,26.94993394151,-66.6622724380199));
#69476=CARTESIAN_POINT('Ctrl Pts',(-27.334474543738,23.9497622487199,-66.4633855266449));
#69477=CARTESIAN_POINT('Ctrl Pts',(-25.9318991817683,20.5824749988213,-66.2644986152701));
#69478=CARTESIAN_POINT('Ctrl Pts',(-22.3407924787165,19.9423236755932,-66.0656117038951));
#69479=CARTESIAN_POINT('Ctrl Pts',(-19.8610770190493,22.6175530692006,-65.8667247925203));
#69480=CARTESIAN_POINT('Ctrl Pts',(-20.7714010650008,26.149854188966,-65.6678378811455));
#69481=CARTESIAN_POINT('Ctrl Pts',(-24.2352540010928,27.2933417955719,-65.4689509697706));
#69482=CARTESIAN_POINT('Ctrl Pts',(-27.0696486653545,24.9972477303081,-65.2700640583956));
#69483=CARTESIAN_POINT('Ctrl Pts',(-26.6700166783666,21.3714877624793,-65.0711771470207));
#69484=CARTESIAN_POINT('Ctrl Pts',(-23.4035859529662,19.7478278887697,-64.8722902356459));
#69485=CARTESIAN_POINT('Ctrl Pts',(-20.2719293781416,21.6182738694631,-64.6734033242709));
#69486=CARTESIAN_POINT('Ctrl Pts',(-20.1527738254655,25.264044435969,-64.4745164128962));
#69487=CARTESIAN_POINT('Ctrl Pts',(-23.1556131451224,27.3349855480378,-64.2756295015211));
#69488=CARTESIAN_POINT('Ctrl Pts',(-26.5210926011366,25.9280779105288,-64.0767425901465));
#69489=CARTESIAN_POINT('Ctrl Pts',(-27.1566219190331,22.3361503562165,-63.8778556787712));
#69490=CARTESIAN_POINT('Ctrl Pts',(-24.4782035396653,19.8598797622791,-63.6789687673967));
#69491=CARTESIAN_POINT('Ctrl Pts',(-20.947076861243,20.7747488514217,-63.4800818560215));
#69492=CARTESIAN_POINT('Ctrl Pts',(-19.8080479110658,24.2400704988293,-63.2811949446469));
#69493=CARTESIAN_POINT('Ctrl Pts',(-22.1077877206174,27.0715079213585,-63.0823080332718));
#69494=CARTESIAN_POINT('Ctrl Pts',(-25.7330303907009,26.6672101940093,-62.883421121897));
#69495=CARTESIAN_POINT('Ctrl Pts',(-27.3524852774003,23.3986926494214,-62.6845342105221));
#69496=CARTESIAN_POINT('Ctrl Pts',(-25.4780106469702,20.2694457864832,-62.4856472991471));
#69497=CARTESIAN_POINT('Ctrl Pts',(-21.8320897555359,20.1549821558538,-62.2867603877724));
#69498=CARTESIAN_POINT('Ctrl Pts',(-19.7650147792107,23.1604841291662,-62.0878734763974));
#69499=CARTESIAN_POINT('Ctrl Pts',(-21.1762523621812,26.5241502174909,-61.8889865650226));
#69500=CARTESIAN_POINT('Ctrl Pts',(-24.7689948189127,27.1550564775115,-61.6900996536476));
#69501=CARTESIAN_POINT('Ctrl Pts',(-27.2418164459961,24.4734535482986,-61.4912127422729));
#69502=CARTESIAN_POINT('Ctrl Pts',(-26.3224038288408,20.9435071593643,-61.2923258308977));
#69503=CARTESIAN_POINT('Ctrl Pts',(-22.8556192092779,19.8089387520409,-61.0934389195231));
#69504=CARTESIAN_POINT('Ctrl Pts',(-20.0271437178222,22.1123204971208,-60.8945520081478));
#69505=CARTESIAN_POINT('Ctrl Pts',(-20.436106515947,25.7370398654423,-60.6956650967734));
#69506=CARTESIAN_POINT('Ctrl Pts',(-23.7067054665031,27.3522870830397,-60.4967781853982));
#69507=CARTESIAN_POINT('Ctrl Pts',(-26.8335374349911,25.4737869073209,-60.2978912740235));
#69508=CARTESIAN_POINT('Ctrl Pts',(-26.9433089540025,21.8277217292215,-60.0990043626484));
#69509=CARTESIAN_POINT('Ctrl Pts',(-23.9351493046558,19.7645163120668,-59.9001174512737));
#69510=CARTESIAN_POINT('Ctrl Pts',(-20.5733021548222,21.1800815032499,-59.7012305398987));
#69511=CARTESIAN_POINT('Ctrl Pts',(-19.9470199975653,24.7736329122096,-59.5023436285239));
#69512=CARTESIAN_POINT('Ctrl Pts',(-22.6318030354339,27.2430014770267,-59.3034567171489));
#69513=CARTESIAN_POINT('Ctrl Pts',(-26.1605632886902,26.3190468545622,-59.1045698057741));
#69514=CARTESIAN_POINT('Ctrl Pts',(-27.2906692741222,22.8508050044276,-58.9056828943991));
#69515=CARTESIAN_POINT('Ctrl Pts',(-24.9836494083045,20.0252961284803,-58.7067959830244));
#69516=CARTESIAN_POINT('Ctrl Pts',(-21.3594593448955,20.4389233200691,-58.5079090716493));
#69517=CARTESIAN_POINT('Ctrl Pts',(-19.7484224715237,23.7115982599265,-58.3090221602746));
#69518=CARTESIAN_POINT('Ctrl Pts',(-21.6309450814161,26.8360101554002,-58.1101352488995));
#69519=CARTESIAN_POINT('Ctrl Pts',(-25.277148507678,26.9410893809935,-57.9112483375248));
#69520=CARTESIAN_POINT('Ctrl Pts',(-27.3364809486441,23.9302770376352,-57.7123614261497));
#69521=CARTESIAN_POINT('Ctrl Pts',(-25.9165904936644,20.5702543940817,-57.513474514775));
#69522=CARTESIAN_POINT('Ctrl Pts',(-22.3222360840073,19.9485973768181,-57.3145876034));
#69523=CARTESIAN_POINT('Ctrl Pts',(-19.8563246711497,22.6365560768863,-57.1157006920252));
#69524=CARTESIAN_POINT('Ctrl Pts',(-20.7848197686979,26.1641243502388,-56.9168137806502));
#69525=CARTESIAN_POINT('Ctrl Pts',(-24.2545131054074,27.2897660421322,-56.7179268692754));
#69526=CARTESIAN_POINT('Ctrl Pts',(-27.0770506863242,24.9791118763931,-56.5190399579004));
#69527=CARTESIAN_POINT('Ctrl Pts',(-26.6587597863081,21.3554571201701,-56.3201530465256));
#69528=CARTESIAN_POINT('Ctrl Pts',(-23.3840142772543,19.7486332591741,-56.1212661351506));
#69529=CARTESIAN_POINT('Ctrl Pts',(-20.2620276293511,21.6351751854637,-55.9223792237759));
#69530=CARTESIAN_POINT('Ctrl Pts',(-20.161640871205,25.2815108211564,-55.7234923124009));
#69531=CARTESIAN_POINT('Ctrl Pts',(-23.1751009221589,27.3369668753301,-55.5246054010261));
#69532=CARTESIAN_POINT('Ctrl Pts',(-26.5332934946646,25.9127535081333,-55.3257184896511));
#69533=CARTESIAN_POINT('Ctrl Pts',(-27.1503243423656,22.3176020506395,-55.1268315782763));
#69534=CARTESIAN_POINT('Ctrl Pts',(-24.4591944318132,19.8551518737089,-54.9279446669013));
#69535=CARTESIAN_POINT('Ctrl Pts',(-20.932823980616,20.7881859085956,-54.7290577555265));
#69536=CARTESIAN_POINT('Ctrl Pts',(-19.8116484465149,24.259324985479,-54.5301708441516));
#69537=CARTESIAN_POINT('Ctrl Pts',(-22.1259330853401,27.0788865967642,-54.3312839327767));
#69538=CARTESIAN_POINT('Ctrl Pts',(-25.7490465329901,26.6559326810817,-54.1323970214018));
#69539=CARTESIAN_POINT('Ctrl Pts',(-27.3516547204373,23.3791220263656,-53.9335101100269));
#69540=CARTESIAN_POINT('Ctrl Pts',(-25.4610966021844,20.2595657965723,-53.7346231986521));
#69541=CARTESIAN_POINT('Ctrl Pts',(-21.8146347960108,20.1638716721309,-53.5357362872771));
#69542=CARTESIAN_POINT('Ctrl Pts',(-19.7630585328137,23.1799744398794,-53.3368493759022));
#69543=CARTESIAN_POINT('Ctrl Pts',(-21.1915924534886,26.5363313796006,-53.1379624645274));
#69544=CARTESIAN_POINT('Ctrl Pts',(-24.7875350046384,27.1487350358311,-52.9390755531523));
#69545=CARTESIAN_POINT('Ctrl Pts',(-27.2465198674066,24.4544383717626,-52.7401886417776));
#69546=CARTESIAN_POINT('Ctrl Pts',(-26.3089484404444,20.9292715829881,-52.5413017304026));
#69547=CARTESIAN_POINT('Ctrl Pts',(-22.836369372182,19.8125640635364,-52.3424148190278));
#69548=CARTESIAN_POINT('Ctrl Pts',(-20.0197884002008,22.1304753425994,-52.1435279076528));
#69549=CARTESIAN_POINT('Ctrl Pts',(-20.4474046310663,25.7530414811861,-51.944640996278));
#69550=CARTESIAN_POINT('Ctrl Pts',(-23.7262750044905,27.3514313408934,-51.7457540849031));
#69551=CARTESIAN_POINT('Ctrl Pts',(-26.8433956496595,25.456860161762,-51.5468671735283));
#69552=CARTESIAN_POINT('Ctrl Pts',(-26.9343969819104,21.8102782242672,-51.3479802621533));
#69553=CARTESIAN_POINT('Ctrl Pts',(-23.9156564925452,19.7625851498047,-51.1490933507783));
#69554=CARTESIAN_POINT('Ctrl Pts',(-20.5611407443049,21.1954372580634,-50.9502064394036));
#69555=CARTESIAN_POINT('Ctrl Pts',(-19.953365293789,24.7921649473783,-50.7513195280286));
#69556=CARTESIAN_POINT('Ctrl Pts',(-22.6508242491617,27.2476804234881,-50.5524326166538));
#69557=CARTESIAN_POINT('Ctrl Pts',(-26.1747815372389,26.3055731572274,-50.3535457052789));
#69558=CARTESIAN_POINT('Ctrl Pts',(-27.2870191925844,22.8315598487661,-50.154658793904));
#69559=CARTESIAN_POINT('Ctrl Pts',(-24.9654851121375,20.017964180825,-49.955771882529));
#69560=CARTESIAN_POINT('Ctrl Pts',(-21.3434722821983,20.4502420186684,-49.7568849711542));
#69561=CARTESIAN_POINT('Ctrl Pts',(-19.7493033974357,23.7311666804351,-49.5579980597793));
#69562=CARTESIAN_POINT('Ctrl Pts',(-21.6478844997144,26.8458465784991,-49.3591111484045));
#69563=CARTESIAN_POINT('Ctrl Pts',(-25.2945805291721,26.932154967846,-49.1602242370294));
#69564=CARTESIAN_POINT('Ctrl Pts',(-27.3383870235728,23.9107817564105,-48.9613373256547));
#69565=CARTESIAN_POINT('Ctrl Pts',(-25.9012191007766,20.5581127552981,-48.7624504142797));
#69566=CARTESIAN_POINT('Ctrl Pts',(-22.3037122300878,19.9549665170764,-48.5635635029049));
#69567=CARTESIAN_POINT('Ctrl Pts',(-19.8516702073867,22.6555832963033,-48.36467659153));
#69568=CARTESIAN_POINT('Ctrl Pts',(-20.7983117526562,26.1783252474125,-48.1657896801551));
#69569=CARTESIAN_POINT('Ctrl Pts',(-24.2737535477609,27.2860911965973,-47.9669027687802));
#69570=CARTESIAN_POINT('Ctrl Pts',(-27.0843592518706,24.9609381596209,-47.7680158574053));
#69571=CARTESIAN_POINT('Ctrl Pts',(-26.6474205229744,21.339484636997,-47.5691289460303));
#69572=CARTESIAN_POINT('Ctrl Pts',(-23.3644470066332,19.7495393673931,-47.3702420346555));
#69573=CARTESIAN_POINT('Ctrl Pts',(-20.2522130141123,21.6521272484466,-47.1713551232806));
#69574=CARTESIAN_POINT('Ctrl Pts',(-20.1705977106109,25.29893133032,-46.9724682119057));
#69575=CARTESIAN_POINT('Ctrl Pts',(-23.1945986402101,27.3388478597686,-46.7735813005308));
#69576=CARTESIAN_POINT('Ctrl Pts',(-26.545415341606,25.8973665026288,-46.5746943891558));
#69577=CARTESIAN_POINT('Ctrl Pts',(-27.143931368621,22.2990864086478,-46.3758074777811));
#69578=CARTESIAN_POINT('Ctrl Pts',(-24.4401612382193,19.8505219003528,-46.1769205664061));
#69579=CARTESIAN_POINT('Ctrl Pts',(-20.9186404583367,20.8016961568323,-45.9780336550313));
#69580=CARTESIAN_POINT('Ctrl Pts',(-19.8153480499607,24.2785606826592,-45.7791467436562));
#69581=CARTESIAN_POINT('Ctrl Pts',(-22.1441161926188,27.0861717680974,-45.5802598322816));
#69582=CARTESIAN_POINT('Ctrl Pts',(-25.765004410186,26.6445728717935,-45.3813729209065));
#69583=CARTESIAN_POINT('Ctrl Pts',(-27.3507234314122,23.3595559380386,-45.1824860095318));
#69584=CARTESIAN_POINT('Ctrl Pts',(-25.444131922592,20.2497730054484,-44.9835990981568));
#69585=CARTESIAN_POINT('Ctrl Pts',(-21.7972258280291,20.1728509229612,-44.7847121867819));
#69586=CARTESIAN_POINT('Ctrl Pts',(-19.7612026419805,23.1994745624656,-44.585825275407));
#69587=CARTESIAN_POINT('Ctrl Pts',(-21.2069950461263,26.5484334146239,-44.3869383640322));
#69588=CARTESIAN_POINT('Ctrl Pts',(-24.8060424040373,27.1423182391883,-44.1880514526573));
#69589=CARTESIAN_POINT('Ctrl Pts',(-27.2511253426879,24.4353992355138,-43.9891645412823));
#69590=CARTESIAN_POINT('Ctrl Pts',(-26.2954199503044,20.9151054590935,-43.7902776299075));
#69591=CARTESIAN_POINT('Ctrl Pts',(-22.8171384520326,19.8162884187658,-43.5913907185326));
#69592=CARTESIAN_POINT('Ctrl Pts',(-20.0125266351462,22.1486678102704,-43.3925038071577));
#69593=CARTESIAN_POINT('Ctrl Pts',(-20.4587849674954,25.7689847259758,-43.1936168957828));
#69594=CARTESIAN_POINT('Ctrl Pts',(-23.7458398781184,27.3504748726044,-42.9947299844079));
#69595=CARTESIAN_POINT('Ctrl Pts',(-26.8531666004498,25.4398828936568,-42.795843073033));
#69596=CARTESIAN_POINT('Ctrl Pts',(-26.9253953345269,21.7928808262996,-42.5969561616581));
#69597=CARTESIAN_POINT('Ctrl Pts',(-23.8961539977194,19.7607543556508,-42.3980692502833));
#69598=CARTESIAN_POINT('Ctrl Pts',(-20.5490585412428,21.2108554123249,-42.1991823389084));
#69599=CARTESIAN_POINT('Ctrl Pts',(-19.9598059027029,24.8106640735329,-42.0002954275335));
#69600=CARTESIAN_POINT('Ctrl Pts',(-22.6698692965332,27.2522613930669,-41.8014085161585));
#69601=CARTESIAN_POINT('Ctrl Pts',(-26.1889302392874,26.2920264475898,-41.6025216047838));
#69602=CARTESIAN_POINT('Ctrl Pts',(-27.2832700917394,22.8123337374975,-41.4036346934087));
#69603=CARTESIAN_POINT('Ctrl Pts',(-24.9472833142043,20.0107258340757,-41.204747782034));
#69604=CARTESIAN_POINT('Ctrl Pts',(-21.3275436962196,20.4616428633906,-41.0058608706589));
#69605=CARTESIAN_POINT('Ctrl Pts',(-19.7502850434045,23.7507303069612,-40.8069739592842));
#69606=CARTESIAN_POINT('Ctrl Pts',(-21.6648743282153,26.8555956727737,-40.6080870479092));
#69607=CARTESIAN_POINT('Ctrl Pts',(-25.3119663283127,26.9231309388175,-40.4092001365344));
#69608=CARTESIAN_POINT('Ctrl Pts',(-27.3401927180156,23.8912769216447,-40.2103132251595));
#69609=CARTESIAN_POINT('Ctrl Pts',(-25.8857854104263,20.5460504042074,-40.0114263137845));
#69610=CARTESIAN_POINT('Ctrl Pts',(-22.2852214078152,19.9614309275945,-39.8125394024097));
#69611=CARTESIAN_POINT('Ctrl Pts',(-19.8471137510971,22.6746342232557,-39.6136524910347));
#69612=CARTESIAN_POINT('Ctrl Pts',(-20.8118766593559,26.1924565041821,-39.4147655796599));
#69613=CARTESIAN_POINT('Ctrl Pts',(-24.2929748183074,27.2823173563459,-39.215878668285));
#69614=CARTESIAN_POINT('Ctrl Pts',(-27.0915741683264,24.9427270615707,-39.01699175691));
#69615=CARTESIAN_POINT('Ctrl Pts',(-26.635999188841,21.3235707362095,-38.8181048455351));
#69616=CARTESIAN_POINT('Ctrl Pts',(-23.3448846596095,19.7505461894159,-38.6192179341603));
#69617=CARTESIAN_POINT('Ctrl Pts',(-20.2424857924997,21.6691296092051,-38.4203310227854));
#69618=CARTESIAN_POINT('Ctrl Pts',(-20.179644106339,25.3163055018397,-38.2214441114106));
#69619=CARTESIAN_POINT('Ctrl Pts',(-23.2141057826128,27.3406284515096,-38.0225572000355));
#69620=CARTESIAN_POINT('Ctrl Pts',(-26.5574578207479,25.8819173017506,-37.8236702886608));
#69621=CARTESIAN_POINT('Ctrl Pts',(-27.1374431672049,22.2806039208811,-37.6247833772859));
#69622=CARTESIAN_POINT('Ctrl Pts',(-24.4211044632376,19.8459899648987,-37.425896465911));
#69623=CARTESIAN_POINT('Ctrl Pts',(-20.9045266702496,20.8152792381283,-37.227009554536));
#69624=CARTESIAN_POINT('Ctrl Pts',(-19.8191466233683,24.2977770806498,-37.0281226431611));
#69625=CARTESIAN_POINT('Ctrl Pts',(-22.1623365606255,27.0933632423109,-36.8292357317863));
#69626=CARTESIAN_POINT('Ctrl Pts',(-25.7809035994259,26.6331310671643,-36.6303488204115));
#69627=CARTESIAN_POINT('Ctrl Pts',(-27.349691435003,23.3399949029159,-36.4314619090365));
#69628=CARTESIAN_POINT('Ctrl Pts',(-25.4271170577346,20.2400676726077,-36.2325749976617));
#69629=CARTESIAN_POINT('Ctrl Pts',(-21.7798633129051,20.1819196704065,-36.0336880862867));
#69630=CARTESIAN_POINT('Ctrl Pts',(-19.7594471558902,23.2189839801978,-35.8348011749118));
#69631=CARTESIAN_POINT('Ctrl Pts',(-21.222459731946,26.5604560018729,-35.635914263537));
#69632=CARTESIAN_POINT('Ctrl Pts',(-24.8245165266878,27.1358062576196,-35.4370273521619));
#69633=CARTESIAN_POINT('Ctrl Pts',(-27.2556327498007,24.416336644064,-35.2381404407871));
#69634=CARTESIAN_POINT('Ctrl Pts',(-26.2818187169079,20.9010091630639,-35.0392535294122));
#69635=CARTESIAN_POINT('Ctrl Pts',(-22.7979269584237,19.8201117190387,-34.8403666180374));
#69636=CARTESIAN_POINT('Ctrl Pts',(-20.0053586150854,22.1668974180574,-34.6414797066625));
#69637=CARTESIAN_POINT('Ctrl Pts',(-20.4702472236707,25.7848691773366,-34.4425927952876));
#69638=CARTESIAN_POINT('Ctrl Pts',(-23.7653995689437,27.3494177035177,-34.2437058839126));
#69639=CARTESIAN_POINT('Ctrl Pts',(-26.8628500284451,25.4228555528801,-34.0448189725379));
#69640=CARTESIAN_POINT('Ctrl Pts',(-26.9163042503836,21.7755299963262,-33.8459320611629));
#69641=CARTESIAN_POINT('Ctrl Pts',(-23.8766423369686,19.7590239781184,-33.647045149788));
#69642=CARTESIAN_POINT('Ctrl Pts',(-20.5370558657983,21.226335557474,-33.4481582384131));
#69643=CARTESIAN_POINT('Ctrl Pts',(-19.9663416536393,24.8291298004711,-33.2492713270383));
#69644=CARTESIAN_POINT('Ctrl Pts',(-22.6889376728801,27.2567442643736,-33.0503844156634));
#69645=CARTESIAN_POINT('Ctrl Pts',(-26.2030090199139,26.2784070846188,-32.8514975042885));
#69646=CARTESIAN_POINT('Ctrl Pts',(-27.2794220709334,22.7931271800876,-32.6526105929135));
#69647=CARTESIAN_POINT('Ctrl Pts',(-24.9290444968282,20.003581280039,-32.4537236815387));
#69648=CARTESIAN_POINT('Ctrl Pts',(-21.3116740090453,20.4731255521286,-32.2548367701638));
#69649=CARTESIAN_POINT('Ctrl Pts',(-19.7513673834177,23.770288621095,-32.055949858789));
#69650=CARTESIAN_POINT('Ctrl Pts',(-21.6819141167111,26.8652571798861,-31.857062947414));
#69651=CARTESIAN_POINT('Ctrl Pts',(-25.3293054443993,26.9140175330327,-31.6581760360392));
#69652=CARTESIAN_POINT('Ctrl Pts',(-27.341897984124,23.8717630501896,-31.4592891246643));
#69653=CARTESIAN_POINT('Ctrl Pts',(-25.8702898315857,20.5340676604459,-31.2604022132894));
#69654=CARTESIAN_POINT('Ctrl Pts',(-22.2667641071716,19.9679904370741,-31.0615153019145));
#69655=CARTESIAN_POINT('Ctrl Pts',(-19.842655423021,22.6937083529194,-30.8626283905396));
#69656=CARTESIAN_POINT('Ctrl Pts',(-20.8255141293454,26.2065177460884,-30.6637414791646));
#69657=CARTESIAN_POINT('Ctrl Pts',(-24.3121764077089,27.2784446213798,-30.4648545677898));
#69658=CARTESIAN_POINT('Ctrl Pts',(-27.0986952445063,24.924479064812,-30.2659676564149));
#69659=CARTESIAN_POINT('Ctrl Pts',(-26.6244960865576,21.3077158395049,-30.06708074504));
#69660=CARTESIAN_POINT('Ctrl Pts',(-23.325327754559,19.751653698563,-29.8681938336652));
#69661=CARTESIAN_POINT('Ctrl Pts',(-20.2328462222715,21.6861818171993,-29.6693069222903));
#69662=CARTESIAN_POINT('Ctrl Pts',(-20.188779818672,25.3336328753231,-29.4704200109154));
#69663=CARTESIAN_POINT('Ctrl Pts',(-23.2336218324535,27.34230860337,-29.2715330995405));
#69664=CARTESIAN_POINT('Ctrl Pts',(-26.5694206129811,25.8664063148816,-29.0726461881655));
#69665=CARTESIAN_POINT('Ctrl Pts',(-27.1308599100455,22.2621550771006,-28.8737592767907));
#69666=CARTESIAN_POINT('Ctrl Pts',(-24.4020246118471,19.841556187437,-28.6748723654158));
#69667=CARTESIAN_POINT('Ctrl Pts',(-20.8904829903512,20.8289347925503,-28.4759854540409));
#69668=CARTESIAN_POINT('Ctrl Pts',(-19.8230440660809,24.3169736702418,-28.2770985426659));
#69669=CARTESIAN_POINT('Ctrl Pts',(-22.1805937065447,27.1004608288402,-28.0782116312911));
#69670=CARTESIAN_POINT('Ctrl Pts',(-25.796743679403,26.6216075703866,-27.8793247199162));
#69671=CARTESIAN_POINT('Ctrl Pts',(-27.348558758556,23.3204394393384,-27.6804378085414));
#69672=CARTESIAN_POINT('Ctrl Pts',(-25.4100524584835,20.2304500552283,-27.4815508971664));
#69673=CARTESIAN_POINT('Ctrl Pts',(-21.7625477107219,20.1910776741573,-27.2826639857916));
#69674=CARTESIAN_POINT('Ctrl Pts',(-19.7577921210606,23.2385021761025,-27.0837770744166));
#69675=CARTESIAN_POINT('Ctrl Pts',(-21.2379861011544,26.5723988227651,-26.8848901630418));
#69676=CARTESIAN_POINT('Ctrl Pts',(-24.8429568830509,27.1291992636838,-26.6860032516668));
#69677=CARTESIAN_POINT('Ctrl Pts',(-27.2600419693051,24.3972511025463,-26.4871163402919));
#69678=CARTESIAN_POINT('Ctrl Pts',(-26.2681451006692,20.8869830684321,-26.288229428917));
#69679=CARTESIAN_POINT('Ctrl Pts',(-22.7787354004341,19.8240338630426,-26.0893425175421));
#69680=CARTESIAN_POINT('Ctrl Pts',(-19.9982845299614,22.1851636829005,-25.8904556061674));
#69681=CARTESIAN_POINT('Ctrl Pts',(-20.4817910958577,25.8006944143518,-25.6915686947925));
#69682=CARTESIAN_POINT('Ctrl Pts',(-23.784953558661,27.348259861647,-25.4926817834176));
#69683=CARTESIAN_POINT('Ctrl Pts',(-26.8724456770472,25.4057785906337,-25.2937948720426));
#69684=CARTESIAN_POINT('Ctrl Pts',(-26.9071239703822,21.7582261941211,-25.0949079606678));
#69685=CARTESIAN_POINT('Ctrl Pts',(-23.8571220273254,19.7573940630605,-24.8960210492929));
#69686=CARTESIAN_POINT('Ctrl Pts',(-20.5251330360261,21.2418772833075,-24.6971341379179));
#69687=CARTESIAN_POINT('Ctrl Pts',(-19.9729723734095,24.8475616388761,-24.498247226543));
#69688=CARTESIAN_POINT('Ctrl Pts',(-22.708028872916,27.2611289186181,-24.2993603151682));
#69689=CARTESIAN_POINT('Ctrl Pts',(-26.2170175060494,26.2647154292095,-24.1004734037934));
#69690=CARTESIAN_POINT('Ctrl Pts',(-27.2754752321336,22.7739406854847,-23.9015864924183));
#69691=CARTESIAN_POINT('Ctrl Pts',(-24.9107691433134,19.9965307080362,-23.7026995810436));
#69692=CARTESIAN_POINT('Ctrl Pts',(-21.2958636412011,20.4846897806064,-23.5038126696685));
#69693=CARTESIAN_POINT('Ctrl Pts',(-19.7525503887947,23.7898411045674,-23.3049257582937));
#69694=CARTESIAN_POINT('Ctrl Pts',(-21.6990034136701,26.8748308438189,-23.1060388469188));
#69695=CARTESIAN_POINT('Ctrl Pts',(-25.3465974179686,26.9048149919848,-22.9071519355439));
#69696=CARTESIAN_POINT('Ctrl Pts',(-27.3435027767108,23.8522406591371,-22.7082650241691));
#69697=CARTESIAN_POINT('Ctrl Pts',(-25.8547327748668,20.5221648415401,-22.5093781127942));
#69698=CARTESIAN_POINT('Ctrl Pts',(-22.2483408172507,19.9746448716971,-22.3104912014193));
#69699=CARTESIAN_POINT('Ctrl Pts',(-19.838295341298,22.7128051798555,-22.1116042900445));
#69700=CARTESIAN_POINT('Ctrl Pts',(-20.8392238012498,26.2205086005273,-21.9127173786694));
#69701=CARTESIAN_POINT('Ctrl Pts',(-24.3313578071489,27.274473094321,-21.7138304672947));
#69702=CARTESIAN_POINT('Ctrl Pts',(-27.1057222917111,24.9061946528926,-21.5149435559197));
#69703=CARTESIAN_POINT('Ctrl Pts',(-26.6129115209411,21.2919203670162,-21.3160566445449));
#69704=CARTESIAN_POINT('Ctrl Pts',(-23.3057768097138,19.752861865487,-21.1171697331699));
#69705=CARTESIAN_POINT('Ctrl Pts',(-20.2232945588633,21.7032834205684,-20.918282821795));
#69706=CARTESIAN_POINT('Ctrl Pts',(-20.1980046055256,25.350912991618,-20.7193959104201));
#69707=CARTESIAN_POINT('Ctrl Pts',(-23.2531462725832,27.3438882708278,-20.5205089990453));
#69708=CARTESIAN_POINT('Ctrl Pts',(-26.5813034013074,25.8508339530424,-20.3216220876704));
#69709=CARTESIAN_POINT('Ctrl Pts',(-27.1241817715908,22.243740366176,-20.1227351762954));
#69710=CARTESIAN_POINT('Ctrl Pts',(-24.3829221896386,19.8372206854567,-19.9238482649207));
#69711=CARTESIAN_POINT('Ctrl Pts',(-20.8765097907801,20.8426624582443,-19.7249613535456));
#69712=CARTESIAN_POINT('Ctrl Pts',(-19.8270402748213,24.3361499427514,-19.5260744421708));
#69713=CARTESIAN_POINT('Ctrl Pts',(-22.1988871465868,27.107464339609,-19.3271875307959));
#69714=CARTESIAN_POINT('Ctrl Pts',(-25.8125242303759,26.6100026868178,-19.128300619421));
#69715=CARTESIAN_POINT('Ctrl Pts',(-27.3473254320858,23.3008900655,-18.9294137080461));
#69716=CARTESIAN_POINT('Ctrl Pts',(-25.3929385770275,20.2209204081642,-18.7305267966713));
#69717=CARTESIAN_POINT('Ctrl Pts',(-21.7452794803202,20.2003246915387,-18.5316398852963));
#69718=CARTESIAN_POINT('Ctrl Pts',(-19.7562375813478,23.2580286329736,-18.3327529739214));
#69719=CARTESIAN_POINT('Ctrl Pts',(-21.2535737423235,26.5842615608319,-18.1338660625466));
#69720=CARTESIAN_POINT('Ctrl Pts',(-24.8613629844814,27.1224974324572,-17.9349791511717));
#69721=CARTESIAN_POINT('Ctrl Pts',(-27.2643528843624,24.378143116702,-17.7360922397967));
#69722=CARTESIAN_POINT('Ctrl Pts',(-26.2543994639211,20.8730275468708,-17.537205328422));
#69723=CARTESIAN_POINT('Ctrl Pts',(-22.7595642866141,19.8280547468462,-17.3383184170471));
#69724=CARTESIAN_POINT('Ctrl Pts',(-19.9913045672277,22.203466120768,-17.1394315056721));
#69725=CARTESIAN_POINT('Ctrl Pts',(-20.4934162781595,25.8164600176741,-16.9405445942973));
#69726=CARTESIAN_POINT('Ctrl Pts',(-23.8045013291156,27.3470013776734,-16.7416576829224));
#69727=CARTESIAN_POINT('Ctrl Pts',(-26.8819532919847,25.3886524594344,-16.5427707715474));
#69728=CARTESIAN_POINT('Ctrl Pts',(-26.8978547377877,21.7409698782115,-16.3438838601725));
#69729=CARTESIAN_POINT('Ctrl Pts',(-23.8375935860521,19.7558646536676,-16.1449969487976));
#69730=CARTESIAN_POINT('Ctrl Pts',(-20.5132903678653,21.2574801779906,-15.9461100374227));
#69731=CARTESIAN_POINT('Ctrl Pts',(-19.9796978863084,24.865959100329,-15.7472231260478));
#69732=CARTESIAN_POINT('Ctrl Pts',(-22.7271423907501,27.2654152396129,-15.5483362146729));
#69733=CARTESIAN_POINT('Ctrl Pts',(-26.2309553264881,26.2509518441721,-15.3494493032982));
#69734=CARTESIAN_POINT('Ctrl Pts',(-27.2714296799262,22.754774762105,-15.1505623919233));
#69735=CARTESIAN_POINT('Ctrl Pts',(-24.8924577379321,19.9895743048977,-14.9516754805484));
#69736=CARTESIAN_POINT('Ctrl Pts',(-21.2801130116403,20.4963352423877,-14.7527885691735));
#69737=CARTESIAN_POINT('Ctrl Pts',(-19.7538340281876,23.8093872392638,-14.5539016577985));
#69738=CARTESIAN_POINT('Ctrl Pts',(-21.7161417662494,26.8843164108834,-14.3550147464236));
#69739=CARTESIAN_POINT('Ctrl Pts',(-25.3638417908065,26.8955235595285,-14.1561278350487));
#69740=CARTESIAN_POINT('Ctrl Pts',(-27.3450070532511,23.8327102658038,-13.9572409236738));
#69741=CARTESIAN_POINT('Ctrl Pts',(-25.8391146525105,20.5103422628989,-13.758354012299));
#69742=CARTESIAN_POINT('Ctrl Pts',(-22.2299520262449,19.9813940551297,-13.559467100924));
#69743=CARTESIAN_POINT('Ctrl Pts',(-19.8340336214646,22.7319241980239,-13.3605801895492));
#69744=CARTESIAN_POINT('Ctrl Pts',(-20.8530053117815,26.2344286967601,-13.1616932781742));
#69745=CARTESIAN_POINT('Ctrl Pts',(-24.3505185083463,27.2704028804096,-12.9628063667995));
#69746=CARTESIAN_POINT('Ctrl Pts',(-27.1126551237336,24.8878743103246,-12.7639194554245));
#69747=CARTESIAN_POINT('Ctrl Pts',(-26.6012457989672,21.2761847373024,-12.5650325440497));
#69748=CARTESIAN_POINT('Ctrl Pts',(-23.2862323431474,19.7541706581732,-12.3661456326747));
#69749=CARTESIAN_POINT('Ctrl Pts',(-20.2138310553815,21.7204339661432,-12.1672587212998));
#69750=CARTESIAN_POINT('Ctrl Pts',(-20.2073182224554,25.3681453928246,-11.9683718099249));
#69751=CARTESIAN_POINT('Ctrl Pts',(-23.2726785856307,27.345367412024,-11.76948489855));
#69752=CARTESIAN_POINT('Ctrl Pts',(-26.5931058708488,25.8352006288795,-11.5705979871751));
#69753=CARTESIAN_POINT('Ctrl Pts',(-27.1174089288021,22.2253602760722,-11.3717110758003));
#69754=CARTESIAN_POINT('Ctrl Pts',(-24.3637977028,19.8329835738428,-11.1728241644253));
#69755=CARTESIAN_POINT('Ctrl Pts',(-20.8626074418074,20.8564618714457,-10.9739372530505));
#69756=CARTESIAN_POINT('Ctrl Pts',(-19.8311351436954,24.3553053900332,-10.7750503416756));
#69757=CARTESIAN_POINT('Ctrl Pts',(-22.217216396,27.1143735890334,-10.5761634303007));
#69758=CARTESIAN_POINT('Ctrl Pts',(-25.8282448341817,26.5983167239714,-10.3772765189258));
#69759=CARTESIAN_POINT('Ctrl Pts',(-27.3459914882739,23.2813472994325,-10.1783896075509));
#69760=CARTESIAN_POINT('Ctrl Pts',(-25.3757758668614,20.2114789839381,-9.97950269617605));
#69761=CARTESIAN_POINT('Ctrl Pts',(-21.7280590792846,20.2096604775172,-9.78061578480118));
#69762=CARTESIAN_POINT('Ctrl Pts',(-19.7547835779453,23.2775628333863,-9.58172887342627));
#69763=CARTESIAN_POINT('Ctrl Pts',(-21.2692222424017,26.5960439017268,-9.3828419620514));
#69764=CARTESIAN_POINT('Ctrl Pts',(-24.8797343432425,27.1157009415294,-9.18395505067649));
#69765=CARTESIAN_POINT('Ctrl Pts',(-27.2685653807394,24.3590131928669,-8.98506813930161));
#69766=CARTESIAN_POINT('Ctrl Pts',(-26.2405821709042,20.8591429681827,-8.78618122792672));
#69767=CARTESIAN_POINT('Ctrl Pts',(-22.7404141249726,19.8321742639014,-8.58729431655183));
#69768=CARTESIAN_POINT('Ctrl Pts',(-19.9844189118443,22.2218042466703,-8.38840740517693));
#69769=CARTESIAN_POINT('Ctrl Pts',(-20.5051224625242,25.8321655695358,-8.18952049380205));
#69770=CARTESIAN_POINT('Ctrl Pts',(-23.8240423623182,27.345642284945,-7.99063358242715));
#69771=CARTESIAN_POINT('Ctrl Pts',(-26.8913726213182,25.3714776131012,-7.79174667105227));
#69772=CARTESIAN_POINT('Ctrl Pts',(-26.8884967982223,21.7237615058669,-7.59285975967737));
#69773=CARTESIAN_POINT('Ctrl Pts',(-23.8180575306258,19.7544357904668,-7.39397284830249));
#69774=CARTESIAN_POINT('Ctrl Pts',(-20.5015281751307,21.2731438280677,-7.19508593692757));
#69775=CARTESIAN_POINT('Ctrl Pts',(-19.9865180141189,24.8843216973216,-6.99619902555271));
#69776=CARTESIAN_POINT('Ctrl Pts',(-22.7462777198995,27.2696031137762,-6.7973121141778));
#69777=CARTESIAN_POINT('Ctrl Pts',(-26.2448221118963,26.2371166942234,-6.59842520280293));
#69778=CARTESIAN_POINT('Ctrl Pts',(-27.2672855215128,22.7356299178198,-6.39953829142803));
#69779=CARTESIAN_POINT('Ctrl Pts',(-24.8741107659123,19.9827122549589,-6.20065138005315));
#69780=CARTESIAN_POINT('Ctrl Pts',(-21.2644225377335,20.5080616288833,-6.00176446867825));
#69781=CARTESIAN_POINT('Ctrl Pts',(-19.7552182675814,23.8289265072379,-5.80287755730336));
#69782=CARTESIAN_POINT('Ctrl Pts',(-21.7333287203051,26.8937136297246,-5.60399064592847));
#69783=CARTESIAN_POINT('Ctrl Pts',(-25.38103810596,26.8861434818744,-5.40510373455358));
#69784=CARTESIAN_POINT('Ctrl Pts',(-27.3464107738837,23.8131723877192,-5.20621682317869));
#69785=CARTESIAN_POINT('Ctrl Pts',(-25.8234358783764,20.4986002378046,-5.0073299118038));
#69786=CARTESIAN_POINT('Ctrl Pts',(-22.2115982214328,19.9882378085279,-4.8084430004289));
#69787=CARTESIAN_POINT('Ctrl Pts',(-19.8298703764505,22.7510649007961,-4.60955608905403));
#69788=CARTESIAN_POINT('Ctrl Pts',(-20.8668582957487,26.2482776659228,-4.41066917767912));
#69789=CARTESIAN_POINT('Ctrl Pts',(-24.3696580035682,27.2662340875012,-4.21178226630423));
#69790=CARTESIAN_POINT('Ctrl Pts',(-27.1194935568628,24.8695185225726,-4.01289535492935));
#69791=CARTESIAN_POINT('Ctrl Pts',(-26.5894992297616,21.2605093673368,-3.81400844355446));
#69792=CARTESIAN_POINT('Ctrl Pts',(-23.266694872762,19.7555800419401,-3.61512153217957));
#69793=CARTESIAN_POINT('Ctrl Pts',(-20.2044559625963,21.737632999457,-3.41623462080468));
#69794=CARTESIAN_POINT('Ctrl Pts',(-20.2167204226629,25.3853296223073,-3.21734770942979));
#69795=CARTESIAN_POINT('Ctrl Pts',(-23.2922182540157,27.3467459877636,-3.0184607980549));
#69796=CARTESIAN_POINT('Ctrl Pts',(-26.6048277088558,25.819506756655,-2.81957388668));
#69797=CARTESIAN_POINT('Ctrl Pts',(-27.1105415611508,22.2070152938372,-2.62068697530512));
#69798=CARTESIAN_POINT('Ctrl Pts',(-24.3446516581053,19.8288449648733,-2.42180006393022));
#69799=CARTESIAN_POINT('Ctrl Pts',(-20.8487763118266,20.8703326664884,-2.22291315255534));
#69800=CARTESIAN_POINT('Ctrl Pts',(-19.8353285641946,24.3744395044934,-2.02402624118044));
#69801=CARTESIAN_POINT('Ctrl Pts',(-22.2355809690839,27.1211883940276,-1.82513932980556));
#69802=CARTESIAN_POINT('Ctrl Pts',(-25.8439050742452,26.58654999151,-1.62625241843066));
#69803=CARTESIAN_POINT('Ctrl Pts',(-27.3445569624681,23.2618116589932,-1.42736550705577));
#69804=CARTESIAN_POINT('Ctrl Pts',(-25.3585647827739,20.2021260327354,-1.22847859568088));
#69805=CARTESIAN_POINT('Ctrl Pts',(-21.7108869639328,20.2190847847069,-1.02959168430599));
#69806=CARTESIAN_POINT('Ctrl Pts',(-19.753430149382,23.2971042597106,-0.830704772931089));
#69807=CARTESIAN_POINT('Ctrl Pts',(-21.2849311867248,26.6077455332334,-0.631817861556202));
#69808=CARTESIAN_POINT('Ctrl Pts',(-24.8980704725179,27.1088099709984,-0.432930950181307));
#69809=CARTESIAN_POINT('Ctrl Pts',(-27.2726793468103,24.3398618379586,-0.234044038806425));
#69810=CARTESIAN_POINT('Ctrl Pts',(-26.2266935877583,20.8453297002904,-0.0351571274315334));
#69811=CARTESIAN_POINT('Ctrl Pts',(-22.7212854229633,19.8363923050463,0.163729783943363));
#69812=CARTESIAN_POINT('Ctrl Pts',(-19.9776277462716,22.2401775746711,0.362616695318246));
#69813=CARTESIAN_POINT('Ctrl Pts',(-20.5169093387535,25.8478106537611,0.56150360669314));
#69814=CARTESIAN_POINT('Ctrl Pts',(-23.843576140457,27.3441826194761,0.760390518068034));
#69815=CARTESIAN_POINT('Ctrl Pts',(-26.9007034154483,25.3542545067447,0.959277429442919));
#69816=CARTESIAN_POINT('Ctrl Pts',(-26.8790503996589,21.706601533086,1.15816434081781));
#69817=CARTESIAN_POINT('Ctrl Pts',(-23.7985143787261,19.7531075113212,1.3570512521927));
#69818=CARTESIAN_POINT('Ctrl Pts',(-20.4898467695046,21.2888678184727,1.55593816356758));
#69819=CARTESIAN_POINT('Ctrl Pts',(-19.9934325761168,24.9026489432696,1.75482507494249));
#69820=CARTESIAN_POINT('Ctrl Pts',(-22.7654343533035,27.2736924301352,1.95371198631737));
#69821=CARTESIAN_POINT('Ctrl Pts',(-26.258617494823,26.2232103459762,2.15259889769227));
#69822=CARTESIAN_POINT('Ctrl Pts',(-27.2630428667078,22.7165066599418,2.35148580906715));
#69823=CARTESIAN_POINT('Ctrl Pts',(-24.8557287134238,19.9759447400551,2.55037272044204));
#69824=CARTESIAN_POINT('Ctrl Pts',(-21.2487926352574,20.5198686293597,2.74925963181693));
#69825=CARTESIAN_POINT('Ctrl Pts',(-19.756703070296,23.8484583907251,2.94814654319182));
#69826=CARTESIAN_POINT('Ctrl Pts',(-21.7505638204061,26.9030222513286,3.14703345456672));
#69827=CARTESIAN_POINT('Ctrl Pts',(-25.3981859077504,26.8766750075821,3.34592036594163));
#69828=CARTESIAN_POINT('Ctrl Pts',(-27.3477139014116,23.7936275426109,3.5448072773165));
#69829=CARTESIAN_POINT('Ctrl Pts',(-25.807696867931,20.4869390774053,3.74369418869139));
#69830=CARTESIAN_POINT('Ctrl Pts',(-22.193279889165,19.9951759505411,3.94258110006629));
#69831=CARTESIAN_POINT('Ctrl Pts',(-19.8258057165764,22.7702267809692,4.14146801144116));
#69832=CARTESIAN_POINT('Ctrl Pts',(-20.8807823860657,26.2620551410361,4.34035492281606));
#69833=CARTESIAN_POINT('Ctrl Pts',(-24.3887757856436,27.2619668260629,4.53924183419096));
#69834=CARTESIAN_POINT('Ctrl Pts',(-27.1262374098896,24.8511277760402,4.73812874556585));
#69835=CARTESIAN_POINT('Ctrl Pts',(-26.5776721245927,21.2448946724955,4.93701565694073));
#69836=CARTESIAN_POINT('Ctrl Pts',(-23.2471649162744,19.7570899794412,5.13590256831564));
#69837=CARTESIAN_POINT('Ctrl Pts',(-20.1951695289349,21.7548800647585,5.3347894796905));
#69838=CARTESIAN_POINT('Ctrl Pts',(-20.2262109570028,25.4024652247072,5.53367639106541));
#69839=CARTESIAN_POINT('Ctrl Pts',(-23.3117647599631,27.3480239615159,5.73256330244029));
#69840=CARTESIAN_POINT('Ctrl Pts',(-26.6164686047155,25.8037527522356,5.9314502138152));
#69841=CARTESIAN_POINT('Ctrl Pts',(-27.103579850613,22.1887059055884,6.13033712519007));
#69842=CARTESIAN_POINT('Ctrl Pts',(-24.3254845628985,19.8248049682154,6.32922403656497));
#69843=CARTESIAN_POINT('Ctrl Pts',(-20.8350167673442,20.8842744758149,6.52811094793986));
#69844=CARTESIAN_POINT('Ctrl Pts',(-19.839620425199,24.3935517791038,6.72699785931474));
#69845=CARTESIAN_POINT('Ctrl Pts',(-22.2539803792018,27.1279085740085,6.92588477068964));
#69846=CARTESIAN_POINT('Ctrl Pts',(-25.859504535591,26.5747028012364,7.12477168206453));
#69847=CARTESIAN_POINT('Ctrl Pts',(-27.3430218926811,23.2422836618503,7.32365859343941));
#69848=CARTESIAN_POINT('Ctrl Pts',(-25.3413057808361,20.1928618023966,7.52254550481432));
#69849=CARTESIAN_POINT('Ctrl Pts',(-21.6937635893028,20.2285973633762,7.7214324161892));
#69850=CARTESIAN_POINT('Ctrl Pts',(-19.7521773315221,23.3166523941248,7.92031932756408));
#69851=CARTESIAN_POINT('Ctrl Pts',(-21.3007001590269,26.6193661452741,8.11920623893899));
#69852=CARTESIAN_POINT('Ctrl Pts',(-24.9163708864247,27.101824703466,8.31809315031388));
#69853=CARTESIAN_POINT('Ctrl Pts',(-27.2766946735608,24.3206895594619,8.51698006168875));
#69854=CARTESIAN_POINT('Ctrl Pts',(-26.2127340825124,20.8315881092272,8.71586697306367));
#69855=CARTESIAN_POINT('Ctrl Pts',(-22.7021786874711,19.8407087585086,8.91475388443853));
#69856=CARTESIAN_POINT('Ctrl Pts',(-19.9709312504664,22.258585617902,9.11364079581345));
#69857=CARTESIAN_POINT('Ctrl Pts',(-20.5287765945112,25.863394855776,9.31252770718832));
#69858=CARTESIAN_POINT('Ctrl Pts',(-23.8631021459136,27.3426224199458,9.51141461856321));
#69859=CARTESIAN_POINT('Ctrl Pts',(-26.9099454271214,25.3369835967543,9.71030152993811));
#69860=CARTESIAN_POINT('Ctrl Pts',(-26.8695157924143,21.6894904145851,9.909188441313));
#69861=CARTESIAN_POINT('Ctrl Pts',(-23.7789646482203,19.7518798514284,10.1080753526879));
#69862=CARTESIAN_POINT('Ctrl Pts',(-20.4782464605285,21.3046517325413,10.3069622640628));
#69863=CARTESIAN_POINT('Ctrl Pts',(-20.0004413890756,24.9209403525256,10.5058491754377));
#69864=CARTESIAN_POINT('Ctrl Pts',(-22.7846117833373,27.2776830803283,10.7047360868126));
#69865=CARTESIAN_POINT('Ctrl Pts',(-26.2723411097087,26.2092331679301,10.9036229981875));
#69866=CARTESIAN_POINT('Ctrl Pts',(-27.2587018279362,22.6974054952116,11.1025099095624));
#69867=CARTESIAN_POINT('Ctrl Pts',(-24.8373120675665,19.9692719395162,11.3013968209372));
#69868=CARTESIAN_POINT('Ctrl Pts',(-21.2332237183833,20.5317559309471,11.5002837323122));
#69869=CARTESIAN_POINT('Ctrl Pts',(-19.7582883969858,23.8679823721571,11.699170643687));
#69870=CARTESIAN_POINT('Ctrl Pts',(-21.7678466098456,26.9122420290296,11.8980575550619));
#69871=CARTESIAN_POINT('Ctrl Pts',(-25.4152847417835,26.8671183875534,12.0969444664368));
#69872=CARTESIAN_POINT('Ctrl Pts',(-27.3489164013039,23.774076248391,12.2958313778117));
#69873=CARTESIAN_POINT('Ctrl Pts',(-25.7918980382369,20.475359090706,12.4947182891866));
#69874=CARTESIAN_POINT('Ctrl Pts',(-22.1749975148535,20.0022082973181,12.6936052005615));
#69875=CARTESIAN_POINT('Ctrl Pts',(-19.82183974955,22.7894093307791,12.8924921119364));
#69876=CARTESIAN_POINT('Ctrl Pts',(-20.8947772137633,26.2757607570156,13.0913790233113));
#69877=CARTESIAN_POINT('Ctrl Pts',(-24.4078713479767,27.2576012091716,13.2902659346862));
#69878=CARTESIAN_POINT('Ctrl Pts',(-27.132886504111,24.8327025580578,13.4891528460611));
#69879=CARTESIAN_POINT('Ctrl Pts',(-26.565764796863,21.2293410665471,13.6880397574359));
#69880=CARTESIAN_POINT('Ctrl Pts',(-23.2276429912025,19.7587004306651,13.8869266688109));
#69881=CARTESIAN_POINT('Ctrl Pts',(-20.1859720004754,21.7721747050237,14.0858135801857));
#69882=CARTESIAN_POINT('Ctrl Pts',(-20.2357895739884,25.4195517459537,14.2847004915607));
#69883=CARTESIAN_POINT('Ctrl Pts',(-23.3313175855166,27.3492012994163,14.4835874029355));
#69884=CARTESIAN_POINT('Ctrl Pts',(-26.6280282499597,25.7879390330813,14.6824743143104));
#69885=CARTESIAN_POINT('Ctrl Pts',(-27.0965239816645,22.1704325964997,14.8813612256853));
#69886=CARTESIAN_POINT('Ctrl Pts',(-24.306296925082,19.820863690924,15.0802481370602));
#69887=CARTESIAN_POINT('Ctrl Pts',(-20.8213291729697,20.8982869299861,15.2791350484351));
#69888=CARTESIAN_POINT('Ctrl Pts',(-19.8440106129798,24.4126417074145,15.47802195981));
#69889=CARTESIAN_POINT('Ctrl Pts',(-22.272414138794,27.1345339509001,15.6769088711849));
#69890=CARTESIAN_POINT('Ctrl Pts',(-25.8750428048544,26.5627754670849,15.8757957825598));
#69891=CARTESIAN_POINT('Ctrl Pts',(-27.3413863195906,23.2227638254696,16.0746826939346));
#69892=CARTESIAN_POINT('Ctrl Pts',(-25.3239993183881,20.1836865384115,16.2735696053096));
#69893=CARTESIAN_POINT('Ctrl Pts',(-21.676689409141,20.2381979614547,16.4724565166844));
#69894=CARTESIAN_POINT('Ctrl Pts',(-19.7510251575634,23.3362067186294,16.6713434280593));
#69895=CARTESIAN_POINT('Ctrl Pts',(-21.3165287414511,26.6309054299184,16.8702303394342));
#69896=CARTESIAN_POINT('Ctrl Pts',(-24.9346351000264,27.0947453240317,17.0691172508091));
#69897=CARTESIAN_POINT('Ctrl Pts',(-27.2806112545899,24.301496865417,17.268004162184));
#69898=CARTESIAN_POINT('Ctrl Pts',(-26.1987040250745,20.8179185591267,17.4668910735589));
#69899=CARTESIAN_POINT('Ctrl Pts',(-22.6830944247988,19.8451235099081,17.6657779849338));
#69900=CARTESIAN_POINT('Ctrl Pts',(-19.964329601877,22.2770278885748,17.8646648963087));
#69901=CARTESIAN_POINT('Ctrl Pts',(-20.5407239153308,25.8789177626204,18.0635518076836));
#69902=CARTESIAN_POINT('Ctrl Pts',(-23.8826198612747,27.3409617276973,18.2624387190584));
#69903=CARTESIAN_POINT('Ctrl Pts',(-26.9190984114366,25.3196653407859,18.4613256304333));
#69904=CARTESIAN_POINT('Ctrl Pts',(-26.8598932291429,21.6724286037856,18.6602125418082));
#69905=CARTESIAN_POINT('Ctrl Pts',(-23.7594088571501,19.7507528433199,18.8590994531831));
#69906=CARTESIAN_POINT('Ctrl Pts',(-20.4667275555952,21.3204951520206,19.057986364558));
#69907=CARTESIAN_POINT('Ctrl Pts',(-20.0075442672708,24.9391954403919,19.2568732759329));
#69908=CARTESIAN_POINT('Ctrl Pts',(-22.8038095018245,27.2815749586085,19.4557601873078));
#69909=CARTESIAN_POINT('Ctrl Pts',(-26.2859925928962,26.1951855304619,19.6546470986827));
#69910=CARTESIAN_POINT('Ctrl Pts',(-27.2542625202295,22.6783269297847,19.8535340100576));
#69911=CARTESIAN_POINT('Ctrl Pts',(-24.818861316357,19.9626940301626,20.0524209214325));
#69912=CARTESIAN_POINT('Ctrl Pts',(-21.2177161996666,20.5437232186478,20.2513078328074));
#69913=CARTESIAN_POINT('Ctrl Pts',(-19.7599742056419,23.887497934174,20.4501947441822));
#69914=CARTESIAN_POINT('Ctrl Pts',(-21.7851766306525,26.9213727185159,20.6490816555571));
#69915=CARTESIAN_POINT('Ctrl Pts',(-25.4323341549631,26.857473875026,20.847968566932));
#69916=CARTESIAN_POINT('Ctrl Pts',(-27.3500182416961,23.7545190231427,21.0468554783069));
#69917=CARTESIAN_POINT('Ctrl Pts',(-25.7760398079417,20.4638605845609,21.2457423896818));
#69918=CARTESIAN_POINT('Ctrl Pts',(-22.1567515829562,20.0093346625109,21.4446293010567));
#69919=CARTESIAN_POINT('Ctrl Pts',(-19.8179725804642,22.8086120419138,21.6435162124316));
#69920=CARTESIAN_POINT('Ctrl Pts',(-20.908842407997,26.2893941506808,21.8424031238065));
#69921=CARTESIAN_POINT('Ctrl Pts',(-24.426944184561,27.2531373525101,22.0412900351814));
#69922=CARTESIAN_POINT('Ctrl Pts',(-27.1394406633346,24.8142433568688,22.2401769465563));
#69923=CARTESIAN_POINT('Ctrl Pts',(-26.5537775621008,21.2138489616415,22.4390638579311));
#69924=CARTESIAN_POINT('Ctrl Pts',(-23.2081296148507,19.7604113529361,22.637950769306));
#69925=CARTESIAN_POINT('Ctrl Pts',(-20.1768636209402,21.7895164619687,22.8368376806809));
#69926=CARTESIAN_POINT('Ctrl Pts',(-20.2454560197989,25.4365887332747,23.0357245920558));
#69927=CARTESIAN_POINT('Ctrl Pts',(-23.3508762125534,27.350277970271,23.2346115034307));
#69928=CARTESIAN_POINT('Ctrl Pts',(-26.639506338272,25.7720660182269,23.4334984148056));
#69929=CARTESIAN_POINT('Ctrl Pts',(-27.0893741412788,22.152195850804,23.6323853261805));
#69930=CARTESIAN_POINT('Ctrl Pts',(-24.2870892530986,19.8170212374106,23.8312722375554));
#69931=CARTESIAN_POINT('Ctrl Pts',(-20.8077138914136,20.9123696577412,24.0301591489302));
#69932=CARTESIAN_POINT('Ctrl Pts',(-19.8484990111886,24.431708783473,24.2290460603052));
#69933=CARTESIAN_POINT('Ctrl Pts',(-22.2908817594182,27.141064349319,24.42793297168));
#69934=CARTESIAN_POINT('Ctrl Pts',(-25.8905194702402,26.5507683047743,24.6268198830549));
#69935=CARTESIAN_POINT('Ctrl Pts',(-27.3396502866349,23.2032526677418,24.8257067944298));
#69936=CARTESIAN_POINT('Ctrl Pts',(-25.3066458538429,20.174600482701,25.0245937058047));
#69937=CARTESIAN_POINT('Ctrl Pts',(-21.6596648762396,20.2478863268259,25.2234806171796));
#69938=CARTESIAN_POINT('Ctrl Pts',(-19.7499736573778,23.3557667107438,25.4223675285545));
#69939=CARTESIAN_POINT('Ctrl Pts',(-21.3324165158066,26.6423630895425,25.6212544399294));
#69940=CARTESIAN_POINT('Ctrl Pts',(-24.9528626269947,27.0875720048975,25.8201413513043));
#69941=CARTESIAN_POINT('Ctrl Pts',(-27.2844289905532,24.2822842934685,26.0190282626791));
#69942=CARTESIAN_POINT('Ctrl Pts',(-26.1846037788393,20.8043213573341,26.2179151740541));
#69943=CARTESIAN_POINT('Ctrl Pts',(-22.6640331564827,19.8496365458834,26.416802085429));
#69944=CARTESIAN_POINT('Ctrl Pts',(-19.9578229455499,22.2955037023318,26.6156889968038));
#69945=CARTESIAN_POINT('Ctrl Pts',(-20.5527510410596,25.8943793324076,26.8145759081788));
#69946=CARTESIAN_POINT('Ctrl Pts',(-23.9021286627863,27.3391998891404,27.0134628195536));
#69947=CARTESIAN_POINT('Ctrl Pts',(-26.928162327061,25.3023015149534,27.2123497309286));
#69948=CARTESIAN_POINT('Ctrl Pts',(-26.8501825849064,21.6554140656546,27.4112366423034));
#69949=CARTESIAN_POINT('Ctrl Pts',(-23.7398482410897,19.7497312131016,27.6101235536783));
#69950=CARTESIAN_POINT('Ctrl Pts',(-20.4552890053948,21.3363887896213,27.8090104650532));
#69951=CARTESIAN_POINT('Ctrl Pts',(-20.0147435801427,24.9574304667042,28.0078973764281));
#69952=CARTESIAN_POINT('Ctrl Pts',(-22.8230221706751,27.285336346559,28.206784287803));
#69953=CARTESIAN_POINT('Ctrl Pts',(-26.2995807014884,26.1811275020712,28.4056711991778));
#69954=CARTESIAN_POINT('Ctrl Pts',(-27.2497078429493,22.6591587491998,28.6045581105528));
#69955=CARTESIAN_POINT('Ctrl Pts',(-24.8004094605876,19.9564240356054,28.8034450219277));
#69956=CARTESIAN_POINT('Ctrl Pts',(-21.2022090988071,20.5553681827278,29.0023319333025));
#69957=CARTESIAN_POINT('Ctrl Pts',(-19.7618763887169,23.9077643379941,29.2012188446774));
#69958=CARTESIAN_POINT('Ctrl Pts',(-21.8023343633778,26.9289734564946,29.4001057560523));
#69959=CARTESIAN_POINT('Ctrl Pts',(-25.4497485501313,26.8505109829531,29.5989926674272));
#69960=CARTESIAN_POINT('Ctrl Pts',(-27.3506339076343,23.7286560066104,29.797922464558));
#69961=CARTESIAN_POINT('Ctrl Pts',(-26.290666056329,21.5524040433688,29.9305566245639));
#69962=CARTESIAN_POINT('Ctrl Pts',(-25.4168923872279,20.930003392908,29.9968951474449));
#69963=CARTESIAN_POINT('Ctrl Pts',(-25.087202831673,26.6465417208825,-75.274954513805));
#69964=CARTESIAN_POINT('Ctrl Pts',(-26.1190047250109,26.1343711410084,-75.2086588766801));
#69965=CARTESIAN_POINT('Ctrl Pts',(-27.6122618789375,24.0062782296181,-75.0760676024301));
#69966=CARTESIAN_POINT('Ctrl Pts',(-26.1265778059314,20.3717807620434,-74.8771806910553));
#69967=CARTESIAN_POINT('Ctrl Pts',(-22.2702066924084,19.668455682932,-74.6782937796803));
#69968=CARTESIAN_POINT('Ctrl Pts',(-19.5917683008039,22.526906813967,-74.4794068683055));
#69969=CARTESIAN_POINT('Ctrl Pts',(-20.5499578780943,26.3284832670958,-74.2805199569306));
#69970=CARTESIAN_POINT('Ctrl Pts',(-24.2656310039462,27.5756447695868,-74.0816330455557));
#69971=CARTESIAN_POINT('Ctrl Pts',(-27.3236846535468,25.1245829777789,-73.8827461341808));
#69972=CARTESIAN_POINT('Ctrl Pts',(-26.9144050854087,21.2264367862693,-73.6838592228059));
#69973=CARTESIAN_POINT('Ctrl Pts',(-23.4136851936635,19.4638964155144,-73.484972311431));
#69974=CARTESIAN_POINT('Ctrl Pts',(-20.0384958396557,21.4562563619107,-73.2860854000561));
#69975=CARTESIAN_POINT('Ctrl Pts',(-19.8902936837951,25.3728818798044,-73.0871984886812));
#69976=CARTESIAN_POINT('Ctrl Pts',(-23.1052936987138,27.6146334487714,-72.8883115773064));
#69977=CARTESIAN_POINT('Ctrl Pts',(-26.7291676983987,26.1215805639939,-72.6894246659315));
#69978=CARTESIAN_POINT('Ctrl Pts',(-27.4318910772013,22.2656862235542,-72.4905377545565));
#69979=CARTESIAN_POINT('Ctrl Pts',(-24.5677162109303,19.5902041769872,-72.2916508431817));
#69980=CARTESIAN_POINT('Ctrl Pts',(-20.7685793006563,20.5536682854776,-72.0927639318068));
#69981=CARTESIAN_POINT('Ctrl Pts',(-19.5255638134539,24.2707405856734,-71.8938770204319));
#69982=CARTESIAN_POINT('Ctrl Pts',(-21.980896248319,27.3257447430297,-71.694990109057));
#69983=CARTESIAN_POINT('Ctrl Pts',(-25.878333927738,26.9113920423683,-71.4961031976822));
#69984=CARTESIAN_POINT('Ctrl Pts',(-27.6364622567071,23.4084369102996,-71.2972162863072));
#69985=CARTESIAN_POINT('Ctrl Pts',(-25.6397102680719,20.0357984155606,-71.0983293749323));
#69986=CARTESIAN_POINT('Ctrl Pts',(-21.7229237943914,19.8926452212372,-70.8994424635574));
#69987=CARTESIAN_POINT('Ctrl Pts',(-19.4852974888931,23.1105230607847,-70.7005555521826));
#69988=CARTESIAN_POINT('Ctrl Pts',(-20.9830202213933,26.7324749855528,-70.5016686408076));
#69989=CARTESIAN_POINT('Ctrl Pts',(-24.8398117789982,27.4302342914755,-70.3027817294328));
#69990=CARTESIAN_POINT('Ctrl Pts',(-27.5116077263315,24.5626193239777,-70.1038948180579));
#69991=CARTESIAN_POINT('Ctrl Pts',(-26.5432541165811,20.764725111243,-69.905007906683));
#69992=CARTESIAN_POINT('Ctrl Pts',(-22.8245858154009,19.5264944228945,-69.7061209953081));
#69993=CARTESIAN_POINT('Ctrl Pts',(-19.7727436998939,21.9857562787565,-69.5072340839333));
#69994=CARTESIAN_POINT('Ctrl Pts',(-20.1921119209898,25.8826575433156,-69.3083471725583));
#69995=CARTESIAN_POINT('Ctrl Pts',(-23.6973266398938,27.6362763577108,-69.1094602611835));
#69996=CARTESIAN_POINT('Ctrl Pts',(-27.0673927232214,25.6351857135901,-68.9105733498085));
#69997=CARTESIAN_POINT('Ctrl Pts',(-27.205505174831,21.7182182485408,-68.7116864384336));
#69998=CARTESIAN_POINT('Ctrl Pts',(-23.9847503617234,19.4847349587904,-68.5127995270588));
#69999=CARTESIAN_POINT('Ctrl Pts',(-20.3647288821552,20.9871176195064,-68.3139126156839));
#70000=CARTESIAN_POINT('Ctrl Pts',(-19.67193354865,24.8448039465122,-68.115025704309));
#70001=CARTESIAN_POINT('Ctrl Pts',(-22.5429845333374,27.5129072831641,-67.916138792934));
#70002=CARTESIAN_POINT('Ctrl Pts',(-26.3396294062728,26.5396668809304,-67.7172518815593));
#70003=CARTESIAN_POINT('Ctrl Pts',(-27.5730734316282,22.819408152289,-67.5183649701843));
#70004=CARTESIAN_POINT('Ctrl Pts',(-25.1098861289101,19.7707334429356,-67.3194780588094));
#70005=CARTESIAN_POINT('Ctrl Pts',(-21.2135277854729,20.1951163257777,-67.1205911474346));
#70006=CARTESIAN_POINT('Ctrl Pts',(-19.4644213622264,23.7025849132179,-66.9217042360596));
#70007=CARTESIAN_POINT('Ctrl Pts',(-21.4698473623653,27.0700729576938,-66.7228173246848));
#70008=CARTESIAN_POINT('Ctrl Pts',(-25.386989323847,27.2031444622345,-66.5239304133098));
#70009=CARTESIAN_POINT('Ctrl Pts',(-27.6163259029392,23.97951799677,-66.325043501935));
#70010=CARTESIAN_POINT('Ctrl Pts',(-26.1092858000276,20.3614329646103,-66.1261565905601));
#70011=CARTESIAN_POINT('Ctrl Pts',(-22.2507110937587,19.6736027472872,-65.9272696791851));
#70012=CARTESIAN_POINT('Ctrl Pts',(-19.5863047860085,22.5480849961352,-65.7283827678104));
#70013=CARTESIAN_POINT('Ctrl Pts',(-20.5644303691982,26.3434742403671,-65.5294958564353));
#70014=CARTESIAN_POINT('Ctrl Pts',(-24.2862733637496,27.572129560475,-65.3306089450606));
#70015=CARTESIAN_POINT('Ctrl Pts',(-27.3317756179178,25.1050208900719,-65.1317220336856));
#70016=CARTESIAN_POINT('Ctrl Pts',(-26.9023787761313,21.2092119209378,-64.9328351223108));
#70017=CARTESIAN_POINT('Ctrl Pts',(-23.3926621291436,19.4646207855772,-64.7339482109358));
#70018=CARTESIAN_POINT('Ctrl Pts',(-20.0277577006371,21.4743788204509,-64.5350612995609));
#70019=CARTESIAN_POINT('Ctrl Pts',(-19.8997273635616,25.3916887908911,-64.3361743881861));
#70020=CARTESIAN_POINT('Ctrl Pts',(-23.1262201425069,27.6168749671773,-64.1372874768111));
#70021=CARTESIAN_POINT('Ctrl Pts',(-26.7423627350975,26.105179917978,-63.9384005654363));
#70022=CARTESIAN_POINT('Ctrl Pts',(-27.425226697074,22.2457232229035,-63.7395136540614));
#70023=CARTESIAN_POINT('Ctrl Pts',(-24.5473179446962,19.585018356762,-63.5406267426865));
#70024=CARTESIAN_POINT('Ctrl Pts',(-20.7531906149757,20.5680275009666,-63.3417398313116));
#70025=CARTESIAN_POINT('Ctrl Pts',(-19.5293260349772,24.2914485974244,-63.1428529199367));
#70026=CARTESIAN_POINT('Ctrl Pts',(-22.0003519871148,27.3337733525391,-62.9439660085619));
#70027=CARTESIAN_POINT('Ctrl Pts',(-25.8956051298252,26.8993632629622,-62.7450790971869));
#70028=CARTESIAN_POINT('Ctrl Pts',(-27.6356780879611,23.3874043691131,-62.546192185812));
#70029=CARTESIAN_POINT('Ctrl Pts',(-25.6215913468528,20.0250891294288,-62.3473052744372));
#70030=CARTESIAN_POINT('Ctrl Pts',(-21.7041198551841,19.9021001718582,-62.1484183630623));
#70031=CARTESIAN_POINT('Ctrl Pts',(-19.4830877669895,23.1314539206649,-61.9495314516874));
#70032=CARTESIAN_POINT('Ctrl Pts',(-20.9994352588532,26.7456480847409,-61.7506445403125));
#70033=CARTESIAN_POINT('Ctrl Pts',(-24.8597675508181,27.4235446604322,-61.5517576289376));
#70034=CARTESIAN_POINT('Ctrl Pts',(-27.5167665687724,24.5422141708298,-61.3528707175627));
#70035=CARTESIAN_POINT('Ctrl Pts',(-26.5288754915826,20.7493550393392,-61.1539838061878));
#70036=CARTESIAN_POINT('Ctrl Pts',(-22.8038824598357,19.5302832263775,-60.9550968948129));
#70037=CARTESIAN_POINT('Ctrl Pts',(-19.7647402423802,22.0052223678112,-60.7562099834381));
#70038=CARTESIAN_POINT('Ctrl Pts',(-20.2041628602908,25.8999132328981,-60.5573230720631));
#70039=CARTESIAN_POINT('Ctrl Pts',(-23.7183581846015,27.6354651319532,-60.3584361606884));
#70040=CARTESIAN_POINT('Ctrl Pts',(-27.0780786668995,25.6170530202798,-60.1595492493133));
#70041=CARTESIAN_POINT('Ctrl Pts',(-27.1960260412742,21.6994264953798,-59.9606623379385));
#70042=CARTESIAN_POINT('Ctrl Pts',(-23.9638166709638,19.4825521736829,-59.7617754265636));
#70043=CARTESIAN_POINT('Ctrl Pts',(-20.3515769211211,21.0035495968821,-59.5628885151886));
#70044=CARTESIAN_POINT('Ctrl Pts',(-19.6786488544269,24.8647510923725,-59.3640016038139));
#70045=CARTESIAN_POINT('Ctrl Pts',(-22.5633963092817,27.5180398616982,-59.1651146924389));
#70046=CARTESIAN_POINT('Ctrl Pts',(-26.354980960924,26.5252684876387,-58.9662277810641));
#70047=CARTESIAN_POINT('Ctrl Pts',(-27.5692579878596,22.7987096898228,-58.7673408696891));
#70048=CARTESIAN_POINT('Ctrl Pts',(-25.0904097560483,19.7627550433618,-58.5684539583142));
#70049=CARTESIAN_POINT('Ctrl Pts',(-21.1962876188541,20.2071894618475,-58.3695670469394));
#70050=CARTESIAN_POINT('Ctrl Pts',(-19.465259653248,23.7236153965165,-58.1706801355645));
#70051=CARTESIAN_POINT('Ctrl Pts',(-21.4879937926539,27.0807355571606,-57.9717932241896));
#70052=CARTESIAN_POINT('Ctrl Pts',(-25.4057688625309,27.1936411529989,-57.7729063128147));
#70053=CARTESIAN_POINT('Ctrl Pts',(-27.6184817462102,23.9585815142718,-57.5740194014398));
#70054=CARTESIAN_POINT('Ctrl Pts',(-26.0928369107051,20.3483021611443,-57.3751324900649));
#70055=CARTESIAN_POINT('Ctrl Pts',(-22.2307726064942,19.6803437179301,-57.17624557869));
#70056=CARTESIAN_POINT('Ctrl Pts',(-19.5811984800931,22.5685033604062,-56.9773586673151));
#70057=CARTESIAN_POINT('Ctrl Pts',(-20.5788485068248,26.358807252693,-56.7784717559402));
#70058=CARTESIAN_POINT('Ctrl Pts',(-24.3069668988959,27.5682874825533,-56.5795848445653));
#70059=CARTESIAN_POINT('Ctrl Pts',(-27.3397289463067,25.0855342657581,-56.3806979331904));
#70060=CARTESIAN_POINT('Ctrl Pts',(-26.8902834633044,21.1919873057831,-56.1818110218156));
#70061=CARTESIAN_POINT('Ctrl Pts',(-23.3716327420754,19.4654861405022,-55.9829241104406));
#70062=CARTESIAN_POINT('Ctrl Pts',(-20.0171184630454,21.4925389576496,-55.7840371990659));
#70063=CARTESIAN_POINT('Ctrl Pts',(-19.9092548327343,25.4104560840035,-55.5851502876908));
#70064=CARTESIAN_POINT('Ctrl Pts',(-23.1471593820707,27.6190038650373,-55.3862633763161));
#70065=CARTESIAN_POINT('Ctrl Pts',(-26.7554723592479,26.0887141439529,-55.187376464941));
#70066=CARTESIAN_POINT('Ctrl Pts',(-27.4184600727296,22.225793427255,-54.9884895535663));
#70067=CARTESIAN_POINT('Ctrl Pts',(-24.5268930259144,19.5799383319231,-54.7896026421912));
#70068=CARTESIAN_POINT('Ctrl Pts',(-20.7378761703695,20.582465359049,-54.5907157308165));
#70069=CARTESIAN_POINT('Ctrl Pts',(-19.5331947406888,24.3121371709789,-54.3918288194415));
#70070=CARTESIAN_POINT('Ctrl Pts',(-22.0198488306076,27.341701596571,-54.1929419080667));
#70071=CARTESIAN_POINT('Ctrl Pts',(-25.9128141649889,26.8872457934103,-53.9940549966918));
#70072=CARTESIAN_POINT('Ctrl Pts',(-27.6347856705658,23.3663761131036,-53.7951680853169));
#70073=CARTESIAN_POINT('Ctrl Pts',(-25.6034175328204,20.0144732713323,-53.596281173942));
#70074=CARTESIAN_POINT('Ctrl Pts',(-21.6853648387249,19.9116517851892,-53.3973942625671));
#70075=CARTESIAN_POINT('Ctrl Pts',(-19.4809858180664,23.1523958826153,-53.1985073511921));
#70076=CARTESIAN_POINT('Ctrl Pts',(-21.0159178903106,26.7587365078639,-52.9996204398173));
#70077=CARTESIAN_POINT('Ctrl Pts',(-24.8796886218434,27.416752393593,-52.8007335284424));
#70078=CARTESIAN_POINT('Ctrl Pts',(-27.5218203041215,24.5217827313643,-52.6018466170675));
#70079=CARTESIAN_POINT('Ctrl Pts',(-26.514417936956,20.734059187816,-52.4029597056927));
#70080=CARTESIAN_POINT('Ctrl Pts',(-22.7831988821365,19.5341785534718,-52.2040727943177));
#70081=CARTESIAN_POINT('Ctrl Pts',(-19.756837095836,22.024729398193,-52.0051858829429));
#70082=CARTESIAN_POINT('Ctrl Pts',(-20.2163024664992,25.9171066595697,-51.8062989715679));
#70083=CARTESIAN_POINT('Ctrl Pts',(-23.7393852747262,27.6345456535659,-51.6074120601931));
#70084=CARTESIAN_POINT('Ctrl Pts',(-27.0886711279188,25.5988655595124,-51.4085251488182));
#70085=CARTESIAN_POINT('Ctrl Pts',(-27.1864502996043,21.6806837866354,-51.2096382374433));
#70086=CARTESIAN_POINT('Ctrl Pts',(-23.9428720213101,19.4804771771778,-51.0107513260684));
#70087=CARTESIAN_POINT('Ctrl Pts',(-20.3385097207022,21.0200490584739,-50.8118644146935));
#70088=CARTESIAN_POINT('Ctrl Pts',(-19.6854667525116,24.8846634057819,-50.6129775033186));
#70089=CARTESIAN_POINT('Ctrl Pts',(-22.5838342355929,27.5230672991878,-50.4140905919437));
#70090=CARTESIAN_POINT('Ctrl Pts',(-26.370258194032,26.5107912604119,-50.2152036805689));
#70091=CARTESIAN_POINT('Ctrl Pts',(-27.5653360458338,22.7780311422346,-50.0163167691939));
#70092=CARTESIAN_POINT('Ctrl Pts',(-25.0708925710849,19.754877007394,-49.8174298578191));
#70093=CARTESIAN_POINT('Ctrl Pts',(-21.1791098291497,20.2193511846074,-49.618542946444));
#70094=CARTESIAN_POINT('Ctrl Pts',(-19.466206191105,23.7446412859314,-49.4196560350694));
#70095=CARTESIAN_POINT('Ctrl Pts',(-21.5061948700345,27.09130460356,-49.2207691236942));
#70096=CARTESIAN_POINT('Ctrl Pts',(-25.4244992325195,27.1840412988489,-49.0218822123197));
#70097=CARTESIAN_POINT('Ctrl Pts',(-27.6205297868606,23.9376342116029,-48.8229953009445));
#70098=CARTESIAN_POINT('Ctrl Pts',(-26.0763206463049,20.3352562050708,-48.6241083895698));
#70099=CARTESIAN_POINT('Ctrl Pts',(-22.2108690836787,19.6871872359689,-48.4252214781947));
#70100=CARTESIAN_POINT('Ctrl Pts',(-19.5761973487895,22.5889477397143,-48.22633456682));
#70101=CARTESIAN_POINT('Ctrl Pts',(-20.5933453826749,26.3740658420838,-48.0274476554451));
#70102=CARTESIAN_POINT('Ctrl Pts',(-24.327640382126,27.5643389320917,-47.8285607440701));
#70103=CARTESIAN_POINT('Ctrl Pts',(-27.3475818586505,25.0660069585364,-47.6296738326953));
#70104=CARTESIAN_POINT('Ctrl Pts',(-26.8780996441353,21.1748251814955,-47.4307869213203));
#70105=CARTESIAN_POINT('Ctrl Pts',(-23.3506080881922,19.4664597362608,-47.2319000099455));
#70106=CARTESIAN_POINT('Ctrl Pts',(-20.0065728487701,21.5107536214995,-47.0330130985705));
#70107=CARTESIAN_POINT('Ctrl Pts',(-19.9188787834653,25.4291740842155,-46.8341261871958));
#70108=CARTESIAN_POINT('Ctrl Pts',(-23.1681093030625,27.6210249464413,-46.6352392758207));
#70109=CARTESIAN_POINT('Ctrl Pts',(-26.7684970493695,26.072181104098,-46.436352364446));
#70110=CARTESIAN_POINT('Ctrl Pts',(-27.4115909460707,22.2058987279973,-46.237465453071));
#70111=CARTESIAN_POINT('Ctrl Pts',(-24.5064422274687,19.574963515088,-46.0385785416961));
#70112=CARTESIAN_POINT('Ctrl Pts',(-20.7226362499667,20.5969818595133,-45.8396916303212));
#70113=CARTESIAN_POINT('Ctrl Pts',(-19.5371698930469,24.332805555612,-45.6408047189464));
#70114=CARTESIAN_POINT('Ctrl Pts',(-22.0393862277468,27.3495293722852,-45.4419178075714));
#70115=CARTESIAN_POINT('Ctrl Pts',(-25.9299605954365,26.8750398980102,-45.2430308961966));
#70116=CARTESIAN_POINT('Ctrl Pts',(-27.633785018518,23.3453527295727,-45.0441439848217));
#70117=CARTESIAN_POINT('Ctrl Pts',(-25.5851893126678,20.0039511066464,-44.8452570734468));
#70118=CARTESIAN_POINT('Ctrl Pts',(-21.6666592392896,19.9212998165622,-44.6463701620719));
#70119=CARTESIAN_POINT('Ctrl Pts',(-19.4789916992562,23.1733483872337,-44.447483250697));
#70120=CARTESIAN_POINT('Ctrl Pts',(-21.0324676782386,26.7717399104627,-44.2485963393221));
#70121=CARTESIAN_POINT('Ctrl Pts',(-24.8995744645946,27.4098576696907,-44.0497094279473));
#70122=CARTESIAN_POINT('Ctrl Pts',(-27.5267687982487,24.501325547651,-43.8508225165723));
#70123=CARTESIAN_POINT('Ctrl Pts',(-26.4998818359196,20.718837961641,-43.6519356051975));
#70124=CARTESIAN_POINT('Ctrl Pts',(-22.7625356303309,19.5381803011428,-43.4530486938226));
#70125=CARTESIAN_POINT('Ctrl Pts',(-19.7490344697155,22.0442768528926,-43.2541617824477));
#70126=CARTESIAN_POINT('Ctrl Pts',(-20.2285304179152,25.9342373677798,-43.0552748710728));
#70127=CARTESIAN_POINT('Ctrl Pts',(-23.7604073530864,27.6335179468858,-42.8563879596979));
#70128=CARTESIAN_POINT('Ctrl Pts',(-27.0991698255887,25.5806238132462,-42.657501048323));
#70129=CARTESIAN_POINT('Ctrl Pts',(-27.1767782035679,21.6619906189565,-42.4586141369482));
#70130=CARTESIAN_POINT('Ctrl Pts',(-23.9219169677665,19.478510024264,-42.2597272255731));
#70131=CARTESIAN_POINT('Ctrl Pts',(-20.3255276271621,21.0366155670659,-42.0608403141984));
#70132=CARTESIAN_POINT('Ctrl Pts',(-19.6923870622387,24.9045403590919,-41.8619534028234));
#70133=CARTESIAN_POINT('Ctrl Pts',(-22.6042977706932,27.5279894624118,-41.6630664914486));
#70134=CARTESIAN_POINT('Ctrl Pts',(-26.3854607007702,26.4962355828775,-41.4641795800736));
#70135=CARTESIAN_POINT('Ctrl Pts',(-27.5613077094774,22.7573730574781,-41.2652926686988));
#70136=CARTESIAN_POINT('Ctrl Pts',(-25.0513350911988,19.7470995437899,-41.0664057573238));
#70137=CARTESIAN_POINT('Ctrl Pts',(-21.1619948715485,20.2316011717875,-40.867518845949));
#70138=CARTESIAN_POINT('Ctrl Pts',(-19.4672609507149,23.7656620243051,-40.668631934574));
#70139=CARTESIAN_POINT('Ctrl Pts',(-21.524450112203,27.1017798168263,-40.4697450231992));
#70140=CARTESIAN_POINT('Ctrl Pts',(-25.4431799374829,27.1743451541679,-40.2708581118243));
#70141=CARTESIAN_POINT('Ctrl Pts',(-27.6224699706203,23.9166766438388,-40.0719712004494));
#70142=CARTESIAN_POINT('Ctrl Pts',(-26.059737444486,20.3222954420901,-39.8730842890745));
#70143=CARTESIAN_POINT('Ctrl Pts',(-22.1910010527294,19.6941331200593,-39.6741973776996));
#70144=CARTESIAN_POINT('Ctrl Pts',(-19.5713015246209,22.6094175923108,-39.4753104663248));
#70145=CARTESIAN_POINT('Ctrl Pts',(-20.6079206126006,26.3892496042072,-39.2764235549498));
#70146=CARTESIAN_POINT('Ctrl Pts',(-24.34829326562,27.5602840137214,-39.077536643575));
#70147=CARTESIAN_POINT('Ctrl Pts',(-27.3553341468577,25.0464394858545,-38.8786497322));
#70148=CARTESIAN_POINT('Ctrl Pts',(-26.8658276414789,21.1577260028483,-38.6797628208252));
#70149=CARTESIAN_POINT('Ctrl Pts',(-23.3295887246191,19.467541547054,-38.4808759094503));
#70150=CARTESIAN_POINT('Ctrl Pts',(-19.9961211372559,21.5290223293364,-38.2819889980755));
#70151=CARTESIAN_POINT('Ctrl Pts',(-19.9285989607326,25.4478422955252,-38.0831020867004));
#70152=CARTESIAN_POINT('Ctrl Pts',(-23.1890693503378,27.6229381578333,-37.8842151753257));
#70153=CARTESIAN_POINT('Ctrl Pts',(-26.7814364603257,26.0555812365168,-37.6853282639507));
#70154=CARTESIAN_POINT('Ctrl Pts',(-27.4046194991203,22.1860396523133,-37.4864413525758));
#70155=CARTESIAN_POINT('Ctrl Pts',(-24.485966091278,19.5700940380829,-37.287554441201));
#70156=CARTESIAN_POINT('Ctrl Pts',(-20.7074712576047,20.6115766176912,-37.088667529826));
#70157=CARTESIAN_POINT('Ctrl Pts',(-19.5412513867153,24.353453203639,-36.8897806184512));
#70158=CARTESIAN_POINT('Ctrl Pts',(-22.0589636608176,27.3572564722562,-36.6908937070762));
#70159=CARTESIAN_POINT('Ctrl Pts',(-25.9470439668104,26.862745900202,-36.4920067957014));
#70160=CARTESIAN_POINT('Ctrl Pts',(-27.6326761583333,23.3243347756119,-36.2931198843265));
#70161=CARTESIAN_POINT('Ctrl Pts',(-25.5669071694184,19.9935229141944,-36.0942329729517));
#70162=CARTESIAN_POINT('Ctrl Pts',(-21.6480035525516,19.9310440103175,-35.8953460615767));
#70163=CARTESIAN_POINT('Ctrl Pts',(-19.4771054634003,23.1943108793065,-35.6964591502018));
#70164=CARTESIAN_POINT('Ctrl Pts',(-21.0490841840901,26.7846579479644,-35.4975722388269));
#70165=CARTESIAN_POINT('Ctrl Pts',(-24.9194245521232,27.4028606714261,-35.2986853274521));
#70166=CARTESIAN_POINT('Ctrl Pts',(-27.5316119200257,24.4808431617777,-35.0997984160771));
#70167=CARTESIAN_POINT('Ctrl Pts',(-26.4852675736608,20.7036917641565,-34.9009115047023));
#70168=CARTESIAN_POINT('Ctrl Pts',(-22.741893251967,19.5422883633496,-34.7020245933273));
#70169=CARTESIAN_POINT('Ctrl Pts',(-19.741332570778,22.0638642139288,-34.5031376819525));
#70170=CARTESIAN_POINT('Ctrl Pts',(-20.2408463905141,25.9513049035876,-34.3042507705776));
#70171=CARTESIAN_POINT('Ctrl Pts',(-23.7814238626257,27.6323820391462,-34.1053638592027));
#70172=CARTESIAN_POINT('Ctrl Pts',(-27.1095744817079,25.5623282648628,-33.9064769478278));
#70173=CARTESIAN_POINT('Ctrl Pts',(-27.1670100094627,21.643347487687,-33.7075900364529));
#70174=CARTESIAN_POINT('Ctrl Pts',(-23.9009520656134,19.4766507670683,-33.508703125078));
#70175=CARTESIAN_POINT('Ctrl Pts',(-20.3126309845092,21.0532486836677,-33.3098162137031));
#70176=CARTESIAN_POINT('Ctrl Pts',(-19.699409600229,24.92438142559,-33.1109293023283));
#70177=CARTESIAN_POINT('Ctrl Pts',(-22.6247863723266,27.5328062209393,-32.9120423909533));
#70178=CARTESIAN_POINT('Ctrl Pts',(-26.4005880782925,26.4816018407416,-32.7131554795785));
#70179=CARTESIAN_POINT('Ctrl Pts',(-27.5571730855357,22.7367359829647,-32.5142685682036));
#70180=CARTESIAN_POINT('Ctrl Pts',(-25.0317378346372,19.7394228586415,-32.3153816568287));
#70181=CARTESIAN_POINT('Ctrl Pts',(-21.1449431995737,20.24393909878,-32.1164947454538));
#70182=CARTESIAN_POINT('Ctrl Pts',(-19.4684239041284,23.786677054616,-31.9176078340789));
#70183=CARTESIAN_POINT('Ctrl Pts',(-21.54275903542,27.1121609193807,-31.718720922704));
#70184=CARTESIAN_POINT('Ctrl Pts',(-25.4618104824077,27.1645529758905,-31.5198340113291));
#70185=CARTESIAN_POINT('Ctrl Pts',(-27.6243022460767,23.8957093663268,-31.3209470999543));
#70186=CARTESIAN_POINT('Ctrl Pts',(-26.0430877446809,20.3094202156451,-31.1220601885793));
#70187=CARTESIAN_POINT('Ctrl Pts',(-22.1711690401219,19.701181186145,-30.9231732772045));
#70188=CARTESIAN_POINT('Ctrl Pts',(-19.5665111373198,22.6299123757717,-30.7242863658296));
#70189=CARTESIAN_POINT('Ctrl Pts',(-20.6225738103778,26.4043581367141,-30.5253994544547));
#70190=CARTESIAN_POINT('Ctrl Pts',(-24.3689250021044,27.5561228348926,-30.3265125430798));
#70191=CARTESIAN_POINT('Ctrl Pts',(-27.362985605503,25.0268323662238,-30.1276256317049));
#70192=CARTESIAN_POINT('Ctrl Pts',(-26.8534677805267,21.1406902229469,-29.92873872033));
#70193=CARTESIAN_POINT('Ctrl Pts',(-23.3085752083413,19.4687315442152,-29.7298518089551));
#70194=CARTESIAN_POINT('Ctrl Pts',(-19.9857636054592,21.5473445970642,-29.5309648975802));
#70195=CARTESIAN_POINT('Ctrl Pts',(-19.9384151069646,25.4664602232498,-29.3320779862053));
#70196=CARTESIAN_POINT('Ctrl Pts',(-23.2100389684831,27.6247434485159,-29.1331910748305));
#70197=CARTESIAN_POINT('Ctrl Pts',(-26.7942902492392,26.0389149810833,-28.9343041634555));
#70198=CARTESIAN_POINT('Ctrl Pts',(-27.3975459166122,22.1662167264417,-28.7354172520807));
#70199=CARTESIAN_POINT('Ctrl Pts',(-24.4654651599321,19.5653300299422,-28.5365303407058));
#70200=CARTESIAN_POINT('Ctrl Pts',(-20.6923815951358,20.6262492468413,-28.3376434293309));
#70201=CARTESIAN_POINT('Ctrl Pts',(-19.5454391135397,24.3740795679248,-28.138756517956));
#70202=CARTESIAN_POINT('Ctrl Pts',(-22.0785806110445,27.3648826917262,-27.9398696065811));
#70203=CARTESIAN_POINT('Ctrl Pts',(-25.9640638264242,26.85036412576,-27.7409826952062));
#70204=CARTESIAN_POINT('Ctrl Pts',(-27.6314591193952,23.3033228081687,-27.5420957838313));
#70205=CARTESIAN_POINT('Ctrl Pts',(-25.5485715875246,19.9831889703093,-27.3432088724564));
#70206=CARTESIAN_POINT('Ctrl Pts',(-21.6293982728614,19.9408841082468,-27.1443219610815));
#70207=CARTESIAN_POINT('Ctrl Pts',(-19.4753271604816,23.215282803356,-26.9454350497067));
#70208=CARTESIAN_POINT('Ctrl Pts',(-21.0657669675498,26.7974902780584,-26.7465481383317));
#70209=CARTESIAN_POINT('Ctrl Pts',(-24.9392383584286,27.3957615842105,-26.5476612269569));
#70210=CARTESIAN_POINT('Ctrl Pts',(-27.5363495411159,24.4603361165003,-26.3487743155819));
#70211=CARTESIAN_POINT('Ctrl Pts',(-26.4705755374379,20.6886209967165,-26.1498874042071));
#70212=CARTESIAN_POINT('Ctrl Pts',(-22.7212722940406,19.546502631234,-25.9510004928322));
#70213=CARTESIAN_POINT('Ctrl Pts',(-19.7337316031135,22.0834909622628,-25.7521135814573));
#70214=CARTESIAN_POINT('Ctrl Pts',(-20.2532500579395,25.9683088147261,-25.5532266700824));
#70215=CARTESIAN_POINT('Ctrl Pts',(-23.8024342464345,27.6311379604468,-25.3543397587075));
#70216=CARTESIAN_POINT('Ctrl Pts',(-27.1198848205667,25.5439793991697,-25.1554528473327));
#70217=CARTESIAN_POINT('Ctrl Pts',(-27.1571459761329,21.6247548868448,-24.9565659359577));
#70218=CARTESIAN_POINT('Ctrl Pts',(-23.8799778703928,19.4748994548584,-24.7576790245828));
#70219=CARTESIAN_POINT('Ctrl Pts',(-20.2998201344873,21.0699479675242,-24.558792113208));
#70220=CARTESIAN_POINT('Ctrl Pts',(-19.7065341803949,24.9441860795144,-24.3599052018331));
#70221=CARTESIAN_POINT('Ctrl Pts',(-22.6452994975725,27.537517447133,-24.1610182904582));
#70222=CARTESIAN_POINT('Ctrl Pts',(-26.415639925744,26.4668904217786,-23.9621313790834));
#70223=CARTESIAN_POINT('Ctrl Pts',(-27.5529322835708,22.7161204655495,-23.7632444677084));
#70224=CARTESIAN_POINT('Ctrl Pts',(-25.0121013207012,19.7318471553711,-23.5643575563335));
#70225=CARTESIAN_POINT('Ctrl Pts',(-21.1279552650718,20.256364638646,-23.3654706449586));
#70226=CARTESIAN_POINT('Ctrl Pts',(-19.4696950205286,23.8076858199938,-23.1665837335838));
#70227=CARTESIAN_POINT('Ctrl Pts',(-21.5611211545233,27.1224476361376,-22.9676968222088));
#70228=CARTESIAN_POINT('Ctrl Pts',(-25.4803903736092,27.1546650234968,-22.768809910834));
#70229=CARTESIAN_POINT('Ctrl Pts',(-27.626026564677,23.8747329346722,-22.569922999459));
#70230=CARTESIAN_POINT('Ctrl Pts',(-26.0263719880847,20.2966308669121,-22.3710360880842));
#70231=CARTESIAN_POINT('Ctrl Pts',(-22.1513735713785,19.7083312474613,-22.1721491767093));
#70232=CARTESIAN_POINT('Ctrl Pts',(-19.5618263138254,22.6504315470131,-21.9732622653344));
#70233=CARTESIAN_POINT('Ctrl Pts',(-20.6373045877163,26.4193910392483,-21.7743753539595));
#70234=CARTESIAN_POINT('Ctrl Pts',(-24.3895350448656,27.5518555058708,-21.5754884425846));
#70235=CARTESIAN_POINT('Ctrl Pts',(-27.3705360318328,25.0071861192072,-21.3766015312098));
#70236=CARTESIAN_POINT('Ctrl Pts',(-26.8410203887985,21.1237182932167,-21.1777146198348));
#70237=CARTESIAN_POINT('Ctrl Pts',(-23.2875680961884,19.470029696211,-20.97882770846));
#70238=CARTESIAN_POINT('Ctrl Pts',(-19.9755005278409,21.5657199391672,-20.779940797085));
#70239=CARTESIAN_POINT('Ctrl Pts',(-19.9483269620463,25.4850273740393,-20.5810538857102));
#70240=CARTESIAN_POINT('Ctrl Pts',(-23.2310176018315,27.6264407706511,-20.3821669743353));
#70241=CARTESIAN_POINT('Ctrl Pts',(-26.807058075502,26.0221827794312,-20.1832800629604));
#70242=CARTESIAN_POINT('Ctrl Pts',(-27.3903703859868,22.1464304756638,-19.9843931515855));
#70243=CARTESIAN_POINT('Ctrl Pts',(-24.4449399766786,19.560671616906,-19.7855062402106));
#70244=CARTESIAN_POINT('Ctrl Pts',(-20.6773676624156,20.6409993581589,-19.5866193288357));
#70245=CARTESIAN_POINT('Ctrl Pts',(-19.549732962551,24.3946841018984,-19.3877324174608));
#70246=CARTESIAN_POINT('Ctrl Pts',(-22.0982365586042,27.3724078286106,-19.1888455060859));
#70247=CARTESIAN_POINT('Ctrl Pts',(-25.9810197232746,26.837894902785,-18.9899585947111));
#70248=CARTESIAN_POINT('Ctrl Pts',(-27.6301339339536,23.2823173840323,-18.7910716833361));
#70249=CARTESIAN_POINT('Ctrl Pts',(-25.5301830528546,19.9729495488268,-18.5921847719613));
#70250=CARTESIAN_POINT('Ctrl Pts',(-21.6108438932343,19.9508198496008,-18.3932978605864));
#70251=CARTESIAN_POINT('Ctrl Pts',(-19.4736568376225,23.236263603654,-18.1944109492115));
#70252=CARTESIAN_POINT('Ctrl Pts',(-21.0825155865463,26.8102365607052,-17.9955240378366));
#70253=CARTESIAN_POINT('Ctrl Pts',(-24.9590153584717,27.3885605961603,-17.7966371264617));
#70254=CARTESIAN_POINT('Ctrl Pts',(-27.540981535979,24.4398049552278,-17.5977502150868));
#70255=CARTESIAN_POINT('Ctrl Pts',(-26.4558061165702,20.6736260586761,-17.3988633037119));
#70256=CARTESIAN_POINT('Ctrl Pts',(-22.7006733029792,19.5508229931235,-17.199976392337));
#70257=CARTESIAN_POINT('Ctrl Pts',(-19.7262317681373,22.1031565778123,-17.0010894809621));
#70258=CARTESIAN_POINT('Ctrl Pts',(-20.2657410915107,25.9852486506146,-16.8022025695872));
#70259=CARTESIAN_POINT('Ctrl Pts',(-23.8234379477659,27.6297857437541,-16.6033156582124));
#70260=CARTESIAN_POINT('Ctrl Pts',(-27.1301005689551,25.5255777023874,-16.4044287468375));
#70261=CARTESIAN_POINT('Ctrl Pts',(-27.1471863649619,21.6062133091092,-16.2055418354626));
#70262=CARTESIAN_POINT('Ctrl Pts',(-23.8589949378929,19.473256134042,-16.0066549240877));
#70263=CARTESIAN_POINT('Ctrl Pts',(-20.2870954165664,21.0867129761265,-15.8077680127128));
#70264=CARTESIAN_POINT('Ctrl Pts',(-19.7137606139441,24.9639537960686,-15.6088811013379));
#70265=CARTESIAN_POINT('Ctrl Pts',(-22.665836602861,27.5421230161513,-15.409994189963));
#70266=CARTESIAN_POINT('Ctrl Pts',(-26.4306158442705,26.4521017158213,-15.2111072785881));
#70267=CARTESIAN_POINT('Ctrl Pts',(-27.5485854159584,22.6955270515157,-15.0122203672132));
#70268=CARTESIAN_POINT('Ctrl Pts',(-24.9924260697318,19.7243726347242,-14.8133334558383));
#70269=CARTESIAN_POINT('Ctrl Pts',(-21.1110315182003,20.2688774621258,-14.6144465444634));
#70270=CARTESIAN_POINT('Ctrl Pts',(-19.4710742662327,23.8286877637347,-14.4155596330886));
#70271=CARTESIAN_POINT('Ctrl Pts',(-21.5795359829419,27.132639694513,-14.2166727217137));
#70272=CARTESIAN_POINT('Ctrl Pts',(-25.4989191187454,27.1446815590036,-14.0177858103388));
#70273=CARTESIAN_POINT('Ctrl Pts',(-27.6276428807294,23.8537479047216,-13.8188988989639));
#70274=CARTESIAN_POINT('Ctrl Pts',(-26.0095906176419,20.2839277347915,-13.620011987589));
#70275=CARTESIAN_POINT('Ctrl Pts',(-22.1316151710521,19.7155831145417,-13.4211250762141));
#70276=CARTESIAN_POINT('Ctrl Pts',(-19.5572471782792,22.6709745623044,-13.2222381648392));
#70277=CARTESIAN_POINT('Ctrl Pts',(-20.6521125542706,26.4343479134584,-13.0233512534643));
#70278=CARTESIAN_POINT('Ctrl Pts',(-24.4101228477655,27.5474821397344,-12.8244643420894));
#70279=CARTESIAN_POINT('Ctrl Pts',(-27.3779852257712,24.9875012654034,-12.6255774307145));
#70280=CARTESIAN_POINT('Ctrl Pts',(-26.8284857961336,21.1068106633908,-12.4266905193396));
#70281=CARTESIAN_POINT('Ctrl Pts',(-23.266567944821,19.4714359686424,-12.2278036079647));
#70282=CARTESIAN_POINT('Ctrl Pts',(-19.9653321763585,21.5841478687237,-12.0289166965899));
#70283=CARTESIAN_POINT('Ctrl Pts',(-19.9583342633272,25.5035432558892,-11.830029785215));
#70284=CARTESIAN_POINT('Ctrl Pts',(-23.2520046944779,27.6280300792623,-11.6311428738401));
#70285=CARTESIAN_POINT('Ctrl Pts',(-26.8197396007837,26.0053850749412,-11.4322559624652));
#70286=CARTESIAN_POINT('Ctrl Pts',(-27.3830930973862,22.1266814242883,-11.2333690510903));
#70287=CARTESIAN_POINT('Ctrl Pts',(-24.4243910854073,19.5561189224158,-11.0344821397154));
#70288=CARTESIAN_POINT('Ctrl Pts',(-20.6624298572932,20.6558265607855,-10.8355952283405));
#70289=CARTESIAN_POINT('Ctrl Pts',(-19.5541328199681,24.4152662595675,-10.6367083169656));
#70290=CARTESIAN_POINT('Ctrl Pts',(-22.117930982641,27.3798316835035,-10.4378214055907));
#70291=CARTESIAN_POINT('Ctrl Pts',(-25.9979112080529,26.825338561694,-10.2389344942159));
#70292=CARTESIAN_POINT('Ctrl Pts',(-27.6287006371241,23.2613190598182,-10.040047582841));
#70293=CARTESIAN_POINT('Ctrl Pts',(-25.5117420526801,19.9628049210777,-9.84116067146604));
#70294=CARTESIAN_POINT('Ctrl Pts',(-21.5923409053361,19.9608509710958,-9.64227376009116));
#70295=CARTESIAN_POINT('Ctrl Pts',(-19.4720945390846,23.2572527242379,-9.44338684871627));
#70296=CARTESIAN_POINT('Ctrl Pts',(-21.099329597264,26.8228964581455,-9.24449993734137));
#70297=CARTESIAN_POINT('Ctrl Pts',(-24.9787550281883,27.3812578980914,-9.04561302596649));
#70298=CARTESIAN_POINT('Ctrl Pts',(-27.5455077818732,24.4192502220087,-8.84672611459159));
#70299=CARTESIAN_POINT('Ctrl Pts',(-26.4409597024275,20.6587073473808,-8.64783920321671));
#70300=CARTESIAN_POINT('Ctrl Pts',(-22.6800968246285,19.5552493345345,-8.44895229184182));
#70301=CARTESIAN_POINT('Ctrl Pts',(-19.7188332645852,22.1228605394645,-8.25006538046692));
#70302=CARTESIAN_POINT('Ctrl Pts',(-20.2783191602318,26.0021239623703,-8.05117846909204));
#70303=CARTESIAN_POINT('Ctrl Pts',(-23.8444344100502,27.6283254249002,-7.85229155771715));
#70304=CARTESIAN_POINT('Ctrl Pts',(-27.1402214561694,25.507123662136,-7.65340464634224));
#70305=CARTESIAN_POINT('Ctrl Pts',(-27.1371314398662,21.5877232458067,-7.45451773496737));
#70306=CARTESIAN_POINT('Ctrl Pts',(-23.8380038241329,19.4717208481646,-7.25563082359246));
#70307=CARTESIAN_POINT('Ctrl Pts',(-20.2744571679346,21.1035432652248,-7.05674391221759));
#70308=CARTESIAN_POINT('Ctrl Pts',(-19.7210887093864,24.9836840514344,-6.85785700084268));
#70309=CARTESIAN_POINT('Ctrl Pts',(-22.6863971439858,27.5466228059533,-6.65897008946781));
#70310=CARTESIAN_POINT('Ctrl Pts',(-26.4455154370305,26.4372361147506,-6.4600831780929));
#70311=CARTESIAN_POINT('Ctrl Pts',(-27.5441325978844,22.6749562865615,-6.26119626671804));
#70312=CARTESIAN_POINT('Ctrl Pts',(-24.9727126030969,19.7169994947659,-6.06230935534312));
#70313=CARTESIAN_POINT('Ctrl Pts',(-21.0941724074158,20.2814772376461,-5.86342244396824));
#70314=CARTESIAN_POINT('Ctrl Pts',(-19.4725616046925,23.8496823293152,-5.66453553259335));
#70315=CARTESIAN_POINT('Ctrl Pts',(-21.598003032707,27.1427368244307,-5.46564862121845));
#70316=CARTESIAN_POINT('Ctrl Pts',(-25.5173962268293,27.1346028469598,-5.26676170984357));
#70317=CARTESIAN_POINT('Ctrl Pts',(-27.6291511514034,23.8327548325505,-5.06787479846868));
#70318=CARTESIAN_POINT('Ctrl Pts',(-25.9927440780369,20.2713111558993,-4.86898788709378));
#70319=CARTESIAN_POINT('Ctrl Pts',(-22.111894362714,19.7229365952208,-4.6701009757189));
#70320=CARTESIAN_POINT('Ctrl Pts',(-19.552773852022,22.6915408772831,-4.471214064344));
#70321=CARTESIAN_POINT('Ctrl Pts',(-20.6669973176491,26.4492283630071,-4.27232715296912));
#70322=CARTESIAN_POINT('Ctrl Pts',(-24.4306878652549,27.5430028523719,-4.07344024159422));
#70323=CARTESIAN_POINT('Ctrl Pts',(-27.3853329899243,24.9677783264349,-3.87455333021934));
#70324=CARTESIAN_POINT('Ctrl Pts',(-26.8158643346817,21.0899677814989,-3.67566641884444));
#70325=CARTESIAN_POINT('Ctrl Pts',(-23.2455753107149,19.4729503242449,-3.47677950746956));
#70326=CARTESIAN_POINT('Ctrl Pts',(-19.9552588204597,21.602627897418,-3.27789259609466));
#70327=CARTESIAN_POINT('Ctrl Pts',(-19.9684367456271,25.5220073781535,-3.07900568471977));
#70328=CARTESIAN_POINT('Ctrl Pts',(-23.272999690292,27.6295113322349,-2.88011877334488));
#70329=CARTESIAN_POINT('Ctrl Pts',(-26.8323344890412,25.98852231273,-2.68123186196999));
#70330=CARTESIAN_POINT('Ctrl Pts',(-27.3757142436486,22.106970095639,-2.4823449505951));
#70331=CARTESIAN_POINT('Ctrl Pts',(-24.4038190306359,19.5516720671119,-2.28345803922021));
#70332=CARTESIAN_POINT('Ctrl Pts',(-20.6475685756005,20.6707304618203,-2.08457112784532));
#70333=CARTESIAN_POINT('Ctrl Pts',(-19.5586385692006,24.4358254955324,-1.88568421647042));
#70334=CARTESIAN_POINT('Ctrl Pts',(-22.1376633612786,27.3871540596825,-1.68679730509554));
#70335=CARTESIAN_POINT('Ctrl Pts',(-26.0147378331575,26.8126954352138,-1.48791039372065));
#70336=CARTESIAN_POINT('Ctrl Pts',(-27.627159266887,23.2403283919536,-1.28902348234576));
#70337=CARTESIAN_POINT('Ctrl Pts',(-25.4932490756625,19.9527553558813,-1.09013657097086));
#70338=CARTESIAN_POINT('Ctrl Pts',(-21.5738897994712,19.9709772069203,-0.891249659595981));
#70339=CARTESIAN_POINT('Ctrl Pts',(-19.4706403062664,23.278249608924,-0.692362748221079));
#70340=CARTESIAN_POINT('Ctrl Pts',(-21.1162085541538,26.8354696349089,-0.493475836846195));
#70341=CARTESIAN_POINT('Ctrl Pts',(-24.9984568445039,27.3738536835161,-0.294588925471298));
#70342=CARTESIAN_POINT('Ctrl Pts',(-27.549928158859,24.3986724615157,-0.0957020140964179));
#70343=CARTESIAN_POINT('Ctrl Pts',(-26.4260366884199,20.6438652581567,0.103184897278475));
#70344=CARTESIAN_POINT('Ctrl Pts',(-22.6595434042374,19.5597815381747,0.30207180865337));
#70345=CARTESIAN_POINT('Ctrl Pts',(-19.7115362885075,22.1426023250911,0.500958720028255));
#70346=CARTESIAN_POINT('Ctrl Pts',(-20.2909839308012,26.0189343028199,0.699845631403148));
#70347=CARTESIAN_POINT('Ctrl Pts',(-23.865423076909,27.6267570425813,0.898732542778043));
#70348=CARTESIAN_POINT('Ctrl Pts',(-27.1502472140198,25.4886177674228,1.09761945415293));
#70349=CARTESIAN_POINT('Ctrl Pts',(-27.1269814672878,21.5692851868996,1.29650636552782));
#70350=CARTESIAN_POINT('Ctrl Pts',(-23.8170050853494,19.4702936379094,1.49539327690272));
#70351=CARTESIAN_POINT('Ctrl Pts',(-20.2619057234888,21.1204383888387,1.6942801882776));
#70352=CARTESIAN_POINT('Ctrl Pts',(-19.7285182725368,25.0033763227863,1.89316709965249));
#70353=CARTESIAN_POINT('Ctrl Pts',(-22.7069805761205,27.5510166973002,2.09205401102739));
#70354=CARTESIAN_POINT('Ctrl Pts',(-26.4603383092049,26.4222940124852,2.29094092240227));
#70355=CARTESIAN_POINT('Ctrl Pts',(-27.5395739473425,22.6544087157843,2.48982783377716));
#70356=CARTESIAN_POINT('Ctrl Pts',(-24.9529614431771,19.7097279308745,2.68871474515205));
#70357=CARTESIAN_POINT('Ctrl Pts',(-21.077378379462,20.2941636313296,2.88760165652695));
#70358=CARTESIAN_POINT('Ctrl Pts',(-19.4741569964957,23.8706689604074,3.08648856790183));
#70359=CARTESIAN_POINT('Ctrl Pts',(-21.6165218144668,27.1527387583308,3.28537547927672));
#70360=CARTESIAN_POINT('Ctrl Pts',(-25.5358212082423,27.1244291544376,3.48426239065162));
#70361=CARTESIAN_POINT('Ctrl Pts',(-27.6305513367319,23.8117542744471,3.68314930202651));
#70362=CARTESIAN_POINT('Ctrl Pts',(-25.9758328156801,20.2587814645581,3.88203621340138));
#70363=CARTESIAN_POINT('Ctrl Pts',(-22.0922116689392,19.7303914946417,4.08092312477631));
#70364=CARTESIAN_POINT('Ctrl Pts',(-19.5484064535911,22.7121299469694,4.27981003615117));
#70365=CARTESIAN_POINT('Ctrl Pts',(-20.6819584834256,26.4640319935825,4.47869694752607));
#70366=CARTESIAN_POINT('Ctrl Pts',(-24.451229552388,27.5384177624785,4.67758385890096));
#70367=CARTESIAN_POINT('Ctrl Pts',(-27.3925791295866,24.9480178249331,4.87647077027585));
#70368=CARTESIAN_POINT('Ctrl Pts',(-26.8031563388947,21.0731900938547,5.07535768165073));
#70369=CARTESIAN_POINT('Ctrl Pts',(-23.2245907501465,19.47457272289,5.27424459302565));
#70370=CARTESIAN_POINT('Ctrl Pts',(-19.9452807270751,21.6211595355544,5.47313150440051));
#70371=CARTESIAN_POINT('Ctrl Pts',(-19.9786341412437,25.5404192515574,5.67201841577542));
#70372=CARTESIAN_POINT('Ctrl Pts',(-23.294002032935,27.6308844903178,5.87090532715031));
#70373=CARTESIAN_POINT('Ctrl Pts',(-26.8448424065264,25.971594939638,6.06979223852519));
#70374=CARTESIAN_POINT('Ctrl Pts',(-27.3682340203038,22.0872970120394,6.26867914990007));
#70375=CARTESIAN_POINT('Ctrl Pts',(-24.3832243574966,19.54733116883,6.46756606127497));
#70376=CARTESIAN_POINT('Ctrl Pts',(-20.6327842111413,20.6857106663298,6.66645297264987));
#70377=CARTESIAN_POINT('Ctrl Pts',(-19.5632500908522,24.4563612650009,6.86533988402474));
#70378=CARTESIAN_POINT('Ctrl Pts',(-22.1574331716357,27.3943747631147,7.06422679539965));
#70379=CARTESIAN_POINT('Ctrl Pts',(-26.0314991527055,26.7999658583701,7.26311370677453));
#70380=CARTESIAN_POINT('Ctrl Pts',(-27.6255098640867,23.2193459366633,7.46200061814942));
#70381=CARTESIAN_POINT('Ctrl Pts',(-25.4747046118414,19.9428011195373,7.66088752952431));
#70382=CARTESIAN_POINT('Ctrl Pts',(-21.5554910645695,19.9811982887427,7.85977444089922));
#70383=CARTESIAN_POINT('Ctrl Pts',(-19.4692941777034,23.2992537013228,8.05866135227408));
#70384=CARTESIAN_POINT('Ctrl Pts',(-21.133152009946,26.8479557578229,8.257548263649));
#70385=CARTESIAN_POINT('Ctrl Pts',(-25.0181202853465,27.366348148636,8.45643517502387));
#70386=CARTESIAN_POINT('Ctrl Pts',(-27.5542425498025,24.3780722190318,8.65532208639878));
#70387=CARTESIAN_POINT('Ctrl Pts',(-26.4110374699872,20.6291001842993,8.85420899777365));
#70388=CARTESIAN_POINT('Ctrl Pts',(-22.6390135864442,19.5644194839469,9.05309590914856));
#70389=CARTESIAN_POINT('Ctrl Pts',(-19.7043410332642,22.1623814115612,9.25198282052343));
#70390=CARTESIAN_POINT('Ctrl Pts',(-20.3037350676194,26.0356792265119,9.45086973189833));
#70391=CARTESIAN_POINT('Ctrl Pts',(-23.8864033921708,27.6250806383578,9.64975664327322));
#70392=CARTESIAN_POINT('Ctrl Pts',(-27.1601775768371,25.4700605086295,9.84864355464811));
#70393=CARTESIAN_POINT('Ctrl Pts',(-27.1167367161873,21.5508996209716,10.047530466023));
#70394=CARTESIAN_POINT('Ctrl Pts',(-23.7959992779809,19.4689745410956,10.2464173773979));
#70395=CARTESIAN_POINT('Ctrl Pts',(-20.2494414158251,21.1373978992702,10.4453042887728));
#70396=CARTESIAN_POINT('Ctrl Pts',(-19.7360491065219,25.0230300883058,10.6441912001477));
#70397=CARTESIAN_POINT('Ctrl Pts',(-22.7275863538313,27.5553045737599,10.8430781115225));
#70398=CARTESIAN_POINT('Ctrl Pts',(-26.4750840680073,26.4072758049705,11.0419650228975));
#70399=CARTESIAN_POINT('Ctrl Pts',(-27.534909585131,22.6338848836673,11.2408519342723));
#70400=CARTESIAN_POINT('Ctrl Pts',(-24.9331731133515,19.7025581357365,11.4397388456472));
#70401=CARTESIAN_POINT('Ctrl Pts',(-21.0606498793582,20.3069363070043,11.6386257570221));
#70402=CARTESIAN_POINT('Ctrl Pts',(-19.4758603993663,23.8916471008938,11.837512668397));
#70403=CARTESIAN_POINT('Ctrl Pts',(-21.6350918374984,27.1626452311751,12.0363995797719));
#70404=CARTESIAN_POINT('Ctrl Pts',(-25.5541935747473,27.1141607510261,12.2352864911468));
#70405=CARTESIAN_POINT('Ctrl Pts',(-27.6318433996117,23.790746786898,12.4341734025216));
#70406=CARTESIAN_POINT('Ctrl Pts',(-25.9588572786975,20.2463389927879,12.6330603138966));
#70407=CARTESIAN_POINT('Ctrl Pts',(-22.0725676112927,19.7379476152593,12.8319472252714));
#70408=CARTESIAN_POINT('Ctrl Pts',(-19.5441450987166,22.7327412257809,13.0308341366463));
#70409=CARTESIAN_POINT('Ctrl Pts',(-20.6969956551495,26.4787584129081,13.2297210480212));
#70410=CARTESIAN_POINT('Ctrl Pts',(-24.4717473648378,27.5337269915527,13.4286079593961));
#70411=CARTESIAN_POINT('Ctrl Pts',(-27.3997234527448,24.9282202845247,13.627494870771));
#70412=CARTESIAN_POINT('Ctrl Pts',(-26.7903621455173,21.0564780450445,13.8263817821459));
#70413=CARTESIAN_POINT('Ctrl Pts',(-23.203614819179,19.4763031215864,14.0252686935208));
#70414=CARTESIAN_POINT('Ctrl Pts',(-19.9353981606106,21.639742292069,14.2241556048957));
#70415=CARTESIAN_POINT('Ctrl Pts',(-19.9889261799598,25.5587783882113,14.4230425162706));
#70416=CARTESIAN_POINT('Ctrl Pts',(-23.3150111658725,27.632149517124,14.6219294276455));
#70417=CARTESIAN_POINT('Ctrl Pts',(-26.8572630217964,25.9546034042184,14.8208163390203));
#70418=CARTESIAN_POINT('Ctrl Pts',(-27.3606526255678,22.0676626947997,15.0197032503953));
#70419=CARTESIAN_POINT('Ctrl Pts',(-24.3626076117206,19.5430963425982,15.2185901617701));
#70420=CARTESIAN_POINT('Ctrl Pts',(-20.6180771556817,20.7007667773587,15.417477073145));
#70421=CARTESIAN_POINT('Ctrl Pts',(-19.5679672627237,24.4768730238026,15.6163639845199));
#70422=CARTESIAN_POINT('Ctrl Pts',(-22.1772398898387,27.4014936024608,15.8152508958948));
#70423=CARTESIAN_POINT('Ctrl Pts',(-26.048194722544,26.7871501684795,16.0141378072697));
#70424=CARTESIAN_POINT('Ctrl Pts',(-27.6237524724303,23.1983722499541,16.2130247186446));
#70425=CARTESIAN_POINT('Ctrl Pts',(-25.4561091526197,19.9329424758199,16.4119116300195));
#70426=CARTESIAN_POINT('Ctrl Pts',(-21.5371451881725,19.9915139457182,16.6107985413944));
#70427=CARTESIAN_POINT('Ctrl Pts',(-19.468056189066,23.3202644448542,16.8096854527693));
#70428=CARTESIAN_POINT('Ctrl Pts',(-21.1501595156618,26.8603544960221,17.0085723641442));
#70429=CARTESIAN_POINT('Ctrl Pts',(-25.0377448296613,27.3587414923376,17.207459275519));
#70430=CARTESIAN_POINT('Ctrl Pts',(-27.558450840378,24.3574500404358,17.4063461868939));
#70431=CARTESIAN_POINT('Ctrl Pts',(-26.3959624445887,20.6144125170631,17.6052330982688));
#70432=CARTESIAN_POINT('Ctrl Pts',(-22.6185079152614,19.5691630489516,17.8041200096437));
#70433=CARTESIAN_POINT('Ctrl Pts',(-19.69724768952,22.1821972747556,18.0030069210186));
#70434=CARTESIAN_POINT('Ctrl Pts',(-20.3165722327983,26.0523582897283,18.2018938323935));
#70435=CARTESIAN_POINT('Ctrl Pts',(-23.9073747998855,27.6232962566519,18.4007807437684));
#70436=CARTESIAN_POINT('Ctrl Pts',(-27.17001228148,25.4514523774982,18.5996676551433));
#70437=CARTESIAN_POINT('Ctrl Pts',(-27.1063974580369,21.5325670352153,18.7985545665182));
#70438=CARTESIAN_POINT('Ctrl Pts',(-23.7749869586531,19.4677635926774,18.9974414778931));
#70439=CARTESIAN_POINT('Ctrl Pts',(-20.2370645752311,21.1544213471147,19.1963283892679));
#70440=CARTESIAN_POINT('Ctrl Pts',(-19.7436810117847,25.0426448271945,19.3952153006428));
#70441=CARTESIAN_POINT('Ctrl Pts',(-22.7482139310932,27.5594863217094,19.5941022120177));
#70442=CARTESIAN_POINT('Ctrl Pts',(-26.4897523226947,26.3921818901693,19.7929891233926));
#70443=CARTESIAN_POINT('Ctrl Pts',(-27.5301396348492,22.6133853340644,19.9918760347675));
#70444=CARTESIAN_POINT('Ctrl Pts',(-24.9133481379843,19.6954902993422,20.1907629461424));
#70445=CARTESIAN_POINT('Ctrl Pts',(-21.0439873503875,20.319794926211,20.3896498575173));
#70446=CARTESIAN_POINT('Ctrl Pts',(-19.4776717681664,23.9126161948818,20.5885367688922));
#70447=CARTESIAN_POINT('Ctrl Pts',(-21.6537126097211,27.1724559804553,20.787423680267));
#70448=CARTESIAN_POINT('Ctrl Pts',(-25.5725128395008,27.1037979088245,20.986310591642));
#70449=CARTESIAN_POINT('Ctrl Pts',(-27.6330273058053,23.7697329265736,21.1851975030168));
#70450=CARTESIAN_POINT('Ctrl Pts',(-25.9418179169176,20.2339840702973,21.3840844143918));
#70451=CARTESIAN_POINT('Ctrl Pts',(-22.0529627103157,19.7456047568468,21.5829713257666));
#70452=CARTESIAN_POINT('Ctrl Pts',(-19.5399899003186,22.7533741675459,21.7818582371415));
#70453=CARTESIAN_POINT('Ctrl Pts',(-20.7121084343556,26.4934072307538,21.9807451485164));
#70454=CARTESIAN_POINT('Ctrl Pts',(-24.4922407589099,27.5289306638937,22.1796320598913));
#70455=CARTESIAN_POINT('Ctrl Pts',(-27.4067657700838,24.908386229818,22.3785189712661));
#70456=CARTESIAN_POINT('Ctrl Pts',(-26.777482093579,21.0398320779155,22.5774058826411));
#70457=CARTESIAN_POINT('Ctrl Pts',(-23.1826480736459,19.4781414744804,22.776292794016));
#70458=CARTESIAN_POINT('Ctrl Pts',(-19.9256113829413,21.658375674545,22.9751797053909));
#70459=CARTESIAN_POINT('Ctrl Pts',(-19.9993125890499,25.5770843016201,23.1740666167658));
#70460=CARTESIAN_POINT('Ctrl Pts',(-23.3360265323915,27.6333063791363,23.3729535281406));
#70461=CARTESIAN_POINT('Ctrl Pts',(-26.8695960057205,25.9375481567157,23.5718404395156));
#70462=CARTESIAN_POINT('Ctrl Pts',(-27.3529702603396,22.0480676642185,23.7707273508904));
#70463=CARTESIAN_POINT('Ctrl Pts',(-24.3419693396195,19.538967700605,23.9696142622654));
#70464=CARTESIAN_POINT('Ctrl Pts',(-20.6034477989471,20.7158983959945,24.1685011736402));
#70465=CARTESIAN_POINT('Ctrl Pts',(-19.5727899598007,24.4973602283013,24.3673880850151));
#70466=CARTESIAN_POINT('Ctrl Pts',(-22.1970829910656,27.4085103892746,24.56627499639));
#70467=CARTESIAN_POINT('Ctrl Pts',(-26.0648241002076,26.7742487047758,24.7651619077649));
#70468=CARTESIAN_POINT('Ctrl Pts',(-27.6218871385914,23.1774078882897,24.9640488191398));
#70469=CARTESIAN_POINT('Ctrl Pts',(-25.4374631905537,19.9231796846686,25.1629357305147));
#70470=CARTESIAN_POINT('Ctrl Pts',(-21.5188526567968,20.0019239069524,25.3618226418895));
#70471=CARTESIAN_POINT('Ctrl Pts',(-19.4669263724509,23.3412812781227,25.5607095532645));
#70472=CARTESIAN_POINT('Ctrl Pts',(-21.1672306219631,26.8726655297157,25.7595964646393));
#70473=CARTESIAN_POINT('Ctrl Pts',(-25.057329954898,27.3510338996482,25.9584833760142));
#70474=CARTESIAN_POINT('Ctrl Pts',(-27.5625529238418,24.3368065034171,26.1573702873891));
#70475=CARTESIAN_POINT('Ctrl Pts',(-26.3808120026847,20.5998025866847,26.356257198764));
#70476=CARTESIAN_POINT('Ctrl Pts',(-22.5980269510697,19.5740122188322,26.5551441101389));
#70477=CARTESIAN_POINT('Ctrl Pts',(-19.6902564131246,22.2020491793454,26.7540310215138));
#70478=CARTESIAN_POINT('Ctrl Pts',(-20.3294951468089,26.0689714474631,26.9529179328886));
#70479=CARTESIAN_POINT('Ctrl Pts',(-23.9283366298413,27.6214031951935,27.1518048442636));
#70480=CARTESIAN_POINT('Ctrl Pts',(-27.179751283537,25.4327952824294,27.3506917556384));
#70481=CARTESIAN_POINT('Ctrl Pts',(-27.0959635585929,21.5142852430269,27.5495786670134));
#70482=CARTESIAN_POINT('Ctrl Pts',(-23.7539694549667,19.4666658707645,27.7484655783882));
#70483=CARTESIAN_POINT('Ctrl Pts',(-20.2247740742439,21.1714987533596,27.9473524897632));
#70484=CARTESIAN_POINT('Ctrl Pts',(-19.7514165342425,25.0622380103314,28.146239401138));
#70485=CARTESIAN_POINT('Ctrl Pts',(-22.7688575722315,27.5635278603232,28.3451263125129));
#70486=CARTESIAN_POINT('Ctrl Pts',(-26.5043524826052,26.377076810523,28.5440132238879));
#70487=CARTESIAN_POINT('Ctrl Pts',(-27.5252457221917,22.5927894947073,28.7429001352627));
#70488=CARTESIAN_POINT('Ctrl Pts',(-24.8935219757889,19.6887533114419,28.9417870466376));
#70489=CARTESIAN_POINT('Ctrl Pts',(-21.0273252703961,20.3323072149201,29.1406739580125));
#70490=CARTESIAN_POINT('Ctrl Pts',(-19.4797156270952,23.9343920538674,29.3395608693874));
#70491=CARTESIAN_POINT('Ctrl Pts',(-21.6721482617318,27.1806228264275,29.5384477807623));
#70492=CARTESIAN_POINT('Ctrl Pts',(-25.5912242703431,27.0963164159434,29.7373346921371));
#70493=CARTESIAN_POINT('Ctrl Pts',(-27.63368882695,23.7419436154583,29.9362644892681));
#70494=CARTESIAN_POINT('Ctrl Pts',(-26.4947738687757,21.4036029661271,30.068898649274));
#70495=CARTESIAN_POINT('Ctrl Pts',(-25.5559209586874,20.7348455034229,30.1352371721549));
#70496=CARTESIAN_POINT('Ctrl Pts',(-25.1937408823974,26.8611697506233,-75.136612489095));
#70497=CARTESIAN_POINT('Ctrl Pts',(-26.2970650380044,26.3134966205244,-75.07031685197));
#70498=CARTESIAN_POINT('Ctrl Pts',(-27.8938315288374,24.0378889387849,-74.9377255777202));
#70499=CARTESIAN_POINT('Ctrl Pts',(-26.3051630684163,20.151456014636,-74.7388386663452));
#70500=CARTESIAN_POINT('Ctrl Pts',(-22.1814766999306,19.3993779713237,-74.5399517549704));
#70501=CARTESIAN_POINT('Ctrl Pts',(-19.3173747867214,22.4559707153929,-74.3410648435954));
#70502=CARTESIAN_POINT('Ctrl Pts',(-20.3419839806973,26.5210641768467,-74.1421779322206));
#70503=CARTESIAN_POINT('Ctrl Pts',(-24.3152194831348,27.8546762011371,-73.9432910208456));
#70504=CARTESIAN_POINT('Ctrl Pts',(-27.5852507580641,25.2337121388997,-73.7444041094708));
#70505=CARTESIAN_POINT('Ctrl Pts',(-27.1476008207659,21.065354934915,-73.5455171980958));
#70506=CARTESIAN_POINT('Ctrl Pts',(-23.4042186429317,19.1806391005653,-73.346630286721));
#70507=CARTESIAN_POINT('Ctrl Pts',(-19.7950685065841,21.3111051035031,-73.1477433753461));
#70508=CARTESIAN_POINT('Ctrl Pts',(-19.6365932997354,25.4992225805698,-72.9488564639712));
#70509=CARTESIAN_POINT('Ctrl Pts',(-23.0744501205458,27.8963674907323,-72.7499695525964));
#70510=CARTESIAN_POINT('Ctrl Pts',(-26.9495231811252,26.2998194285406,-72.5510826412214));
#70511=CARTESIAN_POINT('Ctrl Pts',(-27.7009578155723,22.1766428820113,-72.3521957298465));
#70512=CARTESIAN_POINT('Ctrl Pts',(-24.6382445793945,19.3157022412448,-72.1533088184717));
#70513=CARTESIAN_POINT('Ctrl Pts',(-20.5757597645979,20.3459515854474,-71.9544219070967));
#70514=CARTESIAN_POINT('Ctrl Pts',(-19.2465811483552,24.32068324995,-71.7555349957219));
#70515=CARTESIAN_POINT('Ctrl Pts',(-21.8721118853346,27.5874536484677,-71.5566480843469));
#70516=CARTESIAN_POINT('Ctrl Pts',(-26.039711464712,27.1443789201376,-71.3577611729721));
#70517=CARTESIAN_POINT('Ctrl Pts',(-27.9197094241392,23.3986065599842,-71.1588742615972));
#70518=CARTESIAN_POINT('Ctrl Pts',(-25.7845469321506,19.7921841029197,-70.9599873502223));
#70519=CARTESIAN_POINT('Ctrl Pts',(-21.5962573421921,19.6391078406365,-70.7611004388474));
#70520=CARTESIAN_POINT('Ctrl Pts',(-19.2035236497863,23.0800419706175,-70.5622135274725));
#70521=CARTESIAN_POINT('Ctrl Pts',(-20.8050652633841,26.953059722229,-70.3633266160976));
#70522=CARTESIAN_POINT('Ctrl Pts',(-24.9292012202206,27.6991861850648,-70.1644397047228));
#70523=CARTESIAN_POINT('Ctrl Pts',(-27.7862002493743,24.6327943873279,-69.9655527933478));
#70524=CARTESIAN_POINT('Ctrl Pts',(-26.7507224743231,20.5716384111603,-69.766665881973));
#70525=CARTESIAN_POINT('Ctrl Pts',(-22.7742841775203,19.2475762656173,-69.5677789705981));
#70526=CARTESIAN_POINT('Ctrl Pts',(-19.5108950067131,21.8773088025077,-69.3688920592232));
#70527=CARTESIAN_POINT('Ctrl Pts',(-19.9593329204414,26.0443347839142,-69.1700051478483));
#70528=CARTESIAN_POINT('Ctrl Pts',(-23.7075214970733,27.9195106390288,-68.9711182364735));
#70529=CARTESIAN_POINT('Ctrl Pts',(-27.3111932287642,25.7797087453964,-68.7722313250984));
#70530=CARTESIAN_POINT('Ctrl Pts',(-27.4588793350163,21.5912256181414,-68.5733444137237));
#70531=CARTESIAN_POINT('Ctrl Pts',(-24.0148688059276,19.2029221263209,-68.3744575023486));
#70532=CARTESIAN_POINT('Ctrl Pts',(-20.1439153137772,20.8094466842194,-68.1755705909739));
#70533=CARTESIAN_POINT('Ctrl Pts',(-19.4030969151261,24.9345394339248,-67.9766836795989));
#70534=CARTESIAN_POINT('Ctrl Pts',(-22.4731629072885,27.7875898886589,-67.7777967682241));
#70535=CARTESIAN_POINT('Ctrl Pts',(-26.5329829421399,26.7468865793022,-67.5789098568492));
#70536=CARTESIAN_POINT('Ctrl Pts',(-27.851926623626,22.768747610067,-67.3800229454743));
#70537=CARTESIAN_POINT('Ctrl Pts',(-25.2179965364443,19.5087454031162,-67.1811360340994));
#70538=CARTESIAN_POINT('Ctrl Pts',(-21.0515511102707,19.9625455840323,-66.9822491227245));
#70539=CARTESIAN_POINT('Ctrl Pts',(-19.1812004354411,23.7131442624633,-66.7833622113496));
#70540=CARTESIAN_POINT('Ctrl Pts',(-21.3256382025381,27.3140592512587,-66.5844752999747));
#70541=CARTESIAN_POINT('Ctrl Pts',(-25.5143079219386,27.4563549829591,-66.3855883885999));
#70542=CARTESIAN_POINT('Ctrl Pts',(-27.8981772621405,24.0092737448201,-66.1867014772249));
#70543=CARTESIAN_POINT('Ctrl Pts',(-26.286672418287,20.1403909303993,-65.9878145658501));
#70544=CARTESIAN_POINT('Ctrl Pts',(-22.1606297088009,19.4048818189811,-65.7889276544751));
#70545=CARTESIAN_POINT('Ctrl Pts',(-19.3115325529678,22.4786169230698,-65.5900407431003));
#70546=CARTESIAN_POINT('Ctrl Pts',(-20.3574596733955,26.5370942917681,-65.3911538317254));
#70547=CARTESIAN_POINT('Ctrl Pts',(-24.3372927264065,27.8509173253781,-65.1922669203505));
#70548=CARTESIAN_POINT('Ctrl Pts',(-27.5939025704812,25.2127940498356,-64.9933800089756));
#70549=CARTESIAN_POINT('Ctrl Pts',(-27.1347408738959,21.0469360793963,-64.7944930976006));
#70550=CARTESIAN_POINT('Ctrl Pts',(-23.3817383053209,19.1814136823847,-64.5956061862259));
#70551=CARTESIAN_POINT('Ctrl Pts',(-19.7835860231326,21.3304837714386,-64.3967192748508));
#70552=CARTESIAN_POINT('Ctrl Pts',(-19.6466809016576,25.5193331458131,-64.1978323634761));
#70553=CARTESIAN_POINT('Ctrl Pts',(-23.0968271398913,27.8987643863169,-63.998945452101));
#70554=CARTESIAN_POINT('Ctrl Pts',(-26.9636328690584,26.2822819254272,-63.8000585407264));
#70555=CARTESIAN_POINT('Ctrl Pts',(-27.6938314751149,22.1552960895905,-63.6011716293512));
#70556=CARTESIAN_POINT('Ctrl Pts',(-24.6164323497271,19.3101569512449,-63.4022847179766));
#70557=CARTESIAN_POINT('Ctrl Pts',(-20.5593043687083,20.3613061505115,-63.2033978066015));
#70558=CARTESIAN_POINT('Ctrl Pts',(-19.2506041588886,24.3428266960193,-63.0045108952267));
#70559=CARTESIAN_POINT('Ctrl Pts',(-21.8929162536123,27.5960387837198,-62.8056239838518));
#70560=CARTESIAN_POINT('Ctrl Pts',(-26.0581798689496,27.131516331915,-62.6067370724768));
#70561=CARTESIAN_POINT('Ctrl Pts',(-27.9188708985218,23.3761160888048,-62.4078501611021));
#70562=CARTESIAN_POINT('Ctrl Pts',(-25.7651720467354,19.7807324723742,-62.208963249727));
#70563=CARTESIAN_POINT('Ctrl Pts',(-21.5761499548322,19.6492181878627,-62.0100763383523));
#70564=CARTESIAN_POINT('Ctrl Pts',(-19.2011607547684,23.1024237121637,-61.8111894269773));
#70565=CARTESIAN_POINT('Ctrl Pts',(-20.8226181555251,26.9671459519908,-61.6123025156025));
#70566=CARTESIAN_POINT('Ctrl Pts',(-24.9505402827237,27.6920328433528,-61.4134156042276));
#70567=CARTESIAN_POINT('Ctrl Pts',(-27.7917166915486,24.6109747933609,-61.2145286928527));
#70568=CARTESIAN_POINT('Ctrl Pts',(-26.7353471543245,20.5552029193142,-61.0156417814778));
#70569=CARTESIAN_POINT('Ctrl Pts',(-22.7521457103933,19.251627700714,-60.8167548701028));
#70570=CARTESIAN_POINT('Ctrl Pts',(-19.5023367669384,21.8981242385019,-60.6178679587281));
#70571=CARTESIAN_POINT('Ctrl Pts',(-19.9722192046344,26.062786600354,-60.418981047353));
#70572=CARTESIAN_POINT('Ctrl Pts',(-23.7300109027001,27.9186431808668,-60.2200941359784));
#70573=CARTESIAN_POINT('Ctrl Pts',(-27.3226198988076,25.7603191332387,-60.0212072246032));
#70574=CARTESIAN_POINT('Ctrl Pts',(-27.4487431285459,21.571131261538,-59.8223203132285));
#70575=CARTESIAN_POINT('Ctrl Pts',(-23.9924840372717,19.2005880352991,-59.6234334018534));
#70576=CARTESIAN_POINT('Ctrl Pts',(-20.1298516874202,20.8270176905143,-59.4245464904788));
#70577=CARTESIAN_POINT('Ctrl Pts',(-19.4102777112886,24.9558692725355,-59.2256595791036));
#70578=CARTESIAN_POINT('Ctrl Pts',(-22.4949895831295,27.7930782463697,-59.026772667729));
#70579=CARTESIAN_POINT('Ctrl Pts',(-26.549398633158,26.7314901207151,-58.8278857563539));
#70580=CARTESIAN_POINT('Ctrl Pts',(-27.8478467015968,22.7466143752181,-58.6289988449792));
#70581=CARTESIAN_POINT('Ctrl Pts',(-25.1971701037923,19.5002139582432,-58.4301119336041));
#70582=CARTESIAN_POINT('Ctrl Pts',(-21.0331158928126,19.975455603626,-58.2312250222293));
#70583=CARTESIAN_POINT('Ctrl Pts',(-19.1820968349725,23.7356325331063,-58.0323381108544));
#70584=CARTESIAN_POINT('Ctrl Pts',(-21.3450425038916,27.3254609589209,-57.8334511994795));
#70585=CARTESIAN_POINT('Ctrl Pts',(-25.5343892173839,27.4461929250044,-57.6345642881046));
#70586=CARTESIAN_POINT('Ctrl Pts',(-27.9004825437762,23.9868859909083,-57.4356773767298));
#70587=CARTESIAN_POINT('Ctrl Pts',(-26.2690833277458,20.126349928207,-57.2367904653548));
#70588=CARTESIAN_POINT('Ctrl Pts',(-22.1393091289809,19.4120900590421,-57.03790355398));
#70589=CARTESIAN_POINT('Ctrl Pts',(-19.3060722890367,22.5004506439263,-56.8390166426051));
#70590=CARTESIAN_POINT('Ctrl Pts',(-20.3728772449516,26.5534901551472,-56.6401297312301));
#70591=CARTESIAN_POINT('Ctrl Pts',(-24.3594206923845,27.8468089229745,-56.4412428198554));
#70592=CARTESIAN_POINT('Ctrl Pts',(-27.6024072062892,25.1919566551229,-56.2423559084803));
#70593=CARTESIAN_POINT('Ctrl Pts',(-27.1218071403008,21.0285174913962,-56.0434689971056));
#70594=CARTESIAN_POINT('Ctrl Pts',(-23.3592512068966,19.1823390218303,-55.8445820857305));
#70595=CARTESIAN_POINT('Ctrl Pts',(-19.7722092967397,21.3499027298354,-55.6456951743558));
#70596=CARTESIAN_POINT('Ctrl Pts',(-19.6568687942637,25.5394013468506,-55.4468082629808));
#70597=CARTESIAN_POINT('Ctrl Pts',(-23.1192178419824,27.9010408547444,-55.247921351606));
#70598=CARTESIAN_POINT('Ctrl Pts',(-26.9776512238312,26.2646747797727,-55.0490344402311));
#70599=CARTESIAN_POINT('Ctrl Pts',(-27.6865958030936,22.1339848038706,-54.8501475288562));
#70600=CARTESIAN_POINT('Ctrl Pts',(-24.5945916200155,19.3047247901372,-54.6512606174813));
#70601=CARTESIAN_POINT('Ctrl Pts',(-20.542928360123,20.3767448095026,-54.4523737061064));
#70602=CARTESIAN_POINT('Ctrl Pts',(-19.2547410348627,24.3649493564789,-54.2534867947315));
#70603=CARTESIAN_POINT('Ctrl Pts',(-21.9137645758749,27.6045165963777,-54.0545998833566));
#70604=CARTESIAN_POINT('Ctrl Pts',(-26.0765817969876,27.1185589057388,-53.8557129719818));
#70605=CARTESIAN_POINT('Ctrl Pts',(-27.9179166206944,23.3536301998417,-53.6568260606067));
#70606=CARTESIAN_POINT('Ctrl Pts',(-25.7457384634566,19.7693807460924,-53.457939149232));
#70607=CARTESIAN_POINT('Ctrl Pts',(-21.556094881439,19.6594318982475,-53.259052237857));
#70608=CARTESIAN_POINT('Ctrl Pts',(-19.1989131033193,23.1248173253513,-53.0601653264822));
#70609=CARTESIAN_POINT('Ctrl Pts',(-20.8402433271325,26.9811416361272,-52.8612784151072));
#70610=CARTESIAN_POINT('Ctrl Pts',(-24.9718422390485,27.6847697513548,-52.6623915037324));
#70611=CARTESIAN_POINT('Ctrl Pts',(-27.7971207408364,24.5891270909661,-52.4635045923575));
#70612=CARTESIAN_POINT('Ctrl Pts',(-26.7198874334676,20.5388467926438,-52.2646176809826));
#70613=CARTESIAN_POINT('Ctrl Pts',(-22.7300283920912,19.2557930434072,-52.0657307696078));
#70614=CARTESIAN_POINT('Ctrl Pts',(-19.4938857914712,21.9189834537864,-51.8668438582328));
#70615=CARTESIAN_POINT('Ctrl Pts',(-19.9852003019322,26.0811718379532,-51.6679569468579));
#70616=CARTESIAN_POINT('Ctrl Pts',(-23.7524955449617,27.9176599662382,-51.469070035483));
#70617=CARTESIAN_POINT('Ctrl Pts',(-27.333946606178,25.740870957263,-51.2701831241082));
#70618=CARTESIAN_POINT('Ctrl Pts',(-27.4385036172981,21.5510893490035,-51.0712962127331));
#70619=CARTESIAN_POINT('Ctrl Pts',(-23.9700875500751,19.198369204551,-50.8724093013584));
#70620=CARTESIAN_POINT('Ctrl Pts',(-20.1158786970995,20.8446608588845,-50.6735223899835));
#70621=CARTESIAN_POINT('Ctrl Pts',(-19.4175682112343,24.9771618641855,-50.4746354786085));
#70622=CARTESIAN_POINT('Ctrl Pts',(-22.516844222024,27.7984541748875,-50.2757485672338));
#70623=CARTESIAN_POINT('Ctrl Pts',(-26.565734850825,26.7160093635963,-50.0768616558588));
#70624=CARTESIAN_POINT('Ctrl Pts',(-27.8436528990832,22.7245024357032,-49.8779747444839));
#70625=CARTESIAN_POINT('Ctrl Pts',(-25.1763000300321,19.4917898339631,-49.6790878331089));
#70626=CARTESIAN_POINT('Ctrl Pts',(-21.0147473761012,19.9884603505462,-49.4802009217342));
#70627=CARTESIAN_POINT('Ctrl Pts',(-19.1831089847741,23.7581158914279,-49.2813140103592));
#70628=CARTESIAN_POINT('Ctrl Pts',(-21.3645052403547,27.3367626286208,-49.0824270989844));
#70629=CARTESIAN_POINT('Ctrl Pts',(-25.5544179358669,27.4359276298519,-48.8835401876094));
#70630=CARTESIAN_POINT('Ctrl Pts',(-27.9026725501486,23.9644866667952,-48.6846532762346));
#70631=CARTESIAN_POINT('Ctrl Pts',(-26.2514221918332,20.1123996548436,-48.4857663648597));
#70632=CARTESIAN_POINT('Ctrl Pts',(-22.1180259372698,19.4194079548613,-48.2868794534847));
#70633=CARTESIAN_POINT('Ctrl Pts',(-19.3007244901924,22.5223121831255,-48.08799254211));
#70634=CARTESIAN_POINT('Ctrl Pts',(-20.3883790126936,26.5698064367551,-47.8891056307349));
#70635=CARTESIAN_POINT('Ctrl Pts',(-24.381527216491,27.842586667586,-47.6902187193602));
#70636=CARTESIAN_POINT('Ctrl Pts',(-27.6108044654305,25.1710757574519,-47.4913318079851));
#70637=CARTESIAN_POINT('Ctrl Pts',(-27.1087787652961,21.010165725994,-47.2924448966104));
#70638=CARTESIAN_POINT('Ctrl Pts',(-23.3367691697513,19.1833801051285,-47.0935579852354));
#70639=CARTESIAN_POINT('Ctrl Pts',(-19.7609326834278,21.3693799945523,-46.8946710738606));
#70640=CARTESIAN_POINT('Ctrl Pts',(-19.6671598563197,25.5594168381109,-46.6957841624856));
#70641=CARTESIAN_POINT('Ctrl Pts',(-23.141619965915,27.9032020331139,-46.4968972511108));
#70642=CARTESIAN_POINT('Ctrl Pts',(-26.9915787571332,26.2469957055673,-46.2980103397358));
#70643=CARTESIAN_POINT('Ctrl Pts',(-27.6792505235205,22.1127110473469,-46.099123428361));
#70644=CARTESIAN_POINT('Ctrl Pts',(-24.572723216718,19.2994051298232,-45.900236516986));
#70645=CARTESIAN_POINT('Ctrl Pts',(-20.5266320415966,20.3922675621942,-45.7013496056113));
#70646=CARTESIAN_POINT('Ctrl Pts',(-19.2589917361332,24.3870504285648,-45.5024626942362));
#70647=CARTESIAN_POINT('Ctrl Pts',(-21.9346562628749,27.6128869764729,-45.3035757828615));
#70648=CARTESIAN_POINT('Ctrl Pts',(-26.0949167806869,27.105506924227,-45.1046888714865));
#70649=CARTESIAN_POINT('Ctrl Pts',(-27.9168466056238,23.3311495211067,-44.9058019601116));
#70650=CARTESIAN_POINT('Ctrl Pts',(-25.7262467027435,19.7581292078445,-44.7069150487368));
#70651=CARTESIAN_POINT('Ctrl Pts',(-21.5360926505501,19.6697487101633,-44.5080281373618));
#70652=CARTESIAN_POINT('Ctrl Pts',(-19.1967807565319,23.1472222120017,-44.309141225987));
#70653=CARTESIAN_POINT('Ctrl Pts',(-20.8579403103511,26.9950464063015,-44.110254314612));
#70654=CARTESIAN_POINT('Ctrl Pts',(-24.9931065251517,27.677397100193,-43.9113674032373));
#70655=CARTESIAN_POINT('Ctrl Pts',(-27.8024122538098,24.5672518597881,-43.7124804918622));
#70656=CARTESIAN_POINT('Ctrl Pts',(-26.7043437215347,20.5225704641884,-43.5135935804875));
#70657=CARTESIAN_POINT('Ctrl Pts',(-22.707932808629,19.2600721835198,-43.3147066691125));
#70658=CARTESIAN_POINT('Ctrl Pts',(-19.4855423042849,21.9398858955148,-43.1158197577376));
#70659=CARTESIAN_POINT('Ctrl Pts',(-19.998275868335,26.0994900095838,-42.9169328463627));
#70660=CARTESIAN_POINT('Ctrl Pts',(-23.7749748280544,27.9165610211672,-42.7180459349879));
#70661=CARTESIAN_POINT('Ctrl Pts',(-27.3451730507276,25.7213647328356,-42.5191590236129));
#70662=CARTESIAN_POINT('Ctrl Pts',(-27.4281610726089,21.5311004116133,-42.3202721122381));
#70663=CARTESIAN_POINT('Ctrl Pts',(-23.9476799378133,19.1962656928772,-42.1213852008632));
#70664=CARTESIAN_POINT('Ctrl Pts',(-20.1019967130816,20.8623757218069,-41.9224982894882));
#70665=CARTESIAN_POINT('Ctrl Pts',(-19.4249682217745,24.9984166446511,-41.7236113781134));
#70666=CARTESIAN_POINT('Ctrl Pts',(-22.5387262448534,27.8037175317566,-41.5247244667385));
#70667=CARTESIAN_POINT('Ctrl Pts',(-26.5819911622529,26.7004447181652,-41.3258375553636));
#70668=CARTESIAN_POINT('Ctrl Pts',(-27.8393453272154,22.7024123774587,-41.1269506439887));
#70669=CARTESIAN_POINT('Ctrl Pts',(-25.1553868681933,19.483473253504,-40.9280637326138));
#70670=CARTESIAN_POINT('Ctrl Pts',(-20.9964460468774,20.0015594801844,-40.729176821239));
#70671=CARTESIAN_POINT('Ctrl Pts',(-19.1842368580253,23.780593741649,-40.530289909864));
#70672=CARTESIAN_POINT('Ctrl Pts',(-21.3840258961909,27.3479639608791,-40.3314029984892));
#70673=CARTESIAN_POINT('Ctrl Pts',(-25.5743935466533,27.4255593695183,-40.1325160871142));
#70674=CARTESIAN_POINT('Ctrl Pts',(-27.904747223225,23.9420763660328,-39.9336291757394));
#70675=CARTESIAN_POINT('Ctrl Pts',(-26.2336894785457,20.0985404799728,-39.7347422643644));
#70676=CARTESIAN_POINT('Ctrl Pts',(-22.0967806976434,19.4268353125242,-39.5358553529896));
#70677=CARTESIAN_POINT('Ctrl Pts',(-19.2954892981446,22.5442009613658,-39.3369684416147));
#70678=CARTESIAN_POINT('Ctrl Pts',(-20.4039645658452,26.5860427042324,-39.1380815302399));
#70679=CARTESIAN_POINT('Ctrl Pts',(-24.4036117129327,27.8382506710969,-38.9391946188649));
#70680=CARTESIAN_POINT('Ctrl Pts',(-27.6190941253889,25.1501519101382,-38.7403077074901));
#70681=CARTESIAN_POINT('Ctrl Pts',(-27.0956560941167,20.9918812694871,-38.5414207961151));
#70682=CARTESIAN_POINT('Ctrl Pts',(-23.314292789629,19.184536904692,-38.3425338847403));
#70683=CARTESIAN_POINT('Ctrl Pts',(-19.7497564820121,21.3889150494678,-38.1436469733653));
#70684=CARTESIAN_POINT('Ctrl Pts',(-19.6775538151261,25.5793790892106,-37.9447600619905));
#70685=CARTESIAN_POINT('Ctrl Pts',(-23.1640329180628,27.9052478641569,-37.7458731506156));
#70686=CARTESIAN_POINT('Ctrl Pts',(-27.0054150999034,26.229245171283,-37.5469862392407));
#70687=CARTESIAN_POINT('Ctrl Pts',(-27.6717958310359,22.0914753837455,-37.3480993278658));
#70688=CARTESIAN_POINT('Ctrl Pts',(-24.5508277193181,19.294198111267,-37.1492124164908));
#70689=CARTESIAN_POINT('Ctrl Pts',(-20.5104158449599,20.4078739972541,-36.9503255051161));
#70690=CARTESIAN_POINT('Ctrl Pts',(-19.2633561500621,24.409129326628,-36.7514385937411));
#70691=CARTESIAN_POINT('Ctrl Pts',(-21.95559076101,27.6211497022014,-36.5525516823663));
#70692=CARTESIAN_POINT('Ctrl Pts',(-26.1131843341947,27.0923607332398,-36.3536647709913));
#70693=CARTESIAN_POINT('Ctrl Pts',(-27.9156608816637,23.3086746483078,-36.1547778596165));
#70694=CARTESIAN_POINT('Ctrl Pts',(-25.7066972811022,19.7469781557811,-35.9558909482416));
#70695=CARTESIAN_POINT('Ctrl Pts',(-21.5161437921982,19.6801683502284,-35.7570040368667));
#70696=CARTESIAN_POINT('Ctrl Pts',(-19.1947637709106,23.1696377784152,-35.5581171254918));
#70697=CARTESIAN_POINT('Ctrl Pts',(-20.8757086362342,27.008859894056,-35.3592302141169));
#70698=CARTESIAN_POINT('Ctrl Pts',(-25.0143325775584,27.6699150852328,-35.160343302742));
#70699=CARTESIAN_POINT('Ctrl Pts',(-27.8075910902507,24.5453496794914,-34.9614563913671));
#70700=CARTESIAN_POINT('Ctrl Pts',(-26.6887164304136,20.5063743652492,-34.7625694799922));
#70701=CARTESIAN_POINT('Ctrl Pts',(-22.6858595455104,19.2644650076606,-34.5636825686173));
#70702=CARTESIAN_POINT('Ctrl Pts',(-19.4773065264707,21.9608310098002,-34.3647956572424));
#70703=CARTESIAN_POINT('Ctrl Pts',(-20.0114455573576,26.1177406298384,-34.1659087458676));
#70704=CARTESIAN_POINT('Ctrl Pts',(-23.7974481563076,27.9153463747746,-33.9670218344926));
#70705=CARTESIAN_POINT('Ctrl Pts',(-27.3562989349707,25.7018009768453,-33.7681349231178));
#70706=CARTESIAN_POINT('Ctrl Pts',(-27.4177157685418,21.5111649790478,-33.5692480117429));
#70707=CARTESIAN_POINT('Ctrl Pts',(-23.9252617942581,19.1942775560179,-33.370361100368));
#70708=CARTESIAN_POINT('Ctrl Pts',(-20.0882061032203,20.8801618098615,-33.1714741889931));
#70709=CARTESIAN_POINT('Ctrl Pts',(-19.4324775468188,25.019633050709,-32.9725872776182));
#70710=CARTESIAN_POINT('Ctrl Pts',(-22.5606350717733,27.8088681775051,-32.7737003662433));
#70711=CARTESIAN_POINT('Ctrl Pts',(-26.5981671366712,26.6847965968643,-32.5748134548684));
#70712=CARTESIAN_POINT('Ctrl Pts',(-27.8349241001381,22.680344785842,-32.3759265434936));
#70713=CARTESIAN_POINT('Ctrl Pts',(-25.1344311724462,19.475264437244,-32.1770396321186));
#70714=CARTESIAN_POINT('Ctrl Pts',(-20.9782123901021,20.0147526454313,-31.9781527207438));
#70715=CARTESIAN_POINT('Ctrl Pts',(-19.1854804248391,23.8030654881368,-31.7792658093688));
#70716=CARTESIAN_POINT('Ctrl Pts',(-21.403603954129,27.3590646588755,-31.580378897994));
#70717=CARTESIAN_POINT('Ctrl Pts',(-25.5943155204161,27.4150884187485,-31.381491986619));
#70718=CARTESIAN_POINT('Ctrl Pts',(-27.9067065080293,23.9196556824641,-31.1826050752442));
#70719=CARTESIAN_POINT('Ctrl Pts',(-26.2158856577764,20.0847727708444,-30.9837181638693));
#70720=CARTESIAN_POINT('Ctrl Pts',(-22.0755739730722,19.4343719352159,-30.7848312524944));
#70721=CARTESIAN_POINT('Ctrl Pts',(-19.2903668516188,22.5661163986241,-30.5859443411196));
#70722=CARTESIAN_POINT('Ctrl Pts',(-20.4196334914102,26.6021985273398,-30.3870574297446));
#70723=CARTESIAN_POINT('Ctrl Pts',(-24.4256735965,27.8338010484055,-30.1881705183698));
#70724=CARTESIAN_POINT('Ctrl Pts',(-27.6272759664994,25.1291856676358,-29.9892836069948));
#70725=CARTESIAN_POINT('Ctrl Pts',(-27.0824394744957,20.9736646063891,-29.79039669562));
#70726=CARTESIAN_POINT('Ctrl Pts',(-23.2918226621234,19.1858093898673,-29.591509784245));
#70727=CARTESIAN_POINT('Ctrl Pts',(-19.7386809886471,21.4085073769292,-29.3926228728702));
#70728=CARTESIAN_POINT('Ctrl Pts',(-19.6880503952571,25.5992875711766,-29.1937359614953));
#70729=CARTESIAN_POINT('Ctrl Pts',(-23.1864561045126,27.9071782936616,-28.9948490501204));
#70730=CARTESIAN_POINT('Ctrl Pts',(-27.0191598854974,26.2114236472851,-28.7959621387456));
#70731=CARTESIAN_POINT('Ctrl Pts',(-27.6642319231788,22.0702783757829,-28.5970752273706));
#70732=CARTESIAN_POINT('Ctrl Pts',(-24.528905708017,19.2891038724476,-28.3981883159958));
#70733=CARTESIAN_POINT('Ctrl Pts',(-20.4942801999204,20.4235637011325,-28.1993014046208));
#70734=CARTESIAN_POINT('Ctrl Pts',(-19.2678341609985,24.4311854656078,-28.000414493246));
#70735=CARTESIAN_POINT('Ctrl Pts',(-21.9765675155443,27.6293045546121,-27.801527581871));
#70736=CARTESIAN_POINT('Ctrl Pts',(-26.1313839734455,27.0791206811336,-27.6026406704962));
#70737=CARTESIAN_POINT('Ctrl Pts',(-27.9143594802346,23.2862061769991,-27.4037537591212));
#70738=CARTESIAN_POINT('Ctrl Pts',(-25.6870907165655,19.7359278853903,-27.2048668477464));
#70739=CARTESIAN_POINT('Ctrl Pts',(-21.4962488350009,19.6906905423363,-27.0059799363715));
#70740=CARTESIAN_POINT('Ctrl Pts',(-19.1928621999026,23.1920634306094,-26.8070930249966));
#70741=CARTESIAN_POINT('Ctrl Pts',(-20.8935478339452,27.0225817333519,-26.6082061136217));
#70742=CARTESIAN_POINT('Ctrl Pts',(-25.0355198338064,27.6623239047374,-26.4093192022468));
#70743=CARTESIAN_POINT('Ctrl Pts',(-27.8126571129269,24.5234211304542,-26.2104322908719));
#70744=CARTESIAN_POINT('Ctrl Pts',(-26.6730059742064,20.4902589250009,-26.011545379497));
#70745=CARTESIAN_POINT('Ctrl Pts',(-22.6638091876472,19.2689713994255,-25.8126584681222));
#70746=CARTESIAN_POINT('Ctrl Pts',(-19.4691786762658,21.9818182416253,-25.6137715567472));
#70747=CARTESIAN_POINT('Ctrl Pts',(-20.024709020021,26.1359232151003,-25.4148846453724));
#70748=CARTESIAN_POINT('Ctrl Pts',(-23.8199149342081,27.9140160592465,-25.2159977339975));
#70749=CARTESIAN_POINT('Ctrl Pts',(-27.367323964086,25.6821802077056,-25.0171108226226));
#70750=CARTESIAN_POINT('Ctrl Pts',(-27.4071679818835,21.4912835795687,-24.8182239112477));
#70751=CARTESIAN_POINT('Ctrl Pts',(-23.9028337134602,19.1924048466563,-24.6193369998728));
#70752=CARTESIAN_POINT('Ctrl Pts',(-20.0745072329483,20.8980186517408,-24.4204500884979));
#70753=CARTESIAN_POINT('Ctrl Pts',(-19.4400959873801,25.0408105201528,-24.2215631771231));
#70754=CARTESIAN_POINT('Ctrl Pts',(-22.5825701222292,27.8139059756478,-24.0226762657481));
#70755=CARTESIAN_POINT('Ctrl Pts',(-26.6142623454384,26.6690654143477,-23.8237893543733));
#70756=CARTESIAN_POINT('Ctrl Pts',(-27.8303893350082,22.6583002456145,-23.6249024429983));
#70757=CARTESIAN_POINT('Ctrl Pts',(-25.1134334980889,19.4671636027058,-23.4260155316235));
#70758=CARTESIAN_POINT('Ctrl Pts',(-20.9600468889425,20.0280394966856,-23.2271286202485));
#70759=CARTESIAN_POINT('Ctrl Pts',(-19.1868396522625,23.8255305354201,-23.0282417088737));
#70760=CARTESIAN_POINT('Ctrl Pts',(-21.4232388953766,27.3700644284562,-22.8293547974988));
#70761=CARTESIAN_POINT('Ctrl Pts',(-25.6141833292499,27.4045150550087,-22.6304678861239));
#70762=CARTESIAN_POINT('Ctrl Pts',(-27.9085503526435,23.8972252102072,-22.431580974749));
#70763=CARTESIAN_POINT('Ctrl Pts',(-26.1980112013026,20.0710968922841,-22.2326940633741));
#70764=CARTESIAN_POINT('Ctrl Pts',(-22.0544063255061,19.4420176232257,-22.0338071519992));
#70765=CARTESIAN_POINT('Ctrl Pts',(-19.2853572863529,22.5880579141706,-21.8349202406243));
#70766=CARTESIAN_POINT('Ctrl Pts',(-20.4353853741828,26.6182734779693,-21.6360333292494));
#70767=CARTESIAN_POINT('Ctrl Pts',(-24.4477122825825,27.8292379174207,-21.4371464178746));
#70768=CARTESIAN_POINT('Ctrl Pts',(-27.6353497719544,25.1081775855218,-21.2382595064997));
#70769=CARTESIAN_POINT('Ctrl Pts',(-27.0691292566558,20.9555162194172,-21.0393725951248));
#70770=CARTESIAN_POINT('Ctrl Pts',(-23.2693593826632,19.1871975269351,-20.8404856837499));
#70771=CARTESIAN_POINT('Ctrl Pts',(-19.7277064968184,21.428156457766,-20.641598772375));
#70772=CARTESIAN_POINT('Ctrl Pts',(-19.6986493185672,25.6191417564607,-20.4427118610002));
#70773=CARTESIAN_POINT('Ctrl Pts',(-23.2088889310798,27.9089932704743,-20.2438249496252));
#70774=CARTESIAN_POINT('Ctrl Pts',(-27.0328127496967,26.1935316058201,-20.0449380382504));
#70775=CARTESIAN_POINT('Ctrl Pts',(-27.6565590003829,22.0491205851516,-19.8460511268754));
#70776=CARTESIAN_POINT('Ctrl Pts',(-24.5069577637188,19.2841225483553,-19.6471642155006));
#70777=CARTESIAN_POINT('Ctrl Pts',(-20.4782255340512,20.4393362580734,-19.4482773041257));
#70778=CARTESIAN_POINT('Ctrl Pts',(-19.2724256502808,24.4532182610454,-19.2493903927508));
#70779=CARTESIAN_POINT('Ctrl Pts',(-21.9975859706218,27.6373513176123,-19.0505034813759));
#70780=CARTESIAN_POINT('Ctrl Pts',(-26.1495152161732,27.0657871187522,-18.851616570001));
#70781=CARTESIAN_POINT('Ctrl Pts',(-27.9129424358214,23.2637447025648,-18.6527296586261));
#70782=CARTESIAN_POINT('Ctrl Pts',(-25.6674275286819,19.7249786894894,-18.4538427472512));
#70783=CARTESIAN_POINT('Ctrl Pts',(-21.4764083061483,19.7013150076628,-18.2549558358763));
#70784=CARTESIAN_POINT('Ctrl Pts',(-19.1910760938974,23.2144985743345,-18.0560689245014));
#70785=CARTESIAN_POINT('Ctrl Pts',(-20.9114574307693,27.0362115605785,-17.8571820131265));
#70786=CARTESIAN_POINT('Ctrl Pts',(-25.056667732462,27.6546237598632,-17.6582951017517));
#70787=CARTESIAN_POINT('Ctrl Pts',(-27.8176101875956,24.5014667937537,-17.4594081903767));
#70788=CARTESIAN_POINT('Ctrl Pts',(-26.6572127692192,20.4742245704813,-17.2605212790019));
#70789=CARTESIAN_POINT('Ctrl Pts',(-22.6417823193444,19.273591239401,-17.061634367627));
#70790=CARTESIAN_POINT('Ctrl Pts',(-19.461158969047,22.0028470348563,-16.8627474562521));
#70791=CARTESIAN_POINT('Ctrl Pts',(-20.0380659048616,26.1540372835553,-16.6638605448772));
#70792=CARTESIAN_POINT('Ctrl Pts',(-23.8423745664162,27.9125701098348,-16.4649736335023));
#70793=CARTESIAN_POINT('Ctrl Pts',(-27.3782478459255,25.6625029453405,-16.2660867221274));
#70794=CARTESIAN_POINT('Ctrl Pts',(-27.3965179921361,21.4714567400069,-16.0671998107525));
#70795=CARTESIAN_POINT('Ctrl Pts',(-23.8803962897337,19.1906476144163,-15.8683128993776));
#70796=CARTESIAN_POINT('Ctrl Pts',(-20.0609004652675,20.9159457742625,-15.6694259880027));
#70797=CARTESIAN_POINT('Ctrl Pts',(-19.44782334158,25.0619484918082,-15.4705390766279));
#70798=CARTESIAN_POINT('Ctrl Pts',(-22.6045308149718,27.8188307926899,-15.271652165253));
#70799=CARTESIAN_POINT('Ctrl Pts',(-26.6302763620529,26.6532515874704,-15.0727652538781));
#70800=CARTESIAN_POINT('Ctrl Pts',(-27.8257411519907,22.6362793409266,-14.8738783425032));
#70801=CARTESIAN_POINT('Ctrl Pts',(-25.0923944015314,19.4591709645508,-14.6749914311283));
#70802=CARTESIAN_POINT('Ctrl Pts',(-20.9419500247604,20.0414196818637,-14.4761045197534));
#70803=CARTESIAN_POINT('Ctrl Pts',(-19.1883145042778,23.8479882882055,-14.2772176083785));
#70804=CARTESIAN_POINT('Ctrl Pts',(-21.4429301996344,27.3809629781424,-14.0783306970036));
#70805=CARTESIAN_POINT('Ctrl Pts',(-25.6339964466844,27.3938395584788,-13.8794437856287));
#70806=CARTESIAN_POINT('Ctrl Pts',(-27.9102787082077,23.8747855436392,-13.6805568742538));
#70807=CARTESIAN_POINT('Ctrl Pts',(-26.1800665827734,20.0575132066841,-13.4816699628789));
#70808=CARTESIAN_POINT('Ctrl Pts',(-22.033278315859,19.4497721739535,-13.2827830515041));
#70809=CARTESIAN_POINT('Ctrl Pts',(-19.2804607350937,22.6100249265848,-13.0838961401291));
#70810=CARTESIAN_POINT('Ctrl Pts',(-20.4512197967597,26.6342671301568,-12.8850092287543));
#70811=CARTESIAN_POINT('Ctrl Pts',(-24.4697271871847,27.8245613990593,-12.6861223173794));
#70812=CARTESIAN_POINT('Ctrl Pts',(-27.6433153278088,25.0871282204823,-12.4872354060045));
#70813=CARTESIAN_POINT('Ctrl Pts',(-27.0557257932998,20.9374365894791,-12.2883484946296));
#70814=CARTESIAN_POINT('Ctrl Pts',(-23.2469035464947,19.1887012791116,-12.0894615832547));
#70815=CARTESIAN_POINT('Ctrl Pts',(-19.7168332973353,21.4478617713041,-11.8905746718798));
#70816=CARTESIAN_POINT('Ctrl Pts',(-19.7093503041991,25.638941118954,-11.6916877605049));
#70817=CARTESIAN_POINT('Ctrl Pts',(-23.2313308033251,27.9106927465004,-11.49280084913));
#70818=CARTESIAN_POINT('Ctrl Pts',(-27.0463733307188,26.175569521003,-11.2939139377551));
#70819=CARTESIAN_POINT('Ctrl Pts',(-27.6487772659703,22.0280025725045,-11.0950270263803));
#70820=CARTESIAN_POINT('Ctrl Pts',(-24.4849844680144,19.2792542709887,-10.8961401150054));
#70821=CARTESIAN_POINT('Ctrl Pts',(-20.4622522727791,20.4551912501253,-10.6972532036305));
#70822=CARTESIAN_POINT('Ctrl Pts',(-19.2771304962409,24.4752271291019,-10.4983662922556));
#70823=CARTESIAN_POINT('Ctrl Pts',(-22.0186455692821,27.6452897779736,-10.2994793808807));
#70824=CARTESIAN_POINT('Ctrl Pts',(-26.1675775819241,27.0523603994167,-10.1005924695058));
#70825=CARTESIAN_POINT('Ctrl Pts',(-27.9114097859742,23.2412908202039,-9.90170555813094));
#70826=CARTESIAN_POINT('Ctrl Pts',(-25.6477082384987,19.7141308582173,-9.70281864675604));
#70827=CARTESIAN_POINT('Ctrl Pts',(-21.4566227313875,19.7120414646744,-9.50393173538115));
#70828=CARTESIAN_POINT('Ctrl Pts',(-19.1894055002238,23.2369426150895,-9.30504482400626));
#70829=CARTESIAN_POINT('Ctrl Pts',(-20.9294369521262,27.0497490145641,-9.10615791263137));
#70830=CARTESIAN_POINT('Ctrl Pts',(-25.0777757131341,27.6468148546534,-8.90727100125649));
#70831=CARTESIAN_POINT('Ctrl Pts',(-27.822450183007,24.4794872511504,-8.70838408988158));
#70832=CARTESIAN_POINT('Ctrl Pts',(-26.6413372339507,20.4582717265789,-8.5094971785067));
#70833=CARTESIAN_POINT('Ctrl Pts',(-22.6197795242843,19.2783244051677,-8.3106102671318));
#70834=CARTESIAN_POINT('Ctrl Pts',(-19.4532476173261,22.0239168322588,-8.11172335575693));
#70835=CARTESIAN_POINT('Ctrl Pts',(-20.0515158579395,26.1720823552048,-7.91283644438202));
#70836=CARTESIAN_POINT('Ctrl Pts',(-23.8648264577823,27.9110085648553,-7.71394953300715));
#70837=CARTESIAN_POINT('Ctrl Pts',(-27.3890702910207,25.6427697111708,-7.51506262163224));
#70838=CARTESIAN_POINT('Ctrl Pts',(-27.3857660815101,21.4516849857467,-7.31617571025736));
#70839=CARTESIAN_POINT('Ctrl Pts',(-23.8579501176399,19.1890059058624,-7.11728879888246));
#70840=CARTESIAN_POINT('Ctrl Pts',(-20.0473861607387,20.9339427023821,-6.91840188750758));
#70841=CARTESIAN_POINT('Ctrl Pts',(-19.455659404654,25.083046405547,-6.71951497613268));
#70842=CARTESIAN_POINT('Ctrl Pts',(-22.6265165680722,27.8236424981302,-6.52062806475779));
#70843=CARTESIAN_POINT('Ctrl Pts',(-26.6462087621649,26.6373555352779,-6.32174115338291));
#70844=CARTESIAN_POINT('Ctrl Pts',(-27.8209796742559,22.6142826553032,-6.12285424200801));
#70845=CARTESIAN_POINT('Ctrl Pts',(-25.0713144402817,19.451286734573,-5.92396733063314));
#70846=CARTESIAN_POINT('Ctrl Pts',(-20.9239222770979,20.0548928464088,-5.72508041925822));
#70847=CARTESIAN_POINT('Ctrl Pts',(-19.1899049418037,23.8704381513923,-5.52619350788335));
#70848=CARTESIAN_POINT('Ctrl Pts',(-21.462677345109,27.391760019137,-5.32730659650845));
#70849=CARTESIAN_POINT('Ctrl Pts',(-25.6537543476985,27.3830622120451,-5.12841968513356));
#70850=CARTESIAN_POINT('Ctrl Pts',(-27.9118915289232,23.8523372773817,-4.92953277375868));
#70851=CARTESIAN_POINT('Ctrl Pts',(-26.1620522776973,20.044022073994,-4.73064586238378));
#70852=CARTESIAN_POINT('Ctrl Pts',(-22.0121905039951,19.4576353819139,-4.53175895100889));
#70853=CARTESIAN_POINT('Ctrl Pts',(-19.2756773275934,22.6320168537699,-4.332872039634));
#70854=CARTESIAN_POINT('Ctrl Pts',(-20.4671363395497,26.6501790600916,-4.13398512825911));
#70855=CARTESIAN_POINT('Ctrl Pts',(-24.4917177269413,27.8197716172427,-3.93509821688421));
#70856=CARTESIAN_POINT('Ctrl Pts',(-27.6511724229859,25.0660381302974,-3.73621130550934));
#70857=CARTESIAN_POINT('Ctrl Pts',(-27.0422294396017,20.9194261956609,-3.53732439413444));
#70858=CARTESIAN_POINT('Ctrl Pts',(-23.2244557486677,19.1903206065495,-3.33843748275955));
#70859=CARTESIAN_POINT('Ctrl Pts',(-19.7060616783232,21.4676227953791,-3.13955057138466));
#70860=CARTESIAN_POINT('Ctrl Pts',(-19.7201530685912,25.6586851339996,-2.94066366000977));
#70861=CARTESIAN_POINT('Ctrl Pts',(-23.2537811265686,27.9122766767063,-2.74177674863487));
#70862=CARTESIAN_POINT('Ctrl Pts',(-27.0598412692263,26.157537868805,-2.54288983726));
#70863=CARTESIAN_POINT('Ctrl Pts',(-27.6408869261465,22.0069248974407,-2.34400292588509));
#70864=CARTESIAN_POINT('Ctrl Pts',(-24.4629864031666,19.2744991693506,-2.14511601451021));
#70865=CARTESIAN_POINT('Ctrl Pts',(-20.4463608393743,20.4711282571522,-1.94622910313531));
#70866=CARTESIAN_POINT('Ctrl Pts',(-19.2819485742067,24.4972114865714,-1.74734219176043));
#70867=CARTESIAN_POINT('Ctrl Pts',(-22.0397457534735,27.6531197253375,-1.54845528038553));
#70868=CARTESIAN_POINT('Ctrl Pts',(-26.18557059207,27.0388408789175,-1.34956836901064));
#70869=CARTESIAN_POINT('Ctrl Pts',(-27.909761571306,23.2188451249141,-1.15068145763575));
#70870=CARTESIAN_POINT('Ctrl Pts',(-25.627933368551,19.7033846790271,-0.951794546260857));
#70871=CARTESIAN_POINT('Ctrl Pts',(-21.4368926350098,19.7228696291338,-0.752907634885971));
#70872=CARTESIAN_POINT('Ctrl Pts',(-19.1878504631509,23.2593949581373,-0.554020723511071));
#70873=CARTESIAN_POINT('Ctrl Pts',(-20.9474859215826,27.0631937365842,-0.355133812136187));
#70874=CARTESIAN_POINT('Ctrl Pts',(-25.0988432164898,27.6388973960336,-0.15624690076129));
#70875=CARTESIAN_POINT('Ctrl Pts',(-27.8271769709077,24.4574830850727,0.0426400106135906));
#70876=CARTESIAN_POINT('Ctrl Pts',(-26.6253797890813,20.442400816023,0.241526921988483));
#70877=CARTESIAN_POINT('Ctrl Pts',(-22.5978013855116,19.2831707713033,0.440413833363379));
#70878=CARTESIAN_POINT('Ctrl Pts',(-19.4454448307434,22.0450270755113,0.63930074473826));
#70879=CARTESIAN_POINT('Ctrl Pts',(-20.0650585228489,26.1900579518786,0.838187656113157));
#70880=CARTESIAN_POINT('Ctrl Pts',(-23.887270013361,27.9093314656867,1.03707456748805));
#70881=CARTESIAN_POINT('Ctrl Pts',(-27.3997910125914,25.6229810281009,1.23596147886293));
#70882=CARTESIAN_POINT('Ctrl Pts',(-27.3749125349168,21.4319688407133,1.43484839023782));
#70883=CARTESIAN_POINT('Ctrl Pts',(-23.8354957919727,19.1874797644976,1.63373530161272));
#70884=CARTESIAN_POINT('Ctrl Pts',(-20.033964677473,20.9520089592048,1.8326222129876));
#70885=CARTESIAN_POINT('Ctrl Pts',(-19.4636039689568,25.1041037023031,2.0315091243625));
#70886=CARTESIAN_POINT('Ctrl Pts',(-22.6485267989372,27.8283409644652,2.23039603573739));
#70887=CARTESIAN_POINT('Ctrl Pts',(-26.662059123587,26.6213776789941,2.42928294711228));
#70888=CARTESIAN_POINT('Ctrl Pts',(-27.8161050279772,22.5923107716267,2.62816985848716));
#70889=CARTESIAN_POINT('Ctrl Pts',(-25.0501941729305,19.4435111216939,2.82705676986206));
#70890=CARTESIAN_POINT('Ctrl Pts',(-20.9059641236666,20.0684586332996,3.02594368123694));
#70891=CARTESIAN_POINT('Ctrl Pts',(-19.1916109226953,23.8928795300895,3.22483059261183));
#70892=CARTESIAN_POINT('Ctrl Pts',(-21.4824798085275,27.4024552653329,3.42371750398671));
#70893=CARTESIAN_POINT('Ctrl Pts',(-25.6734565087343,27.3721833012931,3.62260441536165));
#70894=CARTESIAN_POINT('Ctrl Pts',(-27.9133887720521,23.8298810062832,3.82149132673651));
#70895=CARTESIAN_POINT('Ctrl Pts',(-26.1439687634292,20.030623851711,4.02037823811141));
#70896=CARTESIAN_POINT('Ctrl Pts',(-21.9911434487132,19.4656070387423,4.21926514948628));
#70897=CARTESIAN_POINT('Ctrl Pts',(-19.2710071906058,22.6540331129696,4.41815206086118));
#70898=CARTESIAN_POINT('Ctrl Pts',(-20.4831345807856,26.666008846129,4.61703897223605));
#70899=CARTESIAN_POINT('Ctrl Pts',(-24.5136833191324,27.814868698894,4.815925883611));
#70900=CARTESIAN_POINT('Ctrl Pts',(-27.6589208492834,25.044907873826,5.01481279498585));
#70901=CARTESIAN_POINT('Ctrl Pts',(-27.0286405531965,20.9014855152137,5.21369970636075));
#70902=CARTESIAN_POINT('Ctrl Pts',(-23.2020165840186,19.1920554663387,5.41258661773564));
#70903=CARTESIAN_POINT('Ctrl Pts',(-19.6953919252152,21.4874390063501,5.61147352911051));
#70904=CARTESIAN_POINT('Ctrl Pts',(-19.7310573254847,25.6783732784078,5.81036044048541));
#70905=CARTESIAN_POINT('Ctrl Pts',(-23.2762393059069,27.9137450191198,6.00924735186033));
#70906=CARTESIAN_POINT('Ctrl Pts',(-27.0732162083372,26.1394371270407,6.20813426323521));
#70907=CARTESIAN_POINT('Ctrl Pts',(-27.6328881899946,21.9858881184902,6.40702117461008));
#70908=CARTESIAN_POINT('Ctrl Pts',(-24.440964152095,19.2698573694446,6.605908085985));
#70909=CARTESIAN_POINT('Ctrl Pts',(-20.4305516549384,20.4871468568447,6.80479499735984));
#70910=CARTESIAN_POINT('Ctrl Pts',(-19.2868797565055,24.5191707508981,7.00368190873475));
#70911=CARTESIAN_POINT('Ctrl Pts',(-22.0608859640696,27.6608409522209,7.20256882010963));
#70912=CARTESIAN_POINT('Ctrl Pts',(-26.2034937698199,27.0252289155038,7.40145573148457));
#70913=CARTESIAN_POINT('Ctrl Pts',(-27.9079978354924,23.1964082114763,7.60034264285942));
#70914=CARTESIAN_POINT('Ctrl Pts',(-25.6081034428465,19.6927404366781,7.79922955423434));
#70915=CARTESIAN_POINT('Ctrl Pts',(-21.4172185398362,19.7337992141093,7.99811646560919));
#70916=CARTESIAN_POINT('Ctrl Pts',(-19.1864110238848,23.2818550085209,8.1970033769841));
#70917=CARTESIAN_POINT('Ctrl Pts',(-20.965603860865,27.0765453703715,8.39589028835899));
#70918=CARTESIAN_POINT('Ctrl Pts',(-25.1198696842683,27.6308715938061,8.5947771997339));
#70919=CARTESIAN_POINT('Ctrl Pts',(-27.8317904260442,24.4354548786015,8.79366411110879));
#70920=CARTESIAN_POINT('Ctrl Pts',(-26.609340857462,20.4266122593714,8.99255102248365));
#70921=CARTESIAN_POINT('Ctrl Pts',(-22.5758484854174,19.2881302093852,9.19143793385857));
#70922=CARTESIAN_POINT('Ctrl Pts',(-19.4377508160619,22.0661772052205,9.39032484523341));
#70923=CARTESIAN_POINT('Ctrl Pts',(-20.0786935407278,26.2079635972476,9.58921175660836));
#70924=CARTESIAN_POINT('Ctrl Pts',(-23.9097046384281,27.9075388567697,9.78809866798321));
#70925=CARTESIAN_POINT('Ctrl Pts',(-27.4104097265529,25.6031374205046,9.98698557935814));
#70926=CARTESIAN_POINT('Ctrl Pts',(-27.3639576399603,21.4123088273581,10.185872490733));
#70927=CARTESIAN_POINT('Ctrl Pts',(-23.8130339077415,19.1860692307627,10.3847594021079));
#70928=CARTESIAN_POINT('Ctrl Pts',(-20.0206363711217,20.9701440659991,10.5836463134828));
#70929=CARTESIAN_POINT('Ctrl Pts',(-19.4716568239683,25.1251198240861,10.7825332248577));
#70930=CARTESIAN_POINT('Ctrl Pts',(-22.6705609243254,27.8329260671917,10.9814201362326));
#70931=CARTESIAN_POINT('Ctrl Pts',(-26.6778270263059,26.605318442011,11.1803070476075));
#70932=CARTESIAN_POINT('Ctrl Pts',(-27.8111173423259,22.5703642721228,11.3791939589824));
#70933=CARTESIAN_POINT('Ctrl Pts',(-25.0290341591364,19.4358443319569,11.5780808703573));
#70934=CARTESIAN_POINT('Ctrl Pts',(-20.8880760403332,20.0821166830615,11.7769677817321));
#70935=CARTESIAN_POINT('Ctrl Pts',(-19.1934324017466,23.9153118296306,11.975854693107));
#70936=CARTESIAN_POINT('Ctrl Pts',(-21.5023370651513,27.4130484333204,12.1747416044819));
#70937=CARTESIAN_POINT('Ctrl Pts',(-25.6931024077111,27.3612031144989,12.3736285158569));
#70938=CARTESIAN_POINT('Ctrl Pts',(-27.9147703979196,23.807417325405,12.5725154272317));
#70939=CARTESIAN_POINT('Ctrl Pts',(-26.1258165191579,20.0173188948697,12.7714023386066));
#70940=CARTESIAN_POINT('Ctrl Pts',(-21.9701377077319,19.4736869332006,12.9702892499815));
#70941=CARTESIAN_POINT('Ctrl Pts',(-19.2664504478831,22.6760731207826,13.1691761613564));
#70942=CARTESIAN_POINT('Ctrl Pts',(-20.4992140965357,26.6817560688007,13.3680630727313));
#70943=CARTESIAN_POINT('Ctrl Pts',(-24.5356233816989,27.8098527739337,13.5669499841062));
#70944=CARTESIAN_POINT('Ctrl Pts',(-27.6665604013785,25.0237380109917,13.7658368954811));
#70945=CARTESIAN_POINT('Ctrl Pts',(-27.0149594941717,20.8836150235418,13.9647238068559));
#70946=CARTESIAN_POINT('Ctrl Pts',(-23.1795866471555,19.1939058125079,14.1636107182308));
#70947=CARTESIAN_POINT('Ctrl Pts',(-19.6848243207457,21.5073098791143,14.3624976296057));
#70948=CARTESIAN_POINT('Ctrl Pts',(-19.7420627859315,25.6980050304689,14.5613845409806));
#70949=CARTESIAN_POINT('Ctrl Pts',(-23.2987047462283,27.9150977348318,14.7602714523555));
#70950=CARTESIAN_POINT('Ctrl Pts',(-27.0864977936333,26.1212677753556,14.9591583637304));
#70951=CARTESIAN_POINT('Ctrl Pts',(-27.6247812694709,21.9648927930996,15.1580452751053));
#70952=CARTESIAN_POINT('Ctrl Pts',(-24.4189182983592,19.2653289942726,15.3569321864802));
#70953=CARTESIAN_POINT('Ctrl Pts',(-20.4148251383938,20.5032466247312,15.555819097855));
#70954=CARTESIAN_POINT('Ctrl Pts',(-19.2919239124675,24.5411043401908,15.75470600923));
#70955=CARTESIAN_POINT('Ctrl Pts',(-22.0820656408832,27.6684532540214,15.9535929206049));
#70956=CARTESIAN_POINT('Ctrl Pts',(-26.2213466402339,27.0115248698742,16.1524798319797));
#70957=CARTESIAN_POINT('Ctrl Pts',(-27.90611862527,23.1739806744387,16.3513667433546));
#70958=CARTESIAN_POINT('Ctrl Pts',(-25.5882189868514,19.6821984132284,16.5502536547295));
#70959=CARTESIAN_POINT('Ctrl Pts',(-21.3976009672041,19.7448299299816,16.7491405661044));
#70960=CARTESIAN_POINT('Ctrl Pts',(-19.1850872205686,23.304322171079,16.9480274774793));
#70961=CARTESIAN_POINT('Ctrl Pts',(-20.9837902898725,27.0898035621258,17.1469143888542));
#70962=CARTESIAN_POINT('Ctrl Pts',(-25.1408545592962,27.6227376606435,17.3458013002291));
#70963=CARTESIAN_POINT('Ctrl Pts',(-27.8362904261661,24.4134032154548,17.544688211604));
#70964=CARTESIAN_POINT('Ctrl Pts',(-26.5932208641028,20.4109064749995,17.7435751229789));
#70965=CARTESIAN_POINT('Ctrl Pts',(-22.5539214057241,19.293202587995,17.9424620343537));
#70966=CARTESIAN_POINT('Ctrl Pts',(-19.4301657771629,22.0873666609364,18.1413489457287));
#70967=CARTESIAN_POINT('Ctrl Pts',(-20.092420550266,26.2257988168362,18.3402358571035));
#70968=CARTESIAN_POINT('Ctrl Pts',(-23.9321297384963,27.9056307856063,18.5391227684785));
#70969=CARTESIAN_POINT('Ctrl Pts',(-27.4209261515234,25.5832394142105,18.7380096798533));
#70970=CARTESIAN_POINT('Ctrl Pts',(-27.3529016869309,21.3927054666449,18.9368965912282));
#70971=CARTESIAN_POINT('Ctrl Pts',(-23.7905650601562,19.184774342035,19.1357835026031));
#70972=CARTESIAN_POINT('Ctrl Pts',(-20.007401594867,20.9883475422089,19.3346704139779));
#70973=CARTESIAN_POINT('Ctrl Pts',(-19.4798177562985,25.1460942139971,19.5335573253529));
#70974=CARTESIAN_POINT('Ctrl Pts',(-22.6926183603619,27.8373976848105,19.7324442367278));
#70975=CARTESIAN_POINT('Ctrl Pts',(-26.6935120524933,26.5891782498768,19.9313311481027));
#70976=CARTESIAN_POINT('Ctrl Pts',(-27.8060167494689,22.5484437383441,20.1302180594776));
#70977=CARTESIAN_POINT('Ctrl Pts',(-25.0078349596116,19.4282865685217,20.3291049708524));
#70978=CARTESIAN_POINT('Ctrl Pts',(-20.8702585011083,20.095866633774,20.5279918822274));
#70979=CARTESIAN_POINT('Ctrl Pts',(-19.1953693306909,23.9377344555896,20.7268787936022));
#70980=CARTESIAN_POINT('Ctrl Pts',(-21.5222485887897,27.4235392423947,20.9257657049771));
#70981=CARTESIAN_POINT('Ctrl Pts',(-25.7126915240386,27.3501219426233,21.124652616352));
#70982=CARTESIAN_POINT('Ctrl Pts',(-27.9160363699146,23.7849468300045,21.3235395277269));
#70983=CARTESIAN_POINT('Ctrl Pts',(-26.1075960258935,20.0041075560337,21.5224264391018));
#70984=CARTESIAN_POINT('Ctrl Pts',(-21.9491738376752,19.4818748511826,21.7213133504767));
#70985=CARTESIAN_POINT('Ctrl Pts',(-19.2620072201731,22.6981362931779,21.9202002618515));
#70986=CARTESIAN_POINT('Ctrl Pts',(-20.5153744607142,26.6974203108268,22.1190871732265));
#70987=CARTESIAN_POINT('Ctrl Pts',(-24.5575373332589,27.8047239752771,22.3179740846014));
#70988=CARTESIAN_POINT('Ctrl Pts',(-27.6740908768329,25.0025291027673,22.5168609959763));
#70989=CARTESIAN_POINT('Ctrl Pts',(-27.0011866250572,20.8658151941895,22.7157479073511));
#70990=CARTESIAN_POINT('Ctrl Pts',(-23.1571665324412,19.1958715960246,22.914634818726));
#70991=CARTESIAN_POINT('Ctrl Pts',(-19.6743591449424,21.5272348871214,23.1135217301009));
#70992=CARTESIAN_POINT('Ctrl Pts',(-19.7531691583009,25.7175798699656,23.3124086414758));
#70993=CARTESIAN_POINT('Ctrl Pts',(-23.3211768522295,27.9163347880016,23.5112955528507));
#70994=CARTESIAN_POINT('Ctrl Pts',(-27.099685673169,26.1030302952045,23.7101824642256));
#70995=CARTESIAN_POINT('Ctrl Pts',(-27.6165663794003,21.9439394776331,23.9090693756005));
#70996=CARTESIAN_POINT('Ctrl Pts',(-24.3968494261405,19.2609141637993,24.1079562869754));
#70997=CARTESIAN_POINT('Ctrl Pts',(-20.3991817064806,20.5194271342477,24.3068431983502));
#70998=CARTESIAN_POINT('Ctrl Pts',(-19.2970809084129,24.5630116731296,24.5057301097252));
#70999=CARTESIAN_POINT('Ctrl Pts',(-22.103284222713,27.6759564292301,24.7046170211));
#71000=CARTESIAN_POINT('Ctrl Pts',(-26.2391287301751,26.9977291047774,24.9035039324749));
#71001=CARTESIAN_POINT('Ctrl Pts',(-27.9041239905479,23.1515631088375,25.1023908438499));
#71002=CARTESIAN_POINT('Ctrl Pts',(-25.5682805272645,19.6717588866363,25.3012777552247));
#71003=CARTESIAN_POINT('Ctrl Pts',(-21.378040437354,19.7559614870787,25.5001646665996));
#71004=CARTESIAN_POINT('Ctrl Pts',(-19.1838790875238,23.3267958455017,25.6990515779745));
#71005=CARTESIAN_POINT('Ctrl Pts',(-21.0020447281196,27.102967969889,25.8979384893494));
#71006=CARTESIAN_POINT('Ctrl Pts',(-25.1617972828013,27.6144957943989,26.0968254007243));
#71007=CARTESIAN_POINT('Ctrl Pts',(-27.8406768571304,24.3913287133657,26.2957123120992));
#71008=CARTESIAN_POINT('Ctrl Pts',(-26.5770202265301,20.3952838160355,26.494599223474));
#71009=CARTESIAN_POINT('Ctrl Pts',(-22.5320207456567,19.2983878917809,26.693486134849));
#71010=CARTESIAN_POINT('Ctrl Pts',(-19.4226898806994,22.1085946563589,26.8923730462238));
#71011=CARTESIAN_POINT('Ctrl Pts',(-20.1062392525582,26.2435635625186,27.0912599575988));
#71012=CARTESIAN_POINT('Ctrl Pts',(-23.9545445968963,27.9036065012466,27.2901468689736));
#71013=CARTESIAN_POINT('Ctrl Pts',(-27.4313402400131,25.5632890499054,27.4890337803486));
#71014=CARTESIAN_POINT('Ctrl Pts',(-27.3417445322793,21.3731564203992,27.6879206917233));
#71015=CARTESIAN_POINT('Ctrl Pts',(-23.7680906688437,19.1836005284276,27.8868076030983));
#71016=CARTESIAN_POINT('Ctrl Pts',(-19.9942591430928,21.006608717098,28.0856945144732));
#71017=CARTESIAN_POINT('Ctrl Pts',(-19.4880894883424,25.1670455539585,28.2845814258481));
#71018=CARTESIAN_POINT('Ctrl Pts',(-22.7146929737878,27.8417193740874,28.483468337223));
#71019=CARTESIAN_POINT('Ctrl Pts',(-26.7091242637221,26.5730261189747,28.6823552485979));
#71020=CARTESIAN_POINT('Ctrl Pts',(-27.800783601434,22.5264202402148,28.8812421599727));
#71021=CARTESIAN_POINT('Ctrl Pts',(-24.9866344909904,19.4210825872784,29.0801290713476));
#71022=CARTESIAN_POINT('Ctrl Pts',(-20.8524414419848,20.1092462471125,29.2790159827225));
#71023=CARTESIAN_POINT('Ctrl Pts',(-19.1975548654738,23.9610197697405,29.4779028940975));
#71024=CARTESIAN_POINT('Ctrl Pts',(-21.5419621600858,27.4322721963604,29.6767898054723));
#71025=CARTESIAN_POINT('Ctrl Pts',(-25.7326999905548,27.3421218489336,29.8756767168472));
#71026=CARTESIAN_POINT('Ctrl Pts',(-27.9167437462655,23.7552312243062,30.074606513978));
#71027=CARTESIAN_POINT('Ctrl Pts',(-26.6988816812223,21.2548018888855,30.207240673984));
#71028=CARTESIAN_POINT('Ctrl Pts',(-25.6949495301469,20.5396876139378,30.2735791968649));
#71029=CARTESIAN_POINT('Ctrl Pts',(-25.3002789331219,27.0757977803642,-74.998270464385));
#71030=CARTESIAN_POINT('Ctrl Pts',(-26.4751253509978,26.4926221000403,-74.93197482726));
#71031=CARTESIAN_POINT('Ctrl Pts',(-28.1754011787373,24.0694996479516,-74.79938355301));
#71032=CARTESIAN_POINT('Ctrl Pts',(-26.4837483309012,19.9311312672286,-74.6004966416352));
#71033=CARTESIAN_POINT('Ctrl Pts',(-22.0927467074531,19.1303002597153,-74.4016097302603));
#71034=CARTESIAN_POINT('Ctrl Pts',(-19.0429812726389,22.3850346168187,-74.2027228188854));
#71035=CARTESIAN_POINT('Ctrl Pts',(-20.1340100833004,26.7136450865977,-74.0038359075104));
#71036=CARTESIAN_POINT('Ctrl Pts',(-24.3648079623233,28.1337076326876,-73.8049489961356));
#71037=CARTESIAN_POINT('Ctrl Pts',(-27.8468168625814,25.3428413000204,-73.6060620847608));
#71038=CARTESIAN_POINT('Ctrl Pts',(-27.3807965561229,20.9042730835607,-73.407175173386));
#71039=CARTESIAN_POINT('Ctrl Pts',(-23.3947520922001,18.8973817856161,-73.2082882620109));
#71040=CARTESIAN_POINT('Ctrl Pts',(-19.5516411735125,21.1659538450954,-73.0094013506361));
#71041=CARTESIAN_POINT('Ctrl Pts',(-19.3828929156757,25.6255632813351,-72.8105144392611));
#71042=CARTESIAN_POINT('Ctrl Pts',(-23.0436065423778,28.1781015326929,-72.6116275278863));
#71043=CARTESIAN_POINT('Ctrl Pts',(-27.1698786638517,26.4780582930873,-72.4127406165114));
#71044=CARTESIAN_POINT('Ctrl Pts',(-27.9700245539433,22.0875995404682,-72.2138537051365));
#71045=CARTESIAN_POINT('Ctrl Pts',(-24.7087729478585,19.0412003055027,-72.0149667937617));
#71046=CARTESIAN_POINT('Ctrl Pts',(-20.3829402285396,20.1382348854171,-71.8160798823866));
#71047=CARTESIAN_POINT('Ctrl Pts',(-18.9675984832563,24.3706259142265,-71.6171929710119));
#71048=CARTESIAN_POINT('Ctrl Pts',(-21.7633275223502,27.8491625539056,-71.4183060596369));
#71049=CARTESIAN_POINT('Ctrl Pts',(-26.2010890016861,27.3773657979069,-71.219419148262));
#71050=CARTESIAN_POINT('Ctrl Pts',(-28.2029565915712,23.3887762096687,-71.0205322368872));
#71051=CARTESIAN_POINT('Ctrl Pts',(-25.9293835962292,19.5485697902788,-70.8216453255123));
#71052=CARTESIAN_POINT('Ctrl Pts',(-21.4695908899928,19.3855704600358,-70.6227584141375));
#71053=CARTESIAN_POINT('Ctrl Pts',(-18.9217498106796,23.0495608804504,-70.4238715027624));
#71054=CARTESIAN_POINT('Ctrl Pts',(-20.6271103053749,27.173644458905,-70.2249845913878));
#71055=CARTESIAN_POINT('Ctrl Pts',(-25.0185906614429,27.9681380786542,-70.0260976800127));
#71056=CARTESIAN_POINT('Ctrl Pts',(-28.0607927724171,24.7029694506781,-69.8272107686379));
#71057=CARTESIAN_POINT('Ctrl Pts',(-26.958190832065,20.3785517110777,-69.6283238572629));
#71058=CARTESIAN_POINT('Ctrl Pts',(-22.7239825396399,18.9686581083402,-69.4294369458881));
#71059=CARTESIAN_POINT('Ctrl Pts',(-19.2490463135321,21.7688613262589,-69.2305500345131));
#71060=CARTESIAN_POINT('Ctrl Pts',(-19.726553919893,26.2060120245128,-69.0316631231383));
#71061=CARTESIAN_POINT('Ctrl Pts',(-23.7177163542527,28.2027449203469,-68.8327762117633));
#71062=CARTESIAN_POINT('Ctrl Pts',(-27.554993734307,25.9242317772028,-68.6338893003885));
#71063=CARTESIAN_POINT('Ctrl Pts',(-27.7122534952017,21.464232987742,-68.4350023890136));
#71064=CARTESIAN_POINT('Ctrl Pts',(-24.0449872501318,18.9211092938514,-68.2361154776388));
#71065=CARTESIAN_POINT('Ctrl Pts',(-19.9231017453993,20.6317757489323,-68.0372285662638));
#71066=CARTESIAN_POINT('Ctrl Pts',(-19.1342602816024,25.0242749213373,-67.8383416548889));
#71067=CARTESIAN_POINT('Ctrl Pts',(-22.4033412812393,28.0622724941539,-67.6394547435142));
#71068=CARTESIAN_POINT('Ctrl Pts',(-26.7263364780072,26.9541062776738,-67.4405678321392));
#71069=CARTESIAN_POINT('Ctrl Pts',(-28.1307798156237,22.7180870678451,-67.2416809207643));
#71070=CARTESIAN_POINT('Ctrl Pts',(-25.3261069439786,19.2467573632969,-67.0427940093892));
#71071=CARTESIAN_POINT('Ctrl Pts',(-20.8895744350682,19.7299748422869,-66.8439070980146));
#71072=CARTESIAN_POINT('Ctrl Pts',(-18.8979795086559,23.7237036117087,-66.6450201866394));
#71073=CARTESIAN_POINT('Ctrl Pts',(-21.1814290427109,27.5580455448236,-66.4461332752648));
#71074=CARTESIAN_POINT('Ctrl Pts',(-25.6416265200303,27.7095655036835,-66.2472463638896));
#71075=CARTESIAN_POINT('Ctrl Pts',(-28.1800286213416,24.0390294928702,-66.0483594525151));
#71076=CARTESIAN_POINT('Ctrl Pts',(-26.4640590365463,19.9193488961884,-65.84947254114));
#71077=CARTESIAN_POINT('Ctrl Pts',(-22.070548323843,19.1361608906749,-65.6505856297653));
#71078=CARTESIAN_POINT('Ctrl Pts',(-19.0367603199271,22.4091488500043,-65.4516987183902));
#71079=CARTESIAN_POINT('Ctrl Pts',(-20.1504889775927,26.7307143431692,-65.2528118070154));
#71080=CARTESIAN_POINT('Ctrl Pts',(-24.3883120890633,28.1297050902813,-65.0539248956404));
#71081=CARTESIAN_POINT('Ctrl Pts',(-27.8560295230445,25.3205672095992,-64.8550379842656));
#71082=CARTESIAN_POINT('Ctrl Pts',(-27.3671029716606,20.8846602378549,-64.6561510728907));
#71083=CARTESIAN_POINT('Ctrl Pts',(-23.3708144814982,18.8982065791922,-64.4572641615158));
#71084=CARTESIAN_POINT('Ctrl Pts',(-19.5394143456281,21.1865887224265,-64.2583772501409));
#71085=CARTESIAN_POINT('Ctrl Pts',(-19.3936344397536,25.6469775007352,-64.059490338766));
#71086=CARTESIAN_POINT('Ctrl Pts',(-23.0674341372756,28.1806538054564,-63.8606034273911));
#71087=CARTESIAN_POINT('Ctrl Pts',(-27.1849030030193,26.4593839328764,-63.6617165160162));
#71088=CARTESIAN_POINT('Ctrl Pts',(-27.9624362531557,22.0648689562775,-63.4628296046415));
#71089=CARTESIAN_POINT('Ctrl Pts',(-24.685546754758,19.0352955457279,-63.2639426932664));
#71090=CARTESIAN_POINT('Ctrl Pts',(-20.365418122441,20.1545848000565,-63.0650557818915));
#71091=CARTESIAN_POINT('Ctrl Pts',(-18.9718822827999,24.3942047946143,-62.8661688705168));
#71092=CARTESIAN_POINT('Ctrl Pts',(-21.7854805201097,27.8583042149004,-62.6672819591418));
#71093=CARTESIAN_POINT('Ctrl Pts',(-26.2207546080739,27.363669400868,-62.468395047767));
#71094=CARTESIAN_POINT('Ctrl Pts',(-28.2020637090825,23.3648278084966,-62.2695081363919));
#71095=CARTESIAN_POINT('Ctrl Pts',(-25.908752746618,19.5363758153198,-62.0706212250171));
#71096=CARTESIAN_POINT('Ctrl Pts',(-21.4481800544803,19.3963362038671,-61.8717343136422));
#71097=CARTESIAN_POINT('Ctrl Pts',(-18.9192337425472,23.0733935036625,-61.6728474022673));
#71098=CARTESIAN_POINT('Ctrl Pts',(-20.6458010521971,27.1886438192408,-61.4739604908924));
#71099=CARTESIAN_POINT('Ctrl Pts',(-25.0413130146292,27.9605210262733,-61.2750735795176));
#71100=CARTESIAN_POINT('Ctrl Pts',(-28.066666814325,24.6797354158921,-61.0761866681428));
#71101=CARTESIAN_POINT('Ctrl Pts',(-26.9418188170664,20.3610507992892,-60.8772997567678));
#71102=CARTESIAN_POINT('Ctrl Pts',(-22.7004089609511,18.9729721750507,-60.6784128453929));
#71103=CARTESIAN_POINT('Ctrl Pts',(-19.2399332914964,21.7910261091923,-60.4795259340178));
#71104=CARTESIAN_POINT('Ctrl Pts',(-19.7402755489783,26.2256599678099,-60.2806390226432));
#71105=CARTESIAN_POINT('Ctrl Pts',(-23.7416636207986,28.2018212297804,-60.0817521112681));
#71106=CARTESIAN_POINT('Ctrl Pts',(-27.567161130716,25.9035852461977,-59.8828651998933));
#71107=CARTESIAN_POINT('Ctrl Pts',(-27.7014602158176,21.4428360276963,-59.6839782885185));
#71108=CARTESIAN_POINT('Ctrl Pts',(-24.0211514035796,18.9186238969152,-59.4850913771435));
#71109=CARTESIAN_POINT('Ctrl Pts',(-19.9081264537191,20.6504857841465,-59.2862044657685));
#71110=CARTESIAN_POINT('Ctrl Pts',(-19.1419065681502,25.0469874526984,-59.0873175543938));
#71111=CARTESIAN_POINT('Ctrl Pts',(-22.4265828569774,28.0681166310412,-58.8884306430189));
#71112=CARTESIAN_POINT('Ctrl Pts',(-26.743816305392,26.9377117537917,-58.6895437316441));
#71113=CARTESIAN_POINT('Ctrl Pts',(-28.1264354153342,22.6945190606133,-58.490656820269));
#71114=CARTESIAN_POINT('Ctrl Pts',(-25.3039304515362,19.2376728731248,-58.2917699088942));
#71115=CARTESIAN_POINT('Ctrl Pts',(-20.8699441667711,19.7437217454045,-58.0928829975193));
#71116=CARTESIAN_POINT('Ctrl Pts',(-18.8989340166969,23.7476496696962,-57.8939960861445));
#71117=CARTESIAN_POINT('Ctrl Pts',(-21.2020912151292,27.5701863606814,-57.6951091747695));
#71118=CARTESIAN_POINT('Ctrl Pts',(-25.6630095722369,27.6987446970098,-57.4962222633946));
#71119=CARTESIAN_POINT('Ctrl Pts',(-28.1824833413424,24.0151904675449,-57.2973353520197));
#71120=CARTESIAN_POINT('Ctrl Pts',(-26.4453297447866,19.9043976952695,-57.0984484406449));
#71121=CARTESIAN_POINT('Ctrl Pts',(-22.0478456514677,19.1438364001541,-56.89956152927));
#71122=CARTESIAN_POINT('Ctrl Pts',(-19.0309460979801,22.4323979274461,-56.700674617895));
#71123=CARTESIAN_POINT('Ctrl Pts',(-20.1669059830785,26.7481730576014,-56.5017877065202));
#71124=CARTESIAN_POINT('Ctrl Pts',(-24.4118744858731,28.1253303633956,-56.3029007951453));
#71125=CARTESIAN_POINT('Ctrl Pts',(-27.8650854662716,25.2983790444879,-56.1040138837703));
#71126=CARTESIAN_POINT('Ctrl Pts',(-27.353330817297,20.8650476770091,-55.9051269723955));
#71127=CARTESIAN_POINT('Ctrl Pts',(-23.3468696717177,18.8991919031584,-55.7062400610207));
#71128=CARTESIAN_POINT('Ctrl Pts',(-19.5273001304339,21.2072665020213,-55.5073531496458));
#71129=CARTESIAN_POINT('Ctrl Pts',(-19.4044827557931,25.6683466096977,-55.308466238271));
#71130=CARTESIAN_POINT('Ctrl Pts',(-23.0912763018941,28.1830778444516,-55.1095793268959));
#71131=CARTESIAN_POINT('Ctrl Pts',(-27.1998300884145,26.4406354155924,-54.910692415521));
#71132=CARTESIAN_POINT('Ctrl Pts',(-27.9547315334577,22.0421761804862,-54.7118055041462));
#71133=CARTESIAN_POINT('Ctrl Pts',(-24.6622902141166,19.0295112483513,-54.5129185927712));
#71134=CARTESIAN_POINT('Ctrl Pts',(-20.3479805498764,20.1710242599562,-54.3140316813965));
#71135=CARTESIAN_POINT('Ctrl Pts',(-18.9762873290365,24.4177615419788,-54.1151447700214));
#71136=CARTESIAN_POINT('Ctrl Pts',(-21.8076803211424,27.8673315961845,-53.9162578586467));
#71137=CARTESIAN_POINT('Ctrl Pts',(-26.2403494289864,27.3498720180674,-53.7173709472717));
#71138=CARTESIAN_POINT('Ctrl Pts',(-28.201047570823,23.3408842865797,-53.5184840358969));
#71139=CARTESIAN_POINT('Ctrl Pts',(-25.8880593940927,19.5242882208526,-53.3195971245218));
#71140=CARTESIAN_POINT('Ctrl Pts',(-21.4268249241531,19.4072120113058,-53.1207102131472));
#71141=CARTESIAN_POINT('Ctrl Pts',(-18.9168403885721,23.0972387680874,-52.9218233017722));
#71142=CARTESIAN_POINT('Ctrl Pts',(-20.6645687639545,27.2035467643904,-52.7229363903972));
#71143=CARTESIAN_POINT('Ctrl Pts',(-25.0639958562534,27.9527871091166,-52.5240494790225));
#71144=CARTESIAN_POINT('Ctrl Pts',(-28.0724211775514,24.656471450568,-52.3251625676475));
#71145=CARTESIAN_POINT('Ctrl Pts',(-26.9253569299792,20.3436343974716,-52.1262756562727));
#71146=CARTESIAN_POINT('Ctrl Pts',(-22.6768579020457,18.9774075333426,-51.9273887448976));
#71147=CARTESIAN_POINT('Ctrl Pts',(-19.2309344871063,21.8132375093799,-51.7285018335229));
#71148=CARTESIAN_POINT('Ctrl Pts',(-19.7540981373651,26.2452370163368,-51.5296149221478));
#71149=CARTESIAN_POINT('Ctrl Pts',(-23.7656058151973,28.2007742789105,-51.3307280107731));
#71150=CARTESIAN_POINT('Ctrl Pts',(-27.5792220844372,25.8828763550135,-51.1318410993982));
#71151=CARTESIAN_POINT('Ctrl Pts',(-27.690556934992,21.4214949113717,-50.9329541880232));
#71152=CARTESIAN_POINT('Ctrl Pts',(-23.99730307884,18.9162612319241,-50.7340672766484));
#71153=CARTESIAN_POINT('Ctrl Pts',(-19.8932476734969,20.669272659295,-50.5351803652735));
#71154=CARTESIAN_POINT('Ctrl Pts',(-19.1496696699568,25.0696603225891,-50.3362934538984));
#71155=CARTESIAN_POINT('Ctrl Pts',(-22.4498542084553,28.0738410505872,-50.1374065425237));
#71156=CARTESIAN_POINT('Ctrl Pts',(-26.761211507618,26.9212274667807,-49.9385196311488));
#71157=CARTESIAN_POINT('Ctrl Pts',(-28.1219697523327,22.6709737291715,-49.739632719774));
#71158=CARTESIAN_POINT('Ctrl Pts',(-25.2817074889795,19.2287026605322,-49.5407458083989));
#71159=CARTESIAN_POINT('Ctrl Pts',(-20.8503849230525,19.757569516485,-49.3418588970242));
#71160=CARTESIAN_POINT('Ctrl Pts',(-18.9000117784432,23.7715904969243,-49.1429719856492));
#71161=CARTESIAN_POINT('Ctrl Pts',(-21.2228156106747,27.5822206536816,-48.9440850742744));
#71162=CARTESIAN_POINT('Ctrl Pts',(-25.6843366392143,27.687813960855,-48.7451981628995));
#71163=CARTESIAN_POINT('Ctrl Pts',(-28.1848153134365,23.9913391219875,-48.5463112515245));
#71164=CARTESIAN_POINT('Ctrl Pts',(-26.4265237373615,19.8895431046163,-48.3474243401496));
#71165=CARTESIAN_POINT('Ctrl Pts',(-22.0251827908608,19.1516286737538,-48.1485374287749));
#71166=CARTESIAN_POINT('Ctrl Pts',(-19.0252516315952,22.4556766265364,-47.9496505173999));
#71167=CARTESIAN_POINT('Ctrl Pts',(-20.1834126427124,26.7655470314266,-47.750763606025));
#71168=CARTESIAN_POINT('Ctrl Pts',(-24.435414050856,28.1208344030802,-47.5518766946501));
#71169=CARTESIAN_POINT('Ctrl Pts',(-27.8740270722105,25.2761445563675,-47.3529897832752));
#71170=CARTESIAN_POINT('Ctrl Pts',(-27.339457886457,20.8455062704923,-47.1541028719002));
#71171=CARTESIAN_POINT('Ctrl Pts',(-23.3229302513102,18.9003004739963,-46.9552159605255));
#71172=CARTESIAN_POINT('Ctrl Pts',(-19.5152925180855,21.2280063676051,-46.7563290491504));
#71173=CARTESIAN_POINT('Ctrl Pts',(-19.4154409291741,25.6896595920065,-46.5574421377758));
#71174=CARTESIAN_POINT('Ctrl Pts',(-23.1151306287675,28.1853791197866,-46.3585552264007));
#71175=CARTESIAN_POINT('Ctrl Pts',(-27.2146604648968,26.4218103070366,-46.159668315026));
#71176=CARTESIAN_POINT('Ctrl Pts',(-27.9469101009703,22.0195233666965,-45.9607814036509));
#71177=CARTESIAN_POINT('Ctrl Pts',(-24.6390042059674,19.0238467445585,-45.761894492276));
#71178=CARTESIAN_POINT('Ctrl Pts',(-20.3306278332266,20.1875532648752,-45.5630075809012));
#71179=CARTESIAN_POINT('Ctrl Pts',(-18.9808135792194,24.4412953015176,-45.3641206695263));
#71180=CARTESIAN_POINT('Ctrl Pts',(-21.8299262980028,27.8762445806607,-45.1652337581514));
#71181=CARTESIAN_POINT('Ctrl Pts',(-26.2598729659374,27.3359739504438,-44.9663468467766));
#71182=CARTESIAN_POINT('Ctrl Pts',(-28.1999081927296,23.3169463126407,-44.7674599354016));
#71183=CARTESIAN_POINT('Ctrl Pts',(-25.8673040928193,19.5123073090426,-44.5685730240267));
#71184=CARTESIAN_POINT('Ctrl Pts',(-21.4055260618107,19.4181976037643,-44.3696861126518));
#71185=CARTESIAN_POINT('Ctrl Pts',(-18.9145698138075,23.1210960367697,-44.1707992012769));
#71186=CARTESIAN_POINT('Ctrl Pts',(-20.6834129424635,27.2183529021403,-43.9719122899021));
#71187=CARTESIAN_POINT('Ctrl Pts',(-25.0866385857089,27.9449365306953,-43.7730253785271));
#71188=CARTESIAN_POINT('Ctrl Pts',(-28.0780557093708,24.6331781719254,-43.5741384671524));
#71189=CARTESIAN_POINT('Ctrl Pts',(-26.9088056071499,20.3263029667358,-43.3752515557773));
#71190=CARTESIAN_POINT('Ctrl Pts',(-22.6533299869271,18.9819640658969,-43.1763646444026));
#71191=CARTESIAN_POINT('Ctrl Pts',(-19.2220501388541,21.835494938137,-42.9774777330275));
#71192=CARTESIAN_POINT('Ctrl Pts',(-19.7680213187548,26.2647426513878,-42.7785908216527));
#71193=CARTESIAN_POINT('Ctrl Pts',(-23.7895423030223,28.1996040954486,-42.5797039102778));
#71194=CARTESIAN_POINT('Ctrl Pts',(-27.5911762758664,25.862105652425,-42.3808169989029));
#71195=CARTESIAN_POINT('Ctrl Pts',(-27.6795439416498,21.4002102042704,-42.1819300875281));
#71196=CARTESIAN_POINT('Ctrl Pts',(-23.9734429078603,18.9140213614905,-41.9830431761531));
#71197=CARTESIAN_POINT('Ctrl Pts',(-19.8784657990009,20.6881358765479,-41.7841562647783));
#71198=CARTESIAN_POINT('Ctrl Pts',(-19.1575493813103,25.0922929302101,-41.5852693534033));
#71199=CARTESIAN_POINT('Ctrl Pts',(-22.4731547190136,28.0794456011015,-41.3863824420285));
#71200=CARTESIAN_POINT('Ctrl Pts',(-26.7785216237357,26.904653853453,-41.1874955306535));
#71201=CARTESIAN_POINT('Ctrl Pts',(-28.1173829449534,22.6474516974395,-40.9886086192788));
#71202=CARTESIAN_POINT('Ctrl Pts',(-25.2594386451877,19.219846963218,-40.7897217079038));
#71203=CARTESIAN_POINT('Ctrl Pts',(-20.8308972222064,19.7715177885814,-40.5908347965289));
#71204=CARTESIAN_POINT('Ctrl Pts',(-18.9012127653357,23.7955254589928,-40.3919478851541));
#71205=CARTESIAN_POINT('Ctrl Pts',(-21.2436016801787,27.5941481049319,-40.1930609737791));
#71206=CARTESIAN_POINT('Ctrl Pts',(-25.7056071558235,27.6767735848687,-39.9941740624042));
#71207=CARTESIAN_POINT('Ctrl Pts',(-28.1870244758296,23.9674760882269,-39.7952871510293));
#71208=CARTESIAN_POINT('Ctrl Pts',(-26.4076415126053,19.8747855178556,-39.5964002396544));
#71209=CARTESIAN_POINT('Ctrl Pts',(-22.0025603425576,19.1595375049891,-39.3975133282797));
#71210=CARTESIAN_POINT('Ctrl Pts',(-19.0196770716683,22.4789843304208,-39.1986264169047));
#71211=CARTESIAN_POINT('Ctrl Pts',(-20.2000085190899,26.7828358042576,-38.9997395055298));
#71212=CARTESIAN_POINT('Ctrl Pts',(-24.4589301602452,28.1162173284725,-38.800852594155));
#71213=CARTESIAN_POINT('Ctrl Pts',(-27.8828541039201,25.253864334422,-38.6019656827801));
#71214=CARTESIAN_POINT('Ctrl Pts',(-27.3254845467546,20.8260365361259,-38.4030787714051));
#71215=CARTESIAN_POINT('Ctrl Pts',(-23.2989968546387,18.9015322623302,-38.2041918600302));
#71216=CARTESIAN_POINT('Ctrl Pts',(-19.5033918267683,21.2488077695991,-38.0053049486554));
#71217=CARTESIAN_POINT('Ctrl Pts',(-19.4265086695198,25.7109158828961,-37.8064180372804));
#71218=CARTESIAN_POINT('Ctrl Pts',(-23.1389964857879,28.1875575704805,-37.6075311259056));
#71219=CARTESIAN_POINT('Ctrl Pts',(-27.2293937394812,26.4029091060492,-37.4086442145307));
#71220=CARTESIAN_POINT('Ctrl Pts',(-27.9389721629514,21.9969111151776,-37.2097573031558));
#71221=CARTESIAN_POINT('Ctrl Pts',(-24.6156893473584,19.0183021844513,-37.010870391781));
#71222=CARTESIAN_POINT('Ctrl Pts',(-20.3133604323151,20.2041713768168,-36.811983480406));
#71223=CARTESIAN_POINT('Ctrl Pts',(-18.9854609134091,24.4648054496174,-36.6130965690311));
#71224=CARTESIAN_POINT('Ctrl Pts',(-21.8522178612022,27.8850429321467,-36.4142096576563));
#71225=CARTESIAN_POINT('Ctrl Pts',(-26.2793247015791,27.3219755662776,-36.2153227462814));
#71226=CARTESIAN_POINT('Ctrl Pts',(-28.1986456049942,23.2930145210038,-36.0164358349064));
#71227=CARTESIAN_POINT('Ctrl Pts',(-25.8464873927859,19.5004333973679,-35.8175489235315));
#71228=CARTESIAN_POINT('Ctrl Pts',(-21.3842840318447,19.4292926901393,-35.6186620121567));
#71229=CARTESIAN_POINT('Ctrl Pts',(-18.9124220784208,23.1449646775239,-35.4197751007818));
#71230=CARTESIAN_POINT('Ctrl Pts',(-20.7023330883783,27.2330618401476,-35.2208881894068));
#71231=CARTESIAN_POINT('Ctrl Pts',(-25.1092406029936,27.9369694990394,-35.0220012780321));
#71232=CARTESIAN_POINT('Ctrl Pts',(-28.0835702604755,24.609856197205,-34.8231143666572));
#71233=CARTESIAN_POINT('Ctrl Pts',(-26.8921652871665,20.3090569663418,-34.6242274552823));
#71234=CARTESIAN_POINT('Ctrl Pts',(-22.6298258390536,18.9866416519715,-34.4253405439073));
#71235=CARTESIAN_POINT('Ctrl Pts',(-19.2132804821634,21.8577978056717,-34.2264536325324));
#71236=CARTESIAN_POINT('Ctrl Pts',(-19.782044724201,26.2841763560894,-34.0275667211576));
#71237=CARTESIAN_POINT('Ctrl Pts',(-23.8134724499895,28.1983107104028,-33.8286798097826));
#71238=CARTESIAN_POINT('Ctrl Pts',(-27.6030233882333,25.841273688828,-33.6297928984078));
#71239=CARTESIAN_POINT('Ctrl Pts',(-27.6684215276209,21.3789824704085,-33.4309059870329));
#71240=CARTESIAN_POINT('Ctrl Pts',(-23.9495715229028,18.9119043449678,-33.232019075658));
#71241=CARTESIAN_POINT('Ctrl Pts',(-19.8637812219313,20.7070749360553,-33.0331321642831));
#71242=CARTESIAN_POINT('Ctrl Pts',(-19.1655454934085,25.1148846758278,-32.8342452529083));
#71243=CARTESIAN_POINT('Ctrl Pts',(-22.49648377122,28.0849301340709,-32.6353583415332));
#71244=CARTESIAN_POINT('Ctrl Pts',(-26.79574619505,26.887991352987,-32.4364714301584));
#71245=CARTESIAN_POINT('Ctrl Pts',(-28.1126751147405,22.6239535887192,-32.2375845187835));
#71246=CARTESIAN_POINT('Ctrl Pts',(-25.2371245102552,19.2111060158465,-32.0386976074086));
#71247=CARTESIAN_POINT('Ctrl Pts',(-20.8114815806304,19.7855661920827,-31.8398106960337));
#71248=CARTESIAN_POINT('Ctrl Pts',(-18.9025369455497,23.8194539216577,-31.6409237846589));
#71249=CARTESIAN_POINT('Ctrl Pts',(-21.2644488728379,27.6059683983702,-31.4420368732841));
#71250=CARTESIAN_POINT('Ctrl Pts',(-25.7268205584246,27.6656238616063,-31.243149961909));
#71251=CARTESIAN_POINT('Ctrl Pts',(-28.1891107699821,23.9436019986013,-31.0442630505341));
#71252=CARTESIAN_POINT('Ctrl Pts',(-26.3886835708716,19.8601253260437,-30.8453761391593));
#71253=CARTESIAN_POINT('Ctrl Pts',(-21.9799789060225,19.1675626842868,-30.6464892277844));
#71254=CARTESIAN_POINT('Ctrl Pts',(-19.0142225659176,22.5023204214765,-30.4476023164095));
#71255=CARTESIAN_POINT('Ctrl Pts',(-20.2166931724425,26.8000389179654,-30.2487154050346));
#71256=CARTESIAN_POINT('Ctrl Pts',(-24.4824221908955,28.1114792619185,-30.0498284936597));
#71257=CARTESIAN_POINT('Ctrl Pts',(-27.891566327496,25.2315389690475,-29.8509415822849));
#71258=CARTESIAN_POINT('Ctrl Pts',(-27.3114111684648,20.8066389898312,-29.6520546709101));
#71259=CARTESIAN_POINT('Ctrl Pts',(-23.2750701159057,18.9028872355194,-29.453167759535));
#71260=CARTESIAN_POINT('Ctrl Pts',(-19.4915983718348,21.2696701567942,-29.2542808481603));
#71261=CARTESIAN_POINT('Ctrl Pts',(-19.4376856835497,25.7321149191034,-29.0553939367852));
#71262=CARTESIAN_POINT('Ctrl Pts',(-23.162873240542,28.1896131388074,-28.8565070254105));
#71263=CARTESIAN_POINT('Ctrl Pts',(-27.2440295217556,26.3839323134868,-28.6576201140354));
#71264=CARTESIAN_POINT('Ctrl Pts',(-27.9309179297455,21.9743400251241,-28.4587332026606));
#71265=CARTESIAN_POINT('Ctrl Pts',(-24.5923462561019,19.0128777149528,-28.2598462912857));
#71266=CARTESIAN_POINT('Ctrl Pts',(-20.296178804705,20.2208781554236,-28.0609593799109));
#71267=CARTESIAN_POINT('Ctrl Pts',(-18.9902292084572,24.4882913632907,-27.862072468536));
#71268=CARTESIAN_POINT('Ctrl Pts',(-21.8745544200441,27.893726417498,-27.663185557161));
#71269=CARTESIAN_POINT('Ctrl Pts',(-26.2987041204669,27.3078772365071,-27.4642986457862));
#71270=CARTESIAN_POINT('Ctrl Pts',(-28.1972598410737,23.2690895458294,-27.2654117344113));
#71271=CARTESIAN_POINT('Ctrl Pts',(-25.8256098456067,19.4886668004713,-27.0665248230364));
#71272=CARTESIAN_POINT('Ctrl Pts',(-21.3630993971404,19.4404969764257,-26.8676379116614));
#71273=CARTESIAN_POINT('Ctrl Pts',(-18.9103972393238,23.1688440578629,-26.6687510002866));
#71274=CARTESIAN_POINT('Ctrl Pts',(-20.7213287003407,27.2476731886452,-26.4698640889118));
#71275=CARTESIAN_POINT('Ctrl Pts',(-25.1318013091842,27.9288862252643,-26.2709771775369));
#71276=CARTESIAN_POINT('Ctrl Pts',(-28.0889646847377,24.5865061444081,-26.072090266162));
#71277=CARTESIAN_POINT('Ctrl Pts',(-26.875436410975,20.2918968532854,-25.8732033547871));
#71278=CARTESIAN_POINT('Ctrl Pts',(-22.6063460812538,18.9914401676168,-25.6743164434122));
#71279=CARTESIAN_POINT('Ctrl Pts',(-19.2046257494179,21.8801455209876,-25.4754295320374));
#71280=CARTESIAN_POINT('Ctrl Pts',(-19.7961679821028,26.3035376154745,-25.2765426206624));
#71281=CARTESIAN_POINT('Ctrl Pts',(-23.8373956219815,28.1968941580462,-25.0776557092874));
#71282=CARTESIAN_POINT('Ctrl Pts',(-27.6147631076054,25.8203810162416,-24.8787687979125));
#71283=CARTESIAN_POINT('Ctrl Pts',(-27.6571899876342,21.3578122722926,-24.6798818865377));
#71284=CARTESIAN_POINT('Ctrl Pts',(-23.9256895565276,18.9099102384541,-24.4809949751627));
#71285=CARTESIAN_POINT('Ctrl Pts',(-19.8491943314094,20.7260893359576,-24.2821080637879));
#71286=CARTESIAN_POINT('Ctrl Pts',(-19.1736577943654,25.137434960791,-24.083221152413));
#71287=CARTESIAN_POINT('Ctrl Pts',(-22.5198407468858,28.0902945041627,-23.8843342410382));
#71288=CARTESIAN_POINT('Ctrl Pts',(-26.8128847651328,26.8712404069166,-23.6854473296632));
#71289=CARTESIAN_POINT('Ctrl Pts',(-28.1078463864453,22.6004800256793,-23.4865604182883));
#71290=CARTESIAN_POINT('Ctrl Pts',(-25.2147656754767,19.2024800500406,-23.2876735069134));
#71291=CARTESIAN_POINT('Ctrl Pts',(-20.7921385128133,19.7997143547253,-23.0887865955386));
#71292=CARTESIAN_POINT('Ctrl Pts',(-18.9039842839965,23.8433752508465,-22.8898996841638));
#71293=CARTESIAN_POINT('Ctrl Pts',(-21.2853566362298,27.6176812207748,-22.6910127727887));
#71294=CARTESIAN_POINT('Ctrl Pts',(-25.7479762848906,27.6543650865207,-22.4921258614139));
#71295=CARTESIAN_POINT('Ctrl Pts',(-28.1910741406097,23.9197174857423,-22.2932389500389));
#71296=CARTESIAN_POINT('Ctrl Pts',(-26.3696504145205,19.8455629176561,-22.0943520386642));
#71297=CARTESIAN_POINT('Ctrl Pts',(-21.9574390796337,19.17570399899,-21.8954651272892));
#71298=CARTESIAN_POINT('Ctrl Pts',(-19.0088882588803,22.5256842813281,-21.6965782159143));
#71299=CARTESIAN_POINT('Ctrl Pts',(-20.2334661606494,26.8171559166903,-21.4976913045395));
#71300=CARTESIAN_POINT('Ctrl Pts',(-24.5058895202992,28.1066203289707,-21.2988043931646));
#71301=CARTESIAN_POINT('Ctrl Pts',(-27.9001635120761,25.2091690518364,-21.0999174817896));
#71302=CARTESIAN_POINT('Ctrl Pts',(-27.2972381245131,20.7873141456176,-20.9010305704148));
#71303=CARTESIAN_POINT('Ctrl Pts',(-23.2511506691379,18.9043653576591,-20.7021436590399));
#71304=CARTESIAN_POINT('Ctrl Pts',(-19.4799124657959,21.2905929763648,-20.5032567476651));
#71305=CARTESIAN_POINT('Ctrl Pts',(-19.448971675088,25.7532561388822,-20.30436983629));
#71306=CARTESIAN_POINT('Ctrl Pts',(-23.1867602603281,28.1915457702975,-20.1054829249152));
#71307=CARTESIAN_POINT('Ctrl Pts',(-27.2585674238914,26.364880432209,-19.9065960135404));
#71308=CARTESIAN_POINT('Ctrl Pts',(-27.9227476147789,21.9518106946394,-19.7077091021655));
#71309=CARTESIAN_POINT('Ctrl Pts',(-24.568975550759,19.0075734798047,-19.5088221907905));
#71310=CARTESIAN_POINT('Ctrl Pts',(-20.2790834056867,20.2376731579881,-19.3099352794157));
#71311=CARTESIAN_POINT('Ctrl Pts',(-18.9951183380106,24.5117524201925,-19.1110483680408));
#71312=CARTESIAN_POINT('Ctrl Pts',(-21.8969353826393,27.902294806614,-18.9121614566658));
#71313=CARTESIAN_POINT('Ctrl Pts',(-26.3180107090718,27.2936793347194,-18.713274545291));
#71314=CARTESIAN_POINT('Ctrl Pts',(-28.1957509376891,23.2451720210973,-18.5143876339161));
#71315=CARTESIAN_POINT('Ctrl Pts',(-25.804672004509,19.4770078301521,-18.3155007225413));
#71316=CARTESIAN_POINT('Ctrl Pts',(-21.3419727190624,19.451810165725,-18.1166138111664));
#71317=CARTESIAN_POINT('Ctrl Pts',(-18.9084953501721,23.192733545015,-17.9177268997915));
#71318=CARTESIAN_POINT('Ctrl Pts',(-20.7403992749922,27.2621865604517,-17.7188399884166));
#71319=CARTESIAN_POINT('Ctrl Pts',(-25.1543201064523,27.9206869235662,-17.5199530770417));
#71320=CARTESIAN_POINT('Ctrl Pts',(-28.0942388392121,24.5631286322796,-17.3210661656668));
#71321=CARTESIAN_POINT('Ctrl Pts',(-26.8586194218683,20.2748230822864,-17.1221792542919));
#71322=CARTESIAN_POINT('Ctrl Pts',(-22.5828913357095,18.9963594856784,-16.923292342917));
#71323=CARTESIAN_POINT('Ctrl Pts',(-19.1960861699567,21.9025374919005,-16.7244054315421));
#71324=CARTESIAN_POINT('Ctrl Pts',(-19.8103907182127,26.3228259164959,-16.5255185201673));
#71325=CARTESIAN_POINT('Ctrl Pts',(-23.8613111850665,28.1953544759156,-16.3266316087924));
#71326=CARTESIAN_POINT('Ctrl Pts',(-27.6263951228959,25.7994281882936,-16.1277446974175));
#71327=CARTESIAN_POINT('Ctrl Pts',(-27.6458496193105,21.3367001709045,-15.9288577860426));
#71328=CARTESIAN_POINT('Ctrl Pts',(-23.9017976415744,18.9080390947908,-15.7299708746677));
#71329=CARTESIAN_POINT('Ctrl Pts',(-19.8347055139685,20.7451785723986,-15.5310839632928));
#71330=CARTESIAN_POINT('Ctrl Pts',(-19.1818860692158,25.1599431875476,-15.3321970519179));
#71331=CARTESIAN_POINT('Ctrl Pts',(-22.5432250270827,28.0955385692284,-15.1333101405429));
#71332=CARTESIAN_POINT('Ctrl Pts',(-26.8299368798353,26.8544014591196,-14.9344232291681));
#71333=CARTESIAN_POINT('Ctrl Pts',(-28.1028968880228,22.5770316303375,-14.7355363177932));
#71334=CARTESIAN_POINT('Ctrl Pts',(-25.1923627333311,19.1939692943774,-14.5366494064184));
#71335=CARTESIAN_POINT('Ctrl Pts',(-20.7728685313203,19.8139619016018,-14.3377624950434));
#71336=CARTESIAN_POINT('Ctrl Pts',(-18.9055547423231,23.8672888126763,-14.1388755836686));
#71337=CARTESIAN_POINT('Ctrl Pts',(-21.3063244163269,27.6292862617719,-13.9399886722937));
#71338=CARTESIAN_POINT('Ctrl Pts',(-25.7690737746235,27.6429975579539,-13.7411017609188));
#71339=CARTESIAN_POINT('Ctrl Pts',(-28.1929145356861,23.8958231825571,-13.5422148495439));
#71340=CARTESIAN_POINT('Ctrl Pts',(-26.3505425479049,19.8310986785767,-13.343327938169));
#71341=CARTESIAN_POINT('Ctrl Pts',(-21.9349414606661,19.1839612333653,-13.1444410267941));
#71342=CARTESIAN_POINT('Ctrl Pts',(-19.0036742919084,22.5490752908652,-12.9455541154192));
#71343=CARTESIAN_POINT('Ctrl Pts',(-20.2503270392489,26.8341863468551,-12.7466672040443));
#71344=CARTESIAN_POINT('Ctrl Pts',(-24.5293315266039,28.1016406583841,-12.5477802926694));
#71345=CARTESIAN_POINT('Ctrl Pts',(-27.9086454298464,25.1867551755613,-12.3488933812946));
#71346=CARTESIAN_POINT('Ctrl Pts',(-27.2829657904661,20.7680625155673,-12.1500064699196));
#71347=CARTESIAN_POINT('Ctrl Pts',(-23.2272391481683,18.9059665895809,-11.9511195585448));
#71348=CARTESIAN_POINT('Ctrl Pts',(-19.4683344183123,21.3115756738845,-11.7522326471699));
#71349=CARTESIAN_POINT('Ctrl Pts',(-19.460366345071,25.7743389820187,-11.553345735795));
#71350=CARTESIAN_POINT('Ctrl Pts',(-23.2106569121722,28.1933554137386,-11.3544588244201));
#71351=CARTESIAN_POINT('Ctrl Pts',(-27.2730070606538,26.3457539670648,-11.1555719130452));
#71352=CARTESIAN_POINT('Ctrl Pts',(-27.9144614345543,21.9293237207207,-10.9566850016703));
#71353=CARTESIAN_POINT('Ctrl Pts',(-24.5455778506215,19.0023896195617,-10.7577980902953));
#71354=CARTESIAN_POINT('Ctrl Pts',(-20.262074688265,20.2545559394653,-10.5589111789205));
#71355=CARTESIAN_POINT('Ctrl Pts',(-19.0001281725137,24.5351879986362,-10.3600242675455));
#71356=CARTESIAN_POINT('Ctrl Pts',(-21.919360155923,27.9107478724438,-10.1611373561708));
#71357=CARTESIAN_POINT('Ctrl Pts',(-26.3372439557954,27.2793822371394,-9.9622504447958));
#71358=CARTESIAN_POINT('Ctrl Pts',(-28.1941189348243,23.2212625805896,-9.76336353342093));
#71359=CARTESIAN_POINT('Ctrl Pts',(-25.7836744243174,19.465456795357,-9.56447662204602));
#71360=CARTESIAN_POINT('Ctrl Pts',(-21.3209045574389,19.463231958253,-9.36558971067114));
#71361=CARTESIAN_POINT('Ctrl Pts',(-18.9067164613632,23.2166325059411,-9.16670279929625));
#71362=CARTESIAN_POINT('Ctrl Pts',(-20.7595443069883,27.2766015709828,-8.96781588792135));
#71363=CARTESIAN_POINT('Ctrl Pts',(-25.17679639808,27.9123718112153,-8.76892897654648));
#71364=CARTESIAN_POINT('Ctrl Pts',(-28.0993925841408,24.5397242802923,-8.57004206517157));
#71365=CARTESIAN_POINT('Ctrl Pts',(-26.841714765474,20.2578361057771,-8.37115515379669));
#71366=CARTESIAN_POINT('Ctrl Pts',(-22.5594622239401,19.001399475801,-8.17226824242178));
#71367=CARTESIAN_POINT('Ctrl Pts',(-19.1876619700672,21.9249731250532,-7.97338133104692));
#71368=CARTESIAN_POINT('Ctrl Pts',(-19.8247125556472,26.3420407480393,-7.774494419672));
#71369=CARTESIAN_POINT('Ctrl Pts',(-23.8852185055144,28.1936917048104,-7.57560750829713));
#71370=CARTESIAN_POINT('Ctrl Pts',(-27.637919125872,25.7784157602055,-7.37672059692223));
#71371=CARTESIAN_POINT('Ctrl Pts',(-27.6344007231541,21.3156467256866,-7.17783368554734));
#71372=CARTESIAN_POINT('Ctrl Pts',(-23.8778964111469,18.9062909635603,-6.97894677417245));
#71373=CARTESIAN_POINT('Ctrl Pts',(-19.8203151535427,20.7643421395393,-6.78005986279756));
#71374=CARTESIAN_POINT('Ctrl Pts',(-19.1902300999215,25.1824087596598,-6.58117295142267));
#71375=CARTESIAN_POINT('Ctrl Pts',(-22.5666359921586,28.1006621903073,-6.38228604004778));
#71376=CARTESIAN_POINT('Ctrl Pts',(-26.8469020872991,26.8374749558051,-6.18339912867289));
#71377=CARTESIAN_POINT('Ctrl Pts',(-28.0978267506276,22.553609024045,-5.98451221729801));
#71378=CARTESIAN_POINT('Ctrl Pts',(-25.1699162774664,19.1855739743799,-5.78562530592311));
#71379=CARTESIAN_POINT('Ctrl Pts',(-20.7536721467801,19.8283084551716,-5.58673839454821));
#71380=CARTESIAN_POINT('Ctrl Pts',(-18.9072482789147,23.8911939734695,-5.38785148317334));
#71381=CARTESIAN_POINT('Ctrl Pts',(-21.3273516575109,27.6407832138433,-5.18896457179843));
#71382=CARTESIAN_POINT('Ctrl Pts',(-25.7901124685678,27.6315215771305,-4.99007766042355));
#71383=CARTESIAN_POINT('Ctrl Pts',(-28.1946319064429,23.871919722213,-4.79119074904866));
#71384=CARTESIAN_POINT('Ctrl Pts',(-26.3313604773578,19.8167329920888,-4.59230383767377));
#71385=CARTESIAN_POINT('Ctrl Pts',(-21.9124866452764,19.1923341686068,-4.39341692629887));
#71386=CARTESIAN_POINT('Ctrl Pts',(-18.9985808031649,22.5724928302568,-4.19453001492399));
#71387=CARTESIAN_POINT('Ctrl Pts',(-20.2672753614501,26.851129757176,-3.99564310354909));
#71388=CARTESIAN_POINT('Ctrl Pts',(-24.552747588628,28.0965403821135,-3.7967561921742));
#71389=CARTESIAN_POINT('Ctrl Pts',(-27.9170118560474,25.1642979341598,-3.59786928079932));
#71390=CARTESIAN_POINT('Ctrl Pts',(-27.2685945445218,20.7488846098228,-3.39898236942442));
#71391=CARTESIAN_POINT('Ctrl Pts',(-23.2033361866205,18.9076908888542,-3.20009545804954));
#71392=CARTESIAN_POINT('Ctrl Pts',(-19.4568645361867,21.33261769334,-3.00120854667464));
#71393=CARTESIAN_POINT('Ctrl Pts',(-19.4718693915553,25.7953628898457,-2.80232163529976));
#71394=CARTESIAN_POINT('Ctrl Pts',(-23.2345625628451,28.1950420211776,-2.60343472392486));
#71395=CARTESIAN_POINT('Ctrl Pts',(-27.2873480494116,26.32655342488,-2.40454781254998));
#71396=CARTESIAN_POINT('Ctrl Pts',(-27.9060596086441,21.9068796992424,-2.20566090117508));
#71397=CARTESIAN_POINT('Ctrl Pts',(-24.5221537756973,18.9973262715892,-2.00677398980019));
#71398=CARTESIAN_POINT('Ctrl Pts',(-20.2451531031481,20.2715260524842,-1.8078870784253));
#71399=CARTESIAN_POINT('Ctrl Pts',(-19.0052585792127,24.5585974776105,-1.60900016705041));
#71400=CARTESIAN_POINT('Ctrl Pts',(-21.9418281456682,27.9190853909925,-1.41011325567552));
#71401=CARTESIAN_POINT('Ctrl Pts',(-26.3564033509824,27.2649863226212,-1.21122634430063));
#71402=CARTESIAN_POINT('Ctrl Pts',(-28.1923638757249,23.1973618578745,-1.01233943292574));
#71403=CARTESIAN_POINT('Ctrl Pts',(-25.7626176614396,19.4540140021729,-0.813452521550849));
#71404=CARTESIAN_POINT('Ctrl Pts',(-21.2998954705483,19.4747620513473,-0.614565610175962));
#71405=CARTESIAN_POINT('Ctrl Pts',(-18.9050606200354,23.2405403073507,-0.415678698801063));
#71406=CARTESIAN_POINT('Ctrl Pts',(-20.7787632890114,27.2909178382595,-0.216791787426177));
#71407=CARTESIAN_POINT('Ctrl Pts',(-25.1992295884757,27.9039411085512,-0.0179048760512818));
#71408=CARTESIAN_POINT('Ctrl Pts',(-28.1044257829564,24.5162937086299,0.180982035323599));
#71409=CARTESIAN_POINT('Ctrl Pts',(-26.8247228897429,20.2409363738893,0.379868946698492));
#71410=CARTESIAN_POINT('Ctrl Pts',(-22.5360593667856,19.0065600044316,0.578755858073388));
#71411=CARTESIAN_POINT('Ctrl Pts',(-19.1793533729794,21.9474518259315,0.777642769448271));
#71412=CARTESIAN_POINT('Ctrl Pts',(-19.8391331148967,26.3611816009374,0.976529680823165));
#71413=CARTESIAN_POINT('Ctrl Pts',(-23.9091169498129,28.1919058887919,1.17541659219806));
#71414=CARTESIAN_POINT('Ctrl Pts',(-27.649334811163,25.7573442887791,1.37430350357295));
#71415=CARTESIAN_POINT('Ctrl Pts',(-27.6228436025457,21.2946524945269,1.57319041494784));
#71416=CARTESIAN_POINT('Ctrl Pts',(-23.8539864985959,18.9046658910859,1.77207732632273));
#71417=CARTESIAN_POINT('Ctrl Pts',(-19.8060236314572,20.7835795295708,1.97096423769762));
#71418=CARTESIAN_POINT('Ctrl Pts',(-19.1986896653768,25.2048310818198,2.16985114907251));
#71419=CARTESIAN_POINT('Ctrl Pts',(-22.5900730217541,28.1056652316304,2.3687380604474));
#71420=CARTESIAN_POINT('Ctrl Pts',(-26.863779937969,26.8204613455031,2.56762497182229));
#71421=CARTESIAN_POINT('Ctrl Pts',(-28.092636108612,22.5302128274693,2.76651188319718));
#71422=CARTESIAN_POINT('Ctrl Pts',(-25.1474269026838,19.1772943125133,2.96539879457208));
#71423=CARTESIAN_POINT('Ctrl Pts',(-20.7345498678712,19.8427536352697,3.16428570594695));
#71424=CARTESIAN_POINT('Ctrl Pts',(-18.909064848895,23.9150900997717,3.36317261732185));
#71425=CARTESIAN_POINT('Ctrl Pts',(-21.3484378025882,27.6521717723351,3.56205952869672));
#71426=CARTESIAN_POINT('Ctrl Pts',(-25.8110918092263,27.6199374481484,3.76094644007167));
#71427=CARTESIAN_POINT('Ctrl Pts',(-28.1962262073723,23.8480077381194,3.95983335144652));
#71428=CARTESIAN_POINT('Ctrl Pts',(-26.3121047111783,19.8024662388638,4.15872026282142));
#71429=CARTESIAN_POINT('Ctrl Pts',(-21.8900752284872,19.2008225828429,4.3576071741963));
#71430=CARTESIAN_POINT('Ctrl Pts',(-18.9936079276205,22.5959362789698,4.55649408557119));
#71431=CARTESIAN_POINT('Ctrl Pts',(-20.2843106781455,26.8679856986754,4.75538099694606));
#71432=CARTESIAN_POINT('Ctrl Pts',(-24.5761370858766,28.0913196353095,4.95426790832101));
#71433=CARTESIAN_POINT('Ctrl Pts',(-27.9252625689805,25.1417979227188,5.15315481969587));
#71434=CARTESIAN_POINT('Ctrl Pts',(-27.2541247674984,20.7297809365728,5.35204173107077));
#71435=CARTESIAN_POINT('Ctrl Pts',(-23.1794424178906,18.9095382097875,5.55092864244564));
#71436=CARTESIAN_POINT('Ctrl Pts',(-19.4455031233554,21.3537184771459,5.74981555382054));
#71437=CARTESIAN_POINT('Ctrl Pts',(-19.4834805097256,25.8163273052579,5.9487024651954));
#71438=CARTESIAN_POINT('Ctrl Pts',(-23.2584765788788,28.1966055479217,6.14758937657036));
#71439=CARTESIAN_POINT('Ctrl Pts',(-27.301590010148,26.3072793144432,6.3464762879452));
#71440=CARTESIAN_POINT('Ctrl Pts',(-27.8975423596855,21.8844792249412,6.54536319932011));
#71441=CARTESIAN_POINT('Ctrl Pts',(-24.4987039466931,18.9923835700593,6.74425011069501));
#71442=CARTESIAN_POINT('Ctrl Pts',(-20.2283190987355,20.2885830473596,6.94313702206986));
#71443=CARTESIAN_POINT('Ctrl Pts',(-19.0105094221587,24.5819802367954,7.14202393344476));
#71444=CARTESIAN_POINT('Ctrl Pts',(-21.9643387565034,27.9273071413271,7.34091084481965));
#71445=CARTESIAN_POINT('Ctrl Pts',(-26.3754883869345,27.2504919726375,7.53979775619457));
#71446=CARTESIAN_POINT('Ctrl Pts',(-28.190485806898,23.1734704862893,7.73868466756944));
#71447=CARTESIAN_POINT('Ctrl Pts',(-25.7415022738518,19.4426797538188,7.93757157894435));
#71448=CARTESIAN_POINT('Ctrl Pts',(-21.2789460151029,19.4864001394758,8.13645849031921));
#71449=CARTESIAN_POINT('Ctrl Pts',(-18.9035278700662,23.264456315719,8.3353454016941));
#71450=CARTESIAN_POINT('Ctrl Pts',(-20.7980557117841,27.3051349829202,8.53423231306901));
#71451=CARTESIAN_POINT('Ctrl Pts',(-25.22161908319,27.8953950389761,8.73311922444391));
#71452=CARTESIAN_POINT('Ctrl Pts',(-28.109338302286,24.4928375381713,8.93200613581879));
#71453=CARTESIAN_POINT('Ctrl Pts',(-26.8076442449367,20.2241243344435,9.13089304719368));
#71454=CARTESIAN_POINT('Ctrl Pts',(-22.5126833843905,19.0118409348233,9.32977995856857));
#71455=CARTESIAN_POINT('Ctrl Pts',(-19.1711605988596,21.9699729988797,9.52866686994343));
#71456=CARTESIAN_POINT('Ctrl Pts',(-19.8536520138361,26.3802479679834,9.72755378131836));
#71457=CARTESIAN_POINT('Ctrl Pts',(-23.9330058846853,28.1899970751816,9.92644069269323));
#71458=CARTESIAN_POINT('Ctrl Pts',(-27.6606418762687,25.7362143323797,10.1253276040681));
#71459=CARTESIAN_POINT('Ctrl Pts',(-27.6111785637333,21.2737180337446,10.324214515443));
#71460=CARTESIAN_POINT('Ctrl Pts',(-23.8300685375021,18.9031639204299,10.5231014268179));
#71461=CARTESIAN_POINT('Ctrl Pts',(-19.7918313264183,20.802890232728,10.7219883381927));
#71462=CARTESIAN_POINT('Ctrl Pts',(-19.2072645414147,25.2272095598663,10.9208752495676));
#71463=CARTESIAN_POINT('Ctrl Pts',(-22.6135354948195,28.1105475606235,11.1197621609425));
#71464=CARTESIAN_POINT('Ctrl Pts',(-26.8805699846046,26.8033610790514,11.3186490723174));
#71465=CARTESIAN_POINT('Ctrl Pts',(-28.0873250995208,22.5068436605784,11.5175359836923));
#71466=CARTESIAN_POINT('Ctrl Pts',(-25.1248952049213,19.1691305281772,11.7164228950672));
#71467=CARTESIAN_POINT('Ctrl Pts',(-20.7155022013083,19.8572970591188,11.9153098064422));
#71468=CARTESIAN_POINT('Ctrl Pts',(-18.9110044041271,23.9389765583675,12.114196717817));
#71469=CARTESIAN_POINT('Ctrl Pts',(-21.3695822928042,27.6634516354658,12.3130836291919));
#71470=CARTESIAN_POINT('Ctrl Pts',(-25.8320112406749,27.6082454779718,12.5119705405668));
#71471=CARTESIAN_POINT('Ctrl Pts',(-28.1976973962274,23.8240878639119,12.7108574519416));
#71472=CARTESIAN_POINT('Ctrl Pts',(-26.2927757596185,19.7882987969516,12.9097443633166));
#71473=CARTESIAN_POINT('Ctrl Pts',(-21.867707804171,19.209426251142,13.1086312746914));
#71474=CARTESIAN_POINT('Ctrl Pts',(-18.9887557970497,22.6194050157843,13.3075181860663));
#71475=CARTESIAN_POINT('Ctrl Pts',(-20.3014325379218,26.8847537246933,13.5064050974412));
#71476=CARTESIAN_POINT('Ctrl Pts',(-24.5994993985599,28.0859785563148,13.7052920088161));
#71477=CARTESIAN_POINT('Ctrl Pts',(-27.9333973500122,25.1192557374586,13.904178920191));
#71478=CARTESIAN_POINT('Ctrl Pts',(-27.2395568428261,20.7107520020393,14.1030658315659));
#71479=CARTESIAN_POINT('Ctrl Pts',(-23.1555584751319,18.9115085034293,14.3019527429409));
#71480=CARTESIAN_POINT('Ctrl Pts',(-19.434250480881,21.3748774661597,14.5008396543157));
#71481=CARTESIAN_POINT('Ctrl Pts',(-19.4951993919029,25.8372316727265,14.6997265656906));
#71482=CARTESIAN_POINT('Ctrl Pts',(-23.2823983265842,28.1980459525395,14.8986134770655));
#71483=CARTESIAN_POINT('Ctrl Pts',(-27.31573256547,26.2879321464927,15.0975003884403));
#71484=CARTESIAN_POINT('Ctrl Pts',(-27.8889099133742,21.8621228913996,15.2963872998152));
#71485=CARTESIAN_POINT('Ctrl Pts',(-24.4752289849978,18.9875616459468,15.4952742111901));
#71486=CARTESIAN_POINT('Ctrl Pts',(-20.2115731211057,20.3057264721038,15.694161122565));
#71487=CARTESIAN_POINT('Ctrl Pts',(-19.0158805622113,24.605335656579,15.8930480339399));
#71488=CARTESIAN_POINT('Ctrl Pts',(-21.9868913919278,27.935412905582,16.0919349453148));
#71489=CARTESIAN_POINT('Ctrl Pts',(-26.3944985579235,27.2358995712689,16.2908218566897));
#71490=CARTESIAN_POINT('Ctrl Pts',(-28.1884847781097,23.1495890989232,16.4897087680645));
#71491=CARTESIAN_POINT('Ctrl Pts',(-25.7203288210831,19.431454350637,16.6885956794395));
#71492=CARTESIAN_POINT('Ctrl Pts',(-21.2580567462356,19.4981459142451,16.8874825908143));
#71493=CARTESIAN_POINT('Ctrl Pts',(-18.9021182520713,23.2883798973039,17.0863695021893));
#71494=CARTESIAN_POINT('Ctrl Pts',(-20.8174210640831,27.3192526282294,17.2852564135641));
#71495=CARTESIAN_POINT('Ctrl Pts',(-25.2439642889312,27.8867338289495,17.4841433249391));
#71496=CARTESIAN_POINT('Ctrl Pts',(-28.1141300119542,24.4693563904737,17.6830302363139));
#71497=CARTESIAN_POINT('Ctrl Pts',(-26.7904792836169,20.207400432936,17.8819171476888));
#71498=CARTESIAN_POINT('Ctrl Pts',(-22.4893348961867,19.0172421270384,18.0808040590636));
#71499=CARTESIAN_POINT('Ctrl Pts',(-19.163083864806,21.9925360471172,18.2796909704387));
#71500=CARTESIAN_POINT('Ctrl Pts',(-19.8682688677335,26.3992393439442,18.4785778818134));
#71501=CARTESIAN_POINT('Ctrl Pts',(-23.9568846771073,28.1879653145608,18.6774647931884));
#71502=CARTESIAN_POINT('Ctrl Pts',(-27.6718400215669,25.7150264509229,18.8763517045632));
#71503=CARTESIAN_POINT('Ctrl Pts',(-27.599405915825,21.2528438980745,19.0752386159382));
#71504=CARTESIAN_POINT('Ctrl Pts',(-23.8061431616591,18.9017850913926,19.274125527313));
#71505=CARTESIAN_POINT('Ctrl Pts',(-19.7777386145031,20.8222737373031,19.4730124386879));
#71506=CARTESIAN_POINT('Ctrl Pts',(-19.2159545008122,25.2495436007996,19.6718993500629));
#71507=CARTESIAN_POINT('Ctrl Pts',(-22.6370227896307,28.1153090479114,19.8707862614377));
#71508=CARTESIAN_POINT('Ctrl Pts',(-26.897271782292,26.7861746095843,20.0696731728126));
#71509=CARTESIAN_POINT('Ctrl Pts',(-28.0818938640886,22.4835021426237,20.2685600841875));
#71510=CARTESIAN_POINT('Ctrl Pts',(-25.1023217812389,19.1610828377014,20.4674469955624));
#71511=CARTESIAN_POINT('Ctrl Pts',(-20.696529651829,19.871938341337,20.6663339069373));
#71512=CARTESIAN_POINT('Ctrl Pts',(-18.9130668932155,23.9628527162975,20.8652208183122));
#71513=CARTESIAN_POINT('Ctrl Pts',(-21.3907845678583,27.6746225043341,21.0641077296871));
#71514=CARTESIAN_POINT('Ctrl Pts',(-25.8528702085764,27.5964459764219,21.2629946410619));
#71515=CARTESIAN_POINT('Ctrl Pts',(-28.1990454340238,23.8001607334355,21.4618815524368));
#71516=CARTESIAN_POINT('Ctrl Pts',(-26.2733741348695,19.7742310417702,21.6607684638117));
#71517=CARTESIAN_POINT('Ctrl Pts',(-21.8453849650347,19.2181449455185,21.8596553751866));
#71518=CARTESIAN_POINT('Ctrl Pts',(-18.9840245400275,22.6428984188101,22.0585422865615));
#71519=CARTESIAN_POINT('Ctrl Pts',(-20.3186404870729,26.9014333908998,22.2574291979364));
#71520=CARTESIAN_POINT('Ctrl Pts',(-24.6228339076079,28.0805172866607,22.4563161093113));
#71521=CARTESIAN_POINT('Ctrl Pts',(-27.9414159835821,25.0966719757166,22.6552030206861));
#71522=CARTESIAN_POINT('Ctrl Pts',(-27.2248911565355,20.6917983104636,22.8540899320611));
#71523=CARTESIAN_POINT('Ctrl Pts',(-23.1316849912363,18.9136017175688,23.0529768434359));
#71524=CARTESIAN_POINT('Ctrl Pts',(-19.4231069069434,21.3960940996979,23.2518637548108));
#71525=CARTESIAN_POINT('Ctrl Pts',(-19.5070257275519,25.858075438311,23.4507506661858));
#71526=CARTESIAN_POINT('Ctrl Pts',(-23.3063271720676,28.199363196867,23.6496375775607));
#71527=CARTESIAN_POINT('Ctrl Pts',(-27.3297753406174,26.2685124336933,23.8485244889355));
#71528=CARTESIAN_POINT('Ctrl Pts',(-27.8801624984611,21.8398112910477,24.0474114003104));
#71529=CARTESIAN_POINT('Ctrl Pts',(-24.4517295126615,18.9828606269937,24.2462983116853));
#71530=CARTESIAN_POINT('Ctrl Pts',(-20.194915614014,20.3229558725011,24.4451852230601));
#71531=CARTESIAN_POINT('Ctrl Pts',(-19.021371857025,24.628663117958,24.6440721344351));
#71532=CARTESIAN_POINT('Ctrl Pts',(-22.0094854543603,27.9434024691856,24.84295904581));
#71533=CARTESIAN_POINT('Ctrl Pts',(-26.4134333601426,27.221209504779,25.0418459571849));
#71534=CARTESIAN_POINT('Ctrl Pts',(-28.1863608425043,23.1257183293854,25.2407328685598));
#71535=CARTESIAN_POINT('Ctrl Pts',(-25.6990978639753,19.4203380886039,25.4396197799346));
#71536=CARTESIAN_POINT('Ctrl Pts',(-21.2372282179111,19.5099990672052,25.6385066913096));
#71537=CARTESIAN_POINT('Ctrl Pts',(-18.900831802597,23.3123104128807,25.8373936026844));
#71538=CARTESIAN_POINT('Ctrl Pts',(-20.836858834276,27.3332704100622,26.0362805140593));
#71539=CARTESIAN_POINT('Ctrl Pts',(-25.2662646107047,27.8779576891496,26.2351674254342));
#71540=CARTESIAN_POINT('Ctrl Pts',(-28.118800790419,24.4458509233144,26.4340543368091));
#71541=CARTESIAN_POINT('Ctrl Pts',(-26.7732284503756,20.1907650453861,26.632941248184));
#71542=CARTESIAN_POINT('Ctrl Pts',(-22.4660145402437,19.0227635647297,26.8318281595589));
#71543=CARTESIAN_POINT('Ctrl Pts',(-19.1551233482742,22.0151401333725,27.0307150709338));
#71544=CARTESIAN_POINT('Ctrl Pts',(-19.8829833583075,26.4181556775741,27.2296019823087));
#71545=CARTESIAN_POINT('Ctrl Pts',(-23.9807525639513,28.1858098072997,27.4284888936836));
#71546=CARTESIAN_POINT('Ctrl Pts',(-27.6829291964891,25.6937828173813,27.6273758050585));
#71547=CARTESIAN_POINT('Ctrl Pts',(-27.5875255059658,21.2320275977716,27.8262627164333));
#71548=CARTESIAN_POINT('Ctrl Pts',(-23.7822118827208,18.9005351860905,28.0251496278082));
#71549=CARTESIAN_POINT('Ctrl Pts',(-19.7637442119418,20.8417186808364,28.2240365391831));
#71550=CARTESIAN_POINT('Ctrl Pts',(-19.2247624424421,25.2718530975856,28.422923450558));
#71551=CARTESIAN_POINT('Ctrl Pts',(-22.6605283753441,28.1199108878517,28.6218103619329));
#71552=CARTESIAN_POINT('Ctrl Pts',(-26.9138960448389,26.7689754274264,28.8206972733079));
#71553=CARTESIAN_POINT('Ctrl Pts',(-28.0763214806764,22.4600509857223,29.0195841846826));
#71554=CARTESIAN_POINT('Ctrl Pts',(-25.0797470061916,19.1534118631149,29.2184710960576));
#71555=CARTESIAN_POINT('Ctrl Pts',(-20.6775576135736,19.8861852793049,29.4173580074325));
#71556=CARTESIAN_POINT('Ctrl Pts',(-18.9153941038522,23.9876474856138,29.6162449188074));
#71557=CARTESIAN_POINT('Ctrl Pts',(-21.4117760584397,27.6839215662933,29.8151318301822));
#71558=CARTESIAN_POINT('Ctrl Pts',(-25.8741757107666,27.5879272819239,30.0140187415572));
#71559=CARTESIAN_POINT('Ctrl Pts',(-28.1997986655813,23.7685188331541,30.212948538688));
#71560=CARTESIAN_POINT('Ctrl Pts',(-26.902989493669,21.1060008116438,30.345582698694));
#71561=CARTESIAN_POINT('Ctrl Pts',(-25.8339781016064,20.3445297244528,30.4119212215749));
#71562=CARTESIAN_POINT('Ctrl Pts',(-25.303008770126,27.07863963872,30.));
#71563=CARTESIAN_POINT('Ctrl Pts',(-25.372165991601,27.0367793117585,30.));
#71564=CARTESIAN_POINT('Ctrl Pts',(-25.4398095734417,26.9927043362926,30.));
#71565=CARTESIAN_POINT('Ctrl Pts',(-25.5058238888464,26.9464145021148,30.));
#71566=CARTESIAN_POINT('Ctrl Pts',(-25.6040445244783,26.8775413053185,30.));
#71567=CARTESIAN_POINT('Ctrl Pts',(-25.6986602703167,26.8037666196724,30.));
#71568=CARTESIAN_POINT('Ctrl Pts',(-25.7895165324835,26.7255041386418,29.9999999999999));
#71569=CARTESIAN_POINT('Ctrl Pts',(-25.8831309934207,26.6448657786811,29.9999999999999));
#71570=CARTESIAN_POINT('Ctrl Pts',(-25.9727548341034,26.5594622354632,29.9999999999999));
#71571=CARTESIAN_POINT('Ctrl Pts',(-26.0581747949051,26.4697105300558,29.9999999999999));
#71572=CARTESIAN_POINT('Ctrl Pts',(-26.1435947557068,26.3799588246483,29.9999999999999));
#71573=CARTESIAN_POINT('Ctrl Pts',(-26.2248112247842,26.2858579925564,29.9999999999999));
#71574=CARTESIAN_POINT('Ctrl Pts',(-26.3015603633575,26.1878035338793,29.9999999999999));
#71575=CARTESIAN_POINT('Ctrl Pts',(-26.3266580727016,26.1557387791535,29.9999999999999));
#71576=CARTESIAN_POINT('Ctrl Pts',(-26.351277639249,26.1232511324394,29.9999999999999));
#71577=CARTESIAN_POINT('Ctrl Pts',(-26.3754085552229,26.090354191029,29.9999999999999));
#71578=CARTESIAN_POINT('Ctrl Pts',(-26.3882478224815,26.0728508097559,29.9999999999999));
#71579=CARTESIAN_POINT('Ctrl Pts',(-26.40095096979,26.0552282690474,29.9999999999999));
#71580=CARTESIAN_POINT('Ctrl Pts',(-26.4135007908628,26.0375110010851,29.9999999999999));
#71581=CARTESIAN_POINT('Ctrl Pts',(-26.4827541683328,25.9397422250354,29.9999999999999));
#71582=CARTESIAN_POINT('Ctrl Pts',(-26.5474353352631,25.838967580728,29.9999999999999));
#71583=CARTESIAN_POINT('Ctrl Pts',(-26.6073791953875,25.7355801632597,29.9999999999999));
#71584=CARTESIAN_POINT('Ctrl Pts',(-26.6670422084197,25.632677133275,29.9999999999999));
#71585=CARTESIAN_POINT('Ctrl Pts',(-26.7220124756955,25.5271848669968,29.9999999999999));
#71586=CARTESIAN_POINT('Ctrl Pts',(-26.7720800027759,25.4194716712384,29.9999999999999));
#71587=CARTESIAN_POINT('Ctrl Pts',(-26.8217631081094,25.3125855044405,29.9999999999999));
#71588=CARTESIAN_POINT('Ctrl Pts',(-26.8666187072,25.2035115547606,29.9999999999999));
#71589=CARTESIAN_POINT('Ctrl Pts',(-26.9063912512661,25.0926034302957,29.9999999999999));
#71590=CARTESIAN_POINT('Ctrl Pts',(-26.9261217035927,25.0375838806596,29.9999999999999));
#71591=CARTESIAN_POINT('Ctrl Pts',(-26.9446004248126,24.9821129247898,29.9999999999999));
#71592=CARTESIAN_POINT('Ctrl Pts',(-26.9617912883676,24.9262340987148,29.9999999999999));
#71593=CARTESIAN_POINT('Ctrl Pts',(-26.9712190886198,24.8955890756259,29.9999999999999));
#71594=CARTESIAN_POINT('Ctrl Pts',(-26.9802594893109,24.8648213882773,29.9999999999999));
#71595=CARTESIAN_POINT('Ctrl Pts',(-26.9889060941125,24.8339383022564,29.9999999999999));
#71596=CARTESIAN_POINT('Ctrl Pts',(-26.9958124014672,24.8092710381662,29.9999999999999));
#71597=CARTESIAN_POINT('Ctrl Pts',(-27.0024674727593,24.7845301541386,29.9999999999999));
#71598=CARTESIAN_POINT('Ctrl Pts',(-27.0088679029781,24.759719389574,29.9999999999999));
#71599=CARTESIAN_POINT('Ctrl Pts',(-27.0128989714829,24.7440932694231,29.9999999999999));
#71600=CARTESIAN_POINT('Ctrl Pts',(-27.01682673476,24.7284482963229,29.9999999999999));
#71601=CARTESIAN_POINT('Ctrl Pts',(-27.0206502351512,24.7127873566539,29.9999999999999));
#71602=CARTESIAN_POINT('Ctrl Pts',(-27.0478608574413,24.6013334870476,29.9999999999999));
#71603=CARTESIAN_POINT('Ctrl Pts',(-27.0698033338671,24.489039214073,30.));
#71604=CARTESIAN_POINT('Ctrl Pts',(-27.0862843013029,24.3762416801257,30.));
#71605=CARTESIAN_POINT('Ctrl Pts',(-27.1023222682183,24.2664760899297,30.));
#71606=CARTESIAN_POINT('Ctrl Pts',(-27.1131883921371,24.1562332253948,30.));
#71607=CARTESIAN_POINT('Ctrl Pts',(-27.1186562223202,24.0458250748967,29.9999999999999));
#71608=CARTESIAN_POINT('Ctrl Pts',(-27.1239898578829,23.9381266244706,30.));
#71609=CARTESIAN_POINT('Ctrl Pts',(-27.1241869291797,23.8302703359097,30.));
#71610=CARTESIAN_POINT('Ctrl Pts',(-27.1189905917103,23.7225562298034,30.));
#71611=CARTESIAN_POINT('Ctrl Pts',(-27.1136362903252,23.6115677131976,30.));
#71612=CARTESIAN_POINT('Ctrl Pts',(-27.1025545953272,23.5007293906131,30.));
#71613=CARTESIAN_POINT('Ctrl Pts',(-27.08589991268,23.3903958165813,29.9999999999999));
#71614=CARTESIAN_POINT('Ctrl Pts',(-27.0837870586004,23.3763986275059,30.));
#71615=CARTESIAN_POINT('Ctrl Pts',(-27.0815846280796,23.3624109567061,29.9999999999999));
#71616=CARTESIAN_POINT('Ctrl Pts',(-27.079294639142,23.3484431143664,29.9999999999999));
#71617=CARTESIAN_POINT('Ctrl Pts',(-27.0612875599913,23.2386085040589,30.));
#71618=CARTESIAN_POINT('Ctrl Pts',(-27.0378465367693,23.1298348295592,30.0000000000001));
#71619=CARTESIAN_POINT('Ctrl Pts',(-27.0092238737585,23.0224446555996,30.));
#71620=CARTESIAN_POINT('Ctrl Pts',(-26.9803377976117,22.9140661744904,30.));
#71621=CARTESIAN_POINT('Ctrl Pts',(-26.9461737508747,22.807095979831,30.));
#71622=CARTESIAN_POINT('Ctrl Pts',(-26.9069416225134,22.7018862518515,30.));
#71623=CARTESIAN_POINT('Ctrl Pts',(-26.867984525552,22.5974140820921,30.));
#71624=CARTESIAN_POINT('Ctrl Pts',(-26.8240295442672,22.494677081558,30.));
#71625=CARTESIAN_POINT('Ctrl Pts',(-26.7752423137273,22.3940514357048,30.));
#71626=CARTESIAN_POINT('Ctrl Pts',(-26.7387462248728,22.3187767691279,30.));
#71627=CARTESIAN_POINT('Ctrl Pts',(-26.6995451305428,22.2446842031591,30.));
#71628=CARTESIAN_POINT('Ctrl Pts',(-26.657696641436,22.171946338547,30.));
#71629=CARTESIAN_POINT('Ctrl Pts',(-26.6486184427499,22.1561673032448,30.0000000000001));
#71630=CARTESIAN_POINT('Ctrl Pts',(-26.6394156284804,22.140452073176,30.));
#71631=CARTESIAN_POINT('Ctrl Pts',(-26.6300887346912,22.1248025043154,30.));
#71632=CARTESIAN_POINT('Ctrl Pts',(-26.6211333069317,22.1097762172616,30.));
#71633=CARTESIAN_POINT('Ctrl Pts',(-26.6120689232449,22.0948195888436,30.));
#71634=CARTESIAN_POINT('Ctrl Pts',(-26.6028964652153,22.0799340773755,30.));
#71635=CARTESIAN_POINT('Ctrl Pts',(-26.5446915134282,21.9854762478021,30.));
#71636=CARTESIAN_POINT('Ctrl Pts',(-26.4821368037367,21.8938773251799,30.));
#71637=CARTESIAN_POINT('Ctrl Pts',(-26.41541661494,21.8055000644728,30.));
#71638=CARTESIAN_POINT('Ctrl Pts',(-26.3486964261433,21.7171228037657,30.));
#71639=CARTESIAN_POINT('Ctrl Pts',(-26.2778101710931,21.6319664859985,30.));
#71640=CARTESIAN_POINT('Ctrl Pts',(-26.2029099940981,21.5504386578285,30.));
#71641=CARTESIAN_POINT('Ctrl Pts',(-26.1817683455626,21.5274262597516,30.));
#71642=CARTESIAN_POINT('Ctrl Pts',(-26.1603067285946,21.5047032650586,30.));
#71643=CARTESIAN_POINT('Ctrl Pts',(-26.138528200149,21.4822796060299,30.));
#71644=CARTESIAN_POINT('Ctrl Pts',(-26.1253039434922,21.4686636161837,30.));
#71645=CARTESIAN_POINT('Ctrl Pts',(-26.111962835437,21.4551580014475,30.));
#71646=CARTESIAN_POINT('Ctrl Pts',(-26.0985055360817,21.441765051903,30.));
#71647=CARTESIAN_POINT('Ctrl Pts',(-26.0843007187565,21.4276281588533,30.));
#71648=CARTESIAN_POINT('Ctrl Pts',(-26.0699722263908,21.4136225955588,30.));
#71649=CARTESIAN_POINT('Ctrl Pts',(-26.055525011651,21.3997543967752,30.));
#71650=CARTESIAN_POINT('Ctrl Pts',(-25.9793348914314,21.3266178267456,30.));
#71651=CARTESIAN_POINT('Ctrl Pts',(-25.8998107558415,21.2572639685655,30.));
#71652=CARTESIAN_POINT('Ctrl Pts',(-25.8170969210098,21.1920390863215,30.0000000000001));
#71653=CARTESIAN_POINT('Ctrl Pts',(-25.7366332074316,21.1285885613431,30.0000000000001));
#71654=CARTESIAN_POINT('Ctrl Pts',(-25.6531504319194,21.0690451049871,30.));
#71655=CARTESIAN_POINT('Ctrl Pts',(-25.5667624437507,21.0137725368625,30.));
#71656=CARTESIAN_POINT('Ctrl Pts',(-25.519325225581,20.9834213627177,30.));
#71657=CARTESIAN_POINT('Ctrl Pts',(-25.4710117067709,20.954358818334,30.));
#71658=CARTESIAN_POINT('Ctrl Pts',(-25.421839063434,20.9266516823442,30.));
#71659=CARTESIAN_POINT('Ctrl Pts',(-25.4258417217708,20.9227079640058,-75.));
#71660=CARTESIAN_POINT('Ctrl Pts',(-25.4842059320672,20.955216390944,-75.));
#71661=CARTESIAN_POINT('Ctrl Pts',(-25.5413694620915,20.9896046533121,-75.));
#71662=CARTESIAN_POINT('Ctrl Pts',(-25.5972316032547,21.0258485698905,-75.));
#71663=CARTESIAN_POINT('Ctrl Pts',(-25.6827790864234,21.0813526336248,-75.));
#71664=CARTESIAN_POINT('Ctrl Pts',(-25.7652758004629,21.1412057069617,-75.));
#71665=CARTESIAN_POINT('Ctrl Pts',(-25.8446406274899,21.2050026168559,-75.));
#71666=CARTESIAN_POINT('Ctrl Pts',(-25.926562532402,21.270855017495,-75.));
#71667=CARTESIAN_POINT('Ctrl Pts',(-26.0051480234115,21.3409098030885,-75.));
#71668=CARTESIAN_POINT('Ctrl Pts',(-26.0802881636455,21.4147745487126,-75.));
#71669=CARTESIAN_POINT('Ctrl Pts',(-26.1554000536204,21.4886115235847,-75.));
#71670=CARTESIAN_POINT('Ctrl Pts',(-26.2270696501425,21.5662562350316,-75.));
#71671=CARTESIAN_POINT('Ctrl Pts',(-26.2951612631559,21.6473612899045,-75.));
#71672=CARTESIAN_POINT('Ctrl Pts',(-26.3182008303572,21.6748041023069,-75.));
#71673=CARTESIAN_POINT('Ctrl Pts',(-26.3408305013503,21.7026434173748,-75.));
#71674=CARTESIAN_POINT('Ctrl Pts',(-26.3630441750331,21.7308667323941,-75.));
#71675=CARTESIAN_POINT('Ctrl Pts',(-26.3749498793541,21.7459933813391,-75.));
#71676=CARTESIAN_POINT('Ctrl Pts',(-26.3867376169378,21.7612325170237,-75.));
#71677=CARTESIAN_POINT('Ctrl Pts',(-26.3983920327574,21.7765629294232,-75.));
#71678=CARTESIAN_POINT('Ctrl Pts',(-26.4644154914187,21.8634112850157,-75.));
#71679=CARTESIAN_POINT('Ctrl Pts',(-26.5262623019746,21.9533097457026,-75.));
#71680=CARTESIAN_POINT('Ctrl Pts',(-26.5838341421057,22.0458267042707,-75.));
#71681=CARTESIAN_POINT('Ctrl Pts',(-26.6423689485129,22.13989113311,-75.));
#71682=CARTESIAN_POINT('Ctrl Pts',(-26.6964851411425,22.2366629865775,-75.));
#71683=CARTESIAN_POINT('Ctrl Pts',(-26.7460506419084,22.3357350608551,-75.));
#71684=CARTESIAN_POINT('Ctrl Pts',(-26.7960954821668,22.4357652442423,-75.));
#71685=CARTESIAN_POINT('Ctrl Pts',(-26.8415017721221,22.5381410766061,-75.));
#71686=CARTESIAN_POINT('Ctrl Pts',(-26.8820958404228,22.6424802379775,-75.));
#71687=CARTESIAN_POINT('Ctrl Pts',(-26.9024290437316,22.694742784454,-75.));
#71688=CARTESIAN_POINT('Ctrl Pts',(-26.9215542572118,22.747498419904,-75.));
#71689=CARTESIAN_POINT('Ctrl Pts',(-26.9394454329999,22.8007016269248,-75.));
#71690=CARTESIAN_POINT('Ctrl Pts',(-26.9525616993856,22.8397056277868,-75.));
#71691=CARTESIAN_POINT('Ctrl Pts',(-26.9650146663652,22.8789502128774,-75.));
#71692=CARTESIAN_POINT('Ctrl Pts',(-26.9767929984843,22.918417862835,-75.));
#71693=CARTESIAN_POINT('Ctrl Pts',(-26.980825387984,22.9319298724862,-75.));
#71694=CARTESIAN_POINT('Ctrl Pts',(-26.984778192821,22.9454664712351,-75.));
#71695=CARTESIAN_POINT('Ctrl Pts',(-26.9886485069943,22.9590178538402,-75.));
#71696=CARTESIAN_POINT('Ctrl Pts',(-27.0202317423094,23.0696022887205,-75.));
#71697=CARTESIAN_POINT('Ctrl Pts',(-27.046374962193,23.181334637174,-75.));
#71698=CARTESIAN_POINT('Ctrl Pts',(-27.0669439642748,23.293784455837,-75.));
#71699=CARTESIAN_POINT('Ctrl Pts',(-27.0874483325601,23.4058809244124,-75.));
#71700=CARTESIAN_POINT('Ctrl Pts',(-27.1024139517669,23.5186912072283,-75.));
#71701=CARTESIAN_POINT('Ctrl Pts',(-27.1116662797041,23.6318186576043,-75.));
#71702=CARTESIAN_POINT('Ctrl Pts',(-27.1202480664253,23.736747455851,-75.));
#71703=CARTESIAN_POINT('Ctrl Pts',(-27.1239145828038,23.8419499369186,-75.));
#71704=CARTESIAN_POINT('Ctrl Pts',(-27.1224887512111,23.9471230379589,-75.));
#71705=CARTESIAN_POINT('Ctrl Pts',(-27.1214315592659,24.0251043057544,-75.));
#71706=CARTESIAN_POINT('Ctrl Pts',(-27.1175740459907,24.1030697257956,-75.));
#71707=CARTESIAN_POINT('Ctrl Pts',(-27.110991898551,24.1809217806606,-75.));
#71708=CARTESIAN_POINT('Ctrl Pts',(-27.1089458950028,24.2051214179296,-75.));
#71709=CARTESIAN_POINT('Ctrl Pts',(-27.1066365391915,24.2293101033335,-75.));
#71710=CARTESIAN_POINT('Ctrl Pts',(-27.1040658591694,24.253484904205,-75.));
#71711=CARTESIAN_POINT('Ctrl Pts',(-27.1016965285288,24.2757662056281,-75.));
#71712=CARTESIAN_POINT('Ctrl Pts',(-27.0991044565744,24.2980408276541,-75.));
#71713=CARTESIAN_POINT('Ctrl Pts',(-27.0962953485937,24.3202756476038,-75.));
#71714=CARTESIAN_POINT('Ctrl Pts',(-27.0821928071296,24.4319009295238,-75.));
#71715=CARTESIAN_POINT('Ctrl Pts',(-27.0626133321251,24.5426515225154,-75.));
#71716=CARTESIAN_POINT('Ctrl Pts',(-27.0378716668943,24.6522326854476,-75.));
#71717=CARTESIAN_POINT('Ctrl Pts',(-27.0126702012133,24.7638503106628,-75.));
#71718=CARTESIAN_POINT('Ctrl Pts',(-26.9821127731921,24.8742552769071,-75.));
#71719=CARTESIAN_POINT('Ctrl Pts',(-26.9464772616989,24.9831449167715,-75.));
#71720=CARTESIAN_POINT('Ctrl Pts',(-26.9101118870068,25.094264762898,-75.));
#71721=CARTESIAN_POINT('Ctrl Pts',(-26.8684581529784,25.2038073287541,-75.));
#71722=CARTESIAN_POINT('Ctrl Pts',(-26.8217568024216,25.3114493823763,-75.));
#71723=CARTESIAN_POINT('Ctrl Pts',(-26.7832118857427,25.4002916522152,-75.));
#71724=CARTESIAN_POINT('Ctrl Pts',(-26.7412274435804,25.4878394728692,-75.));
#71725=CARTESIAN_POINT('Ctrl Pts',(-26.6959129135712,25.5739046319901,-75.));
#71726=CARTESIAN_POINT('Ctrl Pts',(-26.6858732433753,25.5929728163619,-75.));
#71727=CARTESIAN_POINT('Ctrl Pts',(-26.6756700236405,25.6119681875733,-75.));
#71728=CARTESIAN_POINT('Ctrl Pts',(-26.6653042992829,25.63088863441,-75.));
#71729=CARTESIAN_POINT('Ctrl Pts',(-26.6561483093346,25.6476009658473,-75.));
#71730=CARTESIAN_POINT('Ctrl Pts',(-26.6468698353721,25.6642469346371,-75.));
#71731=CARTESIAN_POINT('Ctrl Pts',(-26.6374723605576,25.6808210785559,-75.));
#71732=CARTESIAN_POINT('Ctrl Pts',(-26.5781216176399,25.7854968317996,-75.));
#71733=CARTESIAN_POINT('Ctrl Pts',(-26.5139994851696,25.8873614230389,-75.));
#71734=CARTESIAN_POINT('Ctrl Pts',(-26.4453803727087,25.9860816677649,-75.));
#71735=CARTESIAN_POINT('Ctrl Pts',(-26.3762554483936,26.0855296087295,-75.));
#71736=CARTESIAN_POINT('Ctrl Pts',(-26.3025666925354,26.1817875091273,-75.));
#71737=CARTESIAN_POINT('Ctrl Pts',(-26.2245441756349,26.2745003905634,-75.));
#71738=CARTESIAN_POINT('Ctrl Pts',(-26.1893020912291,26.3163779833772,-75.));
#71739=CARTESIAN_POINT('Ctrl Pts',(-26.1531751604097,26.3575320336574,-75.));
#71740=CARTESIAN_POINT('Ctrl Pts',(-26.1161815127994,26.3979281671849,-75.));
#71741=CARTESIAN_POINT('Ctrl Pts',(-26.0949645293092,26.4210965799662,-75.));
#71742=CARTESIAN_POINT('Ctrl Pts',(-26.0734574109817,26.4440206775451,-75.));
#71743=CARTESIAN_POINT('Ctrl Pts',(-26.0516898669499,26.4666667346163,-75.));
#71744=CARTESIAN_POINT('Ctrl Pts',(-25.9662054925696,26.5556011600195,-75.));
#71745=CARTESIAN_POINT('Ctrl Pts',(-25.8766542573217,26.6403121959665,-75.));
#71746=CARTESIAN_POINT('Ctrl Pts',(-25.7832911788552,26.7204449987284,-75.));
#71747=CARTESIAN_POINT('Ctrl Pts',(-25.6911368051049,26.7995403796505,-75.));
#71748=CARTESIAN_POINT('Ctrl Pts',(-25.5952681674086,26.8741760556854,-75.));
#71749=CARTESIAN_POINT('Ctrl Pts',(-25.4958878475418,26.9439845596524,-75.0000000000001));
#71750=CARTESIAN_POINT('Ctrl Pts',(-25.4316916215268,26.9890784223451,-75.0000000000001));
#71751=CARTESIAN_POINT('Ctrl Pts',(-25.3660292286572,27.0321574883894,-75.0000000000001));
#71752=CARTESIAN_POINT('Ctrl Pts',(-25.2989470070244,27.0731145261455,-75.0000000000001));
#71753=CARTESIAN_POINT('Ctrl Pts',(-21.2666653996577,20.3445903493589,-75.4118502628812));
#71754=CARTESIAN_POINT('Ctrl Pts',(-20.1976516050523,21.1060288780026,-75.3455104329369));
#71755=CARTESIAN_POINT('Ctrl Pts',(-18.9008443259664,23.7684865465132,-75.2128749658675));
#71756=CARTESIAN_POINT('Ctrl Pts',(-21.2264059286695,27.5877942357118,-75.013943861673));
#71757=CARTESIAN_POINT('Ctrl Pts',(-25.688658539591,27.6837853569551,-74.8150569502983));
#71758=CARTESIAN_POINT('Ctrl Pts',(-28.1849582354078,23.9876330729271,-74.6161700389233));
#71759=CARTESIAN_POINT('Ctrl Pts',(-26.4228527910817,19.886306014703,-74.4172831275484));
#71760=CARTESIAN_POINT('Ctrl Pts',(-22.0208084558691,19.1535567442735,-74.2183962161735));
#71761=CARTESIAN_POINT('Ctrl Pts',(-19.0243327220968,22.4600869091669,-74.0195093047986));
#71762=CARTESIAN_POINT('Ctrl Pts',(-20.1867198546258,26.7688693666575,-73.8206223934237));
#71763=CARTESIAN_POINT('Ctrl Pts',(-24.439947370569,28.1197603121436,-73.6217354820488));
#71764=CARTESIAN_POINT('Ctrl Pts',(-27.8756000908746,25.2717963687883,-73.4228485706739));
#71765=CARTESIAN_POINT('Ctrl Pts',(-27.3366360814689,20.8418079302662,-73.2239616592991));
#71766=CARTESIAN_POINT('Ctrl Pts',(-23.3183008240058,18.9006883998381,-73.0250747479242));
#71767=CARTESIAN_POINT('Ctrl Pts',(-19.5131125903956,21.2321039860555,-72.8261878365494));
#71768=CARTESIAN_POINT('Ctrl Pts',(-19.4177120435377,25.6937121854946,-72.6273009251744));
#71769=CARTESIAN_POINT('Ctrl Pts',(-23.1197666849278,28.1856570601434,-72.4284140137995));
#71770=CARTESIAN_POINT('Ctrl Pts',(-27.2174008641755,26.4180611767357,-72.2295271024246));
#71771=CARTESIAN_POINT('Ctrl Pts',(-27.9452368903513,22.0151907171623,-72.0306401910497));
#71772=CARTESIAN_POINT('Ctrl Pts',(-24.6344547962064,19.022912750906,-71.8317532796748));
#71773=CARTESIAN_POINT('Ctrl Pts',(-20.3273828139243,20.1908757445163,-71.6328663683));
#71774=CARTESIAN_POINT('Ctrl Pts',(-18.9818548120982,24.4458214122759,-71.433979456925));
#71775=CARTESIAN_POINT('Ctrl Pts',(-21.8342969973335,27.8778150860887,-71.2350925455501));
#71776=CARTESIAN_POINT('Ctrl Pts',(-26.2635568195445,27.3331457550989,-71.0362056341753));
#71777=CARTESIAN_POINT('Ctrl Pts',(-28.1995200568178,23.3123182533585,-70.8373187228003));
#71778=CARTESIAN_POINT('Ctrl Pts',(-25.8632006285602,19.510132198389,-70.6384318114255));
#71779=CARTESIAN_POINT('Ctrl Pts',(-21.4014780064369,19.4204741742239,-70.4395449000505));
#71780=CARTESIAN_POINT('Ctrl Pts',(-18.9142969861975,23.1257323182947,-70.2406579886757));
#71781=CARTESIAN_POINT('Ctrl Pts',(-20.687166048478,27.221088542356,-70.0417710773009));
#71782=CARTESIAN_POINT('Ctrl Pts',(-25.0909688389096,27.9432577096414,-69.8428841659259));
#71783=CARTESIAN_POINT('Ctrl Pts',(-28.0789839743286,24.6286275830399,-69.6439972545512));
#71784=CARTESIAN_POINT('Ctrl Pts',(-26.9054788870104,20.3230622157861,-69.445110343176));
#71785=CARTESIAN_POINT('Ctrl Pts',(-22.648805255472,18.9830111280192,-69.2462234318014));
#71786=CARTESIAN_POINT('Ctrl Pts',(-19.2204852406392,21.8398676521317,-69.0473365204262));
#71787=CARTESIAN_POINT('Ctrl Pts',(-19.7708542625673,26.268422863778,-68.8484496090516));
#71788=CARTESIAN_POINT('Ctrl Pts',(-23.7941698536879,28.1992100031105,-68.6495626976765));
#71789=CARTESIAN_POINT('Ctrl Pts',(-27.5933461066773,25.8579993927866,-68.4506757863017));
#71790=CARTESIAN_POINT('Ctrl Pts',(-27.6772621620609,21.3961650817951,-68.2517888749267));
#71791=CARTESIAN_POINT('Ctrl Pts',(-23.9688062798515,18.9137545007584,-68.0529019635519));
#71792=CARTESIAN_POINT('Ctrl Pts',(-19.8757349905908,20.6918924999483,-67.854015052177));
#71793=CARTESIAN_POINT('Ctrl Pts',(-19.1592337738934,25.0966210193459,-67.6551281408021));
#71794=CARTESIAN_POINT('Ctrl Pts',(-22.4777064986191,28.0803680090189,-67.4562412294273));
#71795=CARTESIAN_POINT('Ctrl Pts',(-26.7817580908333,26.901322965483,-67.2573543180523));
#71796=CARTESIAN_POINT('Ctrl Pts',(-28.1163300606876,22.6429283172139,-67.0584674066776));
#71797=CARTESIAN_POINT('Ctrl Pts',(-25.255063920929,19.2182876936448,-66.8595804953024));
#71798=CARTESIAN_POINT('Ctrl Pts',(-20.8272206586329,19.7743554661939,-66.6606935839279));
#71799=CARTESIAN_POINT('Ctrl Pts',(-18.9016128126505,23.8001524986608,-66.4618066725527));
#71800=CARTESIAN_POINT('Ctrl Pts',(-21.2477107288177,27.5963126495084,-66.262919761178));
#71801=CARTESIAN_POINT('Ctrl Pts',(-25.7096493384775,27.6744866014112,-66.0640328498029));
#71802=CARTESIAN_POINT('Ctrl Pts',(-28.1872853693601,23.9628391206286,-65.8651459384281));
#71803=CARTESIAN_POINT('Ctrl Pts',(-26.4038813779779,19.8720595461892,-65.6662590270532));
#71804=CARTESIAN_POINT('Ctrl Pts',(-21.998234424688,19.1612274660918,-65.4673721156783));
#71805=CARTESIAN_POINT('Ctrl Pts',(-19.0187605223013,22.4835372933243,-65.2684852043034));
#71806=CARTESIAN_POINT('Ctrl Pts',(-20.2033435693833,26.7860679820812,-65.0695982929285));
#71807=CARTESIAN_POINT('Ctrl Pts',(-24.4634521817448,28.1151586238398,-64.8707113815536));
#71808=CARTESIAN_POINT('Ctrl Pts',(-27.8844077422721,25.2494876071271,-64.6718244701788));
#71809=CARTESIAN_POINT('Ctrl Pts',(-27.3226421400403,20.8223636274675,-64.4729375588038));
#71810=CARTESIAN_POINT('Ctrl Pts',(-23.2943703336322,18.9019382639541,-64.2740506474291));
#71811=CARTESIAN_POINT('Ctrl Pts',(-19.5012325720103,21.2529196004361,-64.075163736054));
#71812=CARTESIAN_POINT('Ctrl Pts',(-19.4288008530583,25.7149551190328,-63.8762768246794));
#71813=CARTESIAN_POINT('Ctrl Pts',(-23.143633785296,28.1878124963781,-63.6773899133043));
#71814=CARTESIAN_POINT('Ctrl Pts',(-27.2321148698893,26.399145466422,-63.4785030019295));
#71815=CARTESIAN_POINT('Ctrl Pts',(-27.937276636128,21.992587375739,-63.2796160905546));
#71816=CARTESIAN_POINT('Ctrl Pts',(-24.6111352086973,19.0173914951528,-63.0807291791796));
#71817=CARTESIAN_POINT('Ctrl Pts',(-20.3101325491186,20.2075105839101,-62.8818422678048));
#71818=CARTESIAN_POINT('Ctrl Pts',(-18.9865254366552,24.4693261049017,-62.6829553564298));
#71819=CARTESIAN_POINT('Ctrl Pts',(-21.8565965842846,27.8865909367042,-62.484068445055));
#71820=CARTESIAN_POINT('Ctrl Pts',(-26.2829939492395,27.319128435169,-62.28518153368));
#71821=CARTESIAN_POINT('Ctrl Pts',(-28.1982336497336,23.288388526321,-62.0862946223052));
#71822=CARTESIAN_POINT('Ctrl Pts',(-25.8423727865607,19.4982794360047,-61.8874077109303));
#71823=CARTESIAN_POINT('Ctrl Pts',(-21.3802477489149,19.4315900699627,-61.6885207995554));
#71824=CARTESIAN_POINT('Ctrl Pts',(-18.9121731205785,23.149602301262,-61.4896338881805));
#71825=CARTESIAN_POINT('Ctrl Pts',(-20.7061002267723,27.2357781247906,-61.2907469768056));
#71826=CARTESIAN_POINT('Ctrl Pts',(-25.1135621568407,27.9352684093035,-61.0918600654307));
#71827=CARTESIAN_POINT('Ctrl Pts',(-28.0844750881974,24.6053008903289,-60.8929731540559));
#71828=CARTESIAN_POINT('Ctrl Pts',(-26.8888219288037,20.3058333831184,-60.6940862426809));
#71829=CARTESIAN_POINT('Ctrl Pts',(-22.6253065574715,18.9877119920681,-60.4951993313061));
#71830=CARTESIAN_POINT('Ctrl Pts',(-19.211738113964,21.8621785172896,-60.2963124199312));
#71831=CARTESIAN_POINT('Ctrl Pts',(-19.7848965749885,26.2878419366748,-60.0974255085563));
#71832=CARTESIAN_POINT('Ctrl Pts',(-23.8180979106871,28.1978928021876,-59.8985385971813));
#71833=CARTESIAN_POINT('Ctrl Pts',(-27.6051720526345,25.8371563140293,-59.6996516858066));
#71834=CARTESIAN_POINT('Ctrl Pts',(-27.6661189553175,21.3749491473704,-59.5007647744315));
#71835=CARTESIAN_POINT('Ctrl Pts',(-23.9449335826159,18.9116613555929,-59.3018778630568));
#71836=CARTESIAN_POINT('Ctrl Pts',(-19.8610697875519,20.7108455669771,-59.1029909516818));
#71837=CARTESIAN_POINT('Ctrl Pts',(-19.1672521432397,25.1192040369259,-58.904104040307));
#71838=CARTESIAN_POINT('Ctrl Pts',(-22.5010402387668,28.0858290987175,-58.705217128932));
#71839=CARTESIAN_POINT('Ctrl Pts',(-26.7989654729617,26.8846438488917,-58.5063302175572));
#71840=CARTESIAN_POINT('Ctrl Pts',(-28.111598959566,22.6194356883239,-58.3074433061823));
#71841=CARTESIAN_POINT('Ctrl Pts',(-25.2327418173569,19.2095692865597,-58.1085563948074));
#71842=CARTESIAN_POINT('Ctrl Pts',(-20.8078196731909,19.7884227578258,-57.9096694834325));
#71843=CARTESIAN_POINT('Ctrl Pts',(-18.9029608060273,23.8240788407097,-57.7107825720576));
#71844=CARTESIAN_POINT('Ctrl Pts',(-21.2685690093912,27.6081117622506,-57.5118956606827));
#71845=CARTESIAN_POINT('Ctrl Pts',(-25.7308509148911,27.6633161006365,-57.3130087493078));
#71846=CARTESIAN_POINT('Ctrl Pts',(-28.189347790487,23.9389637494465,-57.1141218379329));
#71847=CARTESIAN_POINT('Ctrl Pts',(-26.384909453667,19.8574187464186,-56.915234926558));
#71848=CARTESIAN_POINT('Ctrl Pts',(-21.975661744827,19.1692748913867,-56.7163480151832));
#71849=CARTESIAN_POINT('Ctrl Pts',(-19.013329465835,22.5068780421479,-56.5174611038082));
#71850=CARTESIAN_POINT('Ctrl Pts',(-20.2200448167264,26.8032538852337,-56.3185741924334));
#71851=CARTESIAN_POINT('Ctrl Pts',(-24.4869387026215,28.1103972934484,-56.1196872810584));
#71852=CARTESIAN_POINT('Ctrl Pts',(-27.8930974153251,25.2271543021274,-55.9208003696836));
#71853=CARTESIAN_POINT('Ctrl Pts',(-27.3085498924968,20.8029807616021,-55.7219134583087));
#71854=CARTESIAN_POINT('Ctrl Pts',(-23.2704457461589,18.9033170475574,-55.5230265469337));
#71855=CARTESIAN_POINT('Ctrl Pts',(-19.4894603120249,21.2737930482783,-55.3241396355589));
#71856=CARTESIAN_POINT('Ctrl Pts',(-19.4399986293641,25.7361423023235,-55.125252724184));
#71857=CARTESIAN_POINT('Ctrl Pts',(-23.1675117908829,28.1898441900499,-54.9263658128092));
#71858=CARTESIAN_POINT('Ctrl Pts',(-27.2467312421439,26.3801547162498,-54.7274789014342));
#71859=CARTESIAN_POINT('Ctrl Pts',(-27.9292001682125,21.970025070981,-54.5285919900594));
#71860=CARTESIAN_POINT('Ctrl Pts',(-24.5877874898543,19.0119904809134,-54.3297050786844));
#71861=CARTESIAN_POINT('Ctrl Pts',(-20.2929681534049,20.2242339343449,-54.1308181673096));
#71862=CARTESIAN_POINT('Ctrl Pts',(-18.9913169884309,24.4928064788673,-53.9319312559346));
#71863=CARTESIAN_POINT('Ctrl Pts',(-21.8789410537244,27.8952518613337,-53.7330443445599));
#71864=CARTESIAN_POINT('Ctrl Pts',(-26.3023586634269,27.3050112550531,-53.5341574331848));
#71865=CARTESIAN_POINT('Ctrl Pts',(-28.1968240781874,23.2644657330469,-53.3352705218101));
#71866=CARTESIAN_POINT('Ctrl Pts',(-25.8214842060198,19.4865340482728,-53.136383610435));
#71867=CARTESIAN_POINT('Ctrl Pts',(-21.3590749938369,19.442815103254,-52.9374966990602));
#71868=CARTESIAN_POINT('Ctrl Pts',(-18.9101721577264,23.1734829017077,-52.7386097876853));
#71869=CARTESIAN_POINT('Ctrl Pts',(-20.7251097713536,27.2503700453221,-52.5397228763104));
#71870=CARTESIAN_POINT('Ctrl Pts',(-25.1361140491286,27.9271629121431,-52.3408359649356));
#71871=CARTESIAN_POINT('Ctrl Pts',(-28.0898460512646,24.5819462401343,-52.1419490535606));
#71872=CARTESIAN_POINT('Ctrl Pts',(-26.8720765029738,20.2886905232705,-51.9430621421858));
#71873=CARTESIAN_POINT('Ctrl Pts',(-22.6018323693044,18.9925337572925,-51.7441752308108));
#71874=CARTESIAN_POINT('Ctrl Pts',(-19.2031059521021,21.8845341141631,-51.545288319436));
#71875=CARTESIAN_POINT('Ctrl Pts',(-19.7990386642963,26.3071884671128,-51.3464014080611));
#71876=CARTESIAN_POINT('Ctrl Pts',(-23.8420188701422,28.196452445033,-51.1475144966862));
#71877=CARTESIAN_POINT('Ctrl Pts',(-27.6168905486605,25.8162526353847,-50.9486275853114));
#71878=CARTESIAN_POINT('Ctrl Pts',(-27.6548666836312,21.3537908555707,-50.7497406739364));
#71879=CARTESIAN_POINT('Ctrl Pts',(-23.9210504268616,18.9096911268747,-50.5508537625616));
#71880=CARTESIAN_POINT('Ctrl Pts',(-19.8465023429102,20.7298738744846,-50.3519668511866));
#71881=CARTESIAN_POINT('Ctrl Pts',(-19.1753866562207,25.141745479394,-50.1530799398118));
#71882=CARTESIAN_POINT('Ctrl Pts',(-22.524401781634,28.0911700017174,-49.9541930284368));
#71883=CARTESIAN_POINT('Ctrl Pts',(-26.8160867685523,26.8678763754001,-49.755306117062));
#71884=CARTESIAN_POINT('Ctrl Pts',(-28.1067469888788,22.5959677248325,-49.556419205687));
#71885=CARTESIAN_POINT('Ctrl Pts',(-25.2103751300742,19.2009659017617,-49.3575322943122));
#71886=CARTESIAN_POINT('Ctrl Pts',(-20.7884913585431,19.802589732904,-49.1586453829372));
#71887=CARTESIAN_POINT('Ctrl Pts',(-18.9044319464049,23.8479979267284,-48.9597584715625));
#71888=CARTESIAN_POINT('Ctrl Pts',(-21.2894877515194,27.6198033471629,-48.7608715601874));
#71889=CARTESIAN_POINT('Ctrl Pts',(-25.7519947083708,27.6520366091907,-48.5619846488127));
#71890=CARTESIAN_POINT('Ctrl Pts',(-28.1912872818085,23.9150780779383,-48.3630977374377));
#71891=CARTESIAN_POINT('Ctrl Pts',(-26.3658624147475,19.8428758017929,-48.1642108260628));
#71892=CARTESIAN_POINT('Ctrl Pts',(-21.953130789511,19.1774384067162,-47.965323914688));
#71893=CARTESIAN_POINT('Ctrl Pts',(-19.0080186317479,22.5302464389967,-47.7664370033131));
#71894=CARTESIAN_POINT('Ctrl Pts',(-20.2368343101097,26.8203535882111,-47.5675500919381));
#71895=CARTESIAN_POINT('Ctrl Pts',(-24.5104004025703,28.1055151253339,-47.3686631805633));
#71896=CARTESIAN_POINT('Ctrl Pts',(-27.9016720088104,25.2047765614785,-47.1697762691884));
#71897=CARTESIAN_POINT('Ctrl Pts',(-27.2943580551114,20.7836706947557,-46.9708893578135));
#71898=CARTESIAN_POINT('Ctrl Pts',(-23.2465285731905,18.9048189687216,-46.7720024464386));
#71899=CARTESIAN_POINT('Ctrl Pts',(-19.4777956575895,21.2947268192451,-46.5731155350638));
#71900=CARTESIAN_POINT('Ctrl Pts',(-19.4513053218883,25.7572715624655,-46.3742286236887));
#71901=CARTESIAN_POINT('Ctrl Pts',(-23.1913999385863,28.1917529407624,-46.175341712314));
#71902=CARTESIAN_POINT('Ctrl Pts',(-27.261249662668,26.3610889774635,-45.976454800939));
#71903=CARTESIAN_POINT('Ctrl Pts',(-27.9210076640546,21.9475046401323,-45.7775678895642));
#71904=CARTESIAN_POINT('Ctrl Pts',(-24.5644122777257,19.0067097245348,-45.5786809781893));
#71905=CARTESIAN_POINT('Ctrl Pts',(-20.2758900713606,20.2410454198139,-45.3797940668144));
#71906=CARTESIAN_POINT('Ctrl Pts',(-18.9962293458869,24.5162618764169,-45.1809071554395));
#71907=CARTESIAN_POINT('Ctrl Pts',(-21.901329810678,27.9037976493055,-44.9820202440646));
#71908=CARTESIAN_POINT('Ctrl Pts',(-26.3216504504911,27.2907945788645,-44.7831333326896));
#71909=CARTESIAN_POINT('Ctrl Pts',(-28.1952913787241,23.2405505127397,-44.5842464213149));
#71910=CARTESIAN_POINT('Ctrl Pts',(-25.8005354408843,19.4748963436331,-44.3853595099398));
#71911=CARTESIAN_POINT('Ctrl Pts',(-21.3379603020264,19.4541489781311,-44.1864725985652));
#71912=CARTESIAN_POINT('Ctrl Pts',(-18.908294150784,23.1973734860435,-43.9875856871901));
#71913=CARTESIAN_POINT('Ctrl Pts',(-20.7441941784308,27.2648639176997,-43.7886987758153));
#71914=CARTESIAN_POINT('Ctrl Pts',(-25.1586239182123,27.9189414327251,-43.5898118644403));
#71915=CARTESIAN_POINT('Ctrl Pts',(-28.0950967211891,24.5585642514394,-43.3909249530655));
#71916=CARTESIAN_POINT('Ctrl Pts',(-26.8552430532619,20.2716340904436,-43.1920380416906));
#71917=CARTESIAN_POINT('Ctrl Pts',(-22.5783833130001,18.9974762959544,-42.9931511303156));
#71918=CARTESIAN_POINT('Ctrl Pts',(-19.1945889837971,21.9069338503419,-42.7942642189409));
#71919=CARTESIAN_POINT('Ctrl Pts',(-19.813280155743,26.3264619424445,-42.5953773075658));
#71920=CARTESIAN_POINT('Ctrl Pts',(-23.8659320981805,28.194888969809,-42.3964903961911));
#71921=CARTESIAN_POINT('Ctrl Pts',(-27.6285012842304,25.7952889107751,-42.1976034848161));
#71922=CARTESIAN_POINT('Ctrl Pts',(-27.6435056451722,21.332690767061,-41.9987165734413));
#71923=CARTESIAN_POINT('Ctrl Pts',(-23.8971574454602,18.9078438668127,-41.7998296620662));
#71924=CARTESIAN_POINT('Ctrl Pts',(-19.8320330426836,20.7489769182455,-41.6009427506916));
#71925=CARTESIAN_POINT('Ctrl Pts',(-19.1836370972827,25.1642447494326,-41.4020558393165));
#71926=CARTESIAN_POINT('Ctrl Pts',(-22.5477905081707,28.0963905764916,-41.2031689279418));
#71927=CARTESIAN_POINT('Ctrl Pts',(-26.8331215239135,26.8510209893242,-41.0042820165667));
#71928=CARTESIAN_POINT('Ctrl Pts',(-28.1017742771965,22.5725250486092,-40.805395105192));
#71929=CARTESIAN_POINT('Ctrl Pts',(-25.1879644517681,19.192477767229,-40.6065081938169));
#71930=CARTESIAN_POINT('Ctrl Pts',(-20.7692362268642,19.8168560160224,-40.4076212824422));
#71931=CARTESIAN_POINT('Ctrl Pts',(-18.9060261948002,23.8719091228934,-40.2087343710672));
#71932=CARTESIAN_POINT('Ctrl Pts',(-21.3104664008835,27.631387094434,-40.0098474596923));
#71933=CARTESIAN_POINT('Ctrl Pts',(-25.7730801586343,27.6406484259655,-39.8109605483174));
#71934=CARTESIAN_POINT('Ctrl Pts',(-28.1931037919306,23.8911827390422,-39.6120736369426));
#71935=CARTESIAN_POINT('Ctrl Pts',(-26.3467407659406,19.8284310976806,-39.4131867255677));
#71936=CARTESIAN_POINT('Ctrl Pts',(-21.9306421557803,19.1857177957581,-39.2142998141928));
#71937=CARTESIAN_POINT('Ctrl Pts',(-19.0028281607701,22.5536418646396,-39.0154129028179));
#71938=CARTESIAN_POINT('Ctrl Pts',(-20.2537116046342,26.8373666378943,-38.816525991443));
#71939=CARTESIAN_POINT('Ctrl Pts',(-24.5338366598877,28.1005122488671,-38.6176390800681));
#71940=CARTESIAN_POINT('Ctrl Pts',(-27.910131295513,25.1823549781609,-38.4187521686932));
#71941=CARTESIAN_POINT('Ctrl Pts',(-27.2800670039488,20.7644339386194,-38.2198652573183));
#71942=CARTESIAN_POINT('Ctrl Pts',(-23.2226194484999,18.9064439876479,-38.0209783459435));
#71943=CARTESIAN_POINT('Ctrl Pts',(-19.4662389178021,21.3157203586197,-37.8220914345685));
#71944=CARTESIAN_POINT('Ctrl Pts',(-19.4627206310189,25.7783423395616,-37.6232045231937));
#71945=CARTESIAN_POINT('Ctrl Pts',(-23.2152975954025,28.1935386979362,-37.4243176118188));
#71946=CARTESIAN_POINT('Ctrl Pts',(-27.2756697467429,26.3419487552794,-37.2254307004438));
#71947=CARTESIAN_POINT('Ctrl Pts',(-27.912699340745,21.9250266799544,-37.026543789069));
#71948=CARTESIAN_POINT('Ctrl Pts',(-24.5410101917235,19.0015493659496,-36.827656877694));
#71949=CARTESIAN_POINT('Ctrl Pts',(-20.258898755532,20.2579445948353,-36.6287699663193));
#71950=CARTESIAN_POINT('Ctrl Pts',(-19.0012623788527,24.5396916760138,-36.4298830549443));
#71951=CARTESIAN_POINT('Ctrl Pts',(-21.9237622618732,27.9122280741679,-36.2309961435695));
#71952=CARTESIAN_POINT('Ctrl Pts',(-26.3408687992257,27.2764787833259,-36.0321092321945));
#71953=CARTESIAN_POINT('Ctrl Pts',(-28.1936355919582,23.2166434991209,-35.8332223208196));
#71954=CARTESIAN_POINT('Ctrl Pts',(-25.7795270462683,19.4633666304692,-35.6343354094447));
#71955=CARTESIAN_POINT('Ctrl Pts',(-21.3169042329942,19.4655913942613,-35.4354484980699));
#71956=CARTESIAN_POINT('Ctrl Pts',(-18.906539149516,23.221273421201,-35.2365615866949));
#71957=CARTESIAN_POINT('Ctrl Pts',(-20.7633529422927,27.2792593578551,-35.0376746753201));
#71958=CARTESIAN_POINT('Ctrl Pts',(-25.1810911676103,27.9106041889076,-34.8387877639452));
#71959=CARTESIAN_POINT('Ctrl Pts',(-28.1002269588351,24.5351555438356,-34.6399008525703));
#71960=CARTESIAN_POINT('Ctrl Pts',(-26.8383220257315,20.2546645366102,-34.4410139411954));
#71961=CARTESIAN_POINT('Ctrl Pts',(-22.5549600099273,19.0025394770835,-34.2421270298205));
#71962=CARTESIAN_POINT('Ctrl Pts',(-19.1861874347372,21.9293771322627,-34.0432401184457));
#71963=CARTESIAN_POINT('Ctrl Pts',(-19.827620671948,26.3456618519484,-33.8443532070707));
#71964=CARTESIAN_POINT('Ctrl Pts',(-23.8898369611334,28.1932024179458,-33.6454662956958));
#71965=CARTESIAN_POINT('Ctrl Pts',(-27.6400039516757,25.7742656957109,-33.446579384321));
#71966=CARTESIAN_POINT('Ctrl Pts',(-27.6320361409929,21.3116494409653,-33.247692472946));
#71967=CARTESIAN_POINT('Ctrl Pts',(-23.8732552715437,18.9061196243572,-33.0488055615712));
#71968=CARTESIAN_POINT('Ctrl Pts',(-19.8176622702888,20.768154192055,-32.8499186501963));
#71969=CARTESIAN_POINT('Ctrl Pts',(-19.1920032478,25.1867012508411,-32.6510317388214));
#71970=CARTESIAN_POINT('Ctrl Pts',(-22.5712057986073,28.1014906847019,-32.4521448274465));
#71971=CARTESIAN_POINT('Ctrl Pts',(-26.8500692876472,26.8340781373091,-32.2532579160716));
#71972=CARTESIAN_POINT('Ctrl Pts',(-28.0966809562897,22.5491082808535,-32.0543710046967));
#71973=CARTESIAN_POINT('Ctrl Pts',(-25.1655103762915,19.1841051078859,-31.8554840933218));
#71974=CARTESIAN_POINT('Ctrl Pts',(-20.7500547883893,19.8312212291436,-31.656597181947));
#71975=CARTESIAN_POINT('Ctrl Pts',(-18.9077435089677,23.8958117955898,-31.457710270572));
#71976=CARTESIAN_POINT('Ctrl Pts',(-21.3315044015777,27.6428626971101,-31.2588233591972));
#71977=CARTESIAN_POINT('Ctrl Pts',(-25.7941067069455,27.6291518527325,-31.0599364478223));
#71978=CARTESIAN_POINT('Ctrl Pts',(-28.1947972727182,23.8672783659527,-30.8610495364474));
#71979=CARTESIAN_POINT('Ctrl Pts',(-26.3275450139443,19.8140850168471,-30.6621626250725));
#71980=CARTESIAN_POINT('Ctrl Pts',(-21.9081964395532,19.1941128391196,-30.4632757136976));
#71981=CARTESIAN_POINT('Ctrl Pts',(-18.9977581904422,22.5770636991292,-30.2643888023227));
#71982=CARTESIAN_POINT('Ctrl Pts',(-20.270676253074,26.8542925834601,-30.0655018909478));
#71983=CARTESIAN_POINT('Ctrl Pts',(-24.5572468535441,28.0953887966177,-29.8666149795729));
#71984=CARTESIAN_POINT('Ctrl Pts',(-27.9184750512729,25.1598901463163,-29.667728068198));
#71985=CARTESIAN_POINT('Ctrl Pts',(-27.2656771177025,20.7452710029411,-29.4688411568231));
#71986=CARTESIAN_POINT('Ctrl Pts',(-23.1987190056467,18.9081920612753,-29.2699542454482));
#71987=CARTESIAN_POINT('Ctrl Pts',(-19.4547903989006,21.3367731101012,-29.0710673340734));
#71988=CARTESIAN_POINT('Ctrl Pts',(-19.4742442542653,25.7993540752649,-28.8721804226984));
#71989=CARTESIAN_POINT('Ctrl Pts',(-23.2392041280753,28.1952014142512,-28.6732935113236));
#71990=CARTESIAN_POINT('Ctrl Pts',(-27.2899911122557,26.3227345568877,-28.4744065999487));
#71991=CARTESIAN_POINT('Ctrl Pts',(-27.9042754184428,21.9025917860827,-28.2755196885738));
#71992=CARTESIAN_POINT('Ctrl Pts',(-24.5175818519714,18.9965095419007,-28.0766327771989));
#71993=CARTESIAN_POINT('Ctrl Pts',(-20.2419946561664,20.2749310116035,-27.877745865824));
#71994=CARTESIAN_POINT('Ctrl Pts',(-19.0064159539593,24.5630952567998,-27.6788589544491));
#71995=CARTESIAN_POINT('Ctrl Pts',(-21.9462378128801,27.9205429125257,-27.4799720430743));
#71996=CARTESIAN_POINT('Ctrl Pts',(-26.36001320037,27.2620642477869,-27.2810851316994));
#71997=CARTESIAN_POINT('Ctrl Pts',(-28.1918567617659,23.1927453256942,-27.0821982203245));
#71998=CARTESIAN_POINT('Ctrl Pts',(-25.758459578866,19.451945214303,-26.8833113089496));
#71999=CARTESIAN_POINT('Ctrl Pts',(-21.2959073446981,19.4771420484359,-26.6844243975747));
#72000=CARTESIAN_POINT('Ctrl Pts',(-18.9049072004276,23.245182073864,-26.4855374861998));
#72001=CARTESIAN_POINT('Ctrl Pts',(-20.7825855552577,27.2935559843285,-26.2866505748249));
#72002=CARTESIAN_POINT('Ctrl Pts',(-25.2035152019707,27.9021514016165,-26.08776366345));
#72003=CARTESIAN_POINT('Ctrl Pts',(-28.105236628258,24.5117207376222,-25.8888767520751));
#72004=CARTESIAN_POINT('Ctrl Pts',(-26.8213138687676,20.2377823114409,-25.6899898407003));
#72005=CARTESIAN_POINT('Ctrl Pts',(-22.5315630807722,19.007723166512,-25.4911029293253));
#72006=CARTESIAN_POINT('Ctrl Pts',(-19.1779015275521,21.9518633652088,-25.2922160179505));
#72007=CARTESIAN_POINT('Ctrl Pts',(-19.842059832907,26.3647876868526,-25.0933291065755));
#72008=CARTESIAN_POINT('Ctrl Pts',(-23.9137328255541,28.1913928341347,-24.8944421952007));
#72009=CARTESIAN_POINT('Ctrl Pts',(-27.6513982461906,25.7531835472795,-24.6955552838258));
#72010=CARTESIAN_POINT('Ctrl Pts',(-27.6204584750198,21.2906674348507,-24.4966683724509));
#72011=CARTESIAN_POINT('Ctrl Pts',(-23.8493445384875,18.9045184451978,-24.297781461076));
#72012=CARTESIAN_POINT('Ctrl Pts',(-19.8033904065325,20.7874051877409,-24.0988945497011));
#72013=CARTESIAN_POINT('Ctrl Pts',(-19.200484886081,25.209114388552,-23.9000076383262));
#72014=CARTESIAN_POINT('Ctrl Pts',(-22.5946470324697,28.1064701912023,-23.7011207269513));
#72015=CARTESIAN_POINT('Ctrl Pts',(-26.8669296106604,26.8170482683175,-23.5022338155764));
#72016=CARTESIAN_POINT('Ctrl Pts',(-28.0914671611242,22.5257180420785,-23.3033469042016));
#72017=CARTESIAN_POINT('Ctrl Pts',(-25.1430134986476,19.1758481455965,-23.1044599928266));
#72018=CARTESIAN_POINT('Ctrl Pts',(-20.7309475514009,19.8456849916087,-22.9055730814518));
#72019=CARTESIAN_POINT('Ctrl Pts',(-18.9095838434007,23.919705311429,-22.7066861700768));
#72020=CARTESIAN_POINT('Ctrl Pts',(-21.3526011961228,27.654229851103,-22.507799258702));
#72021=CARTESIAN_POINT('Ctrl Pts',(-25.8150737961289,27.6175471941357,-22.3089123473271));
#72022=CARTESIAN_POINT('Ctrl Pts',(-28.1963676792964,23.8433655921035,-22.1100254359522));
#72023=CARTESIAN_POINT('Ctrl Pts',(-26.3082756674204,19.7998379394444,-21.9111385245773));
#72024=CARTESIAN_POINT('Ctrl Pts',(-21.8857942356115,19.2026233143433,-21.7122516132024));
#72025=CARTESIAN_POINT('Ctrl Pts',(-18.9928088551114,22.6005113218181,-21.5133647018276));
#72026=CARTESIAN_POINT('Ctrl Pts',(-20.2877278058888,26.8711309763936,-21.3144777904526));
#72027=CARTESIAN_POINT('Ctrl Pts',(-24.5806303632008,28.0901449043502,-21.1155908790778));
#72028=CARTESIAN_POINT('Ctrl Pts',(-27.9267030549918,25.137382661233,-20.9167039677029));
#72029=CARTESIAN_POINT('Ctrl Pts',(-27.2511887776856,20.7261823955133,-20.717817056328));
#72030=CARTESIAN_POINT('Ctrl Pts',(-23.174827877961,18.9100631432824,-20.5189301449531));
#72031=CARTESIAN_POINT('Ctrl Pts',(-19.4434504042556,21.3578845158201,-20.3200432335782));
#72032=CARTESIAN_POINT('Ctrl Pts',(-19.4858758862669,25.820306212792,-20.1211563222033));
#72033=CARTESIAN_POINT('Ctrl Pts',(-23.2631189031139,28.1967410456474,-19.9222694108284));
#72034=CARTESIAN_POINT('Ctrl Pts',(-27.3042133797093,26.3034468914392,-19.7233824994535));
#72035=CARTESIAN_POINT('Ctrl Pts',(-27.8957361203712,21.880200553012,-19.5244955880786));
#72036=CARTESIAN_POINT('Ctrl Pts',(-24.4941278792892,18.9915903859367,-19.3256086767037));
#72037=CARTESIAN_POINT('Ctrl Pts',(-20.2251782211997,20.2920042200011,-19.1267217653289));
#72038=CARTESIAN_POINT('Ctrl Pts',(-19.011689934644,24.5864719986112,-18.927834853954));
#72039=CARTESIAN_POINT('Ctrl Pts',(-21.9687558681268,27.9287419440471,-18.7289479425791));
#72040=CARTESIAN_POINT('Ctrl Pts',(-26.3790831466232,27.2475513542133,-18.5300610312042));
#72041=CARTESIAN_POINT('Ctrl Pts',(-28.1899549352836,23.1688566257294,-18.3311741198293));
#72042=CARTESIAN_POINT('Ctrl Pts',(-25.7373335969374,19.4406323977869,-18.1322872084544));
#72043=CARTESIAN_POINT('Ctrl Pts',(-21.2749701935273,19.4888006345782,-17.9334002970795));
#72044=CARTESIAN_POINT('Ctrl Pts',(-18.9033983467632,23.2690988104849,-17.7345133857046));
#72045=CARTESIAN_POINT('Ctrl Pts',(-20.8018915076875,27.3077534182785,-17.5356264743297));
#72046=CARTESIAN_POINT('Ctrl Pts',(-25.2258954270864,27.8935832948393,-17.3367395629548));
#72047=CARTESIAN_POINT('Ctrl Pts',(-28.1101255967088,24.4882604537905,-17.1378526515799));
#72048=CARTESIAN_POINT('Ctrl Pts',(-26.804219033063,20.2209878622919,-16.9389657402051));
#72049=CARTESIAN_POINT('Ctrl Pts',(-22.5081931455219,19.0130272268794,-16.7400788288302));
#72050=CARTESIAN_POINT('Ctrl Pts',(-19.1697314818073,21.9743919533248,-16.5411919174553));
#72051=CARTESIAN_POINT('Ctrl Pts',(-19.8565972560014,26.3838389403481,-16.3423050060804));
#72052=CARTESIAN_POINT('Ctrl Pts',(-23.9376190582342,28.189460266327,-16.1434180947055));
#72053=CARTESIAN_POINT('Ctrl Pts',(-27.662683865842,25.7320430241293,-15.9445311833306));
#72054=CARTESIAN_POINT('Ctrl Pts',(-27.6087729540455,21.2697453047119,-15.7456442719557));
#72055=CARTESIAN_POINT('Ctrl Pts',(-23.8254258798941,18.9030403717642,-15.5467573605808));
#72056=CARTESIAN_POINT('Ctrl Pts',(-19.7892178295995,20.8067293951777,-15.3478704492059));
#72057=CARTESIAN_POINT('Ctrl Pts',(-19.2090817873736,25.2314835686476,-15.148983537831));
#72058=CARTESIAN_POINT('Ctrl Pts',(-22.6181135885969,28.1113289640424,-14.9500966264561));
#72059=CARTESIAN_POINT('Ctrl Pts',(-26.8837020461773,26.7999318336181,-14.7512097150813));
#72060=CARTESIAN_POINT('Ctrl Pts',(-28.0861330298587,22.5023549520939,-14.5523228037064));
#72061=CARTESIAN_POINT('Ctrl Pts',(-25.1204744149729,19.1677070991591,-14.3534358923315));
#72062=CARTESIAN_POINT('Ctrl Pts',(-20.711915022215,19.8602469201477,-14.1545489809566));
#72063=CARTESIAN_POINT('Ctrl Pts',(-18.9115471493331,23.9435890372648,-13.9556620695817));
#72064=CARTESIAN_POINT('Ctrl Pts',(-21.3737562254823,27.6654882551987,-13.7567751582068));
#72065=CARTESIAN_POINT('Ctrl Pts',(-25.8359808705851,27.6058347576825,-13.5578882468319));
#72066=CARTESIAN_POINT('Ctrl Pts',(-28.1978149700514,23.819445051151,-13.359001335457));
#72067=CARTESIAN_POINT('Ctrl Pts',(-26.2889332369806,19.7856902430007,-13.1601144240821));
#72068=CARTESIAN_POINT('Ctrl Pts',(-21.8634361375834,19.2112489959131,-12.9612275127073));
#72069=CARTESIAN_POINT('Ctrl Pts',(-18.9879802859286,22.6239841113762,-12.7623406013324));
#72070=CARTESIAN_POINT('Ctrl Pts',(-20.3048658112352,26.8878813705002,-12.5634536899575));
#72071=CARTESIAN_POINT('Ctrl Pts',(-24.6039865692263,28.0847807110209,-12.3645667785826));
#72072=CARTESIAN_POINT('Ctrl Pts',(-27.9348150886385,25.1148331193285,-12.1656798672077));
#72073=CARTESIAN_POINT('Ctrl Pts',(-27.2366023678193,20.7071686221583,-11.9667929558328));
#72074=CARTESIAN_POINT('Ctrl Pts',(-23.150946698525,18.9120571840877,-11.7679060444579));
#72075=CARTESIAN_POINT('Ctrl Pts',(-19.4322192343616,21.3790540163528,-11.569019133083));
#72076=CARTESIAN_POINT('Ctrl Pts',(-19.4976152188011,25.8411981969398,-11.3701322217081));
#72077=CARTESIAN_POINT('Ctrl Pts',(-23.2870412868087,28.1981575513269,-11.1712453103332));
#72078=CARTESIAN_POINT('Ctrl Pts',(-27.3183361722328,26.2840862700306,-10.9723583989584));
#72079=CARTESIAN_POINT('Ctrl Pts',(-27.8870816728095,21.8578535740801,-10.7734714875834));
#72080=CARTESIAN_POINT('Ctrl Pts',(-24.4706488951754,18.9867920284081,-10.5745845762086));
#72081=CARTESIAN_POINT('Ctrl Pts',(-20.2084498962448,20.3091637676113,-10.3756976648337));
#72082=CARTESIAN_POINT('Ctrl Pts',(-19.0170841811534,24.6098212819959,-10.1768107534588));
#72083=CARTESIAN_POINT('Ctrl Pts',(-21.9913158309151,27.9368249514686,-9.97792384208393));
#72084=CARTESIAN_POINT('Ctrl Pts',(-26.3980781326575,27.2329404871772,-9.77903693070902));
#72085=CARTESIAN_POINT('Ctrl Pts',(-28.1879301629076,23.1449780322445,-9.58015001933414));
#72086=CARTESIAN_POINT('Ctrl Pts',(-25.7161496602922,19.4294284806953,-9.38126310795925));
#72087=CARTESIAN_POINT('Ctrl Pts',(-21.2540933342885,19.5005668437512,-9.18237619658437));
#72088=CARTESIAN_POINT('Ctrl Pts',(-18.9020126285053,23.2930229973027,-8.98348928520946));
#72089=CARTESIAN_POINT('Ctrl Pts',(-20.8212702880001,27.321851283492,-8.78460237383459));
#72090=CARTESIAN_POINT('Ctrl Pts',(-25.2482312499118,27.8849000956191,-8.58571546245968));
#72091=CARTESIAN_POINT('Ctrl Pts',(-28.1148937346359,24.4647753140061,-8.38682855108481));
#72092=CARTESIAN_POINT('Ctrl Pts',(-26.7870379716082,20.2042816341936,-8.1879416397099));
#72093=CARTESIAN_POINT('Ctrl Pts',(-22.4848508234485,19.0184515176349,-7.98905472833502));
#72094=CARTESIAN_POINT('Ctrl Pts',(-19.161677513998,21.996962299634,-7.79016781696012));
#72095=CARTESIAN_POINT('Ctrl Pts',(-19.8712325560094,26.4028151076025,-7.59128090558524));
#72096=CARTESIAN_POINT('Ctrl Pts',(-23.9614950262208,28.1874047657335,-7.39239399421034));
#72097=CARTESIAN_POINT('Ctrl Pts',(-27.6738605115759,25.7108446864556,-7.19350708283546));
#72098=CARTESIAN_POINT('Ctrl Pts',(-27.5969798877205,21.2488836049575,-6.99462017146056));
#72099=CARTESIAN_POINT('Ctrl Pts',(-23.801499929576,18.9016854432229,-6.79573326008568));
#72100=CARTESIAN_POINT('Ctrl Pts',(-19.7751449150443,20.8261263022999,-6.59684634871078));
#72101=CARTESIAN_POINT('Ctrl Pts',(-19.2177937238713,25.2538081983746,-6.3979594373359));
#72102=CARTESIAN_POINT('Ctrl Pts',(-22.6416048451565,28.1160668744714,-6.199072525961));
#72103=CARTESIAN_POINT('Ctrl Pts',(-26.9003861497507,26.7827292867736,-6.00018561458611));
#72104=CARTESIAN_POINT('Ctrl Pts',(-28.0806787038404,22.4790196299904,-5.80129870321121));
#72105=CARTESIAN_POINT('Ctrl Pts',(-25.0978937225233,19.1596821843009,-5.60241179183632));
#72106=CARTESIAN_POINT('Ctrl Pts',(-20.6929577051683,19.8749066288887,-5.40352488046145));
#72107=CARTESIAN_POINT('Ctrl Pts',(-18.9136333747395,23.9674623402106,-5.20463796908654));
#72108=CARTESIAN_POINT('Ctrl Pts',(-21.3949689290764,27.6766376110642,-5.00575105771166));
#72109=CARTESIAN_POINT('Ctrl Pts',(-25.8568273763043,27.5940148537369,-4.80686414633676));
#72110=CARTESIAN_POINT('Ctrl Pts',(-28.1991391066322,23.7955173769579,-4.60797723496188));
#72111=CARTESIAN_POINT('Ctrl Pts',(-26.2695182351733,19.771642302411,-4.40909032358698));
#72112=CARTESIAN_POINT('Ctrl Pts',(-21.8411227379283,19.2199896552601,-4.2102034122121));
#72113=CARTESIAN_POINT('Ctrl Pts',(-18.9832726108445,22.6474814458054,-4.01131650083721));
#72114=CARTESIAN_POINT('Ctrl Pts',(-20.3220898149793,26.9045433219168,-3.81242958946232));
#72115=CARTESIAN_POINT('Ctrl Pts',(-24.6273148527125,28.0792963587734,-3.61354267808743));
#72116=CARTESIAN_POINT('Ctrl Pts',(-27.9428109372554,25.0922421181359,-3.41465576671254));
#72117=CARTESIAN_POINT('Ctrl Pts',(-27.2219182746241,20.6882301867157,-3.21576885533764));
#72118=CARTESIAN_POINT('Ctrl Pts',(-23.1270761001584,18.9141741308522,-3.01688194396275));
#72119=CARTESIAN_POINT('Ctrl Pts',(-19.4210971868294,21.4002810507353,-2.81799503258785));
#72120=CARTESIAN_POINT('Ctrl Pts',(-19.5094619407915,25.8620294740987,-2.61910812121298));
#72121=CARTESIAN_POINT('Ctrl Pts',(-23.3109706452488,28.199450893754,-2.42022120983808));
#72122=CARTESIAN_POINT('Ctrl Pts',(-27.3323591155911,26.2646532056929,-2.22133429846319));
#72123=CARTESIAN_POINT('Ctrl Pts',(-27.8783123050894,21.8355514414517,-2.02244738708831));
#72124=CARTESIAN_POINT('Ctrl Pts',(-24.4471455217919,18.9821145964656,-1.82356047571341));
#72125=CARTESIAN_POINT('Ctrl Pts',(-20.1918101245799,20.3264091997288,-1.62467356433851));
#72126=CARTESIAN_POINT('Ctrl Pts',(-19.0225985505471,24.6331424882292,-1.42578665296364));
#72127=CARTESIAN_POINT('Ctrl Pts',(-22.013917103436,27.9447917206012,-1.22689974158873));
#72128=CARTESIAN_POINT('Ctrl Pts',(-26.4169976551308,27.218232033847,-1.02801283021384));
#72129=CARTESIAN_POINT('Ctrl Pts',(-28.1857824982912,23.1211101779908,-0.829125918838952));
#72130=CARTESIAN_POINT('Ctrl Pts',(-25.6949083302767,19.4183337599166,-0.630239007464067));
#72131=CARTESIAN_POINT('Ctrl Pts',(-21.2332773201901,19.5124403641663,-0.431352096089173));
#72132=CARTESIAN_POINT('Ctrl Pts',(-18.9007500823737,23.3169540003584,-0.232465184714285));
#72133=CARTESIAN_POINT('Ctrl Pts',(-20.8407213826837,27.3358492063947,-0.0335782733393948));
#72134=CARTESIAN_POINT('Ctrl Pts',(-25.2705220785774,27.8761020340494,0.165308638035495));
#72135=CARTESIAN_POINT('Ctrl Pts',(-28.1195409156902,24.441265940594,0.364195549410388));
#72136=CARTESIAN_POINT('Ctrl Pts',(-26.7697711396785,20.1876640698386,0.563082460785278));
#72137=CARTESIAN_POINT('Ctrl Pts',(-22.461536733092,19.0239958950423,0.761969372160167));
#72138=CARTESIAN_POINT('Ctrl Pts',(-19.1537398375437,22.0195738060519,0.96085628353506));
#72139=CARTESIAN_POINT('Ctrl Pts',(-19.8859653451146,26.4217156857727,1.15974319490995));
#72140=CARTESIAN_POINT('Ctrl Pts',(-23.9853600968326,28.1852263868222,1.35863010628484));
#72141=CARTESIAN_POINT('Ctrl Pts',(-27.6849278872261,25.6895890959863,1.55751701765973));
#72142=CARTESIAN_POINT('Ctrl Pts',(-27.5850795885454,21.2280828883946,1.75640392903463));
#72143=CARTESIAN_POINT('Ctrl Pts',(-23.7775673215383,18.9004536954778,1.95529084040951));
#72144=CARTESIAN_POINT('Ctrl Pts',(-19.7611720357803,20.8455953951155,2.15417775178442));
#72145=CARTESIAN_POINT('Ctrl Pts',(-19.2266204647196,25.27608768616,2.35306466315927));
#72146=CARTESIAN_POINT('Ctrl Pts',(-22.6651201796618,28.1206837969411,2.5519515745342));
#72147=CARTESIAN_POINT('Ctrl Pts',(-26.9169814792741,26.7654410836283,2.75083848590907));
#72148=CARTESIAN_POINT('Ctrl Pts',(-28.075104327602,22.4557126941228,2.94972539728396));
#72149=CARTESIAN_POINT('Ctrl Pts',(-25.0752720196569,19.151773613671,3.14861230865887));
#72150=CARTESIAN_POINT('Ctrl Pts',(-20.6740761026041,19.8896637293692,3.34749922003375));
#72151=CARTESIAN_POINT('Ctrl Pts',(-18.9158424643382,23.9913245876556,3.54638613140863));
#72152=CARTESIAN_POINT('Ctrl Pts',(-21.4162387447966,27.6876776232568,3.74527304278354));
#72153=CARTESIAN_POINT('Ctrl Pts',(-25.8776127608824,27.5820877955107,3.94415995415842));
#72154=CARTESIAN_POINT('Ctrl Pts',(-28.2003400539506,23.7715832035748,4.1430468655333));
#72155=CARTESIAN_POINT('Ctrl Pts',(-26.2500311764703,19.7576944899272,4.3419337769082));
#72156=CARTESIAN_POINT('Ctrl Pts',(-21.8188546279217,19.2288450607684,4.54082068828309));
#72157=CARTESIAN_POINT('Ctrl Pts',(-18.978685954606,22.6710027024584,4.73970759965797));
#72158=CARTESIAN_POINT('Ctrl Pts',(-20.3393993607078,26.9211163891241,4.93859451103288));
#72159=CARTESIAN_POINT('Ctrl Pts',(-24.6506145954909,28.0736919929358,5.13748142240776));
#72160=CARTESIAN_POINT('Ctrl Pts',(-27.9506903889628,25.0696102562865,5.33636833378264));
#72161=CARTESIAN_POINT('Ctrl Pts',(-27.2071368872086,20.6693675910284,5.53525524515755));
#72162=CARTESIAN_POINT('Ctrl Pts',(-23.1032167153998,18.9164139274794,5.73414215653244));
#72163=CARTESIAN_POINT('Ctrl Pts',(-19.4100845563787,21.42156505648,5.93302906790731));
#72164=CARTESIAN_POINT('Ctrl Pts',(-19.5214157383157,25.8827994922676,6.13191597928223));
#72165=CARTESIAN_POINT('Ctrl Pts',(-23.3349063443381,28.2006210386571,6.3308028906571));
#72166=CARTESIAN_POINT('Ctrl Pts',(-27.346281838195,26.2451482133761,6.52968980203199));
#72167=CARTESIAN_POINT('Ctrl Pts',(-27.8694282495872,21.8132947461036,6.72857671340688));
#72168=CARTESIAN_POINT('Ctrl Pts',(-24.4236183819465,18.9775582140545,6.92746362478179));
#72169=CARTESIAN_POINT('Ctrl Pts',(-20.1752593471366,20.3437400593731,7.12635053615665));
#72170=CARTESIAN_POINT('Ctrl Pts',(-19.0282328967019,24.6564349993302,7.32523744753157));
#72171=CARTESIAN_POINT('Ctrl Pts',(-22.0365590867865,27.9526420403365,7.52412435890644));
#72172=CARTESIAN_POINT('Ctrl Pts',(-26.4358412127014,27.2034263839771,7.72301127028133));
#72173=CARTESIAN_POINT('Ctrl Pts',(-28.1835119983449,23.0972536954341,7.92189818165623));
#72174=CARTESIAN_POINT('Ctrl Pts',(-25.6736101697574,19.4073485294465,8.12078509303112));
#72175=CARTESIAN_POINT('Ctrl Pts',(-21.212522702829,19.5244208811907,8.31967200440601));
#72176=CARTESIAN_POINT('Ctrl Pts',(-18.8996107418241,23.3408911855124,8.5185589157809));
#72177=CARTESIAN_POINT('Ctrl Pts',(-20.8602442763108,27.3497468160602,8.71744582715579));
#72178=CARTESIAN_POINT('Ctrl Pts',(-25.2927673224061,27.8671893432668,8.91633273853067));
#72179=CARTESIAN_POINT('Ctrl Pts',(-28.1240670167278,24.417732956521,9.11521964990558));
#72180=CARTESIAN_POINT('Ctrl Pts',(-26.7524189948213,20.1711356095702,9.31410656128044));
#72181=CARTESIAN_POINT('Ctrl Pts',(-22.4382514922448,19.0296602121829,9.51299347265536));
#72182=CARTESIAN_POINT('Ctrl Pts',(-19.1459186627819,22.0422258734042,9.71188038403022));
#72183=CARTESIAN_POINT('Ctrl Pts',(-19.9007952329182,26.4405401740185,9.91076729540515));
#72184=CARTESIAN_POINT('Ctrl Pts',(-24.0092136376771,28.182925187317,10.10965420678));
#72185=CARTESIAN_POINT('Ctrl Pts',(-27.6958856995223,25.668276815966,10.308541118155));
#72186=CARTESIAN_POINT('Ctrl Pts',(-27.5730723718623,21.2073437062143,10.5074280295298));
#72187=CARTESIAN_POINT('Ctrl Pts',(-23.7536286899636,18.8993451611687,10.7063149409047));
#72188=CARTESIAN_POINT('Ctrl Pts',(-19.74729956207,20.8651361577193,10.9052018522796));
#72189=CARTESIAN_POINT('Ctrl Pts',(-19.2355617760216,25.2983214416274,11.1040887636545));
#72190=CARTESIAN_POINT('Ctrl Pts',(-22.6886589689878,28.125179609109,11.3029756750294));
#72191=CARTESIAN_POINT('Ctrl Pts',(-26.9334875949936,26.7480676822966,11.5018625864043));
#72192=CARTESIAN_POINT('Ctrl Pts',(-28.0694100488568,22.4324347620937,11.7007494977791));
#72193=CARTESIAN_POINT('Ctrl Pts',(-25.0526099058185,19.143981596836,11.8996364091541));
#72194=CARTESIAN_POINT('Ctrl Pts',(-20.6552707148596,19.9045178305457,12.098523320529));
#72195=CARTESIAN_POINT('Ctrl Pts',(-18.9181743595909,24.0151751472824,12.2974102319038));
#72196=CARTESIAN_POINT('Ctrl Pts',(-21.4375651090214,27.6986079992308,12.4962971432787));
#72197=CARTESIAN_POINT('Ctrl Pts',(-25.8983364735341,27.5700538990548,12.6951840546536));
#72198=CARTESIAN_POINT('Ctrl Pts',(-28.2014177801836,23.747643165226,12.8940709660285));
#72199=CARTESIAN_POINT('Ctrl Pts',(-26.2304725772522,19.7438471751471,13.0929578774034));
#72200=CARTESIAN_POINT('Ctrl Pts',(-21.7966323976384,19.2378149777817,13.2918447887783));
#72201=CARTESIAN_POINT('Ctrl Pts',(-18.9742204387534,22.6945472580531,13.4907317001532));
#72202=CARTESIAN_POINT('Ctrl Pts',(-20.3567939897411,26.937600132958,13.6896186115281));
#72203=CARTESIAN_POINT('Ctrl Pts',(-24.6738851801498,28.0679677620165,13.888505522903));
#72204=CARTESIAN_POINT('Ctrl Pts',(-27.958453234966,25.0469381334941,14.0873924342778));
#72205=CARTESIAN_POINT('Ctrl Pts',(-27.19225859726,20.6505813349302,14.2862793456527));
#72206=CARTESIAN_POINT('Ctrl Pts',(-23.0793691764913,18.9187765146178,14.4851662570276));
#72207=CARTESIAN_POINT('Ctrl Pts',(-19.3991816348293,21.4429054695892,14.6840531684025));
#72208=CARTESIAN_POINT('Ctrl Pts',(-19.533476294614,25.9035077010689,14.8829400797774));
#72209=CARTESIAN_POINT('Ctrl Pts',(-23.3588477498126,28.2016679550287,15.0818269911523));
#72210=CARTESIAN_POINT('Ctrl Pts',(-27.360103971111,26.2255718099364,15.2807139025272));
#72211=CARTESIAN_POINT('Ctrl Pts',(-27.8604297417186,21.7910840778083,15.4796008139021));
#72212=CARTESIAN_POINT('Ctrl Pts',(-24.4000680990767,18.9731230019129,15.678487725277));
#72213=CARTESIAN_POINT('Ctrl Pts',(-20.1587980024883,20.3611558872995,15.8773746366519));
#72214=CARTESIAN_POINT('Ctrl Pts',(-19.0339870703151,24.6796981980787,16.0762615480267));
#72215=CARTESIAN_POINT('Ctrl Pts',(-22.0592411809838,27.9603757026515,16.2751484594016));
#72216=CARTESIAN_POINT('Ctrl Pts',(-26.4546083060402,27.1885239298975,16.4740353707766));
#72217=CARTESIAN_POINT('Ctrl Pts',(-28.1811187232336,23.0734092167393,16.6729222821514));
#72218=CARTESIAN_POINT('Ctrl Pts',(-25.6522557431073,19.3964730803787,16.8718091935263));
#72219=CARTESIAN_POINT('Ctrl Pts',(-21.1918300321744,19.5365080773572,17.0706961049012));
#72220=CARTESIAN_POINT('Ctrl Pts',(-18.8985946370477,23.3648339184615,17.2695830162761));
#72221=CARTESIAN_POINT('Ctrl Pts',(-20.8798384515504,27.3635437442206,17.468469927651));
#72222=CARTESIAN_POINT('Ctrl Pts',(-25.3149663919288,27.8581622594458,17.6673568390259));
#72223=CARTESIAN_POINT('Ctrl Pts',(-28.1284719178129,24.3941769853794,17.8662437504008));
#72224=CARTESIAN_POINT('Ctrl Pts',(-26.7349819968456,20.1546966913704,18.0651306617757));
#72225=CARTESIAN_POINT('Ctrl Pts',(-22.4149957179343,19.0354443189599,18.2640175731505));
#72226=CARTESIAN_POINT('Ctrl Pts',(-19.1382141969635,22.0649179014414,18.4629044845255));
#72227=CARTESIAN_POINT('Ctrl Pts',(-19.915721826448,26.4592880735162,18.6617913959003));
#72228=CARTESIAN_POINT('Ctrl Pts',(-24.0330550166675,28.1805012281969,18.8606783072753));
#72229=CARTESIAN_POINT('Ctrl Pts',(-27.7067336580968,25.6469084111413,19.0595652186501));
#72230=CARTESIAN_POINT('Ctrl Pts',(-27.560958555846,21.1866666079772,19.258452130025));
#72231=CARTESIAN_POINT('Ctrl Pts',(-23.7296846691934,18.8983598696701,19.4573390413999));
#72232=CARTESIAN_POINT('Ctrl Pts',(-19.7335278615154,20.8847480723076,19.6562259527748));
#72233=CARTESIAN_POINT('Ctrl Pts',(-19.2446174208448,25.320508875612,19.8551128641497));
#72234=CARTESIAN_POINT('Ctrl Pts',(-22.7122205893882,28.1295541918424,20.0539997755246));
#72235=CARTESIAN_POINT('Ctrl Pts',(-26.9499040595195,26.73060954315,20.2528866868994));
#72236=CARTESIAN_POINT('Ctrl Pts',(-28.0635960184952,22.4091864507369,20.4517735982743));
#72237=CARTESIAN_POINT('Ctrl Pts',(-25.0299079815236,19.1363063402742,20.6506605096492));
#72238=CARTESIAN_POINT('Ctrl Pts',(-20.6365420402524,19.9194685388046,20.8495474210241));
#72239=CARTESIAN_POINT('Ctrl Pts',(-18.9206289987058,24.0390133870832,21.048434332399));
#72240=CARTESIAN_POINT('Ctrl Pts',(-21.4589474566307,27.709428449346,21.2473212437739));
#72241=CARTESIAN_POINT('Ctrl Pts',(-25.9189979651091,27.5579134832514,21.4462081551488));
#72242=CARTESIAN_POINT('Ctrl Pts',(-28.2023722567724,23.7236978962898,21.6450950665237));
#72243=CARTESIAN_POINT('Ctrl Pts',(-26.2108429557959,19.7301007250066,21.8439819778986));
#72244=CARTESIAN_POINT('Ctrl Pts',(-21.7744566359379,19.246899168609,22.0428688892735));
#72245=CARTESIAN_POINT('Ctrl Pts',(-18.969876181617,22.7181144886908,22.2417558006483));
#72246=CARTESIAN_POINT('Ctrl Pts',(-20.3742732411446,26.9539941166208,22.4406427120233));
#72247=CARTESIAN_POINT('Ctrl Pts',(-24.69712599005,28.0621238177003,22.6395296233981));
#72248=CARTESIAN_POINT('Ctrl Pts',(-27.9660992695595,25.0242263505381,22.838416534773));
#72249=CARTESIAN_POINT('Ctrl Pts',(-27.1772837990336,20.6318719162339,23.0373034461479));
#72250=CARTESIAN_POINT('Ctrl Pts',(-23.0555341153588,18.9212618296573,23.2361903575228));
#72251=CARTESIAN_POINT('Ctrl Pts',(-19.3883887110968,21.4643017245793,23.4350772688977));
#72252=CARTESIAN_POINT('Ctrl Pts',(-19.5456432900926,25.9241535517461,23.6339641802726));
#72253=CARTESIAN_POINT('Ctrl Pts',(-23.3827942272672,28.2025916151584,23.8328510916475));
#72254=CARTESIAN_POINT('Ctrl Pts',(-27.3738251480522,26.2059245140626,24.0317380030224));
#72255=CARTESIAN_POINT('Ctrl Pts',(-27.8513170199678,21.7689200252309,24.2306249143973));
#72256=CARTESIAN_POINT('Ctrl Pts',(-24.3764952971655,18.9688090773561,24.4295118257721));
#72257=CARTESIAN_POINT('Ctrl Pts',(-20.142426526967,20.378656222412,24.6283987371471));
#72258=CARTESIAN_POINT('Ctrl Pts',(-19.0398609186662,24.7029314672756,24.8272856485219));
#72259=CARTESIAN_POINT('Ctrl Pts',(-22.0819627854415,27.9679925040413,25.0261725598969));
#72260=CARTESIAN_POINT('Ctrl Pts',(-26.4732984369799,27.1735250638085,25.2250594712717));
#72261=CARTESIAN_POINT('Ctrl Pts',(-28.1786027380087,23.0495773788407,25.4239463826466));
#72262=CARTESIAN_POINT('Ctrl Pts',(-25.6308456131075,19.3857076912915,25.6228332940215));
#72263=CARTESIAN_POINT('Ctrl Pts',(-21.1711998623744,19.5487016505103,25.8217202053964));
#72264=CARTESIAN_POINT('Ctrl Pts',(-18.8977017839806,23.3887815305051,26.0206071167713));
#72265=CARTESIAN_POINT('Ctrl Pts',(-20.8995034099329,27.3772396899469,26.2194940281462));
#72266=CARTESIAN_POINT('Ctrl Pts',(-25.3371186597208,27.8490208996796,26.4183809395211));
#72267=CARTESIAN_POINT('Ctrl Pts',(-28.1327555762001,24.3705988819437,26.6172678508959));
#72268=CARTESIAN_POINT('Ctrl Pts',(-26.7174604681214,20.1383473154802,26.8161547622709));
#72269=CARTESIAN_POINT('Ctrl Pts',(-22.3917702901644,19.0413488841658,27.0150416736457));
#72270=CARTESIAN_POINT('Ctrl Pts',(-19.1306261462195,22.0876477366323,27.2139285850206));
#72271=CARTESIAN_POINT('Ctrl Pts',(-19.9307456705459,26.4779618183849,27.4128154963955));
#72272=CARTESIAN_POINT('Ctrl Pts',(-24.0568818264179,28.1779490395339,27.6117024077704));
#72273=CARTESIAN_POINT('Ctrl Pts',(-27.7174748282288,25.625494897365,27.8105893191453));
#72274=CARTESIAN_POINT('Ctrl Pts',(-27.54873213085,21.1660324105898,28.0094762305202));
#72275=CARTESIAN_POINT('Ctrl Pts',(-23.7057478472643,18.8975351032718,28.2083631418951));
#72276=CARTESIAN_POINT('Ctrl Pts',(-19.7198347282729,20.904360271747,28.40725005327));
#72277=CARTESIAN_POINT('Ctrl Pts',(-19.2538297777398,25.3427822320754,28.6061369646448));
#72278=CARTESIAN_POINT('Ctrl Pts',(-22.7357239416392,28.1335566023601,28.8050238760198));
#72279=CARTESIAN_POINT('Ctrl Pts',(-26.9663824108126,26.7135408490309,29.0039107873946));
#72280=CARTESIAN_POINT('Ctrl Pts',(-28.0573752707713,22.3850730121439,29.2027976987696));
#72281=CARTESIAN_POINT('Ctrl Pts',(-25.0077103293766,19.1304459024294,29.4016846101444));
#72282=CARTESIAN_POINT('Ctrl Pts',(-20.6168533946832,19.9312505216016,29.6005715215193));
#72283=CARTESIAN_POINT('Ctrl Pts',(-18.9252562888303,24.0694825381366,29.7994584328942));
#72284=CARTESIAN_POINT('Ctrl Pts',(-20.6254760904471,26.4925251454433,29.9320497071441));
#72285=CARTESIAN_POINT('Ctrl Pts',(-21.8002837957285,27.0756816094313,29.9983453442691));
#72286=CARTESIAN_POINT('Ctrl Pts',(-21.4056980533955,20.5397621095878,-75.2735003480446));
#72287=CARTESIAN_POINT('Ctrl Pts',(-20.4017695023793,21.2548416367245,-75.2071605181002));
#72288=CARTESIAN_POINT('Ctrl Pts',(-19.1839163191839,23.7551997076661,-75.0745250510308));
#72289=CARTESIAN_POINT('Ctrl Pts',(-21.3678897177328,27.3419747835828,-74.8755939468365));
#72290=CARTESIAN_POINT('Ctrl Pts',(-25.5584650129784,27.4321216345841,-74.6767070354616));
#72291=CARTESIAN_POINT('Ctrl Pts',(-27.9027813811771,23.9610038383834,-74.4778201240867));
#72292=CARTESIAN_POINT('Ctrl Pts',(-26.2479589884383,20.1093797044535,-74.2789332127118));
#72293=CARTESIAN_POINT('Ctrl Pts',(-22.1139262816015,19.4212427346286,-74.080046301337));
#72294=CARTESIAN_POINT('Ctrl Pts',(-19.2998863162224,22.526459948928,-73.881159389962));
#72295=CARTESIAN_POINT('Ctrl Pts',(-20.3915033145888,26.5729088825349,-73.6822724785872));
#72296=CARTESIAN_POINT('Ctrl Pts',(-24.3857796829293,27.8415529321505,-73.4833855672123));
#72297=CARTESIAN_POINT('Ctrl Pts',(-27.6122580265173,25.1669828476232,-73.2844986558374));
#72298=CARTESIAN_POINT('Ctrl Pts',(-27.1061080032505,21.0067073707803,-73.0856117444625));
#72299=CARTESIAN_POINT('Ctrl Pts',(-23.3324228432654,19.1837698863755,-72.8867248330876));
#72300=CARTESIAN_POINT('Ctrl Pts',(-19.7589075818257,21.3732408577498,-72.6878379217128));
#72301=CARTESIAN_POINT('Ctrl Pts',(-19.6693153490062,25.5632109755048,-72.4889510103378));
#72302=CARTESIAN_POINT('Ctrl Pts',(-23.1459761467135,27.9034376590548,-72.290064098963));
#72303=CARTESIAN_POINT('Ctrl Pts',(-26.9941322368646,26.2434591040856,-72.091177187588));
#72304=CARTESIAN_POINT('Ctrl Pts',(-27.6776550976768,22.1086505701856,-71.8922902762132));
#72305=CARTESIAN_POINT('Ctrl Pts',(-24.5684448262307,19.2985527977709,-71.6934033648382));
#72306=CARTESIAN_POINT('Ctrl Pts',(-20.5236022282072,20.3954061795816,-71.4945164534635));
#72307=CARTESIAN_POINT('Ctrl Pts',(-19.2599946077614,24.3912960927353,-71.2956295420884));
#72308=CARTESIAN_POINT('Ctrl Pts',(-21.938770283371,27.6143381651901,-71.0967426307136));
#72309=CARTESIAN_POINT('Ctrl Pts',(-26.0983615045746,27.1028301799775,-70.8978557193387));
#72310=CARTESIAN_POINT('Ctrl Pts',(-27.9164566287204,23.3268045121349,-70.6989688079639));
#72311=CARTESIAN_POINT('Ctrl Pts',(-25.7223803781076,19.7561086463548,-70.5000818965888));
#72312=CARTESIAN_POINT('Ctrl Pts',(-21.5323028041158,19.6719093116581,-70.3011949852142));
#72313=CARTESIAN_POINT('Ctrl Pts',(-19.1965499351028,23.1515785717638,-70.102308073839));
#72314=CARTESIAN_POINT('Ctrl Pts',(-20.8614806196438,26.99759539649,-69.9034211624643));
#72315=CARTESIAN_POINT('Ctrl Pts',(-24.9971647208865,27.6757964163086,-69.7045342510893));
#72316=CARTESIAN_POINT('Ctrl Pts',(-27.803259198295,24.5629723938821,-69.5056473397145));
#72317=CARTESIAN_POINT('Ctrl Pts',(-26.701201144539,20.5195446829723,-69.3067604283396));
#72318=CARTESIAN_POINT('Ctrl Pts',(-22.7036884719959,19.2610805231846,-69.1078735169647));
#72319=CARTESIAN_POINT('Ctrl Pts',(-19.4840963935033,21.9440017775089,-68.9089866055898));
#72320=CARTESIAN_POINT('Ctrl Pts',(-20.0009570528289,26.1029312872671,-68.7100996942149));
#72321=CARTESIAN_POINT('Ctrl Pts',(-23.7793193265963,27.916165452151,-68.5112127828401));
#72322=CARTESIAN_POINT('Ctrl Pts',(-27.3471886375126,25.7174958114912,-68.3123258714651));
#72323=CARTESIAN_POINT('Ctrl Pts',(-27.4259955942737,21.5273133486342,-68.1134389600903));
#72324=CARTESIAN_POINT('Ctrl Pts',(-23.9433232853466,19.1960404780467,-67.9145520487153));
#72325=CARTESIAN_POINT('Ctrl Pts',(-20.0994522807164,20.8659193084615,-67.7156651373405));
#72326=CARTESIAN_POINT('Ctrl Pts',(-19.4265741271225,25.0024727771007,-67.5167782259656));
#72327=CARTESIAN_POINT('Ctrl Pts',(-22.5430067970579,27.804558968184,-67.3178913145907));
#72328=CARTESIAN_POINT('Ctrl Pts',(-26.585012896769,26.6972982498353,-67.1190044032158));
#72329=CARTESIAN_POINT('Ctrl Pts',(-27.8383315262235,22.6981693419905,-66.9201174918409));
#72330=CARTESIAN_POINT('Ctrl Pts',(-25.1512691288489,19.4820326407425,-66.721230580466));
#72331=CARTESIAN_POINT('Ctrl Pts',(-20.9930082225112,20.0042450911138,-66.5223436690911));
#72332=CARTESIAN_POINT('Ctrl Pts',(-19.1846380177503,23.7849377275274,-66.3234567577163));
#72333=CARTESIAN_POINT('Ctrl Pts',(-21.3878974082326,27.3499745669935,-66.1245698463413));
#72334=CARTESIAN_POINT('Ctrl Pts',(-25.5781778196954,27.4233890193208,-65.9256829349665));
#72335=CARTESIAN_POINT('Ctrl Pts',(-27.9049668311952,23.9377194273396,-65.7267960235915));
#72336=CARTESIAN_POINT('Ctrl Pts',(-26.2301426203391,20.0960006100355,-65.5279091122166));
#72337=CARTESIAN_POINT('Ctrl Pts',(-22.0927266352278,19.4284464364696,-65.3290222008418));
#72338=CARTESIAN_POINT('Ctrl Pts',(-19.2946533711521,22.5484825928889,-65.1301352894669));
#72339=CARTESIAN_POINT('Ctrl Pts',(-20.4071149203071,26.589060386986,-64.931248378092));
#72340=CARTESIAN_POINT('Ctrl Pts',(-24.4078534402043,27.8372314104878,-64.7323614667171));
#72341=CARTESIAN_POINT('Ctrl Pts',(-27.6205294377469,25.146032320247,-64.5334745553423));
#72342=CARTESIAN_POINT('Ctrl Pts',(-27.0929660611986,20.9884469041403,-64.3345876439672));
#72343=CARTESIAN_POINT('Ctrl Pts',(-23.3099493236091,19.1849436544572,-64.1357007325925));
#72344=CARTESIAN_POINT('Ctrl Pts',(-19.7477508598977,21.3927891457973,-63.9368138212175));
#72345=CARTESIAN_POINT('Ctrl Pts',(-19.6797290335917,25.583160566047,-63.7379269098427));
#72346=CARTESIAN_POINT('Ctrl Pts',(-23.1683901357664,27.9054618649038,-63.5390399984677));
#72347=CARTESIAN_POINT('Ctrl Pts',(-27.0079504032068,26.2256950473984,-63.3401530870929));
#72348=CARTESIAN_POINT('Ctrl Pts',(-27.6701794911614,22.0874233980783,-63.1412661757179));
#72349=CARTESIAN_POINT('Ctrl Pts',(-24.5465450155675,19.2933676950938,-62.9423792643431));
#72350=CARTESIAN_POINT('Ctrl Pts',(-20.5074022189665,20.4110282326302,-62.7434923529682));
#72351=CARTESIAN_POINT('Ctrl Pts',(-19.2643808686007,24.4133697386781,-62.5446054415934));
#72352=CARTESIAN_POINT('Ctrl Pts',(-21.9597121946251,27.6225797117789,-62.3457185302184));
#72353=CARTESIAN_POINT('Ctrl Pts',(-26.1166152348344,27.0896662827878,-62.1468316188435));
#72354=CARTESIAN_POINT('Ctrl Pts',(-27.9152485425322,23.3043317093402,-61.9479447074687));
#72355=CARTESIAN_POINT('Ctrl Pts',(-25.7028206069009,19.7449775209885,-61.7490577960937));
#72356=CARTESIAN_POINT('Ctrl Pts',(-21.5123651178303,19.6823484333594,-61.5501708847189));
#72357=CARTESIAN_POINT('Ctrl Pts',(-19.1945553777414,23.173995267913,-61.3512839733439));
#72358=CARTESIAN_POINT('Ctrl Pts',(-20.8792620199174,27.0113906265264,-61.1523970619691));
#72359=CARTESIAN_POINT('Ctrl Pts',(-25.0183824797664,27.6682935321061,-60.9535101505941));
#72360=CARTESIAN_POINT('Ctrl Pts',(-27.8084159942293,24.5410659106062,-60.7546232392194));
#72361=CARTESIAN_POINT('Ctrl Pts',(-26.685558319347,20.5033648010071,-60.5557363278443));
#72362=CARTESIAN_POINT('Ctrl Pts',(-22.681620455705,19.2654951824313,-60.3568494164696));
#72363=CARTESIAN_POINT('Ctrl Pts',(-19.4758818220422,21.9649542803137,-60.1579625050946));
#72364=CARTESIAN_POINT('Ctrl Pts',(-20.0141444208808,26.1211680600887,-59.9590755937197));
#72365=CARTESIAN_POINT('Ctrl Pts',(-23.8017905610305,27.9149284469595,-59.7601886823449));
#72366=CARTESIAN_POINT('Ctrl Pts',(-27.358294579128,25.6979217311929,-59.5613017709699));
#72367=CARTESIAN_POINT('Ctrl Pts',(-27.4155308243559,21.5073891134064,-59.3624148595951));
#72368=CARTESIAN_POINT('Ctrl Pts',(-23.9209040401828,19.1940747707718,-59.1635279482201));
#72369=CARTESIAN_POINT('Ctrl Pts',(-20.0856799457743,20.8837184474582,-58.9646410368453));
#72370=CARTESIAN_POINT('Ctrl Pts',(-19.434104310512,25.0236808627504,-58.7657541254704));
#72371=CARTESIAN_POINT('Ctrl Pts',(-22.5649198986986,27.809687567923,-58.5668672140955));
#72372=CARTESIAN_POINT('Ctrl Pts',(-26.6011726341775,26.6816346153375,-58.3679803027206));
#72373=CARTESIAN_POINT('Ctrl Pts',(-27.8338884708415,22.6761070253018,-58.1690933913457));
#72374=CARTESIAN_POINT('Ctrl Pts',(-25.1303060718632,19.473845040324,-57.9702064799708));
#72375=CARTESIAN_POINT('Ctrl Pts',(-20.9747884359177,20.0174559175559,-57.7713195685959));
#72376=CARTESIAN_POINT('Ctrl Pts',(-19.1859039406453,23.8074073514233,-57.5724326572211));
#72377=CARTESIAN_POINT('Ctrl Pts',(-21.407485764808,27.3610553090927,-57.3735457458461));
#72378=CARTESIAN_POINT('Ctrl Pts',(-25.5980885710774,27.4128986171263,-57.1746588344714));
#72379=CARTESIAN_POINT('Ctrl Pts',(-27.9069036850169,23.9152976710286,-56.9757719230963));
#72380=CARTESIAN_POINT('Ctrl Pts',(-26.2123257721566,20.0822511926065,-56.7768850117216));
#72381=CARTESIAN_POINT('Ctrl Pts',(-22.0715282579012,19.4360039067815,-56.5779981003465));
#72382=CARTESIAN_POINT('Ctrl Pts',(-19.2895529761186,22.5704022764929,-56.3791111889718));
#72383=CARTESIAN_POINT('Ctrl Pts',(-20.4227993381602,26.6051999531328,-56.1802242775967));
#72384=CARTESIAN_POINT('Ctrl Pts',(-24.4299100207564,27.8327599662979,-55.981337366222));
#72385=CARTESIAN_POINT('Ctrl Pts',(-27.6286900535603,25.1250587438152,-55.782450454847));
#72386=CARTESIAN_POINT('Ctrl Pts',(-27.0797317982467,20.9702441339412,-55.5835635434722));
#72387=CARTESIAN_POINT('Ctrl Pts',(-23.2874813474644,19.1862384929635,-55.3846766320972));
#72388=CARTESIAN_POINT('Ctrl Pts',(-19.7366953356669,21.4123917462059,-55.1857897207224));
#72389=CARTESIAN_POINT('Ctrl Pts',(-19.690245050689,25.6030578006088,-54.9869028093475));
#72390=CARTESIAN_POINT('Ctrl Pts',(-23.1908143660906,27.9073698620638,-54.7880158979726));
#72391=CARTESIAN_POINT('Ctrl Pts',(-27.0216768803512,26.2078605195381,-54.5891289865977));
#72392=CARTESIAN_POINT('Ctrl Pts',(-27.6625947464435,22.0662347641827,-54.3902420752228));
#72393=CARTESIAN_POINT('Ctrl Pts',(-24.5246187863028,19.2882955132131,-54.1913551638479));
#72394=CARTESIAN_POINT('Ctrl Pts',(-20.4912828508116,20.4267334078627,-53.9924682524731));
#72395=CARTESIAN_POINT('Ctrl Pts',(-19.2688806941927,24.4354205465643,-53.7935813410981));
#72396=CARTESIAN_POINT('Ctrl Pts',(-21.9806962557675,27.6307133294717,-53.5946944297233));
#72397=CARTESIAN_POINT('Ctrl Pts',(-26.1348009584921,27.0764086052445,-53.3958075183484));
#72398=CARTESIAN_POINT('Ctrl Pts',(-27.9139247905591,23.2818654181574,-53.1969206069734));
#72399=CARTESIAN_POINT('Ctrl Pts',(-25.6832037951245,19.7339472329358,-52.9980336955985));
#72400=CARTESIAN_POINT('Ctrl Pts',(-21.4924814330418,19.692890047943,-52.7991467842237));
#72401=CARTESIAN_POINT('Ctrl Pts',(-19.1926762404031,23.1964219351121,-52.6002598728488));
#72402=CARTESIAN_POINT('Ctrl Pts',(-20.8971141979184,27.0250941406527,-52.4013729614739));
#72403=CARTESIAN_POINT('Ctrl Pts',(-25.0395613351389,27.6606815255441,-52.202486050099));
#72404=CARTESIAN_POINT('Ctrl Pts',(-27.8134599545569,24.5191331719944,-52.0035991387242));
#72405=CARTESIAN_POINT('Ctrl Pts',(-26.6698324127457,20.4872656575404,-51.8047122273491));
#72406=CARTESIAN_POINT('Ctrl Pts',(-22.6595754570046,19.270023381973,-51.6058253159744));
#72407=CARTESIAN_POINT('Ctrl Pts',(-19.4677752159405,21.9859487914132,-51.4069384045994));
#72408=CARTESIAN_POINT('Ctrl Pts',(-20.0274254910585,26.1393367070863,-51.2080514932246));
#72409=CARTESIAN_POINT('Ctrl Pts',(-23.8242551300434,27.9135757837119,-51.0091645818496));
#72410=CARTESIAN_POINT('Ctrl Pts',(-27.3692996127346,25.6782907405373,-50.8102776704749));
#72411=CARTESIAN_POINT('Ctrl Pts',(-27.4049636297446,21.4875190113221,-50.6113907590997));
#72412=CARTESIAN_POINT('Ctrl Pts',(-23.8984749732513,19.1922244963672,-50.4125038477251));
#72413=CARTESIAN_POINT('Ctrl Pts',(-20.0719994173611,20.9015882460338,-50.2136169363501));
#72414=CARTESIAN_POINT('Ctrl Pts',(-19.4417435663115,25.0448499045242,-50.0147300249752));
#72415=CARTESIAN_POINT('Ctrl Pts',(-22.586859110333,27.8147032983438,-49.8158431136003));
#72416=CARTESIAN_POINT('Ctrl Pts',(-26.6172515262933,26.6658880034122,-49.6169562022254));
#72417=CARTESIAN_POINT('Ctrl Pts',(-27.8293319048493,22.6540678722973,-49.4180692908506));
#72418=CARTESIAN_POINT('Ctrl Pts',(-25.1093011455769,19.4657654592394,-49.2191823794755));
#72419=CARTESIAN_POINT('Ctrl Pts',(-20.9566368956703,20.0307603583726,-49.0202954681009));
#72420=CARTESIAN_POINT('Ctrl Pts',(-19.1872855129273,23.829870161061,-48.8214085567257));
#72421=CARTESIAN_POINT('Ctrl Pts',(-21.4271309018305,27.3720350700269,-48.6225216453511));
#72422=CARTESIAN_POINT('Ctrl Pts',(-25.6179450575493,27.4023058599883,-48.423634733976));
#72423=CARTESIAN_POINT('Ctrl Pts',(-27.9087250934233,23.8928662415108,-48.2247478226013));
#72424=CARTESIAN_POINT('Ctrl Pts',(-26.1944383826017,20.0685936725639,-48.0258609112262));
#72425=CARTESIAN_POINT('Ctrl Pts',(-22.0503690647856,19.4436703991666,-47.8269739998515));
#72426=CARTESIAN_POINT('Ctrl Pts',(-19.2845654839116,22.5923479248151,-47.6280870884765));
#72427=CARTESIAN_POINT('Ctrl Pts',(-20.4385666293305,26.621258567268,-47.4292001771016));
#72428=CARTESIAN_POINT('Ctrl Pts',(-24.4519432915644,27.828175041402,-47.2303132657268));
#72429=CARTESIAN_POINT('Ctrl Pts',(-27.6367425962466,25.1040434371298,-47.0314263543518));
#72430=CARTESIAN_POINT('Ctrl Pts',(-27.0664040088257,20.9521097305061,-46.832539442977));
#72431=CARTESIAN_POINT('Ctrl Pts',(-23.2650203344038,19.1876489719916,-46.6336525316021));
#72432=CARTESIAN_POINT('Ctrl Pts',(-19.7257408655894,21.4320509970594,-46.4347656202272));
#72433=CARTESIAN_POINT('Ctrl Pts',(-19.70086335281,25.6229006385828,-46.2358787088523));
#72434=CARTESIAN_POINT('Ctrl Pts',(-23.2132481210444,27.9091624014555,-46.0369917974774));
#72435=CARTESIAN_POINT('Ctrl Pts',(-27.0353113694039,26.1899555686286,-45.8381048861025));
#72436=CARTESIAN_POINT('Ctrl Pts',(-27.6549010301699,22.0450854547685,-45.6392179747276));
#72437=CARTESIAN_POINT('Ctrl Pts',(-24.5026667376387,19.28333626748,-45.4403310633527));
#72438=CARTESIAN_POINT('Ctrl Pts',(-20.4752445412525,20.4425213521647,-45.2414441519778));
#72439=CARTESIAN_POINT('Ctrl Pts',(-19.2734939703991,24.4574478986848,-45.0425572406029));
#72440=CARTESIAN_POINT('Ctrl Pts',(-22.001721908047,27.6387388204235,-44.843670329228));
#72441=CARTESIAN_POINT('Ctrl Pts',(-26.1529181950812,27.0630574892923,-44.6447834178532));
#72442=CARTESIAN_POINT('Ctrl Pts',(-27.9124854071207,23.2594062388733,-44.4458965064782));
#72443=CARTESIAN_POINT('Ctrl Pts',(-25.6635304629989,19.7230180718576,-44.2470095951034));
#72444=CARTESIAN_POINT('Ctrl Pts',(-21.4726522764289,19.7035338774615,-44.0481226837284));
#72445=CARTESIAN_POINT('Ctrl Pts',(-19.1909125729949,23.2188579783477,-43.8492357723537));
#72446=CARTESIAN_POINT('Ctrl Pts',(-20.9150366805287,27.0387055761348,-43.6503488609786));
#72447=CARTESIAN_POINT('Ctrl Pts',(-25.0607007258249,27.6529605981239,-43.4514619496039));
#72448=CARTESIAN_POINT('Ctrl Pts',(-27.8183909456027,24.4971747593445,-43.2525750382288));
#72449=CARTESIAN_POINT('Ctrl Pts',(-26.6540238414595,20.4712476791197,-43.0536881268542));
#72450=CARTESIAN_POINT('Ctrl Pts',(-22.6375540600525,19.2746650018495,-42.854801215479));
#72451=CARTESIAN_POINT('Ctrl Pts',(-19.4597767900149,22.0069847544649,-42.6559143041044));
#72452=CARTESIAN_POINT('Ctrl Pts',(-20.0407999114304,26.1574367468242,-42.4570273927293));
#72453=CARTESIAN_POINT('Ctrl Pts',(-23.8467124383548,27.9121074982472,-42.2581404813545));
#72454=CARTESIAN_POINT('Ctrl Pts',(-27.3802034467131,25.6586033597219,-42.0592535699795));
#72455=CARTESIAN_POINT('Ctrl Pts',(-27.3942942904567,21.4677035689108,-41.8603666586047));
#72456=CARTESIAN_POINT('Ctrl Pts',(-23.8760366788917,19.1904897038634,-41.6614797472298));
#72457=CARTESIAN_POINT('Ctrl Pts',(-20.0584110579928,20.9195282306625,-41.4625928358549));
#72458=CARTESIAN_POINT('Ctrl Pts',(-19.4494916920911,25.0659793414713,-41.26370592448));
#72459=CARTESIAN_POINT('Ctrl Pts',(-22.6088238506017,27.8196060265358,-41.0648190131051));
#72460=CARTESIAN_POINT('Ctrl Pts',(-26.6332491470472,26.6500588313235,-40.8659321017303));
#72461=CARTESIAN_POINT('Ctrl Pts',(-27.8246619489901,22.6320524669849,-40.6670451903554));
#72462=CARTESIAN_POINT('Ctrl Pts',(-25.0882549065923,19.4577941115868,-40.4681582789804));
#72463=CARTESIAN_POINT('Ctrl Pts',(-20.9385540827603,20.0441580610137,-40.2692713676056));
#72464=CARTESIAN_POINT('Ctrl Pts',(-19.1887826979866,23.8523255612065,-40.0703844562306));
#72465=CARTESIAN_POINT('Ctrl Pts',(-21.4468322987298,27.3829135588469,-39.8714975448559));
#72466=CARTESIAN_POINT('Ctrl Pts',(-25.6377467529413,27.3916110286012,-39.6726106334809));
#72467=CARTESIAN_POINT('Ctrl Pts',(-27.9104310081496,23.8704257331889,-39.4737237221061));
#72468=CARTESIAN_POINT('Ctrl Pts',(-26.1764809256665,20.0550284118138,-39.2748368107311));
#72469=CARTESIAN_POINT('Ctrl Pts',(-22.0292496165711,19.4514457104732,-39.0759498993563));
#72470=CARTESIAN_POINT('Ctrl Pts',(-19.2796910266931,22.6143189563253,-38.8770629879813));
#72471=CARTESIAN_POINT('Ctrl Pts',(-20.4544163760059,26.6372358038602,-38.6781760766065));
#72472=CARTESIAN_POINT('Ctrl Pts',(-24.4739526687759,27.8234767572942,-38.4792891652316));
#72473=CARTESIAN_POINT('Ctrl Pts',(-27.6446868524243,25.0829869570684,-38.2804022538567));
#72474=CARTESIAN_POINT('Ctrl Pts',(-27.0529830461042,20.9340441743723,-38.0815153424818));
#72475=CARTESIAN_POINT('Ctrl Pts',(-23.2425668796141,19.189175054166,-37.8826284311069));
#72476=CARTESIAN_POINT('Ctrl Pts',(-19.7148877399443,21.451766377414,-37.683741519732));
#72477=CARTESIAN_POINT('Ctrl Pts',(-19.711583658584,25.6426885541605,-37.4848546083571));
#72478=CARTESIAN_POINT('Ctrl Pts',(-23.2356908061633,27.9108394355789,-37.2859676969822));
#72479=CARTESIAN_POINT('Ctrl Pts',(-27.0488535090693,26.1719806691275,-37.0870807856073));
#72480=CARTESIAN_POINT('Ctrl Pts',(-27.6470985462135,22.0239760302641,-36.8881938742324));
#72481=CARTESIAN_POINT('Ctrl Pts',(-24.4806894512747,19.278490089308,-36.6893069628576));
#72482=CARTESIAN_POINT('Ctrl Pts',(-20.459287715283,20.4583916471769,-36.4904200514827));
#72483=CARTESIAN_POINT('Ctrl Pts',(-19.2782205749742,24.4794512113442,-36.2915331401078));
#72484=CARTESIAN_POINT('Ctrl Pts',(-22.0227885943122,27.6466559719694,-36.0926462287329));
#72485=CARTESIAN_POINT('Ctrl Pts',(-26.1709664645193,27.0496132887177,-35.893759317358));
#72486=CARTESIAN_POINT('Ctrl Pts',(-27.9109304303589,23.2369547666261,-35.6948724059831));
#72487=CARTESIAN_POINT('Ctrl Pts',(-25.6438011318411,19.712190327362,-35.4959854946082));
#72488=CARTESIAN_POINT('Ctrl Pts',(-21.4528781734377,19.7142796398676,-35.2970985832333));
#72489=CARTESIAN_POINT('Ctrl Pts',(-19.1892644222517,23.2413028030948,-35.0982116718584));
#72490=CARTESIAN_POINT('Ctrl Pts',(-20.9330289928265,27.0522245722874,-34.8993247604835));
#72491=CARTESIAN_POINT('Ctrl Pts',(-25.0818000916583,27.6451309544398,-34.7004378491086));
#72492=CARTESIAN_POINT('Ctrl Pts',(-27.8232088367022,24.4751912545249,-34.5015509377338));
#72493=CARTESIAN_POINT('Ctrl Pts',(-26.6381330243943,20.4553112902,-34.3026640263588));
#72494=CARTESIAN_POINT('Ctrl Pts',(-22.6155568483864,19.2794199190639,-34.103777114984));
#72495=CARTESIAN_POINT('Ctrl Pts',(-19.4518867562131,22.028061612044,-33.9048902036091));
#72496=CARTESIAN_POINT('Ctrl Pts',(-20.0542673275921,26.1754676996755,-33.7060032922341));
#72497=CARTESIAN_POINT('Ctrl Pts',(-23.869161890876,27.9105236294732,-33.5071163808593));
#72498=CARTESIAN_POINT('Ctrl Pts',(-27.3910057921265,25.6388601104361,-33.3082294694844));
#72499=CARTESIAN_POINT('Ctrl Pts',(-27.3835230892152,21.4479433112553,-33.1093425581096));
#72500=CARTESIAN_POINT('Ctrl Pts',(-23.853589751689,19.1888704392302,-32.9104556467346));
#72501=CARTESIAN_POINT('Ctrl Pts',(-20.0449152277426,20.9375379259584,-32.7115687353598));
#72502=CARTESIAN_POINT('Ctrl Pts',(-19.4573484825355,25.0870686136899,-32.5126818239848));
#72503=CARTESIAN_POINT('Ctrl Pts',(-22.6308135374686,27.8243956225835,-32.31379491261));
#72504=CARTESIAN_POINT('Ctrl Pts',(-26.6491650725236,26.6341475185233,-32.1149080012351));
#72505=CARTESIAN_POINT('Ctrl Pts',(-27.8198787270113,22.6100613927433,-31.9160210898602));
#72506=CARTESIAN_POINT('Ctrl Pts',(-25.0671679126064,19.4499312085962,-31.7171341784853));
#72507=CARTESIAN_POINT('Ctrl Pts',(-20.9205404763582,20.0576486704582,-31.5182472671104));
#72508=CARTESIAN_POINT('Ctrl Pts',(-19.1903954561497,23.8747729568218,-31.3193603557355));
#72509=CARTESIAN_POINT('Ctrl Pts',(-21.4665894334457,27.3936904872877,-31.1204734443606));
#72510=CARTESIAN_POINT('Ctrl Pts',(-25.6574931325347,27.3808144063633,-30.9215865329857));
#72511=CARTESIAN_POINT('Ctrl Pts',(-27.9120213839913,23.8479767407064,-30.7226996216109));
#72512=CARTESIAN_POINT('Ctrl Pts',(-26.1584538771994,20.0415557698175,-30.5238127102359));
#72513=CARTESIAN_POINT('Ctrl Pts',(-22.008170472895,19.4593296346659,-30.3249257988611));
#72514=CARTESIAN_POINT('Ctrl Pts',(-19.2749297336295,22.6363147888206,-30.1260388874862));
#72515=CARTESIAN_POINT('Ctrl Pts',(-20.4703481581894,26.653131239534,-29.9271519761113));
#72516=CARTESIAN_POINT('Ctrl Pts',(-24.4959375691721,27.8186652384729,-29.7282650647364));
#72517=CARTESIAN_POINT('Ctrl Pts',(-27.6525226115814,25.0618898615992,-29.5293781533615));
#72518=CARTESIAN_POINT('Ctrl Pts',(-27.0394692657196,20.9160479442529,-29.3304912419866));
#72519=CARTESIAN_POINT('Ctrl Pts',(-23.2201215780816,19.1908166990471,-29.1316043306117));
#72520=CARTESIAN_POINT('Ctrl Pts',(-19.7041362463246,21.4715373648386,-28.9327174192368));
#72521=CARTESIAN_POINT('Ctrl Pts',(-19.7224056839372,25.6624210229886,-28.7338305078619));
#72522=CARTESIAN_POINT('Ctrl Pts',(-23.2581418267462,27.9124009199948,-28.5349435964871));
#72523=CARTESIAN_POINT('Ctrl Pts',(-27.0623029404989,26.1539362973452,-28.3360566851121));
#72524=CARTESIAN_POINT('Ctrl Pts',(-27.6391875013296,22.0029070500411,-28.1371697737373));
#72525=CARTESIAN_POINT('Ctrl Pts',(-24.4586875095798,19.2737571071142,-27.9382828623624));
#72526=CARTESIAN_POINT('Ctrl Pts',(-20.4434127957375,20.4743438723577,-27.7393959509875));
#72527=CARTESIAN_POINT('Ctrl Pts',(-19.2830603826693,24.5014299014843,-27.5405090396126));
#72528=CARTESIAN_POINT('Ctrl Pts',(-22.0438957563241,27.6544645743154,-27.3416221282377));
#72529=CARTESIAN_POINT('Ctrl Pts',(-26.1889452885512,27.0360763597742,-27.1427352168628));
#72530=CARTESIAN_POINT('Ctrl Pts',(-27.9092599014785,23.2145115963496,-26.9438483054879));
#72531=CARTESIAN_POINT('Ctrl Pts',(-25.6240163244518,19.7014642863698,-26.744961394113));
#72532=CARTESIAN_POINT('Ctrl Pts',(-21.4331596480554,19.7251270504131,-26.5460744827382));
#72533=CARTESIAN_POINT('Ctrl Pts',(-19.1877318318474,23.2637558145954,-26.3471875713632));
#72534=CARTESIAN_POINT('Ctrl Pts',(-20.9510906580395,27.0656507708756,-26.1483006599883));
#72535=CARTESIAN_POINT('Ctrl Pts',(-25.1028588735346,27.6371928019669,-25.9494137486134));
#72536=CARTESIAN_POINT('Ctrl Pts',(-27.8279135001877,24.4531832400693,-25.7505268372386));
#72537=CARTESIAN_POINT('Ctrl Pts',(-26.6221603826357,20.4394569130743,-25.5516399258637));
#72538=CARTESIAN_POINT('Ctrl Pts',(-22.593584404903,19.2842880076173,-25.3527530144888));
#72539=CARTESIAN_POINT('Ctrl Pts',(-19.4441053236104,22.0491788056415,-25.1538661031139));
#72540=CARTESIAN_POINT('Ctrl Pts',(-20.0678273826751,26.193429087844,-24.954979191739));
#72541=CARTESIAN_POINT('Ctrl Pts',(-23.8916028927267,27.9088242193601,-24.7560922803641));
#72542=CARTESIAN_POINT('Ctrl Pts',(-27.4017063627272,25.6190615158492,-24.5572053689893));
#72543=CARTESIAN_POINT('Ctrl Pts',(-27.3726503114427,21.428238761976,-24.3583184576143));
#72544=CARTESIAN_POINT('Ctrl Pts',(-23.8311347864567,19.1873667453757,-24.1594315462395));
#72545=CARTESIAN_POINT('Ctrl Pts',(-20.0315122842318,20.9556168546889,-23.9605446348646));
#72546=CARTESIAN_POINT('Ctrl Pts',(-19.4653137294506,25.1081171623423,-23.7616577234897));
#72547=CARTESIAN_POINT('Ctrl Pts',(-22.6528275882359,27.8290719595691,-23.5627708121148));
#72548=CARTESIAN_POINT('Ctrl Pts',(-26.6649988809719,26.6181544866401,-23.3638839007399));
#72549=CARTESIAN_POINT('Ctrl Pts',(-27.814982365662,22.5880952323066,-23.164996989365));
#72550=CARTESIAN_POINT('Ctrl Pts',(-25.0460407223967,19.4421769586241,-22.9661100779901));
#72551=CARTESIAN_POINT('Ctrl Pts',(-20.9025965538004,20.0712318292229,-22.7672231666153));
#72552=CARTESIAN_POINT('Ctrl Pts',(-19.1921237446807,23.8972117530806,-22.5683362552403));
#72553=CARTESIAN_POINT('Ctrl Pts',(-21.4864017824403,27.4043655697748,-22.3694493438655));
#72554=CARTESIAN_POINT('Ctrl Pts',(-25.6771836730771,27.369916279371,-22.1705624324905));
#72555=CARTESIAN_POINT('Ctrl Pts',(-27.9134961788053,23.8255198589316,-21.9716755211157));
#72556=CARTESIAN_POINT('Ctrl Pts',(-26.1403577148932,20.0281761035817,-21.7727886097408));
#72557=CARTESIAN_POINT('Ctrl Pts',(-21.9871321923262,19.4673219628314,-21.5739016983659));
#72558=CARTESIAN_POINT('Ctrl Pts',(-19.2702817308889,22.6583348394408,-21.375014786991));
#72559=CARTESIAN_POINT('Ctrl Pts',(-20.4863615537098,26.6689444530814,-21.1761278756161));
#72560=CARTESIAN_POINT('Ctrl Pts',(-24.5178974101823,27.8137406124369,-20.9772409642412));
#72561=CARTESIAN_POINT('Ctrl Pts',(-27.6602496660805,25.0407527097676,-20.7783540528663));
#72562=CARTESIAN_POINT('Ctrl Pts',(-27.025863025769,20.8981215170238,-20.5794671414914));
#72563=CARTESIAN_POINT('Ctrl Pts',(-23.1976850245772,19.1925738631339,-20.3805802301165));
#72564=CARTESIAN_POINT('Ctrl Pts',(-19.6934866696307,21.4913634354284,-20.1816933187417));
#72565=CARTESIAN_POINT('Ctrl Pts',(-19.7333291421004,25.682097522183,-19.9828064073668));
#72566=CARTESIAN_POINT('Ctrl Pts',(-23.2806005878712,27.9138468133262,-19.7839194959919));
#72567=CARTESIAN_POINT('Ctrl Pts',(-27.0756593073007,26.1358229314335,-19.585032584617));
#72568=CARTESIAN_POINT('Ctrl Pts',(-27.6311681051505,21.981879072399,-19.3861456732421));
#72569=CARTESIAN_POINT('Ctrl Pts',(-24.4366614955757,19.2691374463162,-19.1872587618672));
#72570=CARTESIAN_POINT('Ctrl Pts',(-20.4276202032802,20.4903776049946,-18.9883718504923));
#72571=CARTESIAN_POINT('Ctrl Pts',(-19.288013265236,24.523383386699,-18.7894849391174));
#72572=CARTESIAN_POINT('Ctrl Pts',(-22.0650428347712,27.6621644205442,-18.5905980277425));
#72573=CARTESIAN_POINT('Ctrl Pts',(-26.2068541907623,27.0224470611721,-18.3917111163676));
#72574=CARTESIAN_POINT('Ctrl Pts',(-27.9074738647463,23.1920773227581,-18.1928242049927));
#72575=CARTESIAN_POINT('Ctrl Pts',(-25.6041765651021,19.6908402331065,-17.9939372936179));
#72576=CARTESIAN_POINT('Ctrl Pts',(-21.4134972227966,19.7360758216561,-17.795050382243));
#72577=CARTESIAN_POINT('Ctrl Pts',(-19.1863148423934,23.2862164178749,-17.5961634708681));
#72578=CARTESIAN_POINT('Ctrl Pts',(-20.9692211975579,27.078983816123,-17.3972765594932));
#72579=CARTESIAN_POINT('Ctrl Pts',(-25.123876513424,27.6291463510555,-17.1983896481183));
#72580=CARTESIAN_POINT('Ctrl Pts',(-27.832504811392,24.4311512991602,-16.9995027367434));
#72581=CARTESIAN_POINT('Ctrl Pts',(-26.6061063394368,20.4236849678625,-16.8006158253685));
#72582=CARTESIAN_POINT('Ctrl Pts',(-22.5716373118425,19.2892691385119,-16.6017289139936));
#72583=CARTESIAN_POINT('Ctrl Pts',(-19.4364326984041,22.0703357756807,-16.4028420026187));
#72584=CARTESIAN_POINT('Ctrl Pts',(-20.0814797173563,26.211320435377,-16.2039550912438));
#72585=CARTESIAN_POINT('Ctrl Pts',(-23.9140348492504,27.9070093129403,-16.005068179869));
#72586=CARTESIAN_POINT('Ctrl Pts',(-27.4123048749644,25.5992081005977,-15.8061812684941));
#72587=CARTESIAN_POINT('Ctrl Pts',(-27.3616762452531,21.4085904432168,-15.6072943571192));
#72588=CARTESIAN_POINT('Ctrl Pts',(-23.808672378221,19.185978662146,-15.4084074457443));
#72589=CARTESIAN_POINT('Ctrl Pts',(-20.0182025826206,20.9737645377867,-15.2095205343694));
#72590=CARTESIAN_POINT('Ctrl Pts',(-19.4733872217679,25.1291244296706,-15.0106336229945));
#72591=CARTESIAN_POINT('Ctrl Pts',(-22.6748654195614,27.8336349135756,-14.8117467116196));
#72592=CARTESIAN_POINT('Ctrl Pts',(-26.6807501528174,26.6020801594677,-14.6128598002447));
#72593=CARTESIAN_POINT('Ctrl Pts',(-27.8099729946892,22.5661545677486,-14.4139728888698));
#72594=CARTESIAN_POINT('Ctrl Pts',(-25.0248738958048,19.4345315671475,-14.2150859774949));
#72595=CARTESIAN_POINT('Ctrl Pts',(-20.8847227905765,20.0849071773727,-14.01619906612));
#72596=CARTESIAN_POINT('Ctrl Pts',(-19.1939675177824,23.9196413553853,-13.8173121547452));
#72597=CARTESIAN_POINT('Ctrl Pts',(-21.5062688207131,27.4149385234332,-13.6184252433703));
#72598=CARTESIAN_POINT('Ctrl Pts',(-25.6968178527955,27.3589169364095,-13.4195383319954));
#72599=CARTESIAN_POINT('Ctrl Pts',(-27.9148553535118,23.8030556829416,-13.2206514206205));
#72600=CARTESIAN_POINT('Ctrl Pts',(-26.1221929182718,20.0148897676498,-13.0217645092456));
#72601=CARTESIAN_POINT('Ctrl Pts',(-21.9661353323509,19.4754224831835,-12.8228775978707));
#72602=CARTESIAN_POINT('Ctrl Pts',(-19.2657471416371,22.6803785246842,-12.6239906864958));
#72603=CARTESIAN_POINT('Ctrl Pts',(-20.5024561382339,26.6846750254737,-12.4251037751209));
#72604=CARTESIAN_POINT('Ctrl Pts',(-24.5398316099007,27.8087030096821,-12.226216863746));
#72605=CARTESIAN_POINT('Ctrl Pts',(-27.6678678111651,25.019576061679,-12.0273299523711));
#72606=CARTESIAN_POINT('Ctrl Pts',(-27.0121646867995,20.8802653677112,-11.8284430409963));
#72607=CARTESIAN_POINT('Ctrl Pts',(-23.1752578136387,19.1944464998637,-11.6295561296213));
#72608=CARTESIAN_POINT('Ctrl Pts',(-19.682939292062,21.5112440638194,-11.4306692182465));
#72609=CARTESIAN_POINT('Ctrl Pts',(-19.7443537436168,25.701717530343,-11.2317823068716));
#72610=CARTESIAN_POINT('Ctrl Pts',(-23.3030664944112,27.9151770772588,-11.0328953954967));
#72611=CARTESIAN_POINT('Ctrl Pts',(-27.0889222555488,26.1176410513722,-10.8340084841218));
#72612=CARTESIAN_POINT('Ctrl Pts',(-27.6230405701793,21.9608926545511,-10.6351215727469));
#72613=CARTESIAN_POINT('Ctrl Pts',(-24.4146119929223,19.264631229329,-10.436234661372));
#72614=CARTESIAN_POINT('Ctrl Pts',(-20.4119103563936,20.5064924202153,-10.2373477499971));
#72615=CARTESIAN_POINT('Ctrl Pts',(-19.2930790914296,24.5453110852506,-10.0384608386222));
#72616=CARTESIAN_POINT('Ctrl Pts',(-22.0862292692843,27.6697553066202,-9.83957392724733));
#72617=CARTESIAN_POINT('Ctrl Pts',(-26.2246926965909,27.0087257540695,-9.64068701587243));
#72618=CARTESIAN_POINT('Ctrl Pts',(-27.9055723674896,23.1696525403292,-9.44180010449755));
#72619=CARTESIAN_POINT('Ctrl Pts',(-25.5842823795188,19.6803184490956,-9.24291319312266));
#72620=CARTESIAN_POINT('Ctrl Pts',(-21.3938914186887,19.7471256634687,-9.04402628174778));
#72621=CARTESIAN_POINT('Ctrl Pts',(-19.1850134914383,23.3086840177575,-8.84513937037286));
#72622=CARTESIAN_POINT('Ctrl Pts',(-20.9874201309466,27.0922233547217,-8.64625245899801));
#72623=CARTESIAN_POINT('Ctrl Pts',(-25.1448524543876,27.6209918149259,-8.44736554762308));
#72624=CARTESIAN_POINT('Ctrl Pts',(-27.8369826486513,24.4090960156147,-8.24847863624822));
#72625=CARTESIAN_POINT('Ctrl Pts',(-26.5899713202086,20.4079958724997,-8.0495917248733));
#72626=CARTESIAN_POINT('Ctrl Pts',(-22.5497161507734,19.2943631797545,-7.85070481349842));
#72627=CARTESIAN_POINT('Ctrl Pts',(-19.4288690839087,22.0915319615302,-7.65181790212353));
#72628=CARTESIAN_POINT('Ctrl Pts',(-20.0952239698672,26.2291412681779,-7.45293099074865));
#72629=CARTESIAN_POINT('Ctrl Pts',(-23.9364571660305,27.905078958306,-7.25404407937375));
#72630=CARTESIAN_POINT('Ctrl Pts',(-27.4228010479919,25.5793003907701,-7.05515716799886));
#72631=CARTESIAN_POINT('Ctrl Pts',(-27.3506011814443,21.388998875632,-6.85627025662397));
#72632=CARTESIAN_POINT('Ctrl Pts',(-23.7862031222059,19.1847062263234,-6.65738334524908));
#72633=CARTESIAN_POINT('Ctrl Pts',(-20.0049864755982,20.9919804943623,-6.45849643387418));
#72634=CARTESIAN_POINT('Ctrl Pts',(-19.4815687455506,25.1500898590101,-6.25960952249932));
#72635=CARTESIAN_POINT('Ctrl Pts',(-22.6969264474718,27.838084363691,-6.0607226111244));
#72636=CARTESIAN_POINT('Ctrl Pts',(-26.6964184706725,26.5859249629543,-5.86183569974952));
#72637=CARTESIAN_POINT('Ctrl Pts',(-27.8048507468344,22.5442399804672,-5.66294878837463));
#72638=CARTESIAN_POINT('Ctrl Pts',(-25.0036679937236,19.4269952367594,-5.46406187699974));
#72639=CARTESIAN_POINT('Ctrl Pts',(-20.8669196603177,20.0986743525289,-5.26517496562485));
#72640=CARTESIAN_POINT('Ctrl Pts',(-19.1959267265971,23.9420611693814,-5.06628805424996));
#72641=CARTESIAN_POINT('Ctrl Pts',(-21.5261900218144,27.4254090680936,-4.86740114287507));
#72642=CARTESIAN_POINT('Ctrl Pts',(-25.7163951514103,27.347816668947,-4.66851423150017));
#72643=CARTESIAN_POINT('Ctrl Pts',(-27.9160988720948,23.7805848080068,-4.46962732012529));
#72644=CARTESIAN_POINT('Ctrl Pts',(-26.1039599686777,20.0016971140919,-4.27074040875039));
#72645=CARTESIAN_POINT('Ctrl Pts',(-21.9451804493579,19.4836309810696,-4.07185349737551));
#72646=CARTESIAN_POINT('Ctrl Pts',(-19.2613260860344,22.7024452604228,-3.87296658600062));
#72647=CARTESIAN_POINT('Ctrl Pts',(-20.518631485277,26.7003225398718,-3.67407967462572));
#72648=CARTESIAN_POINT('Ctrl Pts',(-24.5617395870999,27.8035525636983,-3.47519276325084));
#72649=CARTESIAN_POINT('Ctrl Pts',(-27.6753768449648,24.9983604784866,-3.27630585187594));
#72650=CARTESIAN_POINT('Ctrl Pts',(-26.9983746117987,20.8624799694792,-3.07741894050105));
#72651=CARTESIAN_POINT('Ctrl Pts',(-23.1528405395576,19.1964345596142,-2.87853202912616));
#72652=CARTESIAN_POINT('Ctrl Pts',(-19.6724943931097,21.5311787232013,-2.67964511775127));
#72653=CARTESIAN_POINT('Ctrl Pts',(-19.755479196349,25.7212805275649,-2.48075820637638));
#72654=CARTESIAN_POINT('Ctrl Pts',(-23.3255389510499,27.9163916765421,-2.28187129500149));
#72655=CARTESIAN_POINT('Ctrl Pts',(-27.102091433793,26.0993911389568,-2.0829843836266));
#72656=CARTESIAN_POINT('Ctrl Pts',(-27.6148051117849,21.9399483526093,-1.88409747225172));
#72657=CARTESIAN_POINT('Ctrl Pts',(-24.3925395859019,19.2602385755614,-1.68521056087682));
#72658=CARTESIAN_POINT('Ctrl Pts',(-20.3962836713676,20.5226878909986,-1.48632364950193));
#72659=CARTESIAN_POINT('Ctrl Pts',(-19.2982577270124,24.5672124160846,-1.28743673812705));
#72660=CARTESIAN_POINT('Ctrl Pts',(-22.1074544984513,27.677237031395,-1.08854982675215));
#72661=CARTESIAN_POINT('Ctrl Pts',(-26.2424603333401,26.9949128020628,-0.88966291537726));
#72662=CARTESIAN_POINT('Ctrl Pts',(-27.9035554600959,23.14723784329,-0.690776004002363));
#72663=CARTESIAN_POINT('Ctrl Pts',(-25.5643342948712,19.6698992131499,-0.491889092627479));
#72664=CARTESIAN_POINT('Ctrl Pts',(-21.3743427552598,19.7582762830453,-0.293002181252585));
#72665=CARTESIAN_POINT('Ctrl Pts',(-19.1838278134659,23.331158018882,-0.0941152698776977));
#72666=CARTESIAN_POINT('Ctrl Pts',(-21.0056869759584,27.1053690358419,0.104771641497192));
#72667=CARTESIAN_POINT('Ctrl Pts',(-25.1657861405909,27.6127294096622,0.303658552872082));
#72668=CARTESIAN_POINT('Ctrl Pts',(-27.8413468933091,24.3870179738681,0.502545464246976));
#72669=CARTESIAN_POINT('Ctrl Pts',(-26.5737557525075,20.392390042726,0.701432375621864));
#72670=CARTESIAN_POINT('Ctrl Pts',(-22.5278215025772,19.2995699963595,0.900319286996756));
#72671=CARTESIAN_POINT('Ctrl Pts',(-19.4214146805498,22.1127668015191,1.09920619837165));
#72672=CARTESIAN_POINT('Ctrl Pts',(-20.1090597760031,26.2468911140184,1.29809310974654));
#72673=CARTESIAN_POINT('Ctrl Pts',(-23.9588692489054,27.9030332066094,1.49698002112143));
#72674=CARTESIAN_POINT('Ctrl Pts',(-27.4331946036748,25.5593389138944,1.69586693249632));
#72675=CARTESIAN_POINT('Ctrl Pts',(-27.3394254134909,21.3694645783718,1.89475384387121));
#72676=CARTESIAN_POINT('Ctrl Pts',(-23.7637276138164,19.1835494716255,2.0936407552461));
#72677=CARTESIAN_POINT('Ctrl Pts',(-19.9918643133737,21.0102642417176,2.292527666621));
#72678=CARTESIAN_POINT('Ctrl Pts',(-19.4898580839996,25.1710128948049,2.49141457799587));
#72679=CARTESIAN_POINT('Ctrl Pts',(-22.7190100873796,27.8424201920111,2.69030148937078));
#72680=CARTESIAN_POINT('Ctrl Pts',(-26.7120034193478,26.5696893251909,2.88918840074566));
#72681=CARTESIAN_POINT('Ctrl Pts',(-27.7996157578303,22.5223520511699,3.08807531212054));
#72682=CARTESIAN_POINT('Ctrl Pts',(-24.9824235780812,19.4195681671619,3.28696222349545));
#72683=CARTESIAN_POINT('Ctrl Pts',(-20.8491876347826,20.1125329898798,3.48584913487033));
#72684=CARTESIAN_POINT('Ctrl Pts',(-19.1980013192086,23.9644706009737,3.68473604624521));
#72685=CARTESIAN_POINT('Ctrl Pts',(-21.5461648578586,27.4357769263005,3.88362295762013));
#72686=CARTESIAN_POINT('Ctrl Pts',(-25.7359150501498,27.3366157711258,4.082509868995));
#72687=CARTESIAN_POINT('Ctrl Pts',(-27.9172267016021,23.7581078295755,4.2813967803699));
#72688=CARTESIAN_POINT('Ctrl Pts',(-26.0856593492601,19.9885984924956,4.48028369174478));
#72689=CARTESIAN_POINT('Ctrl Pts',(-21.9242680986235,19.4919472389751,4.67917060311969));
#72690=CARTESIAN_POINT('Ctrl Pts',(-19.2570186812331,22.7245344619175,4.87805751449454));
#72691=CARTESIAN_POINT('Ctrl Pts',(-20.5348871662136,26.7158865816374,5.07694442586947));
#72692=CARTESIAN_POINT('Ctrl Pts',(-24.5836207612481,27.7982894109654,5.27583133724435));
#72693=CARTESIAN_POINT('Ctrl Pts',(-27.6827765685001,24.9771065223749,5.47471824861922));
#72694=CARTESIAN_POINT('Ctrl Pts',(-26.9844931661851,20.8447657936171,5.67360515999414));
#72695=CARTESIAN_POINT('Ctrl Pts',(-23.1304337963616,19.1985379897045,5.87249207136902));
#72696=CARTESIAN_POINT('Ctrl Pts',(-19.6621522495498,21.5511668853325,6.0713789827439));
#72697=CARTESIAN_POINT('Ctrl Pts',(-19.7667052054878,25.7407859954551,6.2702658941188));
#72698=CARTESIAN_POINT('Ctrl Pts',(-23.3480173622973,27.9174905789912,6.46915280549369));
#72699=CARTESIAN_POINT('Ctrl Pts',(-27.1151664930678,26.0810736777856,6.66803971686857));
#72700=CARTESIAN_POINT('Ctrl Pts',(-27.6064619481956,21.9190467215694,6.86692662824348));
#72701=CARTESIAN_POINT('Ctrl Pts',(-24.3704448594037,19.2559596014127,7.06581353961836));
#72702=CARTESIAN_POINT('Ctrl Pts',(-20.3807405622883,20.5389635881862,7.26470045099325));
#72703=CARTESIAN_POINT('Ctrl Pts',(-19.3035490347575,24.5890867988448,7.46358736236814));
#72704=CARTESIAN_POINT('Ctrl Pts',(-22.128717959832,27.6846093966129,7.66247427374303));
#72705=CARTESIAN_POINT('Ctrl Pts',(-26.2601566301919,26.9810085711767,7.86136118511791));
#72706=CARTESIAN_POINT('Ctrl Pts',(-27.9014231960102,23.1248338255997,8.06024809649283));
#72707=CARTESIAN_POINT('Ctrl Pts',(-25.544332839757,19.6595828013654,8.2591350078677));
#72708=CARTESIAN_POINT('Ctrl Pts',(-21.3548517505231,19.769527384909,8.45802191924259));
#72709=CARTESIAN_POINT('Ctrl Pts',(-19.182757839895,23.3536378257174,8.65690883061749));
#72710=CARTESIAN_POINT('Ctrl Pts',(-21.0240212485464,27.1184205111404,8.85579574199238));
#72711=CARTESIAN_POINT('Ctrl Pts',(-25.1866770173191,27.6043593542072,9.05468265336725));
#72712=CARTESIAN_POINT('Ctrl Pts',(-27.8455974297187,24.3649177589591,9.25356956474216));
#72713=CARTESIAN_POINT('Ctrl Pts',(-26.557460066024,20.3768678920752,9.45245647611703));
#72714=CARTESIAN_POINT('Ctrl Pts',(-22.5059539474326,19.3048894503536,9.65134338749194));
#72715=CARTESIAN_POINT('Ctrl Pts',(-19.4140696858589,22.1340397329529,9.85023029886681));
#72716=CARTESIAN_POINT('Ctrl Pts',(-20.1229867691341,26.2645695025515,10.0491172102417));
#72717=CARTESIAN_POINT('Ctrl Pts',(-23.9812705039851,27.9008721120599,10.2480041216166));
#72718=CARTESIAN_POINT('Ctrl Pts',(-27.4434852665982,25.5393241989229,10.4468910329915));
#72719=CARTESIAN_POINT('Ctrl Pts',(-27.3281492375358,21.3499880690689,10.6457779443664));
#72720=CARTESIAN_POINT('Ctrl Pts',(-23.7412464486233,19.1825084287052,10.8446648557413));
#72721=CARTESIAN_POINT('Ctrl Pts',(-19.9788364436668,21.0286152953575,11.0435517671161));
#72722=CARTESIAN_POINT('Ctrl Pts',(-19.4982550174582,25.191892982623,11.242438678491));
#72723=CARTESIAN_POINT('Ctrl Pts',(-22.7411157540979,27.8466422836418,11.4413255898659));
#72724=CARTESIAN_POINT('Ctrl Pts',(-26.727504585863,26.5533736764001,11.6402125012408));
#72725=CARTESIAN_POINT('Ctrl Pts',(-27.7942681663972,22.5004913598574,11.8390994126157));
#72726=CARTESIAN_POINT('Ctrl Pts',(-24.9611412118258,19.4122505551629,12.0379863239906));
#72727=CARTESIAN_POINT('Ctrl Pts',(-20.8315271838466,20.1264827221902,12.2368732353655));
#72728=CARTESIAN_POINT('Ctrl Pts',(-19.2001912406427,23.9868690563425,12.4357601467404));
#72729=CARTESIAN_POINT('Ctrl Pts',(-21.5661927995398,27.4460418233196,12.6346470581153));
#72730=CARTESIAN_POINT('Ctrl Pts',(-25.7553770317623,27.3253145397543,12.8335339694901));
#72731=CARTESIAN_POINT('Ctrl Pts',(-27.918238812148,23.7356253432576,13.0324208808651));
#72732=CARTESIAN_POINT('Ctrl Pts',(-26.0672915449605,19.9755942499566,13.2313077922399));
#72733=CARTESIAN_POINT('Ctrl Pts',(-21.9033988342966,19.5003710365307,13.4301947036148));
#72734=CARTESIAN_POINT('Ctrl Pts',(-19.2528250413737,22.7466455438341,13.6290816149897));
#72735=CARTESIAN_POINT('Ctrl Pts',(-20.5512227502902,26.7313667383445,13.8279685263646));
#72736=CARTESIAN_POINT('Ctrl Pts',(-24.6054745525237,27.7929136909498,14.0268554377395));
#72737=CARTESIAN_POINT('Ctrl Pts',(-27.6900667856881,24.9558147565452,14.2257423491144));
#72738=CARTESIAN_POINT('Ctrl Pts',(-26.9705207177986,20.8271233095267,14.4246292604893));
#72739=CARTESIAN_POINT('Ctrl Pts',(-23.1080381777993,19.2007567343966,14.6235161718642));
#72740=CARTESIAN_POINT('Ctrl Pts',(-19.6519131354353,21.5712080205535,14.8224030832391));
#72741=CARTESIAN_POINT('Ctrl Pts',(-19.7780314735584,25.760233417145,15.0212899946139));
#72742=CARTESIAN_POINT('Ctrl Pts',(-23.3705011325054,27.9184737554865,15.2201769059889));
#72743=CARTESIAN_POINT('Ctrl Pts',(-27.1281470869014,26.0626891532467,15.4190638173638));
#72744=CARTESIAN_POINT('Ctrl Pts',(-27.5980113004945,21.898188315297,15.6179507287386));
#72745=CARTESIAN_POINT('Ctrl Pts',(-24.3483283989083,19.2517944202697,15.8168376401135));
#72746=CARTESIAN_POINT('Ctrl Pts',(-20.3652814410273,20.5553190804943,16.0157245514884));
#72747=CARTESIAN_POINT('Ctrl Pts',(-19.3089528744526,24.6109336538896,16.2146114628633));
#72748=CARTESIAN_POINT('Ctrl Pts',(-22.1500190899732,27.6918722069163,16.4134983742382));
#72749=CARTESIAN_POINT('Ctrl Pts',(-26.2777811182176,26.9670134298545,16.6123852856131));
#72750=CARTESIAN_POINT('Ctrl Pts',(-27.899175631735,23.1024410809349,16.811272196988));
#72751=CARTESIAN_POINT('Ctrl Pts',(-25.5242785441877,19.6493694871132,17.0101591083628));
#72752=CARTESIAN_POINT('Ctrl Pts',(-21.335418920964,19.7808786709211,17.2090460197378));
#72753=CARTESIAN_POINT('Ctrl Pts',(-19.1818035990787,23.3761228425789,17.4079329311126));
#72754=CARTESIAN_POINT('Ctrl Pts',(-21.0424224628768,27.1313774347708,17.6068198424875));
#72755=CARTESIAN_POINT('Ctrl Pts',(-25.2075245309924,27.5958818703561,17.8057067538624));
#72756=CARTESIAN_POINT('Ctrl Pts',(-27.8497341452466,24.3427959565135,18.0045936652373));
#72757=CARTESIAN_POINT('Ctrl Pts',(-26.5410846925722,20.3614298318631,18.2034805766122));
#72758=CARTESIAN_POINT('Ctrl Pts',(-22.4841140648005,19.3103214007783,18.4023674879871));
#72759=CARTESIAN_POINT('Ctrl Pts',(-19.4068342944688,22.1553501921275,18.601254399362));
#72760=CARTESIAN_POINT('Ctrl Pts',(-20.1370045802135,26.2821759653235,18.8001413107369));
#72761=CARTESIAN_POINT('Ctrl Pts',(-24.0036603376662,27.8985957319239,18.9990282221118));
#72762=CARTESIAN_POINT('Ctrl Pts',(-27.4536727640731,25.5192567762184,19.1979151334866));
#72763=CARTESIAN_POINT('Ctrl Pts',(-27.3167729523822,21.3305698638249,19.3968020448616));
#72764=CARTESIAN_POINT('Ctrl Pts',(-23.7187602223476,19.1815831251482,19.5956889562364));
#72765=CARTESIAN_POINT('Ctrl Pts',(-19.9659032116986,21.0470331690039,19.7945758676113));
#72766=CARTESIAN_POINT('Ctrl Pts',(-19.5067593234192,25.2127295691698,19.9934627789862));
#72767=CARTESIAN_POINT('Ctrl Pts',(-22.7632428618561,27.8507505267037,20.1923496903611));
#72768=CARTESIAN_POINT('Ctrl Pts',(-26.7429215594582,26.5369784489248,20.391236601736));
#72769=CARTESIAN_POINT('Ctrl Pts',(-27.7888081142389,22.4786584858086,20.5901235131109));
#72770=CARTESIAN_POINT('Ctrl Pts',(-24.9398214589118,19.4050425946691,20.7890104244858));
#72771=CARTESIAN_POINT('Ctrl Pts',(-20.8139387754876,20.1405231798108,20.9878973358607));
#72772=CARTESIAN_POINT('Ctrl Pts',(-19.2024964328697,24.0092559419588,21.1867842472355));
#72773=CARTESIAN_POINT('Ctrl Pts',(-21.586273316144,27.4562034871449,21.3856711586105));
#72774=CARTESIAN_POINT('Ctrl Pts',(-25.7747805805317,27.3139132743005,21.5845580699853));
#72775=CARTESIAN_POINT('Ctrl Pts',(-27.919135176913,23.7131379448084,21.7834449813602));
#72776=CARTESIAN_POINT('Ctrl Pts',(-26.0488570425013,19.9626847310703,21.9823318927351));
#72777=CARTESIAN_POINT('Ctrl Pts',(-21.8825732093851,19.5089021505166,22.18121880411));
#72778=CARTESIAN_POINT('Ctrl Pts',(-19.2487452775818,22.768777920259,22.3801057154849));
#72779=CARTESIAN_POINT('Ctrl Pts',(-20.5676378046356,26.746762599789,22.5789926268598));
#72780=CARTESIAN_POINT('Ctrl Pts',(-24.6273003818304,27.7874255461016,22.7778795382347));
#72781=CARTESIAN_POINT('Ctrl Pts',(-27.6972473033478,24.9344857451995,22.9767664496096));
#72782=CARTESIAN_POINT('Ctrl Pts',(-26.9564576368906,20.8095529847125,23.1756533609844));
#72783=CARTESIAN_POINT('Ctrl Pts',(-23.0856542773232,19.2030907348922,23.3745402723594));
#72784=CARTESIAN_POINT('Ctrl Pts',(-19.6417773220915,21.5913015978093,23.5734271837343));
#72785=CARTESIAN_POINT('Ctrl Pts',(-19.7894577004254,25.7796222772883,23.7723140951091));
#72786=CARTESIAN_POINT('Ctrl Pts',(-23.3929896658942,27.9193411800047,23.9712010064841));
#72787=CARTESIAN_POINT('Ctrl Pts',(-27.1410328713078,26.0442380524495,24.1700879178589));
#72788=CARTESIAN_POINT('Ctrl Pts',(-27.5894533926459,21.8773736866169,24.3689748292338));
#72789=CARTESIAN_POINT('Ctrl Pts',(-24.3261907904083,19.2477431423055,24.5678617406087));
#72790=CARTESIAN_POINT('Ctrl Pts',(-20.3499067173511,20.5717539348997,24.7667486519836));
#72791=CARTESIAN_POINT('Ctrl Pts',(-19.314469102675,24.6327524015971,24.9656355633585));
#72792=CARTESIAN_POINT('Ctrl Pts',(-22.1713573248539,27.6990252711903,25.1645224747334));
#72793=CARTESIAN_POINT('Ctrl Pts',(-26.2953333295803,26.9529277464185,25.3634093861082));
#72794=CARTESIAN_POINT('Ctrl Pts',(-27.8968128283606,23.080060207451,25.5622962974831));
#72795=CARTESIAN_POINT('Ctrl Pts',(-25.5041719366806,19.6392595320107,25.761183208858));
#72796=CARTESIAN_POINT('Ctrl Pts',(-21.316044786992,19.7923298573219,25.960070120233));
#72797=CARTESIAN_POINT('Ctrl Pts',(-19.1809651059832,23.398612441479,26.1589570316078));
#72798=CARTESIAN_POINT('Ctrl Pts',(-21.0608901508285,27.1442395241256,26.3578439429827));
#72799=CARTESIAN_POINT('Ctrl Pts',(-25.2283280923853,27.5872970680732,26.5567308543576));
#72800=CARTESIAN_POINT('Ctrl Pts',(-27.85375699975,24.320653369264,26.7556177657325));
#72801=CARTESIAN_POINT('Ctrl Pts',(-26.524629934895,20.3460758623164,26.9545046771074));
#72802=CARTESIAN_POINT('Ctrl Pts',(-22.4623026811071,19.3158664757075,27.1533915884823));
#72803=CARTESIAN_POINT('Ctrl Pts',(-19.399708230402,22.1766961566261,27.3522784998572));
#72804=CARTESIAN_POINT('Ctrl Pts',(-20.1511137209111,26.2997127882555,27.5511654112321));
#72805=CARTESIAN_POINT('Ctrl Pts',(-24.0260364891328,27.8961989293013,27.750052322607));
#72806=CARTESIAN_POINT('Ctrl Pts',(-27.4637599747539,25.4991469909509,27.9489392339819));
#72807=CARTESIAN_POINT('Ctrl Pts',(-27.3052909142717,21.3111919474789,28.1478261453567));
#72808=CARTESIAN_POINT('Ctrl Pts',(-23.6962807566228,19.1808085733704,28.3467130567316));
#72809=CARTESIAN_POINT('Ctrl Pts',(-19.9530437635938,21.0654513101587,28.5455999681065));
#72810=CARTESIAN_POINT('Ctrl Pts',(-19.5154108002811,25.2336468469387,28.7444868794814));
#72811=CARTESIAN_POINT('Ctrl Pts',(-22.7853152490305,27.854509256677,28.9433737908563));
#72812=CARTESIAN_POINT('Ctrl Pts',(-26.7583966519409,26.5209489557215,29.1422607022312));
#72813=CARTESIAN_POINT('Ctrl Pts',(-27.782966107073,22.456013156451,29.3411476136061));
#72814=CARTESIAN_POINT('Ctrl Pts',(-24.9189752763196,19.3995389604751,29.540034524981));
#72815=CARTESIAN_POINT('Ctrl Pts',(-20.7954488425069,20.151587834895,29.7389214363559));
#72816=CARTESIAN_POINT('Ctrl Pts',(-19.206841997626,24.0378700261007,29.9378083477307));
#72817=CARTESIAN_POINT('Ctrl Pts',(-20.8035465588388,26.3133894497781,30.0703996219807));
#72818=CARTESIAN_POINT('Ctrl Pts',(-21.9068279226878,26.8610413387076,30.1366952591057));
#72819=CARTESIAN_POINT('Ctrl Pts',(-21.5447307071333,20.7349338698167,-75.1351504332081));
#72820=CARTESIAN_POINT('Ctrl Pts',(-20.6058873997063,21.4036543954464,-75.0688106032636));
#72821=CARTESIAN_POINT('Ctrl Pts',(-19.4669883124013,23.7419128688188,-74.9361751361943));
#72822=CARTESIAN_POINT('Ctrl Pts',(-21.5093735067961,27.0961553314539,-74.7372440319998));
#72823=CARTESIAN_POINT('Ctrl Pts',(-25.4282714863658,27.1804579122132,-74.538357120625));
#72824=CARTESIAN_POINT('Ctrl Pts',(-27.6206045269464,23.9343746038397,-74.33947020925));
#72825=CARTESIAN_POINT('Ctrl Pts',(-26.0730651857951,20.332453394204,-74.1405832978753));
#72826=CARTESIAN_POINT('Ctrl Pts',(-22.2070441073339,19.6889287249836,-73.9416963865003));
#72827=CARTESIAN_POINT('Ctrl Pts',(-19.5754399103481,22.5928329886891,-73.7428094751254));
#72828=CARTESIAN_POINT('Ctrl Pts',(-20.5962867745515,26.3769483984124,-73.5439225637506));
#72829=CARTESIAN_POINT('Ctrl Pts',(-24.3316119952896,27.5633455521573,-73.3450356523755));
#72830=CARTESIAN_POINT('Ctrl Pts',(-27.3489159621601,25.0621693264582,-73.1461487410009));
#72831=CARTESIAN_POINT('Ctrl Pts',(-26.875579925032,21.1716068112945,-72.9472618296257));
#72832=CARTESIAN_POINT('Ctrl Pts',(-23.3465448625251,19.4668513729129,-72.7483749182512));
#72833=CARTESIAN_POINT('Ctrl Pts',(-20.0047025732559,21.5143777294443,-72.5494880068759));
#72834=CARTESIAN_POINT('Ctrl Pts',(-19.9209186544747,25.432709765515,-72.3506010955013));
#72835=CARTESIAN_POINT('Ctrl Pts',(-23.1721856084992,27.6212182579661,-72.1517141841263));
#72836=CARTESIAN_POINT('Ctrl Pts',(-26.7708636095538,26.0688570314354,-71.9528272727514));
#72837=CARTESIAN_POINT('Ctrl Pts',(-27.4100733050024,22.202110423209,-71.7539403613766));
#72838=CARTESIAN_POINT('Ctrl Pts',(-24.502434856255,19.5741928446358,-71.5550534500015));
#72839=CARTESIAN_POINT('Ctrl Pts',(-20.7198216424902,20.5999366146469,-71.3561665386268));
#72840=CARTESIAN_POINT('Ctrl Pts',(-19.5381344034245,24.3367707731949,-71.1572796272518));
#72841=CARTESIAN_POINT('Ctrl Pts',(-22.0432435694086,27.3508612442913,-70.9583927158769));
#72842=CARTESIAN_POINT('Ctrl Pts',(-25.9331661896048,26.8725146048559,-70.7595058045021));
#72843=CARTESIAN_POINT('Ctrl Pts',(-27.6333932006229,23.3412907709111,-70.5606188931271));
#72844=CARTESIAN_POINT('Ctrl Pts',(-25.581560127655,20.0020850943206,-70.3617319817523));
#72845=CARTESIAN_POINT('Ctrl Pts',(-21.6631276017948,19.9233444490922,-70.1628450703774));
#72846=CARTESIAN_POINT('Ctrl Pts',(-19.4788028840082,23.1774248252328,-69.9639581590025));
#72847=CARTESIAN_POINT('Ctrl Pts',(-21.0357951908098,26.774102250624,-69.7650712476277));
#72848=CARTESIAN_POINT('Ctrl Pts',(-24.9033606028634,27.4083351229759,-69.5661843362526));
#72849=CARTESIAN_POINT('Ctrl Pts',(-27.5275344222612,24.4973172047244,-69.3672974248779));
#72850=CARTESIAN_POINT('Ctrl Pts',(-26.4969234020677,20.7160271501586,-69.1684105135028));
#72851=CARTESIAN_POINT('Ctrl Pts',(-22.7585716885195,19.5391499183498,-68.9695236021282));
#72852=CARTESIAN_POINT('Ctrl Pts',(-19.7477075463674,22.0481359028861,-68.7706366907531));
#72853=CARTESIAN_POINT('Ctrl Pts',(-20.2310598430906,25.9374397107561,-68.5717497793784));
#72854=CARTESIAN_POINT('Ctrl Pts',(-23.7644687995049,27.6331209011918,-68.3728628680034));
#72855=CARTESIAN_POINT('Ctrl Pts',(-27.1010311683477,25.5769922301957,-68.1739759566284));
#72856=CARTESIAN_POINT('Ctrl Pts',(-27.1747290264866,21.6584616154734,-67.9750890452537));
#72857=CARTESIAN_POINT('Ctrl Pts',(-23.9178402908416,19.4783264553349,-67.7762021338787));
#72858=CARTESIAN_POINT('Ctrl Pts',(-20.3231695708421,21.0399461169747,-67.5773152225038));
#72859=CARTESIAN_POINT('Ctrl Pts',(-19.6939144803516,24.9083245348555,-67.3784283111289));
#72860=CARTESIAN_POINT('Ctrl Pts',(-22.6083070954968,27.5287499273489,-67.1795413997541));
#72861=CARTESIAN_POINT('Ctrl Pts',(-26.3882677027047,26.4932735341877,-66.9806544883791));
#72862=CARTESIAN_POINT('Ctrl Pts',(-27.5603329917596,22.753410366767,-66.7817675770043));
#72863=CARTESIAN_POINT('Ctrl Pts',(-25.0474743367688,19.7457775878401,-66.5828806656294));
#72864=CARTESIAN_POINT('Ctrl Pts',(-21.1587957863896,20.2341347160336,-66.3839937542544));
#72865=CARTESIAN_POINT('Ctrl Pts',(-19.4676632228503,23.769722956394,-66.1851068428796));
#72866=CARTESIAN_POINT('Ctrl Pts',(-21.5280840876475,27.1036364844786,-65.9862199315048));
#72867=CARTESIAN_POINT('Ctrl Pts',(-25.4467063009133,27.1722914372305,-65.7873330201298));
#72868=CARTESIAN_POINT('Ctrl Pts',(-27.6226482930303,23.9125997340508,-65.588446108755));
#72869=CARTESIAN_POINT('Ctrl Pts',(-26.0564038627002,20.3199416738818,-65.38955919738));
#72870=CARTESIAN_POINT('Ctrl Pts',(-22.1872188457677,19.6956654068475,-65.1906722860052));
#72871=CARTESIAN_POINT('Ctrl Pts',(-19.5705462200028,22.6134278924535,-64.9917853746302));
#72872=CARTESIAN_POINT('Ctrl Pts',(-20.6108862712309,26.392052791891,-64.7928984632553));
#72873=CARTESIAN_POINT('Ctrl Pts',(-24.3522546986636,27.5593041971357,-64.5940115518805));
#72874=CARTESIAN_POINT('Ctrl Pts',(-27.3566511332218,25.042577033367,-64.3951246405055));
#72875=CARTESIAN_POINT('Ctrl Pts',(-26.8632899823566,21.154530180813,-64.1962377291308));
#72876=CARTESIAN_POINT('Ctrl Pts',(-23.3255283135862,19.4679490449603,-63.9973508177557));
#72877=CARTESIAN_POINT('Ctrl Pts',(-19.9942691477852,21.5326586911586,-63.798463906381));
#72878=CARTESIAN_POINT('Ctrl Pts',(-19.930657214125,25.4513660130612,-63.5995769950059));
#72879=CARTESIAN_POINT('Ctrl Pts',(-23.1931464862368,27.6231112334295,-63.4006900836312));
#72880=CARTESIAN_POINT('Ctrl Pts',(-26.7837859365242,26.0522446283749,-63.2018031722561));
#72881=CARTESIAN_POINT('Ctrl Pts',(-27.4030823461947,22.1822594204177,-63.0029162608814));
#72882=CARTESIAN_POINT('Ctrl Pts',(-24.4819548224377,19.569343895035,-62.8040293495064));
#72883=CARTESIAN_POINT('Ctrl Pts',(-20.7046718888146,20.6145458813503,-62.6051424381316));
#72884=CARTESIAN_POINT('Ctrl Pts',(-19.5422363005461,24.3574133724544,-62.4062555267567));
#72885=CARTESIAN_POINT('Ctrl Pts',(-22.0628278049658,27.3585684868534,-62.2073686153818));
#72886=CARTESIAN_POINT('Ctrl Pts',(-25.9502365204291,26.8602041304068,-62.0084817040069));
#72887=CARTESIAN_POINT('Ctrl Pts',(-27.632263435331,23.3202748923593,-61.809594792632));
#72888=CARTESIAN_POINT('Ctrl Pts',(-25.563268427241,19.9916756059724,-61.6107078812572));
#72889=CARTESIAN_POINT('Ctrl Pts',(-21.6444824867456,19.9331067967561,-61.4118209698822));
#72890=CARTESIAN_POINT('Ctrl Pts',(-19.4769376349045,23.1983882345641,-61.2129340585074));
#72891=CARTESIAN_POINT('Ctrl Pts',(-21.0524238130624,26.787003128262,-61.0140471471324));
#72892=CARTESIAN_POINT('Ctrl Pts',(-24.923202802692,27.4013186549087,-60.8151602357575));
#72893=CARTESIAN_POINT('Ctrl Pts',(-27.5323569002611,24.4768309308833,-60.6162733243827));
#72894=CARTESIAN_POINT('Ctrl Pts',(-26.4822947098904,20.7008962188961,-60.4173864130077));
#72895=CARTESIAN_POINT('Ctrl Pts',(-22.7379343539384,19.5432783727942,-60.2184995016329));
#72896=CARTESIAN_POINT('Ctrl Pts',(-19.7400255301204,22.0677300433379,-60.019612590258));
#72897=CARTESIAN_POINT('Ctrl Pts',(-20.243392266773,25.9544941835025,-59.8207256788831));
#72898=CARTESIAN_POINT('Ctrl Pts',(-23.7854832113739,27.6319640917314,-59.6218387675081));
#72899=CARTESIAN_POINT('Ctrl Pts',(-27.1114171056218,25.5586871483564,-59.4229518561334));
#72900=CARTESIAN_POINT('Ctrl Pts',(-27.1649426933942,21.6398290794425,-59.2240649447584));
#72901=CARTESIAN_POINT('Ctrl Pts',(-23.8968744977499,19.4764881859506,-59.0251780333836));
#72902=CARTESIAN_POINT('Ctrl Pts',(-20.3102901039966,21.0565913279393,-58.8262911220085));
#72903=CARTESIAN_POINT('Ctrl Pts',(-19.7009564777843,24.9281576885748,-58.6274042106338));
#72904=CARTESIAN_POINT('Ctrl Pts',(-22.6287995586302,27.5335460371286,-58.4285172992588));
#72905=CARTESIAN_POINT('Ctrl Pts',(-26.4033797953935,26.4786253817834,-58.229630387884));
#72906=CARTESIAN_POINT('Ctrl Pts',(-27.5561779821169,22.7327783622798,-58.030743476509));
#72907=CARTESIAN_POINT('Ctrl Pts',(-25.0278703263696,19.7381207940882,-57.8318565651343));
#72908=CARTESIAN_POINT('Ctrl Pts',(-21.1417571986447,20.2464890772859,-57.6329696537593));
#72909=CARTESIAN_POINT('Ctrl Pts',(-19.4688470752633,23.7907358621368,-57.4340827423844));
#72910=CARTESIAN_POINT('Ctrl Pts',(-21.546402520225,27.1139988559349,-57.2351958310095));
#72911=CARTESIAN_POINT('Ctrl Pts',(-25.4653262272634,27.1624811336161,-57.0363089196346));
#72912=CARTESIAN_POINT('Ctrl Pts',(-27.6244595795468,23.8916315926108,-56.8374220082598));
#72913=CARTESIAN_POINT('Ctrl Pts',(-26.0397420906462,20.3070836387943,-56.6385350968848));
#72914=CARTESIAN_POINT('Ctrl Pts',(-22.1673947709755,19.7027329221764,-56.43964818551));
#72915=CARTESIAN_POINT('Ctrl Pts',(-19.5657764864021,22.633926510838,-56.240761274135));
#72916=CARTESIAN_POINT('Ctrl Pts',(-20.6255538595941,26.4071460210318,-56.0418743627602));
#72917=CARTESIAN_POINT('Ctrl Pts',(-24.3728813388913,27.5551226391475,-55.8429874513852));
#72918=CARTESIAN_POINT('Ctrl Pts',(-27.3642826917954,25.022963185503,-55.6441005400104));
#72919=CARTESIAN_POINT('Ctrl Pts',(-26.8509137039966,21.1375075062804,-55.4452136286355));
#72920=CARTESIAN_POINT('Ctrl Pts',(-23.3045169487698,19.4691599383696,-55.2463267172607));
#72921=CARTESIAN_POINT('Ctrl Pts',(-19.9839303593089,21.5509904441336,-55.0474398058857));
#72922=CARTESIAN_POINT('Ctrl Pts',(-19.9404914720138,25.4699732988941,-54.8485528945108));
#72923=CARTESIAN_POINT('Ctrl Pts',(-23.2141169412984,27.6248955340777,-54.649665983136));
#72924=CARTESIAN_POINT('Ctrl Pts',(-26.7966225185585,26.0355663228262,-54.450779071761));
#72925=CARTESIAN_POINT('Ctrl Pts',(-27.3959893246748,22.1624444573844,-54.2518921603862));
#72926=CARTESIAN_POINT('Ctrl Pts',(-24.4614500827513,19.5646005455128,-54.0530052490112));
#72927=CARTESIAN_POINT('Ctrl Pts',(-20.6895975482185,20.6292328813803,-53.8541183376364));
#72928=CARTESIAN_POINT('Ctrl Pts',(-19.5464443999544,24.3780346142614,-53.6552314262614));
#72929=CARTESIAN_POINT('Ctrl Pts',(-22.0824514578106,27.3661747976098,-53.4563445148867));
#72930=CARTESIAN_POINT('Ctrl Pts',(-25.9672432535572,26.8478059554361,-53.2574576035116));
#72931=CARTESIAN_POINT('Ctrl Pts',(-27.6310255029309,23.2992651032679,-53.0585706921369));
#72932=CARTESIAN_POINT('Ctrl Pts',(-25.5449233842291,19.9813604175989,-52.8596837807619));
#72933=CARTESIAN_POINT('Ctrl Pts',(-21.6258878722466,19.9429649926319,-52.660796869387));
#72934=CARTESIAN_POINT('Ctrl Pts',(-19.4751803230796,23.2193609685167,-52.4619099580122));
#72935=CARTESIAN_POINT('Ctrl Pts',(-21.0691186244834,26.7998182359834,-52.2630230466372));
#72936=CARTESIAN_POINT('Ctrl Pts',(-24.9430086211493,27.3942001389451,-52.0641361352625));
#72937=CARTESIAN_POINT('Ctrl Pts',(-27.5370738578491,24.4563201038546,-51.8652492238873));
#72938=CARTESIAN_POINT('Ctrl Pts',(-26.4675883225176,20.6858407918102,-51.6663623125127));
#72939=CARTESIAN_POINT('Ctrl Pts',(-22.7173185447046,19.5475130066537,-51.4674754011376));
#72940=CARTESIAN_POINT('Ctrl Pts',(-19.732444479779,22.0873634686633,-51.2685884897629));
#72941=CARTESIAN_POINT('Ctrl Pts',(-20.2558123178206,25.9714849470598,-51.0697015783878));
#72942=CARTESIAN_POINT('Ctrl Pts',(-23.8064913899446,27.6306991223907,-50.8708146670131));
#72943=CARTESIAN_POINT('Ctrl Pts',(-27.1217086768087,25.5403288456899,-50.6719277556381));
#72944=CARTESIAN_POINT('Ctrl Pts',(-27.1550605758581,21.6212471670735,-50.4730408442632));
#72945=CARTESIAN_POINT('Ctrl Pts',(-23.8758995196408,19.4747578658597,-50.2741539328884));
#72946=CARTESIAN_POINT('Ctrl Pts',(-20.2974964918121,21.0733026175832,-50.0752670215135));
#72947=CARTESIAN_POINT('Ctrl Pts',(-19.7081004764024,24.9479543296544,-49.8763801101385));
#72948=CARTESIAN_POINT('Ctrl Pts',(-22.6493164390321,27.5382365949702,-49.6774931987637));
#72949=CARTESIAN_POINT('Ctrl Pts',(-26.4184162840345,26.4638996314242,-49.4786062873887));
#72950=CARTESIAN_POINT('Ctrl Pts',(-27.5519168208199,22.7121680197622,-49.2797193760139));
#72951=CARTESIAN_POINT('Ctrl Pts',(-25.0082271610796,19.730565016717,-49.0808324646389));
#72952=CARTESIAN_POINT('Ctrl Pts',(-21.1247824327975,20.258930983841,-48.8819455532642));
#72953=CARTESIAN_POINT('Ctrl Pts',(-19.4701390794497,23.8117423953937,-48.6830586418892));
#72954=CARTESIAN_POINT('Ctrl Pts',(-21.5647740521415,27.1242667928908,-48.4841717305144));
#72955=CARTESIAN_POINT('Ctrl Pts',(-25.4838954067279,27.1525751107861,-48.2852848191394));
#72956=CARTESIAN_POINT('Ctrl Pts',(-27.6261629050381,23.8706544050833,-48.0863979077646));
#72957=CARTESIAN_POINT('Ctrl Pts',(-26.023014350456,20.294311543335,-47.8875109963896));
#72958=CARTESIAN_POINT('Ctrl Pts',(-22.1476073400601,19.709902391617,-47.6886240850148));
#72959=CARTESIAN_POINT('Ctrl Pts',(-19.5611123360753,22.6544494106336,-47.4897371736399));
#72960=CARTESIAN_POINT('Ctrl Pts',(-20.6402989485513,26.422163546325,-47.290850262265));
#72961=CARTESIAN_POINT('Ctrl Pts',(-24.3934861805585,27.5508349574702,-47.0919633508901));
#72962=CARTESIAN_POINT('Ctrl Pts',(-27.3718131836827,25.003310312781,-46.8930764395152));
#72963=CARTESIAN_POINT('Ctrl Pts',(-26.8384499625401,21.1205487662565,-46.6941895281402));
#72964=CARTESIAN_POINT('Ctrl Pts',(-23.283512095617,19.4704789752617,-46.4953026167655));
#72965=CARTESIAN_POINT('Ctrl Pts',(-19.9736860735894,21.5693751748738,-46.2964157053904));
#72966=CARTESIAN_POINT('Ctrl Pts',(-19.9504213837315,25.4885297147003,-46.0975287940157));
#72967=CARTESIAN_POINT('Ctrl Pts',(-23.2350963035024,27.6265718621486,-45.8986418826407));
#72968=CARTESIAN_POINT('Ctrl Pts',(-26.8093730761399,26.0188221597938,-45.6997549712659));
#72969=CARTESIAN_POINT('Ctrl Pts',(-27.3887943962852,22.1426662694047,-45.500868059891));
#72970=CARTESIAN_POINT('Ctrl Pts',(-24.4409211975515,19.5599628104253,-45.3019811485161));
#72971=CARTESIAN_POINT('Ctrl Pts',(-20.6745990111445,20.6439972845154,-45.1030942371412));
#72972=CARTESIAN_POINT('Ctrl Pts',(-19.5507585949113,24.3986339209527,-44.9042073257663));
#72973=CARTESIAN_POINT('Ctrl Pts',(-22.1021140054161,27.3736799915414,-44.7053204143916));
#72974=CARTESIAN_POINT('Ctrl Pts',(-25.9841859396713,26.8353203997202,-44.5064335030164));
#72975=CARTESIAN_POINT('Ctrl Pts',(-27.6296794355174,23.278261965007,-44.3075465916417));
#72976=CARTESIAN_POINT('Ctrl Pts',(-25.5265254851134,19.9711398000821,-44.1086596802667));
#72977=CARTESIAN_POINT('Ctrl Pts',(-21.6073442508314,19.9529187767919,-43.9097727688919));
#72978=CARTESIAN_POINT('Ctrl Pts',(-19.4735309952058,23.240342470652,-43.710885857517));
#72979=CARTESIAN_POINT('Ctrl Pts',(-21.0858791826267,26.8125472345698,-43.511998946142));
#72980=CARTESIAN_POINT('Ctrl Pts',(-24.9627775334374,27.3869797635227,-43.3131120347672));
#72981=CARTESIAN_POINT('Ctrl Pts',(-27.5416851700163,24.4357852672497,-43.1142251233922));
#72982=CARTESIAN_POINT('Ctrl Pts',(-26.4528046296572,20.6708612677958,-42.9153382120174));
#72983=CARTESIAN_POINT('Ctrl Pts',(-22.6967248071047,19.5518537077446,-42.7164513006426));
#72984=CARTESIAN_POINT('Ctrl Pts',(-19.7249645962329,22.107035658588,-42.5175643892676));
#72985=CARTESIAN_POINT('Ctrl Pts',(-20.2683196671178,25.9884115512041,-42.3186774778927));
#72986=CARTESIAN_POINT('Ctrl Pts',(-23.827492778529,27.6293260266853,-42.1197905665179));
#72987=CARTESIAN_POINT('Ctrl Pts',(-27.1319056091957,25.5219178086689,-41.9209036551429));
#72988=CARTESIAN_POINT('Ctrl Pts',(-27.1450829357411,21.6027163707607,-41.7220167437681));
#72989=CARTESIAN_POINT('Ctrl Pts',(-23.8549159123231,19.473135540914,-41.5231298323931));
#72990=CARTESIAN_POINT('Ctrl Pts',(-20.2847890733021,21.0900795430794,-41.3242429210183));
#72991=CARTESIAN_POINT('Ctrl Pts',(-19.7153462868994,24.9677139335101,-41.1253560096434));
#72992=CARTESIAN_POINT('Ctrl Pts',(-22.6698571930328,27.5428214765801,-40.9264690982685));
#72993=CARTESIAN_POINT('Ctrl Pts',(-26.4333767701808,26.4490966733227,-40.7275821868936));
#72994=CARTESIAN_POINT('Ctrl Pts',(-27.5475496207836,22.6915798853607,-40.5286952755187));
#72995=CARTESIAN_POINT('Ctrl Pts',(-24.9885453614165,19.7231104559445,-40.3298083641438));
#72996=CARTESIAN_POINT('Ctrl Pts',(-21.1078719386565,20.271460106005,-40.130921452769));
#72997=CARTESIAN_POINT('Ctrl Pts',(-19.471539201173,23.8327419995197,-39.932034541394));
#72998=CARTESIAN_POINT('Ctrl Pts',(-21.5831981965761,27.1344400232601,-39.7331476300192));
#72999=CARTESIAN_POINT('Ctrl Pts',(-25.5024133472483,27.1425736312368,-39.5342607186442));
#73000=CARTESIAN_POINT('Ctrl Pts',(-27.6277582243685,23.8496687273357,-39.3353738072694));
#73001=CARTESIAN_POINT('Ctrl Pts',(-26.0062210853925,20.281625725947,-39.1364868958945));
#73002=CARTESIAN_POINT('Ctrl Pts',(-22.127857077362,19.7171736251884,-38.9375999845196));
#73003=CARTESIAN_POINT('Ctrl Pts',(-19.556553892616,22.6749960480111,-38.7387130731447));
#73004=CARTESIAN_POINT('Ctrl Pts',(-20.6551211473777,26.4371049698264,-38.5398261617698));
#73005=CARTESIAN_POINT('Ctrl Pts',(-24.4140686776643,27.5464412657212,-38.340939250395));
#73006=CARTESIAN_POINT('Ctrl Pts',(-27.3792424093357,24.9836189359757,-38.14205233902));
#73007=CARTESIAN_POINT('Ctrl Pts',(-26.8258990882597,21.1036544101253,-37.9431654276452));
#73008=CARTESIAN_POINT('Ctrl Pts',(-23.2625143107282,19.471906120684,-37.7442785162702));
#73009=CARTESIAN_POINT('Ctrl Pts',(-19.9635365620865,21.5878123962085,-37.5453916048954));
#73010=CARTESIAN_POINT('Ctrl Pts',(-19.960446686149,25.5070347687594,-37.3465046935204));
#73011=CARTESIAN_POINT('Ctrl Pts',(-23.2560840169241,27.6281401732216,-37.1476177821456));
#73012=CARTESIAN_POINT('Ctrl Pts',(-26.8220372713958,26.0020125829756,-36.9487308707706));
#73013=CARTESIAN_POINT('Ctrl Pts',(-27.3814977516819,22.122925380574,-36.7498439593958));
#73014=CARTESIAN_POINT('Ctrl Pts',(-24.4203687108259,19.5554308126663,-36.5509570480209));
#73015=CARTESIAN_POINT('Ctrl Pts',(-20.6596766750338,20.6588386995185,-36.3520701366461));
#73016=CARTESIAN_POINT('Ctrl Pts',(-19.5551787710958,24.4192107466747,-36.1531832252711));
#73017=CARTESIAN_POINT('Ctrl Pts',(-22.1218149267513,27.3810838697706,-35.9542963138963));
#73018=CARTESIAN_POINT('Ctrl Pts',(-26.0010641298127,26.8227477941097,-35.7554094025213));
#73019=CARTESIAN_POINT('Ctrl Pts',(-27.6282252687597,23.2572660341312,-35.5565224911465));
#73020=CARTESIAN_POINT('Ctrl Pts',(-25.5080752174138,19.9610140242549,-35.3576355797715));
#73021=CARTESIAN_POINT('Ctrl Pts',(-21.5888521138813,19.9629678854739,-35.1587486683967));
#73022=CARTESIAN_POINT('Ctrl Pts',(-19.4719896949873,23.2613321849885,-34.9598617570218));
#73023=CARTESIAN_POINT('Ctrl Pts',(-21.1027050433604,26.8251897867199,-34.7609748456469));
#73024=CARTESIAN_POINT('Ctrl Pts',(-24.9825090157064,27.3796577199719,-34.562087934272));
#73025=CARTESIAN_POINT('Ctrl Pts',(-27.5461907145694,24.4152269652145,-34.3632010228971));
#73026=CARTESIAN_POINT('Ctrl Pts',(-26.4379440230572,20.6559580437898,-34.1643141115222));
#73027=CARTESIAN_POINT('Ctrl Pts',(-22.6761536868454,19.5563003610444,-33.9654272001473));
#73028=CARTESIAN_POINT('Ctrl Pts',(-19.7175860776892,22.126746091825,-33.7665402887725));
#73029=CARTESIAN_POINT('Ctrl Pts',(-20.2809139832361,26.0052735474027,-33.5676533773975));
#73030=CARTESIAN_POINT('Ctrl Pts',(-23.8484868206187,27.6278448410005,-33.3687664660227));
#73031=CARTESIAN_POINT('Ctrl Pts',(-27.1420076325773,25.5034545251612,-33.1698795546478));
#73032=CARTESIAN_POINT('Ctrl Pts',(-27.1350100374375,21.5842371815452,-32.9709926432729));
#73033=CARTESIAN_POINT('Ctrl Pts',(-23.8339242318343,19.4716212541032,-32.7721057318979));
#73034=CARTESIAN_POINT('Ctrl Pts',(-20.2721681851962,21.1069216598618,-32.5732188205231));
#73035=CARTESIAN_POINT('Ctrl Pts',(-19.7226937172709,24.9874359765389,-32.3743319091482));
#73036=CARTESIAN_POINT('Ctrl Pts',(-22.6904212763297,27.5473005604653,-32.1754449977733));
#73037=CARTESIAN_POINT('Ctrl Pts',(-26.4482608574,26.4342168997375,-31.9765580863984));
#73038=CARTESIAN_POINT('Ctrl Pts',(-27.543076497733,22.6710145046333,-31.7776711750235));
#73039=CARTESIAN_POINT('Ctrl Pts',(-24.9688254489214,19.7157573093065,-31.5787842636486));
#73040=CARTESIAN_POINT('Ctrl Pts',(-21.091026164327,20.2840761117728,-31.3798973522737));
#73041=CARTESIAN_POINT('Ctrl Pts',(-19.4730474033318,23.8537341180536,-31.1810104408989));
#73042=CARTESIAN_POINT('Ctrl Pts',(-21.6016744653136,27.1445182774654,-30.9821235295239));
#73043=CARTESIAN_POINT('Ctrl Pts',(-25.520879558124,27.1324769599941,-30.7832366181491));
#73044=CARTESIAN_POINT('Ctrl Pts',(-27.629245495264,23.8286751154602,-30.5843497067742));
#73045=CARTESIAN_POINT('Ctrl Pts',(-25.9893627404548,20.2690265227877,-30.3854627953993));
#73046=CARTESIAN_POINT('Ctrl Pts',(-22.1081445062367,19.7245464302124,-30.1865758840244));
#73047=CARTESIAN_POINT('Ctrl Pts',(-19.552101276817,22.6955658785119,-29.9876889726495));
#73048=CARTESIAN_POINT('Ctrl Pts',(-20.6700200633047,26.4519698956079,-29.7888020612746));
#73049=CARTESIAN_POINT('Ctrl Pts',(-24.4346282848001,27.5419416803281,-29.5899151498998));
#73050=CARTESIAN_POINT('Ctrl Pts',(-27.3865701718898,24.9638895768821,-29.3910282385248));
#73051=CARTESIAN_POINT('Ctrl Pts',(-26.8132614137367,21.0868248855645,-29.19214132715));
#73052=CARTESIAN_POINT('Ctrl Pts',(-23.2415241505165,19.473441336819,-28.993254415775));
#73053=CARTESIAN_POINT('Ctrl Pts',(-19.9534820937486,21.606301619576,-28.7943675044002));
#73054=CARTESIAN_POINT('Ctrl Pts',(-19.970567113609,25.5254879707124,-28.5954805930253));
#73055=CARTESIAN_POINT('Ctrl Pts',(-23.2770795254171,27.6296004257387,-28.3965936816504));
#73056=CARTESIAN_POINT('Ctrl Pts',(-26.8346147687422,25.9851380378026,-28.1977067702755));
#73057=CARTESIAN_POINT('Ctrl Pts',(-27.3740995842164,22.1032223139994,-27.9988198589006));
#73058=CARTESIAN_POINT('Ctrl Pts',(-24.399793167188,19.5510046723275,-27.7999329475257));
#73059=CARTESIAN_POINT('Ctrl Pts',(-20.6448309353086,20.6737567331121,-27.6010460361508));
#73060=CARTESIAN_POINT('Ctrl Pts',(-19.5597048113794,24.4397645461687,-27.4021591247759));
#73061=CARTESIAN_POINT('Ctrl Pts',(-22.1415536997682,27.388386236105,-27.2032722134011));
#73062=CARTESIAN_POINT('Ctrl Pts',(-26.0178773767323,26.8100884717615,-27.0043853020261));
#73063=CARTESIAN_POINT('Ctrl Pts',(-27.6266630411912,23.2362778670052,-26.8054983906513));
#73064=CARTESIAN_POINT('Ctrl Pts',(-25.4895730700376,19.9509833584364,-26.6066114792763));
#73065=CARTESIAN_POINT('Ctrl Pts',(-21.5704119514127,19.9731120523902,-26.4077245679015));
#73066=CARTESIAN_POINT('Ctrl Pts',(-19.4705564632671,23.2823295553269,-26.2088376565266));
#73067=CARTESIAN_POINT('Ctrl Pts',(-21.1195957608214,26.8377455574228,-26.0099507451517));
#73068=CARTESIAN_POINT('Ctrl Pts',(-25.0022025450986,27.3722342023172,-25.8110638337769));
#73069=CARTESIAN_POINT('Ctrl Pts',(-27.5505903721173,24.3946457425163,-25.6121769224019));
#73070=CARTESIAN_POINT('Ctrl Pts',(-26.4230068965039,20.6411315147079,-25.4132900110271));
#73071=CARTESIAN_POINT('Ctrl Pts',(-22.6556057290338,19.5608528487226,-25.2144030996521));
#73072=CARTESIAN_POINT('Ctrl Pts',(-19.7103091196687,22.1464942460744,-25.0155161882773));
#73073=CARTESIAN_POINT('Ctrl Pts',(-20.2935949324433,26.0220704888353,-24.8166292769023));
#73074=CARTESIAN_POINT('Ctrl Pts',(-23.8694729598992,27.6262556045857,-24.6177423655275));
#73075=CARTESIAN_POINT('Ctrl Pts',(-27.1520144792637,25.4849394844189,-24.4188554541526));
#73076=CARTESIAN_POINT('Ctrl Pts',(-27.1248421478655,21.5658100891014,-24.2199685427777));
#73077=CARTESIAN_POINT('Ctrl Pts',(-23.8129250344257,19.4702150455535,-24.0210816314028));
#73078=CARTESIAN_POINT('Ctrl Pts',(-20.2596341619313,21.1238285216369,-23.822194720028));
#73079=CARTESIAN_POINT('Ctrl Pts',(-19.7301425728201,25.0071199361328,-23.623307808653));
#73080=CARTESIAN_POINT('Ctrl Pts',(-22.7110081440022,27.5516737279358,-23.4244208972782));
#73081=CARTESIAN_POINT('Ctrl Pts',(-26.4630681512832,26.4192607049628,-23.2255339859032));
#73082=CARTESIAN_POINT('Ctrl Pts',(-27.5384975701998,22.6504724225348,-23.0266470745284));
#73083=CARTESIAN_POINT('Ctrl Pts',(-24.9490679461458,19.7085057716518,-22.8277601631535));
#73084=CARTESIAN_POINT('Ctrl Pts',(-21.0742455561998,20.2967786668372,-22.6288732517786));
#73085=CARTESIAN_POINT('Ctrl Pts',(-19.4746636459607,23.8747181947322,-22.4299863404037));
#73086=CARTESIAN_POINT('Ctrl Pts',(-21.6202023687578,27.1545012884469,-22.2310994290288));
#73087=CARTESIAN_POINT('Ctrl Pts',(-25.5392935500252,27.1222853646061,-22.0322125176539));
#73088=CARTESIAN_POINT('Ctrl Pts',(-27.6306246783143,23.8076741257598,-21.833325606279));
#73089=CARTESIAN_POINT('Ctrl Pts',(-25.9724397623662,20.256514267719,-21.6344386949041));
#73090=CARTESIAN_POINT('Ctrl Pts',(-22.0884701490409,19.7320206113193,-21.4355517835292));
#73091=CARTESIAN_POINT('Ctrl Pts',(-19.5477546066665,22.7161583570634,-21.2366648721544));
#73092=CARTESIAN_POINT('Ctrl Pts',(-20.6849953015308,26.4667579297692,-21.0377779607794));
#73093=CARTESIAN_POINT('Ctrl Pts',(-24.4551644571639,27.5373363205236,-20.8388910494046));
#73094=CARTESIAN_POINT('Ctrl Pts',(-27.3937962771691,24.9441227583021,-20.6400041380297));
#73095=CARTESIAN_POINT('Ctrl Pts',(-26.8005372738526,21.0700606385341,-20.4411172266548));
#73096=CARTESIAN_POINT('Ctrl Pts',(-23.2205421711933,19.4750845829856,-20.2422303152799));
#73097=CARTESIAN_POINT('Ctrl Pts',(-19.9435229350058,21.6248423550366,-20.043343403905));
#73098=CARTESIAN_POINT('Ctrl Pts',(-19.980782397934,25.543888831574,-19.8444564925301));
#73099=CARTESIAN_POINT('Ctrl Pts',(-23.2980822726284,27.6309525810051,-19.6455695811552));
#73100=CARTESIAN_POINT('Ctrl Pts',(-26.8471052348921,25.9681989714279,-19.4466826697803));
#73101=CARTESIAN_POINT('Ctrl Pts',(-27.3666000899299,22.0835575917858,-19.2477957584055));
#73102=CARTESIAN_POINT('Ctrl Pts',(-24.3791951118623,19.5466845066959,-19.0489088470305));
#73103=CARTESIAN_POINT('Ctrl Pts',(-20.6300621853608,20.6887509899882,-18.8500219356557));
#73104=CARTESIAN_POINT('Ctrl Pts',(-19.5643365958281,24.4602947747868,-18.6511350242807));
#73105=CARTESIAN_POINT('Ctrl Pts',(-22.1613298014156,27.3955868970413,-18.4522481129059));
#73106=CARTESIAN_POINT('Ctrl Pts',(-26.0346252349013,26.797342768131,-18.253361201531));
#73107=CARTESIAN_POINT('Ctrl Pts',(-27.6249927942088,23.2152980197868,-18.0544742901561));
#73108=CARTESIAN_POINT('Ctrl Pts',(-25.4710195332669,19.9410480684262,-17.8555873787812));
#73109=CARTESIAN_POINT('Ctrl Pts',(-21.5520242520656,19.9833510087338,-17.6567004674063));
#73110=CARTESIAN_POINT('Ctrl Pts',(-19.4692313380238,23.3033340252649,-17.4578135560314));
#73111=CARTESIAN_POINT('Ctrl Pts',(-21.1365508874283,26.8502142139675,-17.2589266446566));
#73112=CARTESIAN_POINT('Ctrl Pts',(-25.0218575997618,27.3647094072718,-17.0600397332816));
#73113=CARTESIAN_POINT('Ctrl Pts',(-27.5548840260751,24.37404214453,-16.8611528219068));
#73114=CARTESIAN_POINT('Ctrl Pts',(-26.4079936458107,20.6263820734331,-16.6622659105319));
#73115=CARTESIAN_POINT('Ctrl Pts',(-22.6350814781631,19.5655110501445,-16.463378999157));
#73116=CARTESIAN_POINT('Ctrl Pts',(-19.703133915001,22.1662795980365,-16.2644920877821));
#73117=CARTESIAN_POINT('Ctrl Pts',(-20.3063621787112,26.0388019304058,-16.0656051764072));
#73118=CARTESIAN_POINT('Ctrl Pts',(-23.8904506402666,27.6245583595535,-15.8667182650323));
#73119=CARTESIAN_POINT('Ctrl Pts',(-27.1619258840868,25.4663731770661,-15.6678313536574));
#73120=CARTESIAN_POINT('Ctrl Pts',(-27.1145795364606,21.5474355817217,-15.4689444422825));
#73121=CARTESIAN_POINT('Ctrl Pts',(-23.7919188765479,19.4689169525278,-15.2700575309077));
#73122=CARTESIAN_POINT('Ctrl Pts',(-20.2471873356418,21.1407996803954,-15.0711706195327));
#73123=CARTESIAN_POINT('Ctrl Pts',(-19.7376926561622,25.0267652906936,-14.8722837081579));
#73124=CARTESIAN_POINT('Ctrl Pts',(-22.7316172505259,27.5559408631087,-14.673396796783));
#73125=CARTESIAN_POINT('Ctrl Pts',(-26.4777982594575,26.4042284853174,-14.4745098854081));
#73126=CARTESIAN_POINT('Ctrl Pts',(-27.5338129595197,22.6299541834031,-14.2756229740332));
#73127=CARTESIAN_POINT('Ctrl Pts',(-24.9292733766367,19.701356035136,-14.0767360626583));
#73128=CARTESIAN_POINT('Ctrl Pts',(-21.057530558938,20.3095674345978,-13.8778491512834));
#73129=CARTESIAN_POINT('Ctrl Pts',(-19.4763878862318,23.8956936735058,-13.6789622399085));
#73130=CARTESIAN_POINT('Ctrl Pts',(-21.6387814159439,27.1643887916678,-13.4800753285336));
#73131=CARTESIAN_POINT('Ctrl Pts',(-25.5576548350058,27.1119991151366,-13.2811884171587));
#73132=CARTESIAN_POINT('Ctrl Pts',(-27.6318957369723,23.786666314732,-13.0823015057838));
#73133=CARTESIAN_POINT('Ctrl Pts',(-25.955452599563,20.2440892922991,-12.8834145944089));
#73134=CARTESIAN_POINT('Ctrl Pts',(-22.0688345271186,19.7395959704539,-12.6845276830341));
#73135=CARTESIAN_POINT('Ctrl Pts',(-19.5435139973455,22.7367729379924,-12.4856407716592));
#73136=CARTESIAN_POINT('Ctrl Pts',(-20.7000464652327,26.4814686804472,-12.2867538602843));
#73137=CARTESIAN_POINT('Ctrl Pts',(-24.4756766505751,27.5326253083435,-12.0878669489094));
#73138=CARTESIAN_POINT('Ctrl Pts',(-27.4009205336917,24.9243190040294,-11.8889800375345));
#73139=CARTESIAN_POINT('Ctrl Pts',(-26.7877270057798,21.053362113264,-11.6900931261596));
#73140=CARTESIAN_POINT('Ctrl Pts',(-23.1995689287524,19.4768358156397,-11.4912062147847));
#73141=CARTESIAN_POINT('Ctrl Pts',(-19.9336593497623,21.6434341112861,-11.2923193034098));
#73142=CARTESIAN_POINT('Ctrl Pts',(-19.9910922684325,25.5622368637462,-11.0934323920349));
#73143=CARTESIAN_POINT('Ctrl Pts',(-23.3190917020137,27.6321966031907,-10.8945454806601));
#73144=CARTESIAN_POINT('Ctrl Pts',(-26.8595083388649,25.9511958327137,-10.6956585692851));
#73145=CARTESIAN_POINT('Ctrl Pts',(-27.3589994675491,22.0639317350221,-10.4967716579103));
#73146=CARTESIAN_POINT('Ctrl Pts',(-24.3585750906692,19.54247043025,-10.2978847465354));
#73147=CARTESIAN_POINT('Ctrl Pts',(-20.6153708165425,20.7038210728193,-10.0989978351605));
#73148=CARTESIAN_POINT('Ctrl Pts',(-19.5690740017059,24.4808008885054,-9.90011092378563));
#73149=CARTESIAN_POINT('Ctrl Pts',(-22.1811427076536,27.4026856617719,-9.70122401241075));
#73150=CARTESIAN_POINT('Ctrl Pts',(-26.0513072605242,26.784511020962,-9.50233710103585));
#73151=CARTESIAN_POINT('Ctrl Pts',(-27.6232145720716,23.1943270484138,-9.30345018966096));
#73152=CARTESIAN_POINT('Ctrl Pts',(-25.4524150987455,19.931208417496,-9.10456327828608));
#73153=CARTESIAN_POINT('Ctrl Pts',(-21.533689503089,19.9936844831863,-8.90567636691117));
#73154=CARTESIAN_POINT('Ctrl Pts',(-19.4680143543712,23.3243450382125,-8.7067894555363));
#73155=CARTESIAN_POINT('Ctrl Pts',(-21.1535699738932,26.8625954259514,-8.50790254416139));
#73156=CARTESIAN_POINT('Ctrl Pts',(-25.0414736588636,27.3570835342327,-8.30901563278651));
#73157=CARTESIAN_POINT('Ctrl Pts',(-27.5590715626666,24.3534167172232,-8.11012872141162));
#73158=CARTESIAN_POINT('Ctrl Pts',(-26.3929046688091,20.6117101108059,-7.91124181003674));
#73159=CARTESIAN_POINT('Ctrl Pts',(-22.6145814780984,19.5702748418738,-7.71235489866183));
#73160=CARTESIAN_POINT('Ctrl Pts',(-19.6960606538194,22.1861016234263,-7.51346798728695));
#73161=CARTESIAN_POINT('Ctrl Pts',(-20.3192153837249,26.0554674287532,-7.31458107591206));
#73162=CARTESIAN_POINT('Ctrl Pts',(-23.91141930584,27.6227531508786,-7.11569416453717));
#73163=CARTESIAN_POINT('Ctrl Pts',(-27.1717415844078,25.4477560950847,-6.91680725316227));
#73164=CARTESIAN_POINT('Ctrl Pts',(-27.104222475168,21.5291141463064,-6.71792034178739));
#73165=CARTESIAN_POINT('Ctrl Pts',(-23.770906314836,19.4677270094237,-6.51903343041249));
#73166=CARTESIAN_POINT('Ctrl Pts',(-20.2348280361521,21.1578346864247,-6.32014651903762));
#73167=CARTESIAN_POINT('Ctrl Pts',(-19.7453437672301,25.0463715196455,-6.12125960766271));
#73168=CARTESIAN_POINT('Ctrl Pts',(-22.7522480497871,27.5601018529106,-5.92237269628783));
#73169=CARTESIAN_POINT('Ctrl Pts',(-26.4924507915943,26.3891206391351,-5.72348578491294));
#73170=CARTESIAN_POINT('Ctrl Pts',(-27.5290227898282,22.609460330944,-5.52459887353805));
#73171=CARTESIAN_POINT('Ctrl Pts',(-24.909442264924,19.6943082892178,-5.32571196216315));
#73172=CARTESIAN_POINT('Ctrl Pts',(-21.040881615467,20.3224420761691,-5.12682505078827));
#73173=CARTESIAN_POINT('Ctrl Pts',(-19.4782200784547,23.9166599985522,-4.92793813941337));
#73174=CARTESIAN_POINT('Ctrl Pts',(-21.6574111145523,27.1741805251229,-4.72905122803848));
#73175=CARTESIAN_POINT('Ctrl Pts',(-25.5759629265164,27.1016184841571,-4.53016431666359));
#73176=CARTESIAN_POINT('Ctrl Pts',(-27.6330586375572,23.7656522390559,-4.33127740528871));
#73177=CARTESIAN_POINT('Ctrl Pts',(-25.9384017021823,20.2317519257727,-4.13239049391381));
#73178=CARTESIAN_POINT('Ctrl Pts',(-22.0492381607876,19.747272306879,-3.93350358253892));
#73179=CARTESIAN_POINT('Ctrl Pts',(-19.5393795612244,22.7574090750401,-3.73461667116403));
#73180=CARTESIAN_POINT('Ctrl Pts',(-20.7151731555746,26.4961017578267,-3.53572975978914));
#73181=CARTESIAN_POINT('Ctrl Pts',(-24.4961643214874,27.5278087686234,-3.33684284841425));
#73182=CARTESIAN_POINT('Ctrl Pts',(-27.4079427526743,24.9044788388371,-3.13795593703936));
#73183=CARTESIAN_POINT('Ctrl Pts',(-26.7748309489734,21.0367297522428,-2.93906902566447));
#73184=CARTESIAN_POINT('Ctrl Pts',(-23.1786049789569,19.4786949883764,-2.74018211428958));
#73185=CARTESIAN_POINT('Ctrl Pts',(-19.9238915993898,21.6620763956673,-2.54129520291469));
#73186=CARTESIAN_POINT('Ctrl Pts',(-20.0014964519067,25.580531581031,-2.34240829153979));
#73187=CARTESIAN_POINT('Ctrl Pts',(-23.340107256851,27.6333324593303,-2.14352138016491));
#73188=CARTESIAN_POINT('Ctrl Pts',(-26.871823751995,25.9341290722209,-1.94463446879002));
#73189=CARTESIAN_POINT('Ctrl Pts',(-27.3512979184802,22.0443452637667,-1.74574755741513));
#73190=CARTESIAN_POINT('Ctrl Pts',(-24.3379336500121,19.5383625546572,-1.54686064604024));
#73191=CARTESIAN_POINT('Ctrl Pts',(-20.6007572181553,20.7189665822683,-1.34797373466534));
#73192=CARTESIAN_POINT('Ctrl Pts',(-19.5739169034777,24.50128234394,-1.14908682329046));
#73193=CARTESIAN_POINT('Ctrl Pts',(-22.2009918934665,27.4096823421886,-0.95019991191556));
#73194=CARTESIAN_POINT('Ctrl Pts',(-26.0679230115496,26.7715935702787,-0.751313000540672));
#73195=CARTESIAN_POINT('Ctrl Pts',(-27.6213284219005,23.1733655085891,-0.552426089165777));
#73196=CARTESIAN_POINT('Ctrl Pts',(-25.4337602594659,19.9214646663832,-0.353539177790892));
#73197=CARTESIAN_POINT('Ctrl Pts',(-21.5154081903294,20.0041122019244,-0.154652266415998));
#73198=CARTESIAN_POINT('Ctrl Pts',(-19.466905544558,23.3453620374057,0.0442346449588902));
#73199=CARTESIAN_POINT('Ctrl Pts',(-21.170652569233,26.874888865289,0.24312155633378));
#73200=CARTESIAN_POINT('Ctrl Pts',(-25.0610502026044,27.3493567852751,0.44200846770867));
#73201=CARTESIAN_POINT('Ctrl Pts',(-27.5631528709278,24.3327700071423,0.640895379083562));
#73202=CARTESIAN_POINT('Ctrl Pts',(-26.3777403653365,20.5971160156136,0.839782290458452));
#73203=CARTESIAN_POINT('Ctrl Pts',(-22.5941062720623,19.5751440976768,1.03866920183334));
#73204=CARTESIAN_POINT('Ctrl Pts',(-19.6890895235559,22.2059597969863,1.23755611320823));
#73205=CARTESIAN_POINT('Ctrl Pts',(-20.3321542068916,26.0720665422642,1.43644302458312));
#73206=CARTESIAN_POINT('Ctrl Pts',(-23.9323784009782,27.6208400263966,1.63532993595801));
#73207=CARTESIAN_POINT('Ctrl Pts',(-27.1814613201236,25.4290887318025,1.83421684733291));
#73208=CARTESIAN_POINT('Ctrl Pts',(-27.0937712384363,21.5108462683488,2.03310375870779));
#73209=CARTESIAN_POINT('Ctrl Pts',(-23.7498879060944,19.4666452477732,2.2319906700827));
#73210=CARTESIAN_POINT('Ctrl Pts',(-20.222556590967,21.1749330883198,2.43087758145757));
#73211=CARTESIAN_POINT('Ctrl Pts',(-19.7530957032797,25.06593810345,2.62976449283247));
#73212=CARTESIAN_POINT('Ctrl Pts',(-22.7728999950974,27.564156587081,2.82865140420734));
#73213=CARTESIAN_POINT('Ctrl Pts',(-26.5070253594215,26.3739375667534,3.02753831558225));
#73214=CARTESIAN_POINT('Ctrl Pts',(-27.5241271880586,22.5889914082169,3.22642522695711));
#73215=CARTESIAN_POINT('Ctrl Pts',(-24.8895751365054,19.6873627206529,3.42531213833204));
#73216=CARTESIAN_POINT('Ctrl Pts',(-21.0242991669612,20.3354022503905,3.62419904970691));
#73217=CARTESIAN_POINT('Ctrl Pts',(-19.480160174079,23.9376166142918,3.82308596108181));
#73218=CARTESIAN_POINT('Ctrl Pts',(-21.6760909709207,27.1838762293441,4.02197287245669));
#73219=CARTESIAN_POINT('Ctrl Pts',(-25.5942173394172,27.0911437467407,4.22085978383159));
#73220=CARTESIAN_POINT('Ctrl Pts',(-27.6341133492534,23.7446324555762,4.41974669520646));
#73221=CARTESIAN_POINT('Ctrl Pts',(-25.92128752205,20.2195024950638,4.61863360658138));
#73222=CARTESIAN_POINT('Ctrl Pts',(-22.0296815693252,19.7550494171818,4.81752051795627));
#73223=CARTESIAN_POINT('Ctrl Pts',(-19.5353514078603,22.7780662213765,5.01640742933116));
#73224=CARTESIAN_POINT('Ctrl Pts',(-20.7303749717194,26.5106567741508,5.21529434070603));
#73225=CARTESIAN_POINT('Ctrl Pts',(-24.5166269270054,27.522886828995,5.41418125208093));
#73226=CARTESIAN_POINT('Ctrl Pts',(-27.4148627480375,24.8846027884633,5.61306816345578));
#73227=CARTESIAN_POINT('Ctrl Pts',(-26.7618494451617,21.0201639962057,5.81195507483073));
#73228=CARTESIAN_POINT('Ctrl Pts',(-23.1576508773234,19.4806620519298,6.01084198620561));
#73229=CARTESIAN_POINT('Ctrl Pts',(-19.9142199427209,21.6807687141851,6.2097288975805));
#73230=CARTESIAN_POINT('Ctrl Pts',(-20.0119946726599,25.5987724986425,6.40861580895537));
#73231=CARTESIAN_POINT('Ctrl Pts',(-23.3611283802564,27.6343601193255,6.60750272033028));
#73232=CARTESIAN_POINT('Ctrl Pts',(-26.8840511479407,25.9169991421951,6.80638963170513));
#73233=CARTESIAN_POINT('Ctrl Pts',(-27.3434956468041,22.0247986970354,7.00527654308008));
#73234=CARTESIAN_POINT('Ctrl Pts',(-24.3172713368611,19.5343609887707,7.20416345445494));
#73235=CARTESIAN_POINT('Ctrl Pts',(-20.58622177744,20.7341871169995,7.40305036582984));
#73236=CARTESIAN_POINT('Ctrl Pts',(-19.5788651728132,24.5217385983595,7.60193727720472));
#73237=CARTESIAN_POINT('Ctrl Pts',(-22.2208768328776,27.4165767528892,7.80082418857962));
#73238=CARTESIAN_POINT('Ctrl Pts',(-26.0844720476824,26.7585907583762,7.99971109995449));
#73239=CARTESIAN_POINT('Ctrl Pts',(-27.6193343936757,23.1524139557652,8.19859801132941));
#73240=CARTESIAN_POINT('Ctrl Pts',(-25.4150555097565,19.9118170732843,8.39748492270429));
#73241=CARTESIAN_POINT('Ctrl Pts',(-21.4971807982172,20.0146338886273,8.59637183407918));
#73242=CARTESIAN_POINT('Ctrl Pts',(-19.4659049379659,23.3663844659224,8.79525874545406));
#73243=CARTESIAN_POINT('Ctrl Pts',(-21.187798220782,26.8870942062206,8.99414565682896));
#73244=CARTESIAN_POINT('Ctrl Pts',(-25.0805867122322,27.3415293651475,9.19303256820384));
#73245=CARTESIAN_POINT('Ctrl Pts',(-27.5671278427097,24.3121025613973,9.39191947957871));
#73246=CARTESIAN_POINT('Ctrl Pts',(-26.3625011372266,20.5826001745801,9.59080639095364));
#73247=CARTESIAN_POINT('Ctrl Pts',(-22.5736564026206,19.5801186885244,9.78969330232851));
#73248=CARTESIAN_POINT('Ctrl Pts',(-19.6822207089359,22.2258535925017,9.98858021370343));
#73249=CARTESIAN_POINT('Ctrl Pts',(-20.3451783053501,26.0885988310845,10.1874671250783));
#73250=CARTESIAN_POINT('Ctrl Pts',(-23.9533273702929,27.6188190368028,10.3863540364532));
#73251=CARTESIAN_POINT('Ctrl Pts',(-27.1910848336742,25.4103715818797,10.5852409478281));
#73252=CARTESIAN_POINT('Ctrl Pts',(-27.0832261032093,21.4926324319235,10.784127859203));
#73253=CARTESIAN_POINT('Ctrl Pts',(-23.7288642072832,19.4656716962415,10.9830147705779));
#73254=CARTESIAN_POINT('Ctrl Pts',(-20.2103733252635,21.1920944329958,11.1819016819528));
#73255=CARTESIAN_POINT('Ctrl Pts',(-19.7609482588949,25.0854645236187,11.3807885933277));
#73256=CARTESIAN_POINT('Ctrl Pts',(-22.793572539208,27.5681049581747,11.5796755047026));
#73257=CARTESIAN_POINT('Ctrl Pts',(-26.5215215767324,26.3586796705037,11.7785624160775));
#73258=CARTESIAN_POINT('Ctrl Pts',(-27.5191262839377,22.5685479576211,11.9774493274523));
#73259=CARTESIAN_POINT('Ctrl Pts',(-24.8696725178331,19.6805195134897,12.1763362388272));
#73260=CARTESIAN_POINT('Ctrl Pts',(-21.0077836528336,20.3484476138346,12.3752231502021));
#73261=CARTESIAN_POINT('Ctrl Pts',(-19.4822081216946,23.9585629654026,12.5741100615771));
#73262=CARTESIAN_POINT('Ctrl Pts',(-21.6948204900581,27.1934756474084,12.7729969729519));
#73263=CARTESIAN_POINT('Ctrl Pts',(-25.6124175899905,27.0805751804539,12.9718838843268));
#73264=CARTESIAN_POINT('Ctrl Pts',(-27.6350598441126,23.7236075212892,13.1707707957017));
#73265=CARTESIAN_POINT('Ctrl Pts',(-25.9041105126688,20.207341324766,13.3696577070766));
#73266=CARTESIAN_POINT('Ctrl Pts',(-22.0101652709548,19.7629270952796,13.5685446184515));
#73267=CARTESIAN_POINT('Ctrl Pts',(-19.5314296439939,22.7987438296151,13.7674315298264));
#73268=CARTESIAN_POINT('Ctrl Pts',(-20.7456515108394,26.5251333437309,13.9663184412013));
#73269=CARTESIAN_POINT('Ctrl Pts',(-24.5370639248974,27.5178596198832,14.1652053525761));
#73270=CARTESIAN_POINT('Ctrl Pts',(-27.4216803364103,24.8646913795963,14.3640922639511));
#73271=CARTESIAN_POINT('Ctrl Pts',(-26.7487828383371,21.0036652841232,14.5629791753259));
#73272=CARTESIAN_POINT('Ctrl Pts',(-23.1367071791074,19.4827369541754,14.7618660867009));
#73273=CARTESIAN_POINT('Ctrl Pts',(-19.9046446360413,21.6995105715179,14.9607529980757));
#73274=CARTESIAN_POINT('Ctrl Pts',(-20.0225866525029,25.616959133221,15.1596399094506));
#73275=CARTESIAN_POINT('Ctrl Pts',(-23.3821545151984,27.6352795559443,15.3585268208255));
#73276=CARTESIAN_POINT('Ctrl Pts',(-26.8961902026918,25.899806496557,15.5574137322004));
#73277=CARTESIAN_POINT('Ctrl Pts',(-27.3355928592704,22.0052925527857,15.7563006435752));
#73278=CARTESIAN_POINT('Ctrl Pts',(-24.29658869874,19.5304658386265,15.9551875549502));
#73279=CARTESIAN_POINT('Ctrl Pts',(-20.5717648795662,20.7494822736892,16.154074466325));
#73280=CARTESIAN_POINT('Ctrl Pts',(-19.5839186785901,24.5421691097005,16.3529613777));
#73281=CARTESIAN_POINT('Ctrl Pts',(-22.2407969989625,27.423368711181,16.5518482890748));
#73282=CARTESIAN_POINT('Ctrl Pts',(-26.100953930395,26.7455029298116,16.7507352004497));
#73283=CARTESIAN_POINT('Ctrl Pts',(-27.6172325402363,23.1314729451304,16.9496221118246));
#73284=CARTESIAN_POINT('Ctrl Pts',(-25.3963013452681,19.9022658938477,17.1485090231995));
#73285=CARTESIAN_POINT('Ctrl Pts',(-21.4790078097535,20.0252492644848,17.3473959345744));
#73286=CARTESIAN_POINT('Ctrl Pts',(-19.4650125611099,23.3874117666964,17.5462828459493));
#73287=CARTESIAN_POINT('Ctrl Pts',(-21.2050064742031,26.899211125321,17.7451697573242));
#73288=CARTESIAN_POINT('Ctrl Pts',(-25.1000826700559,27.3336014812664,17.9440566686991));
#73289=CARTESIAN_POINT('Ctrl Pts',(-27.5709963726804,24.2914149276475,18.1429435800739));
#73290=CARTESIAN_POINT('Ctrl Pts',(-26.3471873882987,20.5681629723558,18.3418304914489));
#73291=CARTESIAN_POINT('Ctrl Pts',(-22.5532324116668,19.5851984825965,18.5407174028237));
#73292=CARTESIAN_POINT('Ctrl Pts',(-19.6754543919742,22.2457824828137,18.7396043141986));
#73293=CARTESIAN_POINT('Ctrl Pts',(-20.3582873339789,26.1050638571306,18.9384912255735));
#73294=CARTESIAN_POINT('Ctrl Pts',(-23.974265658665,27.6166902356509,19.1373781369484));
#73295=CARTESIAN_POINT('Ctrl Pts',(-27.2006118700494,25.3916051412957,19.3362650483233));
#73296=CARTESIAN_POINT('Ctrl Pts',(-27.0725873489185,21.4744731196725,19.5351519596982));
#73297=CARTESIAN_POINT('Ctrl Pts',(-23.7078357755019,19.4648063806263,19.7340388710731));
#73298=CARTESIAN_POINT('Ctrl Pts',(-20.1982785618818,21.2093182657003,19.932925782448));
#73299=CARTESIAN_POINT('Ctrl Pts',(-19.7689012259936,25.1049502627275,20.1318126938229));
#73300=CARTESIAN_POINT('Ctrl Pts',(-22.8142651343239,27.5719468615651,20.3306996051977));
#73301=CARTESIAN_POINT('Ctrl Pts',(-26.5359390593967,26.3433473546996,20.5295865165726));
#73302=CARTESIAN_POINT('Ctrl Pts',(-27.5140202099829,22.5481305208802,20.7284734279475));
#73303=CARTESIAN_POINT('Ctrl Pts',(-24.8497349363,19.6737788490641,20.9273603393224));
#73304=CARTESIAN_POINT('Ctrl Pts',(-20.991335510723,20.3615778208169,21.1262472506973));
#73305=CARTESIAN_POINT('Ctrl Pts',(-19.4843638670336,23.9794984968342,21.3251341620722));
#73306=CARTESIAN_POINT('Ctrl Pts',(-21.7135991756574,27.202978524944,21.5240210734471));
#73307=CARTESIAN_POINT('Ctrl Pts',(-25.6305631959542,27.0699130653494,21.722907984822));
#73308=CARTESIAN_POINT('Ctrl Pts',(-27.6358980970538,23.7025779933274,21.9217948961968));
#73309=CARTESIAN_POINT('Ctrl Pts',(-25.8868711292066,20.1952687371338,22.1206818075718));
#73310=CARTESIAN_POINT('Ctrl Pts',(-21.9906897828324,19.7709051324244,22.3195687189467));
#73311=CARTESIAN_POINT('Ctrl Pts',(-19.5276143735466,22.8194413518271,22.5184556303215));
#73312=CARTESIAN_POINT('Ctrl Pts',(-20.7610023681266,26.5395310829572,22.7173425416964));
#73313=CARTESIAN_POINT('Ctrl Pts',(-24.5574747736107,27.5127272745031,22.9162294530713));
#73314=CARTESIAN_POINT('Ctrl Pts',(-27.428395337136,24.8447451398607,23.1151163644462));
#73315=CARTESIAN_POINT('Ctrl Pts',(-26.7356314747477,20.9872340531911,23.3140032758211));
#73316=CARTESIAN_POINT('Ctrl Pts',(-23.1157744392876,19.484919640127,23.512890187196));
#73317=CARTESIAN_POINT('Ctrl Pts',(-19.8951659330862,21.7183014710393,23.7117770985709));
#73318=CARTESIAN_POINT('Ctrl Pts',(-20.0332721107583,25.6350910028305,23.9106640099458));
#73319=CARTESIAN_POINT('Ctrl Pts',(-23.4031851045212,27.6360907448509,24.1095509213207));
#73320=CARTESIAN_POINT('Ctrl Pts',(-26.9082405945637,25.8825515908363,24.3084378326956));
#73321=CARTESIAN_POINT('Ctrl Pts',(-27.3275897653241,21.9858273480029,24.5073247440704));
#73322=CARTESIAN_POINT('Ctrl Pts',(-24.2758862836511,19.526677207255,24.7062116554454));
#73323=CARTESIAN_POINT('Ctrl Pts',(-20.5573869077351,20.7648516473877,24.9050985668202));
#73324=CARTESIAN_POINT('Ctrl Pts',(-19.589077286684,24.5625733359184,25.1039854781951));
#73325=CARTESIAN_POINT('Ctrl Pts',(-22.2607518642661,27.4300580383393,25.30287238957));
#73326=CARTESIAN_POINT('Ctrl Pts',(-26.1173682221808,26.7323304290285,25.5017593009449));
#73327=CARTESIAN_POINT('Ctrl Pts',(-27.6150229187122,23.1105430360612,25.7006462123198));
#73328=CARTESIAN_POINT('Ctrl Pts',(-25.3774982602538,19.8928113727298,25.8995331236947));
#73329=CARTESIAN_POINT('Ctrl Pts',(-21.4608897116096,20.0359580641337,26.0984200350696));
#73330=CARTESIAN_POINT('Ctrl Pts',(-19.4642284279858,23.4084433524528,26.2973069464445));
#73331=CARTESIAN_POINT('Ctrl Pts',(-21.2222768917239,26.9112393583044,26.4961938578193));
#73332=CARTESIAN_POINT('Ctrl Pts',(-25.11953752505,27.3255732364669,26.6950807691943));
#73333=CARTESIAN_POINT('Ctrl Pts',(-27.5747584232999,24.2707078565843,26.8939676805691));
#73334=CARTESIAN_POINT('Ctrl Pts',(-26.3317994016687,20.5538044091525,27.0928545919441));
#73335=CARTESIAN_POINT('Ctrl Pts',(-22.5328350720498,19.5903840672493,27.2917415033189));
#73336=CARTESIAN_POINT('Ctrl Pts',(-19.6687903145848,22.2657445766198,27.4906284146939));
#73337=CARTESIAN_POINT('Ctrl Pts',(-20.3714817712763,26.1214637581263,27.6895153260686));
#73338=CARTESIAN_POINT('Ctrl Pts',(-23.9951911518478,27.6144488190689,27.8884022374437));
#73339=CARTESIAN_POINT('Ctrl Pts',(-27.210045121279,25.3727990845368,28.0872891488183));
#73340=CARTESIAN_POINT('Ctrl Pts',(-27.0618496976934,21.4563514843679,28.2861760601934));
#73341=CARTESIAN_POINT('Ctrl Pts',(-23.6868136659813,19.4640820434689,28.4850629715682));
#73342=CARTESIAN_POINT('Ctrl Pts',(-20.1862527989148,21.2265423485704,28.6839498829432));
#73343=CARTESIAN_POINT('Ctrl Pts',(-19.7769918228223,25.1245114618019,28.882836794318));
#73344=CARTESIAN_POINT('Ctrl Pts',(-22.8349065564218,27.575461910994,29.081723705693));
#73345=CARTESIAN_POINT('Ctrl Pts',(-26.5504108930691,26.3283570624122,29.2806106170678));
#73346=CARTESIAN_POINT('Ctrl Pts',(-27.5085569433746,22.5269533007581,29.4794975284427));
#73347=CARTESIAN_POINT('Ctrl Pts',(-24.8302402232626,19.6686320185208,29.6783844398176));
#73348=CARTESIAN_POINT('Ctrl Pts',(-20.9740442903307,20.3719251481882,29.8772713511925));
#73349=CARTESIAN_POINT('Ctrl Pts',(-19.4884277064218,24.0062575140647,30.0761582625674));
#73350=CARTESIAN_POINT('Ctrl Pts',(-20.9816170272305,26.134253754113,30.2087495368173));
#73351=CARTESIAN_POINT('Ctrl Pts',(-22.0133720496472,26.646401067984,30.2750451739423));
#73352=CARTESIAN_POINT('Ctrl Pts',(-21.683763360871,20.9301056300456,-74.9968005183715));
#73353=CARTESIAN_POINT('Ctrl Pts',(-20.8100052970332,21.5524671541682,-74.930460688427));
#73354=CARTESIAN_POINT('Ctrl Pts',(-19.7500603056188,23.7286260299716,-74.7978252213578));
#73355=CARTESIAN_POINT('Ctrl Pts',(-21.6508572958594,26.850335879325,-74.5988941171632));
#73356=CARTESIAN_POINT('Ctrl Pts',(-25.2980779597533,26.9287941898422,-74.4000072057885));
#73357=CARTESIAN_POINT('Ctrl Pts',(-27.3384276727157,23.907745369296,-74.2011202944134));
#73358=CARTESIAN_POINT('Ctrl Pts',(-25.8981713831518,20.5555270839545,-74.0022333830388));
#73359=CARTESIAN_POINT('Ctrl Pts',(-22.3001619330665,19.9566147153388,-73.8033464716637));
#73360=CARTESIAN_POINT('Ctrl Pts',(-19.8509935044737,22.6592060284501,-73.6044595602889));
#73361=CARTESIAN_POINT('Ctrl Pts',(-20.8010702345145,26.1809879142899,-73.405572648914));
#73362=CARTESIAN_POINT('Ctrl Pts',(-24.2774443076499,27.2851381721642,-73.2066857375391));
#73363=CARTESIAN_POINT('Ctrl Pts',(-27.0855738978027,24.9573558052932,-73.0077988261642));
#73364=CARTESIAN_POINT('Ctrl Pts',(-26.6450518468136,21.3365062518087,-72.8089119147893));
#73365=CARTESIAN_POINT('Ctrl Pts',(-23.3606668817848,19.7499328594504,-72.6100250034144));
#73366=CARTESIAN_POINT('Ctrl Pts',(-20.2504975646859,21.6555146011386,-72.4111380920396));
#73367=CARTESIAN_POINT('Ctrl Pts',(-20.1725219599432,25.3022085555253,-72.2122511806645));
#73368=CARTESIAN_POINT('Ctrl Pts',(-23.198395070285,27.3389988568772,-72.0133642692899));
#73369=CARTESIAN_POINT('Ctrl Pts',(-26.5475949822429,25.8942549587852,-71.8144773579148));
#73370=CARTESIAN_POINT('Ctrl Pts',(-27.1424915123279,22.2955702762324,-71.61559044654));
#73371=CARTESIAN_POINT('Ctrl Pts',(-24.4364248862794,19.8498328915007,-71.416703535165));
#73372=CARTESIAN_POINT('Ctrl Pts',(-20.9160410567732,20.8044670497123,-71.2178166237902));
#73373=CARTESIAN_POINT('Ctrl Pts',(-19.8162741990877,24.2822454536544,-71.0189297124153));
#73374=CARTESIAN_POINT('Ctrl Pts',(-22.1477168554462,27.0873843233927,-70.8200428010404));
#73375=CARTESIAN_POINT('Ctrl Pts',(-25.7679708746349,26.6421990297343,-70.6211558896656));
#73376=CARTESIAN_POINT('Ctrl Pts',(-27.3503297725253,23.3557770296875,-70.4222689782906));
#73377=CARTESIAN_POINT('Ctrl Pts',(-25.4407398772024,20.2480615422864,-70.2233820669158));
#73378=CARTESIAN_POINT('Ctrl Pts',(-21.7939523994737,20.1747795865263,-70.0244951555408));
#73379=CARTESIAN_POINT('Ctrl Pts',(-19.7610558329135,23.2032710787019,-69.825608244166));
#73380=CARTESIAN_POINT('Ctrl Pts',(-21.2101097619757,26.5506091047579,-69.6267213327911));
#73381=CARTESIAN_POINT('Ctrl Pts',(-24.8095564848403,27.1408738296434,-69.4278344214162));
#73382=CARTESIAN_POINT('Ctrl Pts',(-27.2518096462275,24.4316620155666,-69.2289475100412));
#73383=CARTESIAN_POINT('Ctrl Pts',(-26.2926456595963,20.9125096173449,-69.0300605986664));
#73384=CARTESIAN_POINT('Ctrl Pts',(-22.8134549050434,19.8172193135151,-68.8311736872914));
#73385=CARTESIAN_POINT('Ctrl Pts',(-20.0113186992313,22.1522700282633,-68.6322867759167));
#73386=CARTESIAN_POINT('Ctrl Pts',(-20.4611626333522,25.7719481342452,-68.4333998645416));
#73387=CARTESIAN_POINT('Ctrl Pts',(-23.7496182724133,27.3500763502324,-68.2345129531669));
#73388=CARTESIAN_POINT('Ctrl Pts',(-26.854873699183,25.4364886489002,-68.0356260417919));
#73389=CARTESIAN_POINT('Ctrl Pts',(-26.9234624586994,21.7896098823126,-67.836739130417));
#73390=CARTESIAN_POINT('Ctrl Pts',(-23.8923572963366,19.7606124326231,-67.6378522190422));
#73391=CARTESIAN_POINT('Ctrl Pts',(-20.5468868609678,21.2139729254881,-67.4389653076672));
#73392=CARTESIAN_POINT('Ctrl Pts',(-19.9612548335806,24.8141762926101,-67.2400783962924));
#73393=CARTESIAN_POINT('Ctrl Pts',(-22.6736073939358,27.2529408865141,-67.0411914849174));
#73394=CARTESIAN_POINT('Ctrl Pts',(-26.1915225086404,26.2892488185399,-66.8423045735427));
#73395=CARTESIAN_POINT('Ctrl Pts',(-27.2823344572956,22.8086513915437,-66.6434176621676));
#73396=CARTESIAN_POINT('Ctrl Pts',(-24.9436795446887,20.0095225349377,-66.4445307507929));
#73397=CARTESIAN_POINT('Ctrl Pts',(-21.3245833502678,20.4640243409536,-66.2456438394179));
#73398=CARTESIAN_POINT('Ctrl Pts',(-19.7506884279502,23.7545081852605,-66.046756928043));
#73399=CARTESIAN_POINT('Ctrl Pts',(-21.6682707670623,26.8572984019637,-65.8478700166682));
#73400=CARTESIAN_POINT('Ctrl Pts',(-25.3152347821312,26.9211938551401,-65.6489831052932));
#73401=CARTESIAN_POINT('Ctrl Pts',(-27.3403297548654,23.8874800407619,-65.4500961939183));
#73402=CARTESIAN_POINT('Ctrl Pts',(-25.8826651050613,20.5438827377281,-65.2512092825435));
#73403=CARTESIAN_POINT('Ctrl Pts',(-22.2817110563076,19.9628843772254,-65.0523223711686));
#73404=CARTESIAN_POINT('Ctrl Pts',(-19.8464390688536,22.6783731920182,-64.8534354597936));
#73405=CARTESIAN_POINT('Ctrl Pts',(-20.8146576221548,26.1950451967957,-64.6545485484188));
#73406=CARTESIAN_POINT('Ctrl Pts',(-24.296655957123,27.2813769837839,-64.4556616370439));
#73407=CARTESIAN_POINT('Ctrl Pts',(-27.0927728286966,24.9391217464868,-64.2567747256691));
#73408=CARTESIAN_POINT('Ctrl Pts',(-26.6336139035149,21.3206134574858,-64.0578878142941));
#73409=CARTESIAN_POINT('Ctrl Pts',(-23.3411073035631,19.7509544354633,-63.8590009029193));
#73410=CARTESIAN_POINT('Ctrl Pts',(-20.2407874356726,21.6725282365198,-63.6601139915444));
#73411=CARTESIAN_POINT('Ctrl Pts',(-20.1815853946583,25.3195714600754,-63.4612270801694));
#73412=CARTESIAN_POINT('Ctrl Pts',(-23.2179028367071,27.3407606019554,-63.2623401687946));
#73413=CARTESIAN_POINT('Ctrl Pts',(-26.5596214698418,25.8787942093512,-63.0634532574197));
#73414=CARTESIAN_POINT('Ctrl Pts',(-27.135985201228,22.2770954427571,-62.8645663460447));
#73415=CARTESIAN_POINT('Ctrl Pts',(-24.4173646293078,19.8453200949762,-62.66567943467));
#73416=CARTESIAN_POINT('Ctrl Pts',(-20.9019415586626,20.8180635300704,-62.466792523295));
#73417=CARTESIAN_POINT('Ctrl Pts',(-19.8200917324914,24.3014570062308,-62.2679056119201));
#73418=CARTESIAN_POINT('Ctrl Pts',(-22.1659434153064,27.0945572619281,-62.0690187005452));
#73419=CARTESIAN_POINT('Ctrl Pts',(-25.783857806024,26.6307419780256,-61.8701317891703));
#73420=CARTESIAN_POINT('Ctrl Pts',(-27.3492783281297,23.3362180753784,-61.6712448777954));
#73421=CARTESIAN_POINT('Ctrl Pts',(-25.4237162475812,20.2383736909562,-61.4723579664206));
#73422=CARTESIAN_POINT('Ctrl Pts',(-21.7765998556609,20.1838651601527,-61.2734710550456));
#73423=CARTESIAN_POINT('Ctrl Pts',(-19.7593198920674,23.2227812012153,-61.0745841436708));
#73424=CARTESIAN_POINT('Ctrl Pts',(-21.2255856062074,26.5626156299977,-60.875697232296));
#73425=CARTESIAN_POINT('Ctrl Pts',(-24.8280231256177,27.1343437777115,-60.6768103209209));
#73426=CARTESIAN_POINT('Ctrl Pts',(-27.256297806293,24.4125959511606,-60.4779234095462));
#73427=CARTESIAN_POINT('Ctrl Pts',(-26.2790311004337,20.8984276367849,-60.2790364981711));
#73428=CARTESIAN_POINT('Ctrl Pts',(-22.794248252172,19.8210615631573,-60.0801495867964));
#73429=CARTESIAN_POINT('Ctrl Pts',(-20.0041692381986,22.1705058063621,-59.8812626754214));
#73430=CARTESIAN_POINT('Ctrl Pts',(-20.4726401126653,25.7878203069162,-59.6823757640466));
#73431=CARTESIAN_POINT('Ctrl Pts',(-23.7691758617172,27.3489997365033,-59.4834888526717));
#73432=CARTESIAN_POINT('Ctrl Pts',(-26.8645396321155,25.41945256552,-59.2846019412967));
#73433=CARTESIAN_POINT('Ctrl Pts',(-26.9143545624326,21.7722690454788,-59.0857150299219));
#73434=CARTESIAN_POINT('Ctrl Pts',(-23.8728449553169,19.7589016011293,-58.8868281185469));
#73435=CARTESIAN_POINT('Ctrl Pts',(-20.534900262219,21.2294642084204,-58.6879412071721));
#73436=CARTESIAN_POINT('Ctrl Pts',(-19.9678086450566,24.8326345143992,-58.4890542957972));
#73437=CARTESIAN_POINT('Ctrl Pts',(-22.6926792185619,27.2574045063341,-58.2901673844224));
#73438=CARTESIAN_POINT('Ctrl Pts',(-26.2055869566093,26.2756161482294,-58.0912804730474));
#73439=CARTESIAN_POINT('Ctrl Pts',(-27.2784674933923,22.7894496992577,-57.8923935616725));
#73440=CARTESIAN_POINT('Ctrl Pts',(-24.9254345808759,20.0023965478525,-57.6935066502976));
#73441=CARTESIAN_POINT('Ctrl Pts',(-21.3087259613717,20.4755222370161,-57.4946197389228));
#73442=CARTESIAN_POINT('Ctrl Pts',(-19.7517902098813,23.7740643728503,-57.2957328275478));
#73443=CARTESIAN_POINT('Ctrl Pts',(-21.6853192756418,26.866942402777,-57.0968459161729));
#73444=CARTESIAN_POINT('Ctrl Pts',(-25.3325638834496,26.9120636501059,-56.8979590047981));
#73445=CARTESIAN_POINT('Ctrl Pts',(-27.3420154740766,23.8679655141929,-56.6990720934231));
#73446=CARTESIAN_POINT('Ctrl Pts',(-25.8671584091358,20.5319160849822,-56.5001851820483));
#73447=CARTESIAN_POINT('Ctrl Pts',(-22.2632612840498,19.9694619375712,-56.3012982706734));
#73448=CARTESIAN_POINT('Ctrl Pts',(-19.8419999966857,22.6974507451831,-56.1024113592985));
#73449=CARTESIAN_POINT('Ctrl Pts',(-20.8283083810279,26.2090920889309,-55.9035244479236));
#73450=CARTESIAN_POINT('Ctrl Pts',(-24.3158526570263,27.2774853119971,-55.7046375365487));
#73451=CARTESIAN_POINT('Ctrl Pts',(-27.0998753300306,24.9208676271909,-55.5057506251739));
#73452=CARTESIAN_POINT('Ctrl Pts',(-26.6220956097466,21.3047708786195,-55.3068637137989));
#73453=CARTESIAN_POINT('Ctrl Pts',(-23.3215525500752,19.7520813837756,-55.1079768024241));
#73454=CARTESIAN_POINT('Ctrl Pts',(-20.231165382951,21.6895891420612,-54.9090898910491));
#73455=CARTESIAN_POINT('Ctrl Pts',(-20.1907378933386,25.3368887971795,-54.7102029796743));
#73456=CARTESIAN_POINT('Ctrl Pts',(-23.2374195165061,27.3424212060917,-54.5113160682993));
#73457=CARTESIAN_POINT('Ctrl Pts',(-26.5715681567657,25.8632721261143,-54.3124291569246));
#73458=CARTESIAN_POINT('Ctrl Pts',(-27.129383902906,22.2586541505862,-54.1135422455495));
#73459=CARTESIAN_POINT('Ctrl Pts',(-24.3982813791998,19.8409055778124,-53.9146553341748));
#73460=CARTESIAN_POINT('Ctrl Pts',(-20.8879122456252,20.8317323548981,-53.7157684227997));
#73461=CARTESIAN_POINT('Ctrl Pts',(-19.8240081057162,24.3206486819583,-53.516881511425));
#73462=CARTESIAN_POINT('Ctrl Pts',(-22.1842066598536,27.1016362657478,-53.31799460005));
#73463=CARTESIAN_POINT('Ctrl Pts',(-25.7996855486223,26.6192033056276,-53.1191076886752));
#73464=CARTESIAN_POINT('Ctrl Pts',(-27.3481262153026,23.3166647883784,-52.9202207773002));
#73465=CARTESIAN_POINT('Ctrl Pts',(-25.4066429733337,20.2287736022619,-52.7213338659254));
#73466=CARTESIAN_POINT('Ctrl Pts',(-21.7592943114516,20.1930399373209,-52.5224469545505));
#73467=CARTESIAN_POINT('Ctrl Pts',(-19.7576844057563,23.2423000019213,-52.3235600431756));
#73468=CARTESIAN_POINT('Ctrl Pts',(-21.2411230510481,26.574542331314,-52.1246731318007));
#73469=CARTESIAN_POINT('Ctrl Pts',(-24.8464559071597,27.1277187523461,-51.9257862204258));
#73470=CARTESIAN_POINT('Ctrl Pts',(-27.2606877611413,24.3935070357146,-51.7268993090509));
#73471=CARTESIAN_POINT('Ctrl Pts',(-26.2653442322895,20.8844159260802,-51.528012397676));
#73472=CARTESIAN_POINT('Ctrl Pts',(-22.7750616324048,19.8250026313341,-51.3291254863012));
#73473=CARTESIAN_POINT('Ctrl Pts',(-19.9971137436173,22.1887781459135,-51.1302385749262));
#73474=CARTESIAN_POINT('Ctrl Pts',(-20.4841991445828,25.8036331870332,-50.9313516635514));
#73475=CARTESIAN_POINT('Ctrl Pts',(-23.7887276498457,27.3478224610695,-50.7324647521764));
#73476=CARTESIAN_POINT('Ctrl Pts',(-26.874117740883,25.4023669508426,-50.5335778408016));
#73477=CARTESIAN_POINT('Ctrl Pts',(-26.9051575219715,21.7549753228249,-50.3346909294266));
#73478=CARTESIAN_POINT('Ctrl Pts',(-23.8533240660305,19.7572912353521,-50.1358040180519));
#73479=CARTESIAN_POINT('Ctrl Pts',(-20.522993566263,21.2450169891325,-49.9369171066769));
#73480=CARTESIAN_POINT('Ctrl Pts',(-19.9744573864931,24.8510587547845,-49.738030195302));
#73481=CARTESIAN_POINT('Ctrl Pts',(-22.7117737677313,27.2617698915965,-49.5391432839272));
#73482=CARTESIAN_POINT('Ctrl Pts',(-26.2195810417756,26.2619112594362,-49.3402563725522));
#73483=CARTESIAN_POINT('Ctrl Pts',(-27.2745017367903,22.770268167227,-49.1413694611774));
#73484=CARTESIAN_POINT('Ctrl Pts',(-24.9071531765824,19.9953645741946,-48.9424825498024));
#73485=CARTESIAN_POINT('Ctrl Pts',(-21.2929279699248,20.4871016093095,-48.7435956384276));
#73486=CARTESIAN_POINT('Ctrl Pts',(-19.752992645972,23.7936146297263,-48.5447087270527));
#73487=CARTESIAN_POINT('Ctrl Pts',(-21.7024172024526,26.8764985157549,-48.3458218156778));
#73488=CARTESIAN_POINT('Ctrl Pts',(-25.3498457559064,26.9028443615838,-48.1469349043029));
#73489=CARTESIAN_POINT('Ctrl Pts',(-27.343600716653,23.8484425686559,-47.948047992928));
#73490=CARTESIAN_POINT('Ctrl Pts',(-25.8515903183102,20.520029414106,-47.7491610815531));
#73491=CARTESIAN_POINT('Ctrl Pts',(-22.2448456153347,19.9761343840675,-47.5502741701782));
#73492=CARTESIAN_POINT('Ctrl Pts',(-19.8376591882389,22.716550896452,-47.3513872588034));
#73493=CARTESIAN_POINT('Ctrl Pts',(-20.8420312677722,26.2230685253821,-47.1525003474284));
#73494=CARTESIAN_POINT('Ctrl Pts',(-24.3350290695526,27.2734948735382,-46.9536134360536));
#73495=CARTESIAN_POINT('Ctrl Pts',(-27.1068837711188,24.9025771884323,-46.7547265246786));
#73496=CARTESIAN_POINT('Ctrl Pts',(-26.6104959162545,21.2889878020069,-46.5558396133039));
#73497=CARTESIAN_POINT('Ctrl Pts',(-23.3020038568303,19.7533089785318,-46.3569527019288));
#73498=CARTESIAN_POINT('Ctrl Pts',(-20.2216312815894,21.706699352688,-46.1580657905541));
#73499=CARTESIAN_POINT('Ctrl Pts',(-20.1999794146531,25.3541587908178,-45.959178879179));
#73500=CARTESIAN_POINT('Ctrl Pts',(-23.2569444859605,27.3439813228416,-45.7602919678043));
#73501=CARTESIAN_POINT('Ctrl Pts',(-26.5834347828758,25.8476887509589,-45.5614050564293));
#73502=CARTESIAN_POINT('Ctrl Pts',(-27.1226877624005,22.240247084041,-45.3625181450545));
#73503=CARTESIAN_POINT('Ctrl Pts',(-24.3791756574643,19.8365893533705,-45.1636312336795));
#73504=CARTESIAN_POINT('Ctrl Pts',(-20.8739534810364,20.8454732168662,-44.9647443223047));
#73505=CARTESIAN_POINT('Ctrl Pts',(-19.8280232194233,24.3398199432207,-44.7658574109297));
#73506=CARTESIAN_POINT('Ctrl Pts',(-22.2025061027852,27.1086211626593,-44.5669704995549));
#73507=CARTESIAN_POINT('Ctrl Pts',(-25.8154536842612,26.6075833101481,-44.3680835881799));
#73508=CARTESIAN_POINT('Ctrl Pts',(-27.3468734639142,23.2971176911406,-44.1691966768052));
#73509=CARTESIAN_POINT('Ctrl Pts',(-25.3895205072279,20.2192615283065,-43.9703097654301));
#73510=CARTESIAN_POINT('Ctrl Pts',(-21.7420362252341,20.2023036761223,-43.7714228540554));
#73511=CARTESIAN_POINT('Ctrl Pts',(-19.7561494174165,23.2618269629562,-43.5725359426803));
#73512=CARTESIAN_POINT('Ctrl Pts',(-21.2567216847247,26.5863888930049,-43.3736490313055));
#73513=CARTESIAN_POINT('Ctrl Pts',(-24.86485434105,27.1209989289215,-43.1747621199306));
#73514=CARTESIAN_POINT('Ctrl Pts',(-27.2649793944301,24.3743957751549,-42.9758752085558));
#73515=CARTESIAN_POINT('Ctrl Pts',(-26.2515854178548,20.8704748564718,-42.7769882971808));
#73516=CARTESIAN_POINT('Ctrl Pts',(-22.7558955541571,19.8290424136397,-42.578101385806));
#73517=CARTESIAN_POINT('Ctrl Pts',(-19.9901524024507,22.207086562711,-42.379214474431));
#73518=CARTESIAN_POINT('Ctrl Pts',(-20.4958394228052,25.8193863555838,-42.1803275630562));
#73519=CARTESIAN_POINT('Ctrl Pts',(-23.8082731187033,27.3465445551235,-41.9814406516812));
#73520=CARTESIAN_POINT('Ctrl Pts',(-26.8836077716783,25.3852322576158,-41.7825537403064));
#73521=CARTESIAN_POINT('Ctrl Pts',(-26.8958715810256,21.7377291726105,-41.5836668289315));
#73522=CARTESIAN_POINT('Ctrl Pts',(-23.8337951457545,19.7557813779647,-41.3847799175566));
#73523=CARTESIAN_POINT('Ctrl Pts',(-20.5111670886113,21.2606308554963,-41.1858930061817));
#73524=CARTESIAN_POINT('Ctrl Pts',(-19.9812008817077,24.8694485255489,-40.9870060948069));
#73525=CARTESIAN_POINT('Ctrl Pts',(-22.7308905354638,27.2660369266243,-40.7881191834319));
#73526=CARTESIAN_POINT('Ctrl Pts',(-26.2335043933146,26.248134515322,-40.5892322720571));
#73527=CARTESIAN_POINT('Ctrl Pts',(-27.270437292577,22.7511073037364,-40.3903453606822));
#73528=CARTESIAN_POINT('Ctrl Pts',(-24.8888358162407,19.9884268003022,-40.1914584493072));
#73529=CARTESIAN_POINT('Ctrl Pts',(-21.2771897945526,20.4987621509962,-39.9925715379324));
#73530=CARTESIAN_POINT('Ctrl Pts',(-19.7542957043592,23.8131584378329,-39.7936846265574));
#73531=CARTESIAN_POINT('Ctrl Pts',(-21.7195640944224,26.8859664876731,-39.5947977151827));
#73532=CARTESIAN_POINT('Ctrl Pts',(-25.3670799415552,26.8935362338724,-39.3959108038077));
#73533=CARTESIAN_POINT('Ctrl Pts',(-27.3450854405875,23.8289117214825,-39.1970238924328));
#73534=CARTESIAN_POINT('Ctrl Pts',(-25.8359612451185,20.5082230400801,-38.9981369810579));
#73535=CARTESIAN_POINT('Ctrl Pts',(-22.2264645381529,19.9829015399035,-38.799250069683));
#73536=CARTESIAN_POINT('Ctrl Pts',(-19.833416758539,22.7356731396968,-38.6003631583082));
#73537=CARTESIAN_POINT('Ctrl Pts',(-20.8558259187495,26.2369741357925,-38.4014762469333));
#73538=CARTESIAN_POINT('Ctrl Pts',(-24.3541846865526,27.2694057741485,-38.2025893355583));
#73539=CARTESIAN_POINT('Ctrl Pts',(-27.1137979662469,24.8842509148831,-38.0037024241835));
#73540=CARTESIAN_POINT('Ctrl Pts',(-26.5988151304152,21.2732646458782,-37.8048155128086));
#73541=CARTESIAN_POINT('Ctrl Pts',(-23.2824617418424,19.7546371872021,-37.6059286014337));
#73542=CARTESIAN_POINT('Ctrl Pts',(-20.2121853842287,21.7238584150028,-37.4070416900588));
#73543=CARTESIAN_POINT('Ctrl Pts',(-20.209309713714,25.3713809833582,-37.2081547786839));
#73544=CARTESIAN_POINT('Ctrl Pts',(-23.276477227685,27.3454409108643,-37.009267867309));
#73545=CARTESIAN_POINT('Ctrl Pts',(-26.5952210337223,25.8320444968236,-36.8103809559342));
#73546=CARTESIAN_POINT('Ctrl Pts',(-27.1158969571505,22.2218747308839,-36.6114940445593));
#73547=CARTESIAN_POINT('Ctrl Pts',(-24.360047970377,19.8323715360244,-36.4126071331843));
#73548=CARTESIAN_POINT('Ctrl Pts',(-20.8600656347848,20.8592857518602,-36.2137202218095));
#73549=CARTESIAN_POINT('Ctrl Pts',(-19.8321369672173,24.358970282005,-36.0148333104345));
#73550=CARTESIAN_POINT('Ctrl Pts',(-22.2208412591905,27.1155117675722,-35.8159463990597));
#73551=CARTESIAN_POINT('Ctrl Pts',(-25.8311617951063,26.5958822995014,-35.6170594876848));
#73552=CARTESIAN_POINT('Ctrl Pts',(-27.3455201071605,23.2775773016365,-35.4181725763099));
#73553=CARTESIAN_POINT('Ctrl Pts',(-25.3723493029866,20.2098377211476,-35.219285664935));
#73554=CARTESIAN_POINT('Ctrl Pts',(-21.7248260543247,20.2116561310803,-35.0203987535601));
#73555=CARTESIAN_POINT('Ctrl Pts',(-19.7547149677231,23.2813615668823,-34.8215118421852));
#73556=CARTESIAN_POINT('Ctrl Pts',(-21.2723810938942,26.5981550011522,-34.6226249308104));
#73557=CARTESIAN_POINT('Ctrl Pts',(-24.8832179397545,27.1141844855041,-34.4237380194354));
#73558=CARTESIAN_POINT('Ctrl Pts',(-27.2691725924367,24.3552626759039,-34.2248511080606));
#73559=CARTESIAN_POINT('Ctrl Pts',(-26.23775502172,20.8566047973795,-34.0259641966856));
#73560=CARTESIAN_POINT('Ctrl Pts',(-22.7367505253045,19.8331808030248,-33.8270772853108));
#73561=CARTESIAN_POINT('Ctrl Pts',(-19.9832853991652,22.2254305716062,-33.6281903739359));
#73562=CARTESIAN_POINT('Ctrl Pts',(-20.5075606388801,25.8350793951297,-33.429303462561));
#73563=CARTESIAN_POINT('Ctrl Pts',(-23.8278117503613,27.3451660525278,-33.2304165511861));
#73564=CARTESIAN_POINT('Ctrl Pts',(-26.8930094730282,25.3680489398862,-33.0315296398112));
#73565=CARTESIAN_POINT('Ctrl Pts',(-26.8864969856598,21.7205310518353,-32.8326427284363));
#73566=CARTESIAN_POINT('Ctrl Pts',(-23.8142587119796,19.7543720689762,-32.6337558170614));
#73567=CARTESIAN_POINT('Ctrl Pts',(-20.4994211426499,21.2763053937652,-32.4348689056866));
#73568=CARTESIAN_POINT('Ctrl Pts',(-19.9880389520064,24.8878033393877,-32.2359819943116));
#73569=CARTESIAN_POINT('Ctrl Pts',(-22.750029015191,27.2702054983469,-32.0370950829368));
#73570=CARTESIAN_POINT('Ctrl Pts',(-26.2473566422763,26.2342862809518,-31.8382081715618));
#73571=CARTESIAN_POINT('Ctrl Pts',(-27.2662742684546,22.7319676165231,-31.639321260187));
#73572=CARTESIAN_POINT('Ctrl Pts',(-24.8704829852364,19.9815834100169,-31.4404343488121));
#73573=CARTESIAN_POINT('Ctrl Pts',(-21.2615118522959,20.5105035530874,-31.2415474374372));
#73574=CARTESIAN_POINT('Ctrl Pts',(-19.7556993505138,23.8326952792856,-31.0426605260623));
#73575=CARTESIAN_POINT('Ctrl Pts',(-21.7367594971816,26.8953460676431,-30.8437736146875));
#73576=CARTESIAN_POINT('Ctrl Pts',(-25.3842659837132,26.8841395136247,-30.6448867033125));
#73577=CARTESIAN_POINT('Ctrl Pts',(-27.3464696065371,23.8093734902142,-30.4459997919377));
#73578=CARTESIAN_POINT('Ctrl Pts',(-25.8202716037099,20.496497275758,-30.2471128805627));
#73579=CARTESIAN_POINT('Ctrl Pts',(-22.2081185395785,19.9897632257587,-30.0482259691879));
#73580=CARTESIAN_POINT('Ctrl Pts',(-19.8292728200044,22.7548169682034,-29.849339057813));
#73581=CARTESIAN_POINT('Ctrl Pts',(-20.86969196842,26.250808551682,-29.6504521464381));
#73582=CARTESIAN_POINT('Ctrl Pts',(-24.3733190004281,27.2652181221834,-29.4515652350632));
#73583=CARTESIAN_POINT('Ctrl Pts',(-27.1206177321983,24.865889292165,-29.2526783236883));
#73584=CARTESIAN_POINT('Ctrl Pts',(-26.5870535617536,21.2576018268762,-29.0537914123134));
#73585=CARTESIAN_POINT('Ctrl Pts',(-23.2629267229515,19.7560659745909,-28.8549045009385));
#73586=CARTESIAN_POINT('Ctrl Pts',(-20.2028279411726,21.7410658743133,-28.6560175895637));
#73587=CARTESIAN_POINT('Ctrl Pts',(-20.2187285432812,25.3885549184361,-28.4571306781887));
#73588=CARTESIAN_POINT('Ctrl Pts',(-23.2960172240878,27.3467999314825,-28.2582437668139));
#73589=CARTESIAN_POINT('Ctrl Pts',(-26.6069265969855,25.81633977826,-28.0593568554389));
#73590=CARTESIAN_POINT('Ctrl Pts',(-27.109011667103,22.2035375779578,-27.8604699440641));
#73591=CARTESIAN_POINT('Ctrl Pts',(-24.3408988247963,19.8282522375408,-27.6615830326892));
#73592=CARTESIAN_POINT('Ctrl Pts',(-20.8462490748795,20.8731695938664,-27.4626961213143));
#73593=CARTESIAN_POINT('Ctrl Pts',(-19.8363492400895,24.3780991908532,-27.2638092099394));
#73594=CARTESIAN_POINT('Ctrl Pts',(-22.2392116432122,27.1223078978946,-27.0649222985645));
#73595=CARTESIAN_POINT('Ctrl Pts',(-25.8468094649135,26.5841005837488,-26.8660353871896));
#73596=CARTESIAN_POINT('Ctrl Pts',(-27.3440661809039,23.2580441376607,-26.6671484758148));
#73597=CARTESIAN_POINT('Ctrl Pts',(-25.3551298156233,20.2005024305031,-26.4682615644398));
#73598=CARTESIAN_POINT('Ctrl Pts',(-21.70766425477,20.2210970543674,-26.269374653065));
#73599=CARTESIAN_POINT('Ctrl Pts',(-19.753381094687,23.3009032960584,-26.0704877416901));
#73600=CARTESIAN_POINT('Ctrl Pts',(-21.2881008636032,26.6098403439699,-25.8716008303151));
#73601=CARTESIAN_POINT('Ctrl Pts',(-24.9015462166627,27.1072756026676,-25.6727139189403));
#73602=CARTESIAN_POINT('Ctrl Pts',(-27.2732672440469,24.3361082449633,-25.4738270075654));
#73603=CARTESIAN_POINT('Ctrl Pts',(-26.223853410372,20.8428061163415,-25.2749400961905));
#73604=CARTESIAN_POINT('Ctrl Pts',(-22.7176270531645,19.8374176898278,-25.0760531848156));
#73605=CARTESIAN_POINT('Ctrl Pts',(-19.976512915727,22.2438096865073,-24.8771662734407));
#73606=CARTESIAN_POINT('Ctrl Pts',(-20.5193624822115,25.8507118898268,-24.6782793620658));
#73607=CARTESIAN_POINT('Ctrl Pts',(-23.8473430270719,27.3436869898112,-24.4793924506909));
#73608=CARTESIAN_POINT('Ctrl Pts',(-26.9023225958004,25.3508174529887,-24.2805055393161));
#73609=CARTESIAN_POINT('Ctrl Pts',(-26.8770339842884,21.7033814162266,-24.0816186279412));
#73610=CARTESIAN_POINT('Ctrl Pts',(-23.7947152823949,19.7530633457313,-23.8827317165663));
#73611=CARTESIAN_POINT('Ctrl Pts',(-20.4877560396305,21.2920401885848,-23.6838448051914));
#73612=CARTESIAN_POINT('Ctrl Pts',(-19.9949714161898,24.9061227099231,-23.4849578938165));
#73613=CARTESIAN_POINT('Ctrl Pts',(-22.7691886997684,27.2742754963025,-23.2860709824416));
#73614=CARTESIAN_POINT('Ctrl Pts',(-26.2611374215946,26.2203669232854,-23.0871840710667));
#73615=CARTESIAN_POINT('Ctrl Pts',(-27.2620127747377,22.712849612763,-22.8882971596918));
#73616=CARTESIAN_POINT('Ctrl Pts',(-24.8520951698951,19.9748345846794,-22.6894102483169));
#73617=CARTESIAN_POINT('Ctrl Pts',(-21.2458945585992,20.5223255044515,-22.4905233369421));
#73618=CARTESIAN_POINT('Ctrl Pts',(-19.7572035472408,23.8522246363839,-22.2916364255671));
#73619=CARTESIAN_POINT('Ctrl Pts',(-21.7540029550752,26.9046370071187,-22.0927495141923));
#73620=CARTESIAN_POINT('Ctrl Pts',(-25.4014034269733,26.8746544498414,-21.8938626028174));
#73621=CARTESIAN_POINT('Ctrl Pts',(-27.3477531778232,23.7898283925879,-21.6949756914425));
#73622=CARTESIAN_POINT('Ctrl Pts',(-25.8045218098391,20.4848524318565,-21.4960887800676));
#73623=CARTESIAN_POINT('Ctrl Pts',(-22.1898081057556,19.9967192598074,-21.2972018686927));
#73624=CARTESIAN_POINT('Ctrl Pts',(-19.8252274824439,22.773981874686,-21.0983149573178));
#73625=CARTESIAN_POINT('Ctrl Pts',(-20.883629049352,26.2645714064571,-20.8994280459429));
#73626=CARTESIAN_POINT('Ctrl Pts',(-24.3924315041455,27.2609320286103,-20.700541134568));
#73627=CARTESIAN_POINT('Ctrl Pts',(-27.1273428882579,24.8474928068367,-20.5016542231931));
#73628=CARTESIAN_POINT('Ctrl Pts',(-26.575211521936,21.2419997600445,-20.3027673118182));
#73629=CARTESIAN_POINT('Ctrl Pts',(-23.2433993178095,19.7575953028371,-20.1038804004434));
#73630=CARTESIAN_POINT('Ctrl Pts',(-20.1935592003809,21.7583212746448,-19.9049934890685));
#73631=CARTESIAN_POINT('Ctrl Pts',(-20.2282356537676,25.405680140965,-19.7061065776936));
#73632=CARTESIAN_POINT('Ctrl Pts',(-23.3155639573856,27.348058348684,-19.5072196663187));
#73633=CARTESIAN_POINT('Ctrl Pts',(-26.6185511624836,25.8005750114223,-19.3083327549438));
#73634=CARTESIAN_POINT('Ctrl Pts',(-27.1020320747092,22.1852361111728,-19.1094458435689));
#73635=CARTESIAN_POINT('Ctrl Pts',(-24.3217287281487,19.8242315670756,-18.910558932194));
#73636=CARTESIAN_POINT('Ctrl Pts',(-20.8325041674413,20.8871243749818,-18.7116720208192));
#73637=CARTESIAN_POINT('Ctrl Pts',(-19.8406599264202,24.3972061628746,-18.5127851094442));
#73638=CARTESIAN_POINT('Ctrl Pts',(-22.25761676806,27.1290093735385,-18.3138981980694));
#73639=CARTESIAN_POINT('Ctrl Pts',(-25.8623962790404,26.5722384750899,-18.1150112866944));
#73640=CARTESIAN_POINT('Ctrl Pts',(-27.3425117236713,23.2385187168156,-17.9161243753196));
#73641=CARTESIAN_POINT('Ctrl Pts',(-25.3378625014317,20.1912559037459,-17.7172374639446));
#73642=CARTESIAN_POINT('Ctrl Pts',(-21.6905512813346,20.2306261958117,-17.5183505525698));
#73643=CARTESIAN_POINT('Ctrl Pts',(-19.7521478336541,23.320451632655,-17.3194636411949));
#73644=CARTESIAN_POINT('Ctrl Pts',(-21.3038805772987,26.6214446118121,-17.12057672982));
#73645=CARTESIAN_POINT('Ctrl Pts',(-24.9198386860995,27.1002724634881,-16.9216898184451));
#73646=CARTESIAN_POINT('Ctrl Pts',(-27.2772632407584,24.3169329898997,-16.7228029070702));
#73647=CARTESIAN_POINT('Ctrl Pts',(-26.2098809521846,20.8290791790038,-16.5239159956953));
#73648=CARTESIAN_POINT('Ctrl Pts',(-22.6985256444836,19.841752961777,-16.3250290843204));
#73649=CARTESIAN_POINT('Ctrl Pts',(-19.9698351315979,22.2622234203925,-16.1261421729455));
#73650=CARTESIAN_POINT('Ctrl Pts',(-20.531244640066,25.8662834254346,-15.9272552615707));
#73651=CARTESIAN_POINT('Ctrl Pts',(-23.8668664312827,27.3421074061667,-15.7283683501957));
#73652=CARTESIAN_POINT('Ctrl Pts',(-26.9115468932093,25.3335382535345,-15.5294814388209));
#73653=CARTESIAN_POINT('Ctrl Pts',(-26.8674828276681,21.6862807202267,-15.330594527446));
#73654=CARTESIAN_POINT('Ctrl Pts',(-23.7751653748748,19.7518552429097,-15.1317076160711));
#73655=CARTESIAN_POINT('Ctrl Pts',(-20.4761720886628,21.3078348230044,-14.9328207046962));
#73656=CARTESIAN_POINT('Ctrl Pts',(-20.0019980905566,24.9244061517165,-14.7339337933213));
#73657=CARTESIAN_POINT('Ctrl Pts',(-22.7883690814905,27.2782468126418,-14.5350468819464));
#73658=CARTESIAN_POINT('Ctrl Pts',(-26.2748463660975,26.2063768111669,-14.3361599705715));
#73659=CARTESIAN_POINT('Ctrl Pts',(-27.2576529243502,22.6937537990577,-14.1372730591966));
#73660=CARTESIAN_POINT('Ctrl Pts',(-24.8336728574687,19.9681805031243,-13.9383861478217));
#73661=CARTESIAN_POINT('Ctrl Pts',(-21.2303383272995,20.5342276918229,-13.7394992364469));
#73662=CARTESIAN_POINT('Ctrl Pts',(-19.7588082546812,23.8717459916262,-13.540612325072));
#73663=CARTESIAN_POINT('Ctrl Pts',(-21.7712940111747,26.9138390599026,-13.3417254136971));
#73664=CARTESIAN_POINT('Ctrl Pts',(-25.4184918172162,26.8650812938635,-13.1428385023222));
#73665=CARTESIAN_POINT('Ctrl Pts',(-27.3489361204329,23.7702769465225,-12.9439515909473));
#73666=CARTESIAN_POINT('Ctrl Pts',(-25.7887122808542,20.4732888169482,-12.7450646795724));
#73667=CARTESIAN_POINT('Ctrl Pts',(-22.1715337218863,20.0037694577242,-12.5461777681975));
#73668=CARTESIAN_POINT('Ctrl Pts',(-19.8212808530538,22.7931673513006,-12.3472908568226));
#73669=CARTESIAN_POINT('Ctrl Pts',(-20.8976367922315,26.2782623354208,-12.1484039454477));
#73670=CARTESIAN_POINT('Ctrl Pts',(-24.4115216912494,27.2565476070049,-11.9495170340728));
#73671=CARTESIAN_POINT('Ctrl Pts',(-27.1339732562184,24.8290619463798,-11.750630122698));
#73672=CARTESIAN_POINT('Ctrl Pts',(-26.56328932476,21.2264588588168,-11.551743211323));
#73673=CARTESIAN_POINT('Ctrl Pts',(-23.2238800438662,19.7592251314157,-11.3528562999482));
#73674=CARTESIAN_POINT('Ctrl Pts',(-20.1843794074626,21.7756241587528,-11.1539693885733));
#73675=CARTESIAN_POINT('Ctrl Pts',(-20.2378307932482,25.4227561971494,-10.9550824771984));
#73676=CARTESIAN_POINT('Ctrl Pts',(-23.335116909616,27.3492161291226,-10.7561955658235));
#73677=CARTESIAN_POINT('Ctrl Pts',(-26.630094422181,25.7847506140553,-10.5573086544486));
#73678=CARTESIAN_POINT('Ctrl Pts',(-27.0949583649188,22.1669708154931,-10.3584217430737));
#73679=CARTESIAN_POINT('Ctrl Pts',(-24.3025381884162,19.8203096311709,-10.1595348316988));
#73680=CARTESIAN_POINT('Ctrl Pts',(-20.8188312766913,20.9011497254233,-9.96064792032392));
#73681=CARTESIAN_POINT('Ctrl Pts',(-19.8450689119821,24.4162906917602,-9.76176100894904));
#73682=CARTESIAN_POINT('Ctrl Pts',(-22.2760561460228,27.1356160169234,-9.56287409757416));
#73683=CARTESIAN_POINT('Ctrl Pts',(-25.8779218244577,26.5602962878544,-9.36398718619925));
#73684=CARTESIAN_POINT('Ctrl Pts',(-27.3408567766537,23.2190015564985,-9.16510027482437));
#73685=CARTESIAN_POINT('Ctrl Pts',(-25.3205478179721,20.1820983858963,-8.96621336344948));
#73686=CARTESIAN_POINT('Ctrl Pts',(-21.6734875874893,20.2402433029038,-8.76732645207459));
#73687=CARTESIAN_POINT('Ctrl Pts',(-19.7510152173042,23.3400060586673,-8.56843954069969));
#73688=CARTESIAN_POINT('Ctrl Pts',(-21.3197198168398,26.6329674971811,-8.36955262932482));
#73689=CARTESIAN_POINT('Ctrl Pts',(-24.9380948633393,27.0931752535394,-8.17066571794991));
#73690=CARTESIAN_POINT('Ctrl Pts',(-27.2811604766821,24.2977374188318,-7.97177880657503));
#73691=CARTESIAN_POINT('Ctrl Pts',(-26.1958380174094,20.8154243491121,-7.77289189520014));
#73692=CARTESIAN_POINT('Ctrl Pts',(-22.6794468054235,19.8461865039934,-7.57400498382525));
#73693=CARTESIAN_POINT('Ctrl Pts',(-19.96325222373,22.2806712853224,-7.37511807245035));
#73694=CARTESIAN_POINT('Ctrl Pts',(-20.5432067975827,25.8817935893286,-7.17623116107547));
#73695=CARTESIAN_POINT('Ctrl Pts',(-23.8863814456496,27.340427343451,-6.97734424970057));
#73696=CARTESIAN_POINT('Ctrl Pts',(-26.9206821208237,25.3162117993992,-6.77845733832569));
#73697=CARTESIAN_POINT('Ctrl Pts',(-26.8578437688918,21.6692294169808,-6.57957042695078));
#73698=CARTESIAN_POINT('Ctrl Pts',(-23.755609507466,19.7507477925242,-6.38068351557592));
#73699=CARTESIAN_POINT('Ctrl Pts',(-20.4646695967059,21.3236888784871,-6.18179660420101));
#73700=CARTESIAN_POINT('Ctrl Pts',(-20.0091187889095,24.942653180281,-5.98290969282612));
#73701=CARTESIAN_POINT('Ctrl Pts',(-22.8075696521026,27.2821193421303,-5.78402278145123));
#73702=CARTESIAN_POINT('Ctrl Pts',(-26.2884831125161,26.1923163153157,-5.58513587007634));
#73703=CARTESIAN_POINT('Ctrl Pts',(-27.253194832822,22.6746806814207,-5.38624895870145));
#73704=CARTESIAN_POINT('Ctrl Pts',(-24.8152165361243,19.9616213416763,-5.18736204732655));
#73705=CARTESIAN_POINT('Ctrl Pts',(-21.2148435706164,20.5462097998092,-4.98847513595167));
#73706=CARTESIAN_POINT('Ctrl Pts',(-19.7605134303124,23.891258827723,-4.78958822457678));
#73707=CARTESIAN_POINT('Ctrl Pts',(-21.7886322072903,26.9229519821522,-4.59070131320189));
#73708=CARTESIAN_POINT('Ctrl Pts',(-25.4355307016224,26.8554202993672,-4.39181440182699));
#73709=CARTESIAN_POINT('Ctrl Pts',(-27.3500184030198,23.7507196701049,-4.19292749045211));
#73710=CARTESIAN_POINT('Ctrl Pts',(-25.7728434356868,20.4618067374535,-3.99404057907722));
#73711=CARTESIAN_POINT('Ctrl Pts',(-22.1532958722172,20.0109136326883,-3.79515366770233));
#73712=CARTESIAN_POINT('Ctrl Pts',(-19.8174330364143,22.8123728896575,-3.59626675632743));
#73713=CARTESIAN_POINT('Ctrl Pts',(-20.9117148258723,26.2918809757817,-3.39737984495255));
#73714=CARTESIAN_POINT('Ctrl Pts',(-24.4305890558748,27.2520649735484,-3.19849293357766));
#73715=CARTESIAN_POINT('Ctrl Pts',(-27.1405086603839,24.8105971991879,-2.99960602220276));
#73716=CARTESIAN_POINT('Ctrl Pts',(-26.5512872861481,21.2109795350063,-2.80071911082788));
#73717=CARTESIAN_POINT('Ctrl Pts',(-23.2043694183563,19.7609554171384,-2.60183219945298));
#73718=CARTESIAN_POINT('Ctrl Pts',(-20.17528880567,21.7929740681333,-2.40294528807809));
#73719=CARTESIAN_POINT('Ctrl Pts',(-20.2475137074644,25.4397826344972,-2.2040583767032));
#73720=CARTESIAN_POINT('Ctrl Pts',(-23.3546755626521,27.3502732421183,-2.00517146532831));
#73721=CARTESIAN_POINT('Ctrl Pts',(-26.641556070197,25.7688670054847,-1.80628455395342));
#73722=CARTESIAN_POINT('Ctrl Pts',(-27.0877907251756,22.1487421749243,-1.60739764257854));
#73723=CARTESIAN_POINT('Ctrl Pts',(-24.2833277141221,19.8164865337531,-1.40851073120364));
#73724=CARTESIAN_POINT('Ctrl Pts',(-20.805230764943,20.915245273538,-1.20962381982875));
#73725=CARTESIAN_POINT('Ctrl Pts',(-19.8495760799429,24.4353522717955,-1.01073690845387));
#73726=CARTESIAN_POINT('Ctrl Pts',(-22.2945292884817,27.1421276529823,-0.811849997078973));
#73727=CARTESIAN_POINT('Ctrl Pts',(-25.893385689759,26.5482743384945,-0.612963085704084));
#73728=CARTESIAN_POINT('Ctrl Pts',(-27.3391013837051,23.1994931738883,-0.414076174329188));
#73729=CARTESIAN_POINT('Ctrl Pts',(-25.3031862240606,20.1730301196165,-0.215189262954304));
#73730=CARTESIAN_POINT('Ctrl Pts',(-21.6564736253991,20.2499481208034,-0.0163023515794102));
#73731=CARTESIAN_POINT('Ctrl Pts',(-19.7499832756501,23.3595660559294,0.182584559795477));
#73732=CARTESIAN_POINT('Ctrl Pts',(-21.3356181625077,26.6444086947362,0.381471471170368));
#73733=CARTESIAN_POINT('Ctrl Pts',(-24.9563142646179,27.0859841608879,0.580358382545258));
#73734=CARTESIAN_POINT('Ctrl Pts',(-27.2849588485467,24.2785220404165,0.779245293920151));
#73735=CARTESIAN_POINT('Ctrl Pts',(-26.1817249781655,20.801841988501,0.97813220529504));
#73736=CARTESIAN_POINT('Ctrl Pts',(-22.6603910415476,19.850718198994,1.17701911666993));
#73737=CARTESIAN_POINT('Ctrl Pts',(-19.956764366562,22.2991527924536,1.37590602804482));
#73738=CARTESIAN_POINT('Ctrl Pts',(-20.5552486377801,25.89724197051,1.57479293941972));
#73739=CARTESIAN_POINT('Ctrl Pts',(-23.9058875530509,27.3386468461839,1.7736798507946));
#73740=CARTESIAN_POINT('Ctrl Pts',(-26.9297280365722,25.2988385497105,1.9725667621695));
#73741=CARTESIAN_POINT('Ctrl Pts',(-26.8481170633818,21.652227958326,2.17145367354438));
#73742=CARTESIAN_POINT('Ctrl Pts',(-23.7360481983725,19.7497410239209,2.3703405849193));
#73743=CARTESIAN_POINT('Ctrl Pts',(-20.4532488685604,21.3396019349219,2.56922749629416));
#73744=CARTESIAN_POINT('Ctrl Pts',(-20.0163333225597,24.960863312095,2.76811440766907));
#73745=CARTESIAN_POINT('Ctrl Pts',(-22.8267899028154,27.285892982151,2.96700131904394));
#73746=CARTESIAN_POINT('Ctrl Pts',(-26.3020472994952,26.178185808316,3.16588823041884));
#73747=CARTESIAN_POINT('Ctrl Pts',(-27.2486386182868,22.655630765264,3.36477514179371));
#73748=CARTESIAN_POINT('Ctrl Pts',(-24.7967266949296,19.9551572741439,3.56366205316864));
#73749=CARTESIAN_POINT('Ctrl Pts',(-21.1994106991399,20.5582715109011,3.7625489645435));
#73750=CARTESIAN_POINT('Ctrl Pts',(-19.7623190289495,23.9107626276099,3.9614358759184));
#73751=CARTESIAN_POINT('Ctrl Pts',(-21.8060170839828,26.9319755323878,4.16032278729329));
#73752=CARTESIAN_POINT('Ctrl Pts',(-25.4525196286846,26.8456717223558,4.35920969866818));
#73753=CARTESIAN_POINT('Ctrl Pts',(-27.3509999969048,23.7311570815769,4.55809661004306));
#73754=CARTESIAN_POINT('Ctrl Pts',(-25.7569156948398,20.4504064976324,4.75698352141796));
#73755=CARTESIAN_POINT('Ctrl Pts',(-22.1350950400269,20.0181515953885,4.95587043279287));
#73756=CARTESIAN_POINT('Ctrl Pts',(-19.8136841344875,22.8315979808357,5.15475734416772));
#73757=CARTESIAN_POINT('Ctrl Pts',(-20.9258627772252,26.305426966664,5.35364425554262));
#73758=CARTESIAN_POINT('Ctrl Pts',(-24.4496330927626,27.2474842470246,5.55253116691751));
#73759=CARTESIAN_POINT('Ctrl Pts',(-27.1469489275747,24.7920990545517,5.75141807829239));
#73760=CARTESIAN_POINT('Ctrl Pts',(-26.5392057241383,21.1955621987944,5.95030498966732));
#73761=CARTESIAN_POINT('Ctrl Pts',(-23.1848679582852,19.7627861141549,6.1491919010422));
#73762=CARTESIAN_POINT('Ctrl Pts',(-20.1662876358919,21.8103705430376,6.34807881241708));
#73763=CARTESIAN_POINT('Ctrl Pts',(-20.257284139832,25.45675900183,6.54696572379196));
#73764=CARTESIAN_POINT('Ctrl Pts',(-23.3742393982156,27.3512296596596,6.74585263516687));
#73765=CARTESIAN_POINT('Ctrl Pts',(-26.6529358028134,25.7529246066046,6.94473954654172));
#73766=CARTESIAN_POINT('Ctrl Pts',(-27.0805293454125,22.1305506725013,7.14362645791667));
#73767=CARTESIAN_POINT('Ctrl Pts',(-24.2640978143184,19.8127623761288,7.34251336929153));
#73768=CARTESIAN_POINT('Ctrl Pts',(-20.7917029925916,20.9294106458127,7.54140028066643));
#73769=CARTESIAN_POINT('Ctrl Pts',(-19.854181310869,24.4543903978741,7.7402871920413));
#73770=CARTESIAN_POINT('Ctrl Pts',(-22.3130357059231,27.1485441091656,7.93917410341621));
#73771=CARTESIAN_POINT('Ctrl Pts',(-25.9087874651727,26.5361729455757,8.13806101479108));
#73772=CARTESIAN_POINT('Ctrl Pts',(-27.3372455913412,23.1799940859308,8.336947926166));
#73773=CARTESIAN_POINT('Ctrl Pts',(-25.2857781797561,20.1640513452033,8.53583483754088));
#73774=CARTESIAN_POINT('Ctrl Pts',(-21.6395098459112,20.2597403923456,8.73472174891577));
#73775=CARTESIAN_POINT('Ctrl Pts',(-19.7490520360368,23.3791311061275,8.93360866029067));
#73776=CARTESIAN_POINT('Ctrl Pts',(-21.3515751930175,26.6557679013008,9.13249557166553));
#73777=CARTESIAN_POINT('Ctrl Pts',(-24.9744964071453,27.078699376088,9.33138248304043));
#73778=CARTESIAN_POINT('Ctrl Pts',(-27.2886582557006,24.2592873638354,9.5302693944153));
#73779=CARTESIAN_POINT('Ctrl Pts',(-26.1675422084293,20.788332457085,9.72915630579023));
#73780=CARTESIAN_POINT('Ctrl Pts',(-22.6413588578084,19.8553479266951,9.9280432171651));
#73781=CARTESIAN_POINT('Ctrl Pts',(-19.950371732013,22.3176674520504,10.12693012854));
#73782=CARTESIAN_POINT('Ctrl Pts',(-20.567369841566,25.9126281596176,10.3258170399149));
#73783=CARTESIAN_POINT('Ctrl Pts',(-23.9253842366009,27.3367659615458,10.5247039512898));
#73784=CARTESIAN_POINT('Ctrl Pts',(-26.9386844007501,25.2814189648366,10.7235908626646));
#73785=CARTESIAN_POINT('Ctrl Pts',(-26.8383029688828,21.635276794778,10.9224777740396));
#73786=CARTESIAN_POINT('Ctrl Pts',(-23.7164819659429,19.7488349637779,11.1213646854144));
#73787=CARTESIAN_POINT('Ctrl Pts',(-20.4419102068603,21.355573570634,11.3202515967893));
#73788=CARTESIAN_POINT('Ctrl Pts',(-20.0236415003314,24.9790360646143,11.5191385081642));
#73789=CARTESIAN_POINT('Ctrl Pts',(-22.8460293243181,27.2895676327074,11.7180254195391));
#73790=CARTESIAN_POINT('Ctrl Pts',(-26.3155385676017,26.1639856646073,11.916912330914));
#73791=CARTESIAN_POINT('Ctrl Pts',(-27.2439844014783,22.6366045553847,12.1157992422889));
#73792=CARTESIAN_POINT('Ctrl Pts',(-24.7782038238405,19.9487884718166,12.3146861536638));
#73793=CARTESIAN_POINT('Ctrl Pts',(-21.1840401218207,20.5704125054791,12.5135730650387));
#73794=CARTESIAN_POINT('Ctrl Pts',(-19.7642250027464,23.9302568744627,12.7124599764136));
#73795=CARTESIAN_POINT('Ctrl Pts',(-21.8234481805766,26.9409094714972,12.9113468877884));
#73796=CARTESIAN_POINT('Ctrl Pts',(-25.4694581482187,26.8358358211533,13.1102337991634));
#73797=CARTESIAN_POINT('Ctrl Pts',(-27.351880876077,23.7115896993209,13.3091207105382));
#73798=CARTESIAN_POINT('Ctrl Pts',(-25.7409294803771,20.4390883995754,13.5080076219132));
#73799=CARTESIAN_POINT('Ctrl Pts',(-22.116931707613,20.0254831540288,13.706894533288));
#73800=CARTESIAN_POINT('Ctrl Pts',(-19.8100342466141,22.8508421153961,13.9057814446629));
#73801=CARTESIAN_POINT('Ctrl Pts',(-20.9400802713885,26.3188999491173,14.1046683560378));
#73802=CARTESIAN_POINT('Ctrl Pts',(-24.4686532972713,27.2428055488167,14.3035552674127));
#73803=CARTESIAN_POINT('Ctrl Pts',(-27.1532938871325,24.7735680026474,14.5024421787876));
#73804=CARTESIAN_POINT('Ctrl Pts',(-26.5270449588757,21.1802072587197,14.7013290901624));
#73805=CARTESIAN_POINT('Ctrl Pts',(-23.1653761804155,19.7647171739542,14.9002160015374));
#73806=CARTESIAN_POINT('Ctrl Pts',(-20.1573761366472,21.8278131224823,15.0991029129122));
#73807=CARTESIAN_POINT('Ctrl Pts',(-20.2671418314476,25.4736848492971,15.2979898242872));
#73808=CARTESIAN_POINT('Ctrl Pts',(-23.3938078978913,27.3520853564023,15.496876735662));
#73809=CARTESIAN_POINT('Ctrl Pts',(-26.6642333184823,25.7369238398673,15.6957636470369));
#73810=CARTESIAN_POINT('Ctrl Pts',(-27.0731744180464,22.1123967902745,15.8946505584118));
#73811=CARTESIAN_POINT('Ctrl Pts',(-24.2448489985717,19.8091372569833,16.0935374697867));
#73812=CARTESIAN_POINT('Ctrl Pts',(-20.7782483181051,20.943645466884,16.2924243811616));
#73813=CARTESIAN_POINT('Ctrl Pts',(-19.8588844827275,24.4734045655114,16.4913112925365));
#73814=CARTESIAN_POINT('Ctrl Pts',(-22.3315749079519,27.1548652154458,16.6901982039114));
#73815=CARTESIAN_POINT('Ctrl Pts',(-25.9241267425724,26.5239924297687,16.8890851152863));
#73816=CARTESIAN_POINT('Ctrl Pts',(-27.3352894487376,23.160504809326,17.0879720266612));
#73817=CARTESIAN_POINT('Ctrl Pts',(-25.2683241463485,20.1551623005822,17.286858938036));
#73818=CARTESIAN_POINT('Ctrl Pts',(-21.622596698543,20.2696198580485,17.485745849411));
#73819=CARTESIAN_POINT('Ctrl Pts',(-19.7482215231412,23.3987006908139,17.6846327607858));
#73820=CARTESIAN_POINT('Ctrl Pts',(-21.3675904855294,26.6670448158712,17.8835196721607));
#73821=CARTESIAN_POINT('Ctrl Pts',(-24.9926408091195,27.0713210921768,18.0824065835356));
#73822=CARTESIAN_POINT('Ctrl Pts',(-27.2922586001142,24.2400338987816,18.2812934949105));
#73823=CARTESIAN_POINT('Ctrl Pts',(-26.1532900840252,20.7748961128486,18.4801804062854));
#73824=CARTESIAN_POINT('Ctrl Pts',(-22.622350758533,19.860075564415,18.6790673176603));
#73825=CARTESIAN_POINT('Ctrl Pts',(-19.9440744894795,22.3362147734999,18.8779542290352));
#73826=CARTESIAN_POINT('Ctrl Pts',(-20.5795700877444,25.9279517489378,19.0768411404101));
#73827=CARTESIAN_POINT('Ctrl Pts',(-23.9448709796636,27.334784739378,19.275728051785));
#73828=CARTESIAN_POINT('Ctrl Pts',(-26.9475509760259,25.2639535063728,19.4746149631598));
#73829=CARTESIAN_POINT('Ctrl Pts',(-26.8284017454547,21.61837637552,19.6735018745347));
#73830=CARTESIAN_POINT('Ctrl Pts',(-23.6969113286562,19.7480296361044,19.8723887859096));
#73831=CARTESIAN_POINT('Ctrl Pts',(-20.4306539120651,21.3716033623966,20.0712756972845));
#73832=CARTESIAN_POINT('Ctrl Pts',(-20.031043128568,24.9971709562853,20.2701626086594));
#73833=CARTESIAN_POINT('Ctrl Pts',(-22.8652874067917,27.2931431964264,20.4690495200343));
#73834=CARTESIAN_POINT('Ctrl Pts',(-26.3289565593354,26.1497162604744,20.6679364314092));
#73835=CARTESIAN_POINT('Ctrl Pts',(-27.2392323057267,22.6176025559519,20.8668233427841));
#73836=CARTESIAN_POINT('Ctrl Pts',(-24.7596484136882,19.9425151034591,21.065710254159));
#73837=CARTESIAN_POINT('Ctrl Pts',(-21.1687322459583,20.582632461823,21.2645971655339));
#73838=CARTESIAN_POINT('Ctrl Pts',(-19.7662313011976,23.9497410517098,21.4634840769087));
#73839=CARTESIAN_POINT('Ctrl Pts',(-21.8409250351707,26.9497535627429,21.6623709882836));
#73840=CARTESIAN_POINT('Ctrl Pts',(-25.4863458113769,26.8259128563984,21.8612578996585));
#73841=CARTESIAN_POINT('Ctrl Pts',(-27.3526610171945,23.6920180418461,22.0601448110334));
#73842=CARTESIAN_POINT('Ctrl Pts',(-25.7248852159121,20.4278527431975,22.2590317224083));
#73843=CARTESIAN_POINT('Ctrl Pts',(-22.0988063562796,20.032908114332,22.4579186337832));
#73844=CARTESIAN_POINT('Ctrl Pts',(-19.8064834695114,22.8701047833953,22.6568055451581));
#73845=CARTESIAN_POINT('Ctrl Pts',(-20.9543669316176,26.3322995661252,22.8556924565329));
#73846=CARTESIAN_POINT('Ctrl Pts',(-24.487649165391,27.2380290029044,23.0545793679079));
#73847=CARTESIAN_POINT('Ctrl Pts',(-27.1595433709243,24.7550045345219,23.2534662792827));
#73848=CARTESIAN_POINT('Ctrl Pts',(-26.5148053126048,21.1649151216697,23.4523531906577));
#73849=CARTESIAN_POINT('Ctrl Pts',(-23.145894601252,19.766748545362,23.6512401020325));
#73850=CARTESIAN_POINT('Ctrl Pts',(-20.1485545440809,21.8453013442694,23.8501270134075));
#73851=CARTESIAN_POINT('Ctrl Pts',(-20.2770865210912,25.4905597283727,24.0490139247823));
#73852=CARTESIAN_POINT('Ctrl Pts',(-23.4133805431482,27.3528403096971,24.2479008361572));
#73853=CARTESIAN_POINT('Ctrl Pts',(-26.6754483178192,25.7208651292231,24.4467877475321));
#73854=CARTESIAN_POINT('Ctrl Pts',(-27.0657261380023,22.0942810093889,24.645674658907));
#73855=CARTESIAN_POINT('Ctrl Pts',(-24.225581776894,19.8056112722044,24.8445615702819));
#73856=CARTESIAN_POINT('Ctrl Pts',(-20.7648670981191,20.9579493598755,25.0434484816568));
#73857=CARTESIAN_POINT('Ctrl Pts',(-19.8636854706927,24.4923942702399,25.2423353930317));
#73858=CARTESIAN_POINT('Ctrl Pts',(-22.3501464036785,27.1610908054883,25.4412223044065));
#73859=CARTESIAN_POINT('Ctrl Pts',(-25.9394031147813,26.5117331116385,25.6401092157814));
#73860=CARTESIAN_POINT('Ctrl Pts',(-27.3332330090641,23.1410258646715,25.8389961271563));
#73861=CARTESIAN_POINT('Ctrl Pts',(-25.250824583827,20.146363213449,26.0378830385312));
#73862=CARTESIAN_POINT('Ctrl Pts',(-21.6057346362272,20.2795862709453,26.2367699499061));
#73863=CARTESIAN_POINT('Ctrl Pts',(-19.7474917499884,23.4182742634268,26.435656861281));
#73864=CARTESIAN_POINT('Ctrl Pts',(-21.3836636326193,26.6782391924832,26.6345437726559));
#73865=CARTESIAN_POINT('Ctrl Pts',(-25.0107469577146,27.0638494048605,26.8334306840308));
#73866=CARTESIAN_POINT('Ctrl Pts',(-27.2957598468497,24.2207623439047,27.0323175954057));
#73867=CARTESIAN_POINT('Ctrl Pts',(-26.1389688684423,20.7615329559886,27.2312045067806));
#73868=CARTESIAN_POINT('Ctrl Pts',(-22.6033674629925,19.864901658791,27.4300914181554));
#73869=CARTESIAN_POINT('Ctrl Pts',(-19.9378723987674,22.3547929966136,27.6289783295304));
#73870=CARTESIAN_POINT('Ctrl Pts',(-20.5918498216416,25.9432147279969,27.8278652409052));
#73871=CARTESIAN_POINT('Ctrl Pts',(-23.9643458145628,27.3326987088365,28.0267521522802));
#73872=CARTESIAN_POINT('Ctrl Pts',(-26.9563302678041,25.2464511781227,28.225639063655));
#73873=CARTESIAN_POINT('Ctrl Pts',(-26.8184084811151,21.601511021257,28.4245259750299));
#73874=CARTESIAN_POINT('Ctrl Pts',(-23.6773465753398,19.7473555135675,28.6234128864048));
#73875=CARTESIAN_POINT('Ctrl Pts',(-20.4194618342357,21.387633386982,28.8222997977797));
#73876=CARTESIAN_POINT('Ctrl Pts',(-20.0385728453635,25.0153760766652,29.0211867091546));
#73877=CARTESIAN_POINT('Ctrl Pts',(-22.8844978638131,27.296414565311,29.2200736205295));
#73878=CARTESIAN_POINT('Ctrl Pts',(-26.3424251341972,26.135765169103,29.4189605319043));
#73879=CARTESIAN_POINT('Ctrl Pts',(-27.2341477796763,22.5978934450653,29.6178474432793));
#73880=CARTESIAN_POINT('Ctrl Pts',(-24.7415051702057,19.9377250765665,29.8167343546542));
#73881=CARTESIAN_POINT('Ctrl Pts',(-21.1526397381544,20.5922624614815,30.0156212660291));
#73882=CARTESIAN_POINT('Ctrl Pts',(-19.7700134152175,23.9746450020287,30.2145081774039));
#73883=CARTESIAN_POINT('Ctrl Pts',(-21.1596874956222,25.9551180584479,30.3470994516539));
#73884=CARTESIAN_POINT('Ctrl Pts',(-22.1199161766065,26.4317607972602,30.4133950887789));
#73885=CARTESIAN_POINT('',(-21.6764439629923,20.9249433714536,30.0016351447898));
#73886=CARTESIAN_POINT('Ctrl Pts',(-21.6746633416192,20.9227079640045,30.));
#73887=CARTESIAN_POINT('Ctrl Pts',(-21.6162991313229,20.9552163909426,30.0000000000001));
#73888=CARTESIAN_POINT('Ctrl Pts',(-21.5591356012991,20.9896046533105,30.0000000000001));
#73889=CARTESIAN_POINT('Ctrl Pts',(-21.503273460136,21.0258485698887,30.0000000000001));
#73890=CARTESIAN_POINT('Ctrl Pts',(-21.4177259766631,21.0813526338203,30.));
#73891=CARTESIAN_POINT('Ctrl Pts',(-21.3352292623413,21.1412057073851,30.));
#73892=CARTESIAN_POINT('Ctrl Pts',(-21.2558644350544,21.2050026175341,30.));
#73893=CARTESIAN_POINT('Ctrl Pts',(-21.1739425301015,21.2708550182534,30.));
#73894=CARTESIAN_POINT('Ctrl Pts',(-21.0953570390573,21.3409098039315,30.));
#73895=CARTESIAN_POINT('Ctrl Pts',(-21.020216898794,21.4147745496451,30.));
#73896=CARTESIAN_POINT('Ctrl Pts',(-20.9451050091674,21.4886115242355,30.));
#73897=CARTESIAN_POINT('Ctrl Pts',(-20.8734354129643,21.5662562353673,30.));
#73898=CARTESIAN_POINT('Ctrl Pts',(-20.80534380024,21.6473612898953,30.));
#73899=CARTESIAN_POINT('Ctrl Pts',(-20.7823042330275,21.6748041023109,30.));
#73900=CARTESIAN_POINT('Ctrl Pts',(-20.7596745620235,21.7026434173923,30.));
#73901=CARTESIAN_POINT('Ctrl Pts',(-20.7374608883305,21.7308667324253,30.));
#73902=CARTESIAN_POINT('Ctrl Pts',(-20.7255551836852,21.7459933817826,30.));
#73903=CARTESIAN_POINT('Ctrl Pts',(-20.7137674457841,21.7612325178852,30.));
#73904=CARTESIAN_POINT('Ctrl Pts',(-20.7021130296544,21.7765629307075,30.));
#73905=CARTESIAN_POINT('Ctrl Pts',(-20.6363129063594,21.8631175073289,30.));
#73906=CARTESIAN_POINT('Ctrl Pts',(-20.5746612361573,21.9527016157851,30.));
#73907=CARTESIAN_POINT('Ctrl Pts',(-20.5172553062057,22.044887933698,30.));
#73908=CARTESIAN_POINT('Ctrl Pts',(-20.4582421259944,22.1396552825868,30.));
#73909=CARTESIAN_POINT('Ctrl Pts',(-20.4037151310162,22.2371731196096,29.9999999999999));
#73910=CARTESIAN_POINT('Ctrl Pts',(-20.3538094801165,22.3370248209967,30.));
#73911=CARTESIAN_POINT('Ctrl Pts',(-20.3039038292169,22.4368765223838,30.));
#73912=CARTESIAN_POINT('Ctrl Pts',(-20.2586189951566,22.539062873371,30.));
#73913=CARTESIAN_POINT('Ctrl Pts',(-20.2181277537056,22.6432039299912,29.9999999999999));
#73914=CARTESIAN_POINT('Ctrl Pts',(-20.1978995014436,22.6952297876499,29.9999999999999));
#73915=CARTESIAN_POINT('Ctrl Pts',(-20.1788682282719,22.7477439827443,30.));
#73916=CARTESIAN_POINT('Ctrl Pts',(-20.1610596298732,22.8007016284567,30.));
#73917=CARTESIAN_POINT('Ctrl Pts',(-20.1479433637699,22.8397056285367,30.));
#73918=CARTESIAN_POINT('Ctrl Pts',(-20.1354903970461,22.8789502128354,30.));
#73919=CARTESIAN_POINT('Ctrl Pts',(-20.1237120651554,22.9184178619925,30.));
#73920=CARTESIAN_POINT('Ctrl Pts',(-20.118220135111,22.9368206010388,29.9999999999999));
#73921=CARTESIAN_POINT('Ctrl Pts',(-20.1128766266359,22.9552662915841,29.9999999999999));
#73922=CARTESIAN_POINT('Ctrl Pts',(-20.1076860627291,22.9737395492117,29.9999999999999));
#73923=CARTESIAN_POINT('Ctrl Pts',(-20.0765757289063,23.084461471129,29.9999999999999));
#73924=CARTESIAN_POINT('Ctrl Pts',(-20.0509141219901,23.1963121778044,29.9999999999999));
#73925=CARTESIAN_POINT('Ctrl Pts',(-20.0308372856757,23.3088624101692,30.));
#73926=CARTESIAN_POINT('Ctrl Pts',(-20.0108369308768,23.4209838891087,30.));
#73927=CARTESIAN_POINT('Ctrl Pts',(-19.9963783905913,23.5338004229941,29.9999999999999));
#73928=CARTESIAN_POINT('Ctrl Pts',(-19.9876380605889,23.6469168071079,29.9999999999999));
#73929=CARTESIAN_POINT('Ctrl Pts',(-19.9799173108421,23.7468378963304,30.));
#73930=CARTESIAN_POINT('Ctrl Pts',(-19.9766588595465,23.8469937496122,29.9999999999999));
#73931=CARTESIAN_POINT('Ctrl Pts',(-19.9780163121772,23.9471230379573,29.9999999999999));
#73932=CARTESIAN_POINT('Ctrl Pts',(-19.9790735041223,24.0251043057529,29.9999999999999));
#73933=CARTESIAN_POINT('Ctrl Pts',(-19.9829310173974,24.1030697257942,29.9999999999999));
#73934=CARTESIAN_POINT('Ctrl Pts',(-19.9895131648371,24.1809217806588,29.9999999999999));
#73935=CARTESIAN_POINT('Ctrl Pts',(-19.9915591683848,24.2051214179212,29.9999999999999));
#73936=CARTESIAN_POINT('Ctrl Pts',(-19.9938685241954,24.2293101033187,30.));
#73937=CARTESIAN_POINT('Ctrl Pts',(-19.9964392042166,24.2534849041834,30.));
#73938=CARTESIAN_POINT('Ctrl Pts',(-19.9988085349521,24.2757662065003,30.));
#73939=CARTESIAN_POINT('Ctrl Pts',(-20.0014006070192,24.2980408294194,30.));
#73940=CARTESIAN_POINT('Ctrl Pts',(-20.0042097151299,24.3202756502583,30.));
#73941=CARTESIAN_POINT('Ctrl Pts',(-20.0183122567051,24.4319009323555,30.));
#73942=CARTESIAN_POINT('Ctrl Pts',(-20.0378917318368,24.5426515255195,30.));
#73943=CARTESIAN_POINT('Ctrl Pts',(-20.0626333972095,24.6522326886167,29.9999999999999));
#73944=CARTESIAN_POINT('Ctrl Pts',(-20.0878348626783,24.7638503124199,29.9999999999999));
#73945=CARTESIAN_POINT('Ctrl Pts',(-20.1183922903517,24.8742552772806,30.));
#73946=CARTESIAN_POINT('Ctrl Pts',(-20.1540278013711,24.9831449157989,30.));
#73947=CARTESIAN_POINT('Ctrl Pts',(-20.1903931760521,25.0942647619953,30.));
#73948=CARTESIAN_POINT('Ctrl Pts',(-20.2320469100759,25.2038073279202,29.9999999999999));
#73949=CARTESIAN_POINT('Ctrl Pts',(-20.2787482606345,25.3114493816107,29.9999999999999));
#73950=CARTESIAN_POINT('Ctrl Pts',(-20.3172931777526,25.4002916525151,30.));
#73951=CARTESIAN_POINT('Ctrl Pts',(-20.3592776204364,25.487839474204,30.));
#73952=CARTESIAN_POINT('Ctrl Pts',(-20.4045921510452,25.5739046343225,30.));
#73953=CARTESIAN_POINT('Ctrl Pts',(-20.4146318244921,25.5929728248376,30.));
#73954=CARTESIAN_POINT('Ctrl Pts',(-20.4248350475835,25.6119682021458,30.));
#73955=CARTESIAN_POINT('Ctrl Pts',(-20.4352007754019,25.6308886550293,30.));
#73956=CARTESIAN_POINT('Ctrl Pts',(-20.4443567625954,25.6476009811999,30.));
#73957=CARTESIAN_POINT('Ctrl Pts',(-20.4536352337179,25.6642469447489,30.));
#73958=CARTESIAN_POINT('Ctrl Pts',(-20.4630327056216,25.6808210834781,30.));
#73959=CARTESIAN_POINT('Ctrl Pts',(-20.5226722799696,25.7860062427551,30.));
#73960=CARTESIAN_POINT('Ctrl Pts',(-20.5871297547875,25.8883528199085,30.));
#73961=CARTESIAN_POINT('Ctrl Pts',(-20.6561268215069,25.9875227195612,30.));
#73962=CARTESIAN_POINT('Ctrl Pts',(-20.7250424718538,26.0865755989711,30.));
#73963=CARTESIAN_POINT('Ctrl Pts',(-20.7984873863524,26.1824601011885,30.));
#73964=CARTESIAN_POINT('Ctrl Pts',(-20.8762341567312,26.2748250760474,30.));
#73965=CARTESIAN_POINT('Ctrl Pts',(-20.9113897218986,26.3165907066584,30.));
#73966=CARTESIAN_POINT('Ctrl Pts',(-20.9474255175054,26.3576364424982,30.));
#73967=CARTESIAN_POINT('Ctrl Pts',(-20.9843235564789,26.3979281736167,30.));
#73968=CARTESIAN_POINT('Ctrl Pts',(-21.0055405379232,26.4210965840603,30.));
#73969=CARTESIAN_POINT('Ctrl Pts',(-21.0270476541474,26.4440206793492,30.));
#73970=CARTESIAN_POINT('Ctrl Pts',(-21.0488151960231,26.4666667341842,30.));
#73971=CARTESIAN_POINT('Ctrl Pts',(-21.1342995706145,26.5556011598344,30.));
#73972=CARTESIAN_POINT('Ctrl Pts',(-21.2238508060944,26.6403121960061,30.));
#73973=CARTESIAN_POINT('Ctrl Pts',(-21.3172138848137,26.7204449989692,30.));
#73974=CARTESIAN_POINT('Ctrl Pts',(-21.4093682581618,26.7995403795307,30.));
#73975=CARTESIAN_POINT('Ctrl Pts',(-21.5052368954238,26.8741760552448,30.));
#73976=CARTESIAN_POINT('Ctrl Pts',(-21.6046172148253,26.943984558935,30.));
#73977=CARTESIAN_POINT('Ctrl Pts',(-21.6688134411653,26.9890784218883,30.0000000000001));
#73978=CARTESIAN_POINT('Ctrl Pts',(-21.7344758343746,27.0321574881717,30.));
#73979=CARTESIAN_POINT('Ctrl Pts',(-21.801558056363,27.073114526145,30.));
#73980=CARTESIAN_POINT('Ctrl Pts',(-21.7179950055095,20.8990358449182,30.));
#73981=CARTESIAN_POINT('Ctrl Pts',(-21.7045931386319,20.9082978835791,30.0005450482633));
#73982=CARTESIAN_POINT('Ctrl Pts',(-21.6912615023449,20.917661543581,30.0010900965265));
#73983=CARTESIAN_POINT('Ctrl Pts',(-21.6780016295741,20.9271257482523,30.0016351447898));
#73984=CARTESIAN_POINT('Ctrl Pts',(-21.7974962932627,27.0786396387202,-75.));
#73985=CARTESIAN_POINT('Ctrl Pts',(-21.7283390717874,27.0367793117585,-75.));
#73986=CARTESIAN_POINT('Ctrl Pts',(-21.6606954899468,26.9927043362926,-75.));
#73987=CARTESIAN_POINT('Ctrl Pts',(-21.5946811745421,26.9464145021147,-75.));
#73988=CARTESIAN_POINT('Ctrl Pts',(-21.4964605389816,26.8775413053685,-75.));
#73989=CARTESIAN_POINT('Ctrl Pts',(-21.4018447932092,26.8037666197796,-75.));
#73990=CARTESIAN_POINT('Ctrl Pts',(-21.310988531103,26.7255041388125,-75.));
#73991=CARTESIAN_POINT('Ctrl Pts',(-21.2173740700917,26.6448657787996,-75.));
#73992=CARTESIAN_POINT('Ctrl Pts',(-21.1277502293408,26.5594622355224,-75.));
#73993=CARTESIAN_POINT('Ctrl Pts',(-21.0423302684772,26.4697105300495,-75.));
#73994=CARTESIAN_POINT('Ctrl Pts',(-20.9569103076136,26.3799588245765,-75.));
#73995=CARTESIAN_POINT('Ctrl Pts',(-20.8756938384798,26.2858579924122,-75.));
#73996=CARTESIAN_POINT('Ctrl Pts',(-20.7989446998575,26.1878035336579,-75.));
#73997=CARTESIAN_POINT('Ctrl Pts',(-20.7738469905589,26.1557387789854,-75.));
#73998=CARTESIAN_POINT('Ctrl Pts',(-20.7492274240551,26.123251132326,-75.));
#73999=CARTESIAN_POINT('Ctrl Pts',(-20.7250965081235,26.0903541909719,-75.));
#74000=CARTESIAN_POINT('Ctrl Pts',(-20.7122572410852,26.0728508099985,-75.));
#74001=CARTESIAN_POINT('Ctrl Pts',(-20.6995540939926,26.0552282695939,-75.));
#74002=CARTESIAN_POINT('Ctrl Pts',(-20.6870042731299,26.0375110019382,-75.));
#74003=CARTESIAN_POINT('Ctrl Pts',(-20.6176725248015,25.9396315855219,-75.));
#74004=CARTESIAN_POINT('Ctrl Pts',(-20.5529233324656,25.8387394985084,-75.));
#74005=CARTESIAN_POINT('Ctrl Pts',(-20.4929223796897,25.735229157897,-75.));
#74006=CARTESIAN_POINT('Ctrl Pts',(-20.4330471356119,25.6319356830113,-75.));
#74007=CARTESIAN_POINT('Ctrl Pts',(-20.3778999559587,25.5260340211465,-75.));
#74008=CARTESIAN_POINT('Ctrl Pts',(-20.3276933492384,25.4178965871798,-75.));
#74009=CARTESIAN_POINT('Ctrl Pts',(-20.2785647484585,25.3120810148924,-75.));
#74010=CARTESIAN_POINT('Ctrl Pts',(-20.2341667224708,25.2041238330088,-75.));
#74011=CARTESIAN_POINT('Ctrl Pts',(-20.1947470562131,25.0943679175727,-75.));
#74012=CARTESIAN_POINT('Ctrl Pts',(-20.1639433742703,25.0086014301469,-75.));
#74013=CARTESIAN_POINT('Ctrl Pts',(-20.1361805474816,24.9217363466615,-75.));
#74014=CARTESIAN_POINT('Ctrl Pts',(-20.1115989699483,24.8339383046586,-75.));
#74015=CARTESIAN_POINT('Ctrl Pts',(-20.1046926632002,24.8092710427982,-75.));
#74016=CARTESIAN_POINT('Ctrl Pts',(-20.0980375924697,24.7845301610143,-75.));
#74017=CARTESIAN_POINT('Ctrl Pts',(-20.0916371627657,24.7597193987049,-75.));
#74018=CARTESIAN_POINT('Ctrl Pts',(-20.0876060935858,24.7440932761005,-75.));
#74019=CARTESIAN_POINT('Ctrl Pts',(-20.0836783296642,24.7284483005329,-75.));
#74020=CARTESIAN_POINT('Ctrl Pts',(-20.0798548286623,24.7127873583955,-75.));
#74021=CARTESIAN_POINT('Ctrl Pts',(-20.0526442063565,24.6013334889587,-75.));
#74022=CARTESIAN_POINT('Ctrl Pts',(-20.0307017298995,24.4890392161558,-75.));
#74023=CARTESIAN_POINT('Ctrl Pts',(-20.0142207624146,24.376241682378,-75.));
#74024=CARTESIAN_POINT('Ctrl Pts',(-19.9981827954567,24.2664760923835,-75.));
#74025=CARTESIAN_POINT('Ctrl Pts',(-19.9873166714761,24.1562332280512,-75.));
#74026=CARTESIAN_POINT('Ctrl Pts',(-19.9818488412096,24.0458250777531,-75.));
#74027=CARTESIAN_POINT('Ctrl Pts',(-19.9765152055089,23.9381266263781,-75.));
#74028=CARTESIAN_POINT('Ctrl Pts',(-19.9763181341626,23.8302703368621,-75.));
#74029=CARTESIAN_POINT('Ctrl Pts',(-19.981514471678,23.7225562298032,-75.));
#74030=CARTESIAN_POINT('Ctrl Pts',(-19.9849161460783,23.6520434273831,-75.));
#74031=CARTESIAN_POINT('Ctrl Pts',(-19.9906302912664,23.5815917845486,-75.));
#74032=CARTESIAN_POINT('Ctrl Pts',(-19.9986155805899,23.5112909714078,-75.));
#74033=CARTESIAN_POINT('Ctrl Pts',(-20.003199291308,23.4709369431902,-75.));
#74034=CARTESIAN_POINT('Ctrl Pts',(-20.0085314577195,23.4306326838506,-75.));
#74035=CARTESIAN_POINT('Ctrl Pts',(-20.0146051507011,23.3903958166286,-75.));
#74036=CARTESIAN_POINT('Ctrl Pts',(-20.0167180048619,23.3763986270134,-75.));
#74037=CARTESIAN_POINT('Ctrl Pts',(-20.0189204354708,23.3624109556746,-75.));
#74038=CARTESIAN_POINT('Ctrl Pts',(-20.0212104245034,23.3484431127975,-75.));
#74039=CARTESIAN_POINT('Ctrl Pts',(-20.0392175037149,23.2386085024456,-75.));
#74040=CARTESIAN_POINT('Ctrl Pts',(-20.0626585270014,23.1298348279055,-75.));
#74041=CARTESIAN_POINT('Ctrl Pts',(-20.0912811900811,23.0224446539065,-75.));
#74042=CARTESIAN_POINT('Ctrl Pts',(-20.1201672662221,22.9140661730397,-75.));
#74043=CARTESIAN_POINT('Ctrl Pts',(-20.1543313129296,22.8070959786198,-75.));
#74044=CARTESIAN_POINT('Ctrl Pts',(-20.1935634412397,22.7018862508728,-75.));
#74045=CARTESIAN_POINT('Ctrl Pts',(-20.2325205383007,22.5974140809409,-75.));
#74046=CARTESIAN_POINT('Ctrl Pts',(-20.2764755197019,22.4946770802421,-75.));
#74047=CARTESIAN_POINT('Ctrl Pts',(-20.3252627503745,22.3940514342329,-75.));
#74048=CARTESIAN_POINT('Ctrl Pts',(-20.3617588392728,22.3187767676538,-75.));
#74049=CARTESIAN_POINT('Ctrl Pts',(-20.4009599336471,22.2446842016851,-75.));
#74050=CARTESIAN_POINT('Ctrl Pts',(-20.4428084227994,22.1719463370744,-75.));
#74051=CARTESIAN_POINT('Ctrl Pts',(-20.4518866169818,22.1561673096178,-75.));
#74052=CARTESIAN_POINT('Ctrl Pts',(-20.4610894266242,22.1404520873299,-75.));
#74053=CARTESIAN_POINT('Ctrl Pts',(-20.4704163156628,22.1248025261853,-75.));
#74054=CARTESIAN_POINT('Ctrl Pts',(-20.4793717463345,22.1097762340002,-75.));
#74055=CARTESIAN_POINT('Ctrl Pts',(-20.488436133018,22.0948196004795,-75.));
#74056=CARTESIAN_POINT('Ctrl Pts',(-20.4976085941122,22.0799340839653,-75.));
#74057=CARTESIAN_POINT('Ctrl Pts',(-20.5553350202004,21.986252828736,-75.));
#74058=CARTESIAN_POINT('Ctrl Pts',(-20.6173400240107,21.895383719604,-75.));
#74059=CARTESIAN_POINT('Ctrl Pts',(-20.6834436914446,21.8076804756593,-75.));
#74060=CARTESIAN_POINT('Ctrl Pts',(-20.7483240396607,21.7216002742469,-75.));
#74061=CARTESIAN_POINT('Ctrl Pts',(-20.8171533747666,21.6385693274253,-75.));
#74062=CARTESIAN_POINT('Ctrl Pts',(-20.8897908208752,21.5589625397611,-75.));
#74063=CARTESIAN_POINT('Ctrl Pts',(-20.9134500760797,21.5330332511329,-75.));
#74064=CARTESIAN_POINT('Ctrl Pts',(-20.9375135358778,21.5074675941264,-75.));
#74065=CARTESIAN_POINT('Ctrl Pts',(-20.961976855156,21.4822796143524,-75.));
#74066=CARTESIAN_POINT('Ctrl Pts',(-20.9752011214181,21.4686636145224,-75.));
#74067=CARTESIAN_POINT('Ctrl Pts',(-20.9885422392495,21.4551579899628,-75.));
#74068=CARTESIAN_POINT('Ctrl Pts',(-21.0019995485501,21.4417650307609,-75.));
#74069=CARTESIAN_POINT('Ctrl Pts',(-21.0162043601948,21.4276281436182,-75.));
#74070=CARTESIAN_POINT('Ctrl Pts',(-21.0305328467645,21.4136225861381,-75.));
#74071=CARTESIAN_POINT('Ctrl Pts',(-21.0449800556171,21.3997543930508,-75.));
#74072=CARTESIAN_POINT('Ctrl Pts',(-21.1211701753906,21.3266178236865,-74.9999999999999));
#74073=CARTESIAN_POINT('Ctrl Pts',(-21.2006943104828,21.257263966122,-75.));
#74074=CARTESIAN_POINT('Ctrl Pts',(-21.2834081447689,21.1920390844365,-75.));
#74075=CARTESIAN_POINT('Ctrl Pts',(-21.3638718580856,21.128588559789,-75.));
#74076=CARTESIAN_POINT('Ctrl Pts',(-21.4473546333109,21.0690451037359,-75.));
#74077=CARTESIAN_POINT('Ctrl Pts',(-21.533742621169,21.0137725358826,-75.));
#74078=CARTESIAN_POINT('Ctrl Pts',(-21.5811798388471,20.9834213620921,-75.));
#74079=CARTESIAN_POINT('Ctrl Pts',(-21.6294933571473,20.9543588180351,-75.));
#74080=CARTESIAN_POINT('Ctrl Pts',(-21.6786659999551,20.9266516823435,-75.));
#74081=CARTESIAN_POINT('Origin',(-23.5502525316942,23.5502525316942,30.));
#74082=CARTESIAN_POINT('Origin',(-23.5502525316942,23.5502525316942,-75.));
#74083=CARTESIAN_POINT('',(0.,0.,0.));
#74084=CARTESIAN_POINT('',(2.47151585579234E-14,3.33497734734616E-14,-19.9969220708054));
#74085=CARTESIAN_POINT('',(5.55111512312578E-15,3.9146944449013E-15,-18.4650076839226));
#74086=CARTESIAN_POINT('',(5.68658834969757E-17,-6.36605498892377E-20,-0.43259455443809));
#74087=CARTESIAN_POINT('',(6.26458658242513E-15,4.211253227731E-15,-61.4650076839226));
#74088=CARTESIAN_POINT('',(6.46059445545329E-15,4.211253227731E-15,-75.4650076839226));
#74089=CARTESIAN_POINT('',(41.6278368866821,-51.5221979860496,-19.9969220708054));
#74090=CARTESIAN_POINT('',(47.1005050633884,-1.80604578171052E-14,-19.9969220708054));
#74091=CARTESIAN_POINT('',(-9.84309628765546E-16,-47.1005050633884,-19.9969220708054));
#74092=UNCERTAINTY_MEASURE_WITH_UNIT(LENGTH_MEASURE(0.01),#74104,
'DISTANCE_ACCURACY_VALUE',
'Maximum model space distance between geometric entities at asserted c
onnectivities');
#74093=UNCERTAINTY_MEASURE_WITH_UNIT(LENGTH_MEASURE(0.01),#74104,
'DISTANCE_ACCURACY_VALUE',
'Maximum model space distance between geometric entities at asserted c
onnectivities');
#74094=UNCERTAINTY_MEASURE_WITH_UNIT(LENGTH_MEASURE(0.01),#74104,
'DISTANCE_ACCURACY_VALUE',
'Maximum model space distance between geometric entities at asserted c
onnectivities');
#74095=UNCERTAINTY_MEASURE_WITH_UNIT(LENGTH_MEASURE(0.01),#74104,
'DISTANCE_ACCURACY_VALUE',
'Maximum model space distance between geometric entities at asserted c
onnectivities');
#74096=UNCERTAINTY_MEASURE_WITH_UNIT(LENGTH_MEASURE(0.01),#74104,
'DISTANCE_ACCURACY_VALUE',
'Maximum model space distance between geometric entities at asserted c
onnectivities');
#74097=UNCERTAINTY_MEASURE_WITH_UNIT(LENGTH_MEASURE(0.01),#74104,
'DISTANCE_ACCURACY_VALUE',
'Maximum model space distance between geometric entities at asserted c
onnectivities');
#74098=(
GEOMETRIC_REPRESENTATION_CONTEXT(3)
GLOBAL_UNCERTAINTY_ASSIGNED_CONTEXT((#74092))
GLOBAL_UNIT_ASSIGNED_CONTEXT((#74104,#74106,#74107))
REPRESENTATION_CONTEXT('','3D')
);
#74099=(
GEOMETRIC_REPRESENTATION_CONTEXT(3)
GLOBAL_UNCERTAINTY_ASSIGNED_CONTEXT((#74093))
GLOBAL_UNIT_ASSIGNED_CONTEXT((#74104,#74106,#74107))
REPRESENTATION_CONTEXT('','3D')
);
#74100=(
GEOMETRIC_REPRESENTATION_CONTEXT(3)
GLOBAL_UNCERTAINTY_ASSIGNED_CONTEXT((#74094))
GLOBAL_UNIT_ASSIGNED_CONTEXT((#74104,#74106,#74107))
REPRESENTATION_CONTEXT('','3D')
);
#74101=(
GEOMETRIC_REPRESENTATION_CONTEXT(3)
GLOBAL_UNCERTAINTY_ASSIGNED_CONTEXT((#74095))
GLOBAL_UNIT_ASSIGNED_CONTEXT((#74104,#74106,#74107))
REPRESENTATION_CONTEXT('','3D')
);
#74102=(
GEOMETRIC_REPRESENTATION_CONTEXT(3)
GLOBAL_UNCERTAINTY_ASSIGNED_CONTEXT((#74096))
GLOBAL_UNIT_ASSIGNED_CONTEXT((#74104,#74106,#74107))
REPRESENTATION_CONTEXT('','3D')
);
#74103=(
GEOMETRIC_REPRESENTATION_CONTEXT(3)
GLOBAL_UNCERTAINTY_ASSIGNED_CONTEXT((#74097))
GLOBAL_UNIT_ASSIGNED_CONTEXT((#74104,#74106,#74107))
REPRESENTATION_CONTEXT('','3D')
);
#74104=(
LENGTH_UNIT()
NAMED_UNIT(*)
SI_UNIT(.MILLI.,.METRE.)
);
#74105=(
LENGTH_UNIT()
NAMED_UNIT(*)
SI_UNIT($,.METRE.)
);
#74106=(
NAMED_UNIT(*)
PLANE_ANGLE_UNIT()
SI_UNIT($,.RADIAN.)
);
#74107=(
NAMED_UNIT(*)
SI_UNIT($,.STERADIAN.)
SOLID_ANGLE_UNIT()
);
#74108=SHAPE_DEFINITION_REPRESENTATION(#74113,#74127);
#74109=SHAPE_DEFINITION_REPRESENTATION(#74114,#74128);
#74110=SHAPE_DEFINITION_REPRESENTATION(#74115,#74129);
#74111=SHAPE_DEFINITION_REPRESENTATION(#74116,#74130);
#74112=SHAPE_DEFINITION_REPRESENTATION(#74117,#74131);
#74113=PRODUCT_DEFINITION_SHAPE('',$,#74133);
#74114=PRODUCT_DEFINITION_SHAPE('',$,#74134);
#74115=PRODUCT_DEFINITION_SHAPE('',$,#74135);
#74116=PRODUCT_DEFINITION_SHAPE('',$,#74136);
#74117=PRODUCT_DEFINITION_SHAPE('',$,#74137);
#74118=PRODUCT_DEFINITION_SHAPE($,$,#38);
#74119=PRODUCT_DEFINITION_SHAPE($,$,#39);
#74120=PRODUCT_DEFINITION_SHAPE($,$,#40);
#74121=PRODUCT_DEFINITION_SHAPE($,$,#41);
#74122=PRODUCT_DEFINITION_SHAPE($,$,#42);
#74123=PRODUCT_DEFINITION_SHAPE($,$,#43);
#74124=PRODUCT_DEFINITION_SHAPE($,$,#44);
#74125=PRODUCT_DEFINITION_SHAPE($,$,#45);
#74126=PRODUCT_DEFINITION_SHAPE($,$,#46);
#74127=SHAPE_REPRESENTATION('',(#4622,#4938,#4939,#4940,#4941,#4942,#4943,
#4944,#4945,#4946),#74098);
#74128=SHAPE_REPRESENTATION('',(#4623),#74099);
#74129=SHAPE_REPRESENTATION('',(#4729),#74100);
#74130=SHAPE_REPRESENTATION('',(#4824),#74101);
#74131=SHAPE_REPRESENTATION('',(#4845),#74102);
#74132=PRODUCT_DEFINITION_CONTEXT('part definition',#74149,'design');
#74133=PRODUCT_DEFINITION('BR-170','BR-170',#74138,#74132);
#74134=PRODUCT_DEFINITION('Top_Part','Top_Part',#74139,#74132);
#74135=PRODUCT_DEFINITION('base','Base',#74140,#74132);
#74136=PRODUCT_DEFINITION('Ring_01','Ring_01',#74141,#74132);
#74137=PRODUCT_DEFINITION('Rod_01','Rod_01',#74142,#74132);
#74138=PRODUCT_DEFINITION_FORMATION('',$,#74151);
#74139=PRODUCT_DEFINITION_FORMATION('',$,#74152);
#74140=PRODUCT_DEFINITION_FORMATION('',$,#74153);
#74141=PRODUCT_DEFINITION_FORMATION('',$,#74154);
#74142=PRODUCT_DEFINITION_FORMATION('',$,#74155);
#74143=PRODUCT_RELATED_PRODUCT_CATEGORY('BR-170','BR-170',(#74151));
#74144=PRODUCT_RELATED_PRODUCT_CATEGORY('Top_Part','Top_Part',(#74152));
#74145=PRODUCT_RELATED_PRODUCT_CATEGORY('Base','Base',(#74153));
#74146=PRODUCT_RELATED_PRODUCT_CATEGORY('Ring_01','Ring_01',(#74154));
#74147=PRODUCT_RELATED_PRODUCT_CATEGORY('Rod_01','Rod_01',(#74155));
#74148=APPLICATION_PROTOCOL_DEFINITION('international standard',
'automotive_design',2009,#74149);
#74149=APPLICATION_CONTEXT(
'Core Data for Automotive Mechanical Design Process');
#74150=PRODUCT_CONTEXT('part definition',#74149,'mechanical');
#74151=PRODUCT('BR-170','BR-170',$,(#74150));
#74152=PRODUCT('Top_Part','Top_Part',$,(#74150));
#74153=PRODUCT('base','Base',$,(#74150));
#74154=PRODUCT('Ring_01','Ring_01',$,(#74150));
#74155=PRODUCT('Rod_01','Rod_01',$,(#74150));
#74156=PRESENTATION_STYLE_ASSIGNMENT((#74160));
#74157=PRESENTATION_STYLE_ASSIGNMENT((#74161));
#74158=PRESENTATION_STYLE_ASSIGNMENT((#74162));
#74159=PRESENTATION_STYLE_ASSIGNMENT((#74163));
#74160=SURFACE_STYLE_USAGE(.BOTH.,#74164);
#74161=SURFACE_STYLE_USAGE(.BOTH.,#74165);
#74162=SURFACE_STYLE_USAGE(.BOTH.,#74166);
#74163=SURFACE_STYLE_USAGE(.BOTH.,#74167);
#74164=SURFACE_SIDE_STYLE('',(#74168));
#74165=SURFACE_SIDE_STYLE('',(#74169));
#74166=SURFACE_SIDE_STYLE('',(#74170));
#74167=SURFACE_SIDE_STYLE('',(#74171));
#74168=SURFACE_STYLE_FILL_AREA(#74172);
#74169=SURFACE_STYLE_FILL_AREA(#74173);
#74170=SURFACE_STYLE_FILL_AREA(#74174);
#74171=SURFACE_STYLE_FILL_AREA(#74175);
#74172=FILL_AREA_STYLE('Steel - Satin',(#74176));
#74173=FILL_AREA_STYLE('Opaque(55,55,55)',(#74177));
#74174=FILL_AREA_STYLE('Opaque(52,52,60)',(#74178));
#74175=FILL_AREA_STYLE('Opaque(160,160,160)',(#74179));
#74176=FILL_AREA_STYLE_COLOUR('Steel - Satin',#74180);
#74177=FILL_AREA_STYLE_COLOUR('Opaque(55,55,55)',#74181);
#74178=FILL_AREA_STYLE_COLOUR('Opaque(52,52,60)',#74182);
#74179=FILL_AREA_STYLE_COLOUR('Opaque(160,160,160)',#74183);
#74180=COLOUR_RGB('Steel - Satin', 0.09019608, 0.27058824, 0.51372549);
#74181=COLOUR_RGB('Opaque(55,55,55)', 0.09019608, 0.27058824, 0.51372549);
#74182=COLOUR_RGB('Opaque(52,52,60)', 0.31764706, 0.68627451, 0.89019608);
#74183=COLOUR_RGB('Opaque(160,160,160)', 0.40784314, 0.44705882, 0.49803922);
ENDSEC;
END-ISO-10303-21;
